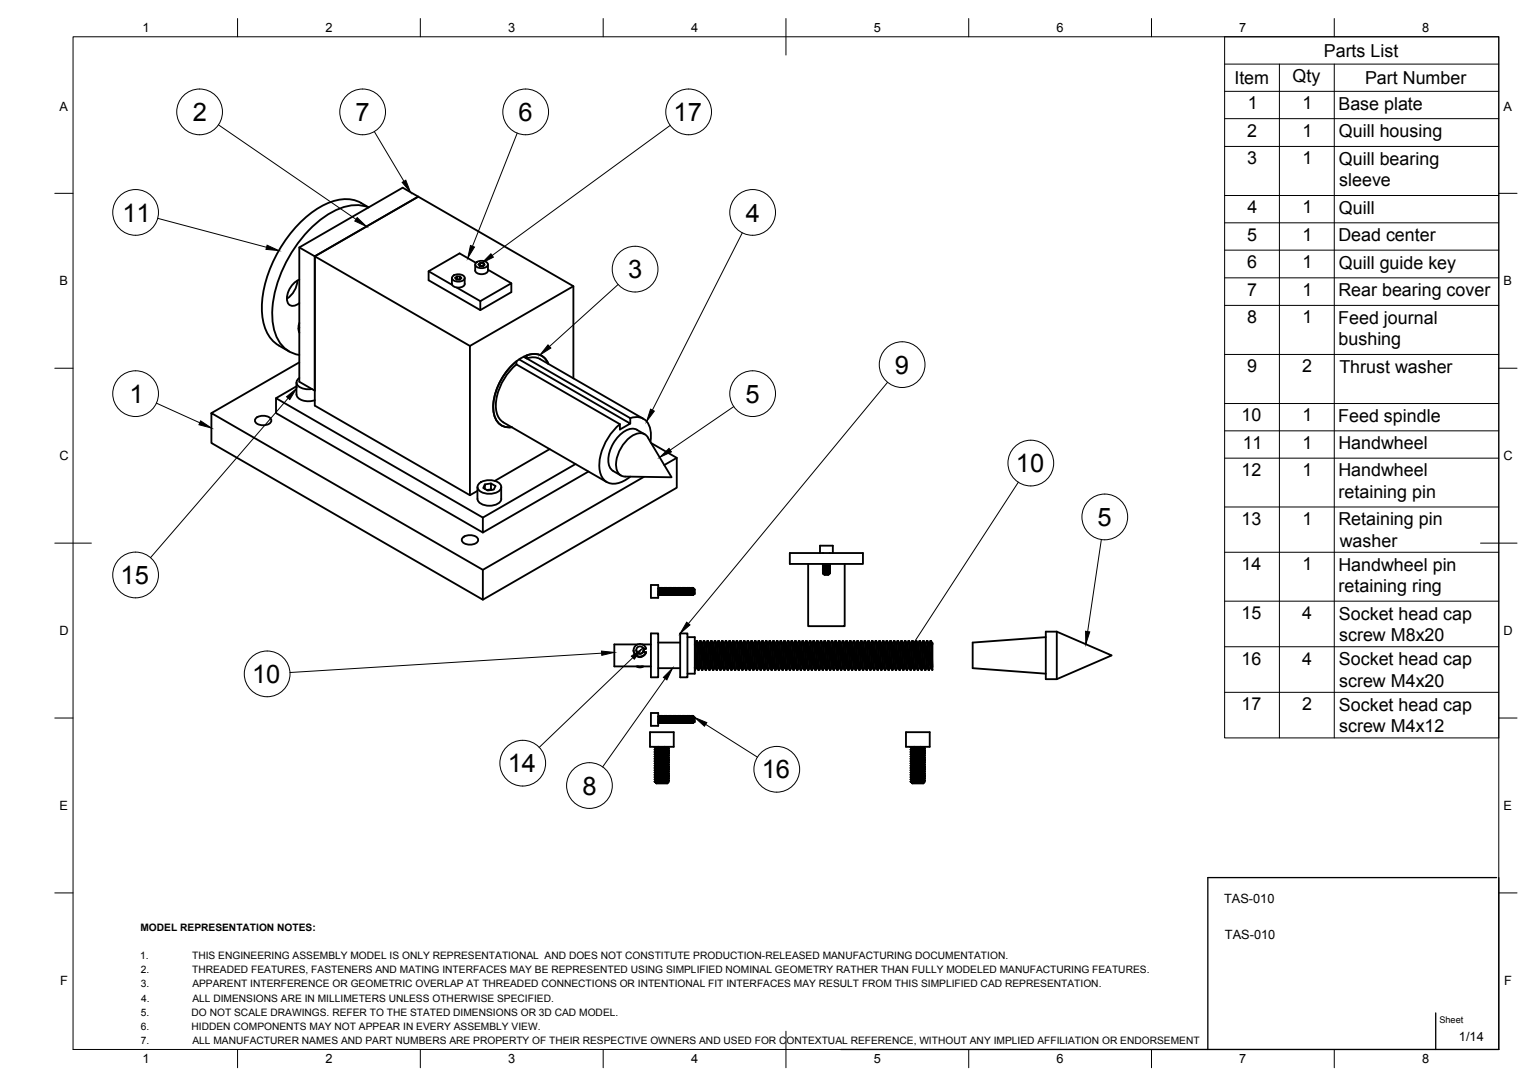
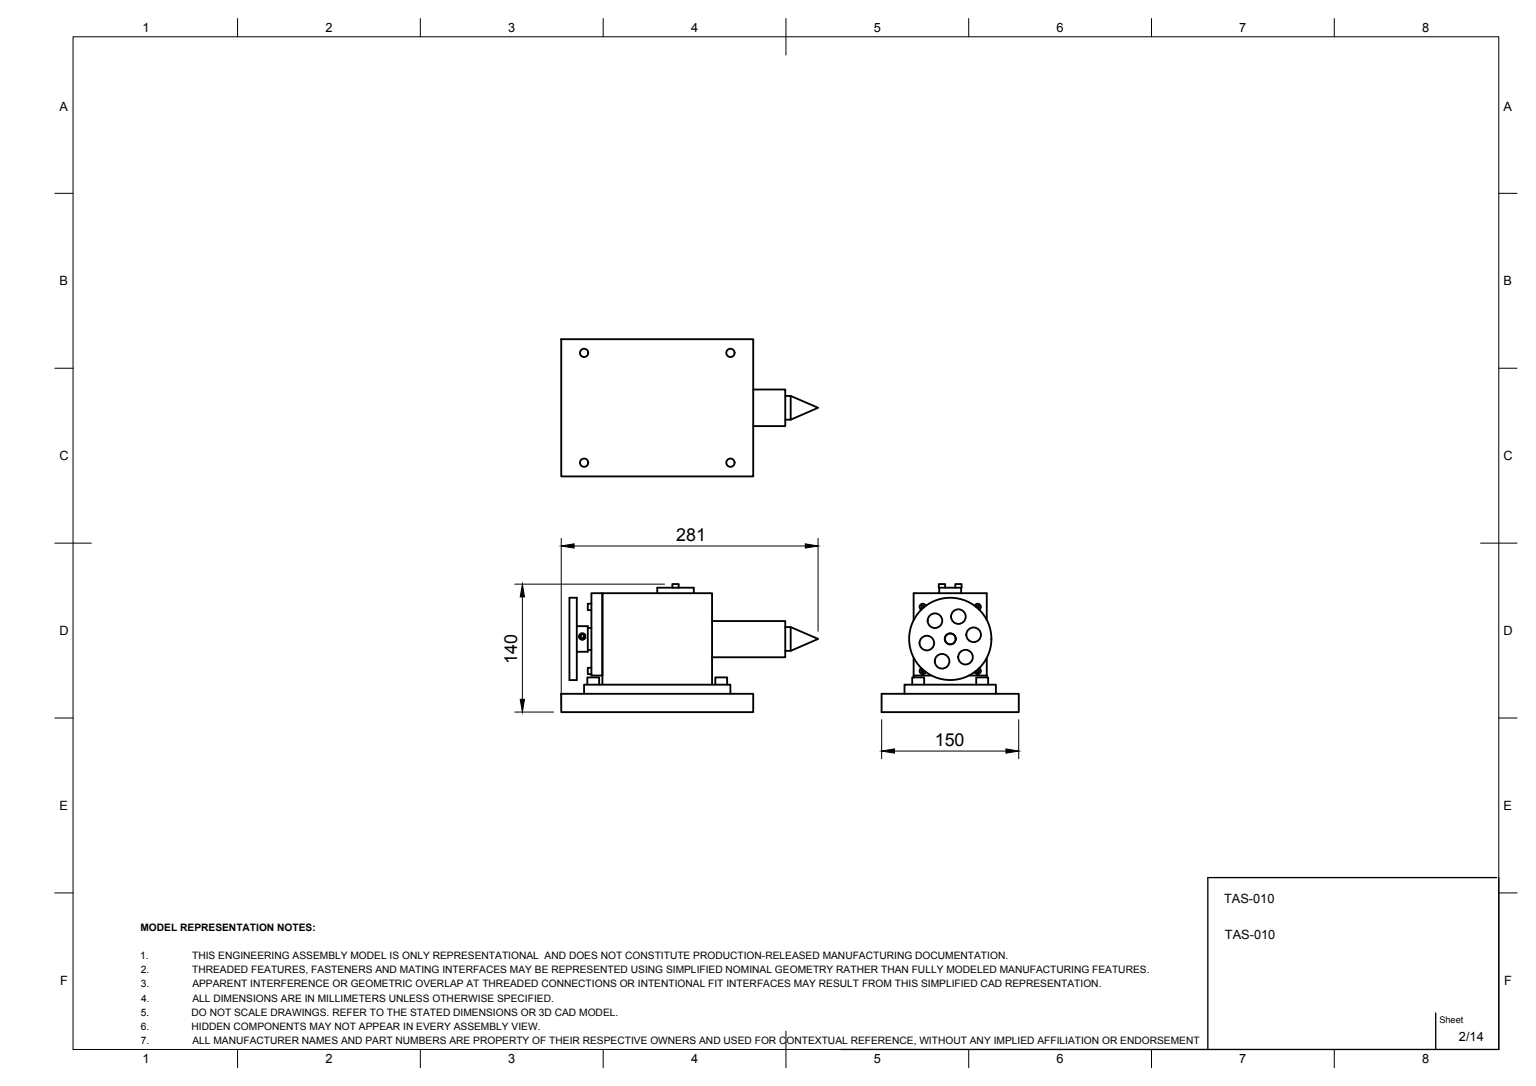
ISO-10303-21;
HEADER;
/* Generated by software containing ST-Developer
 * from STEP Tools, Inc. (www.steptools.com) 
 */

FILE_DESCRIPTION(
/* description */ (
'Independent keyed-quill tailstock, native coupled50mm slider andM16x2
 feed screw, conical dead center, bronze sleeves/thrust washers, cross
-pinned handwheel and bolted guide key. Custom center taper; no standa
rd taper compatibility, machine-bed compatibility or load rating assig
ned.'),
/* implementation_level */ '2;1');

FILE_NAME(
/* name */ 'TAS-010.step',
/* time_stamp */ '2026-11-14T07:17:36-08:00',
/* author */ (''),
/* organization */ (''),
/* preprocessor_version */ 'ST-DEVELOPER v20.2',
/* originating_system */ 'Autodesk Translation Framework v15.17.0.0',
/* authorisation */ '');

FILE_SCHEMA (('AUTOMOTIVE_DESIGN { 1 0 10303 214 3 1 1 }'));
ENDSEC;

DATA;
#10=MECHANICAL_DESIGN_GEOMETRIC_PRESENTATION_REPRESENTATION('',(#153,#154,
#155,#156,#157,#158,#159,#160,#161,#162,#163,#164,#165,#166,#167,#168,#169),
#289387);
#11=ITEM_DEFINED_TRANSFORMATION($,$,#17047,#17864);
#12=ITEM_DEFINED_TRANSFORMATION($,$,#17186,#17865);
#13=ITEM_DEFINED_TRANSFORMATION($,$,#17439,#17866);
#14=ITEM_DEFINED_TRANSFORMATION($,$,#17450,#17867);
#15=ITEM_DEFINED_TRANSFORMATION($,$,#17525,#17868);
#16=ITEM_DEFINED_TRANSFORMATION($,$,#17535,#17869);
#17=ITEM_DEFINED_TRANSFORMATION($,$,#17553,#17870);
#18=ITEM_DEFINED_TRANSFORMATION($,$,#17575,#17871);
#19=ITEM_DEFINED_TRANSFORMATION($,$,#17738,#17872);
#20=ITEM_DEFINED_TRANSFORMATION($,$,#17584,#17873);
#21=ITEM_DEFINED_TRANSFORMATION($,$,#17667,#17874);
#22=ITEM_DEFINED_TRANSFORMATION($,$,#17700,#17875);
#23=ITEM_DEFINED_TRANSFORMATION($,$,#17718,#17876);
#24=ITEM_DEFINED_TRANSFORMATION($,$,#17727,#17877);
#25=ITEM_DEFINED_TRANSFORMATION($,$,#17747,#17878);
#26=ITEM_DEFINED_TRANSFORMATION($,$,#17788,#17879);
#27=ITEM_DEFINED_TRANSFORMATION($,$,#17842,#17880);
#28=ITEM_DEFINED_TRANSFORMATION($,$,#17738,#17881);
#29=ITEM_DEFINED_TRANSFORMATION($,$,#17747,#17882);
#30=ITEM_DEFINED_TRANSFORMATION($,$,#17747,#17883);
#31=ITEM_DEFINED_TRANSFORMATION($,$,#17747,#17884);
#32=ITEM_DEFINED_TRANSFORMATION($,$,#17788,#17885);
#33=ITEM_DEFINED_TRANSFORMATION($,$,#17788,#17886);
#34=ITEM_DEFINED_TRANSFORMATION($,$,#17788,#17887);
#35=ITEM_DEFINED_TRANSFORMATION($,$,#17842,#17888);
#36=(
REPRESENTATION_RELATIONSHIP($,$,#289454,#289453)
REPRESENTATION_RELATIONSHIP_WITH_TRANSFORMATION(#11)
SHAPE_REPRESENTATION_RELATIONSHIP()
);
#37=(
REPRESENTATION_RELATIONSHIP($,$,#289455,#289453)
REPRESENTATION_RELATIONSHIP_WITH_TRANSFORMATION(#12)
SHAPE_REPRESENTATION_RELATIONSHIP()
);
#38=(
REPRESENTATION_RELATIONSHIP($,$,#289456,#289453)
REPRESENTATION_RELATIONSHIP_WITH_TRANSFORMATION(#13)
SHAPE_REPRESENTATION_RELATIONSHIP()
);
#39=(
REPRESENTATION_RELATIONSHIP($,$,#289457,#289453)
REPRESENTATION_RELATIONSHIP_WITH_TRANSFORMATION(#14)
SHAPE_REPRESENTATION_RELATIONSHIP()
);
#40=(
REPRESENTATION_RELATIONSHIP($,$,#289458,#289453)
REPRESENTATION_RELATIONSHIP_WITH_TRANSFORMATION(#15)
SHAPE_REPRESENTATION_RELATIONSHIP()
);
#41=(
REPRESENTATION_RELATIONSHIP($,$,#289459,#289453)
REPRESENTATION_RELATIONSHIP_WITH_TRANSFORMATION(#16)
SHAPE_REPRESENTATION_RELATIONSHIP()
);
#42=(
REPRESENTATION_RELATIONSHIP($,$,#289460,#289453)
REPRESENTATION_RELATIONSHIP_WITH_TRANSFORMATION(#17)
SHAPE_REPRESENTATION_RELATIONSHIP()
);
#43=(
REPRESENTATION_RELATIONSHIP($,$,#289461,#289453)
REPRESENTATION_RELATIONSHIP_WITH_TRANSFORMATION(#18)
SHAPE_REPRESENTATION_RELATIONSHIP()
);
#44=(
REPRESENTATION_RELATIONSHIP($,$,#289467,#289453)
REPRESENTATION_RELATIONSHIP_WITH_TRANSFORMATION(#19)
SHAPE_REPRESENTATION_RELATIONSHIP()
);
#45=(
REPRESENTATION_RELATIONSHIP($,$,#289462,#289453)
REPRESENTATION_RELATIONSHIP_WITH_TRANSFORMATION(#20)
SHAPE_REPRESENTATION_RELATIONSHIP()
);
#46=(
REPRESENTATION_RELATIONSHIP($,$,#289463,#289453)
REPRESENTATION_RELATIONSHIP_WITH_TRANSFORMATION(#21)
SHAPE_REPRESENTATION_RELATIONSHIP()
);
#47=(
REPRESENTATION_RELATIONSHIP($,$,#289464,#289453)
REPRESENTATION_RELATIONSHIP_WITH_TRANSFORMATION(#22)
SHAPE_REPRESENTATION_RELATIONSHIP()
);
#48=(
REPRESENTATION_RELATIONSHIP($,$,#289465,#289453)
REPRESENTATION_RELATIONSHIP_WITH_TRANSFORMATION(#23)
SHAPE_REPRESENTATION_RELATIONSHIP()
);
#49=(
REPRESENTATION_RELATIONSHIP($,$,#289466,#289453)
REPRESENTATION_RELATIONSHIP_WITH_TRANSFORMATION(#24)
SHAPE_REPRESENTATION_RELATIONSHIP()
);
#50=(
REPRESENTATION_RELATIONSHIP($,$,#289468,#289453)
REPRESENTATION_RELATIONSHIP_WITH_TRANSFORMATION(#25)
SHAPE_REPRESENTATION_RELATIONSHIP()
);
#51=(
REPRESENTATION_RELATIONSHIP($,$,#289469,#289453)
REPRESENTATION_RELATIONSHIP_WITH_TRANSFORMATION(#26)
SHAPE_REPRESENTATION_RELATIONSHIP()
);
#52=(
REPRESENTATION_RELATIONSHIP($,$,#289470,#289453)
REPRESENTATION_RELATIONSHIP_WITH_TRANSFORMATION(#27)
SHAPE_REPRESENTATION_RELATIONSHIP()
);
#53=(
REPRESENTATION_RELATIONSHIP($,$,#289467,#289453)
REPRESENTATION_RELATIONSHIP_WITH_TRANSFORMATION(#28)
SHAPE_REPRESENTATION_RELATIONSHIP()
);
#54=(
REPRESENTATION_RELATIONSHIP($,$,#289468,#289453)
REPRESENTATION_RELATIONSHIP_WITH_TRANSFORMATION(#29)
SHAPE_REPRESENTATION_RELATIONSHIP()
);
#55=(
REPRESENTATION_RELATIONSHIP($,$,#289468,#289453)
REPRESENTATION_RELATIONSHIP_WITH_TRANSFORMATION(#30)
SHAPE_REPRESENTATION_RELATIONSHIP()
);
#56=(
REPRESENTATION_RELATIONSHIP($,$,#289468,#289453)
REPRESENTATION_RELATIONSHIP_WITH_TRANSFORMATION(#31)
SHAPE_REPRESENTATION_RELATIONSHIP()
);
#57=(
REPRESENTATION_RELATIONSHIP($,$,#289469,#289453)
REPRESENTATION_RELATIONSHIP_WITH_TRANSFORMATION(#32)
SHAPE_REPRESENTATION_RELATIONSHIP()
);
#58=(
REPRESENTATION_RELATIONSHIP($,$,#289469,#289453)
REPRESENTATION_RELATIONSHIP_WITH_TRANSFORMATION(#33)
SHAPE_REPRESENTATION_RELATIONSHIP()
);
#59=(
REPRESENTATION_RELATIONSHIP($,$,#289469,#289453)
REPRESENTATION_RELATIONSHIP_WITH_TRANSFORMATION(#34)
SHAPE_REPRESENTATION_RELATIONSHIP()
);
#60=(
REPRESENTATION_RELATIONSHIP($,$,#289470,#289453)
REPRESENTATION_RELATIONSHIP_WITH_TRANSFORMATION(#35)
SHAPE_REPRESENTATION_RELATIONSHIP()
);
#61=CONTEXT_DEPENDENT_SHAPE_REPRESENTATION(#36,#289428);
#62=CONTEXT_DEPENDENT_SHAPE_REPRESENTATION(#37,#289429);
#63=CONTEXT_DEPENDENT_SHAPE_REPRESENTATION(#38,#289430);
#64=CONTEXT_DEPENDENT_SHAPE_REPRESENTATION(#39,#289431);
#65=CONTEXT_DEPENDENT_SHAPE_REPRESENTATION(#40,#289432);
#66=CONTEXT_DEPENDENT_SHAPE_REPRESENTATION(#41,#289433);
#67=CONTEXT_DEPENDENT_SHAPE_REPRESENTATION(#42,#289434);
#68=CONTEXT_DEPENDENT_SHAPE_REPRESENTATION(#43,#289435);
#69=CONTEXT_DEPENDENT_SHAPE_REPRESENTATION(#44,#289436);
#70=CONTEXT_DEPENDENT_SHAPE_REPRESENTATION(#45,#289437);
#71=CONTEXT_DEPENDENT_SHAPE_REPRESENTATION(#46,#289438);
#72=CONTEXT_DEPENDENT_SHAPE_REPRESENTATION(#47,#289439);
#73=CONTEXT_DEPENDENT_SHAPE_REPRESENTATION(#48,#289440);
#74=CONTEXT_DEPENDENT_SHAPE_REPRESENTATION(#49,#289441);
#75=CONTEXT_DEPENDENT_SHAPE_REPRESENTATION(#50,#289442);
#76=CONTEXT_DEPENDENT_SHAPE_REPRESENTATION(#51,#289443);
#77=CONTEXT_DEPENDENT_SHAPE_REPRESENTATION(#52,#289444);
#78=CONTEXT_DEPENDENT_SHAPE_REPRESENTATION(#53,#289445);
#79=CONTEXT_DEPENDENT_SHAPE_REPRESENTATION(#54,#289446);
#80=CONTEXT_DEPENDENT_SHAPE_REPRESENTATION(#55,#289447);
#81=CONTEXT_DEPENDENT_SHAPE_REPRESENTATION(#56,#289448);
#82=CONTEXT_DEPENDENT_SHAPE_REPRESENTATION(#57,#289449);
#83=CONTEXT_DEPENDENT_SHAPE_REPRESENTATION(#58,#289450);
#84=CONTEXT_DEPENDENT_SHAPE_REPRESENTATION(#59,#289451);
#85=CONTEXT_DEPENDENT_SHAPE_REPRESENTATION(#60,#289452);
#86=NEXT_ASSEMBLY_USAGE_OCCURRENCE('Base plate:1','Base plate:1',
'Base plate:1',#289472,#289473,'Base plate:1');
#87=NEXT_ASSEMBLY_USAGE_OCCURRENCE('Quill housing:1','Quill housing:1',
'Quill housing:1',#289472,#289474,'Quill housing:1');
#88=NEXT_ASSEMBLY_USAGE_OCCURRENCE('Quill bearing sleeve:1',
'Quill bearing sleeve:1','Quill bearing sleeve:1',#289472,#289475,
'Quill bearing sleeve:1');
#89=NEXT_ASSEMBLY_USAGE_OCCURRENCE('Quill:1','Quill:1','Quill:1',#289472,
#289476,'Quill:1');
#90=NEXT_ASSEMBLY_USAGE_OCCURRENCE('Dead center:1','Dead center:1',
'Dead center:1',#289472,#289477,'Dead center:1');
#91=NEXT_ASSEMBLY_USAGE_OCCURRENCE('Quill guide key:1',
'Quill guide key:1','Quill guide key:1',#289472,#289478,
'Quill guide key:1');
#92=NEXT_ASSEMBLY_USAGE_OCCURRENCE('Rear bearing cover:1',
'Rear bearing cover:1','Rear bearing cover:1',#289472,#289479,
'Rear bearing cover:1');
#93=NEXT_ASSEMBLY_USAGE_OCCURRENCE('Feed journal bushing:1',
'Feed journal bushing:1','Feed journal bushing:1',#289472,#289480,
'Feed journal bushing:1');
#94=NEXT_ASSEMBLY_USAGE_OCCURRENCE('Thrust washer:1','Thrust washer:1',
'Thrust washer:1',#289472,#289486,'Thrust washer:1');
#95=NEXT_ASSEMBLY_USAGE_OCCURRENCE('Feed spindle:1','Feed spindle:1',
'Feed spindle:1',#289472,#289481,'Feed spindle:1');
#96=NEXT_ASSEMBLY_USAGE_OCCURRENCE('Handwheel:1','Handwheel:1',
'Handwheel:1',#289472,#289482,'Handwheel:1');
#97=NEXT_ASSEMBLY_USAGE_OCCURRENCE('Handwheel retaining pin:1',
'Handwheel retaining pin:1','Handwheel retaining pin:1',#289472,#289483,
'Handwheel retaining pin:1');
#98=NEXT_ASSEMBLY_USAGE_OCCURRENCE('Retaining pin washer:1',
'Retaining pin washer:1','Retaining pin washer:1',#289472,#289484,
'Retaining pin washer:1');
#99=NEXT_ASSEMBLY_USAGE_OCCURRENCE('Handwheel pin retaining ring:1',
'Handwheel pin retaining ring:1','Handwheel pin retaining ring:1',#289472,
#289485,'Handwheel pin retaining ring:1');
#100=NEXT_ASSEMBLY_USAGE_OCCURRENCE('Socket head cap screw M8x20:1',
'Socket head cap screw M8x20:1','Socket head cap screw M8x20:1',#289472,
#289487,'Socket head cap screw M8x20:1');
#101=NEXT_ASSEMBLY_USAGE_OCCURRENCE('Socket head cap screw M4x20:1',
'Socket head cap screw M4x20:1','Socket head cap screw M4x20:1',#289472,
#289488,'Socket head cap screw M4x20:1');
#102=NEXT_ASSEMBLY_USAGE_OCCURRENCE('Socket head cap screw M4x12:1',
'Socket head cap screw M4x12:1','Socket head cap screw M4x12:1',#289472,
#289489,'Socket head cap screw M4x12:1');
#103=NEXT_ASSEMBLY_USAGE_OCCURRENCE('Thrust washer:2','Thrust washer:2',
'Thrust washer:2',#289472,#289486,'Thrust washer:2');
#104=NEXT_ASSEMBLY_USAGE_OCCURRENCE('Socket head cap screw M8x20:2',
'Socket head cap screw M8x20:2','Socket head cap screw M8x20:2',#289472,
#289487,'Socket head cap screw M8x20:2');
#105=NEXT_ASSEMBLY_USAGE_OCCURRENCE('Socket head cap screw M8x20:3',
'Socket head cap screw M8x20:3','Socket head cap screw M8x20:3',#289472,
#289487,'Socket head cap screw M8x20:3');
#106=NEXT_ASSEMBLY_USAGE_OCCURRENCE('Socket head cap screw M8x20:4',
'Socket head cap screw M8x20:4','Socket head cap screw M8x20:4',#289472,
#289487,'Socket head cap screw M8x20:4');
#107=NEXT_ASSEMBLY_USAGE_OCCURRENCE('Socket head cap screw M4x20:2',
'Socket head cap screw M4x20:2','Socket head cap screw M4x20:2',#289472,
#289488,'Socket head cap screw M4x20:2');
#108=NEXT_ASSEMBLY_USAGE_OCCURRENCE('Socket head cap screw M4x20:3',
'Socket head cap screw M4x20:3','Socket head cap screw M4x20:3',#289472,
#289488,'Socket head cap screw M4x20:3');
#109=NEXT_ASSEMBLY_USAGE_OCCURRENCE('Socket head cap screw M4x20:4',
'Socket head cap screw M4x20:4','Socket head cap screw M4x20:4',#289472,
#289488,'Socket head cap screw M4x20:4');
#110=NEXT_ASSEMBLY_USAGE_OCCURRENCE('Socket head cap screw M4x12:2',
'Socket head cap screw M4x12:2','Socket head cap screw M4x12:2',#289472,
#289489,'Socket head cap screw M4x12:2');
#111=CONICAL_SURFACE('',#17511,8.5,0.0748598477107669);
#112=CONICAL_SURFACE('',#17528,8.5,0.0748598477107669);
#113=CONICAL_SURFACE('',#17534,13.,0.408907828950925);
#114=CONICAL_SURFACE('',#17748,3.5,0.785398163397448);
#115=CONICAL_SURFACE('',#17774,3.5,0.785398163397448);
#116=CONICAL_SURFACE('',#17789,1.5,0.785398163397448);
#117=CONICAL_SURFACE('',#17828,1.5,0.785398163397448);
#118=CONICAL_SURFACE('',#17849,1.5,0.785398163397449);
#119=SHAPE_REPRESENTATION_RELATIONSHIP('SRR','None',#289454,#136);
#120=SHAPE_REPRESENTATION_RELATIONSHIP('SRR','None',#289455,#137);
#121=SHAPE_REPRESENTATION_RELATIONSHIP('SRR','None',#289456,#138);
#122=SHAPE_REPRESENTATION_RELATIONSHIP('SRR','None',#289457,#139);
#123=SHAPE_REPRESENTATION_RELATIONSHIP('SRR','None',#289458,#140);
#124=SHAPE_REPRESENTATION_RELATIONSHIP('SRR','None',#289459,#141);
#125=SHAPE_REPRESENTATION_RELATIONSHIP('SRR','None',#289460,#142);
#126=SHAPE_REPRESENTATION_RELATIONSHIP('SRR','None',#289461,#143);
#127=SHAPE_REPRESENTATION_RELATIONSHIP('SRR','None',#289462,#144);
#128=SHAPE_REPRESENTATION_RELATIONSHIP('SRR','None',#289463,#145);
#129=SHAPE_REPRESENTATION_RELATIONSHIP('SRR','None',#289464,#146);
#130=SHAPE_REPRESENTATION_RELATIONSHIP('SRR','None',#289465,#147);
#131=SHAPE_REPRESENTATION_RELATIONSHIP('SRR','None',#289466,#148);
#132=SHAPE_REPRESENTATION_RELATIONSHIP('SRR','None',#289467,#149);
#133=SHAPE_REPRESENTATION_RELATIONSHIP('SRR','None',#289468,#150);
#134=SHAPE_REPRESENTATION_RELATIONSHIP('SRR','None',#289469,#151);
#135=SHAPE_REPRESENTATION_RELATIONSHIP('SRR','None',#289470,#152);
#136=ADVANCED_BREP_SHAPE_REPRESENTATION('',(#170),#289370);
#137=ADVANCED_BREP_SHAPE_REPRESENTATION('',(#171),#289371);
#138=ADVANCED_BREP_SHAPE_REPRESENTATION('',(#172),#289372);
#139=ADVANCED_BREP_SHAPE_REPRESENTATION('',(#173),#289373);
#140=ADVANCED_BREP_SHAPE_REPRESENTATION('',(#174),#289374);
#141=ADVANCED_BREP_SHAPE_REPRESENTATION('',(#175),#289375);
#142=ADVANCED_BREP_SHAPE_REPRESENTATION('',(#176),#289376);
#143=ADVANCED_BREP_SHAPE_REPRESENTATION('',(#177),#289377);
#144=ADVANCED_BREP_SHAPE_REPRESENTATION('',(#178),#289378);
#145=ADVANCED_BREP_SHAPE_REPRESENTATION('',(#179),#289379);
#146=ADVANCED_BREP_SHAPE_REPRESENTATION('',(#180),#289380);
#147=ADVANCED_BREP_SHAPE_REPRESENTATION('',(#181),#289381);
#148=ADVANCED_BREP_SHAPE_REPRESENTATION('',(#182),#289382);
#149=ADVANCED_BREP_SHAPE_REPRESENTATION('',(#183),#289383);
#150=ADVANCED_BREP_SHAPE_REPRESENTATION('',(#184),#289384);
#151=ADVANCED_BREP_SHAPE_REPRESENTATION('',(#185),#289385);
#152=ADVANCED_BREP_SHAPE_REPRESENTATION('',(#186),#289386);
#153=STYLED_ITEM('',(#289548),#170);
#154=STYLED_ITEM('',(#289549),#171);
#155=STYLED_ITEM('',(#289550),#172);
#156=STYLED_ITEM('',(#289551),#173);
#157=STYLED_ITEM('',(#289548),#174);
#158=STYLED_ITEM('',(#289552),#175);
#159=STYLED_ITEM('',(#289552),#176);
#160=STYLED_ITEM('',(#289550),#177);
#161=STYLED_ITEM('',(#289548),#178);
#162=STYLED_ITEM('',(#289549),#179);
#163=STYLED_ITEM('',(#289548),#180);
#164=STYLED_ITEM('',(#289550),#181);
#165=STYLED_ITEM('',(#289553),#182);
#166=STYLED_ITEM('',(#289550),#183);
#167=STYLED_ITEM('',(#289553),#184);
#168=STYLED_ITEM('',(#289553),#185);
#169=STYLED_ITEM('',(#289553),#186);
#170=MANIFOLD_SOLID_BREP('Body1',#16841);
#171=MANIFOLD_SOLID_BREP('Body1',#16842);
#172=MANIFOLD_SOLID_BREP('Body1',#16843);
#173=MANIFOLD_SOLID_BREP('Body1',#16844);
#174=MANIFOLD_SOLID_BREP('Body1',#16845);
#175=MANIFOLD_SOLID_BREP('Body1',#16846);
#176=MANIFOLD_SOLID_BREP('Body1',#16847);
#177=MANIFOLD_SOLID_BREP('Body1',#16848);
#178=MANIFOLD_SOLID_BREP('Body1',#16849);
#179=MANIFOLD_SOLID_BREP('Body1',#16850);
#180=MANIFOLD_SOLID_BREP('Body1',#16851);
#181=MANIFOLD_SOLID_BREP('Body1',#16852);
#182=MANIFOLD_SOLID_BREP('Body1',#16853);
#183=MANIFOLD_SOLID_BREP('Body1',#16854);
#184=MANIFOLD_SOLID_BREP('Body1',#16855);
#185=MANIFOLD_SOLID_BREP('Body1',#16856);
#186=MANIFOLD_SOLID_BREP('Body1',#16857);
#187=FACE_BOUND('',#1186,.T.);
#188=FACE_BOUND('',#1187,.T.);
#189=FACE_BOUND('',#1188,.T.);
#190=FACE_BOUND('',#1189,.T.);
#191=FACE_BOUND('',#1190,.T.);
#192=FACE_BOUND('',#1191,.T.);
#193=FACE_BOUND('',#1192,.T.);
#194=FACE_BOUND('',#1193,.T.);
#195=FACE_BOUND('',#1195,.T.);
#196=FACE_BOUND('',#1196,.T.);
#197=FACE_BOUND('',#1197,.T.);
#198=FACE_BOUND('',#1198,.T.);
#199=FACE_BOUND('',#1414,.T.);
#200=FACE_BOUND('',#1416,.T.);
#201=FACE_BOUND('',#1417,.T.);
#202=FACE_BOUND('',#1418,.T.);
#203=FACE_BOUND('',#1419,.T.);
#204=FACE_BOUND('',#1420,.T.);
#205=FACE_BOUND('',#1426,.T.);
#206=FACE_BOUND('',#1427,.T.);
#207=FACE_BOUND('',#1428,.T.);
#208=FACE_BOUND('',#1429,.T.);
#209=FACE_BOUND('',#1432,.T.);
#210=FACE_BOUND('',#1435,.T.);
#211=FACE_BOUND('',#1436,.T.);
#212=FACE_BOUND('',#1437,.T.);
#213=FACE_BOUND('',#1438,.T.);
#214=FACE_BOUND('',#1439,.T.);
#215=FACE_BOUND('',#1441,.T.);
#216=FACE_BOUND('',#1442,.T.);
#217=FACE_BOUND('',#1443,.T.);
#218=FACE_BOUND('',#1502,.T.);
#219=FACE_BOUND('',#1508,.T.);
#220=FACE_BOUND('',#1513,.T.);
#221=FACE_BOUND('',#1517,.T.);
#222=FACE_BOUND('',#1521,.T.);
#223=FACE_BOUND('',#1527,.T.);
#224=FACE_BOUND('',#1528,.T.);
#225=FACE_BOUND('',#1529,.T.);
#226=FACE_BOUND('',#1535,.T.);
#227=FACE_BOUND('',#1536,.T.);
#228=FACE_BOUND('',#1545,.T.);
#229=FACE_BOUND('',#1546,.T.);
#230=FACE_BOUND('',#1547,.T.);
#231=FACE_BOUND('',#1548,.T.);
#232=FACE_BOUND('',#1549,.T.);
#233=FACE_BOUND('',#1558,.T.);
#234=FACE_BOUND('',#1559,.T.);
#235=FACE_BOUND('',#1560,.T.);
#236=FACE_BOUND('',#1561,.T.);
#237=FACE_BOUND('',#1562,.T.);
#238=FACE_BOUND('',#1566,.T.);
#239=FACE_BOUND('',#1568,.T.);
#240=FACE_BOUND('',#1641,.T.);
#241=FACE_BOUND('',#1644,.T.);
#242=FACE_BOUND('',#1646,.T.);
#243=FACE_BOUND('',#1657,.T.);
#244=FACE_BOUND('',#1659,.T.);
#245=FACE_BOUND('',#1661,.T.);
#246=FACE_BOUND('',#1664,.T.);
#247=FACE_BOUND('',#1665,.T.);
#248=FACE_BOUND('',#1666,.T.);
#249=FACE_BOUND('',#1667,.T.);
#250=FACE_BOUND('',#1668,.T.);
#251=FACE_BOUND('',#1669,.T.);
#252=FACE_BOUND('',#1670,.T.);
#253=FACE_BOUND('',#1672,.T.);
#254=FACE_BOUND('',#1673,.T.);
#255=FACE_BOUND('',#1674,.T.);
#256=FACE_BOUND('',#1675,.T.);
#257=FACE_BOUND('',#1676,.T.);
#258=FACE_BOUND('',#1677,.T.);
#259=FACE_BOUND('',#1678,.T.);
#260=FACE_BOUND('',#1681,.T.);
#261=FACE_BOUND('',#1683,.T.);
#262=FACE_BOUND('',#1686,.T.);
#263=FACE_BOUND('',#1694,.T.);
#264=FACE_BOUND('',#1696,.T.);
#265=FACE_BOUND('',#1706,.T.);
#266=FACE_BOUND('',#1708,.T.);
#267=FACE_BOUND('',#1739,.T.);
#268=FACE_BOUND('',#1742,.T.);
#269=FACE_BOUND('',#1786,.T.);
#270=FACE_BOUND('',#1789,.T.);
#271=FACE_BOUND('',#1804,.T.);
#272=FACE_BOUND('',#1807,.T.);
#273=B_SPLINE_SURFACE_WITH_KNOTS('',3,3,((#55782,#55783,#55784,#55785,#55786,
#55787,#55788,#55789,#55790,#55791,#55792,#55793,#55794,#55795,#55796,#55797,
#55798,#55799,#55800,#55801,#55802,#55803,#55804,#55805,#55806,#55807,#55808,
#55809,#55810,#55811,#55812,#55813,#55814,#55815,#55816,#55817,#55818,#55819,
#55820,#55821,#55822,#55823,#55824,#55825,#55826,#55827,#55828,#55829,#55830,
#55831,#55832,#55833,#55834,#55835,#55836,#55837,#55838,#55839,#55840,#55841,
#55842,#55843,#55844,#55845,#55846,#55847,#55848,#55849,#55850,#55851,#55852),
(#55853,#55854,#55855,#55856,#55857,#55858,#55859,#55860,#55861,#55862,
#55863,#55864,#55865,#55866,#55867,#55868,#55869,#55870,#55871,#55872,#55873,
#55874,#55875,#55876,#55877,#55878,#55879,#55880,#55881,#55882,#55883,#55884,
#55885,#55886,#55887,#55888,#55889,#55890,#55891,#55892,#55893,#55894,#55895,
#55896,#55897,#55898,#55899,#55900,#55901,#55902,#55903,#55904,#55905,#55906,
#55907,#55908,#55909,#55910,#55911,#55912,#55913,#55914,#55915,#55916,#55917,
#55918,#55919,#55920,#55921,#55922,#55923),(#55924,#55925,#55926,#55927,
#55928,#55929,#55930,#55931,#55932,#55933,#55934,#55935,#55936,#55937,#55938,
#55939,#55940,#55941,#55942,#55943,#55944,#55945,#55946,#55947,#55948,#55949,
#55950,#55951,#55952,#55953,#55954,#55955,#55956,#55957,#55958,#55959,#55960,
#55961,#55962,#55963,#55964,#55965,#55966,#55967,#55968,#55969,#55970,#55971,
#55972,#55973,#55974,#55975,#55976,#55977,#55978,#55979,#55980,#55981,#55982,
#55983,#55984,#55985,#55986,#55987,#55988,#55989,#55990,#55991,#55992,#55993,
#55994),(#55995,#55996,#55997,#55998,#55999,#56000,#56001,#56002,#56003,
#56004,#56005,#56006,#56007,#56008,#56009,#56010,#56011,#56012,#56013,#56014,
#56015,#56016,#56017,#56018,#56019,#56020,#56021,#56022,#56023,#56024,#56025,
#56026,#56027,#56028,#56029,#56030,#56031,#56032,#56033,#56034,#56035,#56036,
#56037,#56038,#56039,#56040,#56041,#56042,#56043,#56044,#56045,#56046,#56047,
#56048,#56049,#56050,#56051,#56052,#56053,#56054,#56055,#56056,#56057,#56058,
#56059,#56060,#56061,#56062,#56063,#56064,#56065)),.UNSPECIFIED.,.F.,.F.,
 .F.,(4,4),(4,1,1,1,1,1,1,1,1,1,1,1,1,1,1,1,1,1,1,1,1,1,1,1,1,1,1,1,1,1,
1,1,1,1,1,1,1,1,1,1,1,1,1,1,1,1,1,1,1,1,1,1,1,1,1,1,1,1,1,1,1,1,1,1,1,1,
1,1,4),(-0.000703873626500094,0.0807256881124021),(11.8568339491899,12.8481671993964,
13.8387965759765,14.8294259525565,15.8200553291365,16.8106847057165,17.8013140822966,
18.7919434588766,19.7825728354566,20.7732022120367,21.7638315886167,22.7544609651967,
23.7450903417767,24.7357197183568,25.7263490949368,26.7169784715168,27.7076078480968,
28.6982372246769,29.6888666012569,30.6794959778369,31.6701253544169,32.660754730997,
33.651384107577,34.642013484157,35.6326428607371,36.6232722373171,37.6139016138971,
38.6045309904771,39.5951603670572,40.5857897436372,41.5764191202172,42.5670484967972,
43.5576778733773,44.5483072499573,45.5389366265373,46.5295660031174,47.5201953796974,
48.5108247562774,49.5014541328574,50.4920835094375,51.4827128860175,52.4733422625975,
53.4639716391775,54.4546010157576,55.4452303923376,56.4358597689176,57.4264891454977,
58.4171185220777,59.4077478986577,60.3983772752377,61.3890066518178,62.3796360283978,
63.3702654049778,64.3608947815578,65.3515241581379,66.3421535347179,67.3327829112979,
68.3234122878779,69.314041664458,70.304671041038,71.295300417618,72.2859297941981,
73.2765591707781,74.2671885473581,75.2578179239381,76.2484473005182,77.2390766770982,
78.2297060536782,79.2203354302583),.UNSPECIFIED.);
#274=B_SPLINE_SURFACE_WITH_KNOTS('',3,3,((#56163,#56164,#56165,#56166,#56167,
#56168,#56169,#56170,#56171,#56172,#56173,#56174,#56175,#56176,#56177,#56178,
#56179,#56180,#56181,#56182,#56183,#56184,#56185,#56186,#56187,#56188,#56189,
#56190,#56191,#56192,#56193,#56194,#56195,#56196,#56197,#56198,#56199,#56200,
#56201,#56202,#56203,#56204,#56205,#56206,#56207,#56208,#56209,#56210,#56211,
#56212,#56213,#56214,#56215,#56216,#56217,#56218,#56219,#56220,#56221,#56222,
#56223,#56224,#56225,#56226,#56227,#56228,#56229,#56230,#56231,#56232,#56233),
(#56234,#56235,#56236,#56237,#56238,#56239,#56240,#56241,#56242,#56243,
#56244,#56245,#56246,#56247,#56248,#56249,#56250,#56251,#56252,#56253,#56254,
#56255,#56256,#56257,#56258,#56259,#56260,#56261,#56262,#56263,#56264,#56265,
#56266,#56267,#56268,#56269,#56270,#56271,#56272,#56273,#56274,#56275,#56276,
#56277,#56278,#56279,#56280,#56281,#56282,#56283,#56284,#56285,#56286,#56287,
#56288,#56289,#56290,#56291,#56292,#56293,#56294,#56295,#56296,#56297,#56298,
#56299,#56300,#56301,#56302,#56303,#56304),(#56305,#56306,#56307,#56308,
#56309,#56310,#56311,#56312,#56313,#56314,#56315,#56316,#56317,#56318,#56319,
#56320,#56321,#56322,#56323,#56324,#56325,#56326,#56327,#56328,#56329,#56330,
#56331,#56332,#56333,#56334,#56335,#56336,#56337,#56338,#56339,#56340,#56341,
#56342,#56343,#56344,#56345,#56346,#56347,#56348,#56349,#56350,#56351,#56352,
#56353,#56354,#56355,#56356,#56357,#56358,#56359,#56360,#56361,#56362,#56363,
#56364,#56365,#56366,#56367,#56368,#56369,#56370,#56371,#56372,#56373,#56374,
#56375),(#56376,#56377,#56378,#56379,#56380,#56381,#56382,#56383,#56384,
#56385,#56386,#56387,#56388,#56389,#56390,#56391,#56392,#56393,#56394,#56395,
#56396,#56397,#56398,#56399,#56400,#56401,#56402,#56403,#56404,#56405,#56406,
#56407,#56408,#56409,#56410,#56411,#56412,#56413,#56414,#56415,#56416,#56417,
#56418,#56419,#56420,#56421,#56422,#56423,#56424,#56425,#56426,#56427,#56428,
#56429,#56430,#56431,#56432,#56433,#56434,#56435,#56436,#56437,#56438,#56439,
#56440,#56441,#56442,#56443,#56444,#56445,#56446)),.UNSPECIFIED.,.F.,.F.,
 .F.,(4,4),(4,1,1,1,1,1,1,1,1,1,1,1,1,1,1,1,1,1,1,1,1,1,1,1,1,1,1,1,1,1,
1,1,1,1,1,1,1,1,1,1,1,1,1,1,1,1,1,1,1,1,1,1,1,1,1,1,1,1,1,1,1,1,1,1,1,1,
1,1,4),(-0.000445042829947342,0.0809843050226073),(14.3991256467175,15.3897550232976,
16.3803843998776,17.3710137764576,18.3616431530376,19.3522725296177,20.3429019061977,
21.3335312827777,22.3241606593577,23.3147900359378,24.3054194125178,25.2960487890978,
26.2866781656778,27.2773075422579,28.2679369188379,29.2585662954179,30.249195671998,
31.239825048578,32.230454425158,33.221083801738,34.2117131783181,35.2023425548981,
36.1929719314781,37.1836013080582,38.1742306846382,39.1648600612182,40.1554894377982,
41.1461188143783,42.1367481909583,43.1273775675383,44.1180069441183,45.1086363206984,
46.0992656972784,47.0898950738584,48.0805244504384,49.0711538270185,50.0617832035985,
51.0524125801785,52.0430419567586,53.0336713333386,54.0243007099186,55.0149300864986,
56.0055594630787,56.9961888396587,57.9868182162387,58.9774475928187,59.9680769693988,
60.9587063459788,61.9493357225588,62.9399650991389,63.9305944757189,64.9212238522989,
65.9118532288789,66.902482605459,67.893111982039,68.883741358619,69.8743707351991,
70.8650001117791,71.8556294883591,72.8462588649391,73.8368882415191,74.8275176180992,
75.8181469946792,76.8087763712592,77.7994057478393,78.7900351244193,79.7806645009993,
80.7712938775793,81.7626270042512),.UNSPECIFIED.);
#275=B_SPLINE_SURFACE_WITH_KNOTS('',3,3,((#56747,#56748,#56749,#56750,#56751,
#56752,#56753,#56754,#56755,#56756,#56757,#56758,#56759,#56760,#56761,#56762,
#56763,#56764,#56765,#56766,#56767,#56768,#56769,#56770,#56771,#56772,#56773,
#56774,#56775,#56776,#56777,#56778,#56779,#56780,#56781,#56782,#56783,#56784,
#56785,#56786,#56787,#56788,#56789,#56790,#56791,#56792,#56793,#56794,#56795,
#56796,#56797,#56798,#56799,#56800,#56801,#56802,#56803,#56804,#56805,#56806,
#56807,#56808,#56809,#56810,#56811,#56812,#56813,#56814,#56815,#56816,#56817),
(#56818,#56819,#56820,#56821,#56822,#56823,#56824,#56825,#56826,#56827,
#56828,#56829,#56830,#56831,#56832,#56833,#56834,#56835,#56836,#56837,#56838,
#56839,#56840,#56841,#56842,#56843,#56844,#56845,#56846,#56847,#56848,#56849,
#56850,#56851,#56852,#56853,#56854,#56855,#56856,#56857,#56858,#56859,#56860,
#56861,#56862,#56863,#56864,#56865,#56866,#56867,#56868,#56869,#56870,#56871,
#56872,#56873,#56874,#56875,#56876,#56877,#56878,#56879,#56880,#56881,#56882,
#56883,#56884,#56885,#56886,#56887,#56888),(#56889,#56890,#56891,#56892,
#56893,#56894,#56895,#56896,#56897,#56898,#56899,#56900,#56901,#56902,#56903,
#56904,#56905,#56906,#56907,#56908,#56909,#56910,#56911,#56912,#56913,#56914,
#56915,#56916,#56917,#56918,#56919,#56920,#56921,#56922,#56923,#56924,#56925,
#56926,#56927,#56928,#56929,#56930,#56931,#56932,#56933,#56934,#56935,#56936,
#56937,#56938,#56939,#56940,#56941,#56942,#56943,#56944,#56945,#56946,#56947,
#56948,#56949,#56950,#56951,#56952,#56953,#56954,#56955,#56956,#56957,#56958,
#56959),(#56960,#56961,#56962,#56963,#56964,#56965,#56966,#56967,#56968,
#56969,#56970,#56971,#56972,#56973,#56974,#56975,#56976,#56977,#56978,#56979,
#56980,#56981,#56982,#56983,#56984,#56985,#56986,#56987,#56988,#56989,#56990,
#56991,#56992,#56993,#56994,#56995,#56996,#56997,#56998,#56999,#57000,#57001,
#57002,#57003,#57004,#57005,#57006,#57007,#57008,#57009,#57010,#57011,#57012,
#57013,#57014,#57015,#57016,#57017,#57018,#57019,#57020,#57021,#57022,#57023,
#57024,#57025,#57026,#57027,#57028,#57029,#57030)),.UNSPECIFIED.,.F.,.F.,
 .F.,(4,4),(4,1,1,1,1,1,1,1,1,1,1,1,1,1,1,1,1,1,1,1,1,1,1,1,1,1,1,1,1,1,
1,1,1,1,1,1,1,1,1,1,1,1,1,1,1,1,1,1,1,1,1,1,1,1,1,1,1,1,1,1,1,1,1,1,1,1,
1,1,4),(-0.000689732099215623,0.0807182050540442),(11.8568480907172,12.8481671993964,
13.8387965759765,14.8294259525565,15.8200553291365,16.8106847057165,17.8013140822966,
18.7919434588766,19.7825728354566,20.7732022120367,21.7638315886167,22.7544609651967,
23.7450903417767,24.7357197183568,25.7263490949368,26.7169784715168,27.7076078480968,
28.6982372246769,29.6888666012569,30.6794959778369,31.6701253544169,32.660754730997,
33.651384107577,34.642013484157,35.6326428607371,36.6232722373171,37.6139016138971,
38.6045309904771,39.5951603670572,40.5857897436372,41.5764191202172,42.5670484967972,
43.5576778733773,44.5483072499573,45.5389366265373,46.5295660031174,47.5201953796974,
48.5108247562774,49.5014541328574,50.4920835094375,51.4827128860175,52.4733422625975,
53.4639716391775,54.4546010157576,55.4452303923376,56.4358597689176,57.4264891454977,
58.4171185220777,59.4077478986577,60.3983772752377,61.3890066518178,62.3796360283978,
63.3702654049778,64.3608947815578,65.3515241581379,66.3421535347179,67.3327829112979,
68.3234122878779,69.314041664458,70.304671041038,71.295300417618,72.2859297941981,
73.2765591707781,74.2671885473581,75.2578179239381,76.2484473005182,77.2390766770982,
78.2297060536782,79.2203354302583),.UNSPECIFIED.);
#276=B_SPLINE_SURFACE_WITH_KNOTS('',3,3,((#57125,#57126,#57127,#57128,#57129,
#57130,#57131,#57132,#57133,#57134,#57135,#57136,#57137,#57138,#57139,#57140,
#57141,#57142,#57143,#57144,#57145,#57146,#57147,#57148,#57149,#57150,#57151,
#57152,#57153,#57154,#57155,#57156,#57157,#57158,#57159,#57160,#57161,#57162,
#57163,#57164,#57165,#57166,#57167,#57168,#57169,#57170,#57171,#57172,#57173,
#57174,#57175,#57176,#57177,#57178,#57179,#57180,#57181,#57182,#57183,#57184,
#57185,#57186,#57187,#57188,#57189,#57190,#57191,#57192,#57193,#57194,#57195),
(#57196,#57197,#57198,#57199,#57200,#57201,#57202,#57203,#57204,#57205,
#57206,#57207,#57208,#57209,#57210,#57211,#57212,#57213,#57214,#57215,#57216,
#57217,#57218,#57219,#57220,#57221,#57222,#57223,#57224,#57225,#57226,#57227,
#57228,#57229,#57230,#57231,#57232,#57233,#57234,#57235,#57236,#57237,#57238,
#57239,#57240,#57241,#57242,#57243,#57244,#57245,#57246,#57247,#57248,#57249,
#57250,#57251,#57252,#57253,#57254,#57255,#57256,#57257,#57258,#57259,#57260,
#57261,#57262,#57263,#57264,#57265,#57266),(#57267,#57268,#57269,#57270,
#57271,#57272,#57273,#57274,#57275,#57276,#57277,#57278,#57279,#57280,#57281,
#57282,#57283,#57284,#57285,#57286,#57287,#57288,#57289,#57290,#57291,#57292,
#57293,#57294,#57295,#57296,#57297,#57298,#57299,#57300,#57301,#57302,#57303,
#57304,#57305,#57306,#57307,#57308,#57309,#57310,#57311,#57312,#57313,#57314,
#57315,#57316,#57317,#57318,#57319,#57320,#57321,#57322,#57323,#57324,#57325,
#57326,#57327,#57328,#57329,#57330,#57331,#57332,#57333,#57334,#57335,#57336,
#57337),(#57338,#57339,#57340,#57341,#57342,#57343,#57344,#57345,#57346,
#57347,#57348,#57349,#57350,#57351,#57352,#57353,#57354,#57355,#57356,#57357,
#57358,#57359,#57360,#57361,#57362,#57363,#57364,#57365,#57366,#57367,#57368,
#57369,#57370,#57371,#57372,#57373,#57374,#57375,#57376,#57377,#57378,#57379,
#57380,#57381,#57382,#57383,#57384,#57385,#57386,#57387,#57388,#57389,#57390,
#57391,#57392,#57393,#57394,#57395,#57396,#57397,#57398,#57399,#57400,#57401,
#57402,#57403,#57404,#57405,#57406,#57407,#57408)),.UNSPECIFIED.,.F.,.F.,
 .F.,(4,4),(4,1,1,1,1,1,1,1,1,1,1,1,1,1,1,1,1,1,1,1,1,1,1,1,1,1,1,1,1,1,
1,1,1,1,1,1,1,1,1,1,1,1,1,1,1,1,1,1,1,1,1,1,1,1,1,1,1,1,1,1,1,1,1,1,1,1,
1,1,4),(-0.000437656372986427,0.0809703040897196),(14.3991256467175,15.3897550232976,
16.3803843998776,17.3710137764576,18.3616431530376,19.3522725296177,20.3429019061977,
21.3335312827777,22.3241606593577,23.3147900359378,24.3054194125178,25.2960487890978,
26.2866781656779,27.2773075422579,28.2679369188379,29.2585662954179,30.249195671998,
31.239825048578,32.230454425158,33.221083801738,34.2117131783181,35.2023425548981,
36.1929719314781,37.1836013080582,38.1742306846382,39.1648600612182,40.1554894377982,
41.1461188143783,42.1367481909583,43.1273775675383,44.1180069441183,45.1086363206984,
46.0992656972784,47.0898950738584,48.0805244504385,49.0711538270185,50.0617832035985,
51.0524125801785,52.0430419567586,53.0336713333386,54.0243007099186,55.0149300864986,
56.0055594630787,56.9961888396587,57.9868182162387,58.9774475928188,59.9680769693988,
60.9587063459788,61.9493357225588,62.9399650991389,63.9305944757189,64.9212238522989,
65.911853228879,66.902482605459,67.893111982039,68.883741358619,69.8743707351991,
70.8650001117791,71.8556294883591,72.8462588649391,73.8368882415192,74.8275176180992,
75.8181469946792,76.8087763712593,77.7994057478393,78.7900351244193,79.7806645009993,
80.7712938775794,81.7626130033183),.UNSPECIFIED.);
#277=B_SPLINE_SURFACE_WITH_KNOTS('',3,3,((#57712,#57713,#57714,#57715,#57716,
#57717,#57718,#57719,#57720,#57721,#57722,#57723,#57724,#57725,#57726,#57727,
#57728,#57729,#57730,#57731,#57732,#57733,#57734,#57735,#57736,#57737,#57738,
#57739,#57740,#57741,#57742,#57743,#57744,#57745,#57746,#57747,#57748,#57749,
#57750,#57751,#57752,#57753,#57754,#57755,#57756,#57757,#57758,#57759,#57760,
#57761,#57762,#57763,#57764,#57765,#57766,#57767,#57768,#57769,#57770,#57771,
#57772,#57773,#57774,#57775,#57776,#57777,#57778,#57779,#57780,#57781,#57782),
(#57783,#57784,#57785,#57786,#57787,#57788,#57789,#57790,#57791,#57792,
#57793,#57794,#57795,#57796,#57797,#57798,#57799,#57800,#57801,#57802,#57803,
#57804,#57805,#57806,#57807,#57808,#57809,#57810,#57811,#57812,#57813,#57814,
#57815,#57816,#57817,#57818,#57819,#57820,#57821,#57822,#57823,#57824,#57825,
#57826,#57827,#57828,#57829,#57830,#57831,#57832,#57833,#57834,#57835,#57836,
#57837,#57838,#57839,#57840,#57841,#57842,#57843,#57844,#57845,#57846,#57847,
#57848,#57849,#57850,#57851,#57852,#57853),(#57854,#57855,#57856,#57857,
#57858,#57859,#57860,#57861,#57862,#57863,#57864,#57865,#57866,#57867,#57868,
#57869,#57870,#57871,#57872,#57873,#57874,#57875,#57876,#57877,#57878,#57879,
#57880,#57881,#57882,#57883,#57884,#57885,#57886,#57887,#57888,#57889,#57890,
#57891,#57892,#57893,#57894,#57895,#57896,#57897,#57898,#57899,#57900,#57901,
#57902,#57903,#57904,#57905,#57906,#57907,#57908,#57909,#57910,#57911,#57912,
#57913,#57914,#57915,#57916,#57917,#57918,#57919,#57920,#57921,#57922,#57923,
#57924),(#57925,#57926,#57927,#57928,#57929,#57930,#57931,#57932,#57933,
#57934,#57935,#57936,#57937,#57938,#57939,#57940,#57941,#57942,#57943,#57944,
#57945,#57946,#57947,#57948,#57949,#57950,#57951,#57952,#57953,#57954,#57955,
#57956,#57957,#57958,#57959,#57960,#57961,#57962,#57963,#57964,#57965,#57966,
#57967,#57968,#57969,#57970,#57971,#57972,#57973,#57974,#57975,#57976,#57977,
#57978,#57979,#57980,#57981,#57982,#57983,#57984,#57985,#57986,#57987,#57988,
#57989,#57990,#57991,#57992,#57993,#57994,#57995)),.UNSPECIFIED.,.F.,.F.,
 .F.,(4,4),(4,1,1,1,1,1,1,1,1,1,1,1,1,1,1,1,1,1,1,1,1,1,1,1,1,1,1,1,1,1,
1,1,1,1,1,1,1,1,1,1,1,1,1,1,1,1,1,1,1,1,1,1,1,1,1,1,1,1,1,1,1,1,1,1,1,1,
1,1,4),(-0.000703899666689691,0.0807257072263232),(11.8568339231497,12.8481671993964,
13.8387965759764,14.8294259525565,15.8200553291365,16.8106847057165,17.8013140822965,
18.7919434588766,19.7825728354566,20.7732022120366,21.7638315886167,22.7544609651967,
23.7450903417767,24.7357197183567,25.7263490949368,26.7169784715168,27.7076078480968,
28.6982372246768,29.6888666012569,30.6794959778369,31.6701253544169,32.660754730997,
33.651384107577,34.642013484157,35.632642860737,36.6232722373171,37.6139016138971,
38.6045309904771,39.5951603670571,40.5857897436372,41.5764191202172,42.5670484967972,
43.5576778733773,44.5483072499573,45.5389366265373,46.5295660031173,47.5201953796974,
48.5108247562774,49.5014541328574,50.4920835094374,51.4827128860175,52.4733422625975,
53.4639716391775,54.4546010157575,55.4452303923376,56.4358597689176,57.4264891454976,
58.4171185220777,59.4077478986577,60.3983772752377,61.3890066518177,62.3796360283978,
63.3702654049778,64.3608947815578,65.3515241581378,66.3421535347179,67.3327829112979,
68.3234122878779,69.314041664458,70.304671041038,71.295300417618,72.285929794198,
73.2765591707781,74.2671885473581,75.2578179239381,76.2484473005182,77.2390766770982,
78.2297060536782,79.2203354302582),.UNSPECIFIED.);
#278=B_SPLINE_SURFACE_WITH_KNOTS('',3,3,((#58093,#58094,#58095,#58096,#58097,
#58098,#58099,#58100,#58101,#58102,#58103,#58104,#58105,#58106,#58107,#58108,
#58109,#58110,#58111,#58112,#58113,#58114,#58115,#58116,#58117,#58118,#58119,
#58120,#58121,#58122,#58123,#58124,#58125,#58126,#58127,#58128,#58129,#58130,
#58131,#58132,#58133,#58134,#58135,#58136,#58137,#58138,#58139,#58140,#58141,
#58142,#58143,#58144,#58145,#58146,#58147,#58148,#58149,#58150,#58151,#58152,
#58153,#58154,#58155,#58156,#58157,#58158,#58159,#58160,#58161,#58162,#58163),
(#58164,#58165,#58166,#58167,#58168,#58169,#58170,#58171,#58172,#58173,
#58174,#58175,#58176,#58177,#58178,#58179,#58180,#58181,#58182,#58183,#58184,
#58185,#58186,#58187,#58188,#58189,#58190,#58191,#58192,#58193,#58194,#58195,
#58196,#58197,#58198,#58199,#58200,#58201,#58202,#58203,#58204,#58205,#58206,
#58207,#58208,#58209,#58210,#58211,#58212,#58213,#58214,#58215,#58216,#58217,
#58218,#58219,#58220,#58221,#58222,#58223,#58224,#58225,#58226,#58227,#58228,
#58229,#58230,#58231,#58232,#58233,#58234),(#58235,#58236,#58237,#58238,
#58239,#58240,#58241,#58242,#58243,#58244,#58245,#58246,#58247,#58248,#58249,
#58250,#58251,#58252,#58253,#58254,#58255,#58256,#58257,#58258,#58259,#58260,
#58261,#58262,#58263,#58264,#58265,#58266,#58267,#58268,#58269,#58270,#58271,
#58272,#58273,#58274,#58275,#58276,#58277,#58278,#58279,#58280,#58281,#58282,
#58283,#58284,#58285,#58286,#58287,#58288,#58289,#58290,#58291,#58292,#58293,
#58294,#58295,#58296,#58297,#58298,#58299,#58300,#58301,#58302,#58303,#58304,
#58305),(#58306,#58307,#58308,#58309,#58310,#58311,#58312,#58313,#58314,
#58315,#58316,#58317,#58318,#58319,#58320,#58321,#58322,#58323,#58324,#58325,
#58326,#58327,#58328,#58329,#58330,#58331,#58332,#58333,#58334,#58335,#58336,
#58337,#58338,#58339,#58340,#58341,#58342,#58343,#58344,#58345,#58346,#58347,
#58348,#58349,#58350,#58351,#58352,#58353,#58354,#58355,#58356,#58357,#58358,
#58359,#58360,#58361,#58362,#58363,#58364,#58365,#58366,#58367,#58368,#58369,
#58370,#58371,#58372,#58373,#58374,#58375,#58376)),.UNSPECIFIED.,.F.,.F.,
 .F.,(4,4),(4,1,1,1,1,1,1,1,1,1,1,1,1,1,1,1,1,1,1,1,1,1,1,1,1,1,1,1,1,1,
1,1,1,1,1,1,1,1,1,1,1,1,1,1,1,1,1,1,1,1,1,1,1,1,1,1,1,1,1,1,1,1,1,1,1,1,
1,1,4),(-0.000445070994418236,0.080984343609613),(14.3991256467175,15.3897550232975,
16.3803843998776,17.3710137764576,18.3616431530376,19.3522725296176,20.3429019061977,
21.3335312827777,22.3241606593577,23.3147900359377,24.3054194125178,25.2960487890978,
26.2866781656778,27.2773075422579,28.2679369188379,29.2585662954179,30.2491956719979,
31.239825048578,32.230454425158,33.221083801738,34.211713178318,35.2023425548981,
36.1929719314781,37.1836013080581,38.1742306846382,39.1648600612182,40.1554894377982,
41.1461188143782,42.1367481909583,43.1273775675383,44.1180069441183,45.1086363206983,
46.0992656972784,47.0898950738584,48.0805244504384,49.0711538270185,50.0617832035985,
51.0524125801785,52.0430419567585,53.0336713333386,54.0243007099186,55.0149300864986,
56.0055594630786,56.9961888396587,57.9868182162387,58.9774475928187,59.9680769693988,
60.9587063459788,61.9493357225588,62.9399650991388,63.9305944757189,64.9212238522989,
65.9118532288789,66.9024826054589,67.893111982039,68.883741358619,69.874370735199,
70.8650001117791,71.8556294883591,72.8462588649391,73.8368882415191,74.8275176180992,
75.8181469946792,76.8087763712592,77.7994057478392,78.7900351244193,79.7806645009993,
80.7712938775793,81.7626270428382),.UNSPECIFIED.);
#279=B_SPLINE_SURFACE_WITH_KNOTS('',3,3,((#58677,#58678,#58679,#58680,#58681,
#58682,#58683,#58684,#58685,#58686,#58687,#58688,#58689,#58690,#58691,#58692,
#58693,#58694,#58695,#58696,#58697,#58698,#58699,#58700,#58701,#58702,#58703,
#58704,#58705,#58706,#58707,#58708,#58709,#58710,#58711,#58712,#58713,#58714,
#58715,#58716,#58717,#58718,#58719,#58720,#58721,#58722,#58723,#58724,#58725,
#58726,#58727,#58728,#58729,#58730,#58731,#58732,#58733,#58734,#58735,#58736,
#58737,#58738,#58739,#58740,#58741,#58742,#58743,#58744,#58745,#58746,#58747),
(#58748,#58749,#58750,#58751,#58752,#58753,#58754,#58755,#58756,#58757,
#58758,#58759,#58760,#58761,#58762,#58763,#58764,#58765,#58766,#58767,#58768,
#58769,#58770,#58771,#58772,#58773,#58774,#58775,#58776,#58777,#58778,#58779,
#58780,#58781,#58782,#58783,#58784,#58785,#58786,#58787,#58788,#58789,#58790,
#58791,#58792,#58793,#58794,#58795,#58796,#58797,#58798,#58799,#58800,#58801,
#58802,#58803,#58804,#58805,#58806,#58807,#58808,#58809,#58810,#58811,#58812,
#58813,#58814,#58815,#58816,#58817,#58818),(#58819,#58820,#58821,#58822,
#58823,#58824,#58825,#58826,#58827,#58828,#58829,#58830,#58831,#58832,#58833,
#58834,#58835,#58836,#58837,#58838,#58839,#58840,#58841,#58842,#58843,#58844,
#58845,#58846,#58847,#58848,#58849,#58850,#58851,#58852,#58853,#58854,#58855,
#58856,#58857,#58858,#58859,#58860,#58861,#58862,#58863,#58864,#58865,#58866,
#58867,#58868,#58869,#58870,#58871,#58872,#58873,#58874,#58875,#58876,#58877,
#58878,#58879,#58880,#58881,#58882,#58883,#58884,#58885,#58886,#58887,#58888,
#58889),(#58890,#58891,#58892,#58893,#58894,#58895,#58896,#58897,#58898,
#58899,#58900,#58901,#58902,#58903,#58904,#58905,#58906,#58907,#58908,#58909,
#58910,#58911,#58912,#58913,#58914,#58915,#58916,#58917,#58918,#58919,#58920,
#58921,#58922,#58923,#58924,#58925,#58926,#58927,#58928,#58929,#58930,#58931,
#58932,#58933,#58934,#58935,#58936,#58937,#58938,#58939,#58940,#58941,#58942,
#58943,#58944,#58945,#58946,#58947,#58948,#58949,#58950,#58951,#58952,#58953,
#58954,#58955,#58956,#58957,#58958,#58959,#58960)),.UNSPECIFIED.,.F.,.F.,
 .F.,(4,4),(4,1,1,1,1,1,1,1,1,1,1,1,1,1,1,1,1,1,1,1,1,1,1,1,1,1,1,1,1,1,
1,1,1,1,1,1,1,1,1,1,1,1,1,1,1,1,1,1,1,1,1,1,1,1,1,1,1,1,1,1,1,1,1,1,1,1,
1,1,4),(-0.00068967791227708,0.0807181852368366),(11.8568481449041,12.8481671993964,
13.8387965759765,14.8294259525565,15.8200553291365,16.8106847057165,17.8013140822966,
18.7919434588766,19.7825728354566,20.7732022120367,21.7638315886167,22.7544609651967,
23.7450903417767,24.7357197183568,25.7263490949368,26.7169784715168,27.7076078480968,
28.6982372246769,29.6888666012569,30.6794959778369,31.6701253544169,32.660754730997,
33.651384107577,34.642013484157,35.6326428607371,36.6232722373171,37.6139016138971,
38.6045309904771,39.5951603670572,40.5857897436372,41.5764191202172,42.5670484967972,
43.5576778733773,44.5483072499573,45.5389366265373,46.5295660031174,47.5201953796974,
48.5108247562774,49.5014541328574,50.4920835094375,51.4827128860175,52.4733422625975,
53.4639716391775,54.4546010157576,55.4452303923376,56.4358597689176,57.4264891454977,
58.4171185220777,59.4077478986577,60.3983772752377,61.3890066518178,62.3796360283978,
63.3702654049778,64.3608947815578,65.3515241581379,66.3421535347179,67.3327829112979,
68.3234122878779,69.314041664458,70.304671041038,71.295300417618,72.2859297941981,
73.2765591707781,74.2671885473581,75.2578179239381,76.2484473005182,77.2390766770982,
78.2297060536782,79.2203354302583),.UNSPECIFIED.);
#280=B_SPLINE_SURFACE_WITH_KNOTS('',3,3,((#59055,#59056,#59057,#59058,#59059,
#59060,#59061,#59062,#59063,#59064,#59065,#59066,#59067,#59068,#59069,#59070,
#59071,#59072,#59073,#59074,#59075,#59076,#59077,#59078,#59079,#59080,#59081,
#59082,#59083,#59084,#59085,#59086,#59087,#59088,#59089,#59090,#59091,#59092,
#59093,#59094,#59095,#59096,#59097,#59098,#59099,#59100,#59101,#59102,#59103,
#59104,#59105,#59106,#59107,#59108,#59109,#59110,#59111,#59112,#59113,#59114,
#59115,#59116,#59117,#59118,#59119,#59120,#59121,#59122,#59123,#59124,#59125),
(#59126,#59127,#59128,#59129,#59130,#59131,#59132,#59133,#59134,#59135,
#59136,#59137,#59138,#59139,#59140,#59141,#59142,#59143,#59144,#59145,#59146,
#59147,#59148,#59149,#59150,#59151,#59152,#59153,#59154,#59155,#59156,#59157,
#59158,#59159,#59160,#59161,#59162,#59163,#59164,#59165,#59166,#59167,#59168,
#59169,#59170,#59171,#59172,#59173,#59174,#59175,#59176,#59177,#59178,#59179,
#59180,#59181,#59182,#59183,#59184,#59185,#59186,#59187,#59188,#59189,#59190,
#59191,#59192,#59193,#59194,#59195,#59196),(#59197,#59198,#59199,#59200,
#59201,#59202,#59203,#59204,#59205,#59206,#59207,#59208,#59209,#59210,#59211,
#59212,#59213,#59214,#59215,#59216,#59217,#59218,#59219,#59220,#59221,#59222,
#59223,#59224,#59225,#59226,#59227,#59228,#59229,#59230,#59231,#59232,#59233,
#59234,#59235,#59236,#59237,#59238,#59239,#59240,#59241,#59242,#59243,#59244,
#59245,#59246,#59247,#59248,#59249,#59250,#59251,#59252,#59253,#59254,#59255,
#59256,#59257,#59258,#59259,#59260,#59261,#59262,#59263,#59264,#59265,#59266,
#59267),(#59268,#59269,#59270,#59271,#59272,#59273,#59274,#59275,#59276,
#59277,#59278,#59279,#59280,#59281,#59282,#59283,#59284,#59285,#59286,#59287,
#59288,#59289,#59290,#59291,#59292,#59293,#59294,#59295,#59296,#59297,#59298,
#59299,#59300,#59301,#59302,#59303,#59304,#59305,#59306,#59307,#59308,#59309,
#59310,#59311,#59312,#59313,#59314,#59315,#59316,#59317,#59318,#59319,#59320,
#59321,#59322,#59323,#59324,#59325,#59326,#59327,#59328,#59329,#59330,#59331,
#59332,#59333,#59334,#59335,#59336,#59337,#59338)),.UNSPECIFIED.,.F.,.F.,
 .F.,(4,4),(4,1,1,1,1,1,1,1,1,1,1,1,1,1,1,1,1,1,1,1,1,1,1,1,1,1,1,1,1,1,
1,1,1,1,1,1,1,1,1,1,1,1,1,1,1,1,1,1,1,1,1,1,1,1,1,1,1,1,1,1,1,1,1,1,1,1,
1,1,4),(-0.00043763828538554,0.0809702546783821),(14.3991256467175,15.3897550232976,
16.3803843998776,17.3710137764576,18.3616431530376,19.3522725296177,20.3429019061977,
21.3335312827777,22.3241606593577,23.3147900359378,24.3054194125178,25.2960487890978,
26.2866781656779,27.2773075422579,28.2679369188379,29.2585662954179,30.249195671998,
31.239825048578,32.230454425158,33.221083801738,34.2117131783181,35.2023425548981,
36.1929719314781,37.1836013080582,38.1742306846382,39.1648600612182,40.1554894377982,
41.1461188143783,42.1367481909583,43.1273775675383,44.1180069441183,45.1086363206984,
46.0992656972784,47.0898950738584,48.0805244504385,49.0711538270185,50.0617832035985,
51.0524125801785,52.0430419567586,53.0336713333386,54.0243007099186,55.0149300864986,
56.0055594630787,56.9961888396587,57.9868182162387,58.9774475928188,59.9680769693988,
60.9587063459788,61.9493357225588,62.9399650991389,63.9305944757189,64.9212238522989,
65.911853228879,66.902482605459,67.893111982039,68.883741358619,69.8743707351991,
70.8650001117791,71.8556294883591,72.8462588649391,73.8368882415192,74.8275176180992,
75.8181469946792,76.8087763712593,77.7994057478393,78.7900351244193,79.7806645009993,
80.7712938775794,81.7626129539069),.UNSPECIFIED.);
#281=B_SPLINE_SURFACE_WITH_KNOTS('',3,3,((#129776,#129777,#129778,#129779,
#129780,#129781,#129782,#129783,#129784,#129785,#129786,#129787,#129788,
#129789,#129790,#129791,#129792,#129793,#129794,#129795,#129796,#129797,
#129798,#129799,#129800,#129801,#129802,#129803,#129804,#129805,#129806,
#129807,#129808,#129809,#129810,#129811,#129812,#129813,#129814,#129815,
#129816,#129817,#129818,#129819,#129820,#129821,#129822,#129823,#129824,
#129825,#129826,#129827,#129828,#129829,#129830,#129831,#129832,#129833,
#129834,#129835,#129836,#129837,#129838,#129839,#129840,#129841,#129842,
#129843,#129844,#129845,#129846,#129847,#129848,#129849,#129850,#129851,
#129852,#129853,#129854,#129855,#129856,#129857,#129858,#129859,#129860,
#129861,#129862,#129863,#129864,#129865,#129866,#129867,#129868,#129869,
#129870,#129871,#129872,#129873,#129874,#129875,#129876,#129877,#129878,
#129879),(#129880,#129881,#129882,#129883,#129884,#129885,#129886,#129887,
#129888,#129889,#129890,#129891,#129892,#129893,#129894,#129895,#129896,
#129897,#129898,#129899,#129900,#129901,#129902,#129903,#129904,#129905,
#129906,#129907,#129908,#129909,#129910,#129911,#129912,#129913,#129914,
#129915,#129916,#129917,#129918,#129919,#129920,#129921,#129922,#129923,
#129924,#129925,#129926,#129927,#129928,#129929,#129930,#129931,#129932,
#129933,#129934,#129935,#129936,#129937,#129938,#129939,#129940,#129941,
#129942,#129943,#129944,#129945,#129946,#129947,#129948,#129949,#129950,
#129951,#129952,#129953,#129954,#129955,#129956,#129957,#129958,#129959,
#129960,#129961,#129962,#129963,#129964,#129965,#129966,#129967,#129968,
#129969,#129970,#129971,#129972,#129973,#129974,#129975,#129976,#129977,
#129978,#129979,#129980,#129981,#129982,#129983),(#129984,#129985,#129986,
#129987,#129988,#129989,#129990,#129991,#129992,#129993,#129994,#129995,
#129996,#129997,#129998,#129999,#130000,#130001,#130002,#130003,#130004,
#130005,#130006,#130007,#130008,#130009,#130010,#130011,#130012,#130013,
#130014,#130015,#130016,#130017,#130018,#130019,#130020,#130021,#130022,
#130023,#130024,#130025,#130026,#130027,#130028,#130029,#130030,#130031,
#130032,#130033,#130034,#130035,#130036,#130037,#130038,#130039,#130040,
#130041,#130042,#130043,#130044,#130045,#130046,#130047,#130048,#130049,
#130050,#130051,#130052,#130053,#130054,#130055,#130056,#130057,#130058,
#130059,#130060,#130061,#130062,#130063,#130064,#130065,#130066,#130067,
#130068,#130069,#130070,#130071,#130072,#130073,#130074,#130075,#130076,
#130077,#130078,#130079,#130080,#130081,#130082,#130083,#130084,#130085,
#130086,#130087),(#130088,#130089,#130090,#130091,#130092,#130093,#130094,
#130095,#130096,#130097,#130098,#130099,#130100,#130101,#130102,#130103,
#130104,#130105,#130106,#130107,#130108,#130109,#130110,#130111,#130112,
#130113,#130114,#130115,#130116,#130117,#130118,#130119,#130120,#130121,
#130122,#130123,#130124,#130125,#130126,#130127,#130128,#130129,#130130,
#130131,#130132,#130133,#130134,#130135,#130136,#130137,#130138,#130139,
#130140,#130141,#130142,#130143,#130144,#130145,#130146,#130147,#130148,
#130149,#130150,#130151,#130152,#130153,#130154,#130155,#130156,#130157,
#130158,#130159,#130160,#130161,#130162,#130163,#130164,#130165,#130166,
#130167,#130168,#130169,#130170,#130171,#130172,#130173,#130174,#130175,
#130176,#130177,#130178,#130179,#130180,#130181,#130182,#130183,#130184,
#130185,#130186,#130187,#130188,#130189,#130190,#130191)),.UNSPECIFIED.,
 .F.,.F.,.F.,(4,4),(4,1,1,1,1,1,1,1,1,1,1,1,1,1,1,1,1,1,1,1,1,1,1,1,1,1,
1,1,1,1,1,1,1,1,1,1,1,1,1,1,1,1,1,1,1,1,1,1,1,1,1,1,1,1,1,1,1,1,1,1,1,1,
1,1,1,1,1,1,1,1,1,1,1,1,1,1,1,1,1,1,1,1,1,1,1,1,1,1,1,1,1,1,1,1,1,1,1,1,
1,1,1,4),(-0.000353809570517248,0.0451882118607677),(11.8612261946863,12.8591085386934,
13.85663707313,14.8541656075666,15.8516941420032,16.8492226764398,17.8467512108764,
18.844279745313,19.8418082797496,20.8393368141862,21.8368653486228,22.8343938830594,
23.831922417496,24.8294509519326,25.8269794863692,26.8245080208058,27.8220365552424,
28.819565089679,29.8170936241156,30.8146221585522,31.8121506929888,32.8096792274254,
33.807207761862,34.8047362962986,35.8022648307352,36.7997933651718,37.7973218996084,
38.794850434045,39.7923789684816,40.7899075029182,41.7874360373548,42.7849645717913,
43.782493106228,44.7800216406646,45.7775501751012,46.7750787095378,47.7726072439743,
48.7701357784109,49.7676643128475,50.7651928472842,51.7627213817208,52.7602499161573,
53.7577784505939,54.7553069850305,55.7528355194671,56.7503640539037,57.7478925883403,
58.7454211227769,59.7429496572135,60.7404781916501,61.7380067260867,62.7355352605233,
63.7330637949599,64.7305923293965,65.7281208638331,66.7256493982697,67.7231779327063,
68.7207064671429,69.7182350015795,70.7157635360161,71.7132920704527,72.7108206048893,
73.7083491393259,74.7058776737625,75.7034062081991,76.7009347426357,77.6984632770723,
78.6959918115089,79.6935203459455,80.6910488803821,81.6885774148187,82.6861059492553,
83.6836344836919,84.6811630181285,85.6786915525651,86.6762200870017,87.6737486214383,
88.6712771558749,89.6688056903115,90.6663342247481,91.6638627591847,92.6613912936213,
93.6589198280579,94.6564483624945,95.6539768969311,96.6515054313677,97.6490339658043,
98.6465625002409,99.6440910346775,100.641619569114,101.639148103551,102.636676637987,
103.634205172424,104.631733706861,105.629262241297,106.626790775734,107.62431931017,
108.621847844607,109.619376379044,110.61690491348,111.614433447917,112.611961982353),
 .UNSPECIFIED.);
#282=B_SPLINE_SURFACE_WITH_KNOTS('',3,3,((#130274,#130275,#130276,#130277,
#130278,#130279,#130280,#130281,#130282,#130283,#130284,#130285,#130286,
#130287,#130288,#130289,#130290,#130291,#130292,#130293,#130294,#130295,
#130296,#130297,#130298,#130299,#130300,#130301,#130302,#130303,#130304,
#130305,#130306,#130307,#130308,#130309,#130310,#130311,#130312,#130313,
#130314,#130315,#130316,#130317,#130318,#130319,#130320,#130321,#130322,
#130323,#130324,#130325,#130326,#130327,#130328,#130329,#130330,#130331,
#130332,#130333,#130334,#130335,#130336,#130337,#130338,#130339,#130340,
#130341,#130342,#130343,#130344,#130345,#130346,#130347,#130348,#130349,
#130350,#130351,#130352,#130353,#130354,#130355,#130356,#130357,#130358,
#130359,#130360,#130361,#130362,#130363,#130364,#130365,#130366,#130367,
#130368,#130369,#130370,#130371,#130372,#130373,#130374,#130375,#130376,
#130377),(#130378,#130379,#130380,#130381,#130382,#130383,#130384,#130385,
#130386,#130387,#130388,#130389,#130390,#130391,#130392,#130393,#130394,
#130395,#130396,#130397,#130398,#130399,#130400,#130401,#130402,#130403,
#130404,#130405,#130406,#130407,#130408,#130409,#130410,#130411,#130412,
#130413,#130414,#130415,#130416,#130417,#130418,#130419,#130420,#130421,
#130422,#130423,#130424,#130425,#130426,#130427,#130428,#130429,#130430,
#130431,#130432,#130433,#130434,#130435,#130436,#130437,#130438,#130439,
#130440,#130441,#130442,#130443,#130444,#130445,#130446,#130447,#130448,
#130449,#130450,#130451,#130452,#130453,#130454,#130455,#130456,#130457,
#130458,#130459,#130460,#130461,#130462,#130463,#130464,#130465,#130466,
#130467,#130468,#130469,#130470,#130471,#130472,#130473,#130474,#130475,
#130476,#130477,#130478,#130479,#130480,#130481),(#130482,#130483,#130484,
#130485,#130486,#130487,#130488,#130489,#130490,#130491,#130492,#130493,
#130494,#130495,#130496,#130497,#130498,#130499,#130500,#130501,#130502,
#130503,#130504,#130505,#130506,#130507,#130508,#130509,#130510,#130511,
#130512,#130513,#130514,#130515,#130516,#130517,#130518,#130519,#130520,
#130521,#130522,#130523,#130524,#130525,#130526,#130527,#130528,#130529,
#130530,#130531,#130532,#130533,#130534,#130535,#130536,#130537,#130538,
#130539,#130540,#130541,#130542,#130543,#130544,#130545,#130546,#130547,
#130548,#130549,#130550,#130551,#130552,#130553,#130554,#130555,#130556,
#130557,#130558,#130559,#130560,#130561,#130562,#130563,#130564,#130565,
#130566,#130567,#130568,#130569,#130570,#130571,#130572,#130573,#130574,
#130575,#130576,#130577,#130578,#130579,#130580,#130581,#130582,#130583,
#130584,#130585),(#130586,#130587,#130588,#130589,#130590,#130591,#130592,
#130593,#130594,#130595,#130596,#130597,#130598,#130599,#130600,#130601,
#130602,#130603,#130604,#130605,#130606,#130607,#130608,#130609,#130610,
#130611,#130612,#130613,#130614,#130615,#130616,#130617,#130618,#130619,
#130620,#130621,#130622,#130623,#130624,#130625,#130626,#130627,#130628,
#130629,#130630,#130631,#130632,#130633,#130634,#130635,#130636,#130637,
#130638,#130639,#130640,#130641,#130642,#130643,#130644,#130645,#130646,
#130647,#130648,#130649,#130650,#130651,#130652,#130653,#130654,#130655,
#130656,#130657,#130658,#130659,#130660,#130661,#130662,#130663,#130664,
#130665,#130666,#130667,#130668,#130669,#130670,#130671,#130672,#130673,
#130674,#130675,#130676,#130677,#130678,#130679,#130680,#130681,#130682,
#130683,#130684,#130685,#130686,#130687,#130688,#130689)),.UNSPECIFIED.,
 .F.,.F.,.F.,(4,4),(4,1,1,1,1,1,1,1,1,1,1,1,1,1,1,1,1,1,1,1,1,1,1,1,1,1,
1,1,1,1,1,1,1,1,1,1,1,1,1,1,1,1,1,1,1,1,1,1,1,1,1,1,1,1,1,1,1,1,1,1,1,1,
1,1,1,1,1,1,1,1,1,1,1,1,1,1,1,1,1,1,1,1,1,1,1,1,1,1,1,1,1,1,1,1,1,1,1,1,
1,1,1,4),(-0.000311884246383574,0.0452427689821445),(14.398141012777,15.3956695472136,
16.3931980816502,17.3907266160868,18.3882551505234,19.38578368496,20.3833122193966,
21.3808407538332,22.3783692882698,23.3758978227064,24.373426357143,25.3709548915796,
26.3684834260162,27.3660119604528,28.3635404948894,29.361069029326,30.3585975637626,
31.3561260981992,32.3536546326358,33.3511831670724,34.348711701509,35.3462402359456,
36.3437687703822,37.3412973048188,38.3388258392554,39.336354373692,40.3338829081286,
41.3314114425652,42.3289399770018,43.3264685114384,44.323997045875,45.3215255803116,
46.3190541147482,47.3165826491848,48.3141111836214,49.311639718058,50.3091682524946,
51.3066967869312,52.3042253213678,53.3017538558044,54.299282390241,55.2968109246776,
56.2943394591142,57.2918679935508,58.2893965279874,59.286925062424,60.2844535968606,
61.2819821312972,62.2795106657338,63.2770392001704,64.274567734607,65.2720962690436,
66.2696248034802,67.2671533379168,68.2646818723534,69.26221040679,70.2597389412266,
71.2572674756632,72.2547960100998,73.2523245445364,74.249853078973,75.2473816134096,
76.2449101478462,77.2424386822828,78.2399672167194,79.237495751156,80.2350242855926,
81.2325528200292,82.2300813544658,83.2276098889024,84.225138423339,85.2226669577756,
86.2201954922122,87.2177240266488,88.2152525610854,89.212781095522,90.2103096299586,
91.2078381643952,92.2053666988318,93.2028952332684,94.2004237677049,95.1979523021416,
96.1954808365782,97.1930093710148,98.1905379054514,99.1880664398879,100.185594974325,
101.183123508761,102.180652043198,103.178180577634,104.175709112071,105.173237646508,
106.170766180944,107.168294715381,108.165823249817,109.163351784254,110.160880318691,
111.158408853127,112.155937387564,113.153465922,114.150994456437,115.148876776427),
 .UNSPECIFIED.);
#283=B_SPLINE_SURFACE_WITH_KNOTS('',3,3,((#130957,#130958,#130959,#130960,
#130961,#130962,#130963,#130964,#130965,#130966,#130967,#130968,#130969,
#130970,#130971,#130972,#130973,#130974,#130975,#130976,#130977,#130978,
#130979,#130980,#130981,#130982,#130983,#130984,#130985,#130986,#130987,
#130988,#130989,#130990,#130991,#130992,#130993,#130994,#130995,#130996,
#130997,#130998,#130999,#131000,#131001,#131002,#131003,#131004,#131005,
#131006,#131007,#131008,#131009,#131010,#131011,#131012,#131013,#131014,
#131015,#131016,#131017,#131018,#131019,#131020,#131021,#131022,#131023,
#131024,#131025,#131026,#131027,#131028,#131029,#131030,#131031,#131032,
#131033,#131034,#131035,#131036,#131037,#131038,#131039,#131040,#131041,
#131042,#131043,#131044,#131045,#131046,#131047,#131048,#131049,#131050,
#131051,#131052,#131053,#131054,#131055,#131056,#131057,#131058,#131059,
#131060),(#131061,#131062,#131063,#131064,#131065,#131066,#131067,#131068,
#131069,#131070,#131071,#131072,#131073,#131074,#131075,#131076,#131077,
#131078,#131079,#131080,#131081,#131082,#131083,#131084,#131085,#131086,
#131087,#131088,#131089,#131090,#131091,#131092,#131093,#131094,#131095,
#131096,#131097,#131098,#131099,#131100,#131101,#131102,#131103,#131104,
#131105,#131106,#131107,#131108,#131109,#131110,#131111,#131112,#131113,
#131114,#131115,#131116,#131117,#131118,#131119,#131120,#131121,#131122,
#131123,#131124,#131125,#131126,#131127,#131128,#131129,#131130,#131131,
#131132,#131133,#131134,#131135,#131136,#131137,#131138,#131139,#131140,
#131141,#131142,#131143,#131144,#131145,#131146,#131147,#131148,#131149,
#131150,#131151,#131152,#131153,#131154,#131155,#131156,#131157,#131158,
#131159,#131160,#131161,#131162,#131163,#131164),(#131165,#131166,#131167,
#131168,#131169,#131170,#131171,#131172,#131173,#131174,#131175,#131176,
#131177,#131178,#131179,#131180,#131181,#131182,#131183,#131184,#131185,
#131186,#131187,#131188,#131189,#131190,#131191,#131192,#131193,#131194,
#131195,#131196,#131197,#131198,#131199,#131200,#131201,#131202,#131203,
#131204,#131205,#131206,#131207,#131208,#131209,#131210,#131211,#131212,
#131213,#131214,#131215,#131216,#131217,#131218,#131219,#131220,#131221,
#131222,#131223,#131224,#131225,#131226,#131227,#131228,#131229,#131230,
#131231,#131232,#131233,#131234,#131235,#131236,#131237,#131238,#131239,
#131240,#131241,#131242,#131243,#131244,#131245,#131246,#131247,#131248,
#131249,#131250,#131251,#131252,#131253,#131254,#131255,#131256,#131257,
#131258,#131259,#131260,#131261,#131262,#131263,#131264,#131265,#131266,
#131267,#131268),(#131269,#131270,#131271,#131272,#131273,#131274,#131275,
#131276,#131277,#131278,#131279,#131280,#131281,#131282,#131283,#131284,
#131285,#131286,#131287,#131288,#131289,#131290,#131291,#131292,#131293,
#131294,#131295,#131296,#131297,#131298,#131299,#131300,#131301,#131302,
#131303,#131304,#131305,#131306,#131307,#131308,#131309,#131310,#131311,
#131312,#131313,#131314,#131315,#131316,#131317,#131318,#131319,#131320,
#131321,#131322,#131323,#131324,#131325,#131326,#131327,#131328,#131329,
#131330,#131331,#131332,#131333,#131334,#131335,#131336,#131337,#131338,
#131339,#131340,#131341,#131342,#131343,#131344,#131345,#131346,#131347,
#131348,#131349,#131350,#131351,#131352,#131353,#131354,#131355,#131356,
#131357,#131358,#131359,#131360,#131361,#131362,#131363,#131364,#131365,
#131366,#131367,#131368,#131369,#131370,#131371,#131372)),.UNSPECIFIED.,
 .F.,.F.,.F.,(4,4),(4,1,1,1,1,1,1,1,1,1,1,1,1,1,1,1,1,1,1,1,1,1,1,1,1,1,
1,1,1,1,1,1,1,1,1,1,1,1,1,1,1,1,1,1,1,1,1,1,1,1,1,1,1,1,1,1,1,1,1,1,1,1,
1,1,1,1,1,1,1,1,1,1,1,1,1,1,1,1,1,1,1,1,1,1,1,1,1,1,1,1,1,1,1,1,1,1,1,1,
1,1,1,4),(-0.000353803744797756,0.045188208347436),(11.8612262005118,12.8591085386932,
13.8566370731298,14.8541656075664,15.851694142003,16.8492226764396,17.8467512108762,
18.8442797453128,19.8418082797494,20.839336814186,21.8368653486226,22.8343938830592,
23.8319224174958,24.8294509519324,25.826979486369,26.8245080208056,27.8220365552422,
28.8195650896788,29.8170936241154,30.814622158552,31.8121506929886,32.8096792274252,
33.8072077618618,34.8047362962984,35.802264830735,36.7997933651716,37.7973218996082,
38.7948504340448,39.7923789684814,40.789907502918,41.7874360373546,42.7849645717912,
43.7824931062278,44.7800216406644,45.777550175101,46.7750787095376,47.7726072439742,
48.7701357784108,49.7676643128474,50.765192847284,51.7627213817206,52.7602499161572,
53.7577784505938,54.7553069850304,55.752835519467,56.7503640539036,57.7478925883402,
58.7454211227768,59.7429496572134,60.74047819165,61.7380067260866,62.7355352605232,
63.7330637949598,64.7305923293964,65.728120863833,66.7256493982696,67.7231779327062,
68.7207064671428,69.7182350015794,70.715763536016,71.7132920704526,72.7108206048892,
73.7083491393258,74.7058776737624,75.703406208199,76.7009347426356,77.6984632770722,
78.6959918115088,79.6935203459454,80.691048880382,81.6885774148186,82.6861059492552,
83.6836344836918,84.6811630181284,85.678691552565,86.6762200870016,87.6737486214382,
88.6712771558748,89.6688056903114,90.666334224748,91.6638627591846,92.6613912936212,
93.6589198280578,94.6564483624944,95.653976896931,96.6515054313676,97.6490339658042,
98.6465625002408,99.6440910346774,100.641619569114,101.639148103551,102.636676637987,
103.634205172424,104.63173370686,105.629262241297,106.626790775734,107.62431931017,
108.621847844607,109.619376379043,110.61690491348,111.614433447917,112.611961982353),
 .UNSPECIFIED.);
#284=B_SPLINE_SURFACE_WITH_KNOTS('',3,3,((#131455,#131456,#131457,#131458,
#131459,#131460,#131461,#131462,#131463,#131464,#131465,#131466,#131467,
#131468,#131469,#131470,#131471,#131472,#131473,#131474,#131475,#131476,
#131477,#131478,#131479,#131480,#131481,#131482,#131483,#131484,#131485,
#131486,#131487,#131488,#131489,#131490,#131491,#131492,#131493,#131494,
#131495,#131496,#131497,#131498,#131499,#131500,#131501,#131502,#131503,
#131504,#131505,#131506,#131507,#131508,#131509,#131510,#131511,#131512,
#131513,#131514,#131515,#131516,#131517,#131518,#131519,#131520,#131521,
#131522,#131523,#131524,#131525,#131526,#131527,#131528,#131529,#131530,
#131531,#131532,#131533,#131534,#131535,#131536,#131537,#131538,#131539,
#131540,#131541,#131542,#131543,#131544,#131545,#131546,#131547,#131548,
#131549,#131550,#131551,#131552,#131553,#131554,#131555,#131556,#131557,
#131558),(#131559,#131560,#131561,#131562,#131563,#131564,#131565,#131566,
#131567,#131568,#131569,#131570,#131571,#131572,#131573,#131574,#131575,
#131576,#131577,#131578,#131579,#131580,#131581,#131582,#131583,#131584,
#131585,#131586,#131587,#131588,#131589,#131590,#131591,#131592,#131593,
#131594,#131595,#131596,#131597,#131598,#131599,#131600,#131601,#131602,
#131603,#131604,#131605,#131606,#131607,#131608,#131609,#131610,#131611,
#131612,#131613,#131614,#131615,#131616,#131617,#131618,#131619,#131620,
#131621,#131622,#131623,#131624,#131625,#131626,#131627,#131628,#131629,
#131630,#131631,#131632,#131633,#131634,#131635,#131636,#131637,#131638,
#131639,#131640,#131641,#131642,#131643,#131644,#131645,#131646,#131647,
#131648,#131649,#131650,#131651,#131652,#131653,#131654,#131655,#131656,
#131657,#131658,#131659,#131660,#131661,#131662),(#131663,#131664,#131665,
#131666,#131667,#131668,#131669,#131670,#131671,#131672,#131673,#131674,
#131675,#131676,#131677,#131678,#131679,#131680,#131681,#131682,#131683,
#131684,#131685,#131686,#131687,#131688,#131689,#131690,#131691,#131692,
#131693,#131694,#131695,#131696,#131697,#131698,#131699,#131700,#131701,
#131702,#131703,#131704,#131705,#131706,#131707,#131708,#131709,#131710,
#131711,#131712,#131713,#131714,#131715,#131716,#131717,#131718,#131719,
#131720,#131721,#131722,#131723,#131724,#131725,#131726,#131727,#131728,
#131729,#131730,#131731,#131732,#131733,#131734,#131735,#131736,#131737,
#131738,#131739,#131740,#131741,#131742,#131743,#131744,#131745,#131746,
#131747,#131748,#131749,#131750,#131751,#131752,#131753,#131754,#131755,
#131756,#131757,#131758,#131759,#131760,#131761,#131762,#131763,#131764,
#131765,#131766),(#131767,#131768,#131769,#131770,#131771,#131772,#131773,
#131774,#131775,#131776,#131777,#131778,#131779,#131780,#131781,#131782,
#131783,#131784,#131785,#131786,#131787,#131788,#131789,#131790,#131791,
#131792,#131793,#131794,#131795,#131796,#131797,#131798,#131799,#131800,
#131801,#131802,#131803,#131804,#131805,#131806,#131807,#131808,#131809,
#131810,#131811,#131812,#131813,#131814,#131815,#131816,#131817,#131818,
#131819,#131820,#131821,#131822,#131823,#131824,#131825,#131826,#131827,
#131828,#131829,#131830,#131831,#131832,#131833,#131834,#131835,#131836,
#131837,#131838,#131839,#131840,#131841,#131842,#131843,#131844,#131845,
#131846,#131847,#131848,#131849,#131850,#131851,#131852,#131853,#131854,
#131855,#131856,#131857,#131858,#131859,#131860,#131861,#131862,#131863,
#131864,#131865,#131866,#131867,#131868,#131869,#131870)),.UNSPECIFIED.,
 .F.,.F.,.F.,(4,4),(4,1,1,1,1,1,1,1,1,1,1,1,1,1,1,1,1,1,1,1,1,1,1,1,1,1,
1,1,1,1,1,1,1,1,1,1,1,1,1,1,1,1,1,1,1,1,1,1,1,1,1,1,1,1,1,1,1,1,1,1,1,1,
1,1,1,1,1,1,1,1,1,1,1,1,1,1,1,1,1,1,1,1,1,1,1,1,1,1,1,1,1,1,1,1,1,1,1,1,
1,1,1,4),(-0.000311879380046352,0.0452427611100038),(14.3981410127768,15.3956695472134,
16.39319808165,17.3907266160866,18.3882551505232,19.3857836849598,20.3833122193964,
21.380840753833,22.3783692882696,23.3758978227062,24.3734263571428,25.3709548915794,
26.368483426016,27.3660119604526,28.3635404948892,29.3610690293258,30.3585975637624,
31.356126098199,32.3536546326356,33.3511831670722,34.3487117015088,35.3462402359454,
36.343768770382,37.3412973048186,38.3388258392552,39.3363543736918,40.3338829081284,
41.331411442565,42.3289399770016,43.3264685114382,44.3239970458748,45.3215255803114,
46.319054114748,47.3165826491846,48.3141111836212,49.3116397180578,50.3091682524944,
51.306696786931,52.3042253213676,53.3017538558042,54.2992823902408,55.2968109246774,
56.294339459114,57.2918679935506,58.2893965279872,59.2869250624238,60.2844535968604,
61.281982131297,62.2795106657336,63.2770392001702,64.2745677346068,65.2720962690434,
66.26962480348,67.2671533379166,68.2646818723532,69.2622104067898,70.2597389412264,
71.257267475663,72.2547960100996,73.2523245445362,74.2498530789728,75.2473816134094,
76.244910147846,77.2424386822826,78.2399672167192,79.2374957511558,80.2350242855924,
81.232552820029,82.2300813544656,83.2276098889022,84.2251384233388,85.2226669577754,
86.220195492212,87.2177240266486,88.2152525610852,89.2127810955218,90.2103096299584,
91.207838164395,92.2053666988316,93.2028952332682,94.2004237677048,95.1979523021414,
96.195480836578,97.1930093710146,98.1905379054512,99.1880664398878,100.185594974324,
101.183123508761,102.180652043198,103.178180577634,104.175709112071,105.173237646507,
106.170766180944,107.168294715381,108.165823249817,109.163351784254,110.16088031869,
111.158408853127,112.155937387564,113.153465922,114.150994456437,115.148876768553),
 .UNSPECIFIED.);
#285=B_SPLINE_SURFACE_WITH_KNOTS('',3,3,((#132011,#132012,#132013,#132014,
#132015,#132016,#132017,#132018,#132019,#132020,#132021,#132022,#132023,
#132024,#132025,#132026,#132027,#132028,#132029,#132030,#132031,#132032,
#132033,#132034,#132035,#132036,#132037,#132038,#132039,#132040,#132041,
#132042,#132043,#132044,#132045,#132046,#132047,#132048,#132049,#132050,
#132051,#132052,#132053,#132054,#132055,#132056,#132057,#132058,#132059,
#132060,#132061,#132062,#132063,#132064,#132065,#132066,#132067,#132068,
#132069,#132070,#132071,#132072,#132073,#132074,#132075,#132076,#132077,
#132078,#132079,#132080,#132081,#132082,#132083,#132084,#132085,#132086,
#132087,#132088,#132089,#132090,#132091,#132092,#132093,#132094,#132095,
#132096,#132097,#132098,#132099,#132100,#132101,#132102,#132103,#132104,
#132105),(#132106,#132107,#132108,#132109,#132110,#132111,#132112,#132113,
#132114,#132115,#132116,#132117,#132118,#132119,#132120,#132121,#132122,
#132123,#132124,#132125,#132126,#132127,#132128,#132129,#132130,#132131,
#132132,#132133,#132134,#132135,#132136,#132137,#132138,#132139,#132140,
#132141,#132142,#132143,#132144,#132145,#132146,#132147,#132148,#132149,
#132150,#132151,#132152,#132153,#132154,#132155,#132156,#132157,#132158,
#132159,#132160,#132161,#132162,#132163,#132164,#132165,#132166,#132167,
#132168,#132169,#132170,#132171,#132172,#132173,#132174,#132175,#132176,
#132177,#132178,#132179,#132180,#132181,#132182,#132183,#132184,#132185,
#132186,#132187,#132188,#132189,#132190,#132191,#132192,#132193,#132194,
#132195,#132196,#132197,#132198,#132199,#132200),(#132201,#132202,#132203,
#132204,#132205,#132206,#132207,#132208,#132209,#132210,#132211,#132212,
#132213,#132214,#132215,#132216,#132217,#132218,#132219,#132220,#132221,
#132222,#132223,#132224,#132225,#132226,#132227,#132228,#132229,#132230,
#132231,#132232,#132233,#132234,#132235,#132236,#132237,#132238,#132239,
#132240,#132241,#132242,#132243,#132244,#132245,#132246,#132247,#132248,
#132249,#132250,#132251,#132252,#132253,#132254,#132255,#132256,#132257,
#132258,#132259,#132260,#132261,#132262,#132263,#132264,#132265,#132266,
#132267,#132268,#132269,#132270,#132271,#132272,#132273,#132274,#132275,
#132276,#132277,#132278,#132279,#132280,#132281,#132282,#132283,#132284,
#132285,#132286,#132287,#132288,#132289,#132290,#132291,#132292,#132293,
#132294,#132295),(#132296,#132297,#132298,#132299,#132300,#132301,#132302,
#132303,#132304,#132305,#132306,#132307,#132308,#132309,#132310,#132311,
#132312,#132313,#132314,#132315,#132316,#132317,#132318,#132319,#132320,
#132321,#132322,#132323,#132324,#132325,#132326,#132327,#132328,#132329,
#132330,#132331,#132332,#132333,#132334,#132335,#132336,#132337,#132338,
#132339,#132340,#132341,#132342,#132343,#132344,#132345,#132346,#132347,
#132348,#132349,#132350,#132351,#132352,#132353,#132354,#132355,#132356,
#132357,#132358,#132359,#132360,#132361,#132362,#132363,#132364,#132365,
#132366,#132367,#132368,#132369,#132370,#132371,#132372,#132373,#132374,
#132375,#132376,#132377,#132378,#132379,#132380,#132381,#132382,#132383,
#132384,#132385,#132386,#132387,#132388,#132389,#132390)),.UNSPECIFIED.,
 .F.,.F.,.F.,(4,4),(4,1,1,1,1,1,1,1,1,1,1,1,1,1,1,1,1,1,1,1,1,1,1,1,1,1,
1,1,1,1,1,1,1,1,1,1,1,1,1,1,1,1,1,1,1,1,1,1,1,1,1,1,1,1,1,1,1,1,1,1,1,1,
1,1,1,1,1,1,1,1,1,1,1,1,1,1,1,1,1,1,1,1,1,1,1,1,1,1,1,1,1,1,4),(-0.000348318790885902,
0.0451835916777494),(11.8612316854658,12.8591278626027,13.8566757209488,
14.8542235792949,15.851771437641,16.8493192959871,17.8468671543332,18.8444150126793,
19.8419628710254,20.8395107293714,21.8370585877175,22.8346064460636,23.8321543044097,
24.8297021627558,25.8272500211019,26.824797879448,27.822345737794,28.8198935961401,
29.8174414544862,30.8149893128323,31.8125371711784,32.8100850295245,33.8076328878706,
34.8051807462166,35.8027286045627,36.8002764629088,37.7978243212549,38.795372179601,
39.7929200379471,40.7904678962932,41.7880157546393,42.7855636129853,43.7831114713314,
44.7806593296775,45.7782071880236,46.7757550463697,47.7733029047158,48.7708507630619,
49.768398621408,50.765946479754,51.7634943381001,52.7610421964462,53.7585900547923,
54.7561379131384,55.7536857714845,56.7512336298306,57.7487814881766,58.7463293465227,
59.7438772048688,60.7414250632149,61.738972921561,62.7365207799071,63.7340686382532,
64.7316164965993,65.7291643549453,66.7267122132914,67.7242600716375,68.7218079299836,
69.7193557883297,70.7169036466758,71.7144515050219,72.711999363368,73.709547221714,
74.7070950800601,75.7046429384062,76.7021907967523,77.6997386550984,78.6972865134445,
79.6948343717905,80.6923822301366,81.6899300884827,82.6874779468288,83.6850258051749,
84.682573663521,85.6801215218671,86.6776693802132,87.6752172385592,88.6727650969053,
89.6703129552514,90.6678608135975,91.6654086719436,92.6629565302897,93.6605043886358,
94.6580522469819,95.6556001053279,96.653147963674,97.6506958220201,98.6482436803662,
99.6457915387123,100.643339397058,101.640887255404,102.638435113751,103.635982972097),
 .UNSPECIFIED.);
#286=B_SPLINE_SURFACE_WITH_KNOTS('',3,3,((#132563,#132564,#132565,#132566,
#132567,#132568,#132569,#132570,#132571,#132572,#132573,#132574,#132575,
#132576,#132577,#132578,#132579,#132580,#132581,#132582,#132583,#132584,
#132585,#132586,#132587,#132588,#132589,#132590,#132591,#132592,#132593,
#132594,#132595,#132596,#132597,#132598,#132599,#132600,#132601,#132602,
#132603,#132604,#132605,#132606,#132607,#132608,#132609,#132610,#132611,
#132612,#132613,#132614,#132615,#132616,#132617,#132618,#132619,#132620,
#132621,#132622,#132623,#132624,#132625,#132626,#132627,#132628,#132629,
#132630,#132631,#132632,#132633,#132634,#132635,#132636,#132637,#132638,
#132639,#132640,#132641,#132642,#132643,#132644,#132645,#132646,#132647,
#132648,#132649,#132650,#132651,#132652,#132653,#132654,#132655,#132656,
#132657),(#132658,#132659,#132660,#132661,#132662,#132663,#132664,#132665,
#132666,#132667,#132668,#132669,#132670,#132671,#132672,#132673,#132674,
#132675,#132676,#132677,#132678,#132679,#132680,#132681,#132682,#132683,
#132684,#132685,#132686,#132687,#132688,#132689,#132690,#132691,#132692,
#132693,#132694,#132695,#132696,#132697,#132698,#132699,#132700,#132701,
#132702,#132703,#132704,#132705,#132706,#132707,#132708,#132709,#132710,
#132711,#132712,#132713,#132714,#132715,#132716,#132717,#132718,#132719,
#132720,#132721,#132722,#132723,#132724,#132725,#132726,#132727,#132728,
#132729,#132730,#132731,#132732,#132733,#132734,#132735,#132736,#132737,
#132738,#132739,#132740,#132741,#132742,#132743,#132744,#132745,#132746,
#132747,#132748,#132749,#132750,#132751,#132752),(#132753,#132754,#132755,
#132756,#132757,#132758,#132759,#132760,#132761,#132762,#132763,#132764,
#132765,#132766,#132767,#132768,#132769,#132770,#132771,#132772,#132773,
#132774,#132775,#132776,#132777,#132778,#132779,#132780,#132781,#132782,
#132783,#132784,#132785,#132786,#132787,#132788,#132789,#132790,#132791,
#132792,#132793,#132794,#132795,#132796,#132797,#132798,#132799,#132800,
#132801,#132802,#132803,#132804,#132805,#132806,#132807,#132808,#132809,
#132810,#132811,#132812,#132813,#132814,#132815,#132816,#132817,#132818,
#132819,#132820,#132821,#132822,#132823,#132824,#132825,#132826,#132827,
#132828,#132829,#132830,#132831,#132832,#132833,#132834,#132835,#132836,
#132837,#132838,#132839,#132840,#132841,#132842,#132843,#132844,#132845,
#132846,#132847),(#132848,#132849,#132850,#132851,#132852,#132853,#132854,
#132855,#132856,#132857,#132858,#132859,#132860,#132861,#132862,#132863,
#132864,#132865,#132866,#132867,#132868,#132869,#132870,#132871,#132872,
#132873,#132874,#132875,#132876,#132877,#132878,#132879,#132880,#132881,
#132882,#132883,#132884,#132885,#132886,#132887,#132888,#132889,#132890,
#132891,#132892,#132893,#132894,#132895,#132896,#132897,#132898,#132899,
#132900,#132901,#132902,#132903,#132904,#132905,#132906,#132907,#132908,
#132909,#132910,#132911,#132912,#132913,#132914,#132915,#132916,#132917,
#132918,#132919,#132920,#132921,#132922,#132923,#132924,#132925,#132926,
#132927,#132928,#132929,#132930,#132931,#132932,#132933,#132934,#132935,
#132936,#132937,#132938,#132939,#132940,#132941,#132942)),.UNSPECIFIED.,
 .F.,.F.,.F.,(4,4),(4,1,1,1,1,1,1,1,1,1,1,1,1,1,1,1,1,1,1,1,1,1,1,1,1,1,
1,1,1,1,1,1,1,1,1,1,1,1,1,1,1,1,1,1,1,1,1,1,1,1,1,1,1,1,1,1,1,1,1,1,1,1,
1,1,1,1,1,1,1,1,1,1,1,1,1,1,1,1,1,1,1,1,1,1,1,1,1,1,1,1,1,1,4),(-0.000309367040895943,
0.0452373400660471),(14.3981410127769,15.395688871123,16.3932367294691,
17.3907845878152,18.3883324461612,19.3858803045073,20.3834281628534,21.3809760211995,
22.3785238795456,23.3760717378917,24.3736195962378,25.3711674545839,26.3687153129299,
27.366263171276,28.3638110296221,29.3613588879682,30.3589067463143,31.3564546046604,
32.3540024630065,33.3515503213525,34.3490981796986,35.3466460380447,36.3441938963908,
37.3417417547369,38.339289613083,39.3368374714291,40.3343853297752,41.3319331881212,
42.3294810464673,43.3270289048134,44.3245767631595,45.3221246215056,46.3196724798517,
47.3172203381978,48.3147681965438,49.3123160548899,50.309863913236,51.3074117715821,
52.3049596299282,53.3025074882743,54.3000553466204,55.2976032049664,56.2951510633125,
57.2926989216586,58.2902467800047,59.2877946383508,60.2853424966969,61.282890355043,
62.2804382133891,63.2779860717351,64.2755339300812,65.2730817884273,66.2706296467734,
67.2681775051195,68.2657253634656,69.2632732218117,70.2608210801578,71.2583689385038,
72.2559167968499,73.253464655196,74.2510125135421,75.2485603718882,76.2461082302343,
77.2436560885804,78.2412039469264,79.2387518052725,80.2362996636186,81.2338475219647,
82.2313953803108,83.2289432386569,84.226491097003,85.2240389553491,86.2215868136952,
87.2191346720412,88.2166825303873,89.2142303887334,90.2117782470795,91.2093261054256,
92.2068739637717,93.2044218221178,94.2019696804638,95.1995175388099,96.197065397156,
97.1946132555021,98.1921611138482,99.1897089721943,100.18725683054,101.184804688886,
102.182352547233,103.179900405579,104.177448263925,105.174996122271,106.172892337254),
 .UNSPECIFIED.);
#287=B_SPLINE_SURFACE_WITH_KNOTS('',3,3,((#133121,#133122,#133123,#133124,
#133125,#133126,#133127,#133128,#133129,#133130,#133131,#133132,#133133,
#133134,#133135,#133136,#133137,#133138,#133139,#133140,#133141,#133142,
#133143,#133144,#133145,#133146,#133147,#133148,#133149,#133150,#133151,
#133152,#133153,#133154,#133155,#133156,#133157,#133158,#133159,#133160,
#133161,#133162,#133163,#133164,#133165,#133166,#133167,#133168,#133169,
#133170,#133171,#133172,#133173,#133174,#133175,#133176,#133177,#133178,
#133179,#133180,#133181,#133182,#133183,#133184,#133185,#133186,#133187,
#133188,#133189,#133190,#133191,#133192,#133193,#133194,#133195,#133196,
#133197,#133198,#133199,#133200,#133201,#133202,#133203,#133204,#133205,
#133206,#133207,#133208,#133209,#133210,#133211,#133212,#133213,#133214,
#133215),(#133216,#133217,#133218,#133219,#133220,#133221,#133222,#133223,
#133224,#133225,#133226,#133227,#133228,#133229,#133230,#133231,#133232,
#133233,#133234,#133235,#133236,#133237,#133238,#133239,#133240,#133241,
#133242,#133243,#133244,#133245,#133246,#133247,#133248,#133249,#133250,
#133251,#133252,#133253,#133254,#133255,#133256,#133257,#133258,#133259,
#133260,#133261,#133262,#133263,#133264,#133265,#133266,#133267,#133268,
#133269,#133270,#133271,#133272,#133273,#133274,#133275,#133276,#133277,
#133278,#133279,#133280,#133281,#133282,#133283,#133284,#133285,#133286,
#133287,#133288,#133289,#133290,#133291,#133292,#133293,#133294,#133295,
#133296,#133297,#133298,#133299,#133300,#133301,#133302,#133303,#133304,
#133305,#133306,#133307,#133308,#133309,#133310),(#133311,#133312,#133313,
#133314,#133315,#133316,#133317,#133318,#133319,#133320,#133321,#133322,
#133323,#133324,#133325,#133326,#133327,#133328,#133329,#133330,#133331,
#133332,#133333,#133334,#133335,#133336,#133337,#133338,#133339,#133340,
#133341,#133342,#133343,#133344,#133345,#133346,#133347,#133348,#133349,
#133350,#133351,#133352,#133353,#133354,#133355,#133356,#133357,#133358,
#133359,#133360,#133361,#133362,#133363,#133364,#133365,#133366,#133367,
#133368,#133369,#133370,#133371,#133372,#133373,#133374,#133375,#133376,
#133377,#133378,#133379,#133380,#133381,#133382,#133383,#133384,#133385,
#133386,#133387,#133388,#133389,#133390,#133391,#133392,#133393,#133394,
#133395,#133396,#133397,#133398,#133399,#133400,#133401,#133402,#133403,
#133404,#133405),(#133406,#133407,#133408,#133409,#133410,#133411,#133412,
#133413,#133414,#133415,#133416,#133417,#133418,#133419,#133420,#133421,
#133422,#133423,#133424,#133425,#133426,#133427,#133428,#133429,#133430,
#133431,#133432,#133433,#133434,#133435,#133436,#133437,#133438,#133439,
#133440,#133441,#133442,#133443,#133444,#133445,#133446,#133447,#133448,
#133449,#133450,#133451,#133452,#133453,#133454,#133455,#133456,#133457,
#133458,#133459,#133460,#133461,#133462,#133463,#133464,#133465,#133466,
#133467,#133468,#133469,#133470,#133471,#133472,#133473,#133474,#133475,
#133476,#133477,#133478,#133479,#133480,#133481,#133482,#133483,#133484,
#133485,#133486,#133487,#133488,#133489,#133490,#133491,#133492,#133493,
#133494,#133495,#133496,#133497,#133498,#133499,#133500)),.UNSPECIFIED.,
 .F.,.F.,.F.,(4,4),(4,1,1,1,1,1,1,1,1,1,1,1,1,1,1,1,1,1,1,1,1,1,1,1,1,1,
1,1,1,1,1,1,1,1,1,1,1,1,1,1,1,1,1,1,1,1,1,1,1,1,1,1,1,1,1,1,1,1,1,1,1,1,
1,1,1,1,1,1,1,1,1,1,1,1,1,1,1,1,1,1,1,1,1,1,1,1,1,1,1,1,1,1,4),(-0.000348309906186967,
0.0451835872598144),(11.8612316943504,12.8591278626027,13.8566757209488,
14.8542235792949,15.851771437641,16.8493192959871,17.8468671543332,18.8444150126793,
19.8419628710253,20.8395107293714,21.8370585877175,22.8346064460636,23.8321543044097,
24.8297021627558,25.8272500211019,26.8247978794479,27.822345737794,28.8198935961401,
29.8174414544862,30.8149893128323,31.8125371711784,32.8100850295245,33.8076328878706,
34.8051807462166,35.8027286045627,36.8002764629088,37.7978243212549,38.795372179601,
39.7929200379471,40.7904678962932,41.7880157546392,42.7855636129853,43.7831114713314,
44.7806593296775,45.7782071880236,46.7757550463697,47.7733029047158,48.7708507630619,
49.7683986214079,50.765946479754,51.7634943381001,52.7610421964462,53.7585900547923,
54.7561379131384,55.7536857714845,56.7512336298306,57.7487814881766,58.7463293465227,
59.7438772048688,60.7414250632149,61.738972921561,62.7365207799071,63.7340686382532,
64.7316164965992,65.7291643549453,66.7267122132914,67.7242600716375,68.7218079299836,
69.7193557883297,70.7169036466758,71.7144515050219,72.7119993633679,73.709547221714,
74.7070950800601,75.7046429384062,76.7021907967523,77.6997386550984,78.6972865134445,
79.6948343717906,80.6923822301366,81.6899300884827,82.6874779468288,83.6850258051749,
84.682573663521,85.6801215218671,86.6776693802132,87.6752172385592,88.6727650969053,
89.6703129552514,90.6678608135975,91.6654086719436,92.6629565302897,93.6605043886358,
94.6580522469818,95.6556001053279,96.653147963674,97.6506958220201,98.6482436803662,
99.6457915387123,100.643339397058,101.640887255404,102.638435113751,103.635982972097),
 .UNSPECIFIED.);
#288=B_SPLINE_SURFACE_WITH_KNOTS('',3,3,((#133673,#133674,#133675,#133676,
#133677,#133678,#133679,#133680,#133681,#133682,#133683,#133684,#133685,
#133686,#133687,#133688,#133689,#133690,#133691,#133692,#133693,#133694,
#133695,#133696,#133697,#133698,#133699,#133700,#133701,#133702,#133703,
#133704,#133705,#133706,#133707,#133708,#133709,#133710,#133711,#133712,
#133713,#133714,#133715,#133716,#133717,#133718,#133719,#133720,#133721,
#133722,#133723,#133724,#133725,#133726,#133727,#133728,#133729,#133730,
#133731,#133732,#133733,#133734,#133735,#133736,#133737,#133738,#133739,
#133740,#133741,#133742,#133743,#133744,#133745,#133746,#133747,#133748,
#133749,#133750,#133751,#133752,#133753,#133754,#133755,#133756,#133757,
#133758,#133759,#133760,#133761,#133762,#133763,#133764,#133765,#133766,
#133767),(#133768,#133769,#133770,#133771,#133772,#133773,#133774,#133775,
#133776,#133777,#133778,#133779,#133780,#133781,#133782,#133783,#133784,
#133785,#133786,#133787,#133788,#133789,#133790,#133791,#133792,#133793,
#133794,#133795,#133796,#133797,#133798,#133799,#133800,#133801,#133802,
#133803,#133804,#133805,#133806,#133807,#133808,#133809,#133810,#133811,
#133812,#133813,#133814,#133815,#133816,#133817,#133818,#133819,#133820,
#133821,#133822,#133823,#133824,#133825,#133826,#133827,#133828,#133829,
#133830,#133831,#133832,#133833,#133834,#133835,#133836,#133837,#133838,
#133839,#133840,#133841,#133842,#133843,#133844,#133845,#133846,#133847,
#133848,#133849,#133850,#133851,#133852,#133853,#133854,#133855,#133856,
#133857,#133858,#133859,#133860,#133861,#133862),(#133863,#133864,#133865,
#133866,#133867,#133868,#133869,#133870,#133871,#133872,#133873,#133874,
#133875,#133876,#133877,#133878,#133879,#133880,#133881,#133882,#133883,
#133884,#133885,#133886,#133887,#133888,#133889,#133890,#133891,#133892,
#133893,#133894,#133895,#133896,#133897,#133898,#133899,#133900,#133901,
#133902,#133903,#133904,#133905,#133906,#133907,#133908,#133909,#133910,
#133911,#133912,#133913,#133914,#133915,#133916,#133917,#133918,#133919,
#133920,#133921,#133922,#133923,#133924,#133925,#133926,#133927,#133928,
#133929,#133930,#133931,#133932,#133933,#133934,#133935,#133936,#133937,
#133938,#133939,#133940,#133941,#133942,#133943,#133944,#133945,#133946,
#133947,#133948,#133949,#133950,#133951,#133952,#133953,#133954,#133955,
#133956,#133957),(#133958,#133959,#133960,#133961,#133962,#133963,#133964,
#133965,#133966,#133967,#133968,#133969,#133970,#133971,#133972,#133973,
#133974,#133975,#133976,#133977,#133978,#133979,#133980,#133981,#133982,
#133983,#133984,#133985,#133986,#133987,#133988,#133989,#133990,#133991,
#133992,#133993,#133994,#133995,#133996,#133997,#133998,#133999,#134000,
#134001,#134002,#134003,#134004,#134005,#134006,#134007,#134008,#134009,
#134010,#134011,#134012,#134013,#134014,#134015,#134016,#134017,#134018,
#134019,#134020,#134021,#134022,#134023,#134024,#134025,#134026,#134027,
#134028,#134029,#134030,#134031,#134032,#134033,#134034,#134035,#134036,
#134037,#134038,#134039,#134040,#134041,#134042,#134043,#134044,#134045,
#134046,#134047,#134048,#134049,#134050,#134051,#134052)),.UNSPECIFIED.,
 .F.,.F.,.F.,(4,4),(4,1,1,1,1,1,1,1,1,1,1,1,1,1,1,1,1,1,1,1,1,1,1,1,1,1,
1,1,1,1,1,1,1,1,1,1,1,1,1,1,1,1,1,1,1,1,1,1,1,1,1,1,1,1,1,1,1,1,1,1,1,1,
1,1,1,1,1,1,1,1,1,1,1,1,1,1,1,1,1,1,1,1,1,1,1,1,1,1,1,1,1,1,4),(-0.000309363066806194,
0.0452373281646787),(14.3981410127769,15.395688871123,16.3932367294691,
17.3907845878152,18.3883324461612,19.3858803045073,20.3834281628534,21.3809760211995,
22.3785238795456,23.3760717378917,24.3736195962378,25.3711674545838,26.3687153129299,
27.366263171276,28.3638110296221,29.3613588879682,30.3589067463143,31.3564546046604,
32.3540024630065,33.3515503213525,34.3490981796986,35.3466460380447,36.3441938963908,
37.3417417547369,38.339289613083,39.3368374714291,40.3343853297751,41.3319331881212,
42.3294810464673,43.3270289048134,44.3245767631595,45.3221246215056,46.3196724798517,
47.3172203381977,48.3147681965438,49.3123160548899,50.309863913236,51.3074117715821,
52.3049596299282,53.3025074882743,54.3000553466204,55.2976032049664,56.2951510633125,
57.2926989216586,58.2902467800047,59.2877946383508,60.2853424966969,61.282890355043,
62.2804382133891,63.2779860717351,64.2755339300812,65.2730817884273,66.2706296467734,
67.2681775051195,68.2657253634656,69.2632732218117,70.2608210801577,71.2583689385038,
72.2559167968499,73.253464655196,74.2510125135421,75.2485603718882,76.2461082302343,
77.2436560885804,78.2412039469264,79.2387518052725,80.2362996636186,81.2338475219647,
82.2313953803108,83.2289432386569,84.226491097003,85.224038955349,86.2215868136951,
87.2191346720412,88.2166825303873,89.2142303887334,90.2117782470795,91.2093261054256,
92.2068739637717,93.2044218221177,94.2019696804638,95.1995175388099,96.197065397156,
97.1946132555021,98.1921611138482,99.1897089721943,100.18725683054,101.184804688886,
102.182352547233,103.179900405579,104.177448263925,105.174996122271,106.172892325352),
 .UNSPECIFIED.);
#289=B_SPLINE_SURFACE_WITH_KNOTS('',3,3,((#134231,#134232,#134233,#134234,
#134235,#134236,#134237,#134238,#134239,#134240,#134241,#134242,#134243,
#134244,#134245,#134246,#134247,#134248,#134249,#134250,#134251,#134252,
#134253,#134254,#134255,#134256,#134257,#134258,#134259,#134260,#134261,
#134262,#134263,#134264,#134265,#134266,#134267,#134268,#134269,#134270,
#134271,#134272,#134273,#134274,#134275,#134276,#134277,#134278,#134279,
#134280,#134281,#134282,#134283,#134284,#134285,#134286,#134287,#134288,
#134289,#134290,#134291,#134292,#134293,#134294,#134295,#134296,#134297,
#134298,#134299,#134300,#134301,#134302,#134303,#134304,#134305,#134306,
#134307,#134308,#134309,#134310,#134311,#134312,#134313,#134314,#134315,
#134316,#134317,#134318,#134319,#134320,#134321,#134322,#134323,#134324,
#134325),(#134326,#134327,#134328,#134329,#134330,#134331,#134332,#134333,
#134334,#134335,#134336,#134337,#134338,#134339,#134340,#134341,#134342,
#134343,#134344,#134345,#134346,#134347,#134348,#134349,#134350,#134351,
#134352,#134353,#134354,#134355,#134356,#134357,#134358,#134359,#134360,
#134361,#134362,#134363,#134364,#134365,#134366,#134367,#134368,#134369,
#134370,#134371,#134372,#134373,#134374,#134375,#134376,#134377,#134378,
#134379,#134380,#134381,#134382,#134383,#134384,#134385,#134386,#134387,
#134388,#134389,#134390,#134391,#134392,#134393,#134394,#134395,#134396,
#134397,#134398,#134399,#134400,#134401,#134402,#134403,#134404,#134405,
#134406,#134407,#134408,#134409,#134410,#134411,#134412,#134413,#134414,
#134415,#134416,#134417,#134418,#134419,#134420),(#134421,#134422,#134423,
#134424,#134425,#134426,#134427,#134428,#134429,#134430,#134431,#134432,
#134433,#134434,#134435,#134436,#134437,#134438,#134439,#134440,#134441,
#134442,#134443,#134444,#134445,#134446,#134447,#134448,#134449,#134450,
#134451,#134452,#134453,#134454,#134455,#134456,#134457,#134458,#134459,
#134460,#134461,#134462,#134463,#134464,#134465,#134466,#134467,#134468,
#134469,#134470,#134471,#134472,#134473,#134474,#134475,#134476,#134477,
#134478,#134479,#134480,#134481,#134482,#134483,#134484,#134485,#134486,
#134487,#134488,#134489,#134490,#134491,#134492,#134493,#134494,#134495,
#134496,#134497,#134498,#134499,#134500,#134501,#134502,#134503,#134504,
#134505,#134506,#134507,#134508,#134509,#134510,#134511,#134512,#134513,
#134514,#134515),(#134516,#134517,#134518,#134519,#134520,#134521,#134522,
#134523,#134524,#134525,#134526,#134527,#134528,#134529,#134530,#134531,
#134532,#134533,#134534,#134535,#134536,#134537,#134538,#134539,#134540,
#134541,#134542,#134543,#134544,#134545,#134546,#134547,#134548,#134549,
#134550,#134551,#134552,#134553,#134554,#134555,#134556,#134557,#134558,
#134559,#134560,#134561,#134562,#134563,#134564,#134565,#134566,#134567,
#134568,#134569,#134570,#134571,#134572,#134573,#134574,#134575,#134576,
#134577,#134578,#134579,#134580,#134581,#134582,#134583,#134584,#134585,
#134586,#134587,#134588,#134589,#134590,#134591,#134592,#134593,#134594,
#134595,#134596,#134597,#134598,#134599,#134600,#134601,#134602,#134603,
#134604,#134605,#134606,#134607,#134608,#134609,#134610)),.UNSPECIFIED.,
 .F.,.F.,.F.,(4,4),(4,1,1,1,1,1,1,1,1,1,1,1,1,1,1,1,1,1,1,1,1,1,1,1,1,1,
1,1,1,1,1,1,1,1,1,1,1,1,1,1,1,1,1,1,1,1,1,1,1,1,1,1,1,1,1,1,1,1,1,1,1,1,
1,1,1,1,1,1,1,1,1,1,1,1,1,1,1,1,1,1,1,1,1,1,1,1,1,1,1,1,1,1,4),(-0.000351924294538534,
0.0451855438310995),(11.8612280799621,12.8591278626027,13.8566757209488,
14.8542235792949,15.851771437641,16.8493192959871,17.8468671543332,18.8444150126793,
19.8419628710253,20.8395107293714,21.8370585877175,22.8346064460636,23.8321543044097,
24.8297021627558,25.8272500211019,26.8247978794479,27.822345737794,28.8198935961401,
29.8174414544862,30.8149893128323,31.8125371711784,32.8100850295245,33.8076328878706,
34.8051807462166,35.8027286045627,36.8002764629088,37.7978243212549,38.795372179601,
39.7929200379471,40.7904678962932,41.7880157546392,42.7855636129853,43.7831114713314,
44.7806593296775,45.7782071880236,46.7757550463697,47.7733029047158,48.7708507630618,
49.7683986214079,50.765946479754,51.7634943381001,52.7610421964462,53.7585900547923,
54.7561379131384,55.7536857714845,56.7512336298305,57.7487814881766,58.7463293465227,
59.7438772048688,60.7414250632149,61.738972921561,62.7365207799071,63.7340686382531,
64.7316164965992,65.7291643549453,66.7267122132914,67.7242600716375,68.7218079299836,
69.7193557883297,70.7169036466757,71.7144515050218,72.7119993633679,73.709547221714,
74.7070950800601,75.7046429384062,76.7021907967523,77.6997386550984,78.6972865134445,
79.6948343717905,80.6923822301366,81.6899300884827,82.6874779468288,83.6850258051749,
84.682573663521,85.6801215218671,86.6776693802131,87.6752172385592,88.6727650969053,
89.6703129552514,90.6678608135975,91.6654086719436,92.6629565302897,93.6605043886357,
94.6580522469818,95.6556001053279,96.653147963674,97.6506958220201,98.6482436803662,
99.6457915387123,100.643339397058,101.640887255404,102.638435113751,103.635982972097),
 .UNSPECIFIED.);
#290=B_SPLINE_SURFACE_WITH_KNOTS('',3,3,((#134783,#134784,#134785,#134786,
#134787,#134788,#134789,#134790,#134791,#134792,#134793,#134794,#134795,
#134796,#134797,#134798,#134799,#134800,#134801,#134802,#134803,#134804,
#134805,#134806,#134807,#134808,#134809,#134810,#134811,#134812,#134813,
#134814,#134815,#134816,#134817,#134818,#134819,#134820,#134821,#134822,
#134823,#134824,#134825,#134826,#134827,#134828,#134829,#134830,#134831,
#134832,#134833,#134834,#134835,#134836,#134837,#134838,#134839,#134840,
#134841,#134842,#134843,#134844,#134845,#134846,#134847,#134848,#134849,
#134850,#134851,#134852,#134853,#134854,#134855,#134856,#134857,#134858,
#134859,#134860,#134861,#134862,#134863,#134864,#134865,#134866,#134867,
#134868,#134869,#134870,#134871,#134872,#134873,#134874,#134875,#134876,
#134877),(#134878,#134879,#134880,#134881,#134882,#134883,#134884,#134885,
#134886,#134887,#134888,#134889,#134890,#134891,#134892,#134893,#134894,
#134895,#134896,#134897,#134898,#134899,#134900,#134901,#134902,#134903,
#134904,#134905,#134906,#134907,#134908,#134909,#134910,#134911,#134912,
#134913,#134914,#134915,#134916,#134917,#134918,#134919,#134920,#134921,
#134922,#134923,#134924,#134925,#134926,#134927,#134928,#134929,#134930,
#134931,#134932,#134933,#134934,#134935,#134936,#134937,#134938,#134939,
#134940,#134941,#134942,#134943,#134944,#134945,#134946,#134947,#134948,
#134949,#134950,#134951,#134952,#134953,#134954,#134955,#134956,#134957,
#134958,#134959,#134960,#134961,#134962,#134963,#134964,#134965,#134966,
#134967,#134968,#134969,#134970,#134971,#134972),(#134973,#134974,#134975,
#134976,#134977,#134978,#134979,#134980,#134981,#134982,#134983,#134984,
#134985,#134986,#134987,#134988,#134989,#134990,#134991,#134992,#134993,
#134994,#134995,#134996,#134997,#134998,#134999,#135000,#135001,#135002,
#135003,#135004,#135005,#135006,#135007,#135008,#135009,#135010,#135011,
#135012,#135013,#135014,#135015,#135016,#135017,#135018,#135019,#135020,
#135021,#135022,#135023,#135024,#135025,#135026,#135027,#135028,#135029,
#135030,#135031,#135032,#135033,#135034,#135035,#135036,#135037,#135038,
#135039,#135040,#135041,#135042,#135043,#135044,#135045,#135046,#135047,
#135048,#135049,#135050,#135051,#135052,#135053,#135054,#135055,#135056,
#135057,#135058,#135059,#135060,#135061,#135062,#135063,#135064,#135065,
#135066,#135067),(#135068,#135069,#135070,#135071,#135072,#135073,#135074,
#135075,#135076,#135077,#135078,#135079,#135080,#135081,#135082,#135083,
#135084,#135085,#135086,#135087,#135088,#135089,#135090,#135091,#135092,
#135093,#135094,#135095,#135096,#135097,#135098,#135099,#135100,#135101,
#135102,#135103,#135104,#135105,#135106,#135107,#135108,#135109,#135110,
#135111,#135112,#135113,#135114,#135115,#135116,#135117,#135118,#135119,
#135120,#135121,#135122,#135123,#135124,#135125,#135126,#135127,#135128,
#135129,#135130,#135131,#135132,#135133,#135134,#135135,#135136,#135137,
#135138,#135139,#135140,#135141,#135142,#135143,#135144,#135145,#135146,
#135147,#135148,#135149,#135150,#135151,#135152,#135153,#135154,#135155,
#135156,#135157,#135158,#135159,#135160,#135161,#135162)),.UNSPECIFIED.,
 .F.,.F.,.F.,(4,4),(4,1,1,1,1,1,1,1,1,1,1,1,1,1,1,1,1,1,1,1,1,1,1,1,1,1,
1,1,1,1,1,1,1,1,1,1,1,1,1,1,1,1,1,1,1,1,1,1,1,1,1,1,1,1,1,1,1,1,1,1,1,1,
1,1,1,1,1,1,1,1,1,1,1,1,1,1,1,1,1,1,1,1,1,1,1,1,1,1,1,1,1,1,4),(-0.000310865142038579,
0.0452409353936679),(14.3981410127769,15.395688871123,16.3932367294691,
17.3907845878152,18.3883324461612,19.3858803045073,20.3834281628534,21.3809760211995,
22.3785238795456,23.3760717378917,24.3736195962378,25.3711674545838,26.3687153129299,
27.366263171276,28.3638110296221,29.3613588879682,30.3589067463143,31.3564546046604,
32.3540024630065,33.3515503213525,34.3490981796986,35.3466460380447,36.3441938963908,
37.3417417547369,38.339289613083,39.3368374714291,40.3343853297751,41.3319331881212,
42.3294810464673,43.3270289048134,44.3245767631595,45.3221246215056,46.3196724798517,
47.3172203381978,48.3147681965438,49.3123160548899,50.309863913236,51.3074117715821,
52.3049596299282,53.3025074882743,54.3000553466204,55.2976032049664,56.2951510633125,
57.2926989216586,58.2902467800047,59.2877946383508,60.2853424966969,61.282890355043,
62.2804382133891,63.2779860717351,64.2755339300812,65.2730817884273,66.2706296467734,
67.2681775051195,68.2657253634656,69.2632732218117,70.2608210801578,71.2583689385038,
72.2559167968499,73.253464655196,74.2510125135421,75.2485603718882,76.2461082302343,
77.2436560885804,78.2412039469264,79.2387518052725,80.2362996636186,81.2338475219647,
82.2313953803108,83.2289432386569,84.226491097003,85.2240389553491,86.2215868136951,
87.2191346720412,88.2166825303873,89.2142303887334,90.2117782470795,91.2093261054256,
92.2068739637717,93.2044218221178,94.2019696804638,95.1995175388099,96.197065397156,
97.1946132555021,98.1921611138482,99.1897089721943,100.18725683054,101.184804688886,
102.182352547233,103.179900405579,104.177448263925,105.174996122271,106.172895932581),
 .UNSPECIFIED.);
#291=B_SPLINE_SURFACE_WITH_KNOTS('',3,3,((#135341,#135342,#135343,#135344,
#135345,#135346,#135347,#135348,#135349,#135350,#135351,#135352,#135353,
#135354,#135355,#135356,#135357,#135358,#135359,#135360,#135361,#135362,
#135363,#135364,#135365,#135366,#135367,#135368,#135369,#135370,#135371,
#135372,#135373,#135374,#135375,#135376,#135377,#135378,#135379,#135380,
#135381,#135382,#135383,#135384,#135385,#135386,#135387,#135388,#135389,
#135390,#135391,#135392,#135393,#135394,#135395,#135396,#135397,#135398,
#135399,#135400,#135401,#135402,#135403,#135404,#135405,#135406,#135407,
#135408,#135409,#135410,#135411,#135412,#135413,#135414,#135415,#135416,
#135417,#135418,#135419,#135420,#135421,#135422,#135423,#135424,#135425,
#135426,#135427,#135428,#135429,#135430,#135431,#135432,#135433,#135434,
#135435),(#135436,#135437,#135438,#135439,#135440,#135441,#135442,#135443,
#135444,#135445,#135446,#135447,#135448,#135449,#135450,#135451,#135452,
#135453,#135454,#135455,#135456,#135457,#135458,#135459,#135460,#135461,
#135462,#135463,#135464,#135465,#135466,#135467,#135468,#135469,#135470,
#135471,#135472,#135473,#135474,#135475,#135476,#135477,#135478,#135479,
#135480,#135481,#135482,#135483,#135484,#135485,#135486,#135487,#135488,
#135489,#135490,#135491,#135492,#135493,#135494,#135495,#135496,#135497,
#135498,#135499,#135500,#135501,#135502,#135503,#135504,#135505,#135506,
#135507,#135508,#135509,#135510,#135511,#135512,#135513,#135514,#135515,
#135516,#135517,#135518,#135519,#135520,#135521,#135522,#135523,#135524,
#135525,#135526,#135527,#135528,#135529,#135530),(#135531,#135532,#135533,
#135534,#135535,#135536,#135537,#135538,#135539,#135540,#135541,#135542,
#135543,#135544,#135545,#135546,#135547,#135548,#135549,#135550,#135551,
#135552,#135553,#135554,#135555,#135556,#135557,#135558,#135559,#135560,
#135561,#135562,#135563,#135564,#135565,#135566,#135567,#135568,#135569,
#135570,#135571,#135572,#135573,#135574,#135575,#135576,#135577,#135578,
#135579,#135580,#135581,#135582,#135583,#135584,#135585,#135586,#135587,
#135588,#135589,#135590,#135591,#135592,#135593,#135594,#135595,#135596,
#135597,#135598,#135599,#135600,#135601,#135602,#135603,#135604,#135605,
#135606,#135607,#135608,#135609,#135610,#135611,#135612,#135613,#135614,
#135615,#135616,#135617,#135618,#135619,#135620,#135621,#135622,#135623,
#135624,#135625),(#135626,#135627,#135628,#135629,#135630,#135631,#135632,
#135633,#135634,#135635,#135636,#135637,#135638,#135639,#135640,#135641,
#135642,#135643,#135644,#135645,#135646,#135647,#135648,#135649,#135650,
#135651,#135652,#135653,#135654,#135655,#135656,#135657,#135658,#135659,
#135660,#135661,#135662,#135663,#135664,#135665,#135666,#135667,#135668,
#135669,#135670,#135671,#135672,#135673,#135674,#135675,#135676,#135677,
#135678,#135679,#135680,#135681,#135682,#135683,#135684,#135685,#135686,
#135687,#135688,#135689,#135690,#135691,#135692,#135693,#135694,#135695,
#135696,#135697,#135698,#135699,#135700,#135701,#135702,#135703,#135704,
#135705,#135706,#135707,#135708,#135709,#135710,#135711,#135712,#135713,
#135714,#135715,#135716,#135717,#135718,#135719,#135720)),.UNSPECIFIED.,
 .F.,.F.,.F.,(4,4),(4,1,1,1,1,1,1,1,1,1,1,1,1,1,1,1,1,1,1,1,1,1,1,1,1,1,
1,1,1,1,1,1,1,1,1,1,1,1,1,1,1,1,1,1,1,1,1,1,1,1,1,1,1,1,1,1,1,1,1,1,1,1,
1,1,1,1,1,1,1,1,1,1,1,1,1,1,1,1,1,1,1,1,1,1,1,1,1,1,1,1,1,1,4),(-0.000351931351939438,
0.0451855479770649),(11.8612280729047,12.8591278626027,13.8566757209488,
14.8542235792949,15.851771437641,16.8493192959871,17.8468671543332,18.8444150126792,
19.8419628710253,20.8395107293714,21.8370585877175,22.8346064460636,23.8321543044097,
24.8297021627558,25.8272500211019,26.8247978794479,27.822345737794,28.8198935961401,
29.8174414544862,30.8149893128323,31.8125371711784,32.8100850295245,33.8076328878705,
34.8051807462166,35.8027286045627,36.8002764629088,37.7978243212549,38.795372179601,
39.7929200379471,40.7904678962932,41.7880157546392,42.7855636129853,43.7831114713314,
44.7806593296775,45.7782071880236,46.7757550463697,47.7733029047158,48.7708507630618,
49.7683986214079,50.765946479754,51.7634943381001,52.7610421964462,53.7585900547923,
54.7561379131384,55.7536857714844,56.7512336298305,57.7487814881766,58.7463293465227,
59.7438772048688,60.7414250632149,61.738972921561,62.7365207799071,63.7340686382531,
64.7316164965992,65.7291643549453,66.7267122132914,67.7242600716375,68.7218079299836,
69.7193557883297,70.7169036466757,71.7144515050218,72.7119993633679,73.709547221714,
74.7070950800601,75.7046429384062,76.7021907967523,77.6997386550983,78.6972865134445,
79.6948343717905,80.6923822301366,81.6899300884827,82.6874779468288,83.6850258051749,
84.682573663521,85.6801215218671,86.6776693802131,87.6752172385592,88.6727650969053,
89.6703129552514,90.6678608135975,91.6654086719436,92.6629565302896,93.6605043886357,
94.6580522469818,95.6556001053279,96.653147963674,97.6506958220201,98.6482436803662,
99.6457915387122,100.643339397058,101.640887255404,102.638435113751,103.635982972097),
 .UNSPECIFIED.);
#292=B_SPLINE_SURFACE_WITH_KNOTS('',3,3,((#135893,#135894,#135895,#135896,
#135897,#135898,#135899,#135900,#135901,#135902,#135903,#135904,#135905,
#135906,#135907,#135908,#135909,#135910,#135911,#135912,#135913,#135914,
#135915,#135916,#135917,#135918,#135919,#135920,#135921,#135922,#135923,
#135924,#135925,#135926,#135927,#135928,#135929,#135930,#135931,#135932,
#135933,#135934,#135935,#135936,#135937,#135938,#135939,#135940,#135941,
#135942,#135943,#135944,#135945,#135946,#135947,#135948,#135949,#135950,
#135951,#135952,#135953,#135954,#135955,#135956,#135957,#135958,#135959,
#135960,#135961,#135962,#135963,#135964,#135965,#135966,#135967,#135968,
#135969,#135970,#135971,#135972,#135973,#135974,#135975,#135976,#135977,
#135978,#135979,#135980,#135981,#135982,#135983,#135984,#135985,#135986,
#135987),(#135988,#135989,#135990,#135991,#135992,#135993,#135994,#135995,
#135996,#135997,#135998,#135999,#136000,#136001,#136002,#136003,#136004,
#136005,#136006,#136007,#136008,#136009,#136010,#136011,#136012,#136013,
#136014,#136015,#136016,#136017,#136018,#136019,#136020,#136021,#136022,
#136023,#136024,#136025,#136026,#136027,#136028,#136029,#136030,#136031,
#136032,#136033,#136034,#136035,#136036,#136037,#136038,#136039,#136040,
#136041,#136042,#136043,#136044,#136045,#136046,#136047,#136048,#136049,
#136050,#136051,#136052,#136053,#136054,#136055,#136056,#136057,#136058,
#136059,#136060,#136061,#136062,#136063,#136064,#136065,#136066,#136067,
#136068,#136069,#136070,#136071,#136072,#136073,#136074,#136075,#136076,
#136077,#136078,#136079,#136080,#136081,#136082),(#136083,#136084,#136085,
#136086,#136087,#136088,#136089,#136090,#136091,#136092,#136093,#136094,
#136095,#136096,#136097,#136098,#136099,#136100,#136101,#136102,#136103,
#136104,#136105,#136106,#136107,#136108,#136109,#136110,#136111,#136112,
#136113,#136114,#136115,#136116,#136117,#136118,#136119,#136120,#136121,
#136122,#136123,#136124,#136125,#136126,#136127,#136128,#136129,#136130,
#136131,#136132,#136133,#136134,#136135,#136136,#136137,#136138,#136139,
#136140,#136141,#136142,#136143,#136144,#136145,#136146,#136147,#136148,
#136149,#136150,#136151,#136152,#136153,#136154,#136155,#136156,#136157,
#136158,#136159,#136160,#136161,#136162,#136163,#136164,#136165,#136166,
#136167,#136168,#136169,#136170,#136171,#136172,#136173,#136174,#136175,
#136176,#136177),(#136178,#136179,#136180,#136181,#136182,#136183,#136184,
#136185,#136186,#136187,#136188,#136189,#136190,#136191,#136192,#136193,
#136194,#136195,#136196,#136197,#136198,#136199,#136200,#136201,#136202,
#136203,#136204,#136205,#136206,#136207,#136208,#136209,#136210,#136211,
#136212,#136213,#136214,#136215,#136216,#136217,#136218,#136219,#136220,
#136221,#136222,#136223,#136224,#136225,#136226,#136227,#136228,#136229,
#136230,#136231,#136232,#136233,#136234,#136235,#136236,#136237,#136238,
#136239,#136240,#136241,#136242,#136243,#136244,#136245,#136246,#136247,
#136248,#136249,#136250,#136251,#136252,#136253,#136254,#136255,#136256,
#136257,#136258,#136259,#136260,#136261,#136262,#136263,#136264,#136265,
#136266,#136267,#136268,#136269,#136270,#136271,#136272)),.UNSPECIFIED.,
 .F.,.F.,.F.,(4,4),(4,1,1,1,1,1,1,1,1,1,1,1,1,1,1,1,1,1,1,1,1,1,1,1,1,1,
1,1,1,1,1,1,1,1,1,1,1,1,1,1,1,1,1,1,1,1,1,1,1,1,1,1,1,1,1,1,1,1,1,1,1,1,
1,1,1,1,1,1,1,1,1,1,1,1,1,1,1,1,1,1,1,1,1,1,1,1,1,1,1,1,1,1,4),(-0.000310869945906298,
0.0452409448509825),(14.3981410127769,15.395688871123,16.3932367294691,
17.3907845878152,18.3883324461612,19.3858803045073,20.3834281628534,21.3809760211995,
22.3785238795456,23.3760717378917,24.3736195962378,25.3711674545838,26.3687153129299,
27.366263171276,28.3638110296221,29.3613588879682,30.3589067463143,31.3564546046604,
32.3540024630065,33.3515503213525,34.3490981796986,35.3466460380447,36.3441938963908,
37.3417417547369,38.339289613083,39.3368374714291,40.3343853297751,41.3319331881212,
42.3294810464673,43.3270289048134,44.3245767631595,45.3221246215056,46.3196724798517,
47.3172203381978,48.3147681965438,49.3123160548899,50.309863913236,51.3074117715821,
52.3049596299282,53.3025074882743,54.3000553466204,55.2976032049664,56.2951510633125,
57.2926989216586,58.2902467800047,59.2877946383508,60.2853424966969,61.282890355043,
62.2804382133891,63.2779860717351,64.2755339300812,65.2730817884273,66.2706296467734,
67.2681775051195,68.2657253634656,69.2632732218117,70.2608210801578,71.2583689385038,
72.2559167968499,73.253464655196,74.2510125135421,75.2485603718882,76.2461082302343,
77.2436560885804,78.2412039469264,79.2387518052725,80.2362996636186,81.2338475219647,
82.2313953803108,83.2289432386569,84.226491097003,85.2240389553491,86.2215868136951,
87.2191346720412,88.2166825303873,89.2142303887334,90.2117782470795,91.2093261054256,
92.2068739637717,93.2044218221178,94.2019696804638,95.1995175388099,96.197065397156,
97.1946132555021,98.1921611138482,99.1897089721943,100.18725683054,101.184804688886,
102.182352547233,103.179900405579,104.177448263925,105.174996122271,106.172895942038),
 .UNSPECIFIED.);
#293=B_SPLINE_SURFACE_WITH_KNOTS('',3,3,((#180613,#180614,#180615,#180616,
#180617,#180618,#180619,#180620,#180621,#180622,#180623,#180624,#180625,
#180626,#180627,#180628,#180629,#180630,#180631,#180632,#180633,#180634,
#180635,#180636,#180637,#180638,#180639,#180640,#180641,#180642,#180643,
#180644,#180645,#180646,#180647,#180648,#180649,#180650,#180651,#180652,
#180653,#180654,#180655,#180656,#180657,#180658,#180659,#180660,#180661,
#180662,#180663,#180664,#180665,#180666,#180667,#180668,#180669,#180670,
#180671,#180672,#180673,#180674,#180675,#180676,#180677,#180678,#180679,
#180680,#180681,#180682,#180683,#180684,#180685,#180686,#180687,#180688,
#180689,#180690,#180691,#180692,#180693,#180694,#180695,#180696,#180697,
#180698,#180699,#180700,#180701,#180702,#180703,#180704,#180705,#180706,
#180707,#180708,#180709,#180710,#180711,#180712,#180713,#180714,#180715,
#180716,#180717,#180718,#180719,#180720,#180721,#180722,#180723,#180724,
#180725,#180726,#180727,#180728,#180729,#180730,#180731,#180732,#180733,
#180734,#180735,#180736,#180737,#180738,#180739,#180740,#180741,#180742,
#180743,#180744,#180745,#180746,#180747,#180748,#180749,#180750,#180751,
#180752,#180753,#180754,#180755,#180756,#180757,#180758,#180759,#180760,
#180761,#180762,#180763,#180764,#180765,#180766,#180767,#180768,#180769,
#180770,#180771,#180772,#180773,#180774,#180775,#180776,#180777,#180778,
#180779,#180780,#180781,#180782,#180783,#180784,#180785,#180786,#180787,
#180788,#180789,#180790,#180791,#180792,#180793,#180794,#180795,#180796,
#180797,#180798,#180799,#180800,#180801,#180802,#180803,#180804,#180805,
#180806,#180807,#180808,#180809,#180810,#180811,#180812,#180813,#180814,
#180815,#180816,#180817,#180818,#180819,#180820,#180821,#180822,#180823,
#180824,#180825,#180826,#180827,#180828,#180829,#180830,#180831,#180832,
#180833,#180834,#180835,#180836,#180837,#180838,#180839,#180840,#180841,
#180842,#180843,#180844,#180845,#180846,#180847,#180848,#180849,#180850,
#180851,#180852,#180853,#180854,#180855,#180856,#180857,#180858,#180859,
#180860,#180861,#180862,#180863,#180864,#180865,#180866,#180867,#180868,
#180869,#180870,#180871,#180872,#180873,#180874,#180875,#180876,#180877,
#180878,#180879,#180880,#180881,#180882,#180883,#180884,#180885,#180886,
#180887,#180888,#180889,#180890,#180891,#180892,#180893,#180894,#180895,
#180896,#180897,#180898,#180899,#180900,#180901,#180902,#180903,#180904,
#180905,#180906,#180907,#180908,#180909,#180910,#180911,#180912,#180913,
#180914,#180915,#180916,#180917,#180918,#180919,#180920,#180921,#180922,
#180923,#180924,#180925,#180926,#180927,#180928,#180929,#180930,#180931,
#180932,#180933,#180934,#180935,#180936,#180937,#180938,#180939,#180940,
#180941,#180942,#180943,#180944,#180945,#180946,#180947,#180948,#180949,
#180950,#180951,#180952,#180953,#180954,#180955,#180956,#180957,#180958,
#180959,#180960,#180961,#180962,#180963,#180964,#180965,#180966,#180967,
#180968,#180969,#180970,#180971,#180972,#180973,#180974,#180975,#180976,
#180977,#180978,#180979,#180980,#180981,#180982,#180983,#180984,#180985,
#180986,#180987,#180988,#180989,#180990,#180991,#180992,#180993,#180994,
#180995,#180996,#180997,#180998,#180999,#181000,#181001,#181002,#181003,
#181004,#181005,#181006,#181007,#181008,#181009,#181010,#181011,#181012,
#181013,#181014,#181015,#181016,#181017,#181018,#181019,#181020,#181021,
#181022,#181023,#181024,#181025,#181026,#181027,#181028,#181029,#181030,
#181031,#181032,#181033,#181034,#181035,#181036,#181037,#181038,#181039,
#181040,#181041,#181042,#181043,#181044,#181045,#181046,#181047,#181048,
#181049,#181050,#181051,#181052,#181053,#181054,#181055,#181056,#181057,
#181058,#181059,#181060,#181061,#181062,#181063,#181064,#181065,#181066,
#181067,#181068,#181069,#181070,#181071,#181072,#181073,#181074,#181075,
#181076,#181077,#181078,#181079,#181080,#181081,#181082,#181083,#181084,
#181085,#181086,#181087,#181088,#181089,#181090,#181091,#181092,#181093,
#181094,#181095,#181096,#181097,#181098,#181099,#181100,#181101,#181102,
#181103,#181104,#181105,#181106,#181107,#181108,#181109,#181110,#181111,
#181112,#181113,#181114,#181115,#181116,#181117,#181118,#181119,#181120,
#181121,#181122,#181123,#181124,#181125,#181126,#181127,#181128,#181129,
#181130,#181131,#181132,#181133,#181134,#181135,#181136,#181137,#181138,
#181139,#181140,#181141,#181142,#181143,#181144,#181145,#181146,#181147,
#181148,#181149,#181150),(#181151,#181152,#181153,#181154,#181155,#181156,
#181157,#181158,#181159,#181160,#181161,#181162,#181163,#181164,#181165,
#181166,#181167,#181168,#181169,#181170,#181171,#181172,#181173,#181174,
#181175,#181176,#181177,#181178,#181179,#181180,#181181,#181182,#181183,
#181184,#181185,#181186,#181187,#181188,#181189,#181190,#181191,#181192,
#181193,#181194,#181195,#181196,#181197,#181198,#181199,#181200,#181201,
#181202,#181203,#181204,#181205,#181206,#181207,#181208,#181209,#181210,
#181211,#181212,#181213,#181214,#181215,#181216,#181217,#181218,#181219,
#181220,#181221,#181222,#181223,#181224,#181225,#181226,#181227,#181228,
#181229,#181230,#181231,#181232,#181233,#181234,#181235,#181236,#181237,
#181238,#181239,#181240,#181241,#181242,#181243,#181244,#181245,#181246,
#181247,#181248,#181249,#181250,#181251,#181252,#181253,#181254,#181255,
#181256,#181257,#181258,#181259,#181260,#181261,#181262,#181263,#181264,
#181265,#181266,#181267,#181268,#181269,#181270,#181271,#181272,#181273,
#181274,#181275,#181276,#181277,#181278,#181279,#181280,#181281,#181282,
#181283,#181284,#181285,#181286,#181287,#181288,#181289,#181290,#181291,
#181292,#181293,#181294,#181295,#181296,#181297,#181298,#181299,#181300,
#181301,#181302,#181303,#181304,#181305,#181306,#181307,#181308,#181309,
#181310,#181311,#181312,#181313,#181314,#181315,#181316,#181317,#181318,
#181319,#181320,#181321,#181322,#181323,#181324,#181325,#181326,#181327,
#181328,#181329,#181330,#181331,#181332,#181333,#181334,#181335,#181336,
#181337,#181338,#181339,#181340,#181341,#181342,#181343,#181344,#181345,
#181346,#181347,#181348,#181349,#181350,#181351,#181352,#181353,#181354,
#181355,#181356,#181357,#181358,#181359,#181360,#181361,#181362,#181363,
#181364,#181365,#181366,#181367,#181368,#181369,#181370,#181371,#181372,
#181373,#181374,#181375,#181376,#181377,#181378,#181379,#181380,#181381,
#181382,#181383,#181384,#181385,#181386,#181387,#181388,#181389,#181390,
#181391,#181392,#181393,#181394,#181395,#181396,#181397,#181398,#181399,
#181400,#181401,#181402,#181403,#181404,#181405,#181406,#181407,#181408,
#181409,#181410,#181411,#181412,#181413,#181414,#181415,#181416,#181417,
#181418,#181419,#181420,#181421,#181422,#181423,#181424,#181425,#181426,
#181427,#181428,#181429,#181430,#181431,#181432,#181433,#181434,#181435,
#181436,#181437,#181438,#181439,#181440,#181441,#181442,#181443,#181444,
#181445,#181446,#181447,#181448,#181449,#181450,#181451,#181452,#181453,
#181454,#181455,#181456,#181457,#181458,#181459,#181460,#181461,#181462,
#181463,#181464,#181465,#181466,#181467,#181468,#181469,#181470,#181471,
#181472,#181473,#181474,#181475,#181476,#181477,#181478,#181479,#181480,
#181481,#181482,#181483,#181484,#181485,#181486,#181487,#181488,#181489,
#181490,#181491,#181492,#181493,#181494,#181495,#181496,#181497,#181498,
#181499,#181500,#181501,#181502,#181503,#181504,#181505,#181506,#181507,
#181508,#181509,#181510,#181511,#181512,#181513,#181514,#181515,#181516,
#181517,#181518,#181519,#181520,#181521,#181522,#181523,#181524,#181525,
#181526,#181527,#181528,#181529,#181530,#181531,#181532,#181533,#181534,
#181535,#181536,#181537,#181538,#181539,#181540,#181541,#181542,#181543,
#181544,#181545,#181546,#181547,#181548,#181549,#181550,#181551,#181552,
#181553,#181554,#181555,#181556,#181557,#181558,#181559,#181560,#181561,
#181562,#181563,#181564,#181565,#181566,#181567,#181568,#181569,#181570,
#181571,#181572,#181573,#181574,#181575,#181576,#181577,#181578,#181579,
#181580,#181581,#181582,#181583,#181584,#181585,#181586,#181587,#181588,
#181589,#181590,#181591,#181592,#181593,#181594,#181595,#181596,#181597,
#181598,#181599,#181600,#181601,#181602,#181603,#181604,#181605,#181606,
#181607,#181608,#181609,#181610,#181611,#181612,#181613,#181614,#181615,
#181616,#181617,#181618,#181619,#181620,#181621,#181622,#181623,#181624,
#181625,#181626,#181627,#181628,#181629,#181630,#181631,#181632,#181633,
#181634,#181635,#181636,#181637,#181638,#181639,#181640,#181641,#181642,
#181643,#181644,#181645,#181646,#181647,#181648,#181649,#181650,#181651,
#181652,#181653,#181654,#181655,#181656,#181657,#181658,#181659,#181660,
#181661,#181662,#181663,#181664,#181665,#181666,#181667,#181668,#181669,
#181670,#181671,#181672,#181673,#181674,#181675,#181676,#181677,#181678,
#181679,#181680,#181681,#181682,#181683,#181684,#181685,#181686,#181687,
#181688),(#181689,#181690,#181691,#181692,#181693,#181694,#181695,#181696,
#181697,#181698,#181699,#181700,#181701,#181702,#181703,#181704,#181705,
#181706,#181707,#181708,#181709,#181710,#181711,#181712,#181713,#181714,
#181715,#181716,#181717,#181718,#181719,#181720,#181721,#181722,#181723,
#181724,#181725,#181726,#181727,#181728,#181729,#181730,#181731,#181732,
#181733,#181734,#181735,#181736,#181737,#181738,#181739,#181740,#181741,
#181742,#181743,#181744,#181745,#181746,#181747,#181748,#181749,#181750,
#181751,#181752,#181753,#181754,#181755,#181756,#181757,#181758,#181759,
#181760,#181761,#181762,#181763,#181764,#181765,#181766,#181767,#181768,
#181769,#181770,#181771,#181772,#181773,#181774,#181775,#181776,#181777,
#181778,#181779,#181780,#181781,#181782,#181783,#181784,#181785,#181786,
#181787,#181788,#181789,#181790,#181791,#181792,#181793,#181794,#181795,
#181796,#181797,#181798,#181799,#181800,#181801,#181802,#181803,#181804,
#181805,#181806,#181807,#181808,#181809,#181810,#181811,#181812,#181813,
#181814,#181815,#181816,#181817,#181818,#181819,#181820,#181821,#181822,
#181823,#181824,#181825,#181826,#181827,#181828,#181829,#181830,#181831,
#181832,#181833,#181834,#181835,#181836,#181837,#181838,#181839,#181840,
#181841,#181842,#181843,#181844,#181845,#181846,#181847,#181848,#181849,
#181850,#181851,#181852,#181853,#181854,#181855,#181856,#181857,#181858,
#181859,#181860,#181861,#181862,#181863,#181864,#181865,#181866,#181867,
#181868,#181869,#181870,#181871,#181872,#181873,#181874,#181875,#181876,
#181877,#181878,#181879,#181880,#181881,#181882,#181883,#181884,#181885,
#181886,#181887,#181888,#181889,#181890,#181891,#181892,#181893,#181894,
#181895,#181896,#181897,#181898,#181899,#181900,#181901,#181902,#181903,
#181904,#181905,#181906,#181907,#181908,#181909,#181910,#181911,#181912,
#181913,#181914,#181915,#181916,#181917,#181918,#181919,#181920,#181921,
#181922,#181923,#181924,#181925,#181926,#181927,#181928,#181929,#181930,
#181931,#181932,#181933,#181934,#181935,#181936,#181937,#181938,#181939,
#181940,#181941,#181942,#181943,#181944,#181945,#181946,#181947,#181948,
#181949,#181950,#181951,#181952,#181953,#181954,#181955,#181956,#181957,
#181958,#181959,#181960,#181961,#181962,#181963,#181964,#181965,#181966,
#181967,#181968,#181969,#181970,#181971,#181972,#181973,#181974,#181975,
#181976,#181977,#181978,#181979,#181980,#181981,#181982,#181983,#181984,
#181985,#181986,#181987,#181988,#181989,#181990,#181991,#181992,#181993,
#181994,#181995,#181996,#181997,#181998,#181999,#182000,#182001,#182002,
#182003,#182004,#182005,#182006,#182007,#182008,#182009,#182010,#182011,
#182012,#182013,#182014,#182015,#182016,#182017,#182018,#182019,#182020,
#182021,#182022,#182023,#182024,#182025,#182026,#182027,#182028,#182029,
#182030,#182031,#182032,#182033,#182034,#182035,#182036,#182037,#182038,
#182039,#182040,#182041,#182042,#182043,#182044,#182045,#182046,#182047,
#182048,#182049,#182050,#182051,#182052,#182053,#182054,#182055,#182056,
#182057,#182058,#182059,#182060,#182061,#182062,#182063,#182064,#182065,
#182066,#182067,#182068,#182069,#182070,#182071,#182072,#182073,#182074,
#182075,#182076,#182077,#182078,#182079,#182080,#182081,#182082,#182083,
#182084,#182085,#182086,#182087,#182088,#182089,#182090,#182091,#182092,
#182093,#182094,#182095,#182096,#182097,#182098,#182099,#182100,#182101,
#182102,#182103,#182104,#182105,#182106,#182107,#182108,#182109,#182110,
#182111,#182112,#182113,#182114,#182115,#182116,#182117,#182118,#182119,
#182120,#182121,#182122,#182123,#182124,#182125,#182126,#182127,#182128,
#182129,#182130,#182131,#182132,#182133,#182134,#182135,#182136,#182137,
#182138,#182139,#182140,#182141,#182142,#182143,#182144,#182145,#182146,
#182147,#182148,#182149,#182150,#182151,#182152,#182153,#182154,#182155,
#182156,#182157,#182158,#182159,#182160,#182161,#182162,#182163,#182164,
#182165,#182166,#182167,#182168,#182169,#182170,#182171,#182172,#182173,
#182174,#182175,#182176,#182177,#182178,#182179,#182180,#182181,#182182,
#182183,#182184,#182185,#182186,#182187,#182188,#182189,#182190,#182191,
#182192,#182193,#182194,#182195,#182196,#182197,#182198,#182199,#182200,
#182201,#182202,#182203,#182204,#182205,#182206,#182207,#182208,#182209,
#182210,#182211,#182212,#182213,#182214,#182215,#182216,#182217,#182218,
#182219,#182220,#182221,#182222,#182223,#182224,#182225,#182226),(#182227,
#182228,#182229,#182230,#182231,#182232,#182233,#182234,#182235,#182236,
#182237,#182238,#182239,#182240,#182241,#182242,#182243,#182244,#182245,
#182246,#182247,#182248,#182249,#182250,#182251,#182252,#182253,#182254,
#182255,#182256,#182257,#182258,#182259,#182260,#182261,#182262,#182263,
#182264,#182265,#182266,#182267,#182268,#182269,#182270,#182271,#182272,
#182273,#182274,#182275,#182276,#182277,#182278,#182279,#182280,#182281,
#182282,#182283,#182284,#182285,#182286,#182287,#182288,#182289,#182290,
#182291,#182292,#182293,#182294,#182295,#182296,#182297,#182298,#182299,
#182300,#182301,#182302,#182303,#182304,#182305,#182306,#182307,#182308,
#182309,#182310,#182311,#182312,#182313,#182314,#182315,#182316,#182317,
#182318,#182319,#182320,#182321,#182322,#182323,#182324,#182325,#182326,
#182327,#182328,#182329,#182330,#182331,#182332,#182333,#182334,#182335,
#182336,#182337,#182338,#182339,#182340,#182341,#182342,#182343,#182344,
#182345,#182346,#182347,#182348,#182349,#182350,#182351,#182352,#182353,
#182354,#182355,#182356,#182357,#182358,#182359,#182360,#182361,#182362,
#182363,#182364,#182365,#182366,#182367,#182368,#182369,#182370,#182371,
#182372,#182373,#182374,#182375,#182376,#182377,#182378,#182379,#182380,
#182381,#182382,#182383,#182384,#182385,#182386,#182387,#182388,#182389,
#182390,#182391,#182392,#182393,#182394,#182395,#182396,#182397,#182398,
#182399,#182400,#182401,#182402,#182403,#182404,#182405,#182406,#182407,
#182408,#182409,#182410,#182411,#182412,#182413,#182414,#182415,#182416,
#182417,#182418,#182419,#182420,#182421,#182422,#182423,#182424,#182425,
#182426,#182427,#182428,#182429,#182430,#182431,#182432,#182433,#182434,
#182435,#182436,#182437,#182438,#182439,#182440,#182441,#182442,#182443,
#182444,#182445,#182446,#182447,#182448,#182449,#182450,#182451,#182452,
#182453,#182454,#182455,#182456,#182457,#182458,#182459,#182460,#182461,
#182462,#182463,#182464,#182465,#182466,#182467,#182468,#182469,#182470,
#182471,#182472,#182473,#182474,#182475,#182476,#182477,#182478,#182479,
#182480,#182481,#182482,#182483,#182484,#182485,#182486,#182487,#182488,
#182489,#182490,#182491,#182492,#182493,#182494,#182495,#182496,#182497,
#182498,#182499,#182500,#182501,#182502,#182503,#182504,#182505,#182506,
#182507,#182508,#182509,#182510,#182511,#182512,#182513,#182514,#182515,
#182516,#182517,#182518,#182519,#182520,#182521,#182522,#182523,#182524,
#182525,#182526,#182527,#182528,#182529,#182530,#182531,#182532,#182533,
#182534,#182535,#182536,#182537,#182538,#182539,#182540,#182541,#182542,
#182543,#182544,#182545,#182546,#182547,#182548,#182549,#182550,#182551,
#182552,#182553,#182554,#182555,#182556,#182557,#182558,#182559,#182560,
#182561,#182562,#182563,#182564,#182565,#182566,#182567,#182568,#182569,
#182570,#182571,#182572,#182573,#182574,#182575,#182576,#182577,#182578,
#182579,#182580,#182581,#182582,#182583,#182584,#182585,#182586,#182587,
#182588,#182589,#182590,#182591,#182592,#182593,#182594,#182595,#182596,
#182597,#182598,#182599,#182600,#182601,#182602,#182603,#182604,#182605,
#182606,#182607,#182608,#182609,#182610,#182611,#182612,#182613,#182614,
#182615,#182616,#182617,#182618,#182619,#182620,#182621,#182622,#182623,
#182624,#182625,#182626,#182627,#182628,#182629,#182630,#182631,#182632,
#182633,#182634,#182635,#182636,#182637,#182638,#182639,#182640,#182641,
#182642,#182643,#182644,#182645,#182646,#182647,#182648,#182649,#182650,
#182651,#182652,#182653,#182654,#182655,#182656,#182657,#182658,#182659,
#182660,#182661,#182662,#182663,#182664,#182665,#182666,#182667,#182668,
#182669,#182670,#182671,#182672,#182673,#182674,#182675,#182676,#182677,
#182678,#182679,#182680,#182681,#182682,#182683,#182684,#182685,#182686,
#182687,#182688,#182689,#182690,#182691,#182692,#182693,#182694,#182695,
#182696,#182697,#182698,#182699,#182700,#182701,#182702,#182703,#182704,
#182705,#182706,#182707,#182708,#182709,#182710,#182711,#182712,#182713,
#182714,#182715,#182716,#182717,#182718,#182719,#182720,#182721,#182722,
#182723,#182724,#182725,#182726,#182727,#182728,#182729,#182730,#182731,
#182732,#182733,#182734,#182735,#182736,#182737,#182738,#182739,#182740,
#182741,#182742,#182743,#182744,#182745,#182746,#182747,#182748,#182749,
#182750,#182751,#182752,#182753,#182754,#182755,#182756,#182757,#182758,
#182759,#182760,#182761,#182762,#182763,#182764)),.UNSPECIFIED.,.F.,.F.,
 .F.,(4,4),(4,1,1,1,1,1,1,1,1,1,1,1,1,1,1,1,1,1,1,1,1,1,1,1,1,1,1,1,1,1,
1,1,1,1,1,1,1,1,1,1,1,1,1,1,1,1,1,1,1,1,1,1,1,1,1,1,1,1,1,1,1,1,1,1,1,1,
1,1,1,1,1,1,1,1,1,1,1,1,1,1,1,1,1,1,1,1,1,1,1,1,1,1,1,1,1,1,1,1,1,1,1,1,
1,1,1,1,1,1,1,1,1,1,1,1,1,1,1,1,1,1,1,1,1,1,1,1,1,1,1,1,1,1,1,1,1,1,1,1,
1,1,1,1,1,1,1,1,1,1,1,1,1,1,1,1,1,1,1,1,1,1,1,1,1,1,1,1,1,1,1,1,1,1,1,1,
1,1,1,1,1,1,1,1,1,1,1,1,1,1,1,1,1,1,1,1,1,1,1,1,1,1,1,1,1,1,1,1,1,1,1,1,
1,1,1,1,1,1,1,1,1,1,1,1,1,1,1,1,1,1,1,1,1,1,1,1,1,1,1,1,1,1,1,1,1,1,1,1,
1,1,1,1,1,1,1,1,1,1,1,1,1,1,1,1,1,1,1,1,1,1,1,1,1,1,1,1,1,1,1,1,1,1,1,1,
1,1,1,1,1,1,1,1,1,1,1,1,1,1,1,1,1,1,1,1,1,1,1,1,1,1,1,1,1,1,1,1,1,1,1,1,
1,1,1,1,1,1,1,1,1,1,1,1,1,1,1,1,1,1,1,1,1,1,1,1,1,1,1,1,1,1,1,1,1,1,1,1,
1,1,1,1,1,1,1,1,1,1,1,1,1,1,1,1,1,1,1,1,1,1,1,1,1,1,1,1,1,1,1,1,1,1,1,1,
1,1,1,1,1,1,1,1,1,1,1,1,1,1,1,1,1,1,1,1,1,1,1,1,1,1,1,1,1,1,1,1,1,1,1,1,
1,1,1,1,1,1,1,1,1,1,1,1,1,1,1,1,1,1,1,1,1,1,1,1,1,1,1,1,1,1,1,1,1,1,1,1,
1,1,1,1,1,1,1,1,1,1,1,1,1,1,1,1,1,1,1,1,1,1,1,1,1,1,1,1,1,1,1,1,1,1,1,1,
1,1,1,1,1,1,1,1,1,1,1,1,1,1,1,1,1,1,1,1,1,1,1,1,1,1,1,1,1,1,1,1,1,1,1,1,
1,4),(-0.000902833525214243,0.131480103365952),(11.8547611101884,12.3533763570464,
12.851844900354,13.3503134436615,13.8487819869691,14.3472505302766,14.8457190735842,
15.8426561601993,16.8395932468144,17.338061790122,17.8365303334295,18.3349988767371,
18.8334674200446,19.3319359633522,19.8304045066598,20.3288730499673,20.8273415932749,
21.82427867989,22.3227472231976,22.8212157665051,23.8181528531202,24.3166213964278,
24.8150899397353,25.3135584830429,25.8120270263505,26.310495569658,26.8089641129656,
27.3074326562731,27.8059011995807,28.8028382861958,29.3013068295034,29.7997753728109,
30.796712459426,31.2951810027336,31.7936495460412,32.2921180893487,32.7905866326563,
33.2890551759638,33.7875237192714,34.2859922625789,34.7844608058865,35.7813978925016,
36.2798664358092,36.7783349791167,37.7752720657319,38.2737406090394,38.772209152347,
39.2706776956545,39.7691462389621,40.2676147822696,40.7660833255772,41.2645518688848,
41.7630204121923,42.7599574988074,43.258426042115,43.7568945854225,44.7538316720377,
45.2523002153452,45.7507687586528,46.2492373019603,46.7477058452679,47.2461743885754,
47.744642931883,48.2431114751906,48.7415800184981,49.7385171051132,50.2369856484208,
50.7354541917284,51.7323912783435,52.230859821651,52.7293283649586,53.2277969082661,
53.7262654515737,54.2247339948813,54.7232025381888,55.2216710814964,55.7201396248039,
56.7170767114191,57.2155452547266,57.7140137980342,58.7109508846493,59.2094194279568,
59.7078879712644,60.206356514572,60.7048250578795,61.2032936011871,61.7017621444946,
62.2002306878022,62.6986992311097,63.6956363177249,64.1941048610324,64.69257340434,
65.6895104909551,66.1879790342627,66.6864475775702,67.1849161208778,67.6833846641853,
68.1818532074929,68.6803217508004,69.178790294108,69.6772588374156,70.6741959240307,
71.1726644673382,71.6711330106458,72.6680700972609,73.1665386405685,73.665007183876,
74.1634757271836,74.6619442704911,75.1604128137987,75.6588813571063,76.1573499004138,
76.6558184437214,77.6527555303365,78.151224073644,78.6496926169516,79.6466297035667,
80.1450982468743,80.6435667901818,81.1420353334894,81.6405038767969,82.1389724201045,
82.6374409634121,83.1359095067196,83.6343780500272,84.6313151366423,85.1297836799499,
85.6282522232574,86.6251893098725,87.1236578531801,87.6221263964876,88.1205949397952,
88.6190634831028,89.1175320264103,89.6160005697179,90.1144691130254,90.612937656333,
91.6098747429481,92.1083432862557,92.6068118295632,93.6037489161783,94.1022174594859,
94.6006860027935,95.099154546101,95.5976230894086,96.0960916327161,96.5945601760237,
97.0930287193312,97.5914972626388,98.5884343492539,99.0869028925615,99.585371435869,
100.582308522484,101.080777065792,101.579245609099,102.077714152407,102.576182695714,
103.074651239022,103.573119782329,104.071588325637,104.570056868945,105.56699395556,
106.065462498867,106.563931042175,107.56086812879,108.059336672098,108.557805215405,
109.056273758713,109.55474230202,110.053210845328,110.551679388635,111.050147931943,
111.54861647525,112.545553561866,113.044022105173,113.542490648481,114.539427735096,
115.037896278403,115.536364821711,116.034833365018,116.533301908326,117.031770451634,
117.530238994941,118.028707538249,118.527176081556,119.524113168171,120.022581711479,
120.521050254786,121.517987341402,122.016455884709,122.514924428017,123.013392971324,
123.511861514632,124.010330057939,124.508798601247,125.007267144555,125.505735687862,
126.502672774477,127.001141317785,127.499609861092,128.496546947707,128.995015491015,
129.493484034323,129.99195257763,130.490421120938,130.988889664245,131.487358207553,
131.98582675086,132.484295294168,133.481232380783,133.979700924091,134.478169467398,
135.475106554013,135.973575097321,136.472043640628,136.970512183936,137.468980727243,
137.967449270551,138.465917813859,138.964386357166,139.462854900474,140.459791987089,
140.958260530396,141.456729073704,142.453666160319,142.952134703627,143.450603246934,
143.949071790242,144.447540333549,144.946008876857,145.444477420164,145.942945963472,
146.441414506779,147.438351593395,147.936820136702,148.43528868001,149.432225766625,
149.930694309932,150.42916285324,150.927631396547,151.426099939855,151.924568483163,
152.42303702647,152.921505569778,153.419974113085,154.4169111997,154.915379743008,
155.413848286316,156.410785372931,156.909253916238,157.407722459546,157.906191002853,
158.404659546161,158.903128089468,159.401596632776,159.900065176084,160.398533719391,
161.395470806006,161.893939349314,162.392407892621,163.389344979236,163.887813522544,
164.386282065852,164.884750609159,165.383219152467,165.881687695774,166.380156239082,
167.377093325697,168.374030412312,169.370967498927,169.869436042235,170.367904585542,
170.86637312885,171.364841672157,172.361778758772,173.358715845388,174.355652932003,
174.85412147531,175.352590018618,176.349527105233,176.847995648541,177.346464191848,
177.844932735156,178.343401278463,178.841869821771,179.340338365078,179.838806908386,
180.337275451693,181.334212538309,181.832681081616,182.331149624924,183.328086711539,
183.826555254846,184.325023798154,184.823492341461,185.321960884769,185.820429428077,
186.318897971384,186.817366514692,187.315835057999,188.312772144614,188.811240687922,
189.309709231229,190.306646317845,190.805114861152,191.30358340446,191.802051947767,
192.300520491075,192.798989034382,193.29745757769,193.795926120997,194.294394664305,
195.29133175092,195.789800294228,196.288268837535,197.28520592415,197.783674467458,
198.282143010766,198.780611554073,199.279080097381,199.777548640688,200.276017183996,
200.774485727303,201.272954270611,202.269891357226,202.768359900534,203.266828443841,
204.263765530456,204.762234073764,205.260702617071,205.759171160379,206.257639703686,
206.756108246994,207.254576790302,207.753045333609,208.251513876917,209.248450963532,
209.746919506839,210.245388050147,211.242325136762,211.74079368007,212.239262223377,
212.737730766685,213.236199309992,213.7346678533,214.233136396607,214.731604939915,
215.230073483222,216.227010569838,216.725479113145,217.223947656453,218.220884743068,
218.719353286375,219.217821829683,219.71629037299,220.214758916298,220.713227459606,
221.211696002913,221.710164546221,222.208633089528,223.205570176143,223.704038719451,
224.202507262759,225.199444349374,225.697912892681,226.196381435989,226.694849979296,
227.193318522604,227.691787065911,228.190255609219,228.688724152527,229.187192695834,
230.184129782449,230.682598325757,231.181066869064,232.178003955679,232.676472498987,
233.174941042295,233.673409585602,234.17187812891,234.670346672217,235.168815215525,
235.667283758832,236.16575230214,237.162689388755,237.661157932063,238.15962647537,
239.156563561985,239.655032105293,240.1535006486,240.651969191908,241.150437735215,
241.648906278523,242.147374821831,242.645843365138,243.144311908446,244.141248995061,
244.639717538368,245.138186081676,246.135123168291,246.633591711599,247.132060254906,
247.630528798214,248.128997341521,248.627465884829,249.125934428136,249.624402971444,
250.122871514752,251.119808601367,251.618277144674,252.116745687982,253.113682774597,
253.612151317904,254.110619861212,254.60908840452,255.107556947827,255.606025491135,
256.104494034442,256.60296257775,257.101431121057,258.098368207672,258.59683675098,
259.095305294288,260.092242380903,260.59071092421,261.089179467518,261.587648010825,
262.086116554133,262.58458509744,263.083053640748,263.581522184056,264.079990727363,
265.076927813978,265.575396357286,266.073864900593,267.070801987209,267.569270530516,
268.067739073824,268.566207617131,269.064676160439,269.563144703746,270.061613247054,
270.560081790361,271.058550333669,272.055487420284,272.553955963592,273.052424506899,
274.049361593514,274.547830136822,275.046298680129,275.544767223437,276.043235766745,
276.541704310052,277.04017285336,277.538641396667,278.037109939975,279.03404702659,
279.532515569897,280.030984113205,281.02792119982,281.526389743128,282.024858286435,
282.523326829743,283.02179537305,283.520263916358,284.018732459666,284.517201002973,
285.015669546281,286.012606632896,286.511075176203,287.009543719511,288.006480806126,
288.504949349434,289.003417892741,289.501886436049,290.000354979356,290.498823522664,
290.997292065971,291.495760609279,291.994229152586,292.991166239202,293.489634782509,
293.988103325817,294.985040412432,295.483508955739,295.981977499047,296.480446042354,
296.978914585662,297.47738312897,297.975851672277,298.474320215585,298.972788758892,
299.969725845507,300.468194388815,300.966662932122,301.963600018738,302.462068562045,
302.960537105353,303.45900564866,303.957474191968,304.455942735275,304.954411278583,
305.452879821891,305.951348365198,306.948285451813,307.446753995121,307.945222538428,
308.942159625043,309.440628168351,309.939096711659,310.437565254966,310.936033798274,
311.434502341581,311.932970884889,312.431439428196,312.929907971504,313.926845058119,
314.425313601427,314.923782144734,315.920719231349,316.419187774657,316.917656317964,
317.416124861272,317.914593404579,318.413061947887,318.911530491195,319.409999034502,
319.90846757781,320.905404664425,321.90234175104,322.400810294347,322.899278837655,
323.397747380963,323.89621592427,324.394684467578,324.893207835215),
 .UNSPECIFIED.);
#294=B_SPLINE_SURFACE_WITH_KNOTS('',3,3,((#182877,#182878,#182879,#182880,
#182881,#182882,#182883,#182884,#182885,#182886,#182887,#182888,#182889,
#182890,#182891,#182892,#182893,#182894,#182895,#182896,#182897,#182898,
#182899,#182900,#182901,#182902,#182903,#182904,#182905,#182906,#182907,
#182908,#182909,#182910,#182911,#182912,#182913,#182914,#182915,#182916,
#182917,#182918,#182919,#182920,#182921,#182922,#182923,#182924,#182925,
#182926,#182927,#182928,#182929,#182930,#182931,#182932,#182933,#182934,
#182935,#182936,#182937,#182938,#182939,#182940,#182941,#182942,#182943,
#182944,#182945,#182946,#182947,#182948,#182949,#182950,#182951,#182952,
#182953,#182954,#182955,#182956,#182957,#182958,#182959,#182960,#182961,
#182962,#182963,#182964,#182965,#182966,#182967,#182968,#182969,#182970,
#182971,#182972,#182973,#182974,#182975,#182976,#182977,#182978,#182979,
#182980,#182981,#182982,#182983,#182984,#182985,#182986,#182987,#182988,
#182989,#182990,#182991,#182992,#182993,#182994,#182995,#182996,#182997,
#182998,#182999,#183000,#183001,#183002,#183003,#183004,#183005,#183006,
#183007,#183008,#183009,#183010,#183011,#183012,#183013,#183014,#183015,
#183016,#183017,#183018,#183019,#183020,#183021,#183022,#183023,#183024,
#183025,#183026,#183027,#183028,#183029,#183030,#183031,#183032,#183033,
#183034,#183035,#183036,#183037,#183038,#183039,#183040,#183041,#183042,
#183043,#183044,#183045,#183046,#183047,#183048,#183049,#183050,#183051,
#183052,#183053,#183054,#183055,#183056,#183057,#183058,#183059,#183060,
#183061,#183062,#183063,#183064,#183065,#183066,#183067,#183068,#183069,
#183070,#183071,#183072,#183073,#183074,#183075,#183076,#183077,#183078,
#183079,#183080,#183081,#183082,#183083,#183084,#183085,#183086,#183087,
#183088,#183089,#183090,#183091,#183092,#183093,#183094,#183095,#183096,
#183097,#183098,#183099,#183100,#183101,#183102,#183103,#183104,#183105,
#183106,#183107,#183108,#183109,#183110,#183111,#183112,#183113,#183114,
#183115,#183116,#183117,#183118,#183119,#183120,#183121,#183122,#183123,
#183124,#183125,#183126,#183127,#183128,#183129,#183130,#183131,#183132,
#183133,#183134,#183135,#183136,#183137,#183138,#183139,#183140,#183141,
#183142,#183143,#183144,#183145,#183146,#183147,#183148,#183149,#183150,
#183151,#183152,#183153,#183154,#183155,#183156,#183157,#183158,#183159,
#183160,#183161,#183162,#183163,#183164,#183165,#183166,#183167,#183168,
#183169,#183170,#183171,#183172,#183173,#183174,#183175,#183176,#183177,
#183178,#183179,#183180,#183181,#183182,#183183,#183184,#183185,#183186,
#183187,#183188,#183189,#183190,#183191,#183192,#183193,#183194,#183195,
#183196,#183197,#183198,#183199,#183200,#183201,#183202,#183203,#183204,
#183205,#183206,#183207,#183208,#183209,#183210,#183211,#183212,#183213,
#183214,#183215,#183216,#183217,#183218,#183219,#183220,#183221,#183222,
#183223,#183224,#183225,#183226,#183227,#183228,#183229,#183230,#183231,
#183232,#183233,#183234,#183235,#183236,#183237,#183238,#183239,#183240,
#183241,#183242,#183243,#183244,#183245,#183246,#183247,#183248,#183249,
#183250,#183251,#183252,#183253,#183254,#183255,#183256,#183257,#183258,
#183259,#183260,#183261,#183262,#183263,#183264,#183265,#183266,#183267,
#183268,#183269,#183270,#183271,#183272,#183273,#183274,#183275,#183276,
#183277,#183278,#183279,#183280,#183281,#183282,#183283,#183284,#183285,
#183286,#183287,#183288,#183289,#183290,#183291,#183292,#183293,#183294,
#183295,#183296,#183297,#183298,#183299,#183300,#183301,#183302,#183303,
#183304,#183305,#183306,#183307,#183308,#183309,#183310,#183311,#183312,
#183313,#183314,#183315,#183316,#183317,#183318,#183319,#183320,#183321,
#183322,#183323,#183324,#183325,#183326,#183327,#183328,#183329,#183330,
#183331,#183332,#183333,#183334,#183335,#183336,#183337,#183338,#183339,
#183340,#183341,#183342,#183343,#183344,#183345,#183346,#183347,#183348,
#183349,#183350,#183351,#183352,#183353,#183354,#183355,#183356,#183357,
#183358,#183359,#183360,#183361,#183362,#183363,#183364,#183365,#183366,
#183367,#183368,#183369,#183370,#183371,#183372,#183373,#183374,#183375,
#183376,#183377,#183378,#183379,#183380,#183381,#183382,#183383,#183384,
#183385,#183386,#183387,#183388,#183389,#183390,#183391,#183392,#183393,
#183394,#183395,#183396,#183397,#183398,#183399,#183400,#183401,#183402,
#183403,#183404,#183405,#183406,#183407,#183408,#183409,#183410,#183411,
#183412,#183413,#183414),(#183415,#183416,#183417,#183418,#183419,#183420,
#183421,#183422,#183423,#183424,#183425,#183426,#183427,#183428,#183429,
#183430,#183431,#183432,#183433,#183434,#183435,#183436,#183437,#183438,
#183439,#183440,#183441,#183442,#183443,#183444,#183445,#183446,#183447,
#183448,#183449,#183450,#183451,#183452,#183453,#183454,#183455,#183456,
#183457,#183458,#183459,#183460,#183461,#183462,#183463,#183464,#183465,
#183466,#183467,#183468,#183469,#183470,#183471,#183472,#183473,#183474,
#183475,#183476,#183477,#183478,#183479,#183480,#183481,#183482,#183483,
#183484,#183485,#183486,#183487,#183488,#183489,#183490,#183491,#183492,
#183493,#183494,#183495,#183496,#183497,#183498,#183499,#183500,#183501,
#183502,#183503,#183504,#183505,#183506,#183507,#183508,#183509,#183510,
#183511,#183512,#183513,#183514,#183515,#183516,#183517,#183518,#183519,
#183520,#183521,#183522,#183523,#183524,#183525,#183526,#183527,#183528,
#183529,#183530,#183531,#183532,#183533,#183534,#183535,#183536,#183537,
#183538,#183539,#183540,#183541,#183542,#183543,#183544,#183545,#183546,
#183547,#183548,#183549,#183550,#183551,#183552,#183553,#183554,#183555,
#183556,#183557,#183558,#183559,#183560,#183561,#183562,#183563,#183564,
#183565,#183566,#183567,#183568,#183569,#183570,#183571,#183572,#183573,
#183574,#183575,#183576,#183577,#183578,#183579,#183580,#183581,#183582,
#183583,#183584,#183585,#183586,#183587,#183588,#183589,#183590,#183591,
#183592,#183593,#183594,#183595,#183596,#183597,#183598,#183599,#183600,
#183601,#183602,#183603,#183604,#183605,#183606,#183607,#183608,#183609,
#183610,#183611,#183612,#183613,#183614,#183615,#183616,#183617,#183618,
#183619,#183620,#183621,#183622,#183623,#183624,#183625,#183626,#183627,
#183628,#183629,#183630,#183631,#183632,#183633,#183634,#183635,#183636,
#183637,#183638,#183639,#183640,#183641,#183642,#183643,#183644,#183645,
#183646,#183647,#183648,#183649,#183650,#183651,#183652,#183653,#183654,
#183655,#183656,#183657,#183658,#183659,#183660,#183661,#183662,#183663,
#183664,#183665,#183666,#183667,#183668,#183669,#183670,#183671,#183672,
#183673,#183674,#183675,#183676,#183677,#183678,#183679,#183680,#183681,
#183682,#183683,#183684,#183685,#183686,#183687,#183688,#183689,#183690,
#183691,#183692,#183693,#183694,#183695,#183696,#183697,#183698,#183699,
#183700,#183701,#183702,#183703,#183704,#183705,#183706,#183707,#183708,
#183709,#183710,#183711,#183712,#183713,#183714,#183715,#183716,#183717,
#183718,#183719,#183720,#183721,#183722,#183723,#183724,#183725,#183726,
#183727,#183728,#183729,#183730,#183731,#183732,#183733,#183734,#183735,
#183736,#183737,#183738,#183739,#183740,#183741,#183742,#183743,#183744,
#183745,#183746,#183747,#183748,#183749,#183750,#183751,#183752,#183753,
#183754,#183755,#183756,#183757,#183758,#183759,#183760,#183761,#183762,
#183763,#183764,#183765,#183766,#183767,#183768,#183769,#183770,#183771,
#183772,#183773,#183774,#183775,#183776,#183777,#183778,#183779,#183780,
#183781,#183782,#183783,#183784,#183785,#183786,#183787,#183788,#183789,
#183790,#183791,#183792,#183793,#183794,#183795,#183796,#183797,#183798,
#183799,#183800,#183801,#183802,#183803,#183804,#183805,#183806,#183807,
#183808,#183809,#183810,#183811,#183812,#183813,#183814,#183815,#183816,
#183817,#183818,#183819,#183820,#183821,#183822,#183823,#183824,#183825,
#183826,#183827,#183828,#183829,#183830,#183831,#183832,#183833,#183834,
#183835,#183836,#183837,#183838,#183839,#183840,#183841,#183842,#183843,
#183844,#183845,#183846,#183847,#183848,#183849,#183850,#183851,#183852,
#183853,#183854,#183855,#183856,#183857,#183858,#183859,#183860,#183861,
#183862,#183863,#183864,#183865,#183866,#183867,#183868,#183869,#183870,
#183871,#183872,#183873,#183874,#183875,#183876,#183877,#183878,#183879,
#183880,#183881,#183882,#183883,#183884,#183885,#183886,#183887,#183888,
#183889,#183890,#183891,#183892,#183893,#183894,#183895,#183896,#183897,
#183898,#183899,#183900,#183901,#183902,#183903,#183904,#183905,#183906,
#183907,#183908,#183909,#183910,#183911,#183912,#183913,#183914,#183915,
#183916,#183917,#183918,#183919,#183920,#183921,#183922,#183923,#183924,
#183925,#183926,#183927,#183928,#183929,#183930,#183931,#183932,#183933,
#183934,#183935,#183936,#183937,#183938,#183939,#183940,#183941,#183942,
#183943,#183944,#183945,#183946,#183947,#183948,#183949,#183950,#183951,
#183952),(#183953,#183954,#183955,#183956,#183957,#183958,#183959,#183960,
#183961,#183962,#183963,#183964,#183965,#183966,#183967,#183968,#183969,
#183970,#183971,#183972,#183973,#183974,#183975,#183976,#183977,#183978,
#183979,#183980,#183981,#183982,#183983,#183984,#183985,#183986,#183987,
#183988,#183989,#183990,#183991,#183992,#183993,#183994,#183995,#183996,
#183997,#183998,#183999,#184000,#184001,#184002,#184003,#184004,#184005,
#184006,#184007,#184008,#184009,#184010,#184011,#184012,#184013,#184014,
#184015,#184016,#184017,#184018,#184019,#184020,#184021,#184022,#184023,
#184024,#184025,#184026,#184027,#184028,#184029,#184030,#184031,#184032,
#184033,#184034,#184035,#184036,#184037,#184038,#184039,#184040,#184041,
#184042,#184043,#184044,#184045,#184046,#184047,#184048,#184049,#184050,
#184051,#184052,#184053,#184054,#184055,#184056,#184057,#184058,#184059,
#184060,#184061,#184062,#184063,#184064,#184065,#184066,#184067,#184068,
#184069,#184070,#184071,#184072,#184073,#184074,#184075,#184076,#184077,
#184078,#184079,#184080,#184081,#184082,#184083,#184084,#184085,#184086,
#184087,#184088,#184089,#184090,#184091,#184092,#184093,#184094,#184095,
#184096,#184097,#184098,#184099,#184100,#184101,#184102,#184103,#184104,
#184105,#184106,#184107,#184108,#184109,#184110,#184111,#184112,#184113,
#184114,#184115,#184116,#184117,#184118,#184119,#184120,#184121,#184122,
#184123,#184124,#184125,#184126,#184127,#184128,#184129,#184130,#184131,
#184132,#184133,#184134,#184135,#184136,#184137,#184138,#184139,#184140,
#184141,#184142,#184143,#184144,#184145,#184146,#184147,#184148,#184149,
#184150,#184151,#184152,#184153,#184154,#184155,#184156,#184157,#184158,
#184159,#184160,#184161,#184162,#184163,#184164,#184165,#184166,#184167,
#184168,#184169,#184170,#184171,#184172,#184173,#184174,#184175,#184176,
#184177,#184178,#184179,#184180,#184181,#184182,#184183,#184184,#184185,
#184186,#184187,#184188,#184189,#184190,#184191,#184192,#184193,#184194,
#184195,#184196,#184197,#184198,#184199,#184200,#184201,#184202,#184203,
#184204,#184205,#184206,#184207,#184208,#184209,#184210,#184211,#184212,
#184213,#184214,#184215,#184216,#184217,#184218,#184219,#184220,#184221,
#184222,#184223,#184224,#184225,#184226,#184227,#184228,#184229,#184230,
#184231,#184232,#184233,#184234,#184235,#184236,#184237,#184238,#184239,
#184240,#184241,#184242,#184243,#184244,#184245,#184246,#184247,#184248,
#184249,#184250,#184251,#184252,#184253,#184254,#184255,#184256,#184257,
#184258,#184259,#184260,#184261,#184262,#184263,#184264,#184265,#184266,
#184267,#184268,#184269,#184270,#184271,#184272,#184273,#184274,#184275,
#184276,#184277,#184278,#184279,#184280,#184281,#184282,#184283,#184284,
#184285,#184286,#184287,#184288,#184289,#184290,#184291,#184292,#184293,
#184294,#184295,#184296,#184297,#184298,#184299,#184300,#184301,#184302,
#184303,#184304,#184305,#184306,#184307,#184308,#184309,#184310,#184311,
#184312,#184313,#184314,#184315,#184316,#184317,#184318,#184319,#184320,
#184321,#184322,#184323,#184324,#184325,#184326,#184327,#184328,#184329,
#184330,#184331,#184332,#184333,#184334,#184335,#184336,#184337,#184338,
#184339,#184340,#184341,#184342,#184343,#184344,#184345,#184346,#184347,
#184348,#184349,#184350,#184351,#184352,#184353,#184354,#184355,#184356,
#184357,#184358,#184359,#184360,#184361,#184362,#184363,#184364,#184365,
#184366,#184367,#184368,#184369,#184370,#184371,#184372,#184373,#184374,
#184375,#184376,#184377,#184378,#184379,#184380,#184381,#184382,#184383,
#184384,#184385,#184386,#184387,#184388,#184389,#184390,#184391,#184392,
#184393,#184394,#184395,#184396,#184397,#184398,#184399,#184400,#184401,
#184402,#184403,#184404,#184405,#184406,#184407,#184408,#184409,#184410,
#184411,#184412,#184413,#184414,#184415,#184416,#184417,#184418,#184419,
#184420,#184421,#184422,#184423,#184424,#184425,#184426,#184427,#184428,
#184429,#184430,#184431,#184432,#184433,#184434,#184435,#184436,#184437,
#184438,#184439,#184440,#184441,#184442,#184443,#184444,#184445,#184446,
#184447,#184448,#184449,#184450,#184451,#184452,#184453,#184454,#184455,
#184456,#184457,#184458,#184459,#184460,#184461,#184462,#184463,#184464,
#184465,#184466,#184467,#184468,#184469,#184470,#184471,#184472,#184473,
#184474,#184475,#184476,#184477,#184478,#184479,#184480,#184481,#184482,
#184483,#184484,#184485,#184486,#184487,#184488,#184489,#184490),(#184491,
#184492,#184493,#184494,#184495,#184496,#184497,#184498,#184499,#184500,
#184501,#184502,#184503,#184504,#184505,#184506,#184507,#184508,#184509,
#184510,#184511,#184512,#184513,#184514,#184515,#184516,#184517,#184518,
#184519,#184520,#184521,#184522,#184523,#184524,#184525,#184526,#184527,
#184528,#184529,#184530,#184531,#184532,#184533,#184534,#184535,#184536,
#184537,#184538,#184539,#184540,#184541,#184542,#184543,#184544,#184545,
#184546,#184547,#184548,#184549,#184550,#184551,#184552,#184553,#184554,
#184555,#184556,#184557,#184558,#184559,#184560,#184561,#184562,#184563,
#184564,#184565,#184566,#184567,#184568,#184569,#184570,#184571,#184572,
#184573,#184574,#184575,#184576,#184577,#184578,#184579,#184580,#184581,
#184582,#184583,#184584,#184585,#184586,#184587,#184588,#184589,#184590,
#184591,#184592,#184593,#184594,#184595,#184596,#184597,#184598,#184599,
#184600,#184601,#184602,#184603,#184604,#184605,#184606,#184607,#184608,
#184609,#184610,#184611,#184612,#184613,#184614,#184615,#184616,#184617,
#184618,#184619,#184620,#184621,#184622,#184623,#184624,#184625,#184626,
#184627,#184628,#184629,#184630,#184631,#184632,#184633,#184634,#184635,
#184636,#184637,#184638,#184639,#184640,#184641,#184642,#184643,#184644,
#184645,#184646,#184647,#184648,#184649,#184650,#184651,#184652,#184653,
#184654,#184655,#184656,#184657,#184658,#184659,#184660,#184661,#184662,
#184663,#184664,#184665,#184666,#184667,#184668,#184669,#184670,#184671,
#184672,#184673,#184674,#184675,#184676,#184677,#184678,#184679,#184680,
#184681,#184682,#184683,#184684,#184685,#184686,#184687,#184688,#184689,
#184690,#184691,#184692,#184693,#184694,#184695,#184696,#184697,#184698,
#184699,#184700,#184701,#184702,#184703,#184704,#184705,#184706,#184707,
#184708,#184709,#184710,#184711,#184712,#184713,#184714,#184715,#184716,
#184717,#184718,#184719,#184720,#184721,#184722,#184723,#184724,#184725,
#184726,#184727,#184728,#184729,#184730,#184731,#184732,#184733,#184734,
#184735,#184736,#184737,#184738,#184739,#184740,#184741,#184742,#184743,
#184744,#184745,#184746,#184747,#184748,#184749,#184750,#184751,#184752,
#184753,#184754,#184755,#184756,#184757,#184758,#184759,#184760,#184761,
#184762,#184763,#184764,#184765,#184766,#184767,#184768,#184769,#184770,
#184771,#184772,#184773,#184774,#184775,#184776,#184777,#184778,#184779,
#184780,#184781,#184782,#184783,#184784,#184785,#184786,#184787,#184788,
#184789,#184790,#184791,#184792,#184793,#184794,#184795,#184796,#184797,
#184798,#184799,#184800,#184801,#184802,#184803,#184804,#184805,#184806,
#184807,#184808,#184809,#184810,#184811,#184812,#184813,#184814,#184815,
#184816,#184817,#184818,#184819,#184820,#184821,#184822,#184823,#184824,
#184825,#184826,#184827,#184828,#184829,#184830,#184831,#184832,#184833,
#184834,#184835,#184836,#184837,#184838,#184839,#184840,#184841,#184842,
#184843,#184844,#184845,#184846,#184847,#184848,#184849,#184850,#184851,
#184852,#184853,#184854,#184855,#184856,#184857,#184858,#184859,#184860,
#184861,#184862,#184863,#184864,#184865,#184866,#184867,#184868,#184869,
#184870,#184871,#184872,#184873,#184874,#184875,#184876,#184877,#184878,
#184879,#184880,#184881,#184882,#184883,#184884,#184885,#184886,#184887,
#184888,#184889,#184890,#184891,#184892,#184893,#184894,#184895,#184896,
#184897,#184898,#184899,#184900,#184901,#184902,#184903,#184904,#184905,
#184906,#184907,#184908,#184909,#184910,#184911,#184912,#184913,#184914,
#184915,#184916,#184917,#184918,#184919,#184920,#184921,#184922,#184923,
#184924,#184925,#184926,#184927,#184928,#184929,#184930,#184931,#184932,
#184933,#184934,#184935,#184936,#184937,#184938,#184939,#184940,#184941,
#184942,#184943,#184944,#184945,#184946,#184947,#184948,#184949,#184950,
#184951,#184952,#184953,#184954,#184955,#184956,#184957,#184958,#184959,
#184960,#184961,#184962,#184963,#184964,#184965,#184966,#184967,#184968,
#184969,#184970,#184971,#184972,#184973,#184974,#184975,#184976,#184977,
#184978,#184979,#184980,#184981,#184982,#184983,#184984,#184985,#184986,
#184987,#184988,#184989,#184990,#184991,#184992,#184993,#184994,#184995,
#184996,#184997,#184998,#184999,#185000,#185001,#185002,#185003,#185004,
#185005,#185006,#185007,#185008,#185009,#185010,#185011,#185012,#185013,
#185014,#185015,#185016,#185017,#185018,#185019,#185020,#185021,#185022,
#185023,#185024,#185025,#185026,#185027,#185028)),.UNSPECIFIED.,.F.,.F.,
 .F.,(4,4),(4,1,1,1,1,1,1,1,1,1,1,1,1,1,1,1,1,1,1,1,1,1,1,1,1,1,1,1,1,1,
1,1,1,1,1,1,1,1,1,1,1,1,1,1,1,1,1,1,1,1,1,1,1,1,1,1,1,1,1,1,1,1,1,1,1,1,
1,1,1,1,1,1,1,1,1,1,1,1,1,1,1,1,1,1,1,1,1,1,1,1,1,1,1,1,1,1,1,1,1,1,1,1,
1,1,1,1,1,1,1,1,1,1,1,1,1,1,1,1,1,1,1,1,1,1,1,1,1,1,1,1,1,1,1,1,1,1,1,1,
1,1,1,1,1,1,1,1,1,1,1,1,1,1,1,1,1,1,1,1,1,1,1,1,1,1,1,1,1,1,1,1,1,1,1,1,
1,1,1,1,1,1,1,1,1,1,1,1,1,1,1,1,1,1,1,1,1,1,1,1,1,1,1,1,1,1,1,1,1,1,1,1,
1,1,1,1,1,1,1,1,1,1,1,1,1,1,1,1,1,1,1,1,1,1,1,1,1,1,1,1,1,1,1,1,1,1,1,1,
1,1,1,1,1,1,1,1,1,1,1,1,1,1,1,1,1,1,1,1,1,1,1,1,1,1,1,1,1,1,1,1,1,1,1,1,
1,1,1,1,1,1,1,1,1,1,1,1,1,1,1,1,1,1,1,1,1,1,1,1,1,1,1,1,1,1,1,1,1,1,1,1,
1,1,1,1,1,1,1,1,1,1,1,1,1,1,1,1,1,1,1,1,1,1,1,1,1,1,1,1,1,1,1,1,1,1,1,1,
1,1,1,1,1,1,1,1,1,1,1,1,1,1,1,1,1,1,1,1,1,1,1,1,1,1,1,1,1,1,1,1,1,1,1,1,
1,1,1,1,1,1,1,1,1,1,1,1,1,1,1,1,1,1,1,1,1,1,1,1,1,1,1,1,1,1,1,1,1,1,1,1,
1,1,1,1,1,1,1,1,1,1,1,1,1,1,1,1,1,1,1,1,1,1,1,1,1,1,1,1,1,1,1,1,1,1,1,1,
1,1,1,1,1,1,1,1,1,1,1,1,1,1,1,1,1,1,1,1,1,1,1,1,1,1,1,1,1,1,1,1,1,1,1,1,
1,1,1,1,1,1,1,1,1,1,1,1,1,1,1,1,1,1,1,1,1,1,1,1,1,1,1,1,1,1,1,1,1,1,1,1,
1,4),(-0.00284646367232349,0.129536473500696),(14.3987987524829,14.897322120121,
15.3957906634286,15.8942592067361,16.3927277500437,16.8911962933512,17.3896648366588,
18.3866019232739,19.383539009889,19.8820075531966,20.3804760965041,20.8789446398117,
21.3774131831193,21.8758817264268,22.3743502697344,22.8728188130419,23.3712873563495,
24.3682244429646,24.8666929862722,25.3651615295797,26.3620986161948,26.8605671595024,
27.35903570281,27.8575042461175,28.3559727894251,28.8544413327326,29.3529098760402,
29.8513784193477,30.3498469626553,31.3467840492704,31.845252592578,32.3437211358855,
33.3406582225007,33.8391267658082,34.3375953091158,34.8360638524233,35.3345323957309,
35.8330009390384,36.331469482346,36.8299380256536,37.3284065689611,38.3253436555762,
38.8238121988838,39.3222807421914,40.3192178288065,40.817686372114,41.3161549154216,
41.8146234587291,42.3130920020367,42.8115605453443,43.3100290886518,43.8084976319594,
44.3069661752669,45.303903261882,45.8023718051896,46.3008403484972,47.2977774351123,
47.7962459784198,48.2947145217274,48.793183065035,49.2916516083425,49.7901201516501,
50.2885886949576,50.7870572382652,51.2855257815727,52.2824628681879,52.7809314114954,
53.279399954803,54.2763370414181,54.7748055847256,55.2732741280332,55.7717426713408,
56.2702112146483,56.7686797579559,57.2671483012634,57.765616844571,58.2640853878786,
59.2610224744937,59.7594910178012,60.2579595611088,61.2548966477239,61.7533651910315,
62.251833734339,62.7503022776466,63.2487708209541,63.7472393642617,64.2457079075693,
64.7441764508768,65.2426449941844,66.2395820807995,66.738050624107,67.2365191674146,
68.2334562540297,68.7319247973373,69.2303933406448,69.7288618839524,70.22733042726,
70.7257989705675,71.2242675138751,71.7227360571826,72.2212046004902,73.2181416871053,
73.7166102304129,74.2150787737204,75.2120158603355,75.7104844036431,76.2089529469506,
76.7074214902582,77.2058900335658,77.7043585768733,78.2028271201809,78.7012956634885,
79.199764206796,80.1967012934111,80.6951698367187,81.1936383800262,82.1905754666413,
82.6890440099489,83.1875125532565,83.685981096564,84.1844496398716,84.6829181831791,
85.1813867264867,85.6798552697942,86.1783238131018,87.1752608997169,87.6737294430245,
88.1721979863321,89.1691350729472,89.6676036162547,90.1660721595623,90.6645407028698,
91.1630092461774,91.661477789485,92.1599463327925,92.6584148761001,93.1568834194076,
94.1538205060227,94.6522890493303,95.1507575926379,96.147694679253,96.6461632225605,
97.1446317658681,97.6431003091757,98.1415688524832,98.6400373957908,99.1385059390983,
99.6369744824059,100.135443025713,101.132380112329,101.630848655636,102.129317198944,
103.126254285559,103.624722828866,104.123191372174,104.621659915481,105.120128458789,
105.618597002097,106.117065545404,106.615534088712,107.114002632019,108.110939718634,
108.609408261942,109.107876805249,110.104813891865,110.603282435172,111.10175097848,
111.600219521787,112.098688065095,112.597156608402,113.09562515171,113.594093695018,
114.092562238325,115.08949932494,115.587967868248,116.086436411555,117.08337349817,
117.581842041478,118.080310584786,118.578779128093,119.077247671401,119.575716214708,
120.074184758016,120.572653301323,121.071121844631,122.068058931246,122.566527474554,
123.064996017861,124.061933104476,124.560401647784,125.058870191091,125.557338734399,
126.055807277706,126.554275821014,127.052744364322,127.551212907629,128.049681450937,
129.046618537552,129.545087080859,130.043555624167,131.040492710782,131.53896125409,
132.037429797397,132.535898340705,133.034366884012,133.53283542732,134.031303970627,
134.529772513935,135.028241057242,136.025178143858,136.523646687165,137.022115230473,
138.019052317088,138.517520860395,139.015989403703,139.514457947011,140.012926490318,
140.511395033626,141.009863576933,141.508332120241,142.006800663548,143.003737750163,
143.502206293471,144.000674836779,144.997611923394,145.496080466701,145.994549010009,
146.493017553316,146.991486096624,147.489954639931,147.988423183239,148.486891726547,
148.985360269854,149.982297356469,150.480765899777,150.979234443084,151.976171529699,
152.474640073007,152.973108616315,153.471577159622,153.97004570293,154.468514246237,
154.966982789545,155.465451332852,155.96391987616,156.960856962775,157.459325506083,
157.95779404939,158.954731136005,159.453199679313,159.95166822262,160.450136765928,
160.948605309236,161.447073852543,161.945542395851,162.444010939158,162.942479482466,
163.939416569081,164.437885112388,164.936353655696,165.933290742311,166.431759285619,
166.930227828926,167.428696372234,167.927164915541,168.425633458849,168.924102002156,
169.921039088772,170.917976175387,171.914913262002,172.413381805309,172.911850348617,
173.410318891924,173.908787435232,174.905724521847,175.902661608462,176.899598695077,
177.398067238385,177.896535781693,178.893472868308,179.391941411615,179.890409954923,
180.38887849823,180.887347041538,181.385815584845,181.884284128153,182.382752671461,
182.881221214768,183.878158301383,184.376626844691,184.875095387998,185.872032474613,
186.370501017921,186.868969561229,187.367438104536,187.865906647844,188.364375191151,
188.862843734459,189.361312277766,189.859780821074,190.856717907689,191.355186450997,
191.853654994304,192.850592080919,193.349060624227,193.847529167534,194.345997710842,
194.844466254149,195.342934797457,195.841403340765,196.339871884072,196.83834042738,
197.835277513995,198.333746057302,198.83221460061,199.829151687225,200.327620230533,
200.82608877384,201.324557317148,201.823025860455,202.321494403763,202.81996294707,
203.318431490378,203.816900033686,204.813837120301,205.312305663608,205.810774206916,
206.807711293531,207.306179836838,207.804648380146,208.303116923454,208.801585466761,
209.300054010069,209.798522553376,210.296991096684,210.795459639991,211.792396726606,
212.290865269914,212.789333813222,213.786270899837,214.284739443144,214.783207986452,
215.281676529759,215.780145073067,216.278613616374,216.777082159682,217.27555070299,
217.774019246297,218.770956332912,219.26942487622,219.767893419527,220.764830506142,
221.26329904945,221.761767592758,222.260236136065,222.758704679373,223.25717322268,
223.755641765988,224.254110309295,224.752578852603,225.749515939218,226.247984482526,
226.746453025833,227.743390112448,228.241858655756,228.740327199063,229.238795742371,
229.737264285679,230.235732828986,230.734201372294,231.232669915601,231.731138458909,
232.728075545524,233.226544088831,233.725012632139,234.721949718754,235.220418262062,
235.718886805369,236.217355348677,236.715823891984,237.214292435292,237.712760978599,
238.211229521907,238.709698065215,239.70663515183,240.205103695137,240.703572238445,
241.70050932506,242.198977868367,242.697446411675,243.195914954983,243.69438349829,
244.192852041598,244.691320584905,245.189789128213,245.68825767152,246.685194758136,
247.183663301443,247.682131844751,248.679068931366,249.177537474673,249.676006017981,
250.174474561288,250.672943104596,251.171411647904,251.669880191211,252.168348734519,
252.666817277826,253.663754364441,254.162222907749,254.660691451056,255.657628537672,
256.156097080979,256.654565624287,257.153034167594,257.651502710902,258.149971254209,
258.648439797517,259.146908340824,259.645376884132,260.642313970747,261.140782514055,
261.639251057362,262.636188143977,263.134656687285,263.633125230592,264.1315937739,
264.630062317208,265.128530860515,265.626999403823,266.12546794713,266.623936490438,
267.620873577053,268.11934212036,268.617810663668,269.614747750283,270.113216293591,
270.611684836898,271.110153380206,271.608621923513,272.107090466821,272.605559010129,
273.104027553436,273.602496096744,274.599433183359,275.097901726666,275.596370269974,
276.593307356589,277.091775899897,277.590244443204,278.088712986512,278.587181529819,
279.085650073127,279.584118616434,280.082587159742,280.581055703049,281.577992789665,
282.076461332972,282.57492987628,283.571866962895,284.070335506202,284.56880404951,
285.067272592818,285.565741136125,286.064209679433,286.56267822274,287.061146766048,
287.559615309355,288.55655239597,289.055020939278,289.553489482586,290.550426569201,
291.048895112508,291.547363655816,292.045832199123,292.544300742431,293.042769285738,
293.541237829046,294.039706372354,294.538174915661,295.535112002276,296.033580545584,
296.532049088891,297.528986175506,298.027454718814,298.525923262122,299.024391805429,
299.522860348737,300.021328892044,300.519797435352,301.018265978659,301.516734521967,
302.513671608582,303.01214015189,303.510608695197,304.507545781812,305.00601432512,
305.504482868427,306.002951411735,306.501419955042,306.99988849835,307.498357041658,
307.996825584965,308.495294128273,309.492231214888,309.990699758195,310.489168301503,
311.486105388118,311.984573931426,312.483042474733,312.981511018041,313.479979561348,
313.978448104656,314.476916647963,314.975385191271,315.473853734579,316.470790821194,
316.969259364501,317.467727907809,318.464664994424,318.963133537731,319.461602081039,
319.960070624347,320.458539167654,320.957007710962,321.455476254269,321.953944797577,
322.452413340884,323.449350427499,324.446287514115,324.944756057422,325.44322460073,
325.941693144037,326.440161687345,326.938630230652,327.43724547751),
 .UNSPECIFIED.);
#295=B_SPLINE_SURFACE_WITH_KNOTS('',3,3,((#241865,#241866,#241867,#241868,
#241869,#241870,#241871,#241872,#241873,#241874,#241875,#241876,#241877,
#241878,#241879,#241880,#241881,#241882,#241883,#241884,#241885,#241886,
#241887,#241888,#241889,#241890,#241891,#241892,#241893,#241894,#241895,
#241896,#241897,#241898,#241899,#241900,#241901,#241902,#241903,#241904,
#241905,#241906,#241907,#241908,#241909,#241910,#241911,#241912,#241913,
#241914,#241915,#241916,#241917,#241918,#241919,#241920,#241921,#241922,
#241923,#241924,#241925,#241926,#241927,#241928,#241929,#241930,#241931,
#241932,#241933,#241934,#241935,#241936,#241937,#241938,#241939,#241940,
#241941,#241942,#241943,#241944,#241945,#241946,#241947,#241948,#241949,
#241950,#241951,#241952,#241953,#241954,#241955,#241956,#241957,#241958,
#241959,#241960,#241961,#241962,#241963,#241964,#241965,#241966,#241967,
#241968,#241969,#241970,#241971,#241972,#241973,#241974,#241975,#241976,
#241977,#241978,#241979,#241980,#241981,#241982,#241983,#241984,#241985,
#241986,#241987,#241988,#241989,#241990,#241991,#241992,#241993,#241994,
#241995,#241996,#241997,#241998,#241999,#242000,#242001,#242002,#242003,
#242004,#242005,#242006,#242007,#242008,#242009,#242010,#242011,#242012,
#242013,#242014,#242015,#242016,#242017,#242018,#242019,#242020,#242021,
#242022,#242023,#242024,#242025,#242026,#242027,#242028,#242029,#242030,
#242031,#242032,#242033,#242034,#242035,#242036,#242037,#242038,#242039,
#242040,#242041,#242042,#242043,#242044,#242045,#242046,#242047,#242048,
#242049,#242050,#242051,#242052,#242053,#242054,#242055,#242056,#242057,
#242058,#242059,#242060,#242061,#242062,#242063,#242064,#242065,#242066,
#242067,#242068,#242069,#242070,#242071,#242072,#242073,#242074,#242075,
#242076,#242077,#242078,#242079,#242080,#242081,#242082,#242083,#242084,
#242085,#242086,#242087,#242088,#242089,#242090,#242091,#242092,#242093,
#242094,#242095,#242096,#242097,#242098,#242099,#242100,#242101,#242102,
#242103,#242104,#242105,#242106,#242107,#242108,#242109,#242110,#242111,
#242112,#242113,#242114,#242115,#242116,#242117,#242118,#242119,#242120,
#242121,#242122,#242123,#242124,#242125,#242126,#242127,#242128,#242129,
#242130,#242131,#242132,#242133,#242134,#242135,#242136,#242137,#242138,
#242139,#242140,#242141,#242142,#242143,#242144,#242145,#242146,#242147,
#242148,#242149,#242150,#242151,#242152,#242153,#242154,#242155,#242156,
#242157,#242158,#242159,#242160,#242161,#242162,#242163,#242164,#242165,
#242166,#242167,#242168,#242169,#242170,#242171,#242172,#242173,#242174,
#242175,#242176,#242177,#242178,#242179,#242180,#242181,#242182,#242183,
#242184,#242185,#242186,#242187,#242188,#242189,#242190,#242191,#242192,
#242193,#242194,#242195,#242196,#242197,#242198,#242199,#242200,#242201,
#242202,#242203,#242204,#242205,#242206,#242207,#242208,#242209,#242210,
#242211,#242212,#242213,#242214,#242215,#242216,#242217,#242218,#242219,
#242220,#242221,#242222,#242223,#242224,#242225,#242226,#242227,#242228,
#242229,#242230,#242231,#242232,#242233,#242234,#242235,#242236,#242237,
#242238,#242239,#242240,#242241,#242242,#242243,#242244,#242245,#242246,
#242247,#242248,#242249,#242250,#242251,#242252,#242253,#242254,#242255,
#242256,#242257,#242258,#242259,#242260,#242261,#242262,#242263,#242264,
#242265,#242266,#242267,#242268,#242269,#242270,#242271,#242272,#242273,
#242274,#242275,#242276,#242277,#242278,#242279,#242280,#242281,#242282,
#242283,#242284,#242285,#242286,#242287,#242288,#242289,#242290,#242291,
#242292,#242293,#242294,#242295,#242296,#242297,#242298,#242299,#242300,
#242301,#242302,#242303,#242304,#242305,#242306,#242307,#242308,#242309,
#242310,#242311,#242312,#242313,#242314,#242315,#242316,#242317,#242318,
#242319,#242320,#242321,#242322,#242323,#242324,#242325,#242326,#242327,
#242328,#242329,#242330,#242331,#242332,#242333,#242334,#242335,#242336,
#242337,#242338,#242339,#242340,#242341,#242342,#242343,#242344,#242345,
#242346,#242347,#242348,#242349,#242350,#242351,#242352,#242353,#242354,
#242355,#242356,#242357,#242358,#242359,#242360,#242361,#242362,#242363,
#242364,#242365,#242366,#242367,#242368,#242369,#242370,#242371,#242372,
#242373,#242374,#242375,#242376,#242377,#242378,#242379,#242380,#242381,
#242382,#242383,#242384,#242385,#242386,#242387,#242388,#242389,#242390,
#242391,#242392,#242393,#242394,#242395,#242396,#242397,#242398,#242399,
#242400,#242401,#242402,#242403,#242404,#242405,#242406,#242407,#242408,
#242409,#242410,#242411,#242412,#242413,#242414,#242415,#242416,#242417,
#242418,#242419,#242420,#242421,#242422,#242423,#242424,#242425,#242426,
#242427,#242428,#242429,#242430,#242431,#242432,#242433,#242434,#242435,
#242436,#242437,#242438,#242439,#242440,#242441,#242442,#242443,#242444,
#242445,#242446,#242447,#242448,#242449,#242450,#242451,#242452,#242453),
(#242454,#242455,#242456,#242457,#242458,#242459,#242460,#242461,#242462,
#242463,#242464,#242465,#242466,#242467,#242468,#242469,#242470,#242471,
#242472,#242473,#242474,#242475,#242476,#242477,#242478,#242479,#242480,
#242481,#242482,#242483,#242484,#242485,#242486,#242487,#242488,#242489,
#242490,#242491,#242492,#242493,#242494,#242495,#242496,#242497,#242498,
#242499,#242500,#242501,#242502,#242503,#242504,#242505,#242506,#242507,
#242508,#242509,#242510,#242511,#242512,#242513,#242514,#242515,#242516,
#242517,#242518,#242519,#242520,#242521,#242522,#242523,#242524,#242525,
#242526,#242527,#242528,#242529,#242530,#242531,#242532,#242533,#242534,
#242535,#242536,#242537,#242538,#242539,#242540,#242541,#242542,#242543,
#242544,#242545,#242546,#242547,#242548,#242549,#242550,#242551,#242552,
#242553,#242554,#242555,#242556,#242557,#242558,#242559,#242560,#242561,
#242562,#242563,#242564,#242565,#242566,#242567,#242568,#242569,#242570,
#242571,#242572,#242573,#242574,#242575,#242576,#242577,#242578,#242579,
#242580,#242581,#242582,#242583,#242584,#242585,#242586,#242587,#242588,
#242589,#242590,#242591,#242592,#242593,#242594,#242595,#242596,#242597,
#242598,#242599,#242600,#242601,#242602,#242603,#242604,#242605,#242606,
#242607,#242608,#242609,#242610,#242611,#242612,#242613,#242614,#242615,
#242616,#242617,#242618,#242619,#242620,#242621,#242622,#242623,#242624,
#242625,#242626,#242627,#242628,#242629,#242630,#242631,#242632,#242633,
#242634,#242635,#242636,#242637,#242638,#242639,#242640,#242641,#242642,
#242643,#242644,#242645,#242646,#242647,#242648,#242649,#242650,#242651,
#242652,#242653,#242654,#242655,#242656,#242657,#242658,#242659,#242660,
#242661,#242662,#242663,#242664,#242665,#242666,#242667,#242668,#242669,
#242670,#242671,#242672,#242673,#242674,#242675,#242676,#242677,#242678,
#242679,#242680,#242681,#242682,#242683,#242684,#242685,#242686,#242687,
#242688,#242689,#242690,#242691,#242692,#242693,#242694,#242695,#242696,
#242697,#242698,#242699,#242700,#242701,#242702,#242703,#242704,#242705,
#242706,#242707,#242708,#242709,#242710,#242711,#242712,#242713,#242714,
#242715,#242716,#242717,#242718,#242719,#242720,#242721,#242722,#242723,
#242724,#242725,#242726,#242727,#242728,#242729,#242730,#242731,#242732,
#242733,#242734,#242735,#242736,#242737,#242738,#242739,#242740,#242741,
#242742,#242743,#242744,#242745,#242746,#242747,#242748,#242749,#242750,
#242751,#242752,#242753,#242754,#242755,#242756,#242757,#242758,#242759,
#242760,#242761,#242762,#242763,#242764,#242765,#242766,#242767,#242768,
#242769,#242770,#242771,#242772,#242773,#242774,#242775,#242776,#242777,
#242778,#242779,#242780,#242781,#242782,#242783,#242784,#242785,#242786,
#242787,#242788,#242789,#242790,#242791,#242792,#242793,#242794,#242795,
#242796,#242797,#242798,#242799,#242800,#242801,#242802,#242803,#242804,
#242805,#242806,#242807,#242808,#242809,#242810,#242811,#242812,#242813,
#242814,#242815,#242816,#242817,#242818,#242819,#242820,#242821,#242822,
#242823,#242824,#242825,#242826,#242827,#242828,#242829,#242830,#242831,
#242832,#242833,#242834,#242835,#242836,#242837,#242838,#242839,#242840,
#242841,#242842,#242843,#242844,#242845,#242846,#242847,#242848,#242849,
#242850,#242851,#242852,#242853,#242854,#242855,#242856,#242857,#242858,
#242859,#242860,#242861,#242862,#242863,#242864,#242865,#242866,#242867,
#242868,#242869,#242870,#242871,#242872,#242873,#242874,#242875,#242876,
#242877,#242878,#242879,#242880,#242881,#242882,#242883,#242884,#242885,
#242886,#242887,#242888,#242889,#242890,#242891,#242892,#242893,#242894,
#242895,#242896,#242897,#242898,#242899,#242900,#242901,#242902,#242903,
#242904,#242905,#242906,#242907,#242908,#242909,#242910,#242911,#242912,
#242913,#242914,#242915,#242916,#242917,#242918,#242919,#242920,#242921,
#242922,#242923,#242924,#242925,#242926,#242927,#242928,#242929,#242930,
#242931,#242932,#242933,#242934,#242935,#242936,#242937,#242938,#242939,
#242940,#242941,#242942,#242943,#242944,#242945,#242946,#242947,#242948,
#242949,#242950,#242951,#242952,#242953,#242954,#242955,#242956,#242957,
#242958,#242959,#242960,#242961,#242962,#242963,#242964,#242965,#242966,
#242967,#242968,#242969,#242970,#242971,#242972,#242973,#242974,#242975,
#242976,#242977,#242978,#242979,#242980,#242981,#242982,#242983,#242984,
#242985,#242986,#242987,#242988,#242989,#242990,#242991,#242992,#242993,
#242994,#242995,#242996,#242997,#242998,#242999,#243000,#243001,#243002,
#243003,#243004,#243005,#243006,#243007,#243008,#243009,#243010,#243011,
#243012,#243013,#243014,#243015,#243016,#243017,#243018,#243019,#243020,
#243021,#243022,#243023,#243024,#243025,#243026,#243027,#243028,#243029,
#243030,#243031,#243032,#243033,#243034,#243035,#243036,#243037,#243038,
#243039,#243040,#243041,#243042),(#243043,#243044,#243045,#243046,#243047,
#243048,#243049,#243050,#243051,#243052,#243053,#243054,#243055,#243056,
#243057,#243058,#243059,#243060,#243061,#243062,#243063,#243064,#243065,
#243066,#243067,#243068,#243069,#243070,#243071,#243072,#243073,#243074,
#243075,#243076,#243077,#243078,#243079,#243080,#243081,#243082,#243083,
#243084,#243085,#243086,#243087,#243088,#243089,#243090,#243091,#243092,
#243093,#243094,#243095,#243096,#243097,#243098,#243099,#243100,#243101,
#243102,#243103,#243104,#243105,#243106,#243107,#243108,#243109,#243110,
#243111,#243112,#243113,#243114,#243115,#243116,#243117,#243118,#243119,
#243120,#243121,#243122,#243123,#243124,#243125,#243126,#243127,#243128,
#243129,#243130,#243131,#243132,#243133,#243134,#243135,#243136,#243137,
#243138,#243139,#243140,#243141,#243142,#243143,#243144,#243145,#243146,
#243147,#243148,#243149,#243150,#243151,#243152,#243153,#243154,#243155,
#243156,#243157,#243158,#243159,#243160,#243161,#243162,#243163,#243164,
#243165,#243166,#243167,#243168,#243169,#243170,#243171,#243172,#243173,
#243174,#243175,#243176,#243177,#243178,#243179,#243180,#243181,#243182,
#243183,#243184,#243185,#243186,#243187,#243188,#243189,#243190,#243191,
#243192,#243193,#243194,#243195,#243196,#243197,#243198,#243199,#243200,
#243201,#243202,#243203,#243204,#243205,#243206,#243207,#243208,#243209,
#243210,#243211,#243212,#243213,#243214,#243215,#243216,#243217,#243218,
#243219,#243220,#243221,#243222,#243223,#243224,#243225,#243226,#243227,
#243228,#243229,#243230,#243231,#243232,#243233,#243234,#243235,#243236,
#243237,#243238,#243239,#243240,#243241,#243242,#243243,#243244,#243245,
#243246,#243247,#243248,#243249,#243250,#243251,#243252,#243253,#243254,
#243255,#243256,#243257,#243258,#243259,#243260,#243261,#243262,#243263,
#243264,#243265,#243266,#243267,#243268,#243269,#243270,#243271,#243272,
#243273,#243274,#243275,#243276,#243277,#243278,#243279,#243280,#243281,
#243282,#243283,#243284,#243285,#243286,#243287,#243288,#243289,#243290,
#243291,#243292,#243293,#243294,#243295,#243296,#243297,#243298,#243299,
#243300,#243301,#243302,#243303,#243304,#243305,#243306,#243307,#243308,
#243309,#243310,#243311,#243312,#243313,#243314,#243315,#243316,#243317,
#243318,#243319,#243320,#243321,#243322,#243323,#243324,#243325,#243326,
#243327,#243328,#243329,#243330,#243331,#243332,#243333,#243334,#243335,
#243336,#243337,#243338,#243339,#243340,#243341,#243342,#243343,#243344,
#243345,#243346,#243347,#243348,#243349,#243350,#243351,#243352,#243353,
#243354,#243355,#243356,#243357,#243358,#243359,#243360,#243361,#243362,
#243363,#243364,#243365,#243366,#243367,#243368,#243369,#243370,#243371,
#243372,#243373,#243374,#243375,#243376,#243377,#243378,#243379,#243380,
#243381,#243382,#243383,#243384,#243385,#243386,#243387,#243388,#243389,
#243390,#243391,#243392,#243393,#243394,#243395,#243396,#243397,#243398,
#243399,#243400,#243401,#243402,#243403,#243404,#243405,#243406,#243407,
#243408,#243409,#243410,#243411,#243412,#243413,#243414,#243415,#243416,
#243417,#243418,#243419,#243420,#243421,#243422,#243423,#243424,#243425,
#243426,#243427,#243428,#243429,#243430,#243431,#243432,#243433,#243434,
#243435,#243436,#243437,#243438,#243439,#243440,#243441,#243442,#243443,
#243444,#243445,#243446,#243447,#243448,#243449,#243450,#243451,#243452,
#243453,#243454,#243455,#243456,#243457,#243458,#243459,#243460,#243461,
#243462,#243463,#243464,#243465,#243466,#243467,#243468,#243469,#243470,
#243471,#243472,#243473,#243474,#243475,#243476,#243477,#243478,#243479,
#243480,#243481,#243482,#243483,#243484,#243485,#243486,#243487,#243488,
#243489,#243490,#243491,#243492,#243493,#243494,#243495,#243496,#243497,
#243498,#243499,#243500,#243501,#243502,#243503,#243504,#243505,#243506,
#243507,#243508,#243509,#243510,#243511,#243512,#243513,#243514,#243515,
#243516,#243517,#243518,#243519,#243520,#243521,#243522,#243523,#243524,
#243525,#243526,#243527,#243528,#243529,#243530,#243531,#243532,#243533,
#243534,#243535,#243536,#243537,#243538,#243539,#243540,#243541,#243542,
#243543,#243544,#243545,#243546,#243547,#243548,#243549,#243550,#243551,
#243552,#243553,#243554,#243555,#243556,#243557,#243558,#243559,#243560,
#243561,#243562,#243563,#243564,#243565,#243566,#243567,#243568,#243569,
#243570,#243571,#243572,#243573,#243574,#243575,#243576,#243577,#243578,
#243579,#243580,#243581,#243582,#243583,#243584,#243585,#243586,#243587,
#243588,#243589,#243590,#243591,#243592,#243593,#243594,#243595,#243596,
#243597,#243598,#243599,#243600,#243601,#243602,#243603,#243604,#243605,
#243606,#243607,#243608,#243609,#243610,#243611,#243612,#243613,#243614,
#243615,#243616,#243617,#243618,#243619,#243620,#243621,#243622,#243623,
#243624,#243625,#243626,#243627,#243628,#243629,#243630,#243631),(#243632,
#243633,#243634,#243635,#243636,#243637,#243638,#243639,#243640,#243641,
#243642,#243643,#243644,#243645,#243646,#243647,#243648,#243649,#243650,
#243651,#243652,#243653,#243654,#243655,#243656,#243657,#243658,#243659,
#243660,#243661,#243662,#243663,#243664,#243665,#243666,#243667,#243668,
#243669,#243670,#243671,#243672,#243673,#243674,#243675,#243676,#243677,
#243678,#243679,#243680,#243681,#243682,#243683,#243684,#243685,#243686,
#243687,#243688,#243689,#243690,#243691,#243692,#243693,#243694,#243695,
#243696,#243697,#243698,#243699,#243700,#243701,#243702,#243703,#243704,
#243705,#243706,#243707,#243708,#243709,#243710,#243711,#243712,#243713,
#243714,#243715,#243716,#243717,#243718,#243719,#243720,#243721,#243722,
#243723,#243724,#243725,#243726,#243727,#243728,#243729,#243730,#243731,
#243732,#243733,#243734,#243735,#243736,#243737,#243738,#243739,#243740,
#243741,#243742,#243743,#243744,#243745,#243746,#243747,#243748,#243749,
#243750,#243751,#243752,#243753,#243754,#243755,#243756,#243757,#243758,
#243759,#243760,#243761,#243762,#243763,#243764,#243765,#243766,#243767,
#243768,#243769,#243770,#243771,#243772,#243773,#243774,#243775,#243776,
#243777,#243778,#243779,#243780,#243781,#243782,#243783,#243784,#243785,
#243786,#243787,#243788,#243789,#243790,#243791,#243792,#243793,#243794,
#243795,#243796,#243797,#243798,#243799,#243800,#243801,#243802,#243803,
#243804,#243805,#243806,#243807,#243808,#243809,#243810,#243811,#243812,
#243813,#243814,#243815,#243816,#243817,#243818,#243819,#243820,#243821,
#243822,#243823,#243824,#243825,#243826,#243827,#243828,#243829,#243830,
#243831,#243832,#243833,#243834,#243835,#243836,#243837,#243838,#243839,
#243840,#243841,#243842,#243843,#243844,#243845,#243846,#243847,#243848,
#243849,#243850,#243851,#243852,#243853,#243854,#243855,#243856,#243857,
#243858,#243859,#243860,#243861,#243862,#243863,#243864,#243865,#243866,
#243867,#243868,#243869,#243870,#243871,#243872,#243873,#243874,#243875,
#243876,#243877,#243878,#243879,#243880,#243881,#243882,#243883,#243884,
#243885,#243886,#243887,#243888,#243889,#243890,#243891,#243892,#243893,
#243894,#243895,#243896,#243897,#243898,#243899,#243900,#243901,#243902,
#243903,#243904,#243905,#243906,#243907,#243908,#243909,#243910,#243911,
#243912,#243913,#243914,#243915,#243916,#243917,#243918,#243919,#243920,
#243921,#243922,#243923,#243924,#243925,#243926,#243927,#243928,#243929,
#243930,#243931,#243932,#243933,#243934,#243935,#243936,#243937,#243938,
#243939,#243940,#243941,#243942,#243943,#243944,#243945,#243946,#243947,
#243948,#243949,#243950,#243951,#243952,#243953,#243954,#243955,#243956,
#243957,#243958,#243959,#243960,#243961,#243962,#243963,#243964,#243965,
#243966,#243967,#243968,#243969,#243970,#243971,#243972,#243973,#243974,
#243975,#243976,#243977,#243978,#243979,#243980,#243981,#243982,#243983,
#243984,#243985,#243986,#243987,#243988,#243989,#243990,#243991,#243992,
#243993,#243994,#243995,#243996,#243997,#243998,#243999,#244000,#244001,
#244002,#244003,#244004,#244005,#244006,#244007,#244008,#244009,#244010,
#244011,#244012,#244013,#244014,#244015,#244016,#244017,#244018,#244019,
#244020,#244021,#244022,#244023,#244024,#244025,#244026,#244027,#244028,
#244029,#244030,#244031,#244032,#244033,#244034,#244035,#244036,#244037,
#244038,#244039,#244040,#244041,#244042,#244043,#244044,#244045,#244046,
#244047,#244048,#244049,#244050,#244051,#244052,#244053,#244054,#244055,
#244056,#244057,#244058,#244059,#244060,#244061,#244062,#244063,#244064,
#244065,#244066,#244067,#244068,#244069,#244070,#244071,#244072,#244073,
#244074,#244075,#244076,#244077,#244078,#244079,#244080,#244081,#244082,
#244083,#244084,#244085,#244086,#244087,#244088,#244089,#244090,#244091,
#244092,#244093,#244094,#244095,#244096,#244097,#244098,#244099,#244100,
#244101,#244102,#244103,#244104,#244105,#244106,#244107,#244108,#244109,
#244110,#244111,#244112,#244113,#244114,#244115,#244116,#244117,#244118,
#244119,#244120,#244121,#244122,#244123,#244124,#244125,#244126,#244127,
#244128,#244129,#244130,#244131,#244132,#244133,#244134,#244135,#244136,
#244137,#244138,#244139,#244140,#244141,#244142,#244143,#244144,#244145,
#244146,#244147,#244148,#244149,#244150,#244151,#244152,#244153,#244154,
#244155,#244156,#244157,#244158,#244159,#244160,#244161,#244162,#244163,
#244164,#244165,#244166,#244167,#244168,#244169,#244170,#244171,#244172,
#244173,#244174,#244175,#244176,#244177,#244178,#244179,#244180,#244181,
#244182,#244183,#244184,#244185,#244186,#244187,#244188,#244189,#244190,
#244191,#244192,#244193,#244194,#244195,#244196,#244197,#244198,#244199,
#244200,#244201,#244202,#244203,#244204,#244205,#244206,#244207,#244208,
#244209,#244210,#244211,#244212,#244213,#244214,#244215,#244216,#244217,
#244218,#244219,#244220)),.UNSPECIFIED.,.F.,.F.,.F.,(4,4),(4,1,1,1,1,1,
1,1,1,1,1,1,1,1,1,1,1,1,1,1,1,1,1,1,1,1,1,1,1,1,1,1,1,1,1,1,1,1,1,1,1,1,
1,1,1,1,1,1,1,1,1,1,1,1,1,1,1,1,1,1,1,1,1,1,1,1,1,1,1,1,1,1,1,1,1,1,1,1,
1,1,1,1,1,1,1,1,1,1,1,1,1,1,1,1,1,1,1,1,1,1,1,1,1,1,1,1,1,1,1,1,1,1,1,1,
1,1,1,1,1,1,1,1,1,1,1,1,1,1,1,1,1,1,1,1,1,1,1,1,1,1,1,1,1,1,1,1,1,1,1,1,
1,1,1,1,1,1,1,1,1,1,1,1,1,1,1,1,1,1,1,1,1,1,1,1,1,1,1,1,1,1,1,1,1,1,1,1,
1,1,1,1,1,1,1,1,1,1,1,1,1,1,1,1,1,1,1,1,1,1,1,1,1,1,1,1,1,1,1,1,1,1,1,1,
1,1,1,1,1,1,1,1,1,1,1,1,1,1,1,1,1,1,1,1,1,1,1,1,1,1,1,1,1,1,1,1,1,1,1,1,
1,1,1,1,1,1,1,1,1,1,1,1,1,1,1,1,1,1,1,1,1,1,1,1,1,1,1,1,1,1,1,1,1,1,1,1,
1,1,1,1,1,1,1,1,1,1,1,1,1,1,1,1,1,1,1,1,1,1,1,1,1,1,1,1,1,1,1,1,1,1,1,1,
1,1,1,1,1,1,1,1,1,1,1,1,1,1,1,1,1,1,1,1,1,1,1,1,1,1,1,1,1,1,1,1,1,1,1,1,
1,1,1,1,1,1,1,1,1,1,1,1,1,1,1,1,1,1,1,1,1,1,1,1,1,1,1,1,1,1,1,1,1,1,1,1,
1,1,1,1,1,1,1,1,1,1,1,1,1,1,1,1,1,1,1,1,1,1,1,1,1,1,1,1,1,1,1,1,1,1,1,1,
1,1,1,1,1,1,1,1,1,1,1,1,1,1,1,1,1,1,1,1,1,1,1,1,1,1,1,1,1,1,1,1,1,1,1,1,
1,1,1,1,1,1,1,1,1,1,1,1,1,1,1,1,1,1,1,1,1,1,1,1,1,1,1,1,1,1,1,1,1,1,1,1,
1,1,1,1,1,1,1,1,1,1,1,1,1,1,1,1,1,1,1,1,1,1,1,1,1,1,1,1,1,1,1,1,1,1,1,1,
1,1,1,1,1,1,1,1,1,1,1,1,1,1,1,1,1,1,1,1,1,1,1,1,1,1,1,1,1,1,1,1,1,1,1,1,
1,1,1,1,4),(-0.000839536803422264,0.135425581403526),(8.30104296596843,
8.80049912255811,9.2998689904892,9.79923885842029,10.2986087263514,11.2973484622136,
12.2960881980758,13.2948279339379,13.794197801869,14.2935676698001,14.7929375377312,
15.2923074056623,16.2910471415245,16.7904170094556,17.2897868773867,18.2885266132489,
19.287266349111,20.2860060849732,20.7853759529043,21.2847458208354,21.7841156887665,
22.2834855566976,23.2822252925598,23.7815951604909,24.280965028422,25.2797047642841,
26.2784445001463,27.2771842360085,27.7765541039396,28.2759239718707,28.7752938398018,
29.2746637077329,30.2734034435951,30.7727733115261,31.2721431794572,32.2708829153194,
33.2696226511816,34.2683623870438,34.7677322549749,35.267102122906,35.7664719908371,
36.2658418587681,37.2645815946303,37.7639514625614,38.2633213304925,39.2620610663547,
40.2608008022169,41.2595405380791,41.7589104060102,42.2582802739413,42.7576501418723,
43.2570200098034,44.2557597456656,44.7551296135967,45.2544994815278,46.25323921739,
47.2519789532522,48.2507186891144,48.7500885570454,49.2494584249765,49.7488282929076,
50.2481981608387,51.2469378967009,51.746307764632,52.2456776325631,53.2444173684253,
54.2431571042874,55.2418968401496,55.7412667080807,56.2406365760118,56.7400064439429,
57.239376311874,58.2381160477362,58.7374859156673,59.2368557835984,60.2355955194606,
61.2343352553227,62.2330749911849,62.732444859116,63.2318147270471,63.7311845949782,
64.2305544629093,65.2292941987715,65.7286640667025,66.2280339346336,67.2267736704958,
68.225513406358,69.2242531422202,69.7236230101513,70.2229928780824,70.7223627460135,
71.2217326139446,72.2204723498067,72.7198422177378,73.2192120856689,74.2179518215311,
75.2166915573933,76.2154312932555,76.7148011611866,77.2141710291177,77.7135408970487,
78.2129107649798,79.211650500842,79.7110203687731,80.2103902367042,81.2091299725664,
82.2078697084286,83.2066094442908,83.7059793122218,84.2053491801529,84.704719048084,
85.2040889160151,86.2028286518773,86.7021985198084,87.2015683877395,88.2003081236017,
89.1990478594639,90.197787595326,90.6971574632571,91.1965273311882,91.6958971991193,
92.1952670670504,93.1940068029126,93.6933766708437,94.1927465387748,95.191486274637,
96.1902260104991,97.1889657463613,97.6883356142924,98.1877054822235,98.6870753501546,
99.1864452180857,100.185184953948,100.684554821879,101.18392468981,102.182664425672,
103.181404161534,104.180143897397,104.679513765328,105.178883633259,105.67825350119,
106.177623369121,107.176363104983,107.675732972914,108.175102840845,109.173842576708,
110.17258231257,111.171322048432,111.670691916363,112.170061784294,112.669431652225,
113.168801520156,114.167541256018,114.66691112395,115.166280991881,116.165020727743,
117.163760463605,118.162500199467,118.661870067398,119.161239935329,119.66060980326,
120.159979671192,121.158719407054,121.658089274985,122.157459142916,123.156198878778,
124.15493861464,125.153678350502,125.653048218434,126.152418086365,126.651787954296,
127.151157822227,128.149897558089,128.64926742602,129.148637293951,130.147377029813,
131.146116765676,132.144856501538,132.644226369469,133.1435962374,133.642966105331,
134.142335973262,135.141075709124,135.640445577055,136.139815444986,137.138555180849,
138.137294916711,139.136034652573,139.635404520504,140.134774388435,140.634144256366,
141.133514124297,142.13225386016,142.631623728091,143.130993596022,144.129733331884,
145.128473067746,146.127212803608,146.626582671539,147.12595253947,147.625322407402,
148.124692275333,149.123432011195,149.622801879126,150.122171747057,151.120911482919,
152.119651218781,153.118390954644,153.617760822575,154.117130690506,154.616500558437,
155.115870426368,156.11461016223,156.613980030161,157.113349898092,158.112089633955,
159.110829369817,160.109569105679,160.60893897361,161.108308841541,161.607678709472,
162.107048577403,163.105788313265,163.605158181197,164.104528049128,165.10326778499,
166.102007520852,167.100747256714,167.600117124645,168.099486992576,168.598856860507,
169.098226728439,170.096966464301,170.596336332232,171.095706200163,172.094445936025,
173.093185671887,174.091925407749,174.591295275681,175.090665143612,175.590035011543,
176.089404879474,177.088144615336,177.587514483267,178.086884351198,179.08562408706,
180.084363822923,181.083103558785,181.582473426716,182.081843294647,182.581213162578,
183.080583030509,184.079322766371,184.578692634302,185.078062502233,186.076802238096,
187.075541973958,188.07428170982,188.573651577751,189.073021445682,189.572391313613,
190.071761181544,191.070500917407,191.569870785338,192.069240653269,193.067980389131,
194.066720124993,195.065459860855,195.564829728786,196.064199596717,196.563569464649,
197.06293933258,198.061679068442,198.561048936373,199.060418804304,200.059158540166,
201.057898276028,202.056638011891,202.556007879822,203.055377747753,203.554747615684,
204.054117483615,205.052857219477,205.552227087408,206.051596955339,207.050336691201,
208.049076427064,209.047816162926,209.547186030857,210.046555898788,210.545925766719,
211.04529563465,212.044035370512,212.543405238443,213.042775106375,214.041514842237,
215.040254578099,216.038994313961,217.037734049823,218.036473785686,219.035213521548,
220.03395325741,221.032692993272,221.532062861203,222.031432729134,223.030172464996,
223.529542332928,224.028912200859,224.52828206879,225.027651936721,226.026391672583,
227.025131408445,228.023871144307,228.523241012238,229.02261088017,230.021350616032,
230.520720483963,231.020090351894,231.519460219825,232.018830087756,233.017569823618,
234.01630955948,235.015049295343,235.514419163274,236.013789031205,237.012528767067,
237.511898634998,238.011268502929,238.51063837086,239.010008238791,240.008747974654,
241.007487710516,242.006227446378,242.505597314309,243.00496718224,244.003706918102,
244.503076786033,245.002446653964,245.501816521896,246.001186389827,246.999926125689,
247.998665861551,248.997405597413,249.496775465344,249.996145333275,250.994885069138,
251.494254937069,251.993624805,252.492994672931,252.992364540862,253.991104276724,
254.989844012586,255.988583748448,256.48795361638,256.987323484311,257.986063220173,
258.485433088104,258.984802956035,259.484172823966,259.983542691897,260.982282427759,
261.981022163622,262.979761899484,263.479131767415,263.978501635346,264.977241371208,
265.476611239139,265.97598110707,266.475350975001,266.974720842932,267.973460578795,
268.972200314657,269.970940050519,270.47030991845,270.969679786381,271.968419522243,
272.467789390175,272.967159258106,273.466529126037,273.965898993968,274.96463872983,
275.963378465692,276.962118201554,277.461488069485,277.960857937417,278.959597673279,
279.45896754121,279.958337409141,280.457707277072,280.957077145003,281.955816880865,
282.954556616727,283.95329635259,284.452666220521,284.952036088452,285.950775824314,
286.450145692245,286.949515560176,287.448885428107,287.948255296038,288.946995031901,
289.945734767763,290.944474503625,291.443844371556,291.943214239487,292.941953975349,
293.44132384328,293.940693711211,294.440063579143,294.939433447074,295.938173182936,
296.936912918798,297.93565265466,298.435022522591,298.934392390522,299.933132126385,
300.432501994316,300.931871862247,301.431241730178,301.930611598109,302.929351333971,
303.928091069833,304.926830805695,305.426200673627,305.925570541558,306.92431027742,
307.423680145351,307.923050013282,308.422419881213,308.921789749144,309.920529485006,
310.919269220869,311.918008956731,312.417378824662,312.916748692593,313.915488428455,
314.414858296386,314.914228164317,315.413598032248,315.912967900179,316.911707636042,
317.910447371904,318.909187107766,319.408556975697,319.907926843628,320.90666657949,
321.406036447421,321.905406315353,322.404776183284,322.904146051215,323.902885787077,
324.901625522939,325.900365258801,326.399735126732,326.899104994664,327.897844730526,
328.397214598457,328.896584466388,329.395954334319,329.89532420225,330.894063938112,
331.892803673974,332.891543409837,333.390913277768,333.890283145699,334.889022881561,
335.388392749492,335.887762617423,336.387132485354,336.886502353285,337.885242089147,
338.88398182501,339.882721560872,340.382091428803,340.881461296734,341.880201032596,
342.379570900527,342.878940768458,343.37831063639,343.877680504321,344.876420240183,
345.875159976045,346.873899711907,347.373269579838,347.872639447769,348.871379183632,
349.370749051563,349.870118919494,350.369488787425,350.868858655356,351.867598391218,
352.86633812708,353.865077862942,354.364447730874,354.863817598805,355.862557334667,
356.361927202598,356.861297070529,357.36066693846,357.860036806391,358.858776542253,
359.857516278115,360.856256013978,361.355625881909,361.85499574984,362.853735485702,
363.353105353633,363.852475221564,364.351845089495,364.851214957426,365.849954693289,
366.848694429151,367.847434165013,368.346804032944,368.846173900875,369.844913636737,
370.344283504668,370.8436533726,371.343023240531,371.842393108462,372.841132844324,
373.839872580186,374.838612316048,375.337982183979,375.83735205191,376.836091787773,
377.335461655704,377.834831523635,378.334201391566,378.833571259497,379.832310995359,
380.831050731221,381.829790467084,382.329160335015,382.828530202946,383.827269938808,
384.326639806739,384.82600967467,385.325379542601,385.824749410532,386.823489146394,
387.822228882257,388.820968618119,389.32033848605,389.819708353981,390.818448089843,
391.317817957774,391.817187825705,392.316557693636,392.815927561568,393.81466729743,
394.813407033292,395.812146769154,396.311516637085,396.810886505016,397.809626240879,
398.30899610881,398.808365976741,399.307735844672,399.807105712603,400.805845448465,
401.804585184327,402.803324920189,403.302694788121,403.802064656052,404.800804391914,
405.300174259845,405.799544127776,406.298913995707,406.798283863638,407.7970235995,
408.795763335362,409.794503071225,410.293872939156,410.793242807087,411.791982542949,
412.29135241088,412.790722278811,413.290092146742,413.789462014673,414.788201750536,
415.786941486398,416.78568122226,417.285051090191,417.784420958122,418.283790826053,
418.783223976954),.UNSPECIFIED.);
#296=B_SPLINE_SURFACE_WITH_KNOTS('',3,3,((#244442,#244443,#244444,#244445,
#244446,#244447,#244448,#244449,#244450,#244451,#244452,#244453,#244454,
#244455,#244456,#244457,#244458,#244459,#244460,#244461,#244462,#244463,
#244464,#244465,#244466,#244467,#244468,#244469,#244470,#244471,#244472,
#244473,#244474,#244475,#244476,#244477,#244478,#244479,#244480,#244481,
#244482,#244483,#244484,#244485,#244486,#244487,#244488,#244489,#244490,
#244491,#244492,#244493,#244494,#244495,#244496,#244497,#244498,#244499,
#244500,#244501,#244502,#244503,#244504,#244505,#244506,#244507,#244508,
#244509,#244510,#244511,#244512,#244513,#244514,#244515,#244516,#244517,
#244518,#244519,#244520,#244521,#244522,#244523,#244524,#244525,#244526,
#244527,#244528,#244529,#244530,#244531,#244532,#244533,#244534,#244535,
#244536,#244537,#244538,#244539,#244540,#244541,#244542,#244543,#244544,
#244545,#244546,#244547,#244548,#244549,#244550,#244551,#244552,#244553,
#244554,#244555,#244556,#244557,#244558,#244559,#244560,#244561,#244562,
#244563,#244564,#244565,#244566,#244567,#244568,#244569,#244570,#244571,
#244572,#244573,#244574,#244575,#244576,#244577,#244578,#244579,#244580,
#244581,#244582,#244583,#244584,#244585,#244586,#244587,#244588,#244589,
#244590,#244591,#244592,#244593,#244594,#244595,#244596,#244597,#244598,
#244599,#244600,#244601,#244602,#244603,#244604,#244605,#244606,#244607,
#244608,#244609,#244610,#244611,#244612,#244613,#244614,#244615,#244616,
#244617,#244618,#244619,#244620,#244621,#244622,#244623,#244624,#244625,
#244626,#244627,#244628,#244629,#244630,#244631,#244632,#244633,#244634,
#244635,#244636,#244637,#244638,#244639,#244640,#244641,#244642,#244643,
#244644,#244645,#244646,#244647,#244648,#244649,#244650,#244651,#244652,
#244653,#244654,#244655,#244656,#244657,#244658,#244659,#244660,#244661,
#244662,#244663,#244664,#244665,#244666,#244667,#244668,#244669,#244670,
#244671,#244672,#244673,#244674,#244675,#244676,#244677,#244678,#244679,
#244680,#244681,#244682,#244683,#244684,#244685,#244686,#244687,#244688,
#244689,#244690,#244691,#244692,#244693,#244694,#244695,#244696,#244697,
#244698,#244699,#244700,#244701,#244702,#244703,#244704,#244705,#244706,
#244707,#244708,#244709,#244710,#244711,#244712,#244713,#244714,#244715,
#244716,#244717,#244718,#244719,#244720,#244721,#244722,#244723,#244724,
#244725,#244726,#244727,#244728,#244729,#244730,#244731,#244732,#244733,
#244734,#244735,#244736,#244737,#244738,#244739,#244740,#244741,#244742,
#244743,#244744,#244745,#244746,#244747,#244748,#244749,#244750,#244751,
#244752,#244753,#244754,#244755,#244756,#244757,#244758,#244759,#244760,
#244761,#244762,#244763,#244764,#244765,#244766,#244767,#244768,#244769,
#244770,#244771,#244772,#244773,#244774,#244775,#244776,#244777,#244778,
#244779,#244780,#244781,#244782,#244783,#244784,#244785,#244786,#244787,
#244788,#244789,#244790,#244791,#244792,#244793,#244794,#244795,#244796,
#244797,#244798,#244799,#244800,#244801,#244802,#244803,#244804,#244805,
#244806,#244807,#244808,#244809,#244810,#244811,#244812,#244813,#244814,
#244815,#244816,#244817,#244818,#244819,#244820,#244821,#244822,#244823,
#244824,#244825,#244826,#244827,#244828,#244829,#244830,#244831,#244832,
#244833,#244834,#244835,#244836,#244837,#244838,#244839,#244840,#244841,
#244842,#244843,#244844,#244845,#244846,#244847,#244848,#244849,#244850,
#244851,#244852,#244853,#244854,#244855,#244856,#244857,#244858,#244859,
#244860,#244861,#244862,#244863,#244864,#244865,#244866,#244867,#244868,
#244869,#244870,#244871,#244872,#244873,#244874,#244875,#244876,#244877,
#244878,#244879,#244880,#244881,#244882,#244883,#244884,#244885,#244886,
#244887,#244888,#244889,#244890,#244891,#244892,#244893,#244894,#244895,
#244896,#244897,#244898,#244899,#244900,#244901,#244902,#244903,#244904,
#244905,#244906,#244907,#244908,#244909,#244910,#244911,#244912,#244913,
#244914,#244915,#244916,#244917,#244918,#244919,#244920,#244921,#244922,
#244923,#244924,#244925,#244926,#244927,#244928,#244929,#244930,#244931,
#244932,#244933,#244934,#244935,#244936,#244937,#244938,#244939,#244940,
#244941,#244942,#244943,#244944,#244945,#244946,#244947,#244948,#244949,
#244950,#244951,#244952,#244953,#244954,#244955,#244956,#244957,#244958,
#244959,#244960,#244961,#244962,#244963,#244964,#244965,#244966,#244967,
#244968,#244969,#244970,#244971,#244972,#244973,#244974,#244975,#244976,
#244977,#244978,#244979,#244980,#244981,#244982,#244983,#244984,#244985,
#244986,#244987,#244988,#244989,#244990,#244991,#244992,#244993,#244994,
#244995,#244996,#244997,#244998,#244999,#245000,#245001,#245002,#245003,
#245004,#245005,#245006,#245007,#245008,#245009,#245010,#245011,#245012,
#245013,#245014,#245015,#245016,#245017,#245018,#245019,#245020,#245021,
#245022,#245023,#245024,#245025,#245026,#245027,#245028,#245029,#245030),
(#245031,#245032,#245033,#245034,#245035,#245036,#245037,#245038,#245039,
#245040,#245041,#245042,#245043,#245044,#245045,#245046,#245047,#245048,
#245049,#245050,#245051,#245052,#245053,#245054,#245055,#245056,#245057,
#245058,#245059,#245060,#245061,#245062,#245063,#245064,#245065,#245066,
#245067,#245068,#245069,#245070,#245071,#245072,#245073,#245074,#245075,
#245076,#245077,#245078,#245079,#245080,#245081,#245082,#245083,#245084,
#245085,#245086,#245087,#245088,#245089,#245090,#245091,#245092,#245093,
#245094,#245095,#245096,#245097,#245098,#245099,#245100,#245101,#245102,
#245103,#245104,#245105,#245106,#245107,#245108,#245109,#245110,#245111,
#245112,#245113,#245114,#245115,#245116,#245117,#245118,#245119,#245120,
#245121,#245122,#245123,#245124,#245125,#245126,#245127,#245128,#245129,
#245130,#245131,#245132,#245133,#245134,#245135,#245136,#245137,#245138,
#245139,#245140,#245141,#245142,#245143,#245144,#245145,#245146,#245147,
#245148,#245149,#245150,#245151,#245152,#245153,#245154,#245155,#245156,
#245157,#245158,#245159,#245160,#245161,#245162,#245163,#245164,#245165,
#245166,#245167,#245168,#245169,#245170,#245171,#245172,#245173,#245174,
#245175,#245176,#245177,#245178,#245179,#245180,#245181,#245182,#245183,
#245184,#245185,#245186,#245187,#245188,#245189,#245190,#245191,#245192,
#245193,#245194,#245195,#245196,#245197,#245198,#245199,#245200,#245201,
#245202,#245203,#245204,#245205,#245206,#245207,#245208,#245209,#245210,
#245211,#245212,#245213,#245214,#245215,#245216,#245217,#245218,#245219,
#245220,#245221,#245222,#245223,#245224,#245225,#245226,#245227,#245228,
#245229,#245230,#245231,#245232,#245233,#245234,#245235,#245236,#245237,
#245238,#245239,#245240,#245241,#245242,#245243,#245244,#245245,#245246,
#245247,#245248,#245249,#245250,#245251,#245252,#245253,#245254,#245255,
#245256,#245257,#245258,#245259,#245260,#245261,#245262,#245263,#245264,
#245265,#245266,#245267,#245268,#245269,#245270,#245271,#245272,#245273,
#245274,#245275,#245276,#245277,#245278,#245279,#245280,#245281,#245282,
#245283,#245284,#245285,#245286,#245287,#245288,#245289,#245290,#245291,
#245292,#245293,#245294,#245295,#245296,#245297,#245298,#245299,#245300,
#245301,#245302,#245303,#245304,#245305,#245306,#245307,#245308,#245309,
#245310,#245311,#245312,#245313,#245314,#245315,#245316,#245317,#245318,
#245319,#245320,#245321,#245322,#245323,#245324,#245325,#245326,#245327,
#245328,#245329,#245330,#245331,#245332,#245333,#245334,#245335,#245336,
#245337,#245338,#245339,#245340,#245341,#245342,#245343,#245344,#245345,
#245346,#245347,#245348,#245349,#245350,#245351,#245352,#245353,#245354,
#245355,#245356,#245357,#245358,#245359,#245360,#245361,#245362,#245363,
#245364,#245365,#245366,#245367,#245368,#245369,#245370,#245371,#245372,
#245373,#245374,#245375,#245376,#245377,#245378,#245379,#245380,#245381,
#245382,#245383,#245384,#245385,#245386,#245387,#245388,#245389,#245390,
#245391,#245392,#245393,#245394,#245395,#245396,#245397,#245398,#245399,
#245400,#245401,#245402,#245403,#245404,#245405,#245406,#245407,#245408,
#245409,#245410,#245411,#245412,#245413,#245414,#245415,#245416,#245417,
#245418,#245419,#245420,#245421,#245422,#245423,#245424,#245425,#245426,
#245427,#245428,#245429,#245430,#245431,#245432,#245433,#245434,#245435,
#245436,#245437,#245438,#245439,#245440,#245441,#245442,#245443,#245444,
#245445,#245446,#245447,#245448,#245449,#245450,#245451,#245452,#245453,
#245454,#245455,#245456,#245457,#245458,#245459,#245460,#245461,#245462,
#245463,#245464,#245465,#245466,#245467,#245468,#245469,#245470,#245471,
#245472,#245473,#245474,#245475,#245476,#245477,#245478,#245479,#245480,
#245481,#245482,#245483,#245484,#245485,#245486,#245487,#245488,#245489,
#245490,#245491,#245492,#245493,#245494,#245495,#245496,#245497,#245498,
#245499,#245500,#245501,#245502,#245503,#245504,#245505,#245506,#245507,
#245508,#245509,#245510,#245511,#245512,#245513,#245514,#245515,#245516,
#245517,#245518,#245519,#245520,#245521,#245522,#245523,#245524,#245525,
#245526,#245527,#245528,#245529,#245530,#245531,#245532,#245533,#245534,
#245535,#245536,#245537,#245538,#245539,#245540,#245541,#245542,#245543,
#245544,#245545,#245546,#245547,#245548,#245549,#245550,#245551,#245552,
#245553,#245554,#245555,#245556,#245557,#245558,#245559,#245560,#245561,
#245562,#245563,#245564,#245565,#245566,#245567,#245568,#245569,#245570,
#245571,#245572,#245573,#245574,#245575,#245576,#245577,#245578,#245579,
#245580,#245581,#245582,#245583,#245584,#245585,#245586,#245587,#245588,
#245589,#245590,#245591,#245592,#245593,#245594,#245595,#245596,#245597,
#245598,#245599,#245600,#245601,#245602,#245603,#245604,#245605,#245606,
#245607,#245608,#245609,#245610,#245611,#245612,#245613,#245614,#245615,
#245616,#245617,#245618,#245619),(#245620,#245621,#245622,#245623,#245624,
#245625,#245626,#245627,#245628,#245629,#245630,#245631,#245632,#245633,
#245634,#245635,#245636,#245637,#245638,#245639,#245640,#245641,#245642,
#245643,#245644,#245645,#245646,#245647,#245648,#245649,#245650,#245651,
#245652,#245653,#245654,#245655,#245656,#245657,#245658,#245659,#245660,
#245661,#245662,#245663,#245664,#245665,#245666,#245667,#245668,#245669,
#245670,#245671,#245672,#245673,#245674,#245675,#245676,#245677,#245678,
#245679,#245680,#245681,#245682,#245683,#245684,#245685,#245686,#245687,
#245688,#245689,#245690,#245691,#245692,#245693,#245694,#245695,#245696,
#245697,#245698,#245699,#245700,#245701,#245702,#245703,#245704,#245705,
#245706,#245707,#245708,#245709,#245710,#245711,#245712,#245713,#245714,
#245715,#245716,#245717,#245718,#245719,#245720,#245721,#245722,#245723,
#245724,#245725,#245726,#245727,#245728,#245729,#245730,#245731,#245732,
#245733,#245734,#245735,#245736,#245737,#245738,#245739,#245740,#245741,
#245742,#245743,#245744,#245745,#245746,#245747,#245748,#245749,#245750,
#245751,#245752,#245753,#245754,#245755,#245756,#245757,#245758,#245759,
#245760,#245761,#245762,#245763,#245764,#245765,#245766,#245767,#245768,
#245769,#245770,#245771,#245772,#245773,#245774,#245775,#245776,#245777,
#245778,#245779,#245780,#245781,#245782,#245783,#245784,#245785,#245786,
#245787,#245788,#245789,#245790,#245791,#245792,#245793,#245794,#245795,
#245796,#245797,#245798,#245799,#245800,#245801,#245802,#245803,#245804,
#245805,#245806,#245807,#245808,#245809,#245810,#245811,#245812,#245813,
#245814,#245815,#245816,#245817,#245818,#245819,#245820,#245821,#245822,
#245823,#245824,#245825,#245826,#245827,#245828,#245829,#245830,#245831,
#245832,#245833,#245834,#245835,#245836,#245837,#245838,#245839,#245840,
#245841,#245842,#245843,#245844,#245845,#245846,#245847,#245848,#245849,
#245850,#245851,#245852,#245853,#245854,#245855,#245856,#245857,#245858,
#245859,#245860,#245861,#245862,#245863,#245864,#245865,#245866,#245867,
#245868,#245869,#245870,#245871,#245872,#245873,#245874,#245875,#245876,
#245877,#245878,#245879,#245880,#245881,#245882,#245883,#245884,#245885,
#245886,#245887,#245888,#245889,#245890,#245891,#245892,#245893,#245894,
#245895,#245896,#245897,#245898,#245899,#245900,#245901,#245902,#245903,
#245904,#245905,#245906,#245907,#245908,#245909,#245910,#245911,#245912,
#245913,#245914,#245915,#245916,#245917,#245918,#245919,#245920,#245921,
#245922,#245923,#245924,#245925,#245926,#245927,#245928,#245929,#245930,
#245931,#245932,#245933,#245934,#245935,#245936,#245937,#245938,#245939,
#245940,#245941,#245942,#245943,#245944,#245945,#245946,#245947,#245948,
#245949,#245950,#245951,#245952,#245953,#245954,#245955,#245956,#245957,
#245958,#245959,#245960,#245961,#245962,#245963,#245964,#245965,#245966,
#245967,#245968,#245969,#245970,#245971,#245972,#245973,#245974,#245975,
#245976,#245977,#245978,#245979,#245980,#245981,#245982,#245983,#245984,
#245985,#245986,#245987,#245988,#245989,#245990,#245991,#245992,#245993,
#245994,#245995,#245996,#245997,#245998,#245999,#246000,#246001,#246002,
#246003,#246004,#246005,#246006,#246007,#246008,#246009,#246010,#246011,
#246012,#246013,#246014,#246015,#246016,#246017,#246018,#246019,#246020,
#246021,#246022,#246023,#246024,#246025,#246026,#246027,#246028,#246029,
#246030,#246031,#246032,#246033,#246034,#246035,#246036,#246037,#246038,
#246039,#246040,#246041,#246042,#246043,#246044,#246045,#246046,#246047,
#246048,#246049,#246050,#246051,#246052,#246053,#246054,#246055,#246056,
#246057,#246058,#246059,#246060,#246061,#246062,#246063,#246064,#246065,
#246066,#246067,#246068,#246069,#246070,#246071,#246072,#246073,#246074,
#246075,#246076,#246077,#246078,#246079,#246080,#246081,#246082,#246083,
#246084,#246085,#246086,#246087,#246088,#246089,#246090,#246091,#246092,
#246093,#246094,#246095,#246096,#246097,#246098,#246099,#246100,#246101,
#246102,#246103,#246104,#246105,#246106,#246107,#246108,#246109,#246110,
#246111,#246112,#246113,#246114,#246115,#246116,#246117,#246118,#246119,
#246120,#246121,#246122,#246123,#246124,#246125,#246126,#246127,#246128,
#246129,#246130,#246131,#246132,#246133,#246134,#246135,#246136,#246137,
#246138,#246139,#246140,#246141,#246142,#246143,#246144,#246145,#246146,
#246147,#246148,#246149,#246150,#246151,#246152,#246153,#246154,#246155,
#246156,#246157,#246158,#246159,#246160,#246161,#246162,#246163,#246164,
#246165,#246166,#246167,#246168,#246169,#246170,#246171,#246172,#246173,
#246174,#246175,#246176,#246177,#246178,#246179,#246180,#246181,#246182,
#246183,#246184,#246185,#246186,#246187,#246188,#246189,#246190,#246191,
#246192,#246193,#246194,#246195,#246196,#246197,#246198,#246199,#246200,
#246201,#246202,#246203,#246204,#246205,#246206,#246207,#246208),(#246209,
#246210,#246211,#246212,#246213,#246214,#246215,#246216,#246217,#246218,
#246219,#246220,#246221,#246222,#246223,#246224,#246225,#246226,#246227,
#246228,#246229,#246230,#246231,#246232,#246233,#246234,#246235,#246236,
#246237,#246238,#246239,#246240,#246241,#246242,#246243,#246244,#246245,
#246246,#246247,#246248,#246249,#246250,#246251,#246252,#246253,#246254,
#246255,#246256,#246257,#246258,#246259,#246260,#246261,#246262,#246263,
#246264,#246265,#246266,#246267,#246268,#246269,#246270,#246271,#246272,
#246273,#246274,#246275,#246276,#246277,#246278,#246279,#246280,#246281,
#246282,#246283,#246284,#246285,#246286,#246287,#246288,#246289,#246290,
#246291,#246292,#246293,#246294,#246295,#246296,#246297,#246298,#246299,
#246300,#246301,#246302,#246303,#246304,#246305,#246306,#246307,#246308,
#246309,#246310,#246311,#246312,#246313,#246314,#246315,#246316,#246317,
#246318,#246319,#246320,#246321,#246322,#246323,#246324,#246325,#246326,
#246327,#246328,#246329,#246330,#246331,#246332,#246333,#246334,#246335,
#246336,#246337,#246338,#246339,#246340,#246341,#246342,#246343,#246344,
#246345,#246346,#246347,#246348,#246349,#246350,#246351,#246352,#246353,
#246354,#246355,#246356,#246357,#246358,#246359,#246360,#246361,#246362,
#246363,#246364,#246365,#246366,#246367,#246368,#246369,#246370,#246371,
#246372,#246373,#246374,#246375,#246376,#246377,#246378,#246379,#246380,
#246381,#246382,#246383,#246384,#246385,#246386,#246387,#246388,#246389,
#246390,#246391,#246392,#246393,#246394,#246395,#246396,#246397,#246398,
#246399,#246400,#246401,#246402,#246403,#246404,#246405,#246406,#246407,
#246408,#246409,#246410,#246411,#246412,#246413,#246414,#246415,#246416,
#246417,#246418,#246419,#246420,#246421,#246422,#246423,#246424,#246425,
#246426,#246427,#246428,#246429,#246430,#246431,#246432,#246433,#246434,
#246435,#246436,#246437,#246438,#246439,#246440,#246441,#246442,#246443,
#246444,#246445,#246446,#246447,#246448,#246449,#246450,#246451,#246452,
#246453,#246454,#246455,#246456,#246457,#246458,#246459,#246460,#246461,
#246462,#246463,#246464,#246465,#246466,#246467,#246468,#246469,#246470,
#246471,#246472,#246473,#246474,#246475,#246476,#246477,#246478,#246479,
#246480,#246481,#246482,#246483,#246484,#246485,#246486,#246487,#246488,
#246489,#246490,#246491,#246492,#246493,#246494,#246495,#246496,#246497,
#246498,#246499,#246500,#246501,#246502,#246503,#246504,#246505,#246506,
#246507,#246508,#246509,#246510,#246511,#246512,#246513,#246514,#246515,
#246516,#246517,#246518,#246519,#246520,#246521,#246522,#246523,#246524,
#246525,#246526,#246527,#246528,#246529,#246530,#246531,#246532,#246533,
#246534,#246535,#246536,#246537,#246538,#246539,#246540,#246541,#246542,
#246543,#246544,#246545,#246546,#246547,#246548,#246549,#246550,#246551,
#246552,#246553,#246554,#246555,#246556,#246557,#246558,#246559,#246560,
#246561,#246562,#246563,#246564,#246565,#246566,#246567,#246568,#246569,
#246570,#246571,#246572,#246573,#246574,#246575,#246576,#246577,#246578,
#246579,#246580,#246581,#246582,#246583,#246584,#246585,#246586,#246587,
#246588,#246589,#246590,#246591,#246592,#246593,#246594,#246595,#246596,
#246597,#246598,#246599,#246600,#246601,#246602,#246603,#246604,#246605,
#246606,#246607,#246608,#246609,#246610,#246611,#246612,#246613,#246614,
#246615,#246616,#246617,#246618,#246619,#246620,#246621,#246622,#246623,
#246624,#246625,#246626,#246627,#246628,#246629,#246630,#246631,#246632,
#246633,#246634,#246635,#246636,#246637,#246638,#246639,#246640,#246641,
#246642,#246643,#246644,#246645,#246646,#246647,#246648,#246649,#246650,
#246651,#246652,#246653,#246654,#246655,#246656,#246657,#246658,#246659,
#246660,#246661,#246662,#246663,#246664,#246665,#246666,#246667,#246668,
#246669,#246670,#246671,#246672,#246673,#246674,#246675,#246676,#246677,
#246678,#246679,#246680,#246681,#246682,#246683,#246684,#246685,#246686,
#246687,#246688,#246689,#246690,#246691,#246692,#246693,#246694,#246695,
#246696,#246697,#246698,#246699,#246700,#246701,#246702,#246703,#246704,
#246705,#246706,#246707,#246708,#246709,#246710,#246711,#246712,#246713,
#246714,#246715,#246716,#246717,#246718,#246719,#246720,#246721,#246722,
#246723,#246724,#246725,#246726,#246727,#246728,#246729,#246730,#246731,
#246732,#246733,#246734,#246735,#246736,#246737,#246738,#246739,#246740,
#246741,#246742,#246743,#246744,#246745,#246746,#246747,#246748,#246749,
#246750,#246751,#246752,#246753,#246754,#246755,#246756,#246757,#246758,
#246759,#246760,#246761,#246762,#246763,#246764,#246765,#246766,#246767,
#246768,#246769,#246770,#246771,#246772,#246773,#246774,#246775,#246776,
#246777,#246778,#246779,#246780,#246781,#246782,#246783,#246784,#246785,
#246786,#246787,#246788,#246789,#246790,#246791,#246792,#246793,#246794,
#246795,#246796,#246797)),.UNSPECIFIED.,.F.,.F.,.F.,(4,4),(4,1,1,1,1,1,
1,1,1,1,1,1,1,1,1,1,1,1,1,1,1,1,1,1,1,1,1,1,1,1,1,1,1,1,1,1,1,1,1,1,1,1,
1,1,1,1,1,1,1,1,1,1,1,1,1,1,1,1,1,1,1,1,1,1,1,1,1,1,1,1,1,1,1,1,1,1,1,1,
1,1,1,1,1,1,1,1,1,1,1,1,1,1,1,1,1,1,1,1,1,1,1,1,1,1,1,1,1,1,1,1,1,1,1,1,
1,1,1,1,1,1,1,1,1,1,1,1,1,1,1,1,1,1,1,1,1,1,1,1,1,1,1,1,1,1,1,1,1,1,1,1,
1,1,1,1,1,1,1,1,1,1,1,1,1,1,1,1,1,1,1,1,1,1,1,1,1,1,1,1,1,1,1,1,1,1,1,1,
1,1,1,1,1,1,1,1,1,1,1,1,1,1,1,1,1,1,1,1,1,1,1,1,1,1,1,1,1,1,1,1,1,1,1,1,
1,1,1,1,1,1,1,1,1,1,1,1,1,1,1,1,1,1,1,1,1,1,1,1,1,1,1,1,1,1,1,1,1,1,1,1,
1,1,1,1,1,1,1,1,1,1,1,1,1,1,1,1,1,1,1,1,1,1,1,1,1,1,1,1,1,1,1,1,1,1,1,1,
1,1,1,1,1,1,1,1,1,1,1,1,1,1,1,1,1,1,1,1,1,1,1,1,1,1,1,1,1,1,1,1,1,1,1,1,
1,1,1,1,1,1,1,1,1,1,1,1,1,1,1,1,1,1,1,1,1,1,1,1,1,1,1,1,1,1,1,1,1,1,1,1,
1,1,1,1,1,1,1,1,1,1,1,1,1,1,1,1,1,1,1,1,1,1,1,1,1,1,1,1,1,1,1,1,1,1,1,1,
1,1,1,1,1,1,1,1,1,1,1,1,1,1,1,1,1,1,1,1,1,1,1,1,1,1,1,1,1,1,1,1,1,1,1,1,
1,1,1,1,1,1,1,1,1,1,1,1,1,1,1,1,1,1,1,1,1,1,1,1,1,1,1,1,1,1,1,1,1,1,1,1,
1,1,1,1,1,1,1,1,1,1,1,1,1,1,1,1,1,1,1,1,1,1,1,1,1,1,1,1,1,1,1,1,1,1,1,1,
1,1,1,1,1,1,1,1,1,1,1,1,1,1,1,1,1,1,1,1,1,1,1,1,1,1,1,1,1,1,1,1,1,1,1,1,
1,1,1,1,1,1,1,1,1,1,1,1,1,1,1,1,1,1,1,1,1,1,1,1,1,1,1,1,1,1,1,1,1,1,1,1,
1,1,1,1,4),(-0.00304463950594017,0.132890720296283),(11.6147257896704,12.1144027157503,
12.6137725836814,13.1131424516125,13.6125123195436,14.6112520554058,15.6099917912679,
16.6087315271301,17.1081013950612,17.6074712629923,18.1068411309234,18.6062109988545,
19.6049507347167,20.1043206026478,20.6036904705788,21.602430206441,22.6011699423032,
23.5999096781654,24.0992795460965,24.5986494140276,25.0980192819587,25.5973891498898,
26.5961288857519,27.095498753683,27.5948686216141,28.5936083574763,29.5923480933385,
30.5910878292007,31.0904576971318,31.5898275650629,32.0891974329939,32.588567300925,
33.5873070367872,34.0866769047183,34.5860467726494,35.5847865085116,36.5835262443738,
37.582265980236,38.081635848167,38.5810057160981,39.0803755840292,39.5797454519603,
40.5784851878225,41.0778550557536,41.5772249236847,42.5759646595469,43.5747043954091,
44.5734441312712,45.0728139992023,45.5721838671334,46.0715537350645,46.5709236029956,
47.5696633388578,48.0690332067889,48.56840307472,49.5671428105821,50.5658825464443,
51.5646222823065,52.0639921502376,52.5633620181687,53.0627318860998,53.5621017540309,
54.5608414898931,55.0602113578242,55.5595812257552,56.5583209616174,57.5570606974796,
58.5558004333418,59.0551703012729,59.554540169204,60.0539100371351,60.5532799050662,
61.5520196409283,62.0513895088594,62.5507593767905,63.5494991126527,64.5482388485149,
65.5469785843771,66.0463484523082,66.5457183202393,67.0450881881704,67.5444580561014,
68.5431977919636,69.0425676598947,69.5419375278258,70.540677263688,71.5394169995502,
72.5381567354124,73.0375266033435,73.5368964712745,74.0362663392056,74.5356362071367,
75.5343759429989,76.03374581093,76.5331156788611,77.5318554147233,78.5305951505855,
79.5293348864476,80.0287047543787,80.5280746223098,81.0274444902409,81.526814358172,
82.5255540940342,83.0249239619653,83.5242938298964,84.5230335657586,85.5217733016207,
86.5205130374829,87.019882905414,87.5192527733451,88.0186226412762,88.5179925092073,
89.5167322450695,90.0161021130006,90.5154719809317,91.5142117167938,92.512951452656,
93.5116911885182,94.0110610564493,94.5104309243804,95.0098007923115,95.5091706602426,
96.5079103961047,97.0072802640358,97.5066501319669,98.5053898678291,99.5041296036913,
100.502869339553,101.002239207485,101.501609075416,102.000978943347,102.500348811278,
103.49908854714,103.998458415071,104.497828283002,105.496568018864,106.495307754727,
107.494047490589,107.99341735852,108.492787226451,108.992157094382,109.491526962313,
110.490266698175,110.989636566106,111.489006434037,112.4877461699,113.486485905762,
114.485225641624,114.984595509555,115.483965377486,115.983335245417,116.482705113348,
117.481444849211,117.980814717142,118.480184585073,119.478924320935,120.477664056797,
121.476403792659,121.97577366059,122.475143528521,122.974513396453,123.473883264384,
124.472623000246,124.971992868177,125.471362736108,126.47010247197,127.468842207832,
128.467581943695,128.966951811626,129.466321679557,129.965691547488,130.465061415419,
131.463801151281,131.963171019212,132.462540887143,133.461280623006,134.460020358868,
135.45876009473,135.958129962661,136.457499830592,136.956869698523,137.456239566454,
138.454979302316,138.954349170247,139.453719038179,140.452458774041,141.451198509903,
142.449938245765,142.949308113696,143.448677981627,143.948047849558,144.44741771749,
145.446157453352,145.945527321283,146.444897189214,147.443636925076,148.442376660938,
149.4411163968,149.940486264732,150.439856132663,150.939226000594,151.438595868525,
152.437335604387,152.936705472318,153.436075340249,154.434815076111,155.433554811974,
156.432294547836,156.931664415767,157.431034283698,157.930404151629,158.42977401956,
159.428513755422,159.927883623353,160.427253491284,161.425993227147,162.424732963009,
163.423472698871,163.922842566802,164.422212434733,164.921582302664,165.420952170595,
166.419691906458,166.919061774389,167.41843164232,168.417171378182,169.415911114044,
170.414650849906,170.914020717837,171.413390585768,171.9127604537,172.412130321631,
173.410870057493,173.910239925424,174.409609793355,175.408349529217,176.407089265079,
177.405829000942,177.905198868873,178.404568736804,178.903938604735,179.403308472666,
180.402048208528,180.901418076459,181.40078794439,182.399527680252,183.398267416115,
184.397007151977,184.896377019908,185.395746887839,185.89511675577,186.394486623701,
187.393226359563,187.892596227494,188.391966095426,189.390705831288,190.38944556715,
191.388185303012,191.887555170943,192.386925038874,192.886294906805,193.385664774736,
194.384404510599,194.88377437853,195.383144246461,196.381883982323,197.380623718185,
198.379363454047,198.878733321978,199.37810318991,199.877473057841,200.376842925772,
201.375582661634,201.874952529565,202.374322397496,203.373062133358,204.37180186922,
205.370541605083,205.869911473014,206.369281340945,206.868651208876,207.368021076807,
208.366760812669,208.8661306806,209.365500548531,210.364240284394,211.362980020256,
212.361719756118,212.861089624049,213.36045949198,213.859829359911,214.359199227842,
215.357938963704,215.857308831636,216.356678699567,217.355418435429,218.354158171291,
219.352897907153,220.351637643015,221.350377378878,222.34911711474,223.347856850602,
224.346596586464,224.845966454395,225.345336322326,226.344076058189,226.84344592612,
227.342815794051,227.842185661982,228.341555529913,229.340295265775,230.339035001637,
231.337774737499,231.837144605431,232.336514473362,233.335254209224,233.834624077155,
234.333993945086,234.833363813017,235.332733680948,236.33147341681,237.330213152673,
238.328952888535,238.828322756466,239.327692624397,240.326432360259,240.82580222819,
241.325172096121,241.824541964052,242.323911831983,243.322651567846,244.321391303708,
245.32013103957,245.819500907501,246.318870775432,247.317610511294,247.816980379225,
248.316350247157,248.815720115088,249.315089983019,250.313829718881,251.312569454743,
252.311309190605,252.810679058536,253.310048926467,254.30878866233,254.808158530261,
255.307528398192,255.806898266123,256.306268134054,257.305007869916,258.303747605778,
259.302487341641,259.801857209572,260.301227077503,261.299966813365,261.799336681296,
262.298706549227,262.798076417158,263.297446285089,264.296186020951,265.294925756814,
266.293665492676,266.793035360607,267.292405228538,268.2911449644,268.790514832331,
269.289884700262,269.789254568193,270.288624436125,271.287364171987,272.286103907849,
273.284843643711,273.784213511642,274.283583379573,275.282323115435,275.781692983366,
276.281062851298,276.780432719229,277.27980258716,278.278542323022,279.277282058884,
280.276021794746,280.775391662677,281.274761530609,282.273501266471,282.772871134402,
283.272241002333,283.771610870264,284.270980738195,285.269720474057,286.268460209919,
287.267199945782,287.766569813713,288.265939681644,289.264679417506,289.764049285437,
290.263419153368,290.762789021299,291.26215888923,292.260898625093,293.259638360955,
294.258378096817,294.757747964748,295.257117832679,296.255857568541,296.755227436472,
297.254597304403,297.753967172335,298.253337040266,299.252076776128,300.25081651199,
301.249556247852,301.748926115783,302.248295983714,303.247035719577,303.746405587508,
304.245775455439,304.74514532337,305.244515191301,306.243254927163,307.241994663025,
308.240734398887,308.740104266819,309.23947413475,310.238213870612,310.737583738543,
311.236953606474,311.736323474405,312.235693342336,313.234433078198,314.233172814061,
315.231912549923,315.731282417854,316.230652285785,317.229392021647,317.728761889578,
318.228131757509,318.72750162544,319.226871493372,320.225611229234,321.224350965096,
322.223090700958,322.722460568889,323.22183043682,324.220570172682,324.719940040613,
325.219309908545,325.718679776476,326.218049644407,327.216789380269,328.215529116131,
329.214268851993,329.713638719924,330.213008587855,331.211748323718,331.711118191649,
332.21048805958,332.709857927511,333.209227795442,334.207967531304,335.206707267166,
336.205447003029,336.70481687096,337.204186738891,338.202926474753,338.702296342684,
339.201666210615,339.701036078546,340.200405946477,341.19914568234,342.197885418202,
343.196625154064,343.695995021995,344.195364889926,345.194104625788,345.693474493719,
346.19284436165,346.692214229582,347.191584097513,348.190323833375,349.189063569237,
350.187803305099,350.68717317303,351.186543040961,352.185282776823,352.684652644755,
353.184022512686,353.683392380617,354.182762248548,355.18150198441,356.180241720272,
357.178981456134,357.678351324065,358.177721191997,359.176460927859,359.67583079579,
360.175200663721,360.674570531652,361.173940399583,362.172680135445,363.171419871308,
364.17015960717,364.669529475101,365.168899343032,366.167639078894,366.667008946825,
367.166378814756,367.665748682687,368.165118550618,369.163858286481,370.162598022343,
371.161337758205,371.660707626136,372.160077494067,373.158817229929,373.65818709786,
374.157556965792,374.656926833723,375.156296701654,376.155036437516,377.153776173378,
378.15251590924,378.651885777171,379.151255645102,380.149995380965,380.649365248896,
381.148735116827,381.648104984758,382.147474852689,383.146214588551,384.144954324413,
385.143694060276,385.643063928207,386.142433796138,387.141173532,387.640543399931,
388.139913267862,388.639283135793,389.138653003724,390.137392739586,391.136132475449,
392.134872211311,392.634242079242,393.133611947173,394.132351683035,394.631721550966,
395.131091418897,395.630461286828,396.12983115476,397.128570890622,398.127310626484,
399.126050362346,399.625420230277,400.124790098208,401.12352983407,401.622899702002,
402.122269569933,402.621639437864,403.121009305795,404.119749041657,405.118488777519,
406.117228513381,406.616598381312,407.115968249244,408.114707985106,408.614077853037,
409.113447720968,409.612817588899,410.11218745683,411.110927192692,412.109666928554,
413.108406664417,413.607776532348,414.107146400279,415.105886136141,415.605256004072,
416.104625872003,416.603995739934,417.103365607865,418.102105343728,419.10084507959,
420.099584815452,420.598954683383,421.098324551314,421.597694419245,422.097674725987),
 .UNSPECIFIED.);
#297=B_SPLINE_SURFACE_WITH_KNOTS('',3,3,((#259610,#259611,#259612,#259613,
#259614,#259615,#259616,#259617,#259618,#259619,#259620,#259621,#259622,
#259623,#259624,#259625,#259626,#259627,#259628,#259629,#259630,#259631,
#259632,#259633,#259634,#259635,#259636,#259637,#259638,#259639,#259640,
#259641,#259642,#259643,#259644,#259645,#259646,#259647,#259648,#259649,
#259650,#259651,#259652,#259653,#259654,#259655,#259656,#259657,#259658,
#259659,#259660,#259661,#259662,#259663,#259664,#259665,#259666,#259667,
#259668,#259669,#259670,#259671,#259672,#259673,#259674,#259675,#259676,
#259677,#259678,#259679,#259680,#259681,#259682,#259683,#259684,#259685,
#259686,#259687,#259688,#259689,#259690,#259691,#259692,#259693,#259694,
#259695,#259696,#259697,#259698,#259699,#259700,#259701,#259702,#259703,
#259704,#259705,#259706,#259707,#259708,#259709,#259710,#259711,#259712),
(#259713,#259714,#259715,#259716,#259717,#259718,#259719,#259720,#259721,
#259722,#259723,#259724,#259725,#259726,#259727,#259728,#259729,#259730,
#259731,#259732,#259733,#259734,#259735,#259736,#259737,#259738,#259739,
#259740,#259741,#259742,#259743,#259744,#259745,#259746,#259747,#259748,
#259749,#259750,#259751,#259752,#259753,#259754,#259755,#259756,#259757,
#259758,#259759,#259760,#259761,#259762,#259763,#259764,#259765,#259766,
#259767,#259768,#259769,#259770,#259771,#259772,#259773,#259774,#259775,
#259776,#259777,#259778,#259779,#259780,#259781,#259782,#259783,#259784,
#259785,#259786,#259787,#259788,#259789,#259790,#259791,#259792,#259793,
#259794,#259795,#259796,#259797,#259798,#259799,#259800,#259801,#259802,
#259803,#259804,#259805,#259806,#259807,#259808,#259809,#259810,#259811,
#259812,#259813,#259814,#259815),(#259816,#259817,#259818,#259819,#259820,
#259821,#259822,#259823,#259824,#259825,#259826,#259827,#259828,#259829,
#259830,#259831,#259832,#259833,#259834,#259835,#259836,#259837,#259838,
#259839,#259840,#259841,#259842,#259843,#259844,#259845,#259846,#259847,
#259848,#259849,#259850,#259851,#259852,#259853,#259854,#259855,#259856,
#259857,#259858,#259859,#259860,#259861,#259862,#259863,#259864,#259865,
#259866,#259867,#259868,#259869,#259870,#259871,#259872,#259873,#259874,
#259875,#259876,#259877,#259878,#259879,#259880,#259881,#259882,#259883,
#259884,#259885,#259886,#259887,#259888,#259889,#259890,#259891,#259892,
#259893,#259894,#259895,#259896,#259897,#259898,#259899,#259900,#259901,
#259902,#259903,#259904,#259905,#259906,#259907,#259908,#259909,#259910,
#259911,#259912,#259913,#259914,#259915,#259916,#259917,#259918),(#259919,
#259920,#259921,#259922,#259923,#259924,#259925,#259926,#259927,#259928,
#259929,#259930,#259931,#259932,#259933,#259934,#259935,#259936,#259937,
#259938,#259939,#259940,#259941,#259942,#259943,#259944,#259945,#259946,
#259947,#259948,#259949,#259950,#259951,#259952,#259953,#259954,#259955,
#259956,#259957,#259958,#259959,#259960,#259961,#259962,#259963,#259964,
#259965,#259966,#259967,#259968,#259969,#259970,#259971,#259972,#259973,
#259974,#259975,#259976,#259977,#259978,#259979,#259980,#259981,#259982,
#259983,#259984,#259985,#259986,#259987,#259988,#259989,#259990,#259991,
#259992,#259993,#259994,#259995,#259996,#259997,#259998,#259999,#260000,
#260001,#260002,#260003,#260004,#260005,#260006,#260007,#260008,#260009,
#260010,#260011,#260012,#260013,#260014,#260015,#260016,#260017,#260018,
#260019,#260020,#260021)),.UNSPECIFIED.,.F.,.F.,.F.,(4,4),(4,1,1,1,1,1,
1,1,1,1,1,1,1,1,1,1,1,1,1,1,1,1,1,1,1,1,1,1,1,1,1,1,1,1,1,1,1,1,1,1,1,1,
1,1,1,1,1,1,1,1,1,1,1,1,1,1,1,1,1,1,1,1,1,1,1,1,1,1,1,1,1,1,1,1,1,1,1,1,
1,1,1,1,1,1,1,1,1,1,1,1,1,1,1,1,1,1,1,1,1,1,4),(-0.000373081420709297,0.0826691585557874),
(11.61455969934,12.609327240686,13.6034402536173,14.5975532665487,15.59166627948,
16.5857792924113,17.5798923053427,18.574005318274,19.5681183312054,20.5622313441367,
21.556344357068,22.5504573699994,23.5445703829307,24.5386833958621,25.5327964087934,
26.5269094217247,27.5210224346561,28.5151354475874,29.5092484605188,30.5033614734501,
31.4974744863814,32.4915874993128,33.4857005122441,34.4798135251755,35.4739265381068,
36.4680395510381,37.4621525639695,38.4562655769008,39.4503785898322,40.4444916027635,
41.4386046156948,42.4327176286262,43.4268306415575,44.4209436544889,45.4150566674202,
46.4091696803515,47.4032826932829,48.3973957062142,49.3915087191456,50.3856217320769,
51.3797347450082,52.3738477579396,53.3679607708709,54.3620737838023,55.3561867967336,
56.3502998096649,57.3444128225963,58.3385258355276,59.332638848459,60.3267518613903,
61.3208648743217,62.314977887253,63.3090909001843,64.3032039131157,65.297316926047,
66.2914299389783,67.2855429519097,68.279655964841,69.2737689777724,70.2678819907037,
71.2619950036351,72.2561080165664,73.2502210294977,74.2443340424291,75.2384470553604,
76.2325600682917,77.2266730812231,78.2207860941544,79.2148991070858,80.2090121200171,
81.2031251329484,82.1972381458798,83.1913511588111,84.1854641717425,85.1795771846738,
86.1736901976051,87.1678032105365,88.1619162234678,89.1560292363992,90.1501422493305,
91.1442552622619,92.1383682751932,93.1324812881245,94.1265943010559,95.1207073139872,
96.1148203269185,97.1089333398499,98.1030463527812,99.0971593657126,100.091272378644,
101.085385391575,102.079498404507,103.073611417438,104.067724430369,105.061837443301,
106.055950456232,107.050063469163,108.044176482095,109.038289495026,110.032402507957,
111.027172073706),.UNSPECIFIED.);
#298=B_SPLINE_SURFACE_WITH_KNOTS('',3,3,((#260116,#260117,#260118,#260119,
#260120,#260121,#260122,#260123,#260124,#260125,#260126,#260127,#260128,
#260129,#260130,#260131,#260132,#260133,#260134,#260135,#260136,#260137,
#260138,#260139,#260140,#260141,#260142,#260143,#260144,#260145,#260146,
#260147,#260148,#260149,#260150,#260151,#260152,#260153,#260154,#260155,
#260156,#260157,#260158,#260159,#260160,#260161,#260162,#260163,#260164,
#260165,#260166,#260167,#260168,#260169,#260170,#260171,#260172,#260173,
#260174,#260175,#260176,#260177,#260178,#260179,#260180,#260181,#260182,
#260183,#260184,#260185,#260186,#260187,#260188,#260189,#260190,#260191,
#260192,#260193,#260194,#260195,#260196,#260197,#260198,#260199,#260200,
#260201,#260202,#260203,#260204,#260205,#260206,#260207,#260208,#260209,
#260210,#260211,#260212,#260213,#260214,#260215,#260216,#260217,#260218,
#260219,#260220),(#260221,#260222,#260223,#260224,#260225,#260226,#260227,
#260228,#260229,#260230,#260231,#260232,#260233,#260234,#260235,#260236,
#260237,#260238,#260239,#260240,#260241,#260242,#260243,#260244,#260245,
#260246,#260247,#260248,#260249,#260250,#260251,#260252,#260253,#260254,
#260255,#260256,#260257,#260258,#260259,#260260,#260261,#260262,#260263,
#260264,#260265,#260266,#260267,#260268,#260269,#260270,#260271,#260272,
#260273,#260274,#260275,#260276,#260277,#260278,#260279,#260280,#260281,
#260282,#260283,#260284,#260285,#260286,#260287,#260288,#260289,#260290,
#260291,#260292,#260293,#260294,#260295,#260296,#260297,#260298,#260299,
#260300,#260301,#260302,#260303,#260304,#260305,#260306,#260307,#260308,
#260309,#260310,#260311,#260312,#260313,#260314,#260315,#260316,#260317,
#260318,#260319,#260320,#260321,#260322,#260323,#260324,#260325),(#260326,
#260327,#260328,#260329,#260330,#260331,#260332,#260333,#260334,#260335,
#260336,#260337,#260338,#260339,#260340,#260341,#260342,#260343,#260344,
#260345,#260346,#260347,#260348,#260349,#260350,#260351,#260352,#260353,
#260354,#260355,#260356,#260357,#260358,#260359,#260360,#260361,#260362,
#260363,#260364,#260365,#260366,#260367,#260368,#260369,#260370,#260371,
#260372,#260373,#260374,#260375,#260376,#260377,#260378,#260379,#260380,
#260381,#260382,#260383,#260384,#260385,#260386,#260387,#260388,#260389,
#260390,#260391,#260392,#260393,#260394,#260395,#260396,#260397,#260398,
#260399,#260400,#260401,#260402,#260403,#260404,#260405,#260406,#260407,
#260408,#260409,#260410,#260411,#260412,#260413,#260414,#260415,#260416,
#260417,#260418,#260419,#260420,#260421,#260422,#260423,#260424,#260425,
#260426,#260427,#260428,#260429,#260430),(#260431,#260432,#260433,#260434,
#260435,#260436,#260437,#260438,#260439,#260440,#260441,#260442,#260443,
#260444,#260445,#260446,#260447,#260448,#260449,#260450,#260451,#260452,
#260453,#260454,#260455,#260456,#260457,#260458,#260459,#260460,#260461,
#260462,#260463,#260464,#260465,#260466,#260467,#260468,#260469,#260470,
#260471,#260472,#260473,#260474,#260475,#260476,#260477,#260478,#260479,
#260480,#260481,#260482,#260483,#260484,#260485,#260486,#260487,#260488,
#260489,#260490,#260491,#260492,#260493,#260494,#260495,#260496,#260497,
#260498,#260499,#260500,#260501,#260502,#260503,#260504,#260505,#260506,
#260507,#260508,#260509,#260510,#260511,#260512,#260513,#260514,#260515,
#260516,#260517,#260518,#260519,#260520,#260521,#260522,#260523,#260524,
#260525,#260526,#260527,#260528,#260529,#260530,#260531,#260532,#260533,
#260534,#260535)),.UNSPECIFIED.,.F.,.F.,.F.,(4,4),(4,1,1,1,1,1,1,1,1,1,
1,1,1,1,1,1,1,1,1,1,1,1,1,1,1,1,1,1,1,1,1,1,1,1,1,1,1,1,1,1,1,1,1,1,1,1,
1,1,1,1,1,1,1,1,1,1,1,1,1,1,1,1,1,1,1,1,1,1,1,1,1,1,1,1,1,1,1,1,1,1,1,1,
1,1,1,1,1,1,1,1,1,1,1,1,1,1,1,1,1,1,1,1,4),(-0.000656555906784362,0.0823778368201467),
(8.31473274985795,9.3095612095702,10.3043896692825,11.2992181289947,12.294046588707,
13.2888750484192,14.2837035081315,15.2785319678437,16.273360427556,17.2681888872682,
18.2630173469805,19.2578458066927,20.252674266405,21.2475027261172,22.2423311858295,
23.2371596455417,24.231988105254,25.2268165649662,26.2216450246785,27.2164734843908,
28.211301944103,29.2061304038153,30.2009588635275,31.1957873232398,32.190615782952,
33.1854442426643,34.1802727023765,35.1751011620888,36.169929621801,37.1647580815133,
38.1595865412255,39.1544150009378,40.14924346065,41.1440719203623,42.1389003800745,
43.1337288397868,44.1285572994991,45.1233857592113,46.1182142189236,47.1130426786358,
48.1078711383481,49.1026995980603,50.0975280577726,51.0923565174848,52.0871849771971,
53.0820134369093,54.0768418966216,55.0716703563338,56.0664988160461,57.0613272757583,
58.0561557354706,59.0509841951828,60.0458126548951,61.0406411146073,62.0354695743196,
63.0302980340319,64.0251264937441,65.0199549534563,66.0147834131686,67.0096118728809,
68.0044403325931,68.9992687923054,69.9940972520176,70.9889257117299,71.9837541714421,
72.9785826311544,73.9734110908666,74.9682395505789,75.9630680102911,76.9578964700034,
77.9527249297156,78.9475533894279,79.9423818491401,80.9372103088524,81.9320387685647,
82.9268672282769,83.9216956879892,84.9165241477014,85.9113526074137,86.9061810671259,
87.9010095268382,88.8958379865504,89.8906664462627,90.8854949059749,91.8803233656872,
92.8751518253994,93.8699802851117,94.8648087448239,95.8596372045362,96.8544656642484,
97.8492941239607,98.8441225836729,99.8389510433852,100.833779503097,101.82860796281,
102.823436422522,103.818264882234,104.813093341946,105.807921801659,106.802750261371,
107.797578721083,108.792407180795,109.787892196415),.UNSPECIFIED.);
#299=B_SPLINE_SURFACE_WITH_KNOTS('',3,3,((#277484,#277485,#277486,#277487,
#277488,#277489,#277490,#277491,#277492,#277493,#277494,#277495,#277496,
#277497,#277498,#277499,#277500,#277501,#277502,#277503,#277504,#277505,
#277506,#277507,#277508,#277509,#277510,#277511,#277512,#277513,#277514,
#277515,#277516,#277517,#277518,#277519,#277520,#277521,#277522,#277523,
#277524,#277525,#277526,#277527,#277528,#277529,#277530,#277531,#277532,
#277533,#277534,#277535,#277536,#277537,#277538,#277539,#277540,#277541,
#277542,#277543,#277544,#277545,#277546,#277547,#277548,#277549,#277550,
#277551,#277552,#277553,#277554,#277555,#277556,#277557,#277558,#277559,
#277560,#277561,#277562,#277563,#277564,#277565,#277566,#277567,#277568,
#277569,#277570,#277571,#277572,#277573,#277574,#277575,#277576,#277577,
#277578,#277579,#277580,#277581,#277582,#277583,#277584,#277585,#277586,
#277587,#277588,#277589,#277590,#277591,#277592,#277593,#277594,#277595,
#277596,#277597,#277598,#277599,#277600,#277601,#277602,#277603,#277604,
#277605,#277606,#277607,#277608,#277609,#277610,#277611,#277612,#277613,
#277614,#277615,#277616,#277617,#277618,#277619,#277620,#277621,#277622,
#277623,#277624,#277625,#277626,#277627,#277628,#277629,#277630,#277631,
#277632,#277633,#277634,#277635,#277636,#277637,#277638,#277639,#277640,
#277641,#277642,#277643,#277644,#277645,#277646,#277647,#277648,#277649,
#277650,#277651,#277652,#277653,#277654,#277655,#277656,#277657,#277658,
#277659,#277660,#277661),(#277662,#277663,#277664,#277665,#277666,#277667,
#277668,#277669,#277670,#277671,#277672,#277673,#277674,#277675,#277676,
#277677,#277678,#277679,#277680,#277681,#277682,#277683,#277684,#277685,
#277686,#277687,#277688,#277689,#277690,#277691,#277692,#277693,#277694,
#277695,#277696,#277697,#277698,#277699,#277700,#277701,#277702,#277703,
#277704,#277705,#277706,#277707,#277708,#277709,#277710,#277711,#277712,
#277713,#277714,#277715,#277716,#277717,#277718,#277719,#277720,#277721,
#277722,#277723,#277724,#277725,#277726,#277727,#277728,#277729,#277730,
#277731,#277732,#277733,#277734,#277735,#277736,#277737,#277738,#277739,
#277740,#277741,#277742,#277743,#277744,#277745,#277746,#277747,#277748,
#277749,#277750,#277751,#277752,#277753,#277754,#277755,#277756,#277757,
#277758,#277759,#277760,#277761,#277762,#277763,#277764,#277765,#277766,
#277767,#277768,#277769,#277770,#277771,#277772,#277773,#277774,#277775,
#277776,#277777,#277778,#277779,#277780,#277781,#277782,#277783,#277784,
#277785,#277786,#277787,#277788,#277789,#277790,#277791,#277792,#277793,
#277794,#277795,#277796,#277797,#277798,#277799,#277800,#277801,#277802,
#277803,#277804,#277805,#277806,#277807,#277808,#277809,#277810,#277811,
#277812,#277813,#277814,#277815,#277816,#277817,#277818,#277819,#277820,
#277821,#277822,#277823,#277824,#277825,#277826,#277827,#277828,#277829,
#277830,#277831,#277832,#277833,#277834,#277835,#277836,#277837,#277838,
#277839),(#277840,#277841,#277842,#277843,#277844,#277845,#277846,#277847,
#277848,#277849,#277850,#277851,#277852,#277853,#277854,#277855,#277856,
#277857,#277858,#277859,#277860,#277861,#277862,#277863,#277864,#277865,
#277866,#277867,#277868,#277869,#277870,#277871,#277872,#277873,#277874,
#277875,#277876,#277877,#277878,#277879,#277880,#277881,#277882,#277883,
#277884,#277885,#277886,#277887,#277888,#277889,#277890,#277891,#277892,
#277893,#277894,#277895,#277896,#277897,#277898,#277899,#277900,#277901,
#277902,#277903,#277904,#277905,#277906,#277907,#277908,#277909,#277910,
#277911,#277912,#277913,#277914,#277915,#277916,#277917,#277918,#277919,
#277920,#277921,#277922,#277923,#277924,#277925,#277926,#277927,#277928,
#277929,#277930,#277931,#277932,#277933,#277934,#277935,#277936,#277937,
#277938,#277939,#277940,#277941,#277942,#277943,#277944,#277945,#277946,
#277947,#277948,#277949,#277950,#277951,#277952,#277953,#277954,#277955,
#277956,#277957,#277958,#277959,#277960,#277961,#277962,#277963,#277964,
#277965,#277966,#277967,#277968,#277969,#277970,#277971,#277972,#277973,
#277974,#277975,#277976,#277977,#277978,#277979,#277980,#277981,#277982,
#277983,#277984,#277985,#277986,#277987,#277988,#277989,#277990,#277991,
#277992,#277993,#277994,#277995,#277996,#277997,#277998,#277999,#278000,
#278001,#278002,#278003,#278004,#278005,#278006,#278007,#278008,#278009,
#278010,#278011,#278012,#278013,#278014,#278015,#278016,#278017),(#278018,
#278019,#278020,#278021,#278022,#278023,#278024,#278025,#278026,#278027,
#278028,#278029,#278030,#278031,#278032,#278033,#278034,#278035,#278036,
#278037,#278038,#278039,#278040,#278041,#278042,#278043,#278044,#278045,
#278046,#278047,#278048,#278049,#278050,#278051,#278052,#278053,#278054,
#278055,#278056,#278057,#278058,#278059,#278060,#278061,#278062,#278063,
#278064,#278065,#278066,#278067,#278068,#278069,#278070,#278071,#278072,
#278073,#278074,#278075,#278076,#278077,#278078,#278079,#278080,#278081,
#278082,#278083,#278084,#278085,#278086,#278087,#278088,#278089,#278090,
#278091,#278092,#278093,#278094,#278095,#278096,#278097,#278098,#278099,
#278100,#278101,#278102,#278103,#278104,#278105,#278106,#278107,#278108,
#278109,#278110,#278111,#278112,#278113,#278114,#278115,#278116,#278117,
#278118,#278119,#278120,#278121,#278122,#278123,#278124,#278125,#278126,
#278127,#278128,#278129,#278130,#278131,#278132,#278133,#278134,#278135,
#278136,#278137,#278138,#278139,#278140,#278141,#278142,#278143,#278144,
#278145,#278146,#278147,#278148,#278149,#278150,#278151,#278152,#278153,
#278154,#278155,#278156,#278157,#278158,#278159,#278160,#278161,#278162,
#278163,#278164,#278165,#278166,#278167,#278168,#278169,#278170,#278171,
#278172,#278173,#278174,#278175,#278176,#278177,#278178,#278179,#278180,
#278181,#278182,#278183,#278184,#278185,#278186,#278187,#278188,#278189,
#278190,#278191,#278192,#278193,#278194,#278195)),.UNSPECIFIED.,.F.,.F.,
 .F.,(4,4),(4,1,1,1,1,1,1,1,1,1,1,1,1,1,1,1,1,1,1,1,1,1,1,1,1,1,1,1,1,1,
1,1,1,1,1,1,1,1,1,1,1,1,1,1,1,1,1,1,1,1,1,1,1,1,1,1,1,1,1,1,1,1,1,1,1,1,
1,1,1,1,1,1,1,1,1,1,1,1,1,1,1,1,1,1,1,1,1,1,1,1,1,1,1,1,1,1,1,1,1,1,1,1,
1,1,1,1,1,1,1,1,1,1,1,1,1,1,1,1,1,1,1,1,1,1,1,1,1,1,1,1,1,1,1,1,1,1,1,1,
1,1,1,1,1,1,1,1,1,1,1,1,1,1,1,1,1,1,1,1,1,1,1,1,1,1,1,1,1,1,1,1,1,1,1,1,
1,4),(-0.000292625423985075,0.0463342147672139),(11.6151021207979,12.6127553697675,
13.6100892204243,14.607423071081,15.6047569217378,16.6020907723946,17.5994246230513,
18.5967584737081,19.5940923243649,20.5914261750216,21.5887600256784,22.5860938763352,
23.5834277269919,24.5807615776487,25.5780954283055,26.5754292789622,27.572763129619,
28.5700969802757,29.5674308309325,30.5647646815893,31.562098532246,32.5594323829028,
33.5567662335596,34.5541000842163,35.5514339348731,36.5487677855299,37.5461016361866,
38.5434354868434,39.5407693375002,40.5381031881569,41.5354370388137,42.5327708894705,
43.5301047401272,44.527438590784,45.5247724414408,46.5221062920975,47.5194401427543,
48.5167739934111,49.5141078440678,50.5114416947246,51.5087755453814,52.5061093960381,
53.5034432466949,54.5007770973516,55.4981109480084,56.4954447986652,57.4927786493219,
58.4901124999787,59.4874463506355,60.4847802012922,61.482114051949,62.4794479026058,
63.4767817532625,64.4741156039193,65.4714494545761,66.4687833052328,67.4661171558896,
68.4634510065464,69.4607848572031,70.4581187078599,71.4554525585167,72.4527864091734,
73.4501202598302,74.447454110487,75.4447879611437,76.4421218118005,77.4394556624572,
78.436789513114,79.4341233637708,80.4314572144275,81.4287910650843,82.4261249157411,
83.4234587663978,84.4207926170546,85.4181264677114,86.4154603183681,87.4127941690249,
88.4101280196817,89.4074618703384,90.4047957209952,91.402129571652,92.3994634223087,
93.3967972729655,94.3941311236223,95.391464974279,96.3887988249358,97.3861326755925,
98.3834665262493,99.3808003769061,100.378134227563,101.37546807822,102.372801928876,
103.370135779533,104.36746963019,105.364803480847,106.362137331503,107.35947118216,
108.356805032817,109.354138883474,110.35147273413,111.348806584787,112.346140435444,
113.343474286101,114.340808136758,115.338141987414,116.335475838071,117.332809688728,
118.330143539385,119.327477390041,120.324811240698,121.322145091355,122.319478942012,
123.316812792668,124.314146643325,125.311480493982,126.308814344639,127.306148195296,
128.303482045952,129.300815896609,130.298149747266,131.295483597923,132.292817448579,
133.290151299236,134.287485149893,135.28481900055,136.282152851206,137.279486701863,
138.27682055252,139.274154403177,140.271488253833,141.26882210449,142.266155955147,
143.263489805804,144.260823656461,145.258157507117,146.255491357774,147.252825208431,
148.250159059088,149.247492909744,150.244826760401,151.242160611058,152.239494461715,
153.236828312371,154.234162163028,155.231496013685,156.228829864342,157.226163714998,
158.223497565655,159.220831416312,160.218165266969,161.215499117626,162.212832968282,
163.210166818939,164.207500669596,165.204834520253,166.202168370909,167.199502221566,
168.196836072223,169.19416992288,170.191503773536,171.188837624193,172.18617147485,
173.183505325507,174.180839176163,175.17817302682,176.175506877477,177.172840728134,
178.170174578791,179.167508429447,180.164842280104,181.162176130761,182.159509981418,
183.156843832074,184.154177682731,185.151511533388,186.148902899087),
 .UNSPECIFIED.);
#300=B_SPLINE_SURFACE_WITH_KNOTS('',3,3,((#278281,#278282,#278283,#278284,
#278285,#278286,#278287,#278288,#278289,#278290,#278291,#278292,#278293,
#278294,#278295,#278296,#278297,#278298,#278299,#278300,#278301,#278302,
#278303,#278304,#278305,#278306,#278307,#278308,#278309,#278310,#278311,
#278312,#278313,#278314,#278315,#278316,#278317,#278318,#278319,#278320,
#278321,#278322,#278323,#278324,#278325,#278326,#278327,#278328,#278329,
#278330,#278331,#278332,#278333,#278334,#278335,#278336,#278337,#278338,
#278339,#278340,#278341,#278342,#278343,#278344,#278345,#278346,#278347,
#278348,#278349,#278350,#278351,#278352,#278353,#278354,#278355,#278356,
#278357,#278358,#278359,#278360,#278361,#278362,#278363,#278364,#278365,
#278366,#278367,#278368,#278369,#278370,#278371,#278372,#278373,#278374,
#278375,#278376,#278377,#278378,#278379,#278380,#278381,#278382,#278383,
#278384,#278385,#278386,#278387,#278388,#278389,#278390,#278391,#278392,
#278393,#278394,#278395,#278396,#278397,#278398,#278399,#278400,#278401,
#278402,#278403,#278404,#278405,#278406,#278407,#278408,#278409,#278410,
#278411,#278412,#278413,#278414,#278415,#278416,#278417,#278418,#278419,
#278420,#278421,#278422,#278423,#278424,#278425,#278426,#278427,#278428,
#278429,#278430,#278431,#278432,#278433,#278434,#278435,#278436,#278437,
#278438,#278439,#278440,#278441,#278442,#278443,#278444,#278445,#278446,
#278447,#278448,#278449,#278450,#278451,#278452,#278453,#278454,#278455,
#278456,#278457,#278458,#278459,#278460),(#278461,#278462,#278463,#278464,
#278465,#278466,#278467,#278468,#278469,#278470,#278471,#278472,#278473,
#278474,#278475,#278476,#278477,#278478,#278479,#278480,#278481,#278482,
#278483,#278484,#278485,#278486,#278487,#278488,#278489,#278490,#278491,
#278492,#278493,#278494,#278495,#278496,#278497,#278498,#278499,#278500,
#278501,#278502,#278503,#278504,#278505,#278506,#278507,#278508,#278509,
#278510,#278511,#278512,#278513,#278514,#278515,#278516,#278517,#278518,
#278519,#278520,#278521,#278522,#278523,#278524,#278525,#278526,#278527,
#278528,#278529,#278530,#278531,#278532,#278533,#278534,#278535,#278536,
#278537,#278538,#278539,#278540,#278541,#278542,#278543,#278544,#278545,
#278546,#278547,#278548,#278549,#278550,#278551,#278552,#278553,#278554,
#278555,#278556,#278557,#278558,#278559,#278560,#278561,#278562,#278563,
#278564,#278565,#278566,#278567,#278568,#278569,#278570,#278571,#278572,
#278573,#278574,#278575,#278576,#278577,#278578,#278579,#278580,#278581,
#278582,#278583,#278584,#278585,#278586,#278587,#278588,#278589,#278590,
#278591,#278592,#278593,#278594,#278595,#278596,#278597,#278598,#278599,
#278600,#278601,#278602,#278603,#278604,#278605,#278606,#278607,#278608,
#278609,#278610,#278611,#278612,#278613,#278614,#278615,#278616,#278617,
#278618,#278619,#278620,#278621,#278622,#278623,#278624,#278625,#278626,
#278627,#278628,#278629,#278630,#278631,#278632,#278633,#278634,#278635,
#278636,#278637,#278638,#278639,#278640),(#278641,#278642,#278643,#278644,
#278645,#278646,#278647,#278648,#278649,#278650,#278651,#278652,#278653,
#278654,#278655,#278656,#278657,#278658,#278659,#278660,#278661,#278662,
#278663,#278664,#278665,#278666,#278667,#278668,#278669,#278670,#278671,
#278672,#278673,#278674,#278675,#278676,#278677,#278678,#278679,#278680,
#278681,#278682,#278683,#278684,#278685,#278686,#278687,#278688,#278689,
#278690,#278691,#278692,#278693,#278694,#278695,#278696,#278697,#278698,
#278699,#278700,#278701,#278702,#278703,#278704,#278705,#278706,#278707,
#278708,#278709,#278710,#278711,#278712,#278713,#278714,#278715,#278716,
#278717,#278718,#278719,#278720,#278721,#278722,#278723,#278724,#278725,
#278726,#278727,#278728,#278729,#278730,#278731,#278732,#278733,#278734,
#278735,#278736,#278737,#278738,#278739,#278740,#278741,#278742,#278743,
#278744,#278745,#278746,#278747,#278748,#278749,#278750,#278751,#278752,
#278753,#278754,#278755,#278756,#278757,#278758,#278759,#278760,#278761,
#278762,#278763,#278764,#278765,#278766,#278767,#278768,#278769,#278770,
#278771,#278772,#278773,#278774,#278775,#278776,#278777,#278778,#278779,
#278780,#278781,#278782,#278783,#278784,#278785,#278786,#278787,#278788,
#278789,#278790,#278791,#278792,#278793,#278794,#278795,#278796,#278797,
#278798,#278799,#278800,#278801,#278802,#278803,#278804,#278805,#278806,
#278807,#278808,#278809,#278810,#278811,#278812,#278813,#278814,#278815,
#278816,#278817,#278818,#278819,#278820),(#278821,#278822,#278823,#278824,
#278825,#278826,#278827,#278828,#278829,#278830,#278831,#278832,#278833,
#278834,#278835,#278836,#278837,#278838,#278839,#278840,#278841,#278842,
#278843,#278844,#278845,#278846,#278847,#278848,#278849,#278850,#278851,
#278852,#278853,#278854,#278855,#278856,#278857,#278858,#278859,#278860,
#278861,#278862,#278863,#278864,#278865,#278866,#278867,#278868,#278869,
#278870,#278871,#278872,#278873,#278874,#278875,#278876,#278877,#278878,
#278879,#278880,#278881,#278882,#278883,#278884,#278885,#278886,#278887,
#278888,#278889,#278890,#278891,#278892,#278893,#278894,#278895,#278896,
#278897,#278898,#278899,#278900,#278901,#278902,#278903,#278904,#278905,
#278906,#278907,#278908,#278909,#278910,#278911,#278912,#278913,#278914,
#278915,#278916,#278917,#278918,#278919,#278920,#278921,#278922,#278923,
#278924,#278925,#278926,#278927,#278928,#278929,#278930,#278931,#278932,
#278933,#278934,#278935,#278936,#278937,#278938,#278939,#278940,#278941,
#278942,#278943,#278944,#278945,#278946,#278947,#278948,#278949,#278950,
#278951,#278952,#278953,#278954,#278955,#278956,#278957,#278958,#278959,
#278960,#278961,#278962,#278963,#278964,#278965,#278966,#278967,#278968,
#278969,#278970,#278971,#278972,#278973,#278974,#278975,#278976,#278977,
#278978,#278979,#278980,#278981,#278982,#278983,#278984,#278985,#278986,
#278987,#278988,#278989,#278990,#278991,#278992,#278993,#278994,#278995,
#278996,#278997,#278998,#278999,#279000)),.UNSPECIFIED.,.F.,.F.,.F.,(4,
4),(4,1,1,1,1,1,1,1,1,1,1,1,1,1,1,1,1,1,1,1,1,1,1,1,1,1,1,1,1,1,1,1,1,1,
1,1,1,1,1,1,1,1,1,1,1,1,1,1,1,1,1,1,1,1,1,1,1,1,1,1,1,1,1,1,1,1,1,1,1,1,
1,1,1,1,1,1,1,1,1,1,1,1,1,1,1,1,1,1,1,1,1,1,1,1,1,1,1,1,1,1,1,1,1,1,1,1,
1,1,1,1,1,1,1,1,1,1,1,1,1,1,1,1,1,1,1,1,1,1,1,1,1,1,1,1,1,1,1,1,1,1,1,1,
1,1,1,1,1,1,1,1,1,1,1,1,1,1,1,1,1,1,1,1,1,1,1,1,1,1,1,1,1,1,1,1,1,1,1,4),
(-0.000319937213065475,0.0463079691845939),(8.31044140786475,9.30831892272975,
10.3060509227196,11.3037829227095,12.3015149226994,13.2992469226893,14.2969789226792,
15.2947109226691,16.292442922659,17.2901749226489,18.2879069226388,19.2856389226287,
20.2833709226186,21.2811029226085,22.2788349225984,23.2765669225883,24.2742989225782,
25.2720309225681,26.269762922558,27.2674949225479,28.2652269225378,29.2629589225277,
30.2606909225176,31.2584229225075,32.2561549224974,33.2538869224873,34.2516189224772,
35.2493509224671,36.247082922457,37.2448149224469,38.2425469224368,39.2402789224267,
40.2380109224166,41.2357429224065,42.2334749223964,43.2312069223863,44.2289389223762,
45.2266709223661,46.224402922356,47.2221349223459,48.2198669223358,49.2175989223257,
50.2153309223156,51.2130629223055,52.2107949222954,53.2085269222853,54.2062589222752,
55.2039909222651,56.201722922255,57.1994549222449,58.1971869222348,59.1949189222247,
60.1926509222146,61.1903829222045,62.1881149221944,63.1858469221843,64.1835789221742,
65.1813109221641,66.179042922154,67.1767749221439,68.1745069221338,69.1722389221237,
70.1699709221136,71.1677029221035,72.1654349220934,73.1631669220833,74.1608989220732,
75.1586309220631,76.1563629220529,77.1540949220428,78.1518269220327,79.1495589220227,
80.1472909220126,81.1450229220025,82.1427549219923,83.1404869219822,84.1382189219721,
85.135950921962,86.1336829219519,87.1314149219419,88.1291469219317,89.1268789219216,
90.1246109219115,91.1223429219014,92.1200749218913,93.1178069218812,94.1155389218711,
95.113270921861,96.1110029218509,97.1087349218408,98.1064669218307,99.1041989218206,
100.101930921811,101.0996629218,102.09739492179,103.09512692178,104.09285892177,
105.09059092176,106.08832292175,107.08605492174,108.08378692173,109.08151892172,
110.07925092171,111.076982921699,112.074714921689,113.072446921679,114.070178921669,
115.067910921659,116.065642921649,117.063374921639,118.061106921629,119.058838921619,
120.056570921608,121.054302921598,122.052034921588,123.049766921578,124.047498921568,
125.045230921558,126.042962921548,127.040694921538,128.038426921528,129.036158921518,
130.033890921507,131.031622921497,132.029354921487,133.027086921477,134.024818921467,
135.022550921457,136.020282921447,137.018014921437,138.015746921427,139.013478921417,
140.011210921406,141.008942921396,142.006674921386,143.004406921376,144.002138921366,
144.999870921356,145.997602921346,146.995334921336,147.993066921326,148.990798921316,
149.988530921305,150.986262921295,151.983994921285,152.981726921275,153.979458921265,
154.977190921255,155.974922921245,156.972654921235,157.970386921225,158.968118921215,
159.965850921204,160.963582921194,161.961314921184,162.959046921174,163.956778921164,
164.954510921154,165.952242921144,166.949974921134,167.947706921124,168.945438921114,
169.943170921103,170.940902921093,171.938634921083,172.936366921073,173.934098921063,
174.931830921053,175.929562921043,176.927294921033,177.925026921023,178.922758921013,
179.920490921002,180.918222920992,181.915954920982,182.913686920972,183.911418920962,
184.909470858165),.UNSPECIFIED.);
#301=B_SPLINE_SURFACE_WITH_KNOTS('',3,3,((#288259,#288260,#288261,#288262,
#288263,#288264,#288265,#288266,#288267,#288268,#288269,#288270,#288271,
#288272,#288273,#288274,#288275,#288276,#288277,#288278,#288279,#288280,
#288281,#288282,#288283,#288284,#288285,#288286,#288287,#288288,#288289,
#288290,#288291,#288292,#288293,#288294,#288295,#288296,#288297,#288298,
#288299,#288300,#288301,#288302,#288303,#288304,#288305,#288306,#288307,
#288308,#288309,#288310,#288311,#288312,#288313,#288314,#288315,#288316,
#288317,#288318,#288319,#288320,#288321,#288322,#288323,#288324,#288325,
#288326,#288327,#288328,#288329,#288330,#288331,#288332,#288333,#288334,
#288335,#288336,#288337,#288338,#288339,#288340,#288341,#288342,#288343,
#288344,#288345,#288346,#288347,#288348,#288349,#288350,#288351,#288352,
#288353,#288354,#288355,#288356,#288357,#288358,#288359,#288360,#288361,
#288362,#288363,#288364),(#288365,#288366,#288367,#288368,#288369,#288370,
#288371,#288372,#288373,#288374,#288375,#288376,#288377,#288378,#288379,
#288380,#288381,#288382,#288383,#288384,#288385,#288386,#288387,#288388,
#288389,#288390,#288391,#288392,#288393,#288394,#288395,#288396,#288397,
#288398,#288399,#288400,#288401,#288402,#288403,#288404,#288405,#288406,
#288407,#288408,#288409,#288410,#288411,#288412,#288413,#288414,#288415,
#288416,#288417,#288418,#288419,#288420,#288421,#288422,#288423,#288424,
#288425,#288426,#288427,#288428,#288429,#288430,#288431,#288432,#288433,
#288434,#288435,#288436,#288437,#288438,#288439,#288440,#288441,#288442,
#288443,#288444,#288445,#288446,#288447,#288448,#288449,#288450,#288451,
#288452,#288453,#288454,#288455,#288456,#288457,#288458,#288459,#288460,
#288461,#288462,#288463,#288464,#288465,#288466,#288467,#288468,#288469,
#288470),(#288471,#288472,#288473,#288474,#288475,#288476,#288477,#288478,
#288479,#288480,#288481,#288482,#288483,#288484,#288485,#288486,#288487,
#288488,#288489,#288490,#288491,#288492,#288493,#288494,#288495,#288496,
#288497,#288498,#288499,#288500,#288501,#288502,#288503,#288504,#288505,
#288506,#288507,#288508,#288509,#288510,#288511,#288512,#288513,#288514,
#288515,#288516,#288517,#288518,#288519,#288520,#288521,#288522,#288523,
#288524,#288525,#288526,#288527,#288528,#288529,#288530,#288531,#288532,
#288533,#288534,#288535,#288536,#288537,#288538,#288539,#288540,#288541,
#288542,#288543,#288544,#288545,#288546,#288547,#288548,#288549,#288550,
#288551,#288552,#288553,#288554,#288555,#288556,#288557,#288558,#288559,
#288560,#288561,#288562,#288563,#288564,#288565,#288566,#288567,#288568,
#288569,#288570,#288571,#288572,#288573,#288574,#288575,#288576),(#288577,
#288578,#288579,#288580,#288581,#288582,#288583,#288584,#288585,#288586,
#288587,#288588,#288589,#288590,#288591,#288592,#288593,#288594,#288595,
#288596,#288597,#288598,#288599,#288600,#288601,#288602,#288603,#288604,
#288605,#288606,#288607,#288608,#288609,#288610,#288611,#288612,#288613,
#288614,#288615,#288616,#288617,#288618,#288619,#288620,#288621,#288622,
#288623,#288624,#288625,#288626,#288627,#288628,#288629,#288630,#288631,
#288632,#288633,#288634,#288635,#288636,#288637,#288638,#288639,#288640,
#288641,#288642,#288643,#288644,#288645,#288646,#288647,#288648,#288649,
#288650,#288651,#288652,#288653,#288654,#288655,#288656,#288657,#288658,
#288659,#288660,#288661,#288662,#288663,#288664,#288665,#288666,#288667,
#288668,#288669,#288670,#288671,#288672,#288673,#288674,#288675,#288676,
#288677,#288678,#288679,#288680,#288681,#288682)),.UNSPECIFIED.,.F.,.F.,
 .F.,(4,4),(4,1,1,1,1,1,1,1,1,1,1,1,1,1,1,1,1,1,1,1,1,1,1,1,1,1,1,1,1,1,
1,1,1,1,1,1,1,1,1,1,1,1,1,1,1,1,1,1,1,1,1,1,1,1,1,1,1,1,1,1,1,1,1,1,1,1,
1,1,1,1,1,1,1,1,1,1,1,1,1,1,1,1,1,1,1,1,1,1,1,1,1,1,1,1,1,1,1,1,1,1,1,1,
1,4),(-0.000292638147730025,0.0463354487950187),(11.6151020518147,12.6127573616628,
13.610093204215,14.6074290467673,15.6047648893195,16.6021007318718,17.599436574424,
18.5967724169762,19.5941082595285,20.5914441020807,21.588779944633,22.5861157871852,
23.5834516297375,24.5807874722897,25.5781233148419,26.5754591573942,27.5727949999464,
28.5701308424987,29.5674666850509,30.5648025276032,31.5621383701554,32.5594742127077,
33.5568100552599,34.5541458978121,35.5514817403644,36.5488175829166,37.5461534254689,
38.5434892680211,39.5408251105734,40.5381609531256,41.5354967956779,42.5328326382301,
43.5301684807823,44.5275043233346,45.5248401658868,46.5221760084391,47.5195118509913,
48.5168476935436,49.5141835360958,50.5115193786481,51.5088552212003,52.5061910637525,
53.5035269063048,54.500862748857,55.4981985914093,56.4955344339615,57.4928702765138,
58.490206119066,59.4875419616182,60.4848778041705,61.4822136467227,62.479549489275,
63.4768853318272,64.4742211743795,65.4715570169317,66.468892859484,67.4662287020362,
68.4635645445884,69.4609003871407,70.4582362296929,71.4555720722452,72.4529079147974,
73.4502437573497,74.4475795999019,75.4449154424541,76.4422512850064,77.4395871275586,
78.4369229701109,79.4342588126631,80.4315946552154,81.4289304977676,82.4262663403199,
83.4236021828721,84.4209380254243,85.4182738679766,86.4156097105288,87.4129455530811,
88.4102813956333,89.4076172381856,90.4049530807378,91.4022889232901,92.3996247658423,
93.3969606083945,94.3942964509468,95.391632293499,96.3889681360513,97.3863039786035,
98.3836398211558,99.380975663708,100.37831150626,101.375647348812,102.372983191365,
103.370319033917,104.367654876469,105.364990719021,106.362326561574,107.359662404126,
108.356998246678,109.35433408923,110.351669931783,111.349005774335,112.346341616887,
113.343677459439,114.341333934333),.UNSPECIFIED.);
#302=B_SPLINE_SURFACE_WITH_KNOTS('',3,3,((#288765,#288766,#288767,#288768,
#288769,#288770,#288771,#288772,#288773,#288774,#288775,#288776,#288777,
#288778,#288779,#288780,#288781,#288782,#288783,#288784,#288785,#288786,
#288787,#288788,#288789,#288790,#288791,#288792,#288793,#288794,#288795,
#288796,#288797,#288798,#288799,#288800,#288801,#288802,#288803,#288804,
#288805,#288806,#288807,#288808,#288809,#288810,#288811,#288812,#288813,
#288814,#288815,#288816,#288817,#288818,#288819,#288820,#288821,#288822,
#288823,#288824,#288825,#288826,#288827,#288828,#288829,#288830,#288831,
#288832,#288833,#288834,#288835,#288836,#288837,#288838,#288839,#288840,
#288841,#288842,#288843,#288844,#288845,#288846,#288847,#288848,#288849,
#288850,#288851,#288852,#288853,#288854,#288855,#288856,#288857,#288858,
#288859,#288860,#288861,#288862,#288863,#288864,#288865,#288866,#288867,
#288868,#288869,#288870,#288871,#288872),(#288873,#288874,#288875,#288876,
#288877,#288878,#288879,#288880,#288881,#288882,#288883,#288884,#288885,
#288886,#288887,#288888,#288889,#288890,#288891,#288892,#288893,#288894,
#288895,#288896,#288897,#288898,#288899,#288900,#288901,#288902,#288903,
#288904,#288905,#288906,#288907,#288908,#288909,#288910,#288911,#288912,
#288913,#288914,#288915,#288916,#288917,#288918,#288919,#288920,#288921,
#288922,#288923,#288924,#288925,#288926,#288927,#288928,#288929,#288930,
#288931,#288932,#288933,#288934,#288935,#288936,#288937,#288938,#288939,
#288940,#288941,#288942,#288943,#288944,#288945,#288946,#288947,#288948,
#288949,#288950,#288951,#288952,#288953,#288954,#288955,#288956,#288957,
#288958,#288959,#288960,#288961,#288962,#288963,#288964,#288965,#288966,
#288967,#288968,#288969,#288970,#288971,#288972,#288973,#288974,#288975,
#288976,#288977,#288978,#288979,#288980),(#288981,#288982,#288983,#288984,
#288985,#288986,#288987,#288988,#288989,#288990,#288991,#288992,#288993,
#288994,#288995,#288996,#288997,#288998,#288999,#289000,#289001,#289002,
#289003,#289004,#289005,#289006,#289007,#289008,#289009,#289010,#289011,
#289012,#289013,#289014,#289015,#289016,#289017,#289018,#289019,#289020,
#289021,#289022,#289023,#289024,#289025,#289026,#289027,#289028,#289029,
#289030,#289031,#289032,#289033,#289034,#289035,#289036,#289037,#289038,
#289039,#289040,#289041,#289042,#289043,#289044,#289045,#289046,#289047,
#289048,#289049,#289050,#289051,#289052,#289053,#289054,#289055,#289056,
#289057,#289058,#289059,#289060,#289061,#289062,#289063,#289064,#289065,
#289066,#289067,#289068,#289069,#289070,#289071,#289072,#289073,#289074,
#289075,#289076,#289077,#289078,#289079,#289080,#289081,#289082,#289083,
#289084,#289085,#289086,#289087,#289088),(#289089,#289090,#289091,#289092,
#289093,#289094,#289095,#289096,#289097,#289098,#289099,#289100,#289101,
#289102,#289103,#289104,#289105,#289106,#289107,#289108,#289109,#289110,
#289111,#289112,#289113,#289114,#289115,#289116,#289117,#289118,#289119,
#289120,#289121,#289122,#289123,#289124,#289125,#289126,#289127,#289128,
#289129,#289130,#289131,#289132,#289133,#289134,#289135,#289136,#289137,
#289138,#289139,#289140,#289141,#289142,#289143,#289144,#289145,#289146,
#289147,#289148,#289149,#289150,#289151,#289152,#289153,#289154,#289155,
#289156,#289157,#289158,#289159,#289160,#289161,#289162,#289163,#289164,
#289165,#289166,#289167,#289168,#289169,#289170,#289171,#289172,#289173,
#289174,#289175,#289176,#289177,#289178,#289179,#289180,#289181,#289182,
#289183,#289184,#289185,#289186,#289187,#289188,#289189,#289190,#289191,
#289192,#289193,#289194,#289195,#289196)),.UNSPECIFIED.,.F.,.F.,.F.,(4,
4),(4,1,1,1,1,1,1,1,1,1,1,1,1,1,1,1,1,1,1,1,1,1,1,1,1,1,1,1,1,1,1,1,1,1,
1,1,1,1,1,1,1,1,1,1,1,1,1,1,1,1,1,1,1,1,1,1,1,1,1,1,1,1,1,1,1,1,1,1,1,1,
1,1,1,1,1,1,1,1,1,1,1,1,1,1,1,1,1,1,1,1,1,1,1,1,1,1,1,1,1,1,1,1,1,1,1,4),
(-0.000320373313366601,0.0463083434471542),(8.31044130225981,9.30859389336977,
10.3066008639999,11.30460783463,12.30261480526,13.3006217758901,14.2986287465202,
15.2966357171503,16.2946426877804,17.2926496584105,18.2906566290406,19.2886635996707,
20.2866705703008,21.2846775409308,22.2826845115609,23.280691482191,24.2786984528211,
25.2767054234512,26.2747123940813,27.2727193647114,28.2707263353415,29.2687333059716,
30.2667402766016,31.2647472472317,32.2627542178618,33.2607611884919,34.258768159122,
35.2567751297521,36.2547821003822,37.2527890710123,38.2507960416424,39.2488030122724,
40.2468099829025,41.2448169535326,42.2428239241627,43.2408308947928,44.2388378654229,
45.236844836053,46.2348518066831,47.2328587773132,48.2308657479432,49.2288727185733,
50.2268796892034,51.2248866598335,52.2228936304636,53.2209006010937,54.2189075717238,
55.2169145423539,56.214921512984,57.212928483614,58.2109354542441,59.2089424248742,
60.2069493955043,61.2049563661344,62.2029633367645,63.2009703073946,64.1989772780247,
65.1969842486548,66.1949912192848,67.1929981899149,68.191005160545,69.1890121311751,
70.1870191018052,71.1850260724353,72.1830330430654,73.1810400136955,74.1790469843256,
75.1770539549557,76.1750609255857,77.1730678962158,78.1710748668459,79.169081837476,
80.1670888081061,81.1650957787362,82.1631027493663,83.1611097199964,84.1591166906264,
85.1571236612565,86.1551306318866,87.1531376025167,88.1511445731468,89.1491515437769,
90.147158514407,91.1451654850371,92.1431724556672,93.1411794262973,94.1391863969273,
95.1371933675574,96.1352003381875,97.1332073088176,98.1312142794477,99.1292212500778,
100.127228220708,101.125235191338,102.123242161968,103.121249132598,104.119256103228,
105.117263073858,106.115270044488,107.113277015118,108.111283985749,109.109290956379,
110.107297927009,111.105304897639,112.103311868269,113.101639212212),
 .UNSPECIFIED.);
#303=PLANE('',#17160);
#304=PLANE('',#17161);
#305=PLANE('',#17162);
#306=PLANE('',#17163);
#307=PLANE('',#17164);
#308=PLANE('',#17165);
#309=PLANE('',#17166);
#310=PLANE('',#17167);
#311=PLANE('',#17180);
#312=PLANE('',#17181);
#313=PLANE('',#17182);
#314=PLANE('',#17183);
#315=PLANE('',#17184);
#316=PLANE('',#17185);
#317=PLANE('',#17399);
#318=PLANE('',#17400);
#319=PLANE('',#17401);
#320=PLANE('',#17402);
#321=PLANE('',#17403);
#322=PLANE('',#17404);
#323=PLANE('',#17406);
#324=PLANE('',#17407);
#325=PLANE('',#17421);
#326=PLANE('',#17422);
#327=PLANE('',#17423);
#328=PLANE('',#17424);
#329=PLANE('',#17428);
#330=PLANE('',#17429);
#331=PLANE('',#17430);
#332=PLANE('',#17431);
#333=PLANE('',#17432);
#334=PLANE('',#17433);
#335=PLANE('',#17434);
#336=PLANE('',#17435);
#337=PLANE('',#17436);
#338=PLANE('',#17437);
#339=PLANE('',#17438);
#340=PLANE('',#17440);
#341=PLANE('',#17441);
#342=PLANE('',#17442);
#343=PLANE('',#17449);
#344=PLANE('',#17508);
#345=PLANE('',#17513);
#346=PLANE('',#17514);
#347=PLANE('',#17515);
#348=PLANE('',#17516);
#349=PLANE('',#17518);
#350=PLANE('',#17519);
#351=PLANE('',#17524);
#352=PLANE('',#17526);
#353=PLANE('',#17530);
#354=PLANE('',#17542);
#355=PLANE('',#17543);
#356=PLANE('',#17544);
#357=PLANE('',#17545);
#358=PLANE('',#17546);
#359=PLANE('',#17547);
#360=PLANE('',#17548);
#361=PLANE('',#17549);
#362=PLANE('',#17550);
#363=PLANE('',#17551);
#364=PLANE('',#17552);
#365=PLANE('',#17554);
#366=PLANE('',#17555);
#367=PLANE('',#17556);
#368=PLANE('',#17572);
#369=PLANE('',#17573);
#370=PLANE('',#17574);
#371=PLANE('',#17582);
#372=PLANE('',#17583);
#373=PLANE('',#17657);
#374=PLANE('',#17658);
#375=PLANE('',#17665);
#376=PLANE('',#17666);
#377=PLANE('',#17691);
#378=PLANE('',#17698);
#379=PLANE('',#17699);
#380=PLANE('',#17704);
#381=PLANE('',#17706);
#382=PLANE('',#17710);
#383=PLANE('',#17715);
#384=PLANE('',#17717);
#385=PLANE('',#17725);
#386=PLANE('',#17726);
#387=PLANE('',#17728);
#388=PLANE('',#17729);
#389=PLANE('',#17730);
#390=PLANE('',#17737);
#391=PLANE('',#17745);
#392=PLANE('',#17746);
#393=PLANE('',#17775);
#394=PLANE('',#17776);
#395=PLANE('',#17777);
#396=PLANE('',#17778);
#397=PLANE('',#17779);
#398=PLANE('',#17780);
#399=PLANE('',#17781);
#400=PLANE('',#17782);
#401=PLANE('',#17786);
#402=PLANE('',#17787);
#403=PLANE('',#17829);
#404=PLANE('',#17830);
#405=PLANE('',#17831);
#406=PLANE('',#17832);
#407=PLANE('',#17833);
#408=PLANE('',#17834);
#409=PLANE('',#17835);
#410=PLANE('',#17836);
#411=PLANE('',#17840);
#412=PLANE('',#17841);
#413=PLANE('',#17851);
#414=PLANE('',#17852);
#415=PLANE('',#17853);
#416=PLANE('',#17854);
#417=PLANE('',#17855);
#418=PLANE('',#17856);
#419=PLANE('',#17857);
#420=PLANE('',#17858);
#421=PLANE('',#17862);
#422=PLANE('',#17863);
#423=FACE_OUTER_BOUND('',#1073,.T.);
#424=FACE_OUTER_BOUND('',#1074,.T.);
#425=FACE_OUTER_BOUND('',#1075,.T.);
#426=FACE_OUTER_BOUND('',#1076,.T.);
#427=FACE_OUTER_BOUND('',#1077,.T.);
#428=FACE_OUTER_BOUND('',#1078,.T.);
#429=FACE_OUTER_BOUND('',#1079,.T.);
#430=FACE_OUTER_BOUND('',#1080,.T.);
#431=FACE_OUTER_BOUND('',#1081,.T.);
#432=FACE_OUTER_BOUND('',#1082,.T.);
#433=FACE_OUTER_BOUND('',#1083,.T.);
#434=FACE_OUTER_BOUND('',#1084,.T.);
#435=FACE_OUTER_BOUND('',#1085,.T.);
#436=FACE_OUTER_BOUND('',#1086,.T.);
#437=FACE_OUTER_BOUND('',#1087,.T.);
#438=FACE_OUTER_BOUND('',#1088,.T.);
#439=FACE_OUTER_BOUND('',#1089,.T.);
#440=FACE_OUTER_BOUND('',#1090,.T.);
#441=FACE_OUTER_BOUND('',#1091,.T.);
#442=FACE_OUTER_BOUND('',#1092,.T.);
#443=FACE_OUTER_BOUND('',#1093,.T.);
#444=FACE_OUTER_BOUND('',#1094,.T.);
#445=FACE_OUTER_BOUND('',#1095,.T.);
#446=FACE_OUTER_BOUND('',#1096,.T.);
#447=FACE_OUTER_BOUND('',#1097,.T.);
#448=FACE_OUTER_BOUND('',#1098,.T.);
#449=FACE_OUTER_BOUND('',#1099,.T.);
#450=FACE_OUTER_BOUND('',#1100,.T.);
#451=FACE_OUTER_BOUND('',#1101,.T.);
#452=FACE_OUTER_BOUND('',#1102,.T.);
#453=FACE_OUTER_BOUND('',#1103,.T.);
#454=FACE_OUTER_BOUND('',#1104,.T.);
#455=FACE_OUTER_BOUND('',#1105,.T.);
#456=FACE_OUTER_BOUND('',#1106,.T.);
#457=FACE_OUTER_BOUND('',#1107,.T.);
#458=FACE_OUTER_BOUND('',#1108,.T.);
#459=FACE_OUTER_BOUND('',#1109,.T.);
#460=FACE_OUTER_BOUND('',#1110,.T.);
#461=FACE_OUTER_BOUND('',#1111,.T.);
#462=FACE_OUTER_BOUND('',#1112,.T.);
#463=FACE_OUTER_BOUND('',#1113,.T.);
#464=FACE_OUTER_BOUND('',#1114,.T.);
#465=FACE_OUTER_BOUND('',#1115,.T.);
#466=FACE_OUTER_BOUND('',#1116,.T.);
#467=FACE_OUTER_BOUND('',#1117,.T.);
#468=FACE_OUTER_BOUND('',#1118,.T.);
#469=FACE_OUTER_BOUND('',#1119,.T.);
#470=FACE_OUTER_BOUND('',#1120,.T.);
#471=FACE_OUTER_BOUND('',#1121,.T.);
#472=FACE_OUTER_BOUND('',#1122,.T.);
#473=FACE_OUTER_BOUND('',#1123,.T.);
#474=FACE_OUTER_BOUND('',#1124,.T.);
#475=FACE_OUTER_BOUND('',#1125,.T.);
#476=FACE_OUTER_BOUND('',#1126,.T.);
#477=FACE_OUTER_BOUND('',#1127,.T.);
#478=FACE_OUTER_BOUND('',#1128,.T.);
#479=FACE_OUTER_BOUND('',#1129,.T.);
#480=FACE_OUTER_BOUND('',#1130,.T.);
#481=FACE_OUTER_BOUND('',#1131,.T.);
#482=FACE_OUTER_BOUND('',#1132,.T.);
#483=FACE_OUTER_BOUND('',#1133,.T.);
#484=FACE_OUTER_BOUND('',#1134,.T.);
#485=FACE_OUTER_BOUND('',#1135,.T.);
#486=FACE_OUTER_BOUND('',#1136,.T.);
#487=FACE_OUTER_BOUND('',#1137,.T.);
#488=FACE_OUTER_BOUND('',#1138,.T.);
#489=FACE_OUTER_BOUND('',#1139,.T.);
#490=FACE_OUTER_BOUND('',#1140,.T.);
#491=FACE_OUTER_BOUND('',#1141,.T.);
#492=FACE_OUTER_BOUND('',#1142,.T.);
#493=FACE_OUTER_BOUND('',#1143,.T.);
#494=FACE_OUTER_BOUND('',#1144,.T.);
#495=FACE_OUTER_BOUND('',#1145,.T.);
#496=FACE_OUTER_BOUND('',#1146,.T.);
#497=FACE_OUTER_BOUND('',#1147,.T.);
#498=FACE_OUTER_BOUND('',#1148,.T.);
#499=FACE_OUTER_BOUND('',#1149,.T.);
#500=FACE_OUTER_BOUND('',#1150,.T.);
#501=FACE_OUTER_BOUND('',#1151,.T.);
#502=FACE_OUTER_BOUND('',#1152,.T.);
#503=FACE_OUTER_BOUND('',#1153,.T.);
#504=FACE_OUTER_BOUND('',#1154,.T.);
#505=FACE_OUTER_BOUND('',#1155,.T.);
#506=FACE_OUTER_BOUND('',#1156,.T.);
#507=FACE_OUTER_BOUND('',#1157,.T.);
#508=FACE_OUTER_BOUND('',#1158,.T.);
#509=FACE_OUTER_BOUND('',#1159,.T.);
#510=FACE_OUTER_BOUND('',#1160,.T.);
#511=FACE_OUTER_BOUND('',#1161,.T.);
#512=FACE_OUTER_BOUND('',#1162,.T.);
#513=FACE_OUTER_BOUND('',#1163,.T.);
#514=FACE_OUTER_BOUND('',#1164,.T.);
#515=FACE_OUTER_BOUND('',#1165,.T.);
#516=FACE_OUTER_BOUND('',#1166,.T.);
#517=FACE_OUTER_BOUND('',#1167,.T.);
#518=FACE_OUTER_BOUND('',#1168,.T.);
#519=FACE_OUTER_BOUND('',#1169,.T.);
#520=FACE_OUTER_BOUND('',#1170,.T.);
#521=FACE_OUTER_BOUND('',#1171,.T.);
#522=FACE_OUTER_BOUND('',#1172,.T.);
#523=FACE_OUTER_BOUND('',#1173,.T.);
#524=FACE_OUTER_BOUND('',#1174,.T.);
#525=FACE_OUTER_BOUND('',#1175,.T.);
#526=FACE_OUTER_BOUND('',#1176,.T.);
#527=FACE_OUTER_BOUND('',#1177,.T.);
#528=FACE_OUTER_BOUND('',#1178,.T.);
#529=FACE_OUTER_BOUND('',#1179,.T.);
#530=FACE_OUTER_BOUND('',#1180,.T.);
#531=FACE_OUTER_BOUND('',#1181,.T.);
#532=FACE_OUTER_BOUND('',#1182,.T.);
#533=FACE_OUTER_BOUND('',#1183,.T.);
#534=FACE_OUTER_BOUND('',#1184,.T.);
#535=FACE_OUTER_BOUND('',#1185,.T.);
#536=FACE_OUTER_BOUND('',#1194,.T.);
#537=FACE_OUTER_BOUND('',#1199,.T.);
#538=FACE_OUTER_BOUND('',#1200,.T.);
#539=FACE_OUTER_BOUND('',#1201,.T.);
#540=FACE_OUTER_BOUND('',#1202,.T.);
#541=FACE_OUTER_BOUND('',#1203,.T.);
#542=FACE_OUTER_BOUND('',#1204,.T.);
#543=FACE_OUTER_BOUND('',#1205,.T.);
#544=FACE_OUTER_BOUND('',#1206,.T.);
#545=FACE_OUTER_BOUND('',#1207,.T.);
#546=FACE_OUTER_BOUND('',#1208,.T.);
#547=FACE_OUTER_BOUND('',#1209,.T.);
#548=FACE_OUTER_BOUND('',#1210,.T.);
#549=FACE_OUTER_BOUND('',#1211,.T.);
#550=FACE_OUTER_BOUND('',#1212,.T.);
#551=FACE_OUTER_BOUND('',#1213,.T.);
#552=FACE_OUTER_BOUND('',#1214,.T.);
#553=FACE_OUTER_BOUND('',#1215,.T.);
#554=FACE_OUTER_BOUND('',#1216,.T.);
#555=FACE_OUTER_BOUND('',#1217,.T.);
#556=FACE_OUTER_BOUND('',#1218,.T.);
#557=FACE_OUTER_BOUND('',#1219,.T.);
#558=FACE_OUTER_BOUND('',#1220,.T.);
#559=FACE_OUTER_BOUND('',#1221,.T.);
#560=FACE_OUTER_BOUND('',#1222,.T.);
#561=FACE_OUTER_BOUND('',#1223,.T.);
#562=FACE_OUTER_BOUND('',#1224,.T.);
#563=FACE_OUTER_BOUND('',#1225,.T.);
#564=FACE_OUTER_BOUND('',#1226,.T.);
#565=FACE_OUTER_BOUND('',#1227,.T.);
#566=FACE_OUTER_BOUND('',#1228,.T.);
#567=FACE_OUTER_BOUND('',#1229,.T.);
#568=FACE_OUTER_BOUND('',#1230,.T.);
#569=FACE_OUTER_BOUND('',#1231,.T.);
#570=FACE_OUTER_BOUND('',#1232,.T.);
#571=FACE_OUTER_BOUND('',#1233,.T.);
#572=FACE_OUTER_BOUND('',#1234,.T.);
#573=FACE_OUTER_BOUND('',#1235,.T.);
#574=FACE_OUTER_BOUND('',#1236,.T.);
#575=FACE_OUTER_BOUND('',#1237,.T.);
#576=FACE_OUTER_BOUND('',#1238,.T.);
#577=FACE_OUTER_BOUND('',#1239,.T.);
#578=FACE_OUTER_BOUND('',#1240,.T.);
#579=FACE_OUTER_BOUND('',#1241,.T.);
#580=FACE_OUTER_BOUND('',#1242,.T.);
#581=FACE_OUTER_BOUND('',#1243,.T.);
#582=FACE_OUTER_BOUND('',#1244,.T.);
#583=FACE_OUTER_BOUND('',#1245,.T.);
#584=FACE_OUTER_BOUND('',#1246,.T.);
#585=FACE_OUTER_BOUND('',#1247,.T.);
#586=FACE_OUTER_BOUND('',#1248,.T.);
#587=FACE_OUTER_BOUND('',#1249,.T.);
#588=FACE_OUTER_BOUND('',#1250,.T.);
#589=FACE_OUTER_BOUND('',#1251,.T.);
#590=FACE_OUTER_BOUND('',#1252,.T.);
#591=FACE_OUTER_BOUND('',#1253,.T.);
#592=FACE_OUTER_BOUND('',#1254,.T.);
#593=FACE_OUTER_BOUND('',#1255,.T.);
#594=FACE_OUTER_BOUND('',#1256,.T.);
#595=FACE_OUTER_BOUND('',#1257,.T.);
#596=FACE_OUTER_BOUND('',#1258,.T.);
#597=FACE_OUTER_BOUND('',#1259,.T.);
#598=FACE_OUTER_BOUND('',#1260,.T.);
#599=FACE_OUTER_BOUND('',#1261,.T.);
#600=FACE_OUTER_BOUND('',#1262,.T.);
#601=FACE_OUTER_BOUND('',#1263,.T.);
#602=FACE_OUTER_BOUND('',#1264,.T.);
#603=FACE_OUTER_BOUND('',#1265,.T.);
#604=FACE_OUTER_BOUND('',#1266,.T.);
#605=FACE_OUTER_BOUND('',#1267,.T.);
#606=FACE_OUTER_BOUND('',#1268,.T.);
#607=FACE_OUTER_BOUND('',#1269,.T.);
#608=FACE_OUTER_BOUND('',#1270,.T.);
#609=FACE_OUTER_BOUND('',#1271,.T.);
#610=FACE_OUTER_BOUND('',#1272,.T.);
#611=FACE_OUTER_BOUND('',#1273,.T.);
#612=FACE_OUTER_BOUND('',#1274,.T.);
#613=FACE_OUTER_BOUND('',#1275,.T.);
#614=FACE_OUTER_BOUND('',#1276,.T.);
#615=FACE_OUTER_BOUND('',#1277,.T.);
#616=FACE_OUTER_BOUND('',#1278,.T.);
#617=FACE_OUTER_BOUND('',#1279,.T.);
#618=FACE_OUTER_BOUND('',#1280,.T.);
#619=FACE_OUTER_BOUND('',#1281,.T.);
#620=FACE_OUTER_BOUND('',#1282,.T.);
#621=FACE_OUTER_BOUND('',#1283,.T.);
#622=FACE_OUTER_BOUND('',#1284,.T.);
#623=FACE_OUTER_BOUND('',#1285,.T.);
#624=FACE_OUTER_BOUND('',#1286,.T.);
#625=FACE_OUTER_BOUND('',#1287,.T.);
#626=FACE_OUTER_BOUND('',#1288,.T.);
#627=FACE_OUTER_BOUND('',#1289,.T.);
#628=FACE_OUTER_BOUND('',#1290,.T.);
#629=FACE_OUTER_BOUND('',#1291,.T.);
#630=FACE_OUTER_BOUND('',#1292,.T.);
#631=FACE_OUTER_BOUND('',#1293,.T.);
#632=FACE_OUTER_BOUND('',#1294,.T.);
#633=FACE_OUTER_BOUND('',#1295,.T.);
#634=FACE_OUTER_BOUND('',#1296,.T.);
#635=FACE_OUTER_BOUND('',#1297,.T.);
#636=FACE_OUTER_BOUND('',#1298,.T.);
#637=FACE_OUTER_BOUND('',#1299,.T.);
#638=FACE_OUTER_BOUND('',#1300,.T.);
#639=FACE_OUTER_BOUND('',#1301,.T.);
#640=FACE_OUTER_BOUND('',#1302,.T.);
#641=FACE_OUTER_BOUND('',#1303,.T.);
#642=FACE_OUTER_BOUND('',#1304,.T.);
#643=FACE_OUTER_BOUND('',#1305,.T.);
#644=FACE_OUTER_BOUND('',#1306,.T.);
#645=FACE_OUTER_BOUND('',#1307,.T.);
#646=FACE_OUTER_BOUND('',#1308,.T.);
#647=FACE_OUTER_BOUND('',#1309,.T.);
#648=FACE_OUTER_BOUND('',#1310,.T.);
#649=FACE_OUTER_BOUND('',#1311,.T.);
#650=FACE_OUTER_BOUND('',#1312,.T.);
#651=FACE_OUTER_BOUND('',#1313,.T.);
#652=FACE_OUTER_BOUND('',#1314,.T.);
#653=FACE_OUTER_BOUND('',#1315,.T.);
#654=FACE_OUTER_BOUND('',#1316,.T.);
#655=FACE_OUTER_BOUND('',#1317,.T.);
#656=FACE_OUTER_BOUND('',#1318,.T.);
#657=FACE_OUTER_BOUND('',#1319,.T.);
#658=FACE_OUTER_BOUND('',#1320,.T.);
#659=FACE_OUTER_BOUND('',#1321,.T.);
#660=FACE_OUTER_BOUND('',#1322,.T.);
#661=FACE_OUTER_BOUND('',#1323,.T.);
#662=FACE_OUTER_BOUND('',#1324,.T.);
#663=FACE_OUTER_BOUND('',#1325,.T.);
#664=FACE_OUTER_BOUND('',#1326,.T.);
#665=FACE_OUTER_BOUND('',#1327,.T.);
#666=FACE_OUTER_BOUND('',#1328,.T.);
#667=FACE_OUTER_BOUND('',#1329,.T.);
#668=FACE_OUTER_BOUND('',#1330,.T.);
#669=FACE_OUTER_BOUND('',#1331,.T.);
#670=FACE_OUTER_BOUND('',#1332,.T.);
#671=FACE_OUTER_BOUND('',#1333,.T.);
#672=FACE_OUTER_BOUND('',#1334,.T.);
#673=FACE_OUTER_BOUND('',#1335,.T.);
#674=FACE_OUTER_BOUND('',#1336,.T.);
#675=FACE_OUTER_BOUND('',#1337,.T.);
#676=FACE_OUTER_BOUND('',#1338,.T.);
#677=FACE_OUTER_BOUND('',#1339,.T.);
#678=FACE_OUTER_BOUND('',#1340,.T.);
#679=FACE_OUTER_BOUND('',#1341,.T.);
#680=FACE_OUTER_BOUND('',#1342,.T.);
#681=FACE_OUTER_BOUND('',#1343,.T.);
#682=FACE_OUTER_BOUND('',#1344,.T.);
#683=FACE_OUTER_BOUND('',#1345,.T.);
#684=FACE_OUTER_BOUND('',#1346,.T.);
#685=FACE_OUTER_BOUND('',#1347,.T.);
#686=FACE_OUTER_BOUND('',#1348,.T.);
#687=FACE_OUTER_BOUND('',#1349,.T.);
#688=FACE_OUTER_BOUND('',#1350,.T.);
#689=FACE_OUTER_BOUND('',#1351,.T.);
#690=FACE_OUTER_BOUND('',#1352,.T.);
#691=FACE_OUTER_BOUND('',#1353,.T.);
#692=FACE_OUTER_BOUND('',#1354,.T.);
#693=FACE_OUTER_BOUND('',#1355,.T.);
#694=FACE_OUTER_BOUND('',#1356,.T.);
#695=FACE_OUTER_BOUND('',#1357,.T.);
#696=FACE_OUTER_BOUND('',#1358,.T.);
#697=FACE_OUTER_BOUND('',#1359,.T.);
#698=FACE_OUTER_BOUND('',#1360,.T.);
#699=FACE_OUTER_BOUND('',#1361,.T.);
#700=FACE_OUTER_BOUND('',#1362,.T.);
#701=FACE_OUTER_BOUND('',#1363,.T.);
#702=FACE_OUTER_BOUND('',#1364,.T.);
#703=FACE_OUTER_BOUND('',#1365,.T.);
#704=FACE_OUTER_BOUND('',#1366,.T.);
#705=FACE_OUTER_BOUND('',#1367,.T.);
#706=FACE_OUTER_BOUND('',#1368,.T.);
#707=FACE_OUTER_BOUND('',#1369,.T.);
#708=FACE_OUTER_BOUND('',#1370,.T.);
#709=FACE_OUTER_BOUND('',#1371,.T.);
#710=FACE_OUTER_BOUND('',#1372,.T.);
#711=FACE_OUTER_BOUND('',#1373,.T.);
#712=FACE_OUTER_BOUND('',#1374,.T.);
#713=FACE_OUTER_BOUND('',#1375,.T.);
#714=FACE_OUTER_BOUND('',#1376,.T.);
#715=FACE_OUTER_BOUND('',#1377,.T.);
#716=FACE_OUTER_BOUND('',#1378,.T.);
#717=FACE_OUTER_BOUND('',#1379,.T.);
#718=FACE_OUTER_BOUND('',#1380,.T.);
#719=FACE_OUTER_BOUND('',#1381,.T.);
#720=FACE_OUTER_BOUND('',#1382,.T.);
#721=FACE_OUTER_BOUND('',#1383,.T.);
#722=FACE_OUTER_BOUND('',#1384,.T.);
#723=FACE_OUTER_BOUND('',#1385,.T.);
#724=FACE_OUTER_BOUND('',#1386,.T.);
#725=FACE_OUTER_BOUND('',#1387,.T.);
#726=FACE_OUTER_BOUND('',#1388,.T.);
#727=FACE_OUTER_BOUND('',#1389,.T.);
#728=FACE_OUTER_BOUND('',#1390,.T.);
#729=FACE_OUTER_BOUND('',#1391,.T.);
#730=FACE_OUTER_BOUND('',#1392,.T.);
#731=FACE_OUTER_BOUND('',#1393,.T.);
#732=FACE_OUTER_BOUND('',#1394,.T.);
#733=FACE_OUTER_BOUND('',#1395,.T.);
#734=FACE_OUTER_BOUND('',#1396,.T.);
#735=FACE_OUTER_BOUND('',#1397,.T.);
#736=FACE_OUTER_BOUND('',#1398,.T.);
#737=FACE_OUTER_BOUND('',#1399,.T.);
#738=FACE_OUTER_BOUND('',#1400,.T.);
#739=FACE_OUTER_BOUND('',#1401,.T.);
#740=FACE_OUTER_BOUND('',#1402,.T.);
#741=FACE_OUTER_BOUND('',#1403,.T.);
#742=FACE_OUTER_BOUND('',#1404,.T.);
#743=FACE_OUTER_BOUND('',#1405,.T.);
#744=FACE_OUTER_BOUND('',#1406,.T.);
#745=FACE_OUTER_BOUND('',#1407,.T.);
#746=FACE_OUTER_BOUND('',#1408,.T.);
#747=FACE_OUTER_BOUND('',#1409,.T.);
#748=FACE_OUTER_BOUND('',#1410,.T.);
#749=FACE_OUTER_BOUND('',#1411,.T.);
#750=FACE_OUTER_BOUND('',#1412,.T.);
#751=FACE_OUTER_BOUND('',#1413,.T.);
#752=FACE_OUTER_BOUND('',#1415,.T.);
#753=FACE_OUTER_BOUND('',#1421,.T.);
#754=FACE_OUTER_BOUND('',#1422,.T.);
#755=FACE_OUTER_BOUND('',#1423,.T.);
#756=FACE_OUTER_BOUND('',#1424,.T.);
#757=FACE_OUTER_BOUND('',#1425,.T.);
#758=FACE_OUTER_BOUND('',#1430,.T.);
#759=FACE_OUTER_BOUND('',#1431,.T.);
#760=FACE_OUTER_BOUND('',#1433,.T.);
#761=FACE_OUTER_BOUND('',#1434,.T.);
#762=FACE_OUTER_BOUND('',#1440,.T.);
#763=FACE_OUTER_BOUND('',#1444,.T.);
#764=FACE_OUTER_BOUND('',#1445,.T.);
#765=FACE_OUTER_BOUND('',#1446,.T.);
#766=FACE_OUTER_BOUND('',#1447,.T.);
#767=FACE_OUTER_BOUND('',#1448,.T.);
#768=FACE_OUTER_BOUND('',#1449,.T.);
#769=FACE_OUTER_BOUND('',#1450,.T.);
#770=FACE_OUTER_BOUND('',#1451,.T.);
#771=FACE_OUTER_BOUND('',#1452,.T.);
#772=FACE_OUTER_BOUND('',#1453,.T.);
#773=FACE_OUTER_BOUND('',#1454,.T.);
#774=FACE_OUTER_BOUND('',#1455,.T.);
#775=FACE_OUTER_BOUND('',#1456,.T.);
#776=FACE_OUTER_BOUND('',#1457,.T.);
#777=FACE_OUTER_BOUND('',#1458,.T.);
#778=FACE_OUTER_BOUND('',#1459,.T.);
#779=FACE_OUTER_BOUND('',#1460,.T.);
#780=FACE_OUTER_BOUND('',#1461,.T.);
#781=FACE_OUTER_BOUND('',#1462,.T.);
#782=FACE_OUTER_BOUND('',#1463,.T.);
#783=FACE_OUTER_BOUND('',#1464,.T.);
#784=FACE_OUTER_BOUND('',#1465,.T.);
#785=FACE_OUTER_BOUND('',#1466,.T.);
#786=FACE_OUTER_BOUND('',#1467,.T.);
#787=FACE_OUTER_BOUND('',#1468,.T.);
#788=FACE_OUTER_BOUND('',#1469,.T.);
#789=FACE_OUTER_BOUND('',#1470,.T.);
#790=FACE_OUTER_BOUND('',#1471,.T.);
#791=FACE_OUTER_BOUND('',#1472,.T.);
#792=FACE_OUTER_BOUND('',#1473,.T.);
#793=FACE_OUTER_BOUND('',#1474,.T.);
#794=FACE_OUTER_BOUND('',#1475,.T.);
#795=FACE_OUTER_BOUND('',#1476,.T.);
#796=FACE_OUTER_BOUND('',#1477,.T.);
#797=FACE_OUTER_BOUND('',#1478,.T.);
#798=FACE_OUTER_BOUND('',#1479,.T.);
#799=FACE_OUTER_BOUND('',#1480,.T.);
#800=FACE_OUTER_BOUND('',#1481,.T.);
#801=FACE_OUTER_BOUND('',#1482,.T.);
#802=FACE_OUTER_BOUND('',#1483,.T.);
#803=FACE_OUTER_BOUND('',#1484,.T.);
#804=FACE_OUTER_BOUND('',#1485,.T.);
#805=FACE_OUTER_BOUND('',#1486,.T.);
#806=FACE_OUTER_BOUND('',#1487,.T.);
#807=FACE_OUTER_BOUND('',#1488,.T.);
#808=FACE_OUTER_BOUND('',#1489,.T.);
#809=FACE_OUTER_BOUND('',#1490,.T.);
#810=FACE_OUTER_BOUND('',#1491,.T.);
#811=FACE_OUTER_BOUND('',#1492,.T.);
#812=FACE_OUTER_BOUND('',#1493,.T.);
#813=FACE_OUTER_BOUND('',#1494,.T.);
#814=FACE_OUTER_BOUND('',#1495,.T.);
#815=FACE_OUTER_BOUND('',#1496,.T.);
#816=FACE_OUTER_BOUND('',#1497,.T.);
#817=FACE_OUTER_BOUND('',#1498,.T.);
#818=FACE_OUTER_BOUND('',#1499,.T.);
#819=FACE_OUTER_BOUND('',#1500,.T.);
#820=FACE_OUTER_BOUND('',#1501,.T.);
#821=FACE_OUTER_BOUND('',#1503,.T.);
#822=FACE_OUTER_BOUND('',#1504,.T.);
#823=FACE_OUTER_BOUND('',#1505,.T.);
#824=FACE_OUTER_BOUND('',#1506,.T.);
#825=FACE_OUTER_BOUND('',#1507,.T.);
#826=FACE_OUTER_BOUND('',#1509,.T.);
#827=FACE_OUTER_BOUND('',#1510,.T.);
#828=FACE_OUTER_BOUND('',#1511,.T.);
#829=FACE_OUTER_BOUND('',#1512,.T.);
#830=FACE_OUTER_BOUND('',#1514,.T.);
#831=FACE_OUTER_BOUND('',#1515,.T.);
#832=FACE_OUTER_BOUND('',#1516,.T.);
#833=FACE_OUTER_BOUND('',#1518,.T.);
#834=FACE_OUTER_BOUND('',#1519,.T.);
#835=FACE_OUTER_BOUND('',#1520,.T.);
#836=FACE_OUTER_BOUND('',#1522,.T.);
#837=FACE_OUTER_BOUND('',#1523,.T.);
#838=FACE_OUTER_BOUND('',#1524,.T.);
#839=FACE_OUTER_BOUND('',#1525,.T.);
#840=FACE_OUTER_BOUND('',#1526,.T.);
#841=FACE_OUTER_BOUND('',#1530,.T.);
#842=FACE_OUTER_BOUND('',#1531,.T.);
#843=FACE_OUTER_BOUND('',#1532,.T.);
#844=FACE_OUTER_BOUND('',#1533,.T.);
#845=FACE_OUTER_BOUND('',#1534,.T.);
#846=FACE_OUTER_BOUND('',#1537,.T.);
#847=FACE_OUTER_BOUND('',#1538,.T.);
#848=FACE_OUTER_BOUND('',#1539,.T.);
#849=FACE_OUTER_BOUND('',#1540,.T.);
#850=FACE_OUTER_BOUND('',#1541,.T.);
#851=FACE_OUTER_BOUND('',#1542,.T.);
#852=FACE_OUTER_BOUND('',#1543,.T.);
#853=FACE_OUTER_BOUND('',#1544,.T.);
#854=FACE_OUTER_BOUND('',#1550,.T.);
#855=FACE_OUTER_BOUND('',#1551,.T.);
#856=FACE_OUTER_BOUND('',#1552,.T.);
#857=FACE_OUTER_BOUND('',#1553,.T.);
#858=FACE_OUTER_BOUND('',#1554,.T.);
#859=FACE_OUTER_BOUND('',#1555,.T.);
#860=FACE_OUTER_BOUND('',#1556,.T.);
#861=FACE_OUTER_BOUND('',#1557,.T.);
#862=FACE_OUTER_BOUND('',#1563,.T.);
#863=FACE_OUTER_BOUND('',#1564,.T.);
#864=FACE_OUTER_BOUND('',#1565,.T.);
#865=FACE_OUTER_BOUND('',#1567,.T.);
#866=FACE_OUTER_BOUND('',#1569,.T.);
#867=FACE_OUTER_BOUND('',#1570,.T.);
#868=FACE_OUTER_BOUND('',#1571,.T.);
#869=FACE_OUTER_BOUND('',#1572,.T.);
#870=FACE_OUTER_BOUND('',#1573,.T.);
#871=FACE_OUTER_BOUND('',#1574,.T.);
#872=FACE_OUTER_BOUND('',#1575,.T.);
#873=FACE_OUTER_BOUND('',#1576,.T.);
#874=FACE_OUTER_BOUND('',#1577,.T.);
#875=FACE_OUTER_BOUND('',#1578,.T.);
#876=FACE_OUTER_BOUND('',#1579,.T.);
#877=FACE_OUTER_BOUND('',#1580,.T.);
#878=FACE_OUTER_BOUND('',#1581,.T.);
#879=FACE_OUTER_BOUND('',#1582,.T.);
#880=FACE_OUTER_BOUND('',#1583,.T.);
#881=FACE_OUTER_BOUND('',#1584,.T.);
#882=FACE_OUTER_BOUND('',#1585,.T.);
#883=FACE_OUTER_BOUND('',#1586,.T.);
#884=FACE_OUTER_BOUND('',#1587,.T.);
#885=FACE_OUTER_BOUND('',#1588,.T.);
#886=FACE_OUTER_BOUND('',#1589,.T.);
#887=FACE_OUTER_BOUND('',#1590,.T.);
#888=FACE_OUTER_BOUND('',#1591,.T.);
#889=FACE_OUTER_BOUND('',#1592,.T.);
#890=FACE_OUTER_BOUND('',#1593,.T.);
#891=FACE_OUTER_BOUND('',#1594,.T.);
#892=FACE_OUTER_BOUND('',#1595,.T.);
#893=FACE_OUTER_BOUND('',#1596,.T.);
#894=FACE_OUTER_BOUND('',#1597,.T.);
#895=FACE_OUTER_BOUND('',#1598,.T.);
#896=FACE_OUTER_BOUND('',#1599,.T.);
#897=FACE_OUTER_BOUND('',#1600,.T.);
#898=FACE_OUTER_BOUND('',#1601,.T.);
#899=FACE_OUTER_BOUND('',#1602,.T.);
#900=FACE_OUTER_BOUND('',#1603,.T.);
#901=FACE_OUTER_BOUND('',#1604,.T.);
#902=FACE_OUTER_BOUND('',#1605,.T.);
#903=FACE_OUTER_BOUND('',#1606,.T.);
#904=FACE_OUTER_BOUND('',#1607,.T.);
#905=FACE_OUTER_BOUND('',#1608,.T.);
#906=FACE_OUTER_BOUND('',#1609,.T.);
#907=FACE_OUTER_BOUND('',#1610,.T.);
#908=FACE_OUTER_BOUND('',#1611,.T.);
#909=FACE_OUTER_BOUND('',#1612,.T.);
#910=FACE_OUTER_BOUND('',#1613,.T.);
#911=FACE_OUTER_BOUND('',#1614,.T.);
#912=FACE_OUTER_BOUND('',#1615,.T.);
#913=FACE_OUTER_BOUND('',#1616,.T.);
#914=FACE_OUTER_BOUND('',#1617,.T.);
#915=FACE_OUTER_BOUND('',#1618,.T.);
#916=FACE_OUTER_BOUND('',#1619,.T.);
#917=FACE_OUTER_BOUND('',#1620,.T.);
#918=FACE_OUTER_BOUND('',#1621,.T.);
#919=FACE_OUTER_BOUND('',#1622,.T.);
#920=FACE_OUTER_BOUND('',#1623,.T.);
#921=FACE_OUTER_BOUND('',#1624,.T.);
#922=FACE_OUTER_BOUND('',#1625,.T.);
#923=FACE_OUTER_BOUND('',#1626,.T.);
#924=FACE_OUTER_BOUND('',#1627,.T.);
#925=FACE_OUTER_BOUND('',#1628,.T.);
#926=FACE_OUTER_BOUND('',#1629,.T.);
#927=FACE_OUTER_BOUND('',#1630,.T.);
#928=FACE_OUTER_BOUND('',#1631,.T.);
#929=FACE_OUTER_BOUND('',#1632,.T.);
#930=FACE_OUTER_BOUND('',#1633,.T.);
#931=FACE_OUTER_BOUND('',#1634,.T.);
#932=FACE_OUTER_BOUND('',#1635,.T.);
#933=FACE_OUTER_BOUND('',#1636,.T.);
#934=FACE_OUTER_BOUND('',#1637,.T.);
#935=FACE_OUTER_BOUND('',#1638,.T.);
#936=FACE_OUTER_BOUND('',#1639,.T.);
#937=FACE_OUTER_BOUND('',#1640,.T.);
#938=FACE_OUTER_BOUND('',#1642,.T.);
#939=FACE_OUTER_BOUND('',#1643,.T.);
#940=FACE_OUTER_BOUND('',#1645,.T.);
#941=FACE_OUTER_BOUND('',#1647,.T.);
#942=FACE_OUTER_BOUND('',#1648,.T.);
#943=FACE_OUTER_BOUND('',#1649,.T.);
#944=FACE_OUTER_BOUND('',#1650,.T.);
#945=FACE_OUTER_BOUND('',#1651,.T.);
#946=FACE_OUTER_BOUND('',#1652,.T.);
#947=FACE_OUTER_BOUND('',#1653,.T.);
#948=FACE_OUTER_BOUND('',#1654,.T.);
#949=FACE_OUTER_BOUND('',#1655,.T.);
#950=FACE_OUTER_BOUND('',#1656,.T.);
#951=FACE_OUTER_BOUND('',#1658,.T.);
#952=FACE_OUTER_BOUND('',#1660,.T.);
#953=FACE_OUTER_BOUND('',#1662,.T.);
#954=FACE_OUTER_BOUND('',#1663,.T.);
#955=FACE_OUTER_BOUND('',#1671,.T.);
#956=FACE_OUTER_BOUND('',#1679,.T.);
#957=FACE_OUTER_BOUND('',#1680,.T.);
#958=FACE_OUTER_BOUND('',#1682,.T.);
#959=FACE_OUTER_BOUND('',#1684,.T.);
#960=FACE_OUTER_BOUND('',#1685,.T.);
#961=FACE_OUTER_BOUND('',#1687,.T.);
#962=FACE_OUTER_BOUND('',#1688,.T.);
#963=FACE_OUTER_BOUND('',#1689,.T.);
#964=FACE_OUTER_BOUND('',#1690,.T.);
#965=FACE_OUTER_BOUND('',#1691,.T.);
#966=FACE_OUTER_BOUND('',#1692,.T.);
#967=FACE_OUTER_BOUND('',#1693,.T.);
#968=FACE_OUTER_BOUND('',#1695,.T.);
#969=FACE_OUTER_BOUND('',#1697,.T.);
#970=FACE_OUTER_BOUND('',#1698,.T.);
#971=FACE_OUTER_BOUND('',#1699,.T.);
#972=FACE_OUTER_BOUND('',#1700,.T.);
#973=FACE_OUTER_BOUND('',#1701,.T.);
#974=FACE_OUTER_BOUND('',#1702,.T.);
#975=FACE_OUTER_BOUND('',#1703,.T.);
#976=FACE_OUTER_BOUND('',#1704,.T.);
#977=FACE_OUTER_BOUND('',#1705,.T.);
#978=FACE_OUTER_BOUND('',#1707,.T.);
#979=FACE_OUTER_BOUND('',#1709,.T.);
#980=FACE_OUTER_BOUND('',#1710,.T.);
#981=FACE_OUTER_BOUND('',#1711,.T.);
#982=FACE_OUTER_BOUND('',#1712,.T.);
#983=FACE_OUTER_BOUND('',#1713,.T.);
#984=FACE_OUTER_BOUND('',#1714,.T.);
#985=FACE_OUTER_BOUND('',#1715,.T.);
#986=FACE_OUTER_BOUND('',#1716,.T.);
#987=FACE_OUTER_BOUND('',#1717,.T.);
#988=FACE_OUTER_BOUND('',#1718,.T.);
#989=FACE_OUTER_BOUND('',#1719,.T.);
#990=FACE_OUTER_BOUND('',#1720,.T.);
#991=FACE_OUTER_BOUND('',#1721,.T.);
#992=FACE_OUTER_BOUND('',#1722,.T.);
#993=FACE_OUTER_BOUND('',#1723,.T.);
#994=FACE_OUTER_BOUND('',#1724,.T.);
#995=FACE_OUTER_BOUND('',#1725,.T.);
#996=FACE_OUTER_BOUND('',#1726,.T.);
#997=FACE_OUTER_BOUND('',#1727,.T.);
#998=FACE_OUTER_BOUND('',#1728,.T.);
#999=FACE_OUTER_BOUND('',#1729,.T.);
#1000=FACE_OUTER_BOUND('',#1730,.T.);
#1001=FACE_OUTER_BOUND('',#1731,.T.);
#1002=FACE_OUTER_BOUND('',#1732,.T.);
#1003=FACE_OUTER_BOUND('',#1733,.T.);
#1004=FACE_OUTER_BOUND('',#1734,.T.);
#1005=FACE_OUTER_BOUND('',#1735,.T.);
#1006=FACE_OUTER_BOUND('',#1736,.T.);
#1007=FACE_OUTER_BOUND('',#1737,.T.);
#1008=FACE_OUTER_BOUND('',#1738,.T.);
#1009=FACE_OUTER_BOUND('',#1740,.T.);
#1010=FACE_OUTER_BOUND('',#1741,.T.);
#1011=FACE_OUTER_BOUND('',#1743,.T.);
#1012=FACE_OUTER_BOUND('',#1744,.T.);
#1013=FACE_OUTER_BOUND('',#1745,.T.);
#1014=FACE_OUTER_BOUND('',#1746,.T.);
#1015=FACE_OUTER_BOUND('',#1747,.T.);
#1016=FACE_OUTER_BOUND('',#1748,.T.);
#1017=FACE_OUTER_BOUND('',#1749,.T.);
#1018=FACE_OUTER_BOUND('',#1750,.T.);
#1019=FACE_OUTER_BOUND('',#1751,.T.);
#1020=FACE_OUTER_BOUND('',#1752,.T.);
#1021=FACE_OUTER_BOUND('',#1753,.T.);
#1022=FACE_OUTER_BOUND('',#1754,.T.);
#1023=FACE_OUTER_BOUND('',#1755,.T.);
#1024=FACE_OUTER_BOUND('',#1756,.T.);
#1025=FACE_OUTER_BOUND('',#1757,.T.);
#1026=FACE_OUTER_BOUND('',#1758,.T.);
#1027=FACE_OUTER_BOUND('',#1759,.T.);
#1028=FACE_OUTER_BOUND('',#1760,.T.);
#1029=FACE_OUTER_BOUND('',#1761,.T.);
#1030=FACE_OUTER_BOUND('',#1762,.T.);
#1031=FACE_OUTER_BOUND('',#1763,.T.);
#1032=FACE_OUTER_BOUND('',#1764,.T.);
#1033=FACE_OUTER_BOUND('',#1765,.T.);
#1034=FACE_OUTER_BOUND('',#1766,.T.);
#1035=FACE_OUTER_BOUND('',#1767,.T.);
#1036=FACE_OUTER_BOUND('',#1768,.T.);
#1037=FACE_OUTER_BOUND('',#1769,.T.);
#1038=FACE_OUTER_BOUND('',#1770,.T.);
#1039=FACE_OUTER_BOUND('',#1771,.T.);
#1040=FACE_OUTER_BOUND('',#1772,.T.);
#1041=FACE_OUTER_BOUND('',#1773,.T.);
#1042=FACE_OUTER_BOUND('',#1774,.T.);
#1043=FACE_OUTER_BOUND('',#1775,.T.);
#1044=FACE_OUTER_BOUND('',#1776,.T.);
#1045=FACE_OUTER_BOUND('',#1777,.T.);
#1046=FACE_OUTER_BOUND('',#1778,.T.);
#1047=FACE_OUTER_BOUND('',#1779,.T.);
#1048=FACE_OUTER_BOUND('',#1780,.T.);
#1049=FACE_OUTER_BOUND('',#1781,.T.);
#1050=FACE_OUTER_BOUND('',#1782,.T.);
#1051=FACE_OUTER_BOUND('',#1783,.T.);
#1052=FACE_OUTER_BOUND('',#1784,.T.);
#1053=FACE_OUTER_BOUND('',#1785,.T.);
#1054=FACE_OUTER_BOUND('',#1787,.T.);
#1055=FACE_OUTER_BOUND('',#1788,.T.);
#1056=FACE_OUTER_BOUND('',#1790,.T.);
#1057=FACE_OUTER_BOUND('',#1791,.T.);
#1058=FACE_OUTER_BOUND('',#1792,.T.);
#1059=FACE_OUTER_BOUND('',#1793,.T.);
#1060=FACE_OUTER_BOUND('',#1794,.T.);
#1061=FACE_OUTER_BOUND('',#1795,.T.);
#1062=FACE_OUTER_BOUND('',#1796,.T.);
#1063=FACE_OUTER_BOUND('',#1797,.T.);
#1064=FACE_OUTER_BOUND('',#1798,.T.);
#1065=FACE_OUTER_BOUND('',#1799,.T.);
#1066=FACE_OUTER_BOUND('',#1800,.T.);
#1067=FACE_OUTER_BOUND('',#1801,.T.);
#1068=FACE_OUTER_BOUND('',#1802,.T.);
#1069=FACE_OUTER_BOUND('',#1803,.T.);
#1070=FACE_OUTER_BOUND('',#1805,.T.);
#1071=FACE_OUTER_BOUND('',#1806,.T.);
#1072=FACE_OUTER_BOUND('',#1808,.T.);
#1073=EDGE_LOOP('',(#10161,#10162,#10163,#10164,#10165,#10166));
#1074=EDGE_LOOP('',(#10167,#10168,#10169,#10170,#10171,#10172));
#1075=EDGE_LOOP('',(#10173,#10174,#10175,#10176,#10177,#10178));
#1076=EDGE_LOOP('',(#10179,#10180,#10181,#10182,#10183,#10184));
#1077=EDGE_LOOP('',(#10185,#10186,#10187,#10188,#10189,#10190));
#1078=EDGE_LOOP('',(#10191,#10192,#10193,#10194,#10195,#10196));
#1079=EDGE_LOOP('',(#10197,#10198,#10199,#10200,#10201,#10202));
#1080=EDGE_LOOP('',(#10203,#10204,#10205,#10206,#10207,#10208));
#1081=EDGE_LOOP('',(#10209,#10210,#10211,#10212,#10213,#10214));
#1082=EDGE_LOOP('',(#10215,#10216,#10217,#10218,#10219,#10220));
#1083=EDGE_LOOP('',(#10221,#10222,#10223,#10224,#10225,#10226,#10227,#10228));
#1084=EDGE_LOOP('',(#10229,#10230,#10231,#10232,#10233));
#1085=EDGE_LOOP('',(#10234,#10235,#10236,#10237,#10238));
#1086=EDGE_LOOP('',(#10239,#10240,#10241,#10242,#10243));
#1087=EDGE_LOOP('',(#10244,#10245,#10246,#10247,#10248));
#1088=EDGE_LOOP('',(#10249,#10250,#10251,#10252,#10253));
#1089=EDGE_LOOP('',(#10254,#10255,#10256,#10257,#10258));
#1090=EDGE_LOOP('',(#10259,#10260,#10261,#10262,#10263));
#1091=EDGE_LOOP('',(#10264,#10265,#10266,#10267,#10268));
#1092=EDGE_LOOP('',(#10269,#10270,#10271,#10272));
#1093=EDGE_LOOP('',(#10273,#10274,#10275,#10276,#10277,#10278));
#1094=EDGE_LOOP('',(#10279,#10280,#10281,#10282,#10283,#10284));
#1095=EDGE_LOOP('',(#10285,#10286,#10287,#10288,#10289,#10290));
#1096=EDGE_LOOP('',(#10291,#10292,#10293,#10294,#10295,#10296));
#1097=EDGE_LOOP('',(#10297,#10298,#10299,#10300,#10301,#10302));
#1098=EDGE_LOOP('',(#10303,#10304,#10305,#10306,#10307,#10308));
#1099=EDGE_LOOP('',(#10309,#10310,#10311,#10312,#10313,#10314));
#1100=EDGE_LOOP('',(#10315,#10316,#10317,#10318,#10319,#10320));
#1101=EDGE_LOOP('',(#10321,#10322,#10323,#10324,#10325,#10326));
#1102=EDGE_LOOP('',(#10327,#10328,#10329,#10330,#10331,#10332));
#1103=EDGE_LOOP('',(#10333,#10334,#10335,#10336,#10337,#10338,#10339,#10340));
#1104=EDGE_LOOP('',(#10341,#10342,#10343,#10344,#10345));
#1105=EDGE_LOOP('',(#10346,#10347,#10348,#10349,#10350));
#1106=EDGE_LOOP('',(#10351,#10352,#10353,#10354,#10355));
#1107=EDGE_LOOP('',(#10356,#10357,#10358,#10359,#10360));
#1108=EDGE_LOOP('',(#10361,#10362,#10363,#10364,#10365));
#1109=EDGE_LOOP('',(#10366,#10367,#10368,#10369,#10370));
#1110=EDGE_LOOP('',(#10371,#10372,#10373,#10374,#10375));
#1111=EDGE_LOOP('',(#10376,#10377,#10378,#10379,#10380));
#1112=EDGE_LOOP('',(#10381,#10382,#10383,#10384));
#1113=EDGE_LOOP('',(#10385,#10386,#10387,#10388,#10389,#10390));
#1114=EDGE_LOOP('',(#10391,#10392,#10393,#10394,#10395,#10396));
#1115=EDGE_LOOP('',(#10397,#10398,#10399,#10400,#10401,#10402));
#1116=EDGE_LOOP('',(#10403,#10404,#10405,#10406,#10407,#10408));
#1117=EDGE_LOOP('',(#10409,#10410,#10411,#10412,#10413,#10414));
#1118=EDGE_LOOP('',(#10415,#10416,#10417,#10418,#10419,#10420));
#1119=EDGE_LOOP('',(#10421,#10422,#10423,#10424,#10425,#10426));
#1120=EDGE_LOOP('',(#10427,#10428,#10429,#10430,#10431,#10432));
#1121=EDGE_LOOP('',(#10433,#10434,#10435,#10436,#10437,#10438));
#1122=EDGE_LOOP('',(#10439,#10440,#10441,#10442,#10443,#10444));
#1123=EDGE_LOOP('',(#10445,#10446,#10447,#10448,#10449,#10450,#10451,#10452));
#1124=EDGE_LOOP('',(#10453,#10454,#10455,#10456,#10457));
#1125=EDGE_LOOP('',(#10458,#10459,#10460,#10461,#10462));
#1126=EDGE_LOOP('',(#10463,#10464,#10465,#10466,#10467));
#1127=EDGE_LOOP('',(#10468,#10469,#10470,#10471,#10472));
#1128=EDGE_LOOP('',(#10473,#10474,#10475,#10476,#10477));
#1129=EDGE_LOOP('',(#10478,#10479,#10480,#10481,#10482));
#1130=EDGE_LOOP('',(#10483,#10484,#10485,#10486,#10487));
#1131=EDGE_LOOP('',(#10488,#10489,#10490,#10491,#10492));
#1132=EDGE_LOOP('',(#10493,#10494,#10495,#10496));
#1133=EDGE_LOOP('',(#10497,#10498,#10499,#10500,#10501,#10502));
#1134=EDGE_LOOP('',(#10503,#10504,#10505,#10506,#10507,#10508));
#1135=EDGE_LOOP('',(#10509,#10510,#10511,#10512,#10513,#10514));
#1136=EDGE_LOOP('',(#10515,#10516,#10517,#10518,#10519,#10520));
#1137=EDGE_LOOP('',(#10521,#10522,#10523,#10524,#10525,#10526));
#1138=EDGE_LOOP('',(#10527,#10528,#10529,#10530,#10531,#10532));
#1139=EDGE_LOOP('',(#10533,#10534,#10535,#10536,#10537,#10538));
#1140=EDGE_LOOP('',(#10539,#10540,#10541,#10542,#10543,#10544));
#1141=EDGE_LOOP('',(#10545,#10546,#10547,#10548,#10549,#10550));
#1142=EDGE_LOOP('',(#10551,#10552,#10553,#10554,#10555,#10556));
#1143=EDGE_LOOP('',(#10557,#10558,#10559,#10560,#10561,#10562,#10563,#10564));
#1144=EDGE_LOOP('',(#10565,#10566,#10567,#10568,#10569));
#1145=EDGE_LOOP('',(#10570,#10571,#10572,#10573,#10574));
#1146=EDGE_LOOP('',(#10575,#10576,#10577,#10578,#10579));
#1147=EDGE_LOOP('',(#10580,#10581,#10582,#10583,#10584));
#1148=EDGE_LOOP('',(#10585,#10586,#10587,#10588,#10589));
#1149=EDGE_LOOP('',(#10590,#10591,#10592,#10593,#10594));
#1150=EDGE_LOOP('',(#10595,#10596,#10597,#10598,#10599));
#1151=EDGE_LOOP('',(#10600,#10601,#10602,#10603,#10604));
#1152=EDGE_LOOP('',(#10605,#10606,#10607,#10608));
#1153=EDGE_LOOP('',(#10609,#10610,#10611,#10612,#10613,#10614));
#1154=EDGE_LOOP('',(#10615,#10616,#10617,#10618,#10619,#10620));
#1155=EDGE_LOOP('',(#10621,#10622,#10623,#10624,#10625,#10626));
#1156=EDGE_LOOP('',(#10627,#10628,#10629,#10630,#10631,#10632));
#1157=EDGE_LOOP('',(#10633,#10634,#10635,#10636,#10637,#10638));
#1158=EDGE_LOOP('',(#10639,#10640,#10641,#10642,#10643,#10644));
#1159=EDGE_LOOP('',(#10645,#10646,#10647,#10648,#10649,#10650));
#1160=EDGE_LOOP('',(#10651,#10652,#10653,#10654,#10655,#10656));
#1161=EDGE_LOOP('',(#10657,#10658,#10659,#10660,#10661));
#1162=EDGE_LOOP('',(#10662,#10663,#10664,#10665,#10666,#10667,#10668,#10669,
#10670,#10671,#10672,#10673,#10674,#10675,#10676,#10677,#10678,#10679,#10680,
#10681,#10682,#10683,#10684,#10685,#10686,#10687,#10688,#10689,#10690,#10691,
#10692,#10693,#10694,#10695,#10696,#10697,#10698,#10699,#10700,#10701));
#1163=EDGE_LOOP('',(#10702,#10703,#10704,#10705,#10706,#10707,#10708,#10709,
#10710,#10711,#10712,#10713,#10714,#10715,#10716,#10717,#10718,#10719,#10720,
#10721,#10722,#10723,#10724,#10725,#10726,#10727,#10728,#10729,#10730,#10731,
#10732,#10733,#10734,#10735,#10736,#10737,#10738,#10739,#10740,#10741,#10742));
#1164=EDGE_LOOP('',(#10743,#10744,#10745,#10746,#10747));
#1165=EDGE_LOOP('',(#10748,#10749,#10750,#10751,#10752,#10753,#10754,#10755,
#10756,#10757,#10758,#10759,#10760,#10761,#10762,#10763,#10764,#10765,#10766,
#10767,#10768,#10769,#10770,#10771,#10772,#10773,#10774,#10775,#10776,#10777,
#10778,#10779,#10780,#10781,#10782,#10783,#10784,#10785,#10786,#10787));
#1166=EDGE_LOOP('',(#10788,#10789,#10790,#10791,#10792,#10793,#10794,#10795,
#10796,#10797,#10798,#10799,#10800,#10801,#10802,#10803,#10804,#10805,#10806,
#10807,#10808,#10809,#10810,#10811,#10812,#10813,#10814,#10815,#10816,#10817,
#10818,#10819,#10820,#10821,#10822,#10823,#10824,#10825,#10826,#10827,#10828));
#1167=EDGE_LOOP('',(#10829,#10830,#10831,#10832,#10833));
#1168=EDGE_LOOP('',(#10834,#10835,#10836,#10837,#10838,#10839,#10840,#10841,
#10842,#10843,#10844,#10845,#10846,#10847,#10848,#10849,#10850,#10851,#10852,
#10853,#10854,#10855,#10856,#10857,#10858,#10859,#10860,#10861,#10862,#10863,
#10864,#10865,#10866,#10867,#10868,#10869,#10870,#10871,#10872,#10873));
#1169=EDGE_LOOP('',(#10874,#10875,#10876,#10877,#10878,#10879,#10880,#10881,
#10882,#10883,#10884,#10885,#10886,#10887,#10888,#10889,#10890,#10891,#10892,
#10893,#10894,#10895,#10896,#10897,#10898,#10899,#10900,#10901,#10902,#10903,
#10904,#10905,#10906,#10907,#10908,#10909,#10910,#10911,#10912,#10913,#10914));
#1170=EDGE_LOOP('',(#10915,#10916,#10917,#10918,#10919));
#1171=EDGE_LOOP('',(#10920,#10921,#10922,#10923,#10924,#10925,#10926,#10927,
#10928,#10929,#10930,#10931,#10932,#10933,#10934,#10935,#10936,#10937,#10938,
#10939,#10940,#10941,#10942,#10943,#10944,#10945,#10946,#10947,#10948,#10949,
#10950,#10951,#10952,#10953,#10954,#10955,#10956,#10957,#10958,#10959));
#1172=EDGE_LOOP('',(#10960,#10961,#10962,#10963,#10964,#10965,#10966,#10967,
#10968,#10969,#10970,#10971,#10972,#10973,#10974,#10975,#10976,#10977,#10978,
#10979,#10980,#10981,#10982,#10983,#10984,#10985,#10986,#10987,#10988,#10989,
#10990,#10991,#10992,#10993,#10994,#10995,#10996,#10997,#10998,#10999,#11000));
#1173=EDGE_LOOP('',(#11001));
#1174=EDGE_LOOP('',(#11002));
#1175=EDGE_LOOP('',(#11003));
#1176=EDGE_LOOP('',(#11004));
#1177=EDGE_LOOP('',(#11005,#11006,#11007,#11008));
#1178=EDGE_LOOP('',(#11009,#11010,#11011,#11012));
#1179=EDGE_LOOP('',(#11013,#11014,#11015,#11016));
#1180=EDGE_LOOP('',(#11017,#11018,#11019,#11020));
#1181=EDGE_LOOP('',(#11021,#11022,#11023,#11024));
#1182=EDGE_LOOP('',(#11025,#11026,#11027,#11028));
#1183=EDGE_LOOP('',(#11029,#11030,#11031,#11032));
#1184=EDGE_LOOP('',(#11033,#11034,#11035,#11036));
#1185=EDGE_LOOP('',(#11037,#11038,#11039,#11040));
#1186=EDGE_LOOP('',(#11041,#11042,#11043,#11044,#11045));
#1187=EDGE_LOOP('',(#11046,#11047,#11048,#11049,#11050));
#1188=EDGE_LOOP('',(#11051));
#1189=EDGE_LOOP('',(#11052));
#1190=EDGE_LOOP('',(#11053));
#1191=EDGE_LOOP('',(#11054));
#1192=EDGE_LOOP('',(#11055,#11056,#11057,#11058,#11059));
#1193=EDGE_LOOP('',(#11060,#11061,#11062,#11063,#11064));
#1194=EDGE_LOOP('',(#11065,#11066,#11067,#11068));
#1195=EDGE_LOOP('',(#11069));
#1196=EDGE_LOOP('',(#11070));
#1197=EDGE_LOOP('',(#11071));
#1198=EDGE_LOOP('',(#11072));
#1199=EDGE_LOOP('',(#11073,#11074,#11075,#11076));
#1200=EDGE_LOOP('',(#11077,#11078,#11079,#11080,#11081,#11082));
#1201=EDGE_LOOP('',(#11083,#11084,#11085,#11086,#11087,#11088));
#1202=EDGE_LOOP('',(#11089,#11090,#11091,#11092,#11093,#11094));
#1203=EDGE_LOOP('',(#11095,#11096,#11097,#11098,#11099,#11100));
#1204=EDGE_LOOP('',(#11101,#11102,#11103,#11104,#11105,#11106));
#1205=EDGE_LOOP('',(#11107,#11108,#11109,#11110,#11111,#11112));
#1206=EDGE_LOOP('',(#11113,#11114,#11115,#11116,#11117,#11118));
#1207=EDGE_LOOP('',(#11119,#11120,#11121,#11122,#11123,#11124));
#1208=EDGE_LOOP('',(#11125,#11126,#11127,#11128,#11129,#11130));
#1209=EDGE_LOOP('',(#11131,#11132,#11133,#11134,#11135,#11136));
#1210=EDGE_LOOP('',(#11137,#11138,#11139,#11140,#11141,#11142));
#1211=EDGE_LOOP('',(#11143,#11144,#11145,#11146,#11147,#11148));
#1212=EDGE_LOOP('',(#11149,#11150,#11151,#11152,#11153,#11154));
#1213=EDGE_LOOP('',(#11155,#11156,#11157,#11158,#11159,#11160));
#1214=EDGE_LOOP('',(#11161,#11162,#11163,#11164,#11165,#11166));
#1215=EDGE_LOOP('',(#11167,#11168,#11169,#11170,#11171,#11172,#11173,#11174));
#1216=EDGE_LOOP('',(#11175,#11176,#11177,#11178,#11179));
#1217=EDGE_LOOP('',(#11180,#11181,#11182,#11183,#11184,#11185));
#1218=EDGE_LOOP('',(#11186,#11187,#11188,#11189));
#1219=EDGE_LOOP('',(#11190,#11191,#11192,#11193,#11194,#11195));
#1220=EDGE_LOOP('',(#11196,#11197,#11198,#11199));
#1221=EDGE_LOOP('',(#11200,#11201,#11202,#11203,#11204,#11205));
#1222=EDGE_LOOP('',(#11206,#11207,#11208,#11209));
#1223=EDGE_LOOP('',(#11210,#11211,#11212,#11213,#11214,#11215));
#1224=EDGE_LOOP('',(#11216,#11217,#11218,#11219));
#1225=EDGE_LOOP('',(#11220,#11221,#11222,#11223,#11224,#11225));
#1226=EDGE_LOOP('',(#11226,#11227,#11228,#11229));
#1227=EDGE_LOOP('',(#11230,#11231,#11232,#11233,#11234,#11235));
#1228=EDGE_LOOP('',(#11236,#11237,#11238,#11239));
#1229=EDGE_LOOP('',(#11240,#11241,#11242,#11243));
#1230=EDGE_LOOP('',(#11244,#11245,#11246,#11247));
#1231=EDGE_LOOP('',(#11248,#11249,#11250,#11251,#11252,#11253));
#1232=EDGE_LOOP('',(#11254,#11255,#11256,#11257,#11258,#11259));
#1233=EDGE_LOOP('',(#11260,#11261,#11262,#11263,#11264,#11265));
#1234=EDGE_LOOP('',(#11266,#11267,#11268,#11269,#11270,#11271));
#1235=EDGE_LOOP('',(#11272,#11273,#11274,#11275,#11276,#11277));
#1236=EDGE_LOOP('',(#11278,#11279,#11280,#11281,#11282,#11283));
#1237=EDGE_LOOP('',(#11284,#11285,#11286,#11287,#11288,#11289));
#1238=EDGE_LOOP('',(#11290,#11291,#11292,#11293,#11294,#11295));
#1239=EDGE_LOOP('',(#11296,#11297,#11298,#11299,#11300,#11301));
#1240=EDGE_LOOP('',(#11302,#11303,#11304,#11305,#11306,#11307));
#1241=EDGE_LOOP('',(#11308,#11309,#11310,#11311,#11312,#11313));
#1242=EDGE_LOOP('',(#11314,#11315,#11316,#11317,#11318,#11319));
#1243=EDGE_LOOP('',(#11320,#11321,#11322,#11323,#11324,#11325));
#1244=EDGE_LOOP('',(#11326,#11327,#11328,#11329,#11330,#11331));
#1245=EDGE_LOOP('',(#11332,#11333,#11334,#11335,#11336,#11337));
#1246=EDGE_LOOP('',(#11338,#11339,#11340,#11341,#11342,#11343,#11344,#11345));
#1247=EDGE_LOOP('',(#11346,#11347,#11348,#11349,#11350));
#1248=EDGE_LOOP('',(#11351,#11352,#11353,#11354,#11355,#11356));
#1249=EDGE_LOOP('',(#11357,#11358,#11359,#11360));
#1250=EDGE_LOOP('',(#11361,#11362,#11363,#11364,#11365,#11366));
#1251=EDGE_LOOP('',(#11367,#11368,#11369,#11370));
#1252=EDGE_LOOP('',(#11371,#11372,#11373,#11374,#11375,#11376));
#1253=EDGE_LOOP('',(#11377,#11378,#11379,#11380));
#1254=EDGE_LOOP('',(#11381,#11382,#11383,#11384,#11385,#11386));
#1255=EDGE_LOOP('',(#11387,#11388,#11389,#11390));
#1256=EDGE_LOOP('',(#11391,#11392,#11393,#11394,#11395,#11396));
#1257=EDGE_LOOP('',(#11397,#11398,#11399,#11400));
#1258=EDGE_LOOP('',(#11401,#11402,#11403,#11404,#11405,#11406));
#1259=EDGE_LOOP('',(#11407,#11408,#11409,#11410));
#1260=EDGE_LOOP('',(#11411,#11412,#11413,#11414));
#1261=EDGE_LOOP('',(#11415,#11416,#11417,#11418,#11419));
#1262=EDGE_LOOP('',(#11420,#11421,#11422,#11423,#11424,#11425));
#1263=EDGE_LOOP('',(#11426,#11427,#11428,#11429,#11430,#11431));
#1264=EDGE_LOOP('',(#11432,#11433,#11434,#11435,#11436,#11437));
#1265=EDGE_LOOP('',(#11438,#11439,#11440,#11441,#11442,#11443));
#1266=EDGE_LOOP('',(#11444,#11445,#11446,#11447,#11448,#11449));
#1267=EDGE_LOOP('',(#11450,#11451,#11452,#11453,#11454,#11455));
#1268=EDGE_LOOP('',(#11456,#11457,#11458,#11459,#11460,#11461));
#1269=EDGE_LOOP('',(#11462,#11463,#11464,#11465,#11466,#11467));
#1270=EDGE_LOOP('',(#11468,#11469,#11470,#11471,#11472,#11473));
#1271=EDGE_LOOP('',(#11474,#11475,#11476,#11477,#11478,#11479));
#1272=EDGE_LOOP('',(#11480,#11481,#11482,#11483,#11484,#11485));
#1273=EDGE_LOOP('',(#11486,#11487,#11488,#11489,#11490,#11491));
#1274=EDGE_LOOP('',(#11492,#11493,#11494,#11495,#11496,#11497));
#1275=EDGE_LOOP('',(#11498,#11499,#11500,#11501,#11502));
#1276=EDGE_LOOP('',(#11503,#11504,#11505,#11506,#11507,#11508));
#1277=EDGE_LOOP('',(#11509,#11510,#11511,#11512,#11513,#11514));
#1278=EDGE_LOOP('',(#11515,#11516,#11517,#11518,#11519,#11520));
#1279=EDGE_LOOP('',(#11521,#11522,#11523,#11524,#11525,#11526));
#1280=EDGE_LOOP('',(#11527,#11528,#11529,#11530,#11531,#11532));
#1281=EDGE_LOOP('',(#11533,#11534,#11535,#11536,#11537,#11538));
#1282=EDGE_LOOP('',(#11539,#11540,#11541,#11542,#11543,#11544));
#1283=EDGE_LOOP('',(#11545,#11546,#11547,#11548,#11549,#11550));
#1284=EDGE_LOOP('',(#11551,#11552,#11553,#11554,#11555,#11556));
#1285=EDGE_LOOP('',(#11557,#11558,#11559,#11560,#11561,#11562));
#1286=EDGE_LOOP('',(#11563,#11564,#11565,#11566,#11567,#11568));
#1287=EDGE_LOOP('',(#11569,#11570,#11571,#11572,#11573,#11574));
#1288=EDGE_LOOP('',(#11575,#11576,#11577,#11578,#11579,#11580));
#1289=EDGE_LOOP('',(#11581,#11582,#11583,#11584,#11585));
#1290=EDGE_LOOP('',(#11586,#11587,#11588,#11589,#11590,#11591));
#1291=EDGE_LOOP('',(#11592,#11593,#11594,#11595,#11596,#11597));
#1292=EDGE_LOOP('',(#11598,#11599,#11600,#11601,#11602,#11603));
#1293=EDGE_LOOP('',(#11604,#11605,#11606,#11607,#11608,#11609));
#1294=EDGE_LOOP('',(#11610,#11611,#11612,#11613,#11614,#11615));
#1295=EDGE_LOOP('',(#11616,#11617,#11618,#11619,#11620,#11621));
#1296=EDGE_LOOP('',(#11622,#11623,#11624,#11625,#11626,#11627));
#1297=EDGE_LOOP('',(#11628,#11629,#11630,#11631,#11632,#11633));
#1298=EDGE_LOOP('',(#11634,#11635,#11636,#11637,#11638,#11639));
#1299=EDGE_LOOP('',(#11640,#11641,#11642,#11643,#11644,#11645));
#1300=EDGE_LOOP('',(#11646,#11647,#11648,#11649,#11650,#11651));
#1301=EDGE_LOOP('',(#11652,#11653,#11654,#11655,#11656,#11657));
#1302=EDGE_LOOP('',(#11658,#11659,#11660,#11661,#11662,#11663));
#1303=EDGE_LOOP('',(#11664,#11665,#11666,#11667,#11668));
#1304=EDGE_LOOP('',(#11669,#11670,#11671,#11672,#11673,#11674));
#1305=EDGE_LOOP('',(#11675,#11676,#11677,#11678,#11679,#11680));
#1306=EDGE_LOOP('',(#11681,#11682,#11683,#11684,#11685,#11686));
#1307=EDGE_LOOP('',(#11687,#11688,#11689,#11690,#11691,#11692));
#1308=EDGE_LOOP('',(#11693,#11694,#11695,#11696,#11697,#11698));
#1309=EDGE_LOOP('',(#11699,#11700,#11701,#11702,#11703,#11704));
#1310=EDGE_LOOP('',(#11705,#11706,#11707,#11708,#11709,#11710));
#1311=EDGE_LOOP('',(#11711,#11712,#11713,#11714,#11715,#11716));
#1312=EDGE_LOOP('',(#11717,#11718,#11719,#11720,#11721,#11722));
#1313=EDGE_LOOP('',(#11723,#11724,#11725,#11726,#11727,#11728));
#1314=EDGE_LOOP('',(#11729,#11730,#11731,#11732,#11733,#11734));
#1315=EDGE_LOOP('',(#11735,#11736,#11737,#11738,#11739,#11740));
#1316=EDGE_LOOP('',(#11741,#11742,#11743,#11744,#11745,#11746));
#1317=EDGE_LOOP('',(#11747,#11748,#11749,#11750));
#1318=EDGE_LOOP('',(#11751,#11752,#11753,#11754,#11755));
#1319=EDGE_LOOP('',(#11756,#11757,#11758,#11759,#11760));
#1320=EDGE_LOOP('',(#11761,#11762,#11763,#11764,#11765));
#1321=EDGE_LOOP('',(#11766,#11767,#11768,#11769,#11770));
#1322=EDGE_LOOP('',(#11771,#11772,#11773,#11774,#11775));
#1323=EDGE_LOOP('',(#11776,#11777,#11778,#11779,#11780));
#1324=EDGE_LOOP('',(#11781,#11782,#11783,#11784,#11785,#11786));
#1325=EDGE_LOOP('',(#11787,#11788,#11789,#11790,#11791));
#1326=EDGE_LOOP('',(#11792,#11793,#11794,#11795,#11796));
#1327=EDGE_LOOP('',(#11797,#11798,#11799,#11800,#11801));
#1328=EDGE_LOOP('',(#11802,#11803,#11804,#11805,#11806));
#1329=EDGE_LOOP('',(#11807,#11808,#11809,#11810,#11811));
#1330=EDGE_LOOP('',(#11812,#11813,#11814,#11815,#11816));
#1331=EDGE_LOOP('',(#11817,#11818,#11819,#11820));
#1332=EDGE_LOOP('',(#11821,#11822,#11823,#11824,#11825));
#1333=EDGE_LOOP('',(#11826,#11827,#11828,#11829,#11830));
#1334=EDGE_LOOP('',(#11831,#11832,#11833,#11834,#11835));
#1335=EDGE_LOOP('',(#11836,#11837,#11838,#11839,#11840));
#1336=EDGE_LOOP('',(#11841,#11842,#11843,#11844,#11845));
#1337=EDGE_LOOP('',(#11846,#11847,#11848,#11849,#11850));
#1338=EDGE_LOOP('',(#11851,#11852,#11853,#11854,#11855,#11856));
#1339=EDGE_LOOP('',(#11857,#11858,#11859,#11860,#11861));
#1340=EDGE_LOOP('',(#11862,#11863,#11864,#11865,#11866));
#1341=EDGE_LOOP('',(#11867,#11868,#11869,#11870,#11871));
#1342=EDGE_LOOP('',(#11872,#11873,#11874,#11875,#11876));
#1343=EDGE_LOOP('',(#11877,#11878,#11879,#11880,#11881));
#1344=EDGE_LOOP('',(#11882,#11883,#11884,#11885,#11886));
#1345=EDGE_LOOP('',(#11887,#11888,#11889,#11890));
#1346=EDGE_LOOP('',(#11891,#11892,#11893,#11894));
#1347=EDGE_LOOP('',(#11895,#11896,#11897,#11898,#11899));
#1348=EDGE_LOOP('',(#11900,#11901,#11902,#11903));
#1349=EDGE_LOOP('',(#11904,#11905,#11906,#11907,#11908));
#1350=EDGE_LOOP('',(#11909,#11910,#11911,#11912,#11913));
#1351=EDGE_LOOP('',(#11914,#11915,#11916,#11917,#11918));
#1352=EDGE_LOOP('',(#11919,#11920,#11921,#11922,#11923,#11924));
#1353=EDGE_LOOP('',(#11925,#11926,#11927,#11928,#11929));
#1354=EDGE_LOOP('',(#11930,#11931,#11932,#11933,#11934));
#1355=EDGE_LOOP('',(#11935,#11936,#11937,#11938,#11939));
#1356=EDGE_LOOP('',(#11940,#11941,#11942,#11943,#11944));
#1357=EDGE_LOOP('',(#11945,#11946,#11947,#11948));
#1358=EDGE_LOOP('',(#11949,#11950,#11951,#11952));
#1359=EDGE_LOOP('',(#11953,#11954,#11955,#11956));
#1360=EDGE_LOOP('',(#11957,#11958,#11959,#11960));
#1361=EDGE_LOOP('',(#11961,#11962,#11963,#11964,#11965));
#1362=EDGE_LOOP('',(#11966,#11967,#11968,#11969));
#1363=EDGE_LOOP('',(#11970,#11971,#11972,#11973,#11974));
#1364=EDGE_LOOP('',(#11975,#11976,#11977,#11978,#11979));
#1365=EDGE_LOOP('',(#11980,#11981,#11982,#11983,#11984));
#1366=EDGE_LOOP('',(#11985,#11986,#11987,#11988,#11989,#11990));
#1367=EDGE_LOOP('',(#11991,#11992,#11993,#11994,#11995));
#1368=EDGE_LOOP('',(#11996,#11997,#11998,#11999,#12000));
#1369=EDGE_LOOP('',(#12001,#12002,#12003,#12004,#12005));
#1370=EDGE_LOOP('',(#12006,#12007,#12008,#12009,#12010));
#1371=EDGE_LOOP('',(#12011,#12012,#12013,#12014));
#1372=EDGE_LOOP('',(#12015,#12016,#12017,#12018));
#1373=EDGE_LOOP('',(#12019,#12020,#12021,#12022,#12023));
#1374=EDGE_LOOP('',(#12024,#12025,#12026,#12027,#12028));
#1375=EDGE_LOOP('',(#12029,#12030,#12031,#12032,#12033));
#1376=EDGE_LOOP('',(#12034,#12035,#12036,#12037,#12038));
#1377=EDGE_LOOP('',(#12039,#12040,#12041,#12042,#12043,#12044));
#1378=EDGE_LOOP('',(#12045,#12046,#12047,#12048,#12049,#12050));
#1379=EDGE_LOOP('',(#12051,#12052,#12053,#12054,#12055,#12056));
#1380=EDGE_LOOP('',(#12057,#12058,#12059,#12060,#12061,#12062));
#1381=EDGE_LOOP('',(#12063,#12064,#12065,#12066,#12067));
#1382=EDGE_LOOP('',(#12068,#12069,#12070,#12071,#12072,#12073));
#1383=EDGE_LOOP('',(#12074,#12075,#12076,#12077,#12078));
#1384=EDGE_LOOP('',(#12079,#12080,#12081,#12082,#12083,#12084));
#1385=EDGE_LOOP('',(#12085,#12086,#12087,#12088));
#1386=EDGE_LOOP('',(#12089,#12090,#12091,#12092,#12093,#12094,#12095,#12096,
#12097,#12098,#12099,#12100,#12101,#12102,#12103,#12104,#12105,#12106,#12107,
#12108,#12109,#12110,#12111,#12112,#12113,#12114,#12115,#12116,#12117,#12118,
#12119,#12120,#12121,#12122,#12123,#12124,#12125,#12126,#12127,#12128,#12129,
#12130,#12131,#12132,#12133,#12134,#12135,#12136,#12137,#12138,#12139,#12140,
#12141,#12142,#12143,#12144,#12145,#12146,#12147));
#1387=EDGE_LOOP('',(#12148,#12149,#12150,#12151,#12152,#12153,#12154,#12155,
#12156,#12157,#12158,#12159,#12160,#12161,#12162,#12163,#12164,#12165,#12166,
#12167,#12168,#12169,#12170,#12171,#12172,#12173,#12174,#12175,#12176,#12177,
#12178,#12179,#12180,#12181,#12182,#12183,#12184,#12185,#12186,#12187,#12188,
#12189,#12190,#12191,#12192,#12193,#12194,#12195,#12196,#12197,#12198,#12199,
#12200,#12201,#12202,#12203,#12204,#12205,#12206));
#1388=EDGE_LOOP('',(#12207,#12208,#12209,#12210));
#1389=EDGE_LOOP('',(#12211,#12212,#12213,#12214,#12215,#12216,#12217,#12218,
#12219,#12220,#12221,#12222,#12223,#12224,#12225,#12226,#12227,#12228,#12229,
#12230,#12231,#12232,#12233,#12234,#12235,#12236,#12237,#12238,#12239,#12240,
#12241,#12242,#12243,#12244,#12245,#12246,#12247,#12248,#12249,#12250,#12251,
#12252,#12253,#12254,#12255,#12256,#12257,#12258,#12259,#12260,#12261,#12262,
#12263,#12264,#12265,#12266,#12267,#12268,#12269));
#1390=EDGE_LOOP('',(#12270,#12271,#12272,#12273,#12274,#12275,#12276,#12277,
#12278,#12279,#12280,#12281,#12282,#12283,#12284,#12285,#12286,#12287,#12288,
#12289,#12290,#12291,#12292,#12293,#12294,#12295,#12296,#12297,#12298,#12299,
#12300,#12301,#12302,#12303,#12304,#12305,#12306,#12307,#12308,#12309,#12310,
#12311,#12312,#12313,#12314,#12315,#12316,#12317,#12318,#12319,#12320,#12321,
#12322,#12323,#12324,#12325,#12326,#12327,#12328));
#1391=EDGE_LOOP('',(#12329));
#1392=EDGE_LOOP('',(#12330));
#1393=EDGE_LOOP('',(#12331,#12332,#12333,#12334));
#1394=EDGE_LOOP('',(#12335,#12336,#12337,#12338));
#1395=EDGE_LOOP('',(#12339,#12340,#12341,#12342));
#1396=EDGE_LOOP('',(#12343,#12344,#12345,#12346));
#1397=EDGE_LOOP('',(#12347,#12348,#12349,#12350));
#1398=EDGE_LOOP('',(#12351,#12352,#12353,#12354));
#1399=EDGE_LOOP('',(#12355,#12356,#12357,#12358));
#1400=EDGE_LOOP('',(#12359,#12360,#12361,#12362));
#1401=EDGE_LOOP('',(#12363,#12364,#12365,#12366,#12367,#12368,#12369,#12370,
#12371,#12372,#12373,#12374,#12375,#12376,#12377,#12378,#12379,#12380,#12381,
#12382,#12383,#12384,#12385,#12386,#12387,#12388,#12389,#12390,#12391,#12392,
#12393,#12394,#12395,#12396,#12397,#12398,#12399,#12400,#12401,#12402,#12403,
#12404,#12405,#12406,#12407,#12408,#12409,#12410,#12411,#12412,#12413,#12414,
#12415,#12416,#12417));
#1402=EDGE_LOOP('',(#12418,#12419,#12420,#12421,#12422,#12423,#12424,#12425,
#12426,#12427,#12428,#12429,#12430,#12431,#12432,#12433,#12434,#12435,#12436,
#12437,#12438,#12439,#12440,#12441,#12442,#12443,#12444,#12445,#12446,#12447,
#12448,#12449,#12450,#12451,#12452,#12453,#12454,#12455,#12456,#12457,#12458,
#12459,#12460,#12461,#12462,#12463,#12464,#12465,#12466,#12467,#12468,#12469,
#12470,#12471,#12472));
#1403=EDGE_LOOP('',(#12473,#12474,#12475,#12476,#12477,#12478,#12479,#12480,
#12481,#12482,#12483,#12484,#12485,#12486,#12487,#12488,#12489,#12490,#12491,
#12492,#12493,#12494,#12495,#12496,#12497,#12498,#12499,#12500,#12501,#12502,
#12503,#12504,#12505,#12506,#12507,#12508,#12509,#12510,#12511,#12512,#12513,
#12514,#12515,#12516,#12517,#12518,#12519,#12520,#12521,#12522,#12523,#12524,
#12525,#12526,#12527));
#1404=EDGE_LOOP('',(#12528,#12529,#12530,#12531,#12532,#12533,#12534,#12535,
#12536,#12537,#12538,#12539,#12540,#12541,#12542,#12543,#12544,#12545,#12546,
#12547,#12548,#12549,#12550,#12551,#12552,#12553,#12554,#12555,#12556,#12557,
#12558,#12559,#12560,#12561,#12562,#12563,#12564,#12565,#12566,#12567,#12568,
#12569,#12570,#12571,#12572,#12573,#12574,#12575,#12576,#12577,#12578,#12579,
#12580,#12581,#12582));
#1405=EDGE_LOOP('',(#12583,#12584,#12585,#12586,#12587,#12588,#12589,#12590,
#12591,#12592,#12593,#12594,#12595,#12596,#12597,#12598,#12599,#12600,#12601,
#12602,#12603,#12604,#12605,#12606,#12607,#12608,#12609,#12610,#12611,#12612,
#12613,#12614,#12615,#12616,#12617,#12618,#12619,#12620,#12621,#12622,#12623,
#12624,#12625,#12626,#12627,#12628,#12629,#12630,#12631,#12632,#12633,#12634,
#12635));
#1406=EDGE_LOOP('',(#12636,#12637,#12638,#12639,#12640,#12641,#12642,#12643,
#12644,#12645,#12646,#12647,#12648,#12649,#12650,#12651,#12652,#12653,#12654,
#12655,#12656,#12657,#12658,#12659,#12660,#12661,#12662,#12663,#12664,#12665,
#12666,#12667,#12668,#12669,#12670,#12671,#12672,#12673,#12674,#12675,#12676,
#12677,#12678,#12679,#12680,#12681,#12682,#12683,#12684,#12685,#12686,#12687,
#12688));
#1407=EDGE_LOOP('',(#12689,#12690,#12691,#12692,#12693,#12694,#12695,#12696,
#12697,#12698,#12699,#12700,#12701,#12702,#12703,#12704,#12705,#12706,#12707,
#12708,#12709,#12710,#12711,#12712,#12713,#12714,#12715,#12716,#12717,#12718,
#12719,#12720,#12721,#12722,#12723,#12724,#12725,#12726,#12727,#12728,#12729,
#12730,#12731,#12732,#12733,#12734,#12735,#12736,#12737,#12738,#12739,#12740,
#12741));
#1408=EDGE_LOOP('',(#12742,#12743,#12744,#12745,#12746,#12747,#12748,#12749,
#12750,#12751,#12752,#12753,#12754,#12755,#12756,#12757,#12758,#12759,#12760,
#12761,#12762,#12763,#12764,#12765,#12766,#12767,#12768,#12769,#12770,#12771,
#12772,#12773,#12774,#12775,#12776,#12777,#12778,#12779,#12780,#12781,#12782,
#12783,#12784,#12785,#12786,#12787,#12788,#12789,#12790,#12791,#12792,#12793,
#12794));
#1409=EDGE_LOOP('',(#12795,#12796,#12797,#12798,#12799));
#1410=EDGE_LOOP('',(#12800,#12801,#12802,#12803,#12804));
#1411=EDGE_LOOP('',(#12805,#12806,#12807,#12808,#12809));
#1412=EDGE_LOOP('',(#12810,#12811,#12812,#12813,#12814));
#1413=EDGE_LOOP('',(#12815,#12816,#12817,#12818));
#1414=EDGE_LOOP('',(#12819,#12820,#12821,#12822));
#1415=EDGE_LOOP('',(#12823,#12824,#12825,#12826));
#1416=EDGE_LOOP('',(#12827,#12828,#12829,#12830));
#1417=EDGE_LOOP('',(#12831));
#1418=EDGE_LOOP('',(#12832));
#1419=EDGE_LOOP('',(#12833));
#1420=EDGE_LOOP('',(#12834));
#1421=EDGE_LOOP('',(#12835,#12836,#12837,#12838));
#1422=EDGE_LOOP('',(#12839,#12840,#12841,#12842));
#1423=EDGE_LOOP('',(#12843,#12844,#12845,#12846));
#1424=EDGE_LOOP('',(#12847,#12848,#12849,#12850));
#1425=EDGE_LOOP('',(#12851,#12852,#12853,#12854));
#1426=EDGE_LOOP('',(#12855));
#1427=EDGE_LOOP('',(#12856));
#1428=EDGE_LOOP('',(#12857));
#1429=EDGE_LOOP('',(#12858));
#1430=EDGE_LOOP('',(#12859,#12860,#12861,#12862));
#1431=EDGE_LOOP('',(#12863,#12864,#12865,#12866));
#1432=EDGE_LOOP('',(#12867));
#1433=EDGE_LOOP('',(#12868,#12869,#12870,#12871));
#1434=EDGE_LOOP('',(#12872,#12873,#12874,#12875));
#1435=EDGE_LOOP('',(#12876,#12877,#12878,#12879,#12880));
#1436=EDGE_LOOP('',(#12881,#12882,#12883,#12884,#12885));
#1437=EDGE_LOOP('',(#12886,#12887,#12888,#12889,#12890));
#1438=EDGE_LOOP('',(#12891,#12892,#12893,#12894,#12895));
#1439=EDGE_LOOP('',(#12896));
#1440=EDGE_LOOP('',(#12897,#12898,#12899,#12900));
#1441=EDGE_LOOP('',(#12901,#12902,#12903,#12904,#12905));
#1442=EDGE_LOOP('',(#12906,#12907,#12908,#12909,#12910));
#1443=EDGE_LOOP('',(#12911,#12912,#12913,#12914));
#1444=EDGE_LOOP('',(#12915,#12916,#12917,#12918));
#1445=EDGE_LOOP('',(#12919,#12920,#12921,#12922));
#1446=EDGE_LOOP('',(#12923,#12924,#12925,#12926));
#1447=EDGE_LOOP('',(#12927,#12928,#12929,#12930));
#1448=EDGE_LOOP('',(#12931,#12932,#12933,#12934));
#1449=EDGE_LOOP('',(#12935,#12936,#12937,#12938));
#1450=EDGE_LOOP('',(#12939,#12940,#12941,#12942,#12943,#12944,#12945,#12946));
#1451=EDGE_LOOP('',(#12947,#12948,#12949,#12950,#12951,#12952));
#1452=EDGE_LOOP('',(#12953,#12954,#12955,#12956,#12957,#12958));
#1453=EDGE_LOOP('',(#12959,#12960,#12961,#12962,#12963,#12964));
#1454=EDGE_LOOP('',(#12965,#12966,#12967,#12968,#12969,#12970));
#1455=EDGE_LOOP('',(#12971,#12972,#12973,#12974,#12975,#12976));
#1456=EDGE_LOOP('',(#12977,#12978,#12979,#12980,#12981,#12982));
#1457=EDGE_LOOP('',(#12983,#12984,#12985,#12986,#12987,#12988));
#1458=EDGE_LOOP('',(#12989,#12990,#12991,#12992,#12993,#12994));
#1459=EDGE_LOOP('',(#12995,#12996,#12997,#12998,#12999,#13000));
#1460=EDGE_LOOP('',(#13001,#13002,#13003,#13004,#13005,#13006));
#1461=EDGE_LOOP('',(#13007,#13008,#13009,#13010,#13011,#13012));
#1462=EDGE_LOOP('',(#13013,#13014,#13015,#13016,#13017,#13018));
#1463=EDGE_LOOP('',(#13019,#13020,#13021,#13022,#13023,#13024));
#1464=EDGE_LOOP('',(#13025,#13026,#13027,#13028,#13029,#13030));
#1465=EDGE_LOOP('',(#13031,#13032,#13033,#13034,#13035,#13036));
#1466=EDGE_LOOP('',(#13037,#13038,#13039,#13040,#13041,#13042));
#1467=EDGE_LOOP('',(#13043,#13044,#13045,#13046,#13047,#13048));
#1468=EDGE_LOOP('',(#13049,#13050,#13051,#13052,#13053,#13054));
#1469=EDGE_LOOP('',(#13055,#13056,#13057,#13058,#13059,#13060));
#1470=EDGE_LOOP('',(#13061,#13062,#13063,#13064,#13065,#13066));
#1471=EDGE_LOOP('',(#13067,#13068,#13069,#13070,#13071,#13072));
#1472=EDGE_LOOP('',(#13073,#13074,#13075,#13076,#13077,#13078));
#1473=EDGE_LOOP('',(#13079,#13080,#13081,#13082,#13083,#13084));
#1474=EDGE_LOOP('',(#13085,#13086,#13087,#13088,#13089,#13090));
#1475=EDGE_LOOP('',(#13091,#13092,#13093,#13094,#13095,#13096));
#1476=EDGE_LOOP('',(#13097,#13098,#13099,#13100,#13101,#13102));
#1477=EDGE_LOOP('',(#13103,#13104,#13105,#13106,#13107,#13108));
#1478=EDGE_LOOP('',(#13109,#13110,#13111,#13112,#13113,#13114));
#1479=EDGE_LOOP('',(#13115,#13116,#13117,#13118,#13119,#13120));
#1480=EDGE_LOOP('',(#13121,#13122,#13123,#13124,#13125,#13126));
#1481=EDGE_LOOP('',(#13127,#13128,#13129,#13130,#13131,#13132));
#1482=EDGE_LOOP('',(#13133,#13134,#13135,#13136,#13137,#13138));
#1483=EDGE_LOOP('',(#13139,#13140,#13141,#13142,#13143,#13144));
#1484=EDGE_LOOP('',(#13145,#13146,#13147,#13148,#13149,#13150));
#1485=EDGE_LOOP('',(#13151,#13152,#13153,#13154,#13155,#13156));
#1486=EDGE_LOOP('',(#13157,#13158,#13159,#13160,#13161,#13162));
#1487=EDGE_LOOP('',(#13163,#13164,#13165,#13166,#13167,#13168));
#1488=EDGE_LOOP('',(#13169,#13170,#13171,#13172,#13173,#13174));
#1489=EDGE_LOOP('',(#13175,#13176,#13177,#13178,#13179,#13180));
#1490=EDGE_LOOP('',(#13181,#13182,#13183,#13184,#13185,#13186));
#1491=EDGE_LOOP('',(#13187,#13188,#13189,#13190,#13191,#13192));
#1492=EDGE_LOOP('',(#13193,#13194,#13195,#13196,#13197,#13198));
#1493=EDGE_LOOP('',(#13199,#13200,#13201,#13202,#13203,#13204));
#1494=EDGE_LOOP('',(#13205,#13206,#13207,#13208,#13209,#13210));
#1495=EDGE_LOOP('',(#13211,#13212,#13213,#13214,#13215,#13216));
#1496=EDGE_LOOP('',(#13217,#13218,#13219,#13220,#13221,#13222));
#1497=EDGE_LOOP('',(#13223,#13224,#13225,#13226,#13227,#13228));
#1498=EDGE_LOOP('',(#13229,#13230,#13231,#13232,#13233,#13234));
#1499=EDGE_LOOP('',(#13235,#13236,#13237,#13238,#13239,#13240));
#1500=EDGE_LOOP('',(#13241,#13242,#13243,#13244,#13245,#13246,#13247,#13248,
#13249,#13250,#13251,#13252,#13253,#13254,#13255,#13256,#13257,#13258,#13259,
#13260,#13261,#13262,#13263,#13264,#13265,#13266,#13267,#13268,#13269,#13270,
#13271,#13272,#13273,#13274,#13275,#13276,#13277,#13278,#13279,#13280,#13281,
#13282,#13283,#13284,#13285,#13286,#13287,#13288,#13289,#13290,#13291,#13292,
#13293,#13294,#13295,#13296,#13297,#13298,#13299,#13300,#13301,#13302,#13303,
#13304,#13305,#13306,#13307,#13308,#13309,#13310,#13311,#13312,#13313,#13314,
#13315,#13316,#13317,#13318,#13319,#13320,#13321,#13322,#13323,#13324,#13325,
#13326));
#1501=EDGE_LOOP('',(#13327));
#1502=EDGE_LOOP('',(#13328));
#1503=EDGE_LOOP('',(#13329,#13330,#13331,#13332));
#1504=EDGE_LOOP('',(#13333,#13334,#13335,#13336));
#1505=EDGE_LOOP('',(#13337,#13338,#13339,#13340));
#1506=EDGE_LOOP('',(#13341,#13342,#13343,#13344));
#1507=EDGE_LOOP('',(#13345,#13346,#13347,#13348));
#1508=EDGE_LOOP('',(#13349));
#1509=EDGE_LOOP('',(#13350,#13351,#13352,#13353,#13354));
#1510=EDGE_LOOP('',(#13355,#13356,#13357,#13358,#13359,#13360,#13361,#13362,
#13363,#13364,#13365,#13366,#13367,#13368,#13369,#13370,#13371,#13372,#13373,
#13374,#13375,#13376,#13377,#13378,#13379,#13380,#13381,#13382,#13383,#13384,
#13385,#13386,#13387,#13388,#13389,#13390,#13391,#13392,#13393,#13394,#13395,
#13396,#13397,#13398,#13399,#13400,#13401,#13402,#13403,#13404,#13405,#13406,
#13407,#13408,#13409,#13410,#13411,#13412,#13413,#13414,#13415,#13416,#13417,
#13418,#13419,#13420,#13421,#13422,#13423,#13424,#13425,#13426,#13427,#13428,
#13429,#13430,#13431,#13432,#13433,#13434,#13435,#13436,#13437,#13438,#13439,
#13440,#13441,#13442,#13443,#13444,#13445,#13446,#13447,#13448,#13449,#13450,
#13451,#13452,#13453,#13454,#13455,#13456,#13457,#13458,#13459,#13460,#13461,
#13462,#13463,#13464,#13465,#13466,#13467,#13468,#13469,#13470,#13471,#13472,
#13473,#13474,#13475,#13476,#13477,#13478,#13479,#13480,#13481,#13482,#13483,
#13484,#13485,#13486,#13487,#13488,#13489,#13490,#13491,#13492,#13493,#13494,
#13495,#13496,#13497));
#1511=EDGE_LOOP('',(#13498,#13499,#13500,#13501,#13502,#13503,#13504,#13505,
#13506,#13507,#13508,#13509,#13510,#13511,#13512,#13513,#13514,#13515,#13516,
#13517,#13518,#13519,#13520,#13521,#13522,#13523,#13524,#13525,#13526,#13527,
#13528,#13529,#13530,#13531,#13532,#13533,#13534,#13535,#13536,#13537,#13538,
#13539,#13540,#13541,#13542,#13543,#13544,#13545,#13546,#13547,#13548,#13549,
#13550,#13551,#13552,#13553,#13554,#13555,#13556,#13557,#13558,#13559,#13560,
#13561,#13562,#13563,#13564,#13565,#13566,#13567,#13568,#13569,#13570,#13571,
#13572,#13573,#13574,#13575,#13576,#13577,#13578,#13579,#13580,#13581,#13582,
#13583,#13584,#13585,#13586,#13587,#13588,#13589,#13590,#13591,#13592,#13593,
#13594,#13595,#13596,#13597,#13598,#13599,#13600,#13601,#13602,#13603,#13604,
#13605,#13606,#13607,#13608,#13609,#13610,#13611,#13612,#13613,#13614,#13615,
#13616,#13617,#13618,#13619,#13620,#13621,#13622,#13623,#13624,#13625,#13626,
#13627,#13628,#13629,#13630,#13631,#13632,#13633,#13634,#13635,#13636,#13637,
#13638,#13639,#13640));
#1512=EDGE_LOOP('',(#13641));
#1513=EDGE_LOOP('',(#13642));
#1514=EDGE_LOOP('',(#13643,#13644,#13645,#13646));
#1515=EDGE_LOOP('',(#13647,#13648,#13649,#13650));
#1516=EDGE_LOOP('',(#13651,#13652,#13653,#13654));
#1517=EDGE_LOOP('',(#13655,#13656,#13657,#13658));
#1518=EDGE_LOOP('',(#13659));
#1519=EDGE_LOOP('',(#13660,#13661,#13662,#13663));
#1520=EDGE_LOOP('',(#13664));
#1521=EDGE_LOOP('',(#13665));
#1522=EDGE_LOOP('',(#13666,#13667,#13668,#13669));
#1523=EDGE_LOOP('',(#13670,#13671,#13672));
#1524=EDGE_LOOP('',(#13673,#13674,#13675,#13676));
#1525=EDGE_LOOP('',(#13677,#13678,#13679,#13680));
#1526=EDGE_LOOP('',(#13681,#13682,#13683,#13684));
#1527=EDGE_LOOP('',(#13685));
#1528=EDGE_LOOP('',(#13686));
#1529=EDGE_LOOP('',(#13687,#13688,#13689,#13690));
#1530=EDGE_LOOP('',(#13691,#13692,#13693,#13694));
#1531=EDGE_LOOP('',(#13695,#13696,#13697,#13698));
#1532=EDGE_LOOP('',(#13699,#13700,#13701,#13702));
#1533=EDGE_LOOP('',(#13703,#13704,#13705,#13706));
#1534=EDGE_LOOP('',(#13707,#13708,#13709,#13710));
#1535=EDGE_LOOP('',(#13711));
#1536=EDGE_LOOP('',(#13712));
#1537=EDGE_LOOP('',(#13713,#13714,#13715,#13716));
#1538=EDGE_LOOP('',(#13717,#13718,#13719,#13720));
#1539=EDGE_LOOP('',(#13721,#13722,#13723,#13724));
#1540=EDGE_LOOP('',(#13725,#13726,#13727,#13728));
#1541=EDGE_LOOP('',(#13729,#13730,#13731,#13732));
#1542=EDGE_LOOP('',(#13733,#13734,#13735,#13736));
#1543=EDGE_LOOP('',(#13737,#13738,#13739,#13740));
#1544=EDGE_LOOP('',(#13741,#13742,#13743,#13744));
#1545=EDGE_LOOP('',(#13745));
#1546=EDGE_LOOP('',(#13746));
#1547=EDGE_LOOP('',(#13747));
#1548=EDGE_LOOP('',(#13748));
#1549=EDGE_LOOP('',(#13749));
#1550=EDGE_LOOP('',(#13750,#13751,#13752,#13753));
#1551=EDGE_LOOP('',(#13754,#13755,#13756,#13757));
#1552=EDGE_LOOP('',(#13758,#13759,#13760,#13761));
#1553=EDGE_LOOP('',(#13762,#13763,#13764,#13765));
#1554=EDGE_LOOP('',(#13766,#13767,#13768,#13769));
#1555=EDGE_LOOP('',(#13770,#13771,#13772,#13773));
#1556=EDGE_LOOP('',(#13774,#13775,#13776,#13777));
#1557=EDGE_LOOP('',(#13778,#13779,#13780,#13781));
#1558=EDGE_LOOP('',(#13782));
#1559=EDGE_LOOP('',(#13783));
#1560=EDGE_LOOP('',(#13784));
#1561=EDGE_LOOP('',(#13785));
#1562=EDGE_LOOP('',(#13786));
#1563=EDGE_LOOP('',(#13787,#13788,#13789,#13790));
#1564=EDGE_LOOP('',(#13791,#13792,#13793,#13794));
#1565=EDGE_LOOP('',(#13795));
#1566=EDGE_LOOP('',(#13796));
#1567=EDGE_LOOP('',(#13797));
#1568=EDGE_LOOP('',(#13798));
#1569=EDGE_LOOP('',(#13799,#13800,#13801,#13802));
#1570=EDGE_LOOP('',(#13803,#13804,#13805,#13806,#13807,#13808));
#1571=EDGE_LOOP('',(#13809,#13810,#13811,#13812,#13813,#13814));
#1572=EDGE_LOOP('',(#13815,#13816,#13817,#13818,#13819,#13820));
#1573=EDGE_LOOP('',(#13821,#13822,#13823,#13824,#13825,#13826));
#1574=EDGE_LOOP('',(#13827,#13828,#13829,#13830,#13831,#13832));
#1575=EDGE_LOOP('',(#13833,#13834,#13835,#13836,#13837,#13838));
#1576=EDGE_LOOP('',(#13839,#13840,#13841,#13842,#13843,#13844));
#1577=EDGE_LOOP('',(#13845,#13846,#13847,#13848,#13849,#13850));
#1578=EDGE_LOOP('',(#13851,#13852,#13853,#13854,#13855,#13856));
#1579=EDGE_LOOP('',(#13857,#13858,#13859,#13860,#13861,#13862));
#1580=EDGE_LOOP('',(#13863,#13864,#13865,#13866,#13867,#13868));
#1581=EDGE_LOOP('',(#13869,#13870,#13871,#13872,#13873,#13874));
#1582=EDGE_LOOP('',(#13875,#13876,#13877,#13878,#13879,#13880));
#1583=EDGE_LOOP('',(#13881,#13882,#13883,#13884,#13885,#13886));
#1584=EDGE_LOOP('',(#13887,#13888,#13889,#13890,#13891,#13892));
#1585=EDGE_LOOP('',(#13893,#13894,#13895,#13896,#13897,#13898));
#1586=EDGE_LOOP('',(#13899,#13900,#13901,#13902,#13903,#13904));
#1587=EDGE_LOOP('',(#13905,#13906,#13907,#13908,#13909,#13910));
#1588=EDGE_LOOP('',(#13911,#13912,#13913,#13914,#13915,#13916));
#1589=EDGE_LOOP('',(#13917,#13918,#13919,#13920,#13921,#13922));
#1590=EDGE_LOOP('',(#13923,#13924,#13925,#13926,#13927,#13928));
#1591=EDGE_LOOP('',(#13929,#13930,#13931,#13932,#13933,#13934));
#1592=EDGE_LOOP('',(#13935,#13936,#13937,#13938,#13939,#13940));
#1593=EDGE_LOOP('',(#13941,#13942,#13943,#13944,#13945,#13946));
#1594=EDGE_LOOP('',(#13947,#13948,#13949,#13950,#13951,#13952));
#1595=EDGE_LOOP('',(#13953,#13954,#13955,#13956,#13957,#13958));
#1596=EDGE_LOOP('',(#13959,#13960,#13961,#13962,#13963,#13964));
#1597=EDGE_LOOP('',(#13965,#13966,#13967,#13968,#13969,#13970));
#1598=EDGE_LOOP('',(#13971,#13972,#13973,#13974,#13975,#13976));
#1599=EDGE_LOOP('',(#13977,#13978,#13979,#13980,#13981,#13982));
#1600=EDGE_LOOP('',(#13983,#13984,#13985,#13986,#13987,#13988));
#1601=EDGE_LOOP('',(#13989,#13990,#13991,#13992,#13993,#13994));
#1602=EDGE_LOOP('',(#13995,#13996,#13997,#13998,#13999,#14000));
#1603=EDGE_LOOP('',(#14001,#14002,#14003,#14004,#14005,#14006));
#1604=EDGE_LOOP('',(#14007,#14008,#14009,#14010,#14011,#14012));
#1605=EDGE_LOOP('',(#14013,#14014,#14015,#14016,#14017,#14018));
#1606=EDGE_LOOP('',(#14019,#14020,#14021,#14022,#14023,#14024));
#1607=EDGE_LOOP('',(#14025,#14026,#14027,#14028,#14029,#14030));
#1608=EDGE_LOOP('',(#14031,#14032,#14033,#14034,#14035,#14036));
#1609=EDGE_LOOP('',(#14037,#14038,#14039,#14040,#14041,#14042));
#1610=EDGE_LOOP('',(#14043,#14044,#14045,#14046,#14047,#14048));
#1611=EDGE_LOOP('',(#14049,#14050,#14051,#14052,#14053,#14054));
#1612=EDGE_LOOP('',(#14055,#14056,#14057,#14058,#14059,#14060));
#1613=EDGE_LOOP('',(#14061,#14062,#14063,#14064,#14065,#14066));
#1614=EDGE_LOOP('',(#14067,#14068,#14069,#14070,#14071,#14072));
#1615=EDGE_LOOP('',(#14073,#14074,#14075,#14076,#14077,#14078));
#1616=EDGE_LOOP('',(#14079,#14080,#14081,#14082,#14083,#14084));
#1617=EDGE_LOOP('',(#14085,#14086,#14087,#14088,#14089,#14090));
#1618=EDGE_LOOP('',(#14091,#14092,#14093,#14094,#14095,#14096));
#1619=EDGE_LOOP('',(#14097,#14098,#14099,#14100,#14101,#14102));
#1620=EDGE_LOOP('',(#14103,#14104,#14105,#14106,#14107,#14108));
#1621=EDGE_LOOP('',(#14109,#14110,#14111,#14112,#14113,#14114));
#1622=EDGE_LOOP('',(#14115,#14116,#14117,#14118,#14119,#14120));
#1623=EDGE_LOOP('',(#14121,#14122,#14123,#14124,#14125,#14126));
#1624=EDGE_LOOP('',(#14127,#14128,#14129,#14130,#14131,#14132));
#1625=EDGE_LOOP('',(#14133,#14134,#14135,#14136,#14137,#14138));
#1626=EDGE_LOOP('',(#14139,#14140,#14141,#14142,#14143,#14144));
#1627=EDGE_LOOP('',(#14145,#14146,#14147,#14148,#14149,#14150));
#1628=EDGE_LOOP('',(#14151,#14152,#14153,#14154,#14155,#14156));
#1629=EDGE_LOOP('',(#14157,#14158,#14159,#14160,#14161,#14162));
#1630=EDGE_LOOP('',(#14163,#14164,#14165,#14166,#14167,#14168));
#1631=EDGE_LOOP('',(#14169,#14170,#14171,#14172,#14173,#14174));
#1632=EDGE_LOOP('',(#14175,#14176,#14177,#14178,#14179,#14180));
#1633=EDGE_LOOP('',(#14181,#14182,#14183,#14184,#14185,#14186));
#1634=EDGE_LOOP('',(#14187,#14188,#14189,#14190,#14191,#14192,#14193,#14194,
#14195,#14196,#14197,#14198,#14199,#14200,#14201,#14202,#14203,#14204,#14205,
#14206,#14207,#14208,#14209,#14210,#14211,#14212,#14213,#14214,#14215,#14216,
#14217,#14218,#14219,#14220,#14221,#14222,#14223,#14224,#14225,#14226,#14227,
#14228,#14229,#14230,#14231,#14232,#14233,#14234,#14235,#14236,#14237,#14238,
#14239,#14240,#14241,#14242,#14243,#14244,#14245,#14246,#14247,#14248,#14249,
#14250,#14251,#14252,#14253,#14254,#14255,#14256,#14257,#14258,#14259,#14260,
#14261,#14262,#14263,#14264,#14265,#14266,#14267,#14268,#14269,#14270,#14271,
#14272,#14273,#14274,#14275,#14276,#14277,#14278,#14279,#14280,#14281,#14282,
#14283,#14284,#14285));
#1635=EDGE_LOOP('',(#14286,#14287,#14288,#14289,#14290,#14291));
#1636=EDGE_LOOP('',(#14292,#14293,#14294,#14295,#14296,#14297,#14298,#14299));
#1637=EDGE_LOOP('',(#14300,#14301,#14302,#14303,#14304,#14305,#14306,#14307,
#14308,#14309,#14310,#14311,#14312,#14313,#14314,#14315,#14316,#14317,#14318,
#14319,#14320,#14321,#14322,#14323,#14324,#14325,#14326,#14327,#14328,#14329,
#14330,#14331,#14332,#14333,#14334,#14335,#14336,#14337,#14338,#14339,#14340,
#14341,#14342,#14343,#14344,#14345,#14346,#14347,#14348,#14349,#14350,#14351,
#14352,#14353,#14354,#14355,#14356,#14357,#14358,#14359,#14360,#14361,#14362,
#14363,#14364,#14365,#14366,#14367,#14368,#14369,#14370,#14371,#14372,#14373,
#14374,#14375,#14376,#14377,#14378,#14379,#14380,#14381,#14382,#14383,#14384,
#14385,#14386,#14387,#14388,#14389,#14390,#14391,#14392,#14393,#14394,#14395,
#14396,#14397,#14398,#14399,#14400,#14401,#14402,#14403,#14404,#14405,#14406,
#14407,#14408,#14409,#14410,#14411,#14412,#14413,#14414,#14415,#14416,#14417,
#14418,#14419,#14420,#14421,#14422,#14423,#14424,#14425,#14426,#14427,#14428,
#14429,#14430,#14431,#14432,#14433,#14434,#14435,#14436,#14437,#14438,#14439,
#14440,#14441,#14442,#14443,#14444,#14445,#14446,#14447,#14448,#14449,#14450,
#14451,#14452,#14453,#14454,#14455,#14456,#14457,#14458,#14459,#14460,#14461,
#14462,#14463,#14464,#14465,#14466,#14467,#14468,#14469,#14470,#14471,#14472,
#14473,#14474,#14475,#14476,#14477,#14478,#14479,#14480,#14481));
#1638=EDGE_LOOP('',(#14482,#14483,#14484,#14485,#14486,#14487,#14488,#14489,
#14490,#14491,#14492,#14493,#14494,#14495,#14496,#14497,#14498,#14499,#14500,
#14501,#14502,#14503,#14504,#14505,#14506,#14507,#14508,#14509,#14510,#14511,
#14512,#14513,#14514,#14515,#14516,#14517,#14518,#14519,#14520,#14521,#14522,
#14523,#14524,#14525,#14526,#14527,#14528,#14529,#14530,#14531,#14532,#14533,
#14534,#14535,#14536,#14537,#14538,#14539,#14540,#14541,#14542,#14543,#14544,
#14545,#14546,#14547,#14548,#14549,#14550,#14551,#14552,#14553,#14554,#14555,
#14556,#14557,#14558,#14559,#14560,#14561,#14562,#14563,#14564,#14565,#14566,
#14567,#14568,#14569,#14570,#14571,#14572,#14573,#14574,#14575,#14576,#14577,
#14578,#14579,#14580,#14581,#14582,#14583,#14584,#14585,#14586,#14587,#14588,
#14589,#14590,#14591,#14592,#14593,#14594,#14595,#14596,#14597,#14598,#14599,
#14600,#14601,#14602,#14603,#14604,#14605,#14606,#14607,#14608,#14609,#14610,
#14611,#14612,#14613,#14614,#14615,#14616,#14617,#14618,#14619,#14620,#14621,
#14622,#14623,#14624,#14625,#14626,#14627,#14628,#14629,#14630,#14631,#14632,
#14633,#14634,#14635,#14636,#14637,#14638,#14639,#14640,#14641,#14642,#14643,
#14644,#14645,#14646,#14647,#14648,#14649,#14650,#14651,#14652,#14653,#14654,
#14655,#14656,#14657,#14658,#14659,#14660,#14661,#14662));
#1639=EDGE_LOOP('',(#14663,#14664,#14665,#14666));
#1640=EDGE_LOOP('',(#14667));
#1641=EDGE_LOOP('',(#14668));
#1642=EDGE_LOOP('',(#14669,#14670,#14671,#14672));
#1643=EDGE_LOOP('',(#14673,#14674,#14675,#14676,#14677,#14678,#14679,#14680,
#14681));
#1644=EDGE_LOOP('',(#14682,#14683,#14684));
#1645=EDGE_LOOP('',(#14685));
#1646=EDGE_LOOP('',(#14686,#14687,#14688,#14689));
#1647=EDGE_LOOP('',(#14690));
#1648=EDGE_LOOP('',(#14691,#14692,#14693,#14694,#14695,#14696));
#1649=EDGE_LOOP('',(#14697,#14698,#14699,#14700,#14701,#14702,#14703,#14704));
#1650=EDGE_LOOP('',(#14705,#14706,#14707,#14708));
#1651=EDGE_LOOP('',(#14709,#14710,#14711,#14712));
#1652=EDGE_LOOP('',(#14713,#14714,#14715,#14716));
#1653=EDGE_LOOP('',(#14717,#14718,#14719,#14720));
#1654=EDGE_LOOP('',(#14721,#14722,#14723,#14724));
#1655=EDGE_LOOP('',(#14725,#14726,#14727,#14728));
#1656=EDGE_LOOP('',(#14729,#14730,#14731,#14732,#14733,#14734,#14735,#14736,
#14737));
#1657=EDGE_LOOP('',(#14738,#14739,#14740));
#1658=EDGE_LOOP('',(#14741));
#1659=EDGE_LOOP('',(#14742));
#1660=EDGE_LOOP('',(#14743,#14744,#14745,#14746,#14747,#14748,#14749,#14750,
#14751));
#1661=EDGE_LOOP('',(#14752));
#1662=EDGE_LOOP('',(#14753,#14754,#14755,#14756));
#1663=EDGE_LOOP('',(#14757));
#1664=EDGE_LOOP('',(#14758));
#1665=EDGE_LOOP('',(#14759));
#1666=EDGE_LOOP('',(#14760));
#1667=EDGE_LOOP('',(#14761));
#1668=EDGE_LOOP('',(#14762));
#1669=EDGE_LOOP('',(#14763));
#1670=EDGE_LOOP('',(#14764));
#1671=EDGE_LOOP('',(#14765));
#1672=EDGE_LOOP('',(#14766));
#1673=EDGE_LOOP('',(#14767));
#1674=EDGE_LOOP('',(#14768));
#1675=EDGE_LOOP('',(#14769));
#1676=EDGE_LOOP('',(#14770));
#1677=EDGE_LOOP('',(#14771));
#1678=EDGE_LOOP('',(#14772));
#1679=EDGE_LOOP('',(#14773,#14774,#14775,#14776));
#1680=EDGE_LOOP('',(#14777));
#1681=EDGE_LOOP('',(#14778));
#1682=EDGE_LOOP('',(#14779));
#1683=EDGE_LOOP('',(#14780));
#1684=EDGE_LOOP('',(#14781,#14782,#14783,#14784));
#1685=EDGE_LOOP('',(#14785));
#1686=EDGE_LOOP('',(#14786));
#1687=EDGE_LOOP('',(#14787,#14788,#14789,#14790));
#1688=EDGE_LOOP('',(#14791));
#1689=EDGE_LOOP('',(#14792,#14793,#14794,#14795));
#1690=EDGE_LOOP('',(#14796));
#1691=EDGE_LOOP('',(#14797,#14798,#14799,#14800));
#1692=EDGE_LOOP('',(#14801,#14802,#14803,#14804));
#1693=EDGE_LOOP('',(#14805));
#1694=EDGE_LOOP('',(#14806));
#1695=EDGE_LOOP('',(#14807));
#1696=EDGE_LOOP('',(#14808));
#1697=EDGE_LOOP('',(#14809,#14810,#14811,#14812));
#1698=EDGE_LOOP('',(#14813,#14814,#14815,#14816));
#1699=EDGE_LOOP('',(#14817,#14818,#14819,#14820));
#1700=EDGE_LOOP('',(#14821,#14822,#14823,#14824));
#1701=EDGE_LOOP('',(#14825,#14826,#14827,#14828));
#1702=EDGE_LOOP('',(#14829,#14830,#14831,#14832));
#1703=EDGE_LOOP('',(#14833,#14834,#14835,#14836));
#1704=EDGE_LOOP('',(#14837,#14838,#14839,#14840));
#1705=EDGE_LOOP('',(#14841));
#1706=EDGE_LOOP('',(#14842));
#1707=EDGE_LOOP('',(#14843));
#1708=EDGE_LOOP('',(#14844));
#1709=EDGE_LOOP('',(#14845,#14846,#14847,#14848,#14849,#14850,#14851,#14852,
#14853));
#1710=EDGE_LOOP('',(#14854,#14855,#14856,#14857));
#1711=EDGE_LOOP('',(#14858,#14859,#14860,#14861));
#1712=EDGE_LOOP('',(#14862,#14863,#14864,#14865,#14866));
#1713=EDGE_LOOP('',(#14867,#14868,#14869,#14870,#14871));
#1714=EDGE_LOOP('',(#14872,#14873,#14874,#14875,#14876));
#1715=EDGE_LOOP('',(#14877,#14878,#14879,#14880,#14881));
#1716=EDGE_LOOP('',(#14882,#14883,#14884,#14885,#14886,#14887));
#1717=EDGE_LOOP('',(#14888,#14889,#14890,#14891));
#1718=EDGE_LOOP('',(#14892,#14893,#14894,#14895));
#1719=EDGE_LOOP('',(#14896,#14897,#14898,#14899,#14900,#14901));
#1720=EDGE_LOOP('',(#14902,#14903,#14904,#14905,#14906));
#1721=EDGE_LOOP('',(#14907,#14908,#14909,#14910,#14911));
#1722=EDGE_LOOP('',(#14912,#14913,#14914,#14915,#14916));
#1723=EDGE_LOOP('',(#14917,#14918,#14919,#14920,#14921));
#1724=EDGE_LOOP('',(#14922,#14923,#14924,#14925));
#1725=EDGE_LOOP('',(#14926,#14927,#14928,#14929,#14930));
#1726=EDGE_LOOP('',(#14931,#14932,#14933,#14934,#14935,#14936,#14937,#14938,
#14939,#14940,#14941,#14942,#14943,#14944,#14945,#14946,#14947,#14948,#14949,
#14950,#14951,#14952,#14953,#14954,#14955,#14956,#14957,#14958,#14959,#14960,
#14961,#14962,#14963,#14964,#14965,#14966));
#1727=EDGE_LOOP('',(#14967,#14968,#14969));
#1728=EDGE_LOOP('',(#14970,#14971,#14972));
#1729=EDGE_LOOP('',(#14973,#14974,#14975,#14976,#14977,#14978,#14979,#14980,
#14981,#14982,#14983,#14984,#14985,#14986,#14987,#14988,#14989,#14990,#14991,
#14992,#14993,#14994,#14995,#14996,#14997,#14998,#14999,#15000,#15001,#15002,
#15003,#15004,#15005,#15006,#15007,#15008,#15009,#15010,#15011,#15012,#15013,
#15014));
#1730=EDGE_LOOP('',(#15015,#15016,#15017,#15018,#15019,#15020,#15021,#15022,
#15023,#15024,#15025,#15026,#15027,#15028,#15029,#15030,#15031,#15032,#15033,
#15034,#15035,#15036,#15037,#15038,#15039,#15040,#15041,#15042,#15043,#15044,
#15045,#15046,#15047,#15048,#15049,#15050,#15051,#15052,#15053,#15054,#15055));
#1731=EDGE_LOOP('',(#15056,#15057,#15058,#15059));
#1732=EDGE_LOOP('',(#15060,#15061,#15062,#15063));
#1733=EDGE_LOOP('',(#15064,#15065,#15066,#15067));
#1734=EDGE_LOOP('',(#15068,#15069,#15070,#15071));
#1735=EDGE_LOOP('',(#15072,#15073,#15074,#15075));
#1736=EDGE_LOOP('',(#15076,#15077,#15078,#15079));
#1737=EDGE_LOOP('',(#15080,#15081,#15082,#15083,#15084,#15085));
#1738=EDGE_LOOP('',(#15086));
#1739=EDGE_LOOP('',(#15087,#15088,#15089,#15090));
#1740=EDGE_LOOP('',(#15091,#15092,#15093,#15094));
#1741=EDGE_LOOP('',(#15095));
#1742=EDGE_LOOP('',(#15096,#15097,#15098,#15099,#15100,#15101));
#1743=EDGE_LOOP('',(#15102));
#1744=EDGE_LOOP('',(#15103,#15104,#15105,#15106,#15107,#15108,#15109,#15110,
#15111));
#1745=EDGE_LOOP('',(#15112,#15113,#15114,#15115));
#1746=EDGE_LOOP('',(#15116,#15117,#15118,#15119,#15120,#15121));
#1747=EDGE_LOOP('',(#15122,#15123,#15124,#15125));
#1748=EDGE_LOOP('',(#15126,#15127,#15128,#15129,#15130,#15131));
#1749=EDGE_LOOP('',(#15132,#15133,#15134,#15135));
#1750=EDGE_LOOP('',(#15136,#15137,#15138,#15139,#15140,#15141));
#1751=EDGE_LOOP('',(#15142,#15143,#15144,#15145));
#1752=EDGE_LOOP('',(#15146,#15147,#15148,#15149,#15150,#15151));
#1753=EDGE_LOOP('',(#15152,#15153,#15154,#15155,#15156));
#1754=EDGE_LOOP('',(#15157,#15158,#15159,#15160,#15161));
#1755=EDGE_LOOP('',(#15162,#15163,#15164,#15165,#15166,#15167));
#1756=EDGE_LOOP('',(#15168,#15169,#15170,#15171));
#1757=EDGE_LOOP('',(#15172,#15173,#15174,#15175,#15176,#15177));
#1758=EDGE_LOOP('',(#15178,#15179,#15180,#15181,#15182));
#1759=EDGE_LOOP('',(#15183,#15184,#15185,#15186,#15187));
#1760=EDGE_LOOP('',(#15188,#15189,#15190,#15191,#15192));
#1761=EDGE_LOOP('',(#15193,#15194,#15195,#15196,#15197));
#1762=EDGE_LOOP('',(#15198,#15199,#15200,#15201,#15202,#15203));
#1763=EDGE_LOOP('',(#15204,#15205,#15206,#15207,#15208));
#1764=EDGE_LOOP('',(#15209,#15210,#15211,#15212,#15213));
#1765=EDGE_LOOP('',(#15214,#15215,#15216,#15217,#15218));
#1766=EDGE_LOOP('',(#15219,#15220,#15221,#15222,#15223));
#1767=EDGE_LOOP('',(#15224,#15225,#15226,#15227,#15228));
#1768=EDGE_LOOP('',(#15229,#15230,#15231,#15232,#15233));
#1769=EDGE_LOOP('',(#15234,#15235,#15236,#15237,#15238));
#1770=EDGE_LOOP('',(#15239,#15240,#15241,#15242,#15243));
#1771=EDGE_LOOP('',(#15244,#15245,#15246,#15247,#15248));
#1772=EDGE_LOOP('',(#15249,#15250,#15251,#15252,#15253,#15254));
#1773=EDGE_LOOP('',(#15255,#15256,#15257,#15258,#15259,#15260,#15261,#15262,
#15263,#15264,#15265,#15266,#15267,#15268,#15269,#15270,#15271,#15272,#15273,
#15274,#15275,#15276,#15277,#15278,#15279,#15280,#15281,#15282,#15283,#15284,
#15285,#15286,#15287,#15288,#15289,#15290,#15291,#15292,#15293,#15294,#15295,
#15296,#15297,#15298,#15299,#15300,#15301,#15302,#15303,#15304,#15305,#15306,
#15307,#15308,#15309,#15310,#15311,#15312,#15313,#15314));
#1774=EDGE_LOOP('',(#15315,#15316,#15317,#15318,#15319,#15320));
#1775=EDGE_LOOP('',(#15321,#15322,#15323));
#1776=EDGE_LOOP('',(#15324,#15325,#15326,#15327,#15328,#15329,#15330,#15331,
#15332,#15333,#15334,#15335,#15336,#15337,#15338,#15339,#15340,#15341,#15342,
#15343,#15344,#15345,#15346,#15347,#15348,#15349,#15350,#15351,#15352,#15353,
#15354,#15355,#15356,#15357,#15358,#15359,#15360,#15361,#15362,#15363,#15364,
#15365,#15366,#15367,#15368,#15369,#15370,#15371,#15372,#15373,#15374,#15375,
#15376,#15377,#15378,#15379,#15380,#15381,#15382,#15383,#15384,#15385,#15386,
#15387,#15388,#15389,#15390,#15391,#15392,#15393,#15394,#15395,#15396,#15397,
#15398,#15399,#15400));
#1777=EDGE_LOOP('',(#15401,#15402,#15403,#15404,#15405,#15406,#15407,#15408,
#15409,#15410,#15411,#15412,#15413,#15414,#15415,#15416,#15417,#15418,#15419,
#15420,#15421,#15422,#15423,#15424,#15425,#15426,#15427,#15428,#15429,#15430,
#15431,#15432,#15433,#15434,#15435,#15436,#15437,#15438,#15439,#15440,#15441,
#15442,#15443,#15444,#15445,#15446,#15447,#15448,#15449,#15450,#15451,#15452,
#15453,#15454,#15455,#15456,#15457,#15458,#15459,#15460,#15461,#15462,#15463,
#15464,#15465,#15466,#15467,#15468,#15469,#15470,#15471,#15472,#15473,#15474,
#15475));
#1778=EDGE_LOOP('',(#15476,#15477,#15478,#15479));
#1779=EDGE_LOOP('',(#15480,#15481,#15482,#15483));
#1780=EDGE_LOOP('',(#15484,#15485,#15486,#15487));
#1781=EDGE_LOOP('',(#15488,#15489,#15490,#15491));
#1782=EDGE_LOOP('',(#15492,#15493,#15494,#15495));
#1783=EDGE_LOOP('',(#15496,#15497,#15498,#15499));
#1784=EDGE_LOOP('',(#15500,#15501,#15502,#15503,#15504,#15505));
#1785=EDGE_LOOP('',(#15506));
#1786=EDGE_LOOP('',(#15507,#15508,#15509,#15510));
#1787=EDGE_LOOP('',(#15511,#15512,#15513,#15514));
#1788=EDGE_LOOP('',(#15515));
#1789=EDGE_LOOP('',(#15516,#15517,#15518,#15519,#15520,#15521));
#1790=EDGE_LOOP('',(#15522));
#1791=EDGE_LOOP('',(#15523,#15524,#15525,#15526,#15527,#15528,#15529,#15530,
#15531,#15532,#15533,#15534,#15535,#15536,#15537,#15538,#15539,#15540,#15541,
#15542,#15543,#15544,#15545,#15546,#15547,#15548,#15549,#15550,#15551,#15552,
#15553,#15554,#15555,#15556,#15557,#15558));
#1792=EDGE_LOOP('',(#15559,#15560,#15561,#15562,#15563,#15564,#15565,#15566,
#15567,#15568,#15569,#15570,#15571,#15572,#15573,#15574,#15575,#15576,#15577,
#15578,#15579,#15580,#15581));
#1793=EDGE_LOOP('',(#15582,#15583,#15584,#15585,#15586,#15587,#15588,#15589,
#15590));
#1794=EDGE_LOOP('',(#15591,#15592,#15593,#15594,#15595,#15596,#15597,#15598,
#15599,#15600,#15601,#15602,#15603,#15604,#15605,#15606,#15607,#15608,#15609,
#15610,#15611,#15612,#15613,#15614,#15615,#15616,#15617,#15618,#15619));
#1795=EDGE_LOOP('',(#15620,#15621,#15622,#15623,#15624,#15625,#15626,#15627,
#15628,#15629,#15630,#15631,#15632,#15633,#15634,#15635,#15636,#15637,#15638,
#15639,#15640,#15641,#15642,#15643,#15644,#15645,#15646,#15647,#15648,#15649,
#15650,#15651));
#1796=EDGE_LOOP('',(#15652,#15653,#15654,#15655));
#1797=EDGE_LOOP('',(#15656,#15657,#15658,#15659));
#1798=EDGE_LOOP('',(#15660,#15661,#15662,#15663));
#1799=EDGE_LOOP('',(#15664,#15665,#15666,#15667));
#1800=EDGE_LOOP('',(#15668,#15669,#15670,#15671));
#1801=EDGE_LOOP('',(#15672,#15673,#15674,#15675));
#1802=EDGE_LOOP('',(#15676,#15677,#15678,#15679,#15680,#15681));
#1803=EDGE_LOOP('',(#15682));
#1804=EDGE_LOOP('',(#15683,#15684,#15685,#15686));
#1805=EDGE_LOOP('',(#15687,#15688,#15689,#15690));
#1806=EDGE_LOOP('',(#15691));
#1807=EDGE_LOOP('',(#15692,#15693,#15694,#15695,#15696,#15697));
#1808=EDGE_LOOP('',(#15698));
#1809=CIRCLE('',#17049,4.085);
#1810=CIRCLE('',#17059,4.085);
#1811=CIRCLE('',#17061,3.38975);
#1812=CIRCLE('',#17062,3.38975);
#1813=CIRCLE('',#17063,3.38975);
#1814=CIRCLE('',#17073,3.38975);
#1815=CIRCLE('',#17075,4.085);
#1816=CIRCLE('',#17085,4.085);
#1817=CIRCLE('',#17087,3.38975);
#1818=CIRCLE('',#17088,3.38975);
#1819=CIRCLE('',#17089,3.38975);
#1820=CIRCLE('',#17099,3.38975);
#1821=CIRCLE('',#17101,4.085);
#1822=CIRCLE('',#17111,4.085);
#1823=CIRCLE('',#17113,3.38975);
#1824=CIRCLE('',#17114,3.38975);
#1825=CIRCLE('',#17115,3.38975);
#1826=CIRCLE('',#17125,3.38975);
#1827=CIRCLE('',#17127,4.085);
#1828=CIRCLE('',#17137,4.085);
#1829=CIRCLE('',#17139,3.38975);
#1830=CIRCLE('',#17140,3.38975);
#1831=CIRCLE('',#17141,3.38975);
#1832=CIRCLE('',#17151,3.38975);
#1833=CIRCLE('',#17169,4.5);
#1834=CIRCLE('',#17170,4.5);
#1835=CIRCLE('',#17172,4.5);
#1836=CIRCLE('',#17173,4.5);
#1837=CIRCLE('',#17175,4.5);
#1838=CIRCLE('',#17176,4.5);
#1839=CIRCLE('',#17178,4.5);
#1840=CIRCLE('',#17179,4.5);
#1841=CIRCLE('',#17188,2.05475);
#1842=CIRCLE('',#17204,2.05475);
#1843=CIRCLE('',#17206,1.666);
#1844=CIRCLE('',#17207,1.666);
#1845=CIRCLE('',#17222,1.666);
#1846=CIRCLE('',#17224,2.05475);
#1847=CIRCLE('',#17240,2.05475);
#1848=CIRCLE('',#17242,1.666);
#1849=CIRCLE('',#17243,1.666);
#1850=CIRCLE('',#17258,1.666);
#1851=CIRCLE('',#17260,2.05475);
#1852=CIRCLE('',#17274,2.05475);
#1853=CIRCLE('',#17276,2.05475);
#1854=CIRCLE('',#17290,2.05475);
#1855=CIRCLE('',#17292,2.05475);
#1856=CIRCLE('',#17306,2.05475);
#1857=CIRCLE('',#17308,2.05475);
#1858=CIRCLE('',#17322,2.05475);
#1859=CIRCLE('',#17324,1.666);
#1860=CIRCLE('',#17338,1.666);
#1861=CIRCLE('',#17340,1.666);
#1862=CIRCLE('',#17354,1.666);
#1863=CIRCLE('',#17356,1.666);
#1864=CIRCLE('',#17370,1.666);
#1865=CIRCLE('',#17372,1.666);
#1866=CIRCLE('',#17386,1.666);
#1867=CIRCLE('',#17405,22.);
#1868=CIRCLE('',#17408,22.);
#1869=CIRCLE('',#17410,4.5);
#1870=CIRCLE('',#17411,4.5);
#1871=CIRCLE('',#17413,4.5);
#1872=CIRCLE('',#17414,4.5);
#1873=CIRCLE('',#17416,4.5);
#1874=CIRCLE('',#17417,4.5);
#1875=CIRCLE('',#17419,4.5);
#1876=CIRCLE('',#17420,4.5);
#1877=CIRCLE('',#17426,22.);
#1878=CIRCLE('',#17427,22.);
#1879=CIRCLE('',#17443,22.);
#1880=CIRCLE('',#17444,20.);
#1881=CIRCLE('',#17446,20.);
#1882=CIRCLE('',#17448,22.);
#1883=CIRCLE('',#17452,7.01125);
#1884=CIRCLE('',#17453,7.01125);
#1885=CIRCLE('',#17454,7.01125);
#1886=CIRCLE('',#17503,7.01125);
#1887=CIRCLE('',#17506,8.12525);
#1888=CIRCLE('',#17507,8.12524999999999);
#1889=CIRCLE('',#17509,7.);
#1890=CIRCLE('',#17510,4.);
#1891=CIRCLE('',#17512,10.);
#1892=CIRCLE('',#17517,20.);
#1893=CIRCLE('',#17520,4.);
#1894=CIRCLE('',#17523,20.);
#1895=CIRCLE('',#17527,7.);
#1896=CIRCLE('',#17529,10.);
#1897=CIRCLE('',#17531,13.);
#1898=CIRCLE('',#17533,13.);
#1899=CIRCLE('',#17537,2.5);
#1900=CIRCLE('',#17538,2.5);
#1901=CIRCLE('',#17540,2.5);
#1902=CIRCLE('',#17541,2.5);
#1903=CIRCLE('',#17557,2.5);
#1904=CIRCLE('',#17558,2.5);
#1905=CIRCLE('',#17559,2.5);
#1906=CIRCLE('',#17560,2.5);
#1907=CIRCLE('',#17561,7.);
#1908=CIRCLE('',#17563,2.5);
#1909=CIRCLE('',#17565,2.5);
#1910=CIRCLE('',#17567,2.5);
#1911=CIRCLE('',#17569,2.5);
#1912=CIRCLE('',#17571,7.);
#1913=CIRCLE('',#17577,6.);
#1914=CIRCLE('',#17578,6.);
#1915=CIRCLE('',#17580,7.);
#1916=CIRCLE('',#17581,7.);
#1917=CIRCLE('',#17586,6.767);
#1918=CIRCLE('',#17652,7.911);
#1919=CIRCLE('',#17653,7.911);
#1920=CIRCLE('',#17655,6.767);
#1921=CIRCLE('',#17659,10.);
#1922=CIRCLE('',#17660,6.);
#1923=CIRCLE('',#17662,10.);
#1924=CIRCLE('',#17664,6.);
#1925=CIRCLE('',#17671,8.);
#1926=CIRCLE('',#17672,8.);
#1927=CIRCLE('',#17674,8.);
#1928=CIRCLE('',#17675,8.);
#1929=CIRCLE('',#17677,8.);
#1930=CIRCLE('',#17678,8.);
#1931=CIRCLE('',#17680,8.);
#1932=CIRCLE('',#17681,8.);
#1933=CIRCLE('',#17683,8.);
#1934=CIRCLE('',#17684,8.);
#1935=CIRCLE('',#17686,8.);
#1936=CIRCLE('',#17687,8.);
#1937=CIRCLE('',#17689,14.);
#1938=CIRCLE('',#17690,14.);
#1939=CIRCLE('',#17692,6.);
#1940=CIRCLE('',#17694,6.);
#1941=CIRCLE('',#17696,45.);
#1942=CIRCLE('',#17697,45.);
#1943=CIRCLE('',#17702,1.5);
#1944=CIRCLE('',#17703,1.5);
#1945=CIRCLE('',#17705,2.);
#1946=CIRCLE('',#17707,2.);
#1947=CIRCLE('',#17709,2.);
#1948=CIRCLE('',#17711,3.5);
#1949=CIRCLE('',#17712,2.);
#1950=CIRCLE('',#17714,3.5);
#1951=CIRCLE('',#17720,2.);
#1952=CIRCLE('',#17721,2.);
#1953=CIRCLE('',#17723,3.5);
#1954=CIRCLE('',#17724,3.5);
#1955=CIRCLE('',#17731,3.5);
#1956=CIRCLE('',#17732,1.5);
#1957=CIRCLE('',#17734,1.5);
#1958=CIRCLE('',#17736,3.5);
#1959=CIRCLE('',#17740,6.);
#1960=CIRCLE('',#17741,6.);
#1961=CIRCLE('',#17743,12.);
#1962=CIRCLE('',#17744,12.);
#1963=CIRCLE('',#17749,3.933);
#1964=CIRCLE('',#17750,3.22275);
#1965=CIRCLE('',#17751,3.);
#1966=CIRCLE('',#17752,3.22275);
#1967=CIRCLE('',#17754,3.22275);
#1968=CIRCLE('',#17771,3.933);
#1969=CIRCLE('',#17772,3.933);
#1970=CIRCLE('',#17783,6.5);
#1971=CIRCLE('',#17785,6.5);
#1972=CIRCLE('',#17790,1.954);
#1973=CIRCLE('',#17791,1.5555);
#1974=CIRCLE('',#17792,1.);
#1975=CIRCLE('',#17793,1.5555);
#1976=CIRCLE('',#17795,1.5555);
#1977=CIRCLE('',#17824,1.954);
#1978=CIRCLE('',#17825,1.96035170728095);
#1979=CIRCLE('',#17826,1.954);
#1980=CIRCLE('',#17837,3.5);
#1981=CIRCLE('',#17839,3.5);
#1982=CIRCLE('',#17844,1.954);
#1983=CIRCLE('',#17845,1.954);
#1984=CIRCLE('',#17847,1.5555);
#1985=CIRCLE('',#17848,1.5555);
#1986=CIRCLE('',#17850,1.);
#1987=CIRCLE('',#17859,3.5);
#1988=CIRCLE('',#17861,3.5);
#1989=B_SPLINE_CURVE_WITH_KNOTS('',3,(#20219,#20220,#20221,#20222,#20223,
#20224,#20225,#20226,#20227,#20228,#20229,#20230,#20231,#20232,#20233,#20234,
#20235,#20236,#20237,#20238,#20239,#20240,#20241,#20242,#20243,#20244,#20245,
#20246,#20247,#20248,#20249,#20250,#20251,#20252,#20253,#20254,#20255,#20256,
#20257,#20258,#20259,#20260,#20261,#20262,#20263,#20264,#20265,#20266,#20267,
#20268,#20269,#20270,#20271,#20272,#20273,#20274,#20275,#20276,#20277,#20278,
#20279,#20280,#20281,#20282,#20283,#20284,#20285,#20286,#20287,#20288,#20289,
#20290,#20291,#20292,#20293,#20294,#20295,#20296,#20297,#20298,#20299,#20300,
#20301,#20302,#20303,#20304,#20305,#20306,#20307,#20308,#20309,#20310,#20311,
#20312,#20313,#20314,#20315,#20316,#20317,#20318,#20319,#20320,#20321,#20322,
#20323,#20324,#20325,#20326,#20327,#20328,#20329,#20330,#20331,#20332,#20333,
#20334,#20335,#20336,#20337,#20338,#20339,#20340,#20341,#20342,#20343,#20344,
#20345,#20346,#20347,#20348,#20349,#20350,#20351,#20352,#20353,#20354,#20355,
#20356,#20357,#20358,#20359,#20360,#20361,#20362,#20363),.UNSPECIFIED.,
 .F.,.F.,(4,3,3,3,3,3,3,3,3,3,3,3,3,3,3,3,3,3,3,3,3,3,3,3,3,3,3,3,3,3,3,
3,3,3,3,3,3,3,3,3,3,3,3,3,3,3,3,3,4),(74.4826090335725,74.5701170669696,
74.6575762165587,74.7450105784093,74.8324408957047,74.9198879037736,75.0074269134415,
75.0950130962531,75.1827404978775,75.2578179239381,75.3457798849692,75.4336308010057,
75.5213935021216,75.6122752269211,75.6999373474644,75.7875855687495,75.8752403914981,
75.962922316007,76.0506986045304,76.1385311052508,76.2264862371109,76.2484473005182,
76.3362730397008,76.4239894702698,76.5116195619046,76.6025517013038,76.6900866998096,
76.7776100410487,76.8651423567182,76.9527042798826,77.0403648632325,77.1280840300195,
77.2159301399878,77.2390766770982,77.3262112033101,77.4132347402867,77.5001710454324,
77.5913629214631,77.6782061467429,77.7650395395892,77.8518844243916,77.9387621301685,
78.0257467155559,78.1127937623897,78.199978776898,78.2297060536782,78.3409628987117,
78.4504383987289,78.5398161890533),.UNSPECIFIED.);
#1990=B_SPLINE_CURVE_WITH_KNOTS('',3,(#20365,#20366,#20367,#20368),
 .UNSPECIFIED.,.F.,.F.,(4,4),(78.5398163397448,79.2203354302583),
 .UNSPECIFIED.);
#1991=B_SPLINE_CURVE_WITH_KNOTS('',3,(#20372,#20373,#20374,#20375,#20376,
#20377,#20378,#20379,#20380,#20381,#20382,#20383,#20384,#20385,#20386,#20387,
#20388,#20389,#20390,#20391,#20392,#20393,#20394,#20395,#20396,#20397,#20398,
#20399,#20400,#20401,#20402,#20403,#20404,#20405,#20406,#20407,#20408,#20409,
#20410,#20411,#20412,#20413,#20414),.UNSPECIFIED.,.F.,.F.,(4,3,3,3,3,3,
3,3,3,3,3,3,3,3,4),(78.5398163399586,78.6513081866131,78.7649916437635,
78.7900351244193,78.8773287774196,78.9645133671013,79.0516124728846,79.1386521216673,
79.2256605320351,79.3126588903471,79.3996683708265,79.4867645491849,79.5739037704035,
79.6611841726733,79.7442522064414),.UNSPECIFIED.);
#1992=B_SPLINE_CURVE_WITH_KNOTS('',3,(#20415,#20416,#20417,#20418,#20419,
#20420,#20421,#20422,#20423,#20424,#20425,#20426,#20427,#20428,#20429,#20430,
#20431,#20432,#20433,#20434,#20435,#20436,#20437,#20438,#20439,#20440,#20441,
#20442,#20443,#20444,#20445,#20446,#20447,#20448,#20449,#20450,#20451,#20452,
#20453,#20454,#20455,#20456,#20457,#20458,#20459,#20460,#20461,#20462,#20463,
#20464,#20465,#20466,#20467,#20468,#20469,#20470,#20471,#20472,#20473,#20474,
#20475,#20476,#20477,#20478,#20479,#20480,#20481,#20482,#20483,#20484,#20485,
#20486,#20487,#20488,#20489,#20490,#20491,#20492,#20493,#20494,#20495,#20496,
#20497,#20498,#20499,#20500,#20501,#20502,#20503,#20504,#20505,#20506,#20507,
#20508,#20509,#20510,#20511,#20512,#20513,#20514,#20515,#20516,#20517,#20518,
#20519,#20520,#20521,#20522,#20523,#20524,#20525,#20526,#20527,#20528,#20529,
#20530,#20531,#20532,#20533,#20534,#20535,#20536,#20537,#20538,#20539,#20540,
#20541,#20542,#20543,#20544,#20545,#20546,#20547,#20548,#20549,#20550,#20551,
#20552,#20553,#20554,#20555,#20556,#20557,#20558,#20559,#20560,#20561,#20562),
 .UNSPECIFIED.,.F.,.F.,(4,3,3,3,3,3,3,3,3,3,3,3,3,3,3,3,3,3,3,3,3,3,3,3,
3,3,3,3,3,3,3,3,3,3,3,3,3,3,3,3,3,3,3,3,3,3,3,3,3,4),(74.4816274087652,
74.5692304822722,74.6568785799873,74.7446691313286,74.8275176180992,74.9153495028009,
75.0030705517629,75.0907037488907,75.1816341546142,75.2691685016855,75.3566898130181,
75.4442187278137,75.531775885644,75.6194297201104,75.7071409756895,75.7949775432399,
75.8181469946792,75.9059726632625,75.9936877005556,76.0813150947037,76.1722477542731,
76.2597768495321,76.3472931203132,76.4348172103102,76.5223697637486,76.6100193409493,
76.6977265363025,76.785559361159,76.8087763712592,76.8965156836257,76.9841440069646,
77.0716844351596,77.1626495992445,77.2500916523099,77.3375210019096,77.4249583849954,
77.5124245392801,77.5999886071116,77.6876107096917,77.7753597026586,77.7994057478393,
77.8864293135118,77.9733148215533,78.0601212169649,78.1468700360845,78.2335827631578,
78.3203031262511,78.4070268007935,78.4938095091331,78.5398163397448),
 .UNSPECIFIED.);
#1993=B_SPLINE_CURVE_WITH_KNOTS('',3,(#20568,#20569,#20570,#20571,#20572,
#20573,#20574,#20575,#20576,#20577,#20578,#20579,#20580,#20581,#20582,#20583,
#20584,#20585,#20586,#20587,#20588,#20589,#20590,#20591,#20592,#20593,#20594,
#20595,#20596,#20597,#20598,#20599,#20600,#20601,#20602,#20603,#20604,#20605,
#20606,#20607,#20608,#20609,#20610,#20611,#20612,#20613,#20614,#20615,#20616,
#20617,#20618,#20619,#20620,#20621,#20622,#20623,#20624,#20625,#20626,#20627,
#20628,#20629,#20630,#20631,#20632,#20633,#20634,#20635,#20636,#20637,#20638,
#20639,#20640,#20641,#20642,#20643,#20644,#20645,#20646,#20647,#20648,#20649,
#20650,#20651,#20652,#20653,#20654,#20655,#20656,#20657,#20658,#20659,#20660,
#20661,#20662,#20663,#20664,#20665,#20666,#20667,#20668,#20669,#20670,#20671,
#20672,#20673,#20674,#20675,#20676,#20677,#20678,#20679,#20680,#20681,#20682,
#20683,#20684,#20685,#20686,#20687,#20688,#20689,#20690,#20691,#20692,#20693,
#20694,#20695,#20696,#20697,#20698,#20699,#20700,#20701,#20702,#20703,#20704,
#20705,#20706,#20707,#20708,#20709,#20710,#20711,#20712,#20713,#20714,#20715),
 .UNSPECIFIED.,.F.,.F.,(4,3,3,3,3,3,3,3,3,3,3,3,3,3,3,3,3,3,3,3,3,3,3,3,
3,3,3,3,3,3,3,3,3,3,3,3,3,3,3,3,3,3,3,3,3,3,3,3,3,4),(68.1983639736923,
68.2861814027768,68.3234122878779,68.4112289331686,68.4989347821535,68.5865528361021,
68.6774889396466,68.7650083795268,68.8525148961314,68.9400291443268,69.0275717794539,
69.1152113763737,69.2029085438011,69.2907313485085,69.314041664458,69.4018606984001,
69.4895689314358,69.5771893620946,69.6681245719626,69.755646355417,69.8431551993798,
69.9306717562514,70.0182166788918,70.1058585206193,70.19355791062,70.2813828885069,
70.304671041038,70.3924904087626,70.4801989997041,70.5678198116346,70.6587548873826,
70.7462771072879,70.8337864071766,70.9213034388543,71.0088488545995,71.0964912138051,
71.184191136065,71.2720166636101,71.295300417618,71.3826886082915,71.4699662262677,
71.5571567686942,71.6445910516527,71.731686798181,71.8187708746251,71.9058643773058,
71.9935560410698,72.0807764618647,72.1687037471133,72.2566310323619),
 .UNSPECIFIED.);
#1994=B_SPLINE_CURVE_WITH_KNOTS('',3,(#20716,#20717,#20718,#20719,#20720,
#20721,#20722,#20723,#20724,#20725,#20726,#20727,#20728,#20729,#20730,#20731,
#20732,#20733,#20734,#20735,#20736,#20737,#20738,#20739,#20740,#20741,#20742,
#20743,#20744,#20745,#20746,#20747,#20748,#20749,#20750,#20751,#20752,#20753,
#20754,#20755,#20756,#20757,#20758,#20759,#20760,#20761,#20762,#20763,#20764,
#20765,#20766,#20767,#20768,#20769,#20770,#20771,#20772,#20773,#20774,#20775,
#20776,#20777,#20778,#20779,#20780,#20781,#20782,#20783,#20784,#20785,#20786,
#20787,#20788,#20789,#20790,#20791,#20792,#20793,#20794,#20795,#20796,#20797,
#20798,#20799,#20800),.UNSPECIFIED.,.F.,.F.,(4,3,3,3,3,3,3,3,3,3,3,3,3,
3,3,3,3,3,3,3,3,3,3,3,3,3,3,3,4),(72.2566310325652,72.2859297941981,72.3737616647174,
72.4614826996036,72.5491158827769,72.640046293777,72.7275806272787,72.8151019252055,
72.9026308267726,72.9901879715657,73.0778417933396,73.1655530364124,73.2533895918213,
73.2765591707781,73.3643847882656,73.4520997741813,73.5397271167352,73.6306597955631,
73.7181888390195,73.8057050580113,73.8932290962889,73.9807815981339,74.068431124189,
74.1561382685975,74.2439710431921,74.2671885473581,74.3549358239911,74.4425594684545,
74.4826090335725),.UNSPECIFIED.);
#1995=B_SPLINE_CURVE_WITH_KNOTS('',3,(#20802,#20803,#20804,#20805,#20806,
#20807,#20808,#20809,#20810,#20811,#20812,#20813,#20814,#20815,#20816,#20817,
#20818,#20819,#20820,#20821,#20822,#20823,#20824,#20825,#20826,#20827,#20828,
#20829,#20830,#20831,#20832,#20833,#20834,#20835,#20836,#20837,#20838,#20839,
#20840,#20841,#20842,#20843,#20844,#20845,#20846,#20847,#20848,#20849,#20850,
#20851,#20852,#20853,#20854,#20855,#20856,#20857,#20858,#20859,#20860,#20861,
#20862,#20863,#20864,#20865,#20866,#20867,#20868,#20869,#20870,#20871,#20872,
#20873,#20874,#20875,#20876,#20877,#20878,#20879,#20880,#20881,#20882,#20883),
 .UNSPECIFIED.,.F.,.F.,(4,3,3,3,3,3,3,3,3,3,3,3,3,3,3,3,3,3,3,3,3,3,3,3,
3,3,3,4),(72.2566310325652,72.3454126124315,72.4342219267591,72.5230774207564,
72.6120589912192,72.7011092478249,72.7903164501228,72.8462588649391,72.9340782408894,
73.0217868401024,73.1094076603398,73.2003427329872,73.2878649612343,73.3753742694632,
73.4628913094705,73.5504367335256,73.63807910097,73.725779031437,73.8136045670799,
73.8368882415191,73.924681465638,74.0123709321393,74.0999774797657,74.1875218796041,
74.2750311973064,74.362520405566,74.4500269116099,74.4816274087652),
 .UNSPECIFIED.);
#1996=B_SPLINE_CURVE_WITH_KNOTS('',3,(#20884,#20885,#20886,#20887,#20888,
#20889,#20890,#20891,#20892,#20893,#20894,#20895,#20896,#20897,#20898,#20899,
#20900,#20901,#20902,#20903,#20904,#20905,#20906,#20907,#20908,#20909,#20910,
#20911,#20912,#20913,#20914,#20915,#20916,#20917,#20918,#20919,#20920,#20921,
#20922,#20923,#20924,#20925,#20926,#20927,#20928,#20929,#20930,#20931,#20932,
#20933,#20934,#20935,#20936,#20937,#20938,#20939,#20940,#20941,#20942,#20943,
#20944,#20945,#20946,#20947,#20948,#20949,#20950,#20951,#20952,#20953,#20954,
#20955,#20956,#20957,#20958,#20959,#20960,#20961,#20962,#20963,#20964,#20965,
#20966,#20967,#20968,#20969,#20970,#20971,#20972,#20973,#20974,#20975,#20976,
#20977,#20978,#20979,#20980,#20981,#20982,#20983,#20984,#20985,#20986,#20987,
#20988,#20989,#20990,#20991,#20992,#20993,#20994,#20995,#20996,#20997,#20998,
#20999,#21000,#21001,#21002,#21003,#21004,#21005,#21006,#21007,#21008,#21009,
#21010,#21011,#21012,#21013,#21014,#21015,#21016,#21017,#21018,#21019,#21020,
#21021,#21022,#21023,#21024,#21025,#21026,#21027,#21028,#21029,#21030,#21031),
 .UNSPECIFIED.,.F.,.F.,(4,3,3,3,3,3,3,3,3,3,3,3,3,3,3,3,3,3,3,3,3,3,3,3,
3,3,3,3,3,3,3,3,3,3,3,3,3,3,3,3,3,3,3,3,3,3,3,3,3,4),(68.1993401913434,
68.2868763835785,68.3743883543492,68.4618967634435,68.5494222631017,68.6370391881809,
68.7247035247109,68.8125067513156,68.883741358619,68.9715591938061,69.0592662331119,
69.1468854764006,69.2378211337504,69.3253417530268,69.4128494433357,69.5003648582877,
69.5879086519626,69.6755493894878,69.763247688409,69.8510716026728,69.8743707351991,
69.9621887255292,70.0498959227571,70.1375153265216,70.2284509246788,70.3159717097113,
70.4034795674247,70.4909951512383,70.5785391150419,70.6661800236928,70.7538784945183,
70.8417025804987,70.8650001117791,70.9528167537017,71.0405225993166,71.1281406498969,
71.2190767547046,71.3065961912421,71.3941027045195,71.4816169494061,71.569159581247,
71.6567991749293,71.7444963391443,71.8323191406998,71.8556294883591,71.9558798743633,
72.0526975273649,72.1492455770458,72.2453959286712,72.256631032376),
 .UNSPECIFIED.);
#1997=B_SPLINE_CURVE_WITH_KNOTS('',3,(#21037,#21038,#21039,#21040,#21041,
#21042,#21043,#21044,#21045,#21046,#21047,#21048,#21049,#21050,#21051,#21052,
#21053,#21054,#21055,#21056,#21057,#21058,#21059,#21060,#21061,#21062,#21063,
#21064,#21065,#21066,#21067,#21068,#21069,#21070,#21071,#21072,#21073,#21074,
#21075,#21076,#21077,#21078,#21079,#21080,#21081,#21082,#21083,#21084,#21085,
#21086,#21087,#21088,#21089,#21090,#21091,#21092,#21093,#21094,#21095,#21096,
#21097,#21098,#21099,#21100,#21101,#21102,#21103,#21104,#21105,#21106,#21107,
#21108,#21109,#21110,#21111,#21112,#21113,#21114,#21115,#21116,#21117,#21118,
#21119,#21120,#21121,#21122,#21123,#21124,#21125,#21126,#21127,#21128,#21129,
#21130,#21131,#21132,#21133,#21134,#21135,#21136,#21137,#21138,#21139,#21140,
#21141,#21142,#21143,#21144,#21145,#21146,#21147,#21148,#21149,#21150,#21151,
#21152,#21153,#21154,#21155,#21156,#21157,#21158,#21159,#21160,#21161,#21162,
#21163,#21164,#21165,#21166,#21167,#21168,#21169,#21170,#21171,#21172,#21173,
#21174,#21175,#21176,#21177,#21178,#21179,#21180,#21181,#21182,#21183,#21184),
 .UNSPECIFIED.,.F.,.F.,(4,3,3,3,3,3,3,3,3,3,3,3,3,3,3,3,3,3,3,3,3,3,3,3,
3,3,3,3,3,3,3,3,3,3,3,3,3,3,3,3,3,3,3,3,3,3,3,3,3,4),(61.9155759069306,
62.0030907077314,62.0906332894479,62.1782725403716,62.2659688151231,62.3537913799992,
62.3796360283978,62.467453738876,62.5551606542545,62.642779774532,62.7337154783378,
62.8212359776401,62.9087435492969,62.9962588470419,63.0838025250797,63.1714431498601,
63.2591413375884,63.3469651437694,63.3702654049778,63.4580831367133,63.5457900732474,
63.6334092145556,63.7243449104309,63.8118654303222,63.8993730223703,63.986888340288,
64.0744320382573,64.162072682515,64.249770889479,64.337594714396,64.3608947815578,
64.4487125433212,64.5364195101921,64.6240386821059,64.7149743666099,64.8024949175758,
64.8900025408166,64.9775178900099,65.0650616193034,65.1527022947983,65.2404005329847,
65.3282243888632,65.3515241581379,65.4399938083171,65.5283489317369,65.6166094520782,
65.705818520405,65.7939460921638,65.8836959087747,65.9734457253856),
 .UNSPECIFIED.);
#1998=B_SPLINE_CURVE_WITH_KNOTS('',3,(#21185,#21186,#21187,#21188,#21189,
#21190,#21191,#21192,#21193,#21194,#21195,#21196,#21197,#21198,#21199,#21200,
#21201,#21202,#21203,#21204,#21205,#21206,#21207,#21208,#21209,#21210,#21211,
#21212,#21213,#21214,#21215,#21216,#21217,#21218,#21219,#21220,#21221,#21222,
#21223,#21224,#21225,#21226,#21227,#21228,#21229,#21230,#21231,#21232,#21233,
#21234,#21235,#21236,#21237,#21238,#21239,#21240,#21241,#21242,#21243,#21244,
#21245,#21246,#21247,#21248,#21249,#21250,#21251,#21252,#21253,#21254,#21255,
#21256,#21257,#21258,#21259,#21260,#21261,#21262,#21263),.UNSPECIFIED.,
 .F.,.F.,(4,3,3,3,3,3,3,3,3,3,3,3,3,3,3,3,3,3,3,3,3,3,3,3,3,3,4),(65.9734457255974,
66.0719666577025,66.1708766449107,66.2703103694164,66.3421535347179,66.4299713697137,
66.5176784088316,66.6052976519356,66.6962333093559,66.7837539284567,66.8712616185937,
66.9587770333778,67.0463208268888,67.1339615642567,67.2216598630244,67.3094837771413,
67.3327829112979,67.4206084666378,67.5083214326648,67.5959318437032,67.6834846166537,
67.7710004523481,67.8585000197182,67.9460405122724,68.033599715588,68.1212547564394,
68.1983639736923),.UNSPECIFIED.);
#1999=B_SPLINE_CURVE_WITH_KNOTS('',3,(#21265,#21266,#21267,#21268,#21269,
#21270,#21271,#21272,#21273,#21274,#21275,#21276,#21277,#21278,#21279,#21280,
#21281,#21282,#21283,#21284,#21285,#21286,#21287,#21288,#21289,#21290,#21291,
#21292,#21293,#21294,#21295,#21296,#21297,#21298,#21299,#21300,#21301,#21302,
#21303,#21304,#21305,#21306,#21307,#21308,#21309,#21310,#21311,#21312,#21313,
#21314,#21315,#21316,#21317,#21318,#21319,#21320,#21321,#21322,#21323,#21324,
#21325,#21326,#21327,#21328,#21329,#21330,#21331,#21332,#21333,#21334,#21335,
#21336,#21337,#21338,#21339,#21340,#21341,#21342,#21343,#21344,#21345,#21346),
 .UNSPECIFIED.,.F.,.F.,(4,3,3,3,3,3,3,3,3,3,3,3,3,3,3,3,3,3,3,3,3,3,3,3,
3,3,3,4),(65.9734457255662,66.0604573171653,66.1473630253179,66.2341866877522,
66.3209558483152,66.4076973522101,66.4944326209606,66.5811830669334,66.6680217727008,
66.7549076097697,66.8419276275401,66.902482605459,66.9903003674263,67.0780073345023,
67.1656265066219,67.2565621910491,67.3440827422207,67.4315903656668,67.5191057150651,
67.6066494445629,67.6942901202597,67.7819883586472,67.8698122147238,67.893111982039,
67.9809173626158,68.0686254649819,68.1562390275125,68.1993401913434),
 .UNSPECIFIED.);
#2000=B_SPLINE_CURVE_WITH_KNOTS('',3,(#21347,#21348,#21349,#21350,#21351,
#21352,#21353,#21354,#21355,#21356,#21357,#21358,#21359,#21360,#21361,#21362,
#21363,#21364,#21365,#21366,#21367,#21368,#21369,#21370,#21371,#21372,#21373,
#21374,#21375,#21376,#21377,#21378,#21379,#21380,#21381,#21382,#21383,#21384,
#21385,#21386,#21387,#21388,#21389,#21390,#21391,#21392,#21393,#21394,#21395,
#21396,#21397,#21398,#21399,#21400,#21401,#21402,#21403,#21404,#21405,#21406,
#21407,#21408,#21409,#21410,#21411,#21412,#21413,#21414,#21415,#21416,#21417,
#21418,#21419,#21420,#21421,#21422,#21423,#21424,#21425,#21426,#21427,#21428,
#21429,#21430,#21431,#21432,#21433,#21434,#21435,#21436,#21437,#21438,#21439,
#21440,#21441,#21442,#21443,#21444,#21445,#21446,#21447,#21448,#21449,#21450,
#21451,#21452,#21453,#21454,#21455,#21456,#21457,#21458,#21459,#21460,#21461,
#21462,#21463,#21464,#21465,#21466,#21467,#21468,#21469,#21470,#21471,#21472,
#21473,#21474,#21475,#21476,#21477,#21478,#21479,#21480,#21481,#21482,#21483,
#21484,#21485,#21486,#21487,#21488,#21489,#21490,#21491,#21492,#21493,#21494,
#21495,#21496,#21497),.UNSPECIFIED.,.F.,.F.,(4,3,3,3,3,3,3,3,3,3,3,3,3,
3,3,3,3,3,3,3,3,3,3,3,3,3,3,3,3,3,3,3,3,3,3,3,3,3,3,3,3,3,3,3,3,3,3,3,3,
3,4),(61.9154863879853,61.9493357225588,62.0371534448199,62.1248603719797,
62.2124795040232,62.3034152034126,62.3909357143681,62.4784432976163,62.5659586068789,
62.6535022963475,62.741142932374,62.8288411312538,62.9166649483632,62.9399650991389,
63.0277828231756,63.1154897520975,63.2031088858876,63.2940445846165,63.3815650972695,
63.4690726821944,63.5565879931111,63.6441316842093,63.7317723218213,63.8194705222627,
63.9072943408872,63.9305944757189,64.018412204507,64.1061191382139,64.1937382768165,
64.2846739737518,64.3721944912548,64.4597020810347,64.5472173968066,64.6347610927545,
64.7224017351837,64.8100999404289,64.8979237638009,64.9212238522989,65.0090415627175,
65.0967484780368,65.1843675982553,65.2753033020833,65.3628238013271,65.4503313729256,
65.537846670613,65.6253903485929,65.7130309733168,65.800729160989,65.8885529671151,
65.9118532288789,65.9734457253856),.UNSPECIFIED.);
#2001=B_SPLINE_CURVE_WITH_KNOTS('',3,(#21503,#21504,#21505,#21506,#21507,
#21508,#21509,#21510,#21511,#21512,#21513,#21514,#21515,#21516,#21517,#21518,
#21519,#21520,#21521,#21522,#21523,#21524,#21525,#21526,#21527,#21528,#21529,
#21530,#21531,#21532,#21533,#21534,#21535,#21536,#21537,#21538,#21539,#21540,
#21541,#21542,#21543,#21544,#21545,#21546,#21547,#21548,#21549,#21550,#21551,
#21552,#21553,#21554,#21555,#21556,#21557,#21558,#21559,#21560,#21561,#21562,
#21563,#21564,#21565,#21566,#21567,#21568,#21569,#21570,#21571,#21572,#21573,
#21574,#21575,#21576,#21577,#21578,#21579,#21580,#21581,#21582,#21583,#21584,
#21585,#21586,#21587,#21588,#21589,#21590,#21591,#21592,#21593,#21594,#21595,
#21596,#21597,#21598,#21599,#21600,#21601,#21602,#21603,#21604,#21605,#21606,
#21607,#21608,#21609,#21610,#21611,#21612,#21613,#21614,#21615,#21616,#21617,
#21618,#21619,#21620,#21621,#21622,#21623,#21624,#21625,#21626,#21627,#21628,
#21629,#21630,#21631,#21632,#21633,#21634,#21635,#21636,#21637,#21638,#21639,
#21640,#21641,#21642,#21643,#21644,#21645,#21646,#21647,#21648,#21649,#21650),
 .UNSPECIFIED.,.F.,.F.,(4,3,3,3,3,3,3,3,3,3,3,3,3,3,3,3,3,3,3,3,3,3,3,3,
3,3,3,3,3,3,3,3,3,3,3,3,3,3,3,3,3,3,3,3,3,3,3,3,3,4),(55.6330521042359,
55.7206607554735,55.810060632154,55.8975784438563,55.9850858650237,56.0726035486431,
56.1634176037117,56.2510662026952,56.3387753400529,56.4266064512809,56.4358597689176,
56.5236774924357,56.6113844208514,56.6990035541482,56.7899392530668,56.8774597652612,
56.964967349741,57.0524826602265,57.1400263509079,57.2276669881264,57.3153651881873,
57.4031890064531,57.4264891454977,57.5143068691386,57.6020137976755,57.6896329310915,
57.7805686299648,57.8680891422733,57.955596726865,58.0431120374602,58.130655728249,
58.2182963655708,58.305994565733,58.393818384096,58.4171185220777,58.5049362463864,
58.5926431755944,58.6802623096844,58.7711980083061,58.8587185212908,58.9462261065584,
59.0337414178285,59.1212851092902,59.2089257472791,59.2966239481054,59.3844477671235,
59.4077478986577,59.5162980940452,59.6233575451915,59.6902604180837),
 .UNSPECIFIED.);
#2002=B_SPLINE_CURVE_WITH_KNOTS('',3,(#21651,#21652,#21653,#21654,#21655,
#21656,#21657,#21658,#21659,#21660,#21661,#21662,#21663,#21664,#21665,#21666,
#21667,#21668,#21669,#21670,#21671,#21672,#21673,#21674,#21675,#21676,#21677,
#21678,#21679,#21680,#21681,#21682,#21683,#21684,#21685,#21686,#21687,#21688,
#21689,#21690,#21691,#21692,#21693,#21694,#21695,#21696,#21697,#21698,#21699,
#21700,#21701,#21702,#21703,#21704,#21705,#21706,#21707,#21708,#21709,#21710,
#21711,#21712,#21713,#21714,#21715,#21716,#21717,#21718,#21719,#21720,#21721,
#21722,#21723,#21724,#21725,#21726,#21727,#21728,#21729),.UNSPECIFIED.,
 .F.,.F.,(4,3,3,3,3,3,3,3,3,3,3,3,3,3,3,3,3,3,3,3,3,3,3,3,3,3,4),(59.690260418206,
59.778775025335,59.8656202876019,59.9524524305452,60.0392927619904,60.1290638903022,
60.2160327288199,60.3072050020288,60.3983772752377,60.4861949992754,60.5739019281985,
60.6615210619898,60.7524567607183,60.8399772733726,60.9274848582988,61.0150001692168,
61.1025438603164,61.1901844979299,61.2778826983729,61.365706516999,61.3890066518178,
61.4768208703852,61.564528918874,61.6522906658881,61.7398425050512,61.8277092059909,
61.9155759069306),.UNSPECIFIED.);
#2003=B_SPLINE_CURVE_WITH_KNOTS('',3,(#21731,#21732,#21733,#21734,#21735,
#21736,#21737,#21738,#21739,#21740,#21741,#21742,#21743,#21744,#21745,#21746,
#21747,#21748,#21749,#21750,#21751,#21752,#21753,#21754,#21755,#21756,#21757,
#21758,#21759,#21760,#21761,#21762,#21763,#21764,#21765,#21766,#21767,#21768,
#21769,#21770,#21771,#21772,#21773,#21774,#21775,#21776,#21777,#21778,#21779,
#21780,#21781,#21782,#21783,#21784,#21785,#21786,#21787,#21788,#21789,#21790,
#21791,#21792,#21793,#21794,#21795,#21796,#21797,#21798,#21799,#21800,#21801,
#21802,#21803,#21804,#21805,#21806,#21807,#21808,#21809),.UNSPECIFIED.,
 .F.,.F.,(4,3,3,3,3,3,3,3,3,3,3,3,3,3,3,3,3,3,3,3,3,3,3,3,3,3,4),(59.69026041843,
59.7976956857346,59.9067549033635,59.9680769693988,60.0558946930392,60.1436016215755,
60.2312207549911,60.3221564538646,60.4096769661725,60.4971845507636,60.5846998613582,
60.6722435521463,60.7598841894676,60.8475823896291,60.9354062079916,60.9587063459788,
61.0465260468161,61.1342344663959,61.2218546067637,61.3094092403329,61.3969287920588,
61.4844339306926,61.5719453095894,61.6595334389296,61.7471595670043,61.8349150953348,
61.9154863879853),.UNSPECIFIED.);
#2004=B_SPLINE_CURVE_WITH_KNOTS('',3,(#21810,#21811,#21812,#21813,#21814,
#21815,#21816,#21817,#21818,#21819,#21820,#21821,#21822,#21823,#21824,#21825,
#21826,#21827,#21828,#21829,#21830,#21831,#21832,#21833,#21834,#21835,#21836,
#21837,#21838,#21839,#21840,#21841,#21842,#21843,#21844,#21845,#21846,#21847,
#21848,#21849,#21850,#21851,#21852,#21853,#21854,#21855,#21856,#21857,#21858,
#21859,#21860,#21861,#21862,#21863,#21864,#21865,#21866,#21867,#21868,#21869,
#21870,#21871,#21872,#21873,#21874,#21875,#21876,#21877,#21878,#21879,#21880,
#21881,#21882,#21883,#21884,#21885,#21886,#21887,#21888,#21889,#21890,#21891,
#21892,#21893,#21894,#21895,#21896,#21897,#21898,#21899,#21900,#21901,#21902,
#21903,#21904,#21905,#21906,#21907,#21908,#21909,#21910,#21911,#21912,#21913,
#21914,#21915,#21916,#21917,#21918,#21919,#21920,#21921,#21922,#21923,#21924,
#21925,#21926,#21927,#21928,#21929,#21930,#21931,#21932,#21933,#21934,#21935,
#21936,#21937,#21938,#21939,#21940,#21941,#21942,#21943,#21944,#21945,#21946,
#21947,#21948,#21949,#21950,#21951,#21952,#21953,#21954,#21955,#21956,#21957,
#21958,#21959,#21960),.UNSPECIFIED.,.F.,.F.,(4,3,3,3,3,3,3,3,3,3,3,3,3,
3,3,3,3,3,3,3,3,3,3,3,3,3,3,3,3,3,3,3,3,3,3,3,3,3,3,3,3,3,3,3,3,3,3,3,3,
3,4),(55.6321400113866,55.7196839623112,55.8073249236283,55.8950235724135,
55.9828476845365,56.0055594630787,56.0933771867246,56.1810841152679,56.2687032486923,
56.3596389475631,56.4471594598829,56.5346670444873,56.6221823550963,56.7097260459,
56.7973666832387,56.8850648834184,56.9728887018007,56.9961888396587,57.0840065633094,
57.1717134918572,57.2593326252856,57.3502683241548,57.4377888364785,57.5252964210864,
57.6128117316991,57.7003554225064,57.7879960598478,57.8756942600305,57.9635180784152,
57.9868182162387,58.0746359399784,58.1623428686156,58.2499620021338,58.3408977009694,
58.4284182133827,58.51592579808,58.6034411087818,58.6909847996785,58.778625437108,
58.8663236373786,58.9541474558496,58.9774475928187,59.0665491959921,59.1535112710725,
59.2403929922435,59.3272158153754,59.4179769660831,59.5047630081782,59.5915521904114,
59.6783867689599,59.690260418206),.UNSPECIFIED.);
#2005=B_SPLINE_CURVE_WITH_KNOTS('',3,(#21966,#21967,#21968,#21969,#21970,
#21971,#21972,#21973,#21974,#21975,#21976,#21977,#21978,#21979,#21980,#21981,
#21982,#21983,#21984,#21985,#21986,#21987,#21988,#21989,#21990,#21991,#21992,
#21993,#21994,#21995,#21996,#21997,#21998,#21999,#22000,#22001,#22002,#22003,
#22004,#22005,#22006,#22007,#22008,#22009,#22010,#22011,#22012,#22013,#22014,
#22015,#22016,#22017,#22018,#22019,#22020,#22021,#22022,#22023,#22024,#22025,
#22026,#22027,#22028,#22029,#22030,#22031,#22032,#22033,#22034,#22035,#22036,
#22037,#22038,#22039,#22040,#22041,#22042,#22043,#22044,#22045,#22046,#22047,
#22048,#22049,#22050,#22051,#22052,#22053,#22054,#22055,#22056,#22057,#22058,
#22059,#22060,#22061,#22062,#22063,#22064,#22065,#22066,#22067,#22068,#22069,
#22070,#22071,#22072,#22073,#22074,#22075,#22076,#22077,#22078,#22079,#22080,
#22081,#22082,#22083,#22084,#22085,#22086,#22087,#22088,#22089,#22090,#22091,
#22092,#22093,#22094,#22095,#22096,#22097,#22098,#22099,#22100,#22101,#22102,
#22103,#22104,#22105,#22106,#22107,#22108,#22109,#22110,#22111,#22112,#22113),
 .UNSPECIFIED.,.F.,.F.,(4,3,3,3,3,3,3,3,3,3,3,3,3,3,3,3,3,3,3,3,3,3,3,3,
3,3,3,3,3,3,3,3,3,3,3,3,3,3,3,3,3,3,3,3,3,3,3,3,3,4),(49.3487618580268,
49.4365675179812,49.5014541328574,49.5892718565182,49.6769787850765,49.7645979185153,
49.8555336173805,49.943054129715,50.0305617143339,50.1180770249574,50.2056207157755,
50.2932613531282,50.3809595533219,50.4687833717177,50.4920835094375,50.5799012330959,
50.6676081616517,50.7552272950882,50.8461629939543,50.9336835062864,51.0211910909029,
51.1087064015241,51.1962500923399,51.2838907296903,51.3715889298819,51.4594127482754,
51.4827128860175,51.5705306096754,51.6582375382308,51.7458566716667,51.836792370533,
51.9243128828645,52.0118204674805,52.099335778101,52.1868794689162,52.274520106266,
52.3622183064568,52.4500421248497,52.4733422625975,52.5604221705833,52.647391777892,
52.7342748965892,52.8210968701786,52.9078870050405,52.994666687068,53.0814572896196,
53.168330509625,53.2552470964572,53.3422944291726,53.4070751108548),
 .UNSPECIFIED.);
#2006=B_SPLINE_CURVE_WITH_KNOTS('',3,(#22114,#22115,#22116,#22117,#22118,
#22119,#22120,#22121,#22122,#22123,#22124,#22125,#22126,#22127,#22128,#22129,
#22130,#22131,#22132,#22133,#22134,#22135,#22136,#22137,#22138,#22139,#22140,
#22141,#22142,#22143,#22144,#22145,#22146,#22147,#22148,#22149,#22150,#22151,
#22152,#22153,#22154,#22155,#22156,#22157,#22158,#22159,#22160,#22161,#22162,
#22163,#22164,#22165,#22166,#22167,#22168,#22169,#22170,#22171,#22172,#22173,
#22174,#22175,#22176,#22177,#22178,#22179,#22180,#22181,#22182,#22183,#22184,
#22185,#22186,#22187,#22188,#22189,#22190,#22191,#22192,#22193,#22194,#22195,
#22196,#22197,#22198),.UNSPECIFIED.,.F.,.F.,(4,3,3,3,3,3,3,3,3,3,3,3,3,
3,3,3,3,3,3,3,3,3,3,3,3,3,3,3,4),(53.4070751110265,53.4639716391775,53.5517893628235,
53.6394962913669,53.727115424791,53.8180511236619,53.9055716359818,53.9930792205862,
54.0805945311955,54.1681382219994,54.2557788593382,54.3434770595181,54.4313008779004,
54.4546010157576,54.5424187394083,54.6301256679562,54.7177448013845,54.8086805002537,
54.8962010125774,54.9837085971854,55.0712239077979,55.1587675986051,55.2464082359467,
55.3341064361294,55.4219302545142,55.4452303923376,55.5330632331826,55.6207748462577,
55.6330521042359),.UNSPECIFIED.);
#2007=B_SPLINE_CURVE_WITH_KNOTS('',3,(#22200,#22201,#22202,#22203,#22204,
#22205,#22206,#22207,#22208,#22209,#22210,#22211,#22212,#22213,#22214,#22215,
#22216,#22217,#22218,#22219,#22220,#22221,#22222,#22223,#22224,#22225,#22226,
#22227,#22228,#22229,#22230,#22231,#22232,#22233,#22234,#22235,#22236,#22237,
#22238,#22239,#22240,#22241,#22242,#22243,#22244,#22245,#22246,#22247,#22248,
#22249,#22250,#22251,#22252,#22253,#22254,#22255,#22256,#22257,#22258,#22259,
#22260,#22261,#22262,#22263,#22264,#22265,#22266,#22267,#22268,#22269,#22270,
#22271,#22272,#22273,#22274,#22275,#22276,#22277,#22278),.UNSPECIFIED.,
 .F.,.F.,(4,3,3,3,3,3,3,3,3,3,3,3,3,3,3,3,3,3,3,3,3,3,3,3,3,3,4),(53.4070751110265,
53.4952697145472,53.5834738756985,53.6717071431052,53.7600512896597,53.8484511190458,
53.9370104138994,54.0243007099186,54.1121184335766,54.199825362132,54.287444495568,
54.3783801944343,54.465900706766,54.5534082913819,54.6409236020024,54.7284672928175,
54.8161079301673,54.9038061303585,54.9916299487513,55.0149300864986,55.1027351464046,
55.1904358985645,55.2780531741883,55.3665748834878,55.4540907992995,55.543115405343,
55.6321400113866),.UNSPECIFIED.);
#2008=B_SPLINE_CURVE_WITH_KNOTS('',3,(#22279,#22280,#22281,#22282,#22283,
#22284,#22285,#22286,#22287,#22288,#22289,#22290,#22291,#22292,#22293,#22294,
#22295,#22296,#22297,#22298,#22299,#22300,#22301,#22302,#22303,#22304,#22305,
#22306,#22307,#22308,#22309,#22310,#22311,#22312,#22313,#22314,#22315,#22316,
#22317,#22318,#22319,#22320,#22321,#22322,#22323,#22324,#22325,#22326,#22327,
#22328,#22329,#22330,#22331,#22332,#22333,#22334,#22335,#22336,#22337,#22338,
#22339,#22340,#22341,#22342,#22343,#22344,#22345,#22346,#22347,#22348,#22349,
#22350,#22351,#22352,#22353,#22354,#22355,#22356,#22357,#22358,#22359,#22360,
#22361,#22362,#22363,#22364,#22365,#22366,#22367,#22368,#22369,#22370,#22371,
#22372,#22373,#22374,#22375,#22376,#22377,#22378,#22379,#22380,#22381,#22382,
#22383,#22384,#22385,#22386,#22387,#22388,#22389,#22390,#22391,#22392,#22393,
#22394,#22395,#22396,#22397,#22398,#22399,#22400,#22401,#22402,#22403,#22404,
#22405,#22406,#22407,#22408,#22409,#22410,#22411,#22412,#22413,#22414,#22415,
#22416,#22417,#22418,#22419,#22420,#22421,#22422,#22423),.UNSPECIFIED.,
 .F.,.F.,(4,3,3,3,3,3,3,3,3,3,3,3,3,3,3,3,3,3,3,3,3,3,3,3,3,3,3,3,3,3,3,
3,3,3,3,3,3,3,3,3,3,3,3,3,3,3,3,3,4),(49.3498253603234,49.4388200907328,
49.5263372418594,49.6138446717405,49.7013630332064,49.7914680758044,49.8791179240511,
49.9704505638248,50.0617832035985,50.1496009272582,50.2373078558154,50.3249269892531,
50.4158626881187,50.5033832004519,50.5908907850695,50.678406095692,50.7659497865093,
50.853590423861,50.9412886240534,51.029112442448,51.0524125801785,51.1402303038378,
51.2279372323945,51.3155563658318,51.4064920646977,51.4940125770307,51.581520161648,
51.6690354722701,51.7565791630868,51.8442198004381,51.9319180006304,52.0197418190249,
52.0430419567586,52.1308596804195,52.2185666089776,52.3061857424166,52.3971214412818,
52.4846419536162,52.5721495382348,52.6596648488581,52.7472085396768,52.8348491770294,
52.922547377223,53.0103711956187,53.0336713333386,53.1327118219618,53.2314411214165,
53.3295918555088,53.4070751108161),.UNSPECIFIED.);
#2009=B_SPLINE_CURVE_WITH_KNOTS('',3,(#22429,#22430,#22431,#22432,#22433,
#22434,#22435,#22436,#22437,#22438,#22439,#22440,#22441,#22442,#22443,#22444,
#22445,#22446,#22447,#22448,#22449,#22450,#22451,#22452,#22453,#22454,#22455,
#22456,#22457,#22458,#22459,#22460,#22461,#22462,#22463,#22464,#22465,#22466,
#22467,#22468,#22469,#22470,#22471,#22472,#22473,#22474,#22475,#22476,#22477,
#22478,#22479,#22480,#22481,#22482,#22483,#22484,#22485,#22486,#22487,#22488,
#22489,#22490,#22491,#22492,#22493,#22494,#22495,#22496,#22497,#22498,#22499,
#22500,#22501,#22502,#22503,#22504,#22505,#22506,#22507,#22508,#22509,#22510,
#22511,#22512,#22513,#22514,#22515,#22516,#22517,#22518,#22519,#22520,#22521,
#22522,#22523,#22524,#22525,#22526,#22527,#22528,#22529,#22530,#22531,#22532,
#22533,#22534,#22535,#22536,#22537,#22538,#22539,#22540,#22541,#22542,#22543,
#22544,#22545,#22546,#22547,#22548,#22549,#22550,#22551,#22552,#22553,#22554,
#22555,#22556,#22557,#22558,#22559,#22560,#22561,#22562,#22563,#22564,#22565,
#22566,#22567,#22568,#22569,#22570,#22571,#22572,#22573,#22574,#22575,#22576),
 .UNSPECIFIED.,.F.,.F.,(4,3,3,3,3,3,3,3,3,3,3,3,3,3,3,3,3,3,3,3,3,3,3,3,
3,3,3,3,3,3,3,3,3,3,3,3,3,3,3,3,3,3,3,3,3,3,3,3,3,4),(43.0661023012462,
43.1536126300917,43.2411442446049,43.3287694089535,43.4164457561466,43.5042559095106,
43.5576778733773,43.6454955970372,43.7332025255944,43.8208216590323,43.9117573578979,
43.9992778702314,44.0867854548493,44.1743007654716,44.2618444562889,44.3494850936406,
44.4371832938334,44.5250071122282,44.5483072499573,44.6361249736169,44.7238319021739,
44.8114510356116,44.9023867344773,44.9899072468106,45.0774148314283,45.1649301420504,
45.2524738328672,45.3401144702188,45.4278126704111,45.5156364888057,45.5389366265373,
45.6267543501969,45.7144612787542,45.802080412192,45.8930161110577,45.980536623391,
46.0680442080088,46.1555595186313,46.2431032094489,46.3307438468006,46.4184420469933,
46.5062658653882,46.5295660031174,46.6186563250419,46.7076259258587,46.7964937259141,
46.885263700463,46.9739759768097,47.062651294479,47.1238898038469),
 .UNSPECIFIED.);
#2010=B_SPLINE_CURVE_WITH_KNOTS('',3,(#22577,#22578,#22579,#22580,#22581,
#22582,#22583,#22584,#22585,#22586,#22587,#22588,#22589,#22590,#22591,#22592,
#22593,#22594,#22595,#22596,#22597,#22598,#22599,#22600,#22601,#22602,#22603,
#22604,#22605,#22606,#22607,#22608,#22609,#22610,#22611,#22612,#22613,#22614,
#22615,#22616,#22617,#22618,#22619,#22620,#22621,#22622,#22623,#22624,#22625,
#22626,#22627,#22628,#22629,#22630,#22631,#22632,#22633,#22634,#22635,#22636,
#22637,#22638,#22639,#22640,#22641,#22642,#22643,#22644,#22645,#22646,#22647,
#22648,#22649,#22650,#22651,#22652,#22653,#22654,#22655),.UNSPECIFIED.,
 .F.,.F.,(4,3,3,3,3,3,3,3,3,3,3,3,3,3,3,3,3,3,3,3,3,3,3,3,3,3,4),(47.123889804041,
47.2229661979551,47.3199017158507,47.420048547774,47.5201953796974,47.608013103357,
47.695720031914,47.7833391653517,47.8742748642174,47.9617953765507,48.0493029611683,
48.1368182717907,48.2243619626077,48.3120025999592,48.3997008001519,48.4875246185464,
48.5108247562774,48.5986518170988,48.6863658894003,48.773976252068,48.8615284126728,
48.9490430731687,49.0365409030647,49.1240737168936,49.2116250160482,49.2992578782039,
49.3487618580268),.UNSPECIFIED.);
#2011=B_SPLINE_CURVE_WITH_KNOTS('',3,(#22657,#22658,#22659,#22660,#22661,
#22662,#22663,#22664,#22665,#22666,#22667,#22668,#22669,#22670,#22671,#22672,
#22673,#22674,#22675,#22676,#22677,#22678,#22679,#22680,#22681,#22682,#22683,
#22684,#22685,#22686,#22687,#22688,#22689,#22690,#22691,#22692,#22693,#22694,
#22695,#22696,#22697,#22698,#22699,#22700,#22701,#22702,#22703,#22704,#22705,
#22706,#22707,#22708,#22709,#22710,#22711,#22712,#22713,#22714,#22715,#22716,
#22717,#22718,#22719,#22720,#22721,#22722,#22723,#22724,#22725,#22726,#22727,
#22728,#22729,#22730,#22731,#22732,#22733,#22734,#22735,#22736,#22737,#22738),
 .UNSPECIFIED.,.F.,.F.,(4,3,3,3,3,3,3,3,3,3,3,3,3,3,3,3,3,3,3,3,3,3,3,3,
3,3,3,4),(47.1238898040778,47.2112205230625,47.2984421477901,47.3855782233591,
47.4726547355854,47.5596998923632,47.646734849843,47.7337807519318,47.8209134726754,
47.9080890145208,47.9954065966317,48.0805244504384,48.1683421740981,48.2560491026553,
48.3436682360932,48.4346039349589,48.5221244472922,48.60963203191,48.6971473425325,
48.7846910333495,48.8723316707012,48.9600298708938,49.0478536892886,49.0711538270185,
49.1589647615717,49.2466781854582,49.3342970290963,49.3498253603234),
 .UNSPECIFIED.);
#2012=B_SPLINE_CURVE_WITH_KNOTS('',3,(#22739,#22740,#22741,#22742,#22743,
#22744,#22745,#22746,#22747,#22748,#22749,#22750,#22751,#22752,#22753,#22754,
#22755,#22756,#22757,#22758,#22759,#22760,#22761,#22762,#22763,#22764,#22765,
#22766,#22767,#22768,#22769,#22770,#22771,#22772,#22773,#22774,#22775,#22776,
#22777,#22778,#22779,#22780,#22781,#22782,#22783,#22784,#22785,#22786,#22787,
#22788,#22789,#22790,#22791,#22792,#22793,#22794,#22795,#22796,#22797,#22798,
#22799,#22800,#22801,#22802,#22803,#22804,#22805,#22806,#22807,#22808,#22809,
#22810,#22811,#22812,#22813,#22814,#22815,#22816,#22817,#22818,#22819,#22820,
#22821,#22822,#22823,#22824,#22825,#22826,#22827,#22828,#22829,#22830,#22831,
#22832,#22833,#22834,#22835,#22836,#22837,#22838,#22839,#22840,#22841,#22842,
#22843,#22844,#22845,#22846,#22847,#22848,#22849,#22850,#22851,#22852,#22853,
#22854,#22855,#22856,#22857,#22858,#22859,#22860,#22861,#22862,#22863,#22864,
#22865,#22866,#22867,#22868,#22869,#22870,#22871,#22872,#22873,#22874,#22875,
#22876,#22877,#22878,#22879,#22880,#22881,#22882,#22883,#22884,#22885,#22886,
#22887,#22888,#22889),.UNSPECIFIED.,.F.,.F.,(4,3,3,3,3,3,3,3,3,3,3,3,3,
3,3,3,3,3,3,3,3,3,3,3,3,3,3,3,3,3,3,3,3,3,3,3,3,3,3,3,3,3,3,3,3,3,3,3,3,
3,4),(43.0658096208517,43.1273775675383,43.215195291199,43.3029022197572,
43.3905213531959,43.4814570520612,43.5689775643956,43.6564851490144,43.7440004596378,
43.831544150456,43.9191847878087,44.0068829880025,44.0947068063982,44.1180069441183,
44.2058246677777,44.2935315963345,44.381150729772,44.4720864286378,44.5596069409708,
44.6471145255883,44.7346298362104,44.8221735270271,44.9098141643784,44.9975123645708,
45.0853361829653,45.1086363206984,45.1964540443581,45.2841609729151,45.3717801063527,
45.4627158052184,45.5502363175517,45.6377439021694,45.7252592127917,45.8128029036086,
45.9004435409601,45.9881417411528,46.0759655595475,46.0992656972784,46.1870834209382,
46.2747903494953,46.362409482933,46.4533451817987,46.5408656941322,46.62837327875,
46.7158885893725,46.8034322801896,46.8910729175413,46.9787711177341,47.0665949361289,
47.0898950738584,47.1238898038469),.UNSPECIFIED.);
#2013=B_SPLINE_CURVE_WITH_KNOTS('',3,(#22895,#22896,#22897,#22898,#22899,
#22900,#22901,#22902,#22903,#22904,#22905,#22906,#22907,#22908,#22909,#22910,
#22911,#22912,#22913,#22914,#22915,#22916,#22917,#22918,#22919,#22920,#22921,
#22922,#22923,#22924,#22925,#22926,#22927,#22928,#22929,#22930,#22931,#22932,
#22933,#22934,#22935,#22936,#22937,#22938,#22939,#22940,#22941,#22942,#22943,
#22944,#22945,#22946,#22947,#22948,#22949,#22950,#22951,#22952,#22953,#22954,
#22955,#22956,#22957,#22958,#22959,#22960,#22961,#22962,#22963,#22964,#22965,
#22966,#22967,#22968,#22969,#22970,#22971,#22972,#22973,#22974,#22975,#22976,
#22977,#22978,#22979,#22980,#22981,#22982,#22983,#22984,#22985,#22986,#22987,
#22988,#22989,#22990,#22991,#22992,#22993,#22994,#22995,#22996,#22997,#22998,
#22999,#23000,#23001,#23002,#23003,#23004,#23005,#23006,#23007,#23008,#23009,
#23010,#23011,#23012,#23013,#23014,#23015,#23016,#23017,#23018,#23019,#23020,
#23021,#23022,#23023,#23024,#23025,#23026,#23027,#23028,#23029,#23030,#23031,
#23032,#23033,#23034,#23035,#23036,#23037,#23038,#23039,#23040,#23041,#23042),
 .UNSPECIFIED.,.F.,.F.,(4,3,3,3,3,3,3,3,3,3,3,3,3,3,3,3,3,3,3,3,3,3,3,3,
3,3,3,3,3,3,3,3,3,3,3,3,3,3,3,3,3,3,3,3,3,3,3,3,3,4),(36.7834743401322,
36.8711071637446,36.9586711087439,37.0461970549791,37.1337056646341,37.2212175932281,
37.3087534936155,37.3963842592218,37.4840686230105,37.5718836331408,37.6139016138971,
37.7017193375657,37.7894262661317,37.8770453995785,37.9679810984408,38.0555016107834,
38.1430091954105,38.2305245060423,38.3180681968688,38.4057088342298,38.493407034432,
38.5812308528361,38.6045309904771,38.6923487141351,38.7800556426903,38.8676747761262,
38.9586104749926,39.0461309873241,39.13363857194,39.2211538825605,39.3086975733757,
39.3963382107255,39.4840364109164,39.5718602293094,39.5951603670572,39.6829780907158,
39.7706850192718,39.8583041527084,39.9492398515745,40.0367603639067,40.1242679485233,
40.2117832591444,40.2993269499602,40.3869675873106,40.4746657875022,40.5624896058956,
40.5857897436372,40.69875304535,40.809605914276,40.8407044964449),
 .UNSPECIFIED.);
#2014=B_SPLINE_CURVE_WITH_KNOTS('',3,(#23043,#23044,#23045,#23046,#23047,
#23048,#23049,#23050,#23051,#23052,#23053,#23054,#23055,#23056,#23057,#23058,
#23059,#23060,#23061,#23062,#23063,#23064,#23065,#23066,#23067,#23068,#23069,
#23070,#23071,#23072,#23073,#23074,#23075,#23076,#23077,#23078,#23079,#23080,
#23081,#23082,#23083,#23084,#23085,#23086,#23087,#23088,#23089,#23090,#23091,
#23092,#23093,#23094,#23095,#23096,#23097,#23098,#23099,#23100,#23101,#23102,
#23103,#23104,#23105,#23106,#23107,#23108,#23109,#23110,#23111,#23112,#23113,
#23114,#23115,#23116,#23117,#23118,#23119,#23120,#23121,#23122,#23123,#23124),
 .UNSPECIFIED.,.F.,.F.,(4,3,3,3,3,3,3,3,3,3,3,3,3,3,3,3,3,3,3,3,3,3,3,3,
3,3,3,4),(40.8407044966673,40.9273584362594,41.0139637234753,41.1005454082162,
41.1871250286611,41.273724117299,41.360413926364,41.4471549251205,41.5340255171113,
41.5764191202172,41.6642368438767,41.7519437724335,41.8395629058709,41.9304986047367,
42.0180191170698,42.1055267016873,42.1930420123095,42.2805857031267,42.3682263404781,
42.4559245406708,42.5437483590651,42.5670484967972,42.6548657909635,42.7425763493776,
42.8301869080249,42.917739060608,43.005257970339,43.0661023012462),
 .UNSPECIFIED.);
#2015=B_SPLINE_CURVE_WITH_KNOTS('',3,(#23126,#23127,#23128,#23129,#23130,
#23131,#23132,#23133,#23134,#23135,#23136,#23137,#23138,#23139,#23140,#23141,
#23142,#23143,#23144,#23145,#23146,#23147,#23148,#23149,#23150,#23151,#23152,
#23153,#23154,#23155,#23156,#23157,#23158,#23159,#23160,#23161,#23162,#23163,
#23164,#23165,#23166,#23167,#23168,#23169,#23170,#23171,#23172,#23173,#23174,
#23175,#23176,#23177,#23178,#23179,#23180,#23181,#23182,#23183,#23184,#23185,
#23186,#23187,#23188,#23189,#23190,#23191,#23192,#23193,#23194,#23195,#23196,
#23197,#23198,#23199,#23200,#23201,#23202,#23203,#23204),.UNSPECIFIED.,
 .F.,.F.,(4,3,3,3,3,3,3,3,3,3,3,3,3,3,3,3,3,3,3,3,3,3,3,3,3,3,4),(40.8407044968328,
40.9448640922798,41.0502373864949,41.1461188143783,41.2339365380362,41.3216434665914,
41.4092626000271,41.5001982988935,41.5877188112251,41.6752263958409,41.7627417064615,
41.8502853972766,41.9379260346264,42.0256242348173,42.1134480532102,42.1367481909583,
42.224569549295,42.31227922823,42.3999002315181,42.4874540511531,42.574972225742,
42.6624754241101,42.7499842991571,42.8375628974725,42.9251792654583,43.0129084798028,
43.0658096208517),.UNSPECIFIED.);
#2016=B_SPLINE_CURVE_WITH_KNOTS('',3,(#23205,#23206,#23207,#23208,#23209,
#23210,#23211,#23212,#23213,#23214,#23215,#23216,#23217,#23218,#23219,#23220,
#23221,#23222,#23223,#23224,#23225,#23226,#23227,#23228,#23229,#23230,#23231,
#23232,#23233,#23234,#23235,#23236,#23237,#23238,#23239,#23240,#23241,#23242,
#23243,#23244,#23245,#23246,#23247,#23248,#23249,#23250,#23251,#23252,#23253,
#23254,#23255,#23256,#23257,#23258,#23259,#23260,#23261,#23262,#23263,#23264,
#23265,#23266,#23267,#23268,#23269,#23270,#23271,#23272,#23273,#23274,#23275,
#23276,#23277,#23278,#23279,#23280,#23281,#23282,#23283,#23284,#23285,#23286,
#23287,#23288,#23289,#23290,#23291,#23292,#23293,#23294,#23295,#23296,#23297,
#23298,#23299,#23300,#23301,#23302,#23303,#23304,#23305,#23306,#23307,#23308,
#23309,#23310,#23311,#23312,#23313,#23314,#23315,#23316,#23317,#23318,#23319,
#23320,#23321,#23322,#23323,#23324,#23325,#23326,#23327,#23328,#23329,#23330,
#23331,#23332,#23333,#23334,#23335,#23336,#23337,#23338,#23339,#23340,#23341,
#23342,#23343,#23344,#23345,#23346,#23347,#23348,#23349,#23350,#23351,#23352),
 .UNSPECIFIED.,.F.,.F.,(4,3,3,3,3,3,3,3,3,3,3,3,3,3,3,3,3,3,3,3,3,3,3,3,
3,3,3,3,3,3,3,3,3,3,3,3,3,3,3,3,3,3,3,3,3,3,3,3,3,4),(36.7826549237052,
36.8701876778202,36.9578143457823,37.0454928584368,37.1333043041305,37.1836013080582,
37.2714190317939,37.359125960428,37.446745093943,37.5376807927799,37.6252013051928,
37.7127088898905,37.800224200593,37.8877678914908,37.9754085289231,38.0631067291966,
38.1509305476717,38.1742306846382,38.2620484082878,38.349755336835,38.4373744702625,
38.528310169132,38.6158306814555,38.7033382660635,38.7908535766762,38.8783972674837,
38.9660379048259,39.053736105009,39.1415599233944,39.1648600612182,39.2526777848656,
39.3403847134099,39.4280038468351,39.5189395457055,39.6064600580255,39.6939676426297,
39.7814829532385,39.8690266440421,39.9566672813798,40.0443654815587,40.1321892999396,
40.1554894377982,40.242885923383,40.3301773559143,40.4173849585116,40.5045298834924,
40.5916445938404,40.6787389692804,40.7658659689735,40.8407044966673),
 .UNSPECIFIED.);
#2017=B_SPLINE_CURVE_WITH_KNOTS('',3,(#23358,#23359,#23360,#23361,#23362,
#23363,#23364,#23365,#23366,#23367,#23368,#23369,#23370,#23371,#23372,#23373,
#23374,#23375,#23376,#23377,#23378,#23379,#23380,#23381,#23382,#23383,#23384,
#23385,#23386,#23387,#23388,#23389,#23390,#23391,#23392,#23393,#23394,#23395,
#23396,#23397,#23398,#23399,#23400,#23401,#23402,#23403,#23404,#23405,#23406,
#23407,#23408,#23409,#23410,#23411,#23412,#23413,#23414,#23415,#23416,#23417,
#23418,#23419,#23420,#23421,#23422,#23423,#23424,#23425,#23426,#23427,#23428,
#23429,#23430,#23431,#23432,#23433,#23434,#23435,#23436,#23437,#23438,#23439,
#23440,#23441,#23442,#23443,#23444,#23445,#23446,#23447,#23448,#23449,#23450,
#23451,#23452,#23453,#23454,#23455,#23456,#23457,#23458,#23459,#23460,#23461,
#23462,#23463,#23464,#23465,#23466,#23467,#23468,#23469,#23470,#23471,#23472,
#23473,#23474,#23475,#23476,#23477,#23478,#23479,#23480,#23481,#23482,#23483,
#23484,#23485,#23486,#23487,#23488,#23489,#23490,#23491,#23492,#23493,#23494,
#23495,#23496,#23497,#23498,#23499,#23500,#23501,#23502,#23503,#23504,#23505),
 .UNSPECIFIED.,.F.,.F.,(4,3,3,3,3,3,3,3,3,3,3,3,3,3,3,3,3,3,3,3,3,3,3,3,
3,3,3,3,3,3,3,3,3,3,3,3,3,3,3,3,3,3,3,3,3,3,3,3,3,4),(30.499179135538,30.5893375566874,
30.6794959778369,30.7673137002222,30.855020627484,30.9426397596071,31.0335754589583,
31.1210959699375,31.2086035531887,31.2961188624336,31.3836625518638,31.4713031878215,
31.5590013866146,31.6468252036119,31.6701253544169,31.7579430786979,31.8456500078836,
31.9332691419565,32.0242048405866,32.1117253535674,32.1992329388361,32.286748250112,
32.3742919415847,32.4619325795915,32.5496307804401,32.6374545994864,32.660754730997,
32.7485724546252,32.8362793831518,32.9238985165601,33.0148342154372,33.1023547277439,
33.1898623123359,33.2773776229338,33.3649213137274,33.4525619510574,33.5402601512295,
33.6280839696054,33.651384107577,33.738220097311,33.8249459930007,33.9115858335185,
33.9981647381679,34.0847124762968,34.1712506300867,34.2578007697305,34.3444298640546,
34.4311037988402,34.5178962961427,34.557519189277),.UNSPECIFIED.);
#2018=B_SPLINE_CURVE_WITH_KNOTS('',3,(#23506,#23507,#23508,#23509,#23510,
#23511,#23512,#23513,#23514,#23515,#23516,#23517,#23518,#23519,#23520,#23521,
#23522,#23523,#23524,#23525,#23526,#23527,#23528,#23529,#23530,#23531,#23532,
#23533,#23534,#23535,#23536,#23537,#23538,#23539,#23540,#23541,#23542,#23543,
#23544,#23545,#23546,#23547,#23548,#23549,#23550,#23551,#23552,#23553,#23554,
#23555,#23556,#23557,#23558,#23559,#23560,#23561,#23562,#23563,#23564,#23565,
#23566,#23567,#23568,#23569,#23570,#23571,#23572,#23573,#23574,#23575,#23576,
#23577,#23578,#23579,#23580,#23581,#23582,#23583,#23584,#23585,#23586,#23587),
 .UNSPECIFIED.,.F.,.F.,(4,3,3,3,3,3,3,3,3,3,3,3,3,3,3,3,3,3,3,3,3,3,3,3,
3,3,3,4),(34.5575191894877,34.642013484157,34.7298312078922,34.8175381365257,
34.9051572700407,34.9960929688778,35.08361348129,35.1711210659872,35.2586363766893,
35.3461800675866,35.4338207050184,35.5215189052913,35.6093427237659,35.6326428607371,
35.7204605843868,35.8081675129339,35.8957866463615,35.986722345231,36.0742428575545,
36.1617504421624,36.2492657527751,36.3368094435825,36.4244500809247,36.5121482811081,
36.5999720994938,36.6232722373171,36.7110751645277,36.7834743401322),
 .UNSPECIFIED.);
#2019=B_SPLINE_CURVE_WITH_KNOTS('',3,(#23589,#23590,#23591,#23592,#23593,
#23594,#23595,#23596,#23597,#23598,#23599,#23600,#23601,#23602,#23603,#23604,
#23605,#23606,#23607,#23608,#23609,#23610,#23611,#23612,#23613,#23614,#23615,
#23616,#23617,#23618,#23619,#23620,#23621,#23622,#23623,#23624,#23625,#23626,
#23627,#23628,#23629,#23630,#23631,#23632,#23633,#23634,#23635,#23636,#23637,
#23638,#23639,#23640,#23641,#23642,#23643,#23644,#23645,#23646,#23647,#23648,
#23649,#23650,#23651,#23652,#23653,#23654,#23655,#23656,#23657,#23658,#23659,
#23660,#23661,#23662,#23663,#23664,#23665,#23666,#23667,#23668,#23669,#23670),
 .UNSPECIFIED.,.F.,.F.,(4,3,3,3,3,3,3,3,3,3,3,3,3,3,3,3,3,3,3,3,3,3,3,3,
3,3,3,4),(34.5575191894877,34.6452189793789,34.7329127217104,34.8206207339508,
34.9083633387032,34.9962128811143,35.0841246971867,35.1721722031937,35.2023425548981,
35.2901602785259,35.377867207052,35.4654863404597,35.556422039337,35.6439425516432,
35.731450136235,35.8189654468322,35.9065091376253,35.9941497749548,36.0818479751265,
36.1696717935019,36.1929719314781,36.2807796097188,36.3684824147923,36.4561011804982,
36.543654685054,36.6311690814345,36.7186812679009,36.7826549237052),
 .UNSPECIFIED.);
#2020=B_SPLINE_CURVE_WITH_KNOTS('',3,(#23671,#23672,#23673,#23674,#23675,
#23676,#23677,#23678,#23679,#23680,#23681,#23682,#23683,#23684,#23685,#23686,
#23687,#23688,#23689,#23690,#23691,#23692,#23693,#23694,#23695,#23696,#23697,
#23698,#23699,#23700,#23701,#23702,#23703,#23704,#23705,#23706,#23707,#23708,
#23709,#23710,#23711,#23712,#23713,#23714,#23715,#23716,#23717,#23718,#23719,
#23720,#23721,#23722,#23723,#23724,#23725,#23726,#23727,#23728,#23729,#23730,
#23731,#23732,#23733,#23734,#23735,#23736,#23737,#23738,#23739,#23740,#23741,
#23742,#23743,#23744,#23745,#23746,#23747,#23748,#23749,#23750,#23751,#23752,
#23753,#23754,#23755,#23756,#23757,#23758,#23759,#23760,#23761,#23762,#23763,
#23764,#23765,#23766,#23767,#23768,#23769,#23770,#23771,#23772,#23773,#23774,
#23775,#23776,#23777,#23778,#23779,#23780,#23781,#23782,#23783,#23784,#23785,
#23786,#23787,#23788,#23789,#23790,#23791,#23792,#23793,#23794,#23795,#23796,
#23797,#23798,#23799,#23800,#23801,#23802,#23803,#23804,#23805,#23806,#23807,
#23808,#23809,#23810,#23811,#23812,#23813,#23814,#23815,#23816,#23817,#23818),
 .UNSPECIFIED.,.F.,.F.,(4,3,3,3,3,3,3,3,3,3,3,3,3,3,3,3,3,3,3,3,3,3,3,3,
3,3,3,3,3,3,3,3,3,3,3,3,3,3,3,3,3,3,3,3,3,3,3,3,3,4),(30.5002984399058,
30.5878602452616,30.6753851607737,30.7628935103742,30.8504059492333,30.9379431304048,
31.0255755475,31.1132622557034,31.2010787172136,31.239825048578,31.3276427771969,
31.415349710767,31.5029688492647,31.5939045462514,31.6814250637303,31.7689326535164,
31.8564479693238,31.9439916653367,32.0316323078755,32.1193305132559,32.2071543367997,
32.230454425158,32.3182721490473,32.4059790778497,32.4935982115487,32.5845339103224,
32.6720544229544,32.7595620078844,32.8470773188319,32.9346210099875,33.0222616476948,
33.1099598482538,33.1977836670276,33.221083801738,33.3089015241168,33.3966084513723,
33.4842275834887,33.5751632828423,33.6626837938146,33.7501913770588,33.8377066862966,
33.9252503757199,34.0128910116704,34.1005892104557,34.1884130274459,34.2117131783181,
34.313067474497,34.4140179484392,34.5142334839579,34.5575191892806),
 .UNSPECIFIED.);
#2021=B_SPLINE_CURVE_WITH_KNOTS('',3,(#23824,#23825,#23826,#23827,#23828,
#23829,#23830,#23831,#23832,#23833,#23834,#23835,#23836,#23837,#23838,#23839,
#23840,#23841,#23842,#23843,#23844,#23845,#23846,#23847,#23848,#23849,#23850,
#23851,#23852,#23853,#23854,#23855,#23856,#23857,#23858,#23859,#23860,#23861,
#23862,#23863,#23864,#23865,#23866,#23867,#23868,#23869,#23870,#23871,#23872,
#23873,#23874,#23875,#23876,#23877,#23878,#23879,#23880,#23881,#23882,#23883,
#23884,#23885,#23886,#23887,#23888,#23889,#23890,#23891,#23892,#23893,#23894,
#23895,#23896,#23897,#23898,#23899,#23900,#23901,#23902,#23903,#23904,#23905,
#23906,#23907,#23908,#23909,#23910,#23911,#23912,#23913,#23914,#23915,#23916,
#23917,#23918,#23919,#23920,#23921,#23922,#23923,#23924,#23925,#23926,#23927,
#23928,#23929,#23930,#23931,#23932,#23933,#23934,#23935,#23936,#23937,#23938,
#23939,#23940,#23941,#23942,#23943,#23944,#23945,#23946,#23947,#23948,#23949,
#23950,#23951,#23952,#23953,#23954,#23955,#23956,#23957,#23958,#23959,#23960,
#23961,#23962,#23963,#23964,#23965,#23966,#23967,#23968,#23969,#23970,#23971),
 .UNSPECIFIED.,.F.,.F.,(4,3,3,3,3,3,3,3,3,3,3,3,3,3,3,3,3,3,3,3,3,3,3,3,
3,3,3,3,3,3,3,3,3,3,3,3,3,3,3,3,3,3,3,3,3,3,3,3,3,4),(24.2166288571228,
24.3041368674925,24.3916596706009,24.4792726971757,24.566931069276,24.6547311885646,
24.7357197183568,24.8235373294678,24.9112441438101,24.9988631615165,25.0897989031941,
25.1773192967496,25.2648267616694,25.3523419518016,25.4398855214642,25.5275260372822,
25.6152241155778,25.7030478124688,25.7263490949368,25.8141668559407,25.9018738221971,
25.9894929936409,26.0804286783753,26.1679492292338,26.2554568525008,26.3429722018544,
26.4305159314423,26.5181566074283,26.6058548462211,26.6936787028705,26.7169784715168,
26.8047962016822,26.8925031369463,26.9801222772827,27.0710579736345,27.1585784933031,
27.2460860854053,27.3336014036538,27.4211451022311,27.5087857475037,27.5964839557206,
27.6843077822307,27.7076078480968,27.7974230850532,27.8871096166564,27.9766849091007,
28.0661443963394,28.1555357321797,28.2448678041985,28.2743338823081),
 .UNSPECIFIED.);
#2022=B_SPLINE_CURVE_WITH_KNOTS('',3,(#23972,#23973,#23974,#23975,#23976,
#23977,#23978,#23979,#23980,#23981,#23982,#23983,#23984,#23985,#23986,#23987,
#23988,#23989,#23990,#23991,#23992,#23993,#23994,#23995,#23996,#23997,#23998,
#23999,#24000,#24001,#24002,#24003,#24004,#24005,#24006,#24007,#24008,#24009,
#24010,#24011,#24012,#24013,#24014,#24015,#24016,#24017,#24018,#24019,#24020,
#24021,#24022,#24023,#24024,#24025,#24026,#24027,#24028,#24029,#24030,#24031,
#24032,#24033,#24034,#24035,#24036,#24037,#24038,#24039,#24040,#24041,#24042,
#24043,#24044,#24045,#24046,#24047,#24048,#24049,#24050,#24051,#24052,#24053),
 .UNSPECIFIED.,.F.,.F.,(4,3,3,3,3,3,3,3,3,3,3,3,3,3,3,3,3,3,3,3,3,3,3,3,
3,3,3,4),(28.2743338824658,28.3691609854844,28.4643913559285,28.5598306987876,
28.655571310451,28.6982372246769,28.7860549532668,28.8737618868075,28.9613810252757,
29.0523167222734,29.1398372397223,29.227344829478,29.3148601452551,29.4024038412383,
29.4900444837466,29.5777426890967,29.6655665126103,29.6888666012569,29.7766954671533,
29.8670059257014,29.9546146136881,30.0421651506947,30.1296782383663,30.2171745458006,
30.3047008000479,30.392245862666,30.4798596297893,30.499179135538),
 .UNSPECIFIED.);
#2023=B_SPLINE_CURVE_WITH_KNOTS('',3,(#24055,#24056,#24057,#24058,#24059,
#24060,#24061,#24062,#24063,#24064,#24065,#24066,#24067,#24068,#24069,#24070,
#24071,#24072,#24073,#24074,#24075,#24076,#24077,#24078,#24079,#24080,#24081,
#24082,#24083,#24084,#24085,#24086,#24087,#24088,#24089,#24090,#24091,#24092,
#24093,#24094,#24095,#24096,#24097,#24098,#24099,#24100,#24101,#24102,#24103,
#24104,#24105,#24106,#24107,#24108,#24109,#24110,#24111,#24112,#24113,#24114,
#24115,#24116,#24117,#24118,#24119,#24120,#24121,#24122,#24123,#24124,#24125,
#24126,#24127,#24128,#24129,#24130,#24131,#24132,#24133,#24134,#24135,#24136),
 .UNSPECIFIED.,.F.,.F.,(4,3,3,3,3,3,3,3,3,3,3,3,3,3,3,3,3,3,3,3,3,3,3,3,
3,3,3,4),(28.2743338824903,28.3620519963626,28.4496594121888,28.5371792514047,
28.6273526319063,28.7147749201041,28.8021846607065,28.8896026161822,28.9770495498907,
29.0645934767364,29.1521957096281,29.2399222139786,29.2585662954179,29.3463840255884,
29.4340909608579,29.5217101012003,29.61264579755,29.7001663172262,29.7876739093364,
29.8751892275934,29.9627329261795,30.0503735714618,30.1380717796889,30.2258956062094,
30.249195671998,30.3370125939292,30.4247058191897,30.5002984399058),
 .UNSPECIFIED.);
#2024=B_SPLINE_CURVE_WITH_KNOTS('',3,(#24137,#24138,#24139,#24140,#24141,
#24142,#24143,#24144,#24145,#24146,#24147,#24148,#24149,#24150,#24151,#24152,
#24153,#24154,#24155,#24156,#24157,#24158,#24159,#24160,#24161,#24162,#24163,
#24164,#24165,#24166,#24167,#24168,#24169,#24170,#24171,#24172,#24173,#24174,
#24175,#24176,#24177,#24178,#24179,#24180,#24181,#24182,#24183,#24184,#24185,
#24186,#24187,#24188,#24189,#24190,#24191,#24192,#24193,#24194,#24195,#24196,
#24197,#24198,#24199,#24200,#24201,#24202,#24203,#24204,#24205,#24206,#24207,
#24208,#24209,#24210,#24211,#24212,#24213,#24214,#24215,#24216,#24217,#24218,
#24219,#24220,#24221,#24222,#24223,#24224,#24225,#24226,#24227,#24228,#24229,
#24230,#24231,#24232,#24233,#24234,#24235,#24236,#24237,#24238,#24239,#24240,
#24241,#24242,#24243,#24244,#24245,#24246,#24247,#24248,#24249,#24250,#24251,
#24252,#24253,#24254,#24255,#24256,#24257,#24258,#24259,#24260,#24261,#24262,
#24263,#24264,#24265,#24266,#24267,#24268,#24269,#24270,#24271,#24272,#24273,
#24274,#24275,#24276,#24277,#24278,#24279,#24280,#24281,#24282,#24283,#24284,
#24285,#24286,#24287),.UNSPECIFIED.,.F.,.F.,(4,3,3,3,3,3,3,3,3,3,3,3,3,
3,3,3,3,3,3,3,3,3,3,3,3,3,3,3,3,3,3,3,3,3,3,3,3,3,3,3,3,3,3,3,3,3,3,3,3,
3,4),(24.2161577207422,24.3054194125178,24.3932361228833,24.4809420238797,
24.5685601168336,24.6594962008666,24.7470156471117,24.8345221580275,24.9220363884866,
25.0095789938273,25.0972185432613,25.1849156528371,25.272738384953,25.2960487890978,
25.3838667793172,25.4715739764554,25.5591933801517,25.6501289783424,25.7376497633592,
25.8251576210765,25.9126732049139,26.0002171687608,26.0878580774833,26.1755565483974,
26.2633806344902,26.2866781656778,26.374495984922,26.4622030113276,26.5498222447462,
26.6407579069351,26.7282785239503,26.8157862148092,26.9033016331222,26.9908454329701,
27.0784861808025,27.1661844924512,27.2540084228901,27.2773075422579,27.3651251529403,
27.4528319668475,27.540450984113,27.6313867259536,27.7189071190562,27.8064145835193,
27.8939297731919,27.981473342392,28.0691138577458,28.1568119355757,28.2446356320024,
28.2679369188379,28.2743338823081),.UNSPECIFIED.);
#2025=B_SPLINE_CURVE_WITH_KNOTS('',3,(#24293,#24294,#24295,#24296,#24297,
#24298,#24299,#24300,#24301,#24302,#24303,#24304,#24305,#24306,#24307,#24308,
#24309,#24310,#24311,#24312,#24313,#24314,#24315,#24316,#24317,#24318,#24319,
#24320,#24321,#24322,#24323,#24324,#24325,#24326,#24327,#24328,#24329,#24330,
#24331,#24332,#24333,#24334,#24335,#24336,#24337,#24338,#24339,#24340,#24341,
#24342,#24343,#24344,#24345,#24346,#24347,#24348,#24349,#24350,#24351,#24352,
#24353,#24354,#24355,#24356,#24357,#24358,#24359,#24360,#24361,#24362,#24363,
#24364,#24365,#24366,#24367,#24368,#24369,#24370,#24371,#24372,#24373,#24374),
 .UNSPECIFIED.,.F.,.F.,(4,3,3,3,3,3,3,3,3,3,3,3,3,3,3,3,3,3,3,3,3,3,3,3,
3,3,3,4),(15.7079632679489,15.7948129073667,15.8816405851577,15.9684675747776,
16.0553151447895,16.1422596712941,16.2292557094213,16.3163945808846,16.3803843998776,
16.4682246539636,16.5559529120477,16.6435921541955,16.7345198569782,16.8220572814542,
16.9095805630079,16.9971103333933,17.0846672239183,17.1723191161491,17.2600274501478,
17.3478596747392,17.3710137764576,17.4589553852618,17.5467937138014,17.6345494372581,
17.7222397192476,17.8098921203792,17.8975365443745,17.9331346413009),
 .UNSPECIFIED.);
#2026=B_SPLINE_CURVE_WITH_KNOTS('',3,(#24376,#24377,#24378,#24379,#24380),
 .UNSPECIFIED.,.F.,.F.,(4,1,4),(14.3991256467175,15.3897550232976,15.7079551067824),
 .UNSPECIFIED.);
#2027=B_SPLINE_CURVE_WITH_KNOTS('',3,(#24384,#24385,#24386,#24387,#24388,
#24389,#24390,#24391,#24392,#24393,#24394,#24395,#24396,#24397,#24398,#24399,
#24400,#24401,#24402,#24403,#24404,#24405,#24406,#24407,#24408,#24409,#24410,
#24411,#24412,#24413,#24414,#24415,#24416,#24417,#24418,#24419,#24420,#24421,
#24422,#24423,#24424,#24425,#24426,#24427,#24428,#24429,#24430,#24431,#24432,
#24433,#24434,#24435,#24436,#24437,#24438,#24439,#24440,#24441,#24442,#24443,
#24444,#24445,#24446,#24447),.UNSPECIFIED.,.F.,.F.,(4,3,3,3,3,3,3,3,3,3,
3,3,3,3,3,3,3,3,3,3,3,4),(13.8752088702729,13.9625086734267,14.0496981221134,
14.1368008016614,14.2238420656039,14.3108508994986,14.3978484911417,14.4848560152793,
14.5719483730037,14.6590827513909,14.7463566208474,14.8294259525565,14.9162035714637,
15.0028731802399,15.0910094411765,15.1775356372996,15.2640329274542,15.3505229365851,
15.4398830193721,15.5264647163637,15.6172139920484,15.707963267733),
 .UNSPECIFIED.);
#2028=B_SPLINE_CURVE_WITH_KNOTS('',3,(#24448,#24449,#24450,#24451,#24452,
#24453,#24454,#24455,#24456,#24457,#24458,#24459,#24460,#24461,#24462,#24463,
#24464,#24465,#24466,#24467,#24468,#24469,#24470,#24471,#24472,#24473,#24474,
#24475,#24476,#24477,#24478,#24479,#24480,#24481,#24482,#24483,#24484,#24485,
#24486,#24487,#24488,#24489,#24490,#24491,#24492,#24493,#24494,#24495,#24496,
#24497,#24498,#24499,#24500,#24501,#24502,#24503,#24504,#24505,#24506,#24507,
#24508,#24509,#24510,#24511,#24512,#24513,#24514,#24515,#24516,#24517,#24518,
#24519,#24520,#24521,#24522,#24523,#24524,#24525,#24526,#24527,#24528,#24529),
 .UNSPECIFIED.,.F.,.F.,(4,3,3,3,3,3,3,3,3,3,3,3,3,3,3,3,3,3,3,3,3,3,3,3,
3,3,3,4),(15.7079632679489,15.8200553291365,15.9077986255125,15.9954301993008,
16.0829731472548,16.1739370920625,16.2613798278848,16.3488091818115,16.4362458908085,
16.5237106921039,16.6112724073114,16.6988915726886,16.7866367930526,16.8106847057165,
16.8985113458652,16.9862271592627,17.0738551349147,17.1647875033374,17.2523166917918,
17.3398328754298,17.4273566980425,17.5149088038202,17.6025576686082,17.6902639964774,
17.7780957334192,17.8013140822966,17.8891406047116,17.9338701936111),
 .UNSPECIFIED.);
#2029=B_SPLINE_CURVE_WITH_KNOTS('',3,(#24535,#24536,#24537,#24538,#24539,
#24540,#24541,#24542,#24543,#24544,#24545,#24546,#24547,#24548,#24549,#24550,
#24551,#24552,#24553,#24554,#24555,#24556,#24557,#24558,#24559,#24560,#24561,
#24562,#24563,#24564,#24565,#24566,#24567,#24568,#24569,#24570,#24571,#24572,
#24573,#24574,#24575,#24576,#24577,#24578,#24579,#24580,#24581,#24582,#24583,
#24584,#24585,#24586,#24587,#24588,#24589,#24590,#24591,#24592,#24593,#24594,
#24595,#24596,#24597,#24598,#24599,#24600,#24601,#24602,#24603,#24604,#24605,
#24606,#24607,#24608,#24609,#24610,#24611,#24612,#24613,#24614,#24615,#24616,
#24617,#24618,#24619,#24620,#24621,#24622,#24623,#24624,#24625,#24626,#24627,
#24628,#24629,#24630,#24631),.UNSPECIFIED.,.F.,.F.,(4,3,3,3,3,3,3,3,3,3,
3,3,3,3,3,3,3,3,3,3,3,3,3,3,3,3,3,3,3,3,3,3,4),(64.4958550710578,64.5877405518754,
64.6795367572376,64.7712749401722,64.8629839192416,64.9546874336248,65.0464092117959,
65.1382299601248,65.2301041586777,65.3221260934564,65.3815388542818,65.4728325704167,
65.5640050659998,65.655083664424,65.7461008284763,65.837086533478,65.9280653184272,
66.0190617110135,66.1101639042974,66.2013201136695,66.2926413727528,66.3721682308618,
66.4665065443583,66.560706841006,66.6547911225413,66.7487656647496,66.8426763541279,
66.9365429023764,67.0303849773091,67.1242488409515,67.218122240913,67.3120618969904,
67.3627976074418),.UNSPECIFIED.);
#2030=B_SPLINE_CURVE_WITH_KNOTS('',3,(#24639,#24640,#24641,#24642,#24643,
#24644,#24645,#24646,#24647,#24648,#24649,#24650,#24651,#24652,#24653,#24654,
#24655,#24656,#24657,#24658,#24659,#24660,#24661,#24662,#24663,#24664,#24665,
#24666,#24667,#24668,#24669,#24670,#24671,#24672,#24673,#24674,#24675,#24676,
#24677,#24678,#24679,#24680,#24681,#24682,#24683,#24684,#24685,#24686,#24687,
#24688,#24689,#24690,#24691,#24692,#24693,#24694,#24695,#24696,#24697,#24698,
#24699,#24700,#24701,#24702,#24703,#24704,#24705,#24706,#24707,#24708,#24709,
#24710,#24711,#24712,#24713,#24714,#24715,#24716,#24717,#24718,#24719,#24720,
#24721,#24722,#24723,#24724,#24725,#24726,#24727,#24728,#24729,#24730,#24731,
#24732,#24733,#24734,#24735,#24736,#24737,#24738,#24739,#24740,#24741,#24742,
#24743,#24744,#24745,#24746,#24747,#24748,#24749,#24750,#24751,#24752,#24753,
#24754,#24755,#24756,#24757,#24758,#24759,#24760,#24761,#24762,#24763,#24764,
#24765,#24766,#24767,#24768,#24769,#24770,#24771,#24772),.UNSPECIFIED.,
 .F.,.F.,(4,2,2,2,2,2,2,2,2,2,2,2,2,2,2,2,2,2,2,2,2,2,2,2,2,2,2,2,2,2,2,
2,2,2,2,2,2,2,2,2,2,2,2,2,2,2,2,2,2,2,2,2,2,2,2,2,2,2,2,2,2,2,2,2,2,2,4),
(-3.81628572195454,-3.80643866773546,-3.7289890269469,-3.69635642028847,
-3.67358696555601,-3.66320759461619,-3.65514947879411,-3.64613200947775,
-3.63063531030959,-3.55907881352723,-3.50755825416349,-3.49841117462634,
-3.49325168255072,-3.48862143572503,-3.48299898076068,-3.46907587129048,
-3.40635520315938,-3.35744886171428,-3.33831875457717,-3.32860719420934,
-3.32140484128649,-3.31228641200962,-3.29661977844063,-3.21096461869517,
-3.1695503074049,-3.16116346153608,-3.15621127170026,-3.15164116660213,
-3.14477432000345,-3.12611839396488,-3.06726478415051,-3.0201942606498,
-3.0012775305463,-2.99166579553305,-2.98453840907989,-2.97551984633461,
-2.96004985263678,-2.88696905702268,-2.83345567295407,-2.82454988046004,
-2.81951645394583,-2.81494804271254,-2.80940386974122,-2.7983829638169,
-2.73357372147411,-2.67347785362427,-2.65993518965042,-2.65136291329667,
-2.64324935287387,-2.6321021168385,-2.6056649026294,-2.52424439657405,-2.50434946360095,
-2.49082995178553,-2.48488795705161,-2.48038824328513,-2.47493942167255,
-2.46410293089154,-2.41853432457841,-2.37833645217606,-2.33545254736092,
-2.32278435908247,-2.314394627258,-2.30627661646385,-2.29644905848072,-2.27193380836389,
-2.2561223525901),.UNSPECIFIED.);
#2031=B_SPLINE_CURVE_WITH_KNOTS('',3,(#24778,#24779,#24780,#24781,#24782,
#24783,#24784,#24785,#24786,#24787,#24788,#24789,#24790,#24791,#24792,#24793,
#24794,#24795,#24796,#24797,#24798,#24799,#24800,#24801,#24802,#24803,#24804,
#24805,#24806,#24807,#24808,#24809,#24810,#24811,#24812,#24813,#24814,#24815,
#24816,#24817,#24818,#24819,#24820,#24821,#24822,#24823,#24824,#24825,#24826,
#24827,#24828,#24829,#24830,#24831,#24832,#24833,#24834,#24835,#24836,#24837,
#24838,#24839,#24840,#24841,#24842,#24843,#24844,#24845,#24846,#24847,#24848,
#24849,#24850,#24851,#24852,#24853,#24854,#24855,#24856,#24857,#24858,#24859,
#24860,#24861,#24862,#24863,#24864,#24865,#24866,#24867,#24868,#24869,#24870,
#24871,#24872,#24873,#24874,#24875,#24876,#24877,#24878,#24879,#24880,#24881,
#24882,#24883,#24884,#24885,#24886,#24887,#24888,#24889,#24890,#24891,#24892,
#24893,#24894,#24895,#24896,#24897,#24898,#24899,#24900,#24901,#24902,#24903,
#24904,#24905,#24906,#24907,#24908,#24909,#24910,#24911,#24912,#24913,#24914,
#24915,#24916,#24917,#24918,#24919,#24920,#24921,#24922,#24923,#24924,#24925,
#24926,#24927,#24928,#24929,#24930,#24931,#24932,#24933,#24934,#24935,#24936,
#24937,#24938,#24939,#24940,#24941,#24942,#24943,#24944,#24945,#24946,#24947,
#24948,#24949,#24950,#24951,#24952,#24953,#24954,#24955,#24956,#24957),
 .UNSPECIFIED.,.F.,.F.,(4,2,2,2,2,2,2,2,2,2,2,2,2,2,2,2,2,2,2,2,2,2,2,2,
2,2,2,2,2,2,2,2,2,2,2,2,2,2,2,2,2,2,2,2,2,2,2,2,2,2,2,2,2,2,2,2,2,2,2,2,
2,2,2,2,2,2,2,2,2,2,2,2,2,2,2,2,2,2,2,2,2,2,2,2,2,2,2,2,2,4),(-2.01531219133444,
-1.97096131187465,-1.94756113517625,-1.94012698067682,-1.93585896379917,
-1.93117853264063,-1.92401861146501,-1.90127538153087,-1.85608032338612,
-1.7953930822805,-1.77945826407955,-1.77031186389807,-1.76235986603929,
-1.75241944841608,-1.73187216898625,-1.7036030330738,-1.63827855192118,
-1.61166123377425,-1.60392378503505,-1.59912260304415,-1.59439272034915,
-1.58697909918242,-1.56155070245692,-1.50514178477934,-1.45364292800775,
-1.4402684875885,-1.43174241624239,-1.42363150611853,-1.41242250868104,
-1.38366511411774,-1.33624150178711,-1.28002778215006,-1.26961715772864,
-1.26419204985738,-1.25970042936202,-1.25375555082318,-1.24017236639701,
-1.22013779695266,-1.13714097247456,-1.11180009033715,-1.10185986700301,
-1.09371496844786,-1.08536373188661,-1.07288434001335,-1.03233235013473,
-0.990736192507835,-0.940181824435997,-0.931553161911691,-0.926558014688438,
-0.921941243659147,-0.91514398324735,-0.89569732817667,-0.861273493568097,
-0.784285653885893,-0.769118888227675,-0.760212979008701,-0.752212948901535,
-0.741854731159591,-0.718910832501713,-0.685777787176493,-0.621731810715002,
-0.601004644388216,-0.593859184212681,-0.589646692354204,-0.584937044622535,
-0.57754343499821,-0.552081844565888,-0.495521376069438,-0.443741022768495,
-0.430382057575451,-0.421885099929604,-0.413817257681648,-0.402695451495442,
-0.374366526264463,-0.32808343751111,-0.270131437119352,-0.259755235098674,
-0.254347945347254,-0.249852551390498,-0.243889204688283,-0.230266639408721,
-0.210171112010424,-0.130796095410969,-0.10267291099376,-0.0912231649876788,
-0.0831159360069332,-0.0746101682316521,-0.065963232373048,-0.0534862628334782,
-0.00100290464424951),.UNSPECIFIED.);
#2032=B_SPLINE_CURVE_WITH_KNOTS('',3,(#24958,#24959,#24960,#24961,#24962,
#24963,#24964,#24965,#24966,#24967,#24968,#24969,#24970,#24971,#24972,#24973),
 .UNSPECIFIED.,.F.,.F.,(4,3,3,3,3,4),(64.140690693207,64.2575058528083,
64.3766585668236,64.3909094777018,64.4829385165591,64.4958550710578),
 .UNSPECIFIED.);
#2033=B_SPLINE_CURVE_WITH_KNOTS('',3,(#24974,#24975,#24976,#24977,#24978,
#24979,#24980,#24981,#24982,#24983,#24984,#24985,#24986,#24987,#24988,#24989,
#24990,#24991,#24992,#24993,#24994,#24995,#24996,#24997,#24998,#24999,#25000,
#25001,#25002,#25003,#25004,#25005,#25006,#25007,#25008,#25009,#25010,#25011,
#25012,#25013,#25014,#25015,#25016,#25017,#25018,#25019,#25020,#25021,#25022,
#25023,#25024,#25025,#25026,#25027,#25028,#25029,#25030,#25031,#25032,#25033,
#25034,#25035,#25036,#25037,#25038,#25039,#25040,#25041,#25042,#25043,#25044,
#25045,#25046,#25047,#25048,#25049,#25050,#25051,#25052,#25053,#25054,#25055,
#25056,#25057,#25058,#25059,#25060,#25061,#25062,#25063,#25064,#25065,#25066,
#25067,#25068,#25069,#25070,#25071,#25072,#25073,#25074,#25075,#25076,#25077,
#25078,#25079,#25080,#25081,#25082,#25083,#25084,#25085,#25086,#25087,#25088,
#25089,#25090,#25091,#25092,#25093,#25094,#25095,#25096,#25097,#25098,#25099,
#25100,#25101,#25102,#25103,#25104,#25105,#25106,#25107,#25108,#25109,#25110,
#25111,#25112,#25113,#25114,#25115,#25116,#25117,#25118,#25119,#25120,#25121,
#25122,#25123,#25124,#25125,#25126,#25127,#25128,#25129,#25130,#25131,#25132,
#25133,#25134,#25135,#25136,#25137,#25138,#25139,#25140,#25141,#25142,#25143,
#25144,#25145,#25146,#25147,#25148,#25149,#25150,#25151,#25152,#25153,#25154,
#25155,#25156,#25157,#25158,#25159,#25160,#25161,#25162,#25163),
 .UNSPECIFIED.,.F.,.F.,(4,2,2,2,2,2,2,2,2,2,2,2,2,2,2,2,2,2,2,2,2,2,2,2,
2,2,2,2,2,2,2,2,2,2,2,2,2,2,2,2,2,2,2,2,2,2,2,2,2,2,2,2,2,2,2,2,2,2,2,2,
2,2,2,2,2,2,2,2,2,2,2,2,2,2,2,2,2,2,2,2,2,2,2,2,2,2,2,2,2,2,2,2,2,2,4),
(-2.2561223525901,-2.18794493316781,-2.16784145467791,-2.15422362973131,
-2.14827233054965,-2.14377949514829,-2.1383574728123,-2.12763696378004,
-2.07557068505986,-2.02542814297983,-1.99574320518035,-1.98441137185593,
-1.97627866777529,-1.96778863923089,-1.95459516740641,-1.90824864460455,
-1.89817232295126,-1.84077040935874,-1.82031324231676,-1.8132018540541,
-1.80899524807701,-1.80424703975124,-1.79675841565914,-1.77051407282385,
-1.71005738041494,-1.66326870247198,-1.6500470236948,-1.64154701615231,
-1.63341026123651,-1.62208140725898,-1.59245367695536,-1.54248569914341,
-1.49027052229501,-1.47955910320356,-1.47413652359918,-1.46964222528885,
-1.46368601126918,-1.45003657433854,-1.42986341020308,-1.3449342106813,
-1.32115512340047,-1.31144513322938,-1.30335826944968,-1.2949329915766,
-1.28207363598626,-1.23646386735105,-1.22321428986379,-1.16289446283588,
-1.14605691371847,-1.13943804721623,-1.1349042727704,-1.12986844816081,
-1.12103714641948,-1.06611443058207,-0.994986364904734,-0.979376181905608,
-0.970300594820869,-0.96313886242011,-0.953492839907699,-0.93454392951832,
-0.887477121232493,-0.828581870965259,-0.810035182976642,-0.80316990231603,
-0.798593420351695,-0.793649828027475,-0.785249947783325,-0.742837271944505,
-0.671029293352246,-0.647770207755661,-0.637195310418267,-0.629151311747035,
-0.620455931256036,-0.606272863559826,-0.54151183771968,-0.479609055870956,
-0.469567961823065,-0.464219184322762,-0.45971757121563,-0.453661550533784,
-0.439401333543605,-0.41792941366668,-0.369125605709504,-0.317542713439205,
-0.30405674825885,-0.295504788460245,-0.287400283035914,-0.276250164385121,
-0.247956891016996,-0.201846031289555,-0.143710562412784,-0.133296880966846,
-0.127869765806824,-0.123377778264526,-0.121332009443736),.UNSPECIFIED.);
#2034=B_SPLINE_CURVE_WITH_KNOTS('',3,(#25168,#25169,#25170,#25171,#25172,
#25173,#25174,#25175,#25176,#25177,#25178,#25179,#25180,#25181,#25182,#25183,
#25184,#25185,#25186,#25187,#25188,#25189,#25190,#25191,#25192,#25193,#25194,
#25195,#25196,#25197,#25198,#25199,#25200,#25201,#25202,#25203,#25204,#25205,
#25206,#25207,#25208,#25209,#25210,#25211,#25212,#25213,#25214,#25215,#25216,
#25217,#25218,#25219,#25220,#25221,#25222,#25223,#25224,#25225,#25226,#25227,
#25228,#25229,#25230,#25231,#25232,#25233,#25234,#25235,#25236,#25237,#25238,
#25239,#25240,#25241,#25242,#25243,#25244,#25245,#25246,#25247,#25248,#25249,
#25250,#25251,#25252,#25253,#25254,#25255,#25256,#25257,#25258,#25259,#25260,
#25261,#25262,#25263,#25264,#25265,#25266,#25267,#25268,#25269,#25270,#25271,
#25272,#25273,#25274,#25275,#25276,#25277,#25278,#25279,#25280,#25281,#25282,
#25283,#25284,#25285,#25286,#25287,#25288,#25289,#25290,#25291,#25292,#25293,
#25294,#25295,#25296,#25297,#25298,#25299,#25300,#25301,#25302,#25303,#25304,
#25305,#25306,#25307,#25308,#25309,#25310,#25311,#25312,#25313,#25314,#25315,
#25316,#25317,#25318,#25319,#25320,#25321,#25322,#25323,#25324,#25325,#25326,
#25327,#25328,#25329,#25330,#25331,#25332,#25333,#25334,#25335,#25336,#25337,
#25338,#25339,#25340,#25341,#25342,#25343,#25344,#25345,#25346,#25347,#25348,
#25349,#25350,#25351,#25352,#25353,#25354,#25355,#25356,#25357,#25358,#25359),
 .UNSPECIFIED.,.F.,.F.,(4,2,2,2,2,2,2,2,2,2,2,2,2,2,2,2,2,2,2,2,2,2,2,2,
2,2,2,2,2,2,2,2,2,2,2,2,2,2,2,2,2,2,2,2,2,2,2,2,2,2,2,2,2,2,2,2,2,2,2,2,
2,2,2,2,2,2,2,2,2,2,2,2,2,2,2,2,2,2,2,2,2,2,2,2,2,2,2,2,2,2,2,2,2,2,2,4),
(-4.14997297189533,-4.14175280985412,-4.13037581294682,-4.12223295960013,
-4.11375152378661,-4.10061097619511,-4.05524450759479,-3.99356736209229,
-3.96709865418571,-3.95959235541146,-3.95484099186147,-3.95063549212644,
-3.94353654203057,-3.92319554151643,-3.86570010853809,-3.81412382355199,
-3.79835311594367,-3.78933105270749,-3.78136549577479,-3.77124412373233,
-3.74965750732048,-3.67556716598835,-3.63231136666082,-3.62388542106676,
-3.61893613379583,-3.61436226395951,-3.6075125494846,-3.58908242772295,
-3.52272435917552,-3.48920764799781,-3.46609479234241,-3.45571694454457,
-3.44772376651123,-3.43884840681707,-3.42379430597422,-3.34567611473376,
-3.31168948387026,-3.2923933633627,-3.28562337163558,-3.28101831218048,
-3.27602491719038,-3.26739292921559,-3.21666532276177,-3.17490649941335,
-3.13454377999092,-3.12208197223847,-3.11373638625083,-3.10559262176385,
-3.09375529190372,-3.06254761665708,-2.98649192995047,-2.96703260199048,
-2.9537273454854,-2.94783011469683,-2.94338221750868,-2.93793826692684,
-2.92711143942573,-2.88161821217879,-2.84160645049755,-2.79846740250153,
-2.78578352559344,-2.77739365405816,-2.76928310847887,-2.7594740325812,
-2.73505907295769,-2.65099954408003,-2.63089631075354,-2.61727987405498,
-2.61132973271163,-2.60683699047224,-2.60141327344442,-2.59101639031986,
-2.53442580253256,-2.48719093474166,-2.45849676747668,-2.44729230058081,
-2.43917868153043,-2.43064426261403,-2.41724435874358,-2.36459778103599,
-2.31678983370526,-2.29528955557359,-2.28101511737841,-2.27495678142308,
-2.27045484688171,-2.26510755064471,-2.25507378871593,-2.19290431935607,
-2.13594938551761,-2.11923113358561,-2.1090566243364,-2.10108555629539,
-2.09209533465508,-2.07648189546139,-2.02609908967989,-2.01531219133444),
 .UNSPECIFIED.);
#2035=B_SPLINE_CURVE_WITH_KNOTS('',3,(#25361,#25362,#25363,#25364,#25365,
#25366,#25367,#25368,#25369,#25370),.UNSPECIFIED.,.F.,.F.,(4,2,2,2,4),(-0.121332009443736,
-0.117433076213923,-0.103846755183921,-0.0838035258490438,-0.000973468615732111),
 .UNSPECIFIED.);
#2036=B_SPLINE_CURVE_WITH_KNOTS('',3,(#25371,#25372,#25373,#25374,#25375,
#25376,#25377,#25378,#25379,#25380,#25381,#25382,#25383,#25384,#25385,#25386,
#25387,#25388,#25389,#25390,#25391,#25392,#25393,#25394,#25395,#25396,#25397,
#25398,#25399,#25400,#25401,#25402,#25403,#25404,#25405,#25406,#25407,#25408,
#25409,#25410,#25411,#25412,#25413,#25414,#25415,#25416,#25417,#25418,#25419,
#25420,#25421,#25422,#25423,#25424,#25425,#25426,#25427,#25428,#25429,#25430,
#25431,#25432,#25433,#25434,#25435,#25436,#25437,#25438,#25439,#25440,#25441,
#25442,#25443,#25444,#25445,#25446,#25447,#25448,#25449,#25450,#25451,#25452,
#25453,#25454,#25455,#25456,#25457,#25458,#25459,#25460,#25461,#25462,#25463,
#25464,#25465,#25466,#25467,#25468,#25469,#25470,#25471,#25472,#25473,#25474,
#25475,#25476,#25477,#25478,#25479,#25480,#25481,#25482,#25483,#25484,#25485,
#25486,#25487,#25488,#25489,#25490,#25491,#25492,#25493,#25494,#25495,#25496,
#25497,#25498,#25499,#25500,#25501,#25502,#25503,#25504,#25505,#25506,#25507,
#25508,#25509,#25510,#25511,#25512,#25513,#25514,#25515,#25516,#25517,#25518,
#25519,#25520,#25521,#25522,#25523,#25524,#25525,#25526,#25527,#25528,#25529,
#25530,#25531,#25532,#25533,#25534,#25535,#25536,#25537,#25538,#25539,#25540,
#25541,#25542,#25543,#25544,#25545,#25546,#25547,#25548,#25549,#25550),
 .UNSPECIFIED.,.F.,.F.,(4,2,2,2,2,2,2,2,2,2,2,2,2,2,2,2,2,2,2,2,2,2,2,2,
2,2,2,2,2,2,2,2,2,2,2,2,2,2,2,2,2,2,2,2,2,2,2,2,2,2,2,2,2,2,2,2,2,2,2,2,
2,2,2,2,2,2,2,2,2,2,2,2,2,2,2,2,2,2,2,2,2,2,2,2,2,2,2,2,2,4),(-4.27052942922916,
-4.25429608667662,-4.24189246233734,-4.23394077902904,-4.22637806059236,
-4.21788881580779,-4.20471119481784,-4.15669264777507,-4.09273857851959,
-4.07044249891397,-4.06333035151339,-4.05866025259778,-4.05438312449549,
-4.04690037690266,-4.02298512396386,-3.9619226238932,-3.92931818631836,
-3.90663328978521,-3.89632577966203,-3.88834058971791,-3.87942704856534,
-3.86418783388835,-3.78754415413371,-3.75277100860208,-3.73320376740374,
-3.72640049481753,-3.72178935922745,-3.71680797056926,-3.70823233804472,
-3.65874078138611,-3.61839519129027,-3.58981122413048,-3.56910490693356,
-3.55913713158848,-3.55125708078362,-3.54215973658435,-3.52645005771721,
-3.44140062524049,-3.39977130676857,-3.39139790766936,-3.38645964699668,
-3.38187920586303,-3.37499521014691,-3.35631764829852,-3.29020497394183,
-3.25672740134996,-3.23363211907124,-3.22325655728246,-3.21526304321925,
-3.20638518967482,-3.19132148289614,-3.11326159206311,-3.07923831950518,
-3.0599288293698,-3.05315679855113,-3.04855106943138,-3.04355775160095,
-3.03492742643413,-2.98424479437167,-2.94252974762593,-2.90207995312105,
-2.88961004440993,-2.88126237069658,-2.8731190523521,-2.86128689714784,
-2.83012900129916,-2.75400889655473,-2.73454282862846,-2.72123399018241,
-2.71533586833474,-2.7108876553485,-2.70544381965799,-2.69461841189559,
-2.6491539582444,-2.59445299180117,-2.57335947109049,-2.55676425383213,
-2.54757474456073,-2.5396276892574,-2.52974884828246,-2.50954160536983,
-2.41915711567073,-2.39863016650045,-2.38481135655669,-2.37882708512889,
-2.37433114919786,-2.36893101188502,-2.3583292058588,-2.30335561144317,
-2.25592392382822),.UNSPECIFIED.);
#2037=B_SPLINE_CURVE_WITH_KNOTS('',3,(#25556,#25557,#25558,#25559,#25560,
#25561,#25562,#25563,#25564,#25565,#25566,#25567,#25568,#25569,#25570,#25571,
#25572,#25573,#25574,#25575,#25576,#25577,#25578,#25579,#25580,#25581,#25582,
#25583,#25584,#25585,#25586,#25587,#25588,#25589,#25590,#25591,#25592,#25593,
#25594,#25595,#25596,#25597,#25598,#25599,#25600,#25601,#25602,#25603,#25604,
#25605,#25606,#25607,#25608,#25609,#25610,#25611,#25612,#25613,#25614,#25615,
#25616,#25617,#25618,#25619,#25620,#25621,#25622,#25623,#25624,#25625,#25626,
#25627,#25628,#25629,#25630,#25631,#25632,#25633,#25634,#25635,#25636,#25637,
#25638,#25639,#25640,#25641,#25642,#25643,#25644,#25645,#25646,#25647,#25648,
#25649,#25650,#25651,#25652,#25653,#25654,#25655,#25656,#25657,#25658,#25659,
#25660,#25661,#25662,#25663,#25664,#25665,#25666,#25667,#25668,#25669,#25670,
#25671,#25672,#25673,#25674,#25675,#25676,#25677,#25678,#25679,#25680,#25681,
#25682,#25683,#25684,#25685,#25686,#25687,#25688,#25689,#25690,#25691,#25692,
#25693,#25694,#25695,#25696,#25697,#25698,#25699,#25700,#25701,#25702,#25703,
#25704,#25705,#25706,#25707,#25708,#25709,#25710,#25711,#25712,#25713,#25714,
#25715,#25716,#25717,#25718,#25719,#25720,#25721,#25722,#25723,#25724,#25725,
#25726,#25727,#25728,#25729,#25730,#25731,#25732,#25733,#25734,#25735),
 .UNSPECIFIED.,.F.,.F.,(4,2,2,2,2,2,2,2,2,2,2,2,2,2,2,2,2,2,2,2,2,2,2,2,
2,2,2,2,2,2,2,2,2,2,2,2,2,2,2,2,2,2,2,2,2,2,2,2,2,2,2,2,2,2,2,2,2,2,2,2,
2,2,2,2,2,2,2,2,2,2,2,2,2,2,2,2,2,2,2,2,2,2,2,2,2,2,2,2,2,4),(-2.01483558329388,
-1.98146997080009,-1.9013990607951,-1.88509494854619,-1.87587112226953,
-1.86792759796362,-1.85809598862794,-1.83814631598668,-1.81102482899631,
-1.76935892470915,-1.7187272628708,-1.71009908524082,-1.70510649637509,
-1.70050108304905,-1.69372891065386,-1.674416017502,-1.64037990843735,-1.56228782284944,
-1.54722317896616,-1.53834566574842,-1.5303530491234,-1.5199794815247,-1.49689167240493,
-1.46343162693712,-1.39734653935908,-1.3786915508109,-1.37181125363298,
-1.36723185993088,-1.36229324201418,-1.35391632785418,-1.31218521735816,
-1.22725870489533,-1.21151793100958,-1.20241466060299,-1.19453648803323,
-1.18458036031997,-1.16393443449333,-1.13546984099662,-1.09503163767455,
-1.04551525724752,-1.03693915802589,-1.03195810524928,-1.02734787554124,
-1.02054666436825,-1.00099204092101,-0.966251665472124,-0.889497804930624,
-0.874268311749744,-0.865357625128378,-0.857373361616169,-0.84706473601712,
-0.824366315493667,-0.791734014558436,-0.730439506069875,-0.706837621557959,
-0.699385320367477,-0.695114480357264,-0.690439835975098,-0.683302146968559,
-0.660756391237086,-0.616280905357298,-0.554591487400057,-0.538669151672547,
-0.529527229051855,-0.521577711713218,-0.511638641921982,-0.491087788238012,
-0.462808205106245,-0.397376080178613,-0.37088946344326,-0.363163975281902,
-0.358365921414574,-0.353631480009471,-0.346203280632927,-0.320633563231771,
-0.263539306729855,-0.212920748432954,-0.199566083306558,-0.191041640922275,
-0.182924372277182,-0.171693313924057,-0.142789756659854,-0.0949498372545458,
-0.0645510533513762,-0.0348535101730009,-0.026907829164859,-0.0220624118465178,
-0.0178631925402166,-0.0131574371654451,-0.000968299569621017),
 .UNSPECIFIED.);
#2038=B_SPLINE_CURVE_WITH_KNOTS('',3,(#25736,#25737,#25738,#25739,#25740,
#25741),.UNSPECIFIED.,.F.,.F.,(4,2,4),(-4.27074430843839,-4.17177255499699,
-4.14997297189533),.UNSPECIFIED.);
#2039=B_SPLINE_CURVE_WITH_KNOTS('',3,(#25742,#25743,#25744,#25745,#25746,
#25747,#25748,#25749,#25750,#25751,#25752,#25753,#25754,#25755,#25756,#25757,
#25758,#25759,#25760,#25761,#25762,#25763,#25764,#25765,#25766,#25767,#25768,
#25769,#25770,#25771,#25772,#25773,#25774,#25775,#25776,#25777,#25778,#25779,
#25780,#25781,#25782,#25783,#25784,#25785,#25786,#25787,#25788,#25789,#25790,
#25791,#25792,#25793,#25794,#25795,#25796,#25797,#25798,#25799,#25800,#25801,
#25802,#25803,#25804,#25805,#25806,#25807,#25808,#25809,#25810,#25811,#25812,
#25813,#25814,#25815,#25816,#25817,#25818,#25819,#25820,#25821,#25822,#25823,
#25824,#25825,#25826,#25827,#25828,#25829,#25830,#25831,#25832,#25833,#25834,
#25835,#25836,#25837,#25838,#25839,#25840,#25841,#25842,#25843,#25844,#25845,
#25846,#25847,#25848,#25849,#25850,#25851,#25852,#25853,#25854,#25855,#25856,
#25857,#25858,#25859,#25860,#25861,#25862,#25863,#25864,#25865,#25866,#25867,
#25868,#25869,#25870,#25871,#25872,#25873,#25874,#25875,#25876,#25877,#25878,
#25879,#25880,#25881,#25882,#25883,#25884,#25885,#25886,#25887,#25888,#25889,
#25890,#25891,#25892,#25893,#25894,#25895,#25896,#25897,#25898,#25899,#25900,
#25901,#25902,#25903,#25904,#25905,#25906,#25907,#25908,#25909,#25910,#25911,
#25912,#25913,#25914,#25915,#25916,#25917,#25918,#25919,#25920,#25921,#25922,
#25923,#25924,#25925,#25926,#25927,#25928,#25929,#25930,#25931,#25932,#25933,
#25934,#25935),.UNSPECIFIED.,.F.,.F.,(4,2,2,2,2,2,2,2,2,2,2,2,2,2,2,2,2,
2,2,2,2,2,2,2,2,2,2,2,2,2,2,2,2,2,2,2,2,2,2,2,2,2,2,2,2,2,2,2,2,2,2,2,2,
2,2,2,2,2,2,2,2,2,2,2,2,2,2,2,2,2,2,2,2,2,2,2,2,2,2,2,2,2,2,2,2,2,2,2,2,
2,2,2,2,2,2,2,4),(-2.25592392382822,-2.25509772448687,-2.22604616088193,
-2.2147931936834,-2.20667046526772,-2.19814949501622,-2.18481979597181,
-2.13515473211171,-2.06928391620988,-2.05040305233839,-2.04349142525006,
-2.03890564972634,-2.03397616402601,-2.02564434418445,-1.98519838365541,
-1.89804659705601,-1.88275775494733,-1.87375049727423,-1.86578182040898,
-1.85563434551231,-1.83389918493884,-1.80326680949065,-1.78895291866272,
-1.72636402023525,-1.71223008409015,-1.70660547898419,-1.70205886177658,
-1.69705307334562,-1.68836334520215,-1.63267645076848,-1.56213408797115,
-1.54648335400425,-1.53739885166856,-1.52951760645157,-1.51953197034122,
-1.49872281005177,-1.46993969556415,-1.42987384975932,-1.38436881565051,
-1.3735413800765,-1.36809765563457,-1.36365022117063,-1.35775393485197,
-1.34445274399215,-1.3249993145377,-1.24906216761986,-1.21770995572906,
-1.20585609420836,-1.19844969266466,-1.19024380732931,-1.17851142796023,
-1.14552960020076,-1.08405886506413,-1.04375992626897,-1.03531772755092,
-1.03036519774514,-1.02573955510586,-1.0188557138071,-0.998611340913551,
-0.961807728180398,-0.888710974307031,-0.873265031959592,-0.864224769029754,
-0.857058841488895,-0.847365324935507,-0.828162119087105,-0.778739690749397,
-0.715111736795599,-0.701762200208794,-0.695920275116706,-0.691428623404823,
-0.686000538516135,-0.675252405452841,-0.632026708672024,-0.550141623298073,
-0.535601750725324,-0.526833217318771,-0.51881386196569,-0.508222603528512,
-0.483765704786974,-0.447274539175102,-0.392165484605573,-0.368738970813097,
-0.361303430491097,-0.35703583624684,-0.352358179246472,-0.345205180855147,
-0.3225106488646,-0.277490393886692,-0.216546810538548,-0.200615633642746,
-0.19147192401294,-0.183522738882751,-0.173586563679768,-0.153051329620543,
-0.124801908219954,-0.121337432739625),.UNSPECIFIED.);
#2040=B_SPLINE_CURVE_WITH_KNOTS('',3,(#25940,#25941,#25942,#25943,#25944,
#25945,#25946,#25947,#25948,#25949,#25950,#25951,#25952,#25953,#25954,#25955,
#25956,#25957,#25958,#25959,#25960,#25961,#25962,#25963,#25964,#25965,#25966,
#25967,#25968,#25969,#25970,#25971,#25972,#25973,#25974,#25975,#25976,#25977,
#25978,#25979,#25980,#25981,#25982,#25983,#25984,#25985,#25986,#25987,#25988,
#25989,#25990,#25991,#25992,#25993,#25994,#25995,#25996,#25997,#25998,#25999,
#26000,#26001,#26002,#26003,#26004,#26005,#26006,#26007,#26008,#26009,#26010,
#26011,#26012,#26013,#26014,#26015,#26016,#26017,#26018,#26019,#26020,#26021,
#26022,#26023,#26024,#26025,#26026,#26027,#26028,#26029,#26030,#26031,#26032,
#26033,#26034,#26035,#26036,#26037,#26038,#26039,#26040,#26041,#26042,#26043,
#26044,#26045,#26046,#26047,#26048,#26049,#26050,#26051,#26052,#26053,#26054,
#26055,#26056,#26057,#26058,#26059,#26060,#26061,#26062,#26063,#26064,#26065,
#26066,#26067,#26068,#26069,#26070,#26071,#26072,#26073,#26074,#26075,#26076,
#26077,#26078,#26079,#26080,#26081,#26082,#26083,#26084,#26085,#26086,#26087,
#26088,#26089,#26090,#26091,#26092,#26093,#26094,#26095,#26096,#26097,#26098,
#26099,#26100,#26101,#26102,#26103,#26104,#26105,#26106,#26107,#26108,#26109,
#26110,#26111,#26112,#26113,#26114,#26115,#26116,#26117,#26118,#26119,#26120,
#26121,#26122,#26123,#26124,#26125,#26126,#26127,#26128,#26129,#26130,#26131,
#26132,#26133),.UNSPECIFIED.,.F.,.F.,(4,2,2,2,2,2,2,2,2,2,2,2,2,2,2,2,2,
2,2,2,2,2,2,2,2,2,2,2,2,2,2,2,2,2,2,2,2,2,2,2,2,2,2,2,2,2,2,2,2,2,2,2,2,
2,2,2,2,2,2,2,2,2,2,2,2,2,2,2,2,2,2,2,2,2,2,2,2,2,2,2,2,2,2,2,2,2,2,2,2,
2,2,2,2,2,2,2,4),(-4.14962318045641,-4.1028957960099,-4.08275900568692,
-4.06912658694941,-4.06317385603533,-4.0586808858808,-4.0532588951427,-4.04254418367616,
-3.99908569264534,-3.96184529779788,-3.93011045994395,-3.9078403237579,
-3.89760179270109,-3.88962379880533,-3.88067061621028,-3.86523959745287,
-3.79024039014005,-3.75455682673976,-3.73468134476241,-3.72784069100265,
-3.7232225535565,-3.71825409106203,-3.70973957344812,-3.66381801838261,
-3.60658244311081,-3.57472885223454,-3.56312605608663,-3.55494288680084,
-3.54652272604857,-3.53368745502535,-3.49270668607016,-3.42685734092462,
-3.40842353150009,-3.39562367392045,-3.38981395054324,-3.3853295905105,
-3.37979394882608,-3.36849150217141,-3.30279723580273,-3.24230950096875,
-3.22877073103537,-3.22020776403621,-3.21210828654061,-3.20099001525198,
-3.17474106010809,-3.0928213271413,-3.07287792515606,-3.05933836039104,
-3.05340129179138,-3.04890953367263,-3.04347597965416,-3.03270210301197,
-2.98804432518389,-2.94981852831422,-2.91940699686237,-2.89778214898395,
-2.88765353987126,-2.87968669941273,-2.8706678483747,-2.85532494797824,
-2.7812012098716,-2.74502247619566,-2.72498228424258,-2.71812207451106,
-2.71350036536338,-2.70853880595768,-2.70005630817717,-2.65817569796323,
-2.59789249244724,-2.56521190653692,-2.55351264110632,-2.54531207950257,
-2.53789891706674,-2.52791603502456,-2.50204181511961,-2.41971468496225,
-2.39973982716349,-2.38618501249799,-2.38024525794339,-2.37575317598825,
-2.37032132615861,-2.35988651544004,-2.30402094495244,-2.25633609613713,
-2.22748416951023,-2.216258275786,-2.20814066078074,-2.19961225283119,-2.18624359390648,
-2.13506495998405,-2.06320870499089,-2.04961366545058,-2.04373013050453,
-2.03923443671887,-2.0338363107999,-2.02324313951954,-2.01483558329388),
 .UNSPECIFIED.);
#2041=B_SPLINE_CURVE_WITH_KNOTS('',3,(#26135,#26136,#26137,#26138,#26139,
#26140,#26141,#26142,#26143,#26144,#26145,#26146,#26147,#26148,#26149,#26150),
 .UNSPECIFIED.,.F.,.F.,(4,2,2,2,2,2,2,4),(-0.121337432739625,-0.0618078407377174,
-0.0331277321209469,-0.0252541111211411,-0.0204242108037896,-0.0162322866714006,
-0.0115143057840549,-0.000968283308026432),.UNSPECIFIED.);
#2042=B_SPLINE_CURVE_WITH_KNOTS('',3,(#26151,#26152,#26153,#26154,#26155,
#26156,#26157,#26158,#26159,#26160,#26161,#26162,#26163,#26164,#26165,#26166,
#26167,#26168,#26169,#26170,#26171,#26172,#26173,#26174,#26175,#26176,#26177,
#26178,#26179,#26180,#26181,#26182,#26183,#26184,#26185,#26186,#26187,#26188,
#26189,#26190,#26191,#26192,#26193,#26194,#26195,#26196,#26197,#26198,#26199,
#26200,#26201,#26202,#26203,#26204,#26205,#26206,#26207,#26208,#26209,#26210,
#26211,#26212,#26213,#26214,#26215,#26216,#26217,#26218,#26219,#26220,#26221,
#26222,#26223,#26224,#26225,#26226,#26227,#26228,#26229,#26230,#26231,#26232,
#26233,#26234,#26235,#26236,#26237,#26238,#26239,#26240,#26241,#26242,#26243,
#26244,#26245,#26246,#26247,#26248,#26249,#26250,#26251,#26252,#26253,#26254,
#26255,#26256,#26257,#26258,#26259,#26260,#26261,#26262,#26263,#26264,#26265,
#26266,#26267,#26268,#26269,#26270,#26271,#26272,#26273,#26274,#26275,#26276,
#26277,#26278,#26279,#26280,#26281,#26282,#26283,#26284,#26285,#26286,#26287,
#26288,#26289,#26290,#26291,#26292,#26293,#26294,#26295,#26296,#26297,#26298,
#26299,#26300,#26301,#26302,#26303,#26304,#26305,#26306,#26307,#26308,#26309,
#26310,#26311,#26312,#26313,#26314,#26315,#26316,#26317,#26318,#26319,#26320,
#26321,#26322,#26323,#26324,#26325,#26326),.UNSPECIFIED.,.F.,.F.,(4,2,2,
2,2,2,2,2,2,2,2,2,2,2,2,2,2,2,2,2,2,2,2,2,2,2,2,2,2,2,2,2,2,2,2,2,2,2,2,
2,2,2,2,2,2,2,2,2,2,2,2,2,2,2,2,2,2,2,2,2,2,2,2,2,2,2,2,2,2,2,2,2,2,2,2,
2,2,2,2,2,2,2,2,2,2,2,2,4),(-4.27088769108607,-4.20004372531903,-4.14914235892196,
-4.13345932591378,-4.12445452384894,-4.11648529184639,-4.10633337336792,
-4.08457294509138,-3.99632771463989,-3.97593631328513,-3.96218203730146,
-3.95620862655621,-3.95171370854859,-3.94630606005889,-3.93566562522522,
-3.88209760055788,-3.8329164599968,-3.80355051269102,-3.79225658557803,
-3.78412711381278,-3.77561918178471,-3.76235248873147,-3.71447525398381,
-3.65504464061249,-3.62900339592296,-3.62153293064927,-3.6167887482915,
-3.6119989428363,-3.60431519313883,-3.57812380107546,-3.51231833243977,
-3.4839748807748,-3.46339133305325,-3.45344491365451,-3.44549321287851,
-3.436352820761,-3.42044367120488,-3.35783884579242,-3.31405513001084,-3.291699619411,
-3.28458093032357,-3.27990932723283,-3.27563324685243,-3.26815678962916,
-3.24431268032594,-3.18318042327872,-3.15056237791546,-3.12787064523814,
-3.11756164931361,-3.10957592699966,-3.10066242502559,-3.08542491170151,
-3.00875537939623,-2.97399161419925,-2.95442714487183,-2.94762397493205,
-2.9430126787236,-2.93803084840681,-2.92945397631968,-2.87994016749372,
-2.83954993887013,-2.79689367558644,-2.78424620441127,-2.77586347760682,
-2.76774748335614,-2.75791658437811,-2.73336054434251,-2.66292898004654,
-2.62103789304483,-2.61265543376131,-2.60771519135555,-2.60313575224147,
-2.59625740450049,-2.57762166966302,-2.51146558949516,-2.47798053908104,
-2.45488169541337,-2.444505478082,-2.43651181103716,-2.42763414294334,-2.41257164953648,
-2.33450029544884,-2.30048227697617,-2.28117453168675,-2.2744026674282,
-2.26979693117235,-2.2648034725179,-2.2563897994296),.UNSPECIFIED.);
#2043=B_SPLINE_CURVE_WITH_KNOTS('',3,(#26332,#26333,#26334,#26335,#26336,
#26337,#26338,#26339,#26340,#26341,#26342,#26343,#26344,#26345,#26346,#26347,
#26348,#26349,#26350,#26351,#26352,#26353,#26354,#26355,#26356,#26357,#26358,
#26359,#26360,#26361,#26362,#26363,#26364,#26365,#26366,#26367,#26368,#26369,
#26370,#26371,#26372,#26373,#26374,#26375,#26376,#26377,#26378,#26379,#26380,
#26381,#26382,#26383,#26384,#26385,#26386,#26387,#26388,#26389,#26390,#26391,
#26392,#26393,#26394,#26395,#26396,#26397,#26398,#26399,#26400,#26401,#26402,
#26403,#26404,#26405,#26406,#26407,#26408,#26409,#26410,#26411,#26412,#26413,
#26414,#26415,#26416,#26417,#26418,#26419,#26420,#26421,#26422,#26423,#26424,
#26425,#26426,#26427,#26428,#26429,#26430,#26431,#26432,#26433,#26434,#26435,
#26436,#26437,#26438,#26439,#26440,#26441,#26442,#26443,#26444,#26445,#26446,
#26447,#26448,#26449,#26450,#26451,#26452,#26453,#26454,#26455,#26456,#26457,
#26458,#26459,#26460,#26461,#26462,#26463,#26464,#26465,#26466,#26467,#26468,
#26469,#26470,#26471,#26472,#26473,#26474,#26475,#26476,#26477,#26478,#26479,
#26480,#26481,#26482,#26483,#26484,#26485,#26486,#26487,#26488,#26489,#26490,
#26491,#26492,#26493,#26494,#26495,#26496,#26497,#26498,#26499,#26500,#26501,
#26502,#26503,#26504,#26505,#26506,#26507),.UNSPECIFIED.,.F.,.F.,(4,2,2,
2,2,2,2,2,2,2,2,2,2,2,2,2,2,2,2,2,2,2,2,2,2,2,2,2,2,2,2,2,2,2,2,2,2,2,2,
2,2,2,2,2,2,2,2,2,2,2,2,2,2,2,2,2,2,2,2,2,2,2,2,2,2,2,2,2,2,2,2,2,2,2,2,
2,2,2,2,2,2,2,2,2,2,2,2,4),(-2.01518237751153,-2.00712267182729,-1.99118164185661,
-1.98203396219234,-1.97408229311294,-1.96414428584733,-1.94361021744035,
-1.86818283021456,-1.82477456357156,-1.81627202923764,-1.81130564793156,
-1.8066853654038,-1.79983560130326,-1.77989048470612,-1.74400127065025,
-1.66927830353965,-1.65398749885286,-1.64497896036268,-1.63700907656819,
-1.62685996487116,-1.60512088576757,-1.57448259577334,-1.56016142804056,
-1.49755033751929,-1.48342800771361,-1.47780476550589,-1.47325798139218,
-1.46825028170607,-1.45955381381507,-1.40415589212679,-1.33327440080836,
-1.31764360669135,-1.3085625158484,-1.30139983486098,-1.29175690289879,
-1.27283051875749,-1.22620615384422,-1.16811132376968,-1.14856092222509,
-1.14156124308222,-1.13737299838398,-1.13259503869666,-1.12496641779449,
-1.09700639176037,-1.02650397903811,-0.989979396661249,-0.977603521736925,
-0.970106193280953,-0.961980596347843,-0.950708124087972,-0.921502356220064,
-0.872791769537386,-0.818514677423666,-0.80806324464688,-0.80262790350713,
-0.798136169257348,-0.792200997560694,-0.778673625854444,-0.758753957580906,
-0.677230124270598,-0.650589393444395,-0.639425461393946,-0.631318364546774,
-0.622770363894216,-0.609305026236667,-0.551308156133949,-0.490366365208866,
-0.474257389725327,-0.467756145605437,-0.463196460717531,-0.458092893110004,
-0.448941605778493,-0.395505074884607,-0.323317398358109,-0.30778705253575,
-0.29872841746435,-0.291564419957689,-0.281895001676472,-0.262822232408237,
-0.214022824110003,-0.151869558229802,-0.137260569222616,-0.13156168362851,
-0.126997564361412,-0.122030045159923,-0.113518120049323,-0.0671101170439002,
-0.000969905577444465),.UNSPECIFIED.);
#2044=B_SPLINE_CURVE_WITH_KNOTS('',3,(#26508,#26509,#26510,#26511,#26512,
#26513,#26514,#26515,#26516,#26517,#26518,#26519,#26520,#26521,#26522,#26523,
#26524,#26525),.UNSPECIFIED.,.F.,.F.,(4,2,2,2,2,2,2,2,4),(-4.27030726125859,
-4.25516597735123,-4.24333685644313,-4.23537379914972,-4.22781707357167,
-4.21934216175756,-4.20623630186715,-4.15957631638503,-4.14962318045641),
 .UNSPECIFIED.);
#2045=B_SPLINE_CURVE_WITH_KNOTS('',3,(#26526,#26527,#26528,#26529,#26530,
#26531,#26532,#26533,#26534,#26535,#26536,#26537,#26538,#26539,#26540,#26541,
#26542,#26543,#26544,#26545,#26546,#26547,#26548,#26549,#26550,#26551,#26552,
#26553,#26554,#26555,#26556,#26557,#26558,#26559,#26560,#26561,#26562,#26563,
#26564,#26565,#26566,#26567,#26568,#26569,#26570,#26571,#26572,#26573,#26574,
#26575,#26576,#26577,#26578,#26579,#26580,#26581,#26582,#26583,#26584,#26585,
#26586,#26587,#26588,#26589,#26590,#26591,#26592,#26593,#26594,#26595,#26596,
#26597,#26598,#26599,#26600,#26601,#26602,#26603,#26604,#26605,#26606,#26607,
#26608,#26609,#26610,#26611,#26612,#26613,#26614,#26615,#26616,#26617,#26618,
#26619,#26620,#26621,#26622,#26623,#26624,#26625,#26626,#26627,#26628,#26629,
#26630,#26631,#26632,#26633,#26634,#26635,#26636,#26637,#26638,#26639,#26640,
#26641,#26642,#26643,#26644,#26645,#26646,#26647,#26648,#26649,#26650,#26651,
#26652,#26653,#26654,#26655,#26656,#26657,#26658,#26659,#26660,#26661,#26662,
#26663,#26664,#26665,#26666,#26667,#26668,#26669,#26670,#26671,#26672,#26673,
#26674,#26675,#26676,#26677,#26678,#26679,#26680,#26681,#26682,#26683,#26684,
#26685,#26686,#26687,#26688,#26689,#26690,#26691,#26692,#26693,#26694,#26695,
#26696,#26697,#26698,#26699,#26700,#26701,#26702,#26703,#26704,#26705,#26706,
#26707,#26708,#26709,#26710,#26711,#26712,#26713),.UNSPECIFIED.,.F.,.F.,
(4,2,2,2,2,2,2,2,2,2,2,2,2,2,2,2,2,2,2,2,2,2,2,2,2,2,2,2,2,2,2,2,2,2,2,
2,2,2,2,2,2,2,2,2,2,2,2,2,2,2,2,2,2,2,2,2,2,2,2,2,2,2,2,2,2,2,2,2,2,2,2,
2,2,2,2,2,2,2,2,2,2,2,2,2,2,2,2,2,2,2,2,2,2,4),(-2.2563897994296,-2.25617264032142,
-2.20548091493677,-2.16239880479492,-2.13603967360701,-2.11649455008548,
-2.10673645545922,-2.09879612689942,-2.08951252865022,-2.0724450112368,
-2.05054452174938,-1.9913809212883,-1.94809717958013,-1.93959655682586,
-1.93463094162031,-1.93001107380822,-1.92316149683891,-1.90321368826529,
-1.86731364179743,-1.79262592726506,-1.77733406828992,-1.76832595052375,
-1.76035706376507,-1.75021007597095,-1.72847913483958,-1.69785584032169,
-1.6835832988613,-1.62109641911143,-1.60684770186615,-1.60120462159643,
-1.59665354252745,-1.59165708695002,-1.58301162189285,-1.52731288514099,
-1.45668679721837,-1.44104088890487,-1.43195720885795,-1.42407552750146,
-1.41408781097425,-1.39326820372732,-1.36446501805632,-1.32442006286722,
-1.27892357405158,-1.26809647150321,-1.26265268935592,-1.25820507785457,
-1.25230838856538,-1.23900562082609,-1.21954924184611,-1.14358421193059,
-1.11225368255816,-1.1004020157078,-1.09299578363841,-1.08478911903266,
-1.07305370419699,-1.04004773065855,-0.978484287935924,-0.938296895608987,
-0.929857768897369,-0.924905782371132,-0.920279569120465,-0.913393334851917,
-0.89312996778754,-0.856269068150209,-0.783264590511267,-0.767809334516993,
-0.758766858735784,-0.751600905690986,-0.741909614046922,-0.722719555433789,
-0.673279741278467,-0.609661140823291,-0.596298622174021,-0.590454380069076,
-0.585962399243232,-0.580535735965111,-0.569795483902219,-0.526646412262396,
-0.444631843080524,-0.43010976242088,-0.421344692650201,-0.413323926836748,
-0.402724014990961,-0.378213109111515,-0.34159938752182,-0.286177902529273,
-0.263172628756111,-0.255777931681658,-0.251517996100755,-0.246832340785092,
-0.239640249955974,-0.216564334649234,-0.170119922424535,-0.121724239606687),
 .UNSPECIFIED.);
#2046=B_SPLINE_CURVE_WITH_KNOTS('',3,(#26718,#26719,#26720,#26721,#26722,
#26723,#26724,#26725,#26726,#26727,#26728,#26729,#26730,#26731,#26732,#26733,
#26734,#26735,#26736,#26737,#26738,#26739,#26740,#26741,#26742,#26743,#26744,
#26745,#26746,#26747,#26748,#26749,#26750,#26751,#26752,#26753,#26754,#26755,
#26756,#26757,#26758,#26759,#26760,#26761,#26762,#26763,#26764,#26765,#26766,
#26767,#26768,#26769,#26770,#26771,#26772,#26773,#26774,#26775,#26776,#26777,
#26778,#26779,#26780,#26781,#26782,#26783,#26784,#26785,#26786,#26787,#26788,
#26789,#26790,#26791,#26792,#26793,#26794,#26795,#26796,#26797,#26798,#26799,
#26800,#26801,#26802,#26803,#26804,#26805,#26806,#26807,#26808,#26809,#26810,
#26811,#26812,#26813,#26814,#26815,#26816,#26817,#26818,#26819,#26820,#26821,
#26822,#26823,#26824,#26825,#26826,#26827,#26828,#26829,#26830,#26831,#26832,
#26833,#26834,#26835,#26836,#26837,#26838,#26839,#26840,#26841,#26842,#26843,
#26844,#26845,#26846,#26847,#26848,#26849,#26850,#26851,#26852,#26853,#26854,
#26855,#26856,#26857,#26858,#26859,#26860,#26861,#26862,#26863,#26864,#26865,
#26866,#26867,#26868,#26869,#26870,#26871,#26872,#26873,#26874,#26875,#26876,
#26877,#26878,#26879,#26880,#26881,#26882,#26883,#26884,#26885,#26886,#26887,
#26888,#26889,#26890,#26891,#26892,#26893,#26894,#26895,#26896,#26897,#26898,
#26899),.UNSPECIFIED.,.F.,.F.,(4,2,2,2,2,2,2,2,2,2,2,2,2,2,2,2,2,2,2,2,
2,2,2,2,2,2,2,2,2,2,2,2,2,2,2,2,2,2,2,2,2,2,2,2,2,2,2,2,2,2,2,2,2,2,2,2,
2,2,2,2,2,2,2,2,2,2,2,2,2,2,2,2,2,2,2,2,2,2,2,2,2,2,2,2,2,2,2,2,2,2,4),
(-4.150311630865,-4.10299606945067,-4.04866005705388,-4.02763646472151,
-4.01108239179314,-4.00190113589708,-3.9939533593162,-3.98406339802608,
-3.96379447430992,-3.87349631164672,-3.85297464905975,-3.83915834661892,
-3.83317449473006,-3.82867859751466,-3.82327817113619,-3.81267488599199,
-3.75791305318404,-3.70951103085173,-3.68040989731729,-3.66915040706937,
-3.66102658338615,-3.65250766041913,-3.63918796389323,-3.5898475880222,
-3.53168627666754,-3.51420208619552,-3.50188153059365,-3.49615681753122,
-3.49167467013618,-3.48606190448439,-3.47435184063762,-3.40907058508016,
-3.3487781532683,-3.33524332664059,-3.32668061176186,-3.31857983213367,
-3.3074572917442,-3.28117326184155,-3.19928156222836,-3.17933899259548,
-3.16579944878879,-3.15986203239535,-3.1553698585564,-3.14993561436056,
-3.13915984533944,-3.08863721037576,-3.03849098707347,-3.01760520099758,
-3.00113222885726,-2.99196706203714,-2.98401750621197,-2.97410481560841,
-2.95371062609174,-2.87829723089774,-2.83455551857323,-2.82611372437498,
-2.82116050704404,-2.81658746736636,-2.8097455165801,-2.7913770206207,-2.73228693213745,
-2.67531679882263,-2.66188268054417,-2.65334022653678,-2.64522853396833,
-2.63404222977097,-2.60725359781217,-2.52594021823729,-2.50604141679827,
-2.49252268731131,-2.48658854971494,-2.48209635260447,-2.47665900551617,
-2.46619983429442,-2.41081304996555,-2.36281507161715,-2.33385274932512,
-2.32261126610228,-2.31449022374852,-2.30596517243245,-2.29261662411509,
-2.24230405587675,-2.18496900304924,-2.15934795996631,-2.15191388056291,
-2.14717717336084,-2.14295913276517,-2.13579418290333,-2.11299865930798,
-2.06761808012842,-2.01518237751153),.UNSPECIFIED.);
#2047=B_SPLINE_CURVE_WITH_KNOTS('',3,(#26901,#26902,#26903,#26904,#26905,
#26906,#26907,#26908,#26909,#26910,#26911,#26912,#26913,#26914,#26915,#26916),
 .UNSPECIFIED.,.F.,.F.,(4,2,2,2,2,2,2,4),(-0.121724239606687,-0.109689116409445,
-0.0943349200454781,-0.085398485909038,-0.077419071321713,-0.0671558646773077,
-0.0559205022536955,-0.000968878777332341),.UNSPECIFIED.);
#2048=B_SPLINE_CURVE_WITH_KNOTS('',3,(#26917,#26918,#26919,#26920,#26921,
#26922,#26923,#26924,#26925,#26926,#26927,#26928,#26929,#26930,#26931,#26932,
#26933,#26934,#26935,#26936,#26937,#26938,#26939,#26940,#26941,#26942,#26943,
#26944,#26945,#26946,#26947,#26948,#26949,#26950,#26951,#26952,#26953,#26954,
#26955,#26956,#26957,#26958,#26959,#26960,#26961,#26962,#26963,#26964,#26965,
#26966,#26967,#26968,#26969,#26970,#26971,#26972,#26973,#26974,#26975,#26976,
#26977,#26978,#26979,#26980,#26981,#26982,#26983,#26984,#26985,#26986,#26987,
#26988,#26989,#26990,#26991,#26992,#26993,#26994,#26995,#26996,#26997,#26998,
#26999,#27000,#27001,#27002,#27003,#27004,#27005,#27006,#27007,#27008,#27009,
#27010,#27011,#27012,#27013,#27014,#27015,#27016,#27017,#27018,#27019,#27020,
#27021,#27022,#27023,#27024,#27025,#27026,#27027,#27028,#27029,#27030,#27031,
#27032,#27033,#27034,#27035,#27036,#27037,#27038,#27039,#27040,#27041,#27042,
#27043,#27044,#27045,#27046,#27047,#27048,#27049,#27050,#27051,#27052,#27053,
#27054,#27055,#27056,#27057,#27058,#27059,#27060,#27061,#27062,#27063,#27064,
#27065,#27066,#27067,#27068,#27069,#27070,#27071,#27072,#27073,#27074,#27075,
#27076,#27077,#27078,#27079,#27080,#27081,#27082,#27083,#27084,#27085,#27086,
#27087,#27088,#27089,#27090,#27091,#27092,#27093,#27094),.UNSPECIFIED.,
 .F.,.F.,(4,2,2,2,2,2,2,2,2,2,2,2,2,2,2,2,2,2,2,2,2,2,2,2,2,2,2,2,2,2,2,
2,2,2,2,2,2,2,2,2,2,2,2,2,2,2,2,2,2,2,2,2,2,2,2,2,2,2,2,2,2,2,2,2,2,2,2,
2,2,2,2,2,2,2,2,2,2,2,2,2,2,2,2,2,2,2,2,2,4),(-4.27045015464869,-4.20640916810718,
-4.19280331839385,-4.1868548159002,-4.18236190733064,-4.17693615137862,
-4.16620333481853,-4.12235615445556,-4.06637267137441,-4.0450377523509,
-4.02830086392083,-4.01908294880951,-4.01113813674298,-4.00129671497593,
-3.98129639143793,-3.89061914063169,-3.87007413576324,-3.85624671806726,
-3.85026097593406,-3.84576487366844,-3.84036568257061,-3.82976885373702,
-3.77510230313344,-3.7266266749074,-3.69750016649203,-3.68623725311328,
-3.67811277671187,-3.66959477443106,-3.65627992672295,-3.60709454706857,
-3.54879891223297,-3.5229826891724,-3.51553158633684,-3.51079137281393,
-3.50657624053097,-3.49942682828737,-3.47867763530581,-3.41462090646091,
-3.38149031616098,-3.35855667068276,-3.34820724436601,-3.34021640822844,
-3.3313238356518,-3.3161901806783,-3.23866728094364,-3.20435570605279,-3.18494596439479,
-3.17816136321212,-3.17355318203797,-3.16856406508616,-3.15995420526856,
-3.10969996494943,-3.06864322732716,-3.02723231353269,-3.01468240993723,
-3.0063186188984,-2.99818727124355,-2.98829591405804,-2.96334071683561,
-2.87995589929294,-2.85990049593513,-2.84630657219629,-2.84035983369153,
-2.83586679092081,-2.83043907458261,-2.8200257796388,-2.76371298148047,
-2.71629917337403,-2.68754071533038,-2.67632645442353,-2.66821011019436,
-2.65967668629844,-2.64628656644235,-2.59419721711936,-2.54575881315529,
-2.52428005794654,-2.51001496540451,-2.50395752044758,-2.49945507387976,
-2.49410576206915,-2.48406438087974,-2.40806717401893,-2.37295270227563,
-2.34910749997286,-2.3386109027513,-2.33060247116314,-2.32178599736271,
-2.30702015288851,-2.25620565721006),.UNSPECIFIED.);
#2049=B_SPLINE_CURVE_WITH_KNOTS('',3,(#27100,#27101,#27102,#27103,#27104,
#27105,#27106,#27107,#27108,#27109,#27110,#27111,#27112,#27113,#27114,#27115,
#27116,#27117,#27118,#27119,#27120,#27121,#27122,#27123,#27124,#27125,#27126,
#27127,#27128,#27129,#27130,#27131,#27132,#27133,#27134,#27135,#27136,#27137,
#27138,#27139,#27140,#27141,#27142,#27143,#27144,#27145,#27146,#27147,#27148,
#27149,#27150,#27151,#27152,#27153,#27154,#27155,#27156,#27157,#27158,#27159,
#27160,#27161,#27162,#27163,#27164,#27165,#27166,#27167,#27168,#27169,#27170,
#27171,#27172,#27173,#27174,#27175,#27176,#27177,#27178,#27179,#27180,#27181,
#27182,#27183,#27184,#27185,#27186,#27187,#27188,#27189,#27190,#27191,#27192,
#27193,#27194,#27195,#27196,#27197,#27198,#27199,#27200,#27201,#27202,#27203,
#27204,#27205,#27206,#27207,#27208,#27209,#27210,#27211,#27212,#27213,#27214,
#27215,#27216,#27217,#27218,#27219,#27220,#27221,#27222,#27223,#27224,#27225,
#27226,#27227,#27228,#27229,#27230,#27231,#27232,#27233,#27234,#27235,#27236,
#27237,#27238,#27239,#27240,#27241,#27242,#27243,#27244,#27245,#27246,#27247,
#27248,#27249,#27250,#27251,#27252,#27253,#27254,#27255,#27256,#27257,#27258,
#27259,#27260,#27261,#27262,#27263,#27264,#27265,#27266,#27267,#27268,#27269,
#27270,#27271,#27272,#27273,#27274,#27275,#27276,#27277,#27278,#27279),
 .UNSPECIFIED.,.F.,.F.,(4,2,2,2,2,2,2,2,2,2,2,2,2,2,2,2,2,2,2,2,2,2,2,2,
2,2,2,2,2,2,2,2,2,2,2,2,2,2,2,2,2,2,2,2,2,2,2,2,2,2,2,2,2,2,2,2,2,2,2,2,
2,2,2,2,2,2,2,2,2,2,2,2,2,2,2,2,2,2,2,2,2,2,2,2,2,2,2,2,2,4),(-2.01551633957596,
-1.97100294214132,-1.93094368306841,-1.92250712211063,-1.9175550915435,
-1.91292751069057,-1.90603734297219,-1.88574768779601,-1.8488109357755,
-1.77590885108523,-1.76044003913263,-1.75139356733603,-1.74422654750104,
-1.73453655721479,-1.7153596835281,-1.66592165405107,-1.60236003205732,
-1.5889210109553,-1.58306324824702,-1.57856943506887,-1.57315126665527,
-1.562457496166,-1.51975618965176,-1.43698418138697,-1.42256787867547,-1.41382358314604,
-1.40579449200453,-1.39514277907982,-1.37030500794304,-1.33294258801471,
-1.27558170491081,-1.25510795881394,-1.2479925161802,-1.24378379757422,
-1.2390360088733,-1.23154760573345,-1.20529809726063,-1.14480583622687,
-1.09807169318314,-1.08485524782977,-1.07635792298543,-1.06822333168301,
-1.0568969728353,-1.02727497182618,-0.977325459186844,-0.925052903035115,
-0.914344412661386,-0.908923649618214,-0.904430599112063,-0.898476233371473,
-0.884834196318552,-0.864675376124207,-0.779929506593619,-0.75593463786887,
-0.746231063123578,-0.73814638105055,-0.729720122856109,-0.716852606929916,
-0.671103401529981,-0.657071987480944,-0.595146126709241,-0.580266777580344,
-0.574533852783794,-0.569961289634649,-0.565009983052622,-0.556573928640137,
-0.513005122451566,-0.438075136822825,-0.417225725296742,-0.407233269581727,
-0.399279360523891,-0.390173951717792,-0.373990834946602,-0.319159360216256,
-0.254820611503855,-0.242215616854905,-0.23644079240197,-0.231958330174234,
-0.226393722524574,-0.214936164036624,-0.19910293447049,-0.164283060489829,
-0.0964739508057076,-0.0805613449356902,-0.0706123990424877,-0.0626618732903943,
-0.05517979311657,-0.0461811186475704,-0.029023611973482,-0.000968453055024552),
 .UNSPECIFIED.);
#2050=B_SPLINE_CURVE_WITH_KNOTS('',3,(#27280,#27281,#27282,#27283,#27284,
#27285,#27286,#27287,#27288,#27289,#27290,#27291,#27292,#27293,#27294,#27295),
 .UNSPECIFIED.,.F.,.F.,(4,2,2,2,2,2,2,4),(-4.27056840112397,-4.19726488735619,
-4.17775155830065,-4.17095443887722,-4.16634410714741,-4.16135979777357,
-4.15277192253053,-4.150311630865),.UNSPECIFIED.);
#2051=B_SPLINE_CURVE_WITH_KNOTS('',3,(#27296,#27297,#27298,#27299,#27300,
#27301,#27302,#27303,#27304,#27305,#27306,#27307,#27308,#27309,#27310,#27311,
#27312,#27313,#27314,#27315,#27316,#27317,#27318,#27319,#27320,#27321,#27322,
#27323,#27324,#27325,#27326,#27327,#27328,#27329,#27330,#27331,#27332,#27333,
#27334,#27335,#27336,#27337,#27338,#27339,#27340,#27341,#27342,#27343,#27344,
#27345,#27346,#27347,#27348,#27349,#27350,#27351,#27352,#27353,#27354,#27355,
#27356,#27357,#27358,#27359,#27360,#27361,#27362,#27363,#27364,#27365,#27366,
#27367,#27368,#27369,#27370,#27371,#27372,#27373,#27374,#27375,#27376,#27377,
#27378,#27379,#27380,#27381,#27382,#27383,#27384,#27385,#27386,#27387,#27388,
#27389,#27390,#27391,#27392,#27393,#27394,#27395,#27396,#27397,#27398,#27399,
#27400,#27401,#27402,#27403,#27404,#27405,#27406,#27407,#27408,#27409,#27410,
#27411,#27412,#27413,#27414,#27415,#27416,#27417,#27418,#27419,#27420,#27421,
#27422,#27423,#27424,#27425,#27426,#27427,#27428,#27429,#27430,#27431,#27432,
#27433,#27434,#27435,#27436,#27437,#27438,#27439,#27440,#27441,#27442,#27443,
#27444,#27445,#27446,#27447,#27448,#27449,#27450,#27451,#27452,#27453,#27454,
#27455,#27456,#27457,#27458,#27459,#27460,#27461,#27462,#27463,#27464,#27465,
#27466,#27467,#27468,#27469,#27470,#27471,#27472,#27473,#27474,#27475,#27476,
#27477,#27478,#27479,#27480,#27481,#27482,#27483,#27484,#27485,#27486,#27487),
 .UNSPECIFIED.,.F.,.F.,(4,2,2,2,2,2,2,2,2,2,2,2,2,2,2,2,2,2,2,2,2,2,2,2,
2,2,2,2,2,2,2,2,2,2,2,2,2,2,2,2,2,2,2,2,2,2,2,2,2,2,2,2,2,2,2,2,2,2,2,2,
2,2,2,2,2,2,2,2,2,2,2,2,2,2,2,2,2,2,2,2,2,2,2,2,2,2,2,2,2,2,2,2,2,2,2,4),
(-2.25620565721006,-2.22674092288587,-2.17861356694801,-2.17006384376556,
-2.1650876096842,-2.16052647962773,-2.15375021966668,-2.13584867970713,
-2.10485121727545,-2.02455130533443,-2.00841585248802,-1.99922720731249,
-1.99127998732835,-1.98139975680707,-1.96118516900079,-1.886341567801,-1.84187966313487,
-1.83337239223273,-1.82840520954572,-1.82378584202544,-1.81693979999276,
-1.79702333186233,-1.76121833635185,-1.68635600701543,-1.6709014944024,
-1.66194303702644,-1.65396529365384,-1.64373395712913,-1.62150869152567,
-1.5898710638916,-1.55255422062084,-1.50907080851806,-1.49835548384483,
-1.49293315610587,-1.4884399269554,-1.48248678176424,-1.468853485301,-1.44871347772828,
-1.36424333154351,-1.34002873882752,-1.33029090831023,-1.32219763087632,
-1.31378292792677,-1.30097492012888,-1.25610984146421,-1.21740752431863,
-1.17258687220201,-1.16180380234664,-1.15636845560637,-1.15187691404446,
-1.14594225158098,-1.13241706141475,-1.11250160188752,-1.03102495646972,
-1.00434833218206,-0.993179787569088,-0.985072168699662,-0.976526147784555,
-0.963069388925572,-0.905323299020189,-0.844829562827071,-0.828205390863629,
-0.82162099049646,-0.817048046047516,-0.811981325450983,-0.80300411144634,
-0.791565098502637,-0.764730777377551,-0.675964674855657,-0.660849409084116,
-0.651962019042687,-0.643972513331658,-0.633620067058567,-0.610657365934555,
-0.577463843072448,-0.512945867461247,-0.492732449152739,-0.485649855044167,
-0.481447554902438,-0.476692727640427,-0.469168693905066,-0.442487052039814,
-0.379663346979327,-0.335488782814744,-0.322421084625329,-0.313955024257332,
-0.305804270204379,-0.294378107978197,-0.263960037262439,-0.187834051313414,
-0.157993534932162,-0.150022430082447,-0.145171331567268,-0.140480200037555,
-0.133261617963766,-0.121363534210794),.UNSPECIFIED.);
#2052=B_SPLINE_CURVE_WITH_KNOTS('',3,(#27492,#27493,#27494,#27495,#27496,
#27497,#27498,#27499,#27500,#27501,#27502,#27503,#27504,#27505,#27506,#27507,
#27508,#27509,#27510,#27511,#27512,#27513,#27514,#27515,#27516,#27517,#27518,
#27519,#27520,#27521,#27522,#27523,#27524,#27525,#27526,#27527,#27528,#27529,
#27530,#27531,#27532,#27533,#27534,#27535,#27536,#27537,#27538,#27539,#27540,
#27541,#27542,#27543,#27544,#27545,#27546,#27547,#27548,#27549,#27550,#27551,
#27552,#27553,#27554,#27555,#27556,#27557,#27558,#27559,#27560,#27561,#27562,
#27563,#27564,#27565,#27566,#27567,#27568,#27569,#27570,#27571,#27572,#27573,
#27574,#27575,#27576,#27577,#27578,#27579,#27580,#27581,#27582,#27583,#27584,
#27585,#27586,#27587,#27588,#27589,#27590,#27591,#27592,#27593,#27594,#27595,
#27596,#27597,#27598,#27599,#27600,#27601,#27602,#27603,#27604,#27605,#27606,
#27607,#27608,#27609,#27610,#27611,#27612,#27613,#27614,#27615,#27616,#27617,
#27618,#27619,#27620,#27621,#27622,#27623,#27624,#27625,#27626,#27627,#27628,
#27629,#27630,#27631,#27632,#27633,#27634,#27635,#27636,#27637,#27638,#27639,
#27640,#27641,#27642,#27643,#27644,#27645,#27646,#27647,#27648,#27649,#27650,
#27651,#27652,#27653,#27654,#27655,#27656,#27657,#27658,#27659,#27660,#27661,
#27662,#27663,#27664,#27665,#27666,#27667,#27668,#27669,#27670,#27671,#27672,
#27673,#27674,#27675,#27676,#27677,#27678,#27679,#27680,#27681,#27682,#27683,
#27684,#27685),.UNSPECIFIED.,.F.,.F.,(4,2,2,2,2,2,2,2,2,2,2,2,2,2,2,2,2,
2,2,2,2,2,2,2,2,2,2,2,2,2,2,2,2,2,2,2,2,2,2,2,2,2,2,2,2,2,2,2,2,2,2,2,2,
2,2,2,2,2,2,2,2,2,2,2,2,2,2,2,2,2,2,2,2,2,2,2,2,2,2,2,2,2,2,2,2,2,2,2,2,
2,2,2,2,2,2,2,4),(-4.15043685499169,-4.1419927963705,-4.12026298144975,
-4.11011617157691,-4.10214740112473,-4.09313939879801,-4.07784758435589,
-4.00322628867515,-3.967329236326,-3.94738238206905,-3.94053314281837,-3.93591337263554,
-3.93094781458924,-3.92244702024144,-3.87896328723779,-3.80354361600812,
-3.78302437652005,-3.77308986646971,-3.76513953175498,-3.75599179194078,
-3.74004631031488,-3.68203228549128,-3.63484953189147,-3.61158047460792,
-3.60436854905171,-3.59967841803399,-3.5954216481394,-3.58804559255959,
-3.56523623776591,-3.5031541827577,-3.47036983655162,-3.4476000414642,-3.43727858967008,
-3.4292919530732,-3.4203863402354,-3.4051851838402,-3.31684715138366,-3.28986934246889,
-3.27839204643009,-3.26939110276455,-3.26431904240687,-3.25974754922955,
-3.25421199364198,-3.2406204803456,-3.17748921793959,-3.11828981083343,
-3.10478579052343,-3.09622964950842,-3.0881261934985,-3.07698561908038,
-3.05053063620219,-2.96883599039273,-2.94890917238161,-2.93537738443129,
-2.92944143940272,-2.92494955409566,-2.91951464673511,-2.90873472537767,
-2.86397913383808,-2.82548925544464,-2.78030972617508,-2.76747877868622,
-2.75905919739266,-2.7509685826569,-2.74124295120193,-2.71710846127403,
-2.63257753541481,-2.61243936553908,-2.59880592406649,-2.59285268922707,
-2.58835931440768,-2.58293680561772,-2.5722209886904,-2.52875550863412,
-2.49150493957345,-2.45977309719104,-2.43750376856466,-2.42726478468193,
-2.41928611753453,-2.4103318480017,-2.39489808849618,-2.319904261361,-2.28421062147483,
-2.26433104739607,-2.25748949931945,-2.25287089246033,-2.24790207488413,
-2.23938723230488,-2.19354971461565,-2.13624343551609,-2.10493442165203,
-2.09308368434727,-2.08567658415935,-2.07746779196152,-2.06572701939312,
-2.03268716434458,-2.01551633957596),.UNSPECIFIED.);
#2053=B_SPLINE_CURVE_WITH_KNOTS('',3,(#27687,#27688,#27689,#27690,#27691,
#27692,#27693,#27694),.UNSPECIFIED.,.F.,.F.,(4,2,2,4),(-0.121363534210794,
-0.109923186150701,-0.0624718254002537,-0.000969694913198329),
 .UNSPECIFIED.);
#2054=B_SPLINE_CURVE_WITH_KNOTS('',3,(#27695,#27696,#27697,#27698,#27699,
#27700,#27701,#27702,#27703,#27704,#27705,#27706,#27707,#27708,#27709,#27710,
#27711,#27712,#27713,#27714,#27715,#27716,#27717,#27718,#27719,#27720,#27721,
#27722,#27723,#27724,#27725,#27726,#27727,#27728,#27729,#27730,#27731,#27732,
#27733,#27734,#27735,#27736,#27737,#27738,#27739,#27740,#27741,#27742,#27743,
#27744,#27745,#27746,#27747,#27748,#27749,#27750,#27751,#27752,#27753,#27754,
#27755,#27756,#27757,#27758,#27759,#27760,#27761,#27762,#27763,#27764,#27765,
#27766,#27767,#27768,#27769,#27770,#27771,#27772,#27773,#27774,#27775,#27776,
#27777,#27778,#27779,#27780,#27781,#27782,#27783,#27784,#27785,#27786,#27787,
#27788,#27789,#27790,#27791,#27792,#27793,#27794,#27795,#27796,#27797,#27798,
#27799,#27800,#27801,#27802,#27803,#27804,#27805,#27806,#27807,#27808,#27809,
#27810,#27811,#27812,#27813,#27814,#27815,#27816,#27817,#27818,#27819,#27820,
#27821,#27822,#27823,#27824,#27825,#27826,#27827,#27828,#27829,#27830,#27831,
#27832,#27833,#27834,#27835,#27836,#27837,#27838,#27839,#27840,#27841,#27842,
#27843,#27844,#27845,#27846,#27847,#27848,#27849,#27850,#27851,#27852,#27853,
#27854,#27855,#27856,#27857,#27858,#27859,#27860,#27861,#27862,#27863,#27864,
#27865,#27866,#27867,#27868,#27869,#27870,#27871,#27872,#27873,#27874,#27875,
#27876,#27877,#27878,#27879,#27880,#27881,#27882,#27883,#27884,#27885,#27886,
#27887,#27888,#27889,#27890,#27891,#27892,#27893),.UNSPECIFIED.,.F.,.F.,
(4,3,3,3,3,3,3,3,3,3,3,3,3,3,3,3,3,3,3,3,3,3,3,3,3,3,3,3,3,3,3,3,3,3,3,
3,3,3,3,3,3,3,3,3,3,3,3,3,3,3,3,3,3,3,3,3,3,3,3,3,3,3,3,3,3,3,4),(-16.4167960594917,
-16.3231866235492,-16.2295268848231,-16.1346626699374,-16.040780714902,
-15.9454253700912,-15.8500700252804,-15.7580593298271,-15.6661696621755,
-15.574374570756,-15.4826447796787,-15.3909489505858,-15.2992633144944,
-15.207564116827,-15.1157697393145,-15.023926043559,-14.9319324069698,-14.8594406487004,
-14.7674299217847,-14.6755402223328,-14.5837450988209,-14.492015275348,
-14.4003194136853,-14.3086337448901,-14.2169345144247,-14.1251401041729,
-14.0332963756617,-13.9413027066307,-13.8688112721204,-13.7768007118962,
-13.6849111794219,-13.5931162229543,-13.5013865659418,-13.4096908703253,
-13.318005366967,-13.2263063011332,-13.1345120532514,-13.0426684861021,
-12.9506749751077,-12.8781818955404,-12.786171091896,-12.6942813167991,
-12.6024861188083,-12.5107562228943,-12.4190602900613,-12.3273745514424,
-12.2356752525775,-12.1438807765432,-12.0520369835985,-11.9600432530071,
-11.8875525189603,-11.7955415539488,-11.7036516144507,-11.6118562492808,
-11.5201261827394,-11.4284300772306,-11.3367441641075,-11.2450446891281,
-11.1532500355945,-11.0614060641193,-10.969412155172,-10.8969231423803,
-10.8060912020345,-10.7154002356709,-10.6247905981352,-10.5342411095498,
-10.4882942057671),.UNSPECIFIED.);
#2055=B_SPLINE_CURVE_WITH_KNOTS('',3,(#27899,#27900,#27901,#27902,#27903,
#27904,#27905,#27906,#27907,#27908,#27909,#27910,#27911,#27912,#27913,#27914,
#27915,#27916,#27917,#27918,#27919,#27920,#27921,#27922,#27923,#27924,#27925,
#27926,#27927,#27928,#27929,#27930,#27931,#27932,#27933,#27934,#27935,#27936,
#27937,#27938,#27939,#27940,#27941,#27942,#27943,#27944,#27945,#27946,#27947,
#27948,#27949,#27950,#27951,#27952,#27953,#27954,#27955,#27956,#27957,#27958,
#27959,#27960,#27961,#27962,#27963,#27964,#27965,#27966,#27967,#27968,#27969,
#27970,#27971,#27972,#27973,#27974,#27975,#27976,#27977,#27978,#27979,#27980,
#27981,#27982,#27983,#27984,#27985,#27986,#27987,#27988,#27989,#27990,#27991,
#27992,#27993,#27994,#27995,#27996,#27997,#27998,#27999,#28000,#28001,#28002,
#28003,#28004,#28005,#28006,#28007,#28008,#28009,#28010,#28011,#28012,#28013,
#28014,#28015,#28016,#28017,#28018,#28019,#28020,#28021,#28022,#28023,#28024),
 .UNSPECIFIED.,.F.,.F.,(4,2,2,2,2,2,2,2,2,2,2,2,2,2,2,2,2,2,2,2,2,2,2,2,
2,2,2,2,2,2,2,2,2,2,2,2,2,2,2,2,2,2,2,2,2,2,2,2,2,2,2,2,2,2,2,2,2,2,2,2,
2,2,4),(0.000239007866642453,0.00318305016454312,0.00679207464510367,0.0172466284369836,
0.0769673619474505,0.122954072103129,0.140861551821579,0.150881365847671,
0.1596828971895,0.170863291190468,0.194007000851062,0.273005688525858,0.305932246158347,
0.325093786965003,0.331890676084245,0.336513067537287,0.341376727708402,
0.34972879403149,0.393628126390447,0.468758665022071,0.487766655437066,
0.497199828562151,0.5048357524462,0.513704255035803,0.529324403857262,0.619191266485426,
0.658198851426284,0.668293771046563,0.673423197069837,0.677846792969457,
0.683626747950734,0.696674199810325,0.760803263280959,0.8107866841944,0.830135837775079,
0.839912206488528,0.847146427656818,0.856286215974925,0.871959717286507,
0.937838545693914,0.977402766009273,0.998499383907113,1.005550638497,1.0102651641193,
1.01526232509509,1.02379215622777,1.06623872462077,1.12578115720227,1.14775073965833,
1.16486976607114,1.17419354231179,1.1821771218247,1.19200168904993,1.21173750065209,
1.30303662410998,1.32365591982206,1.33752876585011,1.34353448614347,1.34803425906185,
1.35341223548036,1.36396453008937,1.41961717955807,1.42898336541552),
 .UNSPECIFIED.);
#2056=B_SPLINE_CURVE_WITH_KNOTS('',3,(#28027,#28028,#28029,#28030,#28031,
#28032,#28033,#28034,#28035,#28036,#28037,#28038,#28039,#28040,#28041,#28042,
#28043,#28044,#28045,#28046,#28047,#28048,#28049,#28050,#28051,#28052,#28053,
#28054,#28055,#28056,#28057,#28058,#28059,#28060,#28061,#28062,#28063,#28064,
#28065,#28066,#28067,#28068,#28069,#28070,#28071,#28072,#28073,#28074,#28075,
#28076,#28077,#28078,#28079,#28080,#28081,#28082,#28083,#28084,#28085,#28086,
#28087,#28088,#28089,#28090,#28091,#28092,#28093,#28094,#28095,#28096,#28097,
#28098,#28099,#28100,#28101,#28102,#28103,#28104,#28105,#28106,#28107,#28108,
#28109,#28110,#28111,#28112,#28113,#28114,#28115,#28116,#28117,#28118,#28119,
#28120,#28121,#28122,#28123,#28124,#28125,#28126,#28127,#28128,#28129,#28130,
#28131,#28132,#28133,#28134,#28135,#28136,#28137,#28138,#28139,#28140,#28141,
#28142,#28143,#28144,#28145,#28146,#28147,#28148,#28149,#28150,#28151,#28152,
#28153,#28154,#28155,#28156,#28157,#28158,#28159,#28160,#28161,#28162,#28163,
#28164,#28165,#28166,#28167,#28168,#28169,#28170,#28171,#28172,#28173,#28174,
#28175,#28176,#28177,#28178,#28179,#28180,#28181,#28182,#28183,#28184,#28185,
#28186,#28187,#28188,#28189,#28190,#28191,#28192,#28193,#28194,#28195,#28196,
#28197,#28198,#28199,#28200,#28201,#28202,#28203,#28204),.UNSPECIFIED.,
 .F.,.F.,(4,2,2,2,2,2,2,2,2,2,2,2,2,2,2,2,2,2,2,2,2,2,2,2,2,2,2,2,2,2,2,
2,2,2,2,2,2,2,2,2,2,2,2,2,2,2,2,2,2,2,2,2,2,2,2,2,2,2,2,2,2,2,2,2,2,2,2,
2,2,2,2,2,2,2,2,2,2,2,2,2,2,2,2,2,2,2,2,2,4),(-4.02407322506492,-4.01684615812316,
-3.95297570902188,-3.90421498575493,-3.88504620935784,-3.87530282427345,
-3.86807088789497,-3.8589047995826,-3.8431108092334,-3.78310802528751,-3.73942647125242,
-3.71713566051703,-3.70995356631042,-3.70521239123192,-3.70087298610828,
-3.69319560061104,-3.6674783872908,-3.60819888538897,-3.57598547663887,
-3.55347551207692,-3.54316464254709,-3.53514145305865,-3.52614721469809,
-3.51066566198414,-3.43551533470643,-3.39979648673552,-3.37988975750343,
-3.3730303874555,-3.36840094064498,-3.3634498747333,-3.35496208612577,-3.31077821760017,
-3.25221004912553,-3.22001510984916,-3.20840641653873,-3.2002529590541,
-3.19189373426824,-3.1792165221942,-3.14073896558892,-3.07209761455203,
-3.04442119374092,-3.03684141370282,-3.03209247807399,-3.02790838978219,
-3.02091953792342,-3.00145052028715,-2.94323825833587,-2.89127770623233,
-2.87544548946516,-2.86640260894449,-2.85842629218569,-2.84830073736399,
-2.82673707096946,-2.7385292621348,-2.7181541427148,-2.70440489058742,-2.6984244324262,
-2.69392191030839,-2.68850207349082,-2.67813783289135,-2.62020502255187,
-2.57387140102453,-2.5454981561429,-2.53433364362457,-2.52622347853048,
-2.51766973302586,-2.50418970510008,-2.44896022657446,-2.39571829556286,
-2.37097857255921,-2.36362402375918,-2.35890401615598,-2.35467501666104,
-2.34744182311128,-2.32595316564627,-2.26934029012784,-2.21377276203436,
-2.20039586146863,-2.19186910195483,-2.18375812457399,-2.17255001510732,
-2.14562312531643,-2.06445987829934,-2.04457410756517,-2.03106334885449,
-2.02513323148761,-2.02064327949749,-2.01520731591665,-2.01509656764977),
 .UNSPECIFIED.);
#2057=B_SPLINE_CURVE_WITH_KNOTS('',3,(#28210,#28211,#28212,#28213,#28214,
#28215,#28216,#28217,#28218,#28219,#28220,#28221,#28222,#28223,#28224,#28225,
#28226,#28227,#28228,#28229,#28230,#28231,#28232,#28233,#28234,#28235,#28236,
#28237,#28238,#28239,#28240,#28241,#28242,#28243,#28244,#28245,#28246,#28247,
#28248,#28249,#28250,#28251,#28252,#28253,#28254,#28255,#28256,#28257,#28258,
#28259,#28260,#28261,#28262,#28263,#28264,#28265,#28266,#28267,#28268,#28269,
#28270,#28271,#28272,#28273,#28274,#28275,#28276,#28277,#28278,#28279,#28280,
#28281,#28282,#28283,#28284,#28285,#28286,#28287,#28288,#28289,#28290,#28291,
#28292,#28293,#28294,#28295,#28296,#28297,#28298,#28299,#28300,#28301,#28302,
#28303,#28304,#28305,#28306,#28307,#28308,#28309,#28310,#28311,#28312,#28313,
#28314,#28315,#28316,#28317,#28318,#28319,#28320,#28321,#28322,#28323,#28324,
#28325,#28326,#28327,#28328,#28329,#28330,#28331,#28332,#28333,#28334,#28335,
#28336,#28337,#28338,#28339,#28340,#28341,#28342,#28343,#28344,#28345,#28346,
#28347,#28348,#28349,#28350,#28351,#28352,#28353,#28354),.UNSPECIFIED.,
 .F.,.F.,(4,3,3,3,3,3,3,3,3,3,3,3,3,3,3,3,3,3,3,3,3,3,3,3,3,3,3,3,3,3,3,
3,3,3,3,3,3,3,3,3,3,3,3,3,3,3,3,3,4),(74.4826134213612,74.5701017723267,
74.6575413414613,74.7449561905202,74.8323670824359,74.9197947723584,75.0073147299331,
75.0948819850037,75.182590823232,75.2578179239381,75.345788390083,75.4336477306673,
75.5214187672958,75.6122973339486,75.6999675202677,75.787623694431,75.8752863492957,
75.9629759772044,76.0507597426102,76.138599596557,76.2265618479682,76.2484473005182,
76.3363312061505,76.4241058872677,76.5117942396746,76.6027045443526,76.690297437038,
76.7778784327587,76.865468097327,76.9530869976608,77.0408037132434,77.1285785844341,
77.2164793426409,77.2390766770982,77.3260776811172,77.4129675814226,77.4997702486672,
77.5910122242935,77.677722446241,77.7644232260262,77.8511359862967,77.9378821551616,
78.0247366814142,78.1116543275945,78.1987119327436,78.2297060536782,78.3416490186313,
78.4517318766385,78.5398162005936),.UNSPECIFIED.);
#2058=B_SPLINE_CURVE_WITH_KNOTS('',3,(#28356,#28357,#28358,#28359),
 .UNSPECIFIED.,.F.,.F.,(4,4),(78.5398163397448,79.2203354302583),
 .UNSPECIFIED.);
#2059=B_SPLINE_CURVE_WITH_KNOTS('',3,(#28363,#28364,#28365,#28366,#28367,
#28368,#28369,#28370,#28371,#28372,#28373,#28374,#28375,#28376,#28377,#28378,
#28379,#28380,#28381,#28382,#28383,#28384,#28385,#28386,#28387,#28388,#28389,
#28390,#28391,#28392,#28393,#28394,#28395,#28396,#28397,#28398,#28399,#28400,
#28401,#28402,#28403,#28404,#28405),.UNSPECIFIED.,.F.,.F.,(4,3,3,3,3,3,
3,3,3,3,3,3,3,3,4),(78.5398163398758,78.6511929986185,78.7647319104916,
78.7900351244193,78.8773823755869,78.9646206369788,79.0517734317144,79.1388666078676,
79.2259284415399,79.3129800697699,79.4000426173296,79.4871912470598,79.5743826688074,
79.6617143219692,79.7442523237011),.UNSPECIFIED.);
#2060=B_SPLINE_CURVE_WITH_KNOTS('',3,(#28406,#28407,#28408,#28409,#28410,
#28411,#28412,#28413,#28414,#28415,#28416,#28417,#28418,#28419,#28420,#28421,
#28422,#28423,#28424,#28425,#28426,#28427,#28428,#28429,#28430,#28431,#28432,
#28433,#28434,#28435,#28436,#28437,#28438,#28439,#28440,#28441,#28442,#28443,
#28444,#28445,#28446,#28447,#28448,#28449,#28450,#28451,#28452,#28453,#28454,
#28455,#28456,#28457,#28458,#28459,#28460,#28461,#28462,#28463,#28464,#28465,
#28466,#28467,#28468,#28469,#28470,#28471,#28472,#28473,#28474,#28475,#28476,
#28477,#28478,#28479,#28480,#28481,#28482,#28483,#28484,#28485,#28486,#28487,
#28488,#28489,#28490,#28491,#28492,#28493,#28494,#28495,#28496,#28497,#28498,
#28499,#28500,#28501,#28502,#28503,#28504,#28505,#28506,#28507,#28508,#28509,
#28510,#28511,#28512,#28513,#28514,#28515,#28516,#28517,#28518,#28519,#28520,
#28521,#28522,#28523,#28524,#28525,#28526,#28527,#28528,#28529,#28530,#28531,
#28532,#28533,#28534,#28535,#28536,#28537,#28538,#28539,#28540,#28541,#28542,
#28543,#28544,#28545,#28546,#28547,#28548,#28549,#28550,#28551,#28552,#28553),
 .UNSPECIFIED.,.F.,.F.,(4,3,3,3,3,3,3,3,3,3,3,3,3,3,3,3,3,3,3,3,3,3,3,3,
3,3,3,3,3,3,3,3,3,3,3,3,3,3,3,3,3,3,3,3,3,3,3,3,3,4),(74.4816293874842,
74.5692291182483,74.6568738997928,74.7446611966697,74.8275176180992,74.9153514936717,
75.0030745173814,75.0907096711157,75.1816393365611,75.2691755835765,75.356698770865,
75.4442295357681,75.531788515978,75.6194441230468,75.7071571243338,75.7949953852759,
75.8181469946792,75.9059803180108,75.9937030526064,76.0813381770006,76.172267951283,
76.259804809245,76.3473288411951,76.4348606823757,76.522420968548,76.6100782122204,
76.6977930443859,76.7856334044264,76.8087763712593,76.8964962279262,76.9841050707776,
77.0716260157815,77.1625984822888,77.2500211632198,77.3374312133021,77.4248493891094,
77.5122964480626,77.5998416802232,77.6874450752849,77.7751756908071,77.7994057478393,
77.8864521187219,77.9733602235073,78.0601890785893,78.1469602031835,78.2336950644677,
78.3204372261484,78.4071825266451,78.493986476461,78.5398163397448),
 .UNSPECIFIED.);
#2061=B_SPLINE_CURVE_WITH_KNOTS('',3,(#28559,#28560,#28561,#28562,#28563,
#28564,#28565,#28566,#28567,#28568,#28569,#28570,#28571,#28572,#28573,#28574,
#28575,#28576,#28577,#28578,#28579,#28580,#28581,#28582,#28583,#28584,#28585,
#28586,#28587,#28588,#28589,#28590,#28591,#28592,#28593,#28594,#28595,#28596,
#28597,#28598,#28599,#28600,#28601,#28602,#28603,#28604,#28605,#28606,#28607,
#28608,#28609,#28610,#28611,#28612,#28613,#28614,#28615,#28616,#28617,#28618,
#28619,#28620,#28621,#28622,#28623,#28624,#28625,#28626,#28627,#28628,#28629,
#28630,#28631,#28632,#28633,#28634,#28635,#28636,#28637,#28638,#28639,#28640,
#28641,#28642,#28643,#28644,#28645,#28646,#28647,#28648,#28649,#28650,#28651,
#28652,#28653,#28654,#28655,#28656,#28657,#28658,#28659,#28660,#28661,#28662,
#28663,#28664,#28665,#28666,#28667,#28668,#28669,#28670,#28671,#28672,#28673,
#28674,#28675,#28676,#28677,#28678,#28679,#28680,#28681,#28682,#28683,#28684,
#28685,#28686,#28687,#28688,#28689,#28690,#28691,#28692,#28693,#28694,#28695,
#28696,#28697,#28698,#28699,#28700,#28701,#28702,#28703,#28704,#28705,#28706),
 .UNSPECIFIED.,.F.,.F.,(4,3,3,3,3,3,3,3,3,3,3,3,3,3,3,3,3,3,3,3,3,3,3,3,
3,3,3,3,3,3,3,3,3,3,3,3,3,3,3,3,3,3,3,3,3,3,3,3,3,4),(68.1983677761468,
68.2861854312294,68.3234122878779,68.4112283839335,68.4989336833237,68.5865511879601,
68.6774874975223,68.7650063922156,68.8525123660811,68.9400260745581,69.0275681735632,
69.115207242346,69.2029038856652,69.2907261761316,69.314041664458,69.4018609765982,
69.4895694847055,69.5771901870388,69.6681252937887,69.7556473388717,69.8431564403359,
69.9306732503291,70.0182184214548,70.1058605036167,70.1935601296495,70.2813853353724,
70.304671041038,70.392491752492,70.4802016945542,70.5678238633181,70.6587584326056,
70.7462820149109,70.8337926768927,70.9213110688809,71.0088578416761,71.0965015462834,
71.1842028087346,71.2720296586304,71.295300417618,71.3826851492496,71.4699593048868,
71.557146385153,71.6445819660545,71.7316742688595,71.8187549134235,71.9058449991257,
71.9935415074355,72.0807585750809,72.1686948037228,72.2566310323648),
 .UNSPECIFIED.);
#2062=B_SPLINE_CURVE_WITH_KNOTS('',3,(#28707,#28708,#28709,#28710,#28711,
#28712,#28713,#28714,#28715,#28716,#28717,#28718,#28719,#28720,#28721,#28722,
#28723,#28724,#28725,#28726,#28727,#28728,#28729,#28730,#28731,#28732,#28733,
#28734,#28735,#28736,#28737,#28738,#28739,#28740,#28741,#28742,#28743,#28744,
#28745,#28746,#28747,#28748,#28749,#28750,#28751,#28752,#28753,#28754,#28755,
#28756,#28757,#28758,#28759,#28760,#28761,#28762,#28763,#28764,#28765,#28766,
#28767,#28768,#28769,#28770,#28771,#28772,#28773,#28774,#28775,#28776,#28777,
#28778,#28779,#28780,#28781,#28782,#28783,#28784,#28785,#28786,#28787,#28788,
#28789,#28790,#28791),.UNSPECIFIED.,.F.,.F.,(4,3,3,3,3,3,3,3,3,3,3,3,3,
3,3,3,3,3,3,3,3,3,3,3,3,3,3,3,4),(72.2566310325652,72.2859297941981,72.3737636727309,
72.461486699375,72.5491218560152,72.6400515203606,72.7275877701938,72.8151109602629,
72.9026417279069,72.9902007108153,73.0778563205066,73.1655693243747,73.2534075878187,
73.2765591707781,73.3643925061663,73.4521152528864,73.5397503894581,73.6306801591956,
73.7182170293888,73.8057410735688,73.8932729269646,73.9808332253236,74.0684904810804,
74.1562053252846,74.244045697205,74.2671885473581,74.3549162028477,74.4425201963733,
74.4826134213612),.UNSPECIFIED.);
#2063=B_SPLINE_CURVE_WITH_KNOTS('',3,(#28793,#28794,#28795,#28796,#28797,
#28798,#28799,#28800,#28801,#28802,#28803,#28804,#28805,#28806,#28807,#28808,
#28809,#28810,#28811,#28812,#28813,#28814,#28815,#28816,#28817,#28818,#28819,
#28820,#28821,#28822,#28823,#28824,#28825,#28826,#28827,#28828,#28829,#28830,
#28831,#28832,#28833,#28834,#28835,#28836,#28837,#28838,#28839,#28840,#28841,
#28842,#28843,#28844,#28845,#28846,#28847,#28848,#28849,#28850,#28851,#28852,
#28853,#28854,#28855,#28856,#28857,#28858,#28859,#28860,#28861,#28862,#28863,
#28864,#28865,#28866,#28867,#28868,#28869,#28870,#28871,#28872,#28873,#28874),
 .UNSPECIFIED.,.F.,.F.,(4,3,3,3,3,3,3,3,3,3,3,3,3,3,3,3,3,3,3,3,3,3,3,3,
3,3,3,4),(72.2566310325652,72.3454121702325,72.4342210251386,72.5230760434829,
72.6120571169164,72.701106864289,72.7903135426155,72.8462588649391,72.9340795741427,
73.0217895139422,73.1094116804342,73.2003462505698,73.2878698305936,73.3753804902946,
73.462898880005,73.550445650528,73.6380893528825,73.7257906130895,73.8136174607711,
73.8368882415192,73.924678010106,74.0123640175841,74.0999671063111,74.1875080509712,
74.2750139307472,74.3624997101212,74.4500028156712,74.4816293874842),
 .UNSPECIFIED.);
#2064=B_SPLINE_CURVE_WITH_KNOTS('',3,(#28875,#28876,#28877,#28878,#28879,
#28880,#28881,#28882,#28883,#28884,#28885,#28886,#28887,#28888,#28889,#28890,
#28891,#28892,#28893,#28894,#28895,#28896,#28897,#28898,#28899,#28900,#28901,
#28902,#28903,#28904,#28905,#28906,#28907,#28908,#28909,#28910,#28911,#28912,
#28913,#28914,#28915,#28916,#28917,#28918,#28919,#28920,#28921,#28922,#28923,
#28924,#28925,#28926,#28927,#28928,#28929,#28930,#28931,#28932,#28933,#28934,
#28935,#28936,#28937,#28938,#28939,#28940,#28941,#28942,#28943,#28944,#28945,
#28946,#28947,#28948,#28949,#28950,#28951,#28952,#28953,#28954,#28955,#28956,
#28957,#28958,#28959,#28960,#28961,#28962,#28963,#28964,#28965,#28966,#28967,
#28968,#28969,#28970,#28971,#28972,#28973,#28974,#28975,#28976,#28977,#28978,
#28979,#28980,#28981,#28982,#28983,#28984,#28985,#28986,#28987,#28988,#28989,
#28990,#28991,#28992,#28993,#28994,#28995,#28996,#28997,#28998,#28999,#29000,
#29001,#29002,#29003,#29004,#29005,#29006,#29007,#29008,#29009,#29010,#29011,
#29012,#29013,#29014,#29015,#29016,#29017,#29018,#29019,#29020,#29021,#29022),
 .UNSPECIFIED.,.F.,.F.,(4,3,3,3,3,3,3,3,3,3,3,3,3,3,3,3,3,3,3,3,3,3,3,3,
3,3,3,3,3,3,3,3,3,3,3,3,3,3,3,3,3,3,3,3,3,3,3,3,3,4),(68.1993438421936,
68.2868799544457,68.3743918464848,68.4619001781807,68.5494256018561,68.6370424526399,
68.7247067162602,68.8125098704793,68.883741358619,68.9715592198387,69.0592662846378,
69.146885552858,69.2378212006506,69.3253418433216,69.4128495564218,69.5003649935408,
69.5879088087369,69.6755495667265,69.7632478855214,69.8510718186493,69.8743707351991,
69.9621889539972,70.0498963808031,70.1375160149733,70.228451527074,70.3159725431061,
70.403480631639,70.4909964458431,70.5785406393583,70.666181775562,70.75388047295,
70.8417047823176,70.8650001117791,70.9528162087551,71.0405215090665,71.1281390146236,
71.2190753238406,71.306594219448,71.3941001942232,71.4816139036052,71.5691560035092,
71.6567950731775,71.7444917173757,71.8323140087043,71.8556294883591,71.9558798743625,
72.0526994036399,72.149249270526,72.2454013365002,72.2566310323726),
 .UNSPECIFIED.);
#2065=B_SPLINE_CURVE_WITH_KNOTS('',3,(#29028,#29029,#29030,#29031,#29032,
#29033,#29034,#29035,#29036,#29037,#29038,#29039,#29040,#29041,#29042,#29043,
#29044,#29045,#29046,#29047,#29048,#29049,#29050,#29051,#29052,#29053,#29054,
#29055,#29056,#29057,#29058,#29059,#29060,#29061,#29062,#29063,#29064,#29065,
#29066,#29067,#29068,#29069,#29070,#29071,#29072,#29073,#29074,#29075,#29076,
#29077,#29078,#29079,#29080,#29081,#29082,#29083,#29084,#29085,#29086,#29087,
#29088,#29089,#29090,#29091,#29092,#29093,#29094,#29095,#29096,#29097,#29098,
#29099,#29100,#29101,#29102,#29103,#29104,#29105,#29106,#29107,#29108,#29109,
#29110,#29111,#29112,#29113,#29114,#29115,#29116,#29117,#29118,#29119,#29120,
#29121,#29122,#29123,#29124,#29125,#29126,#29127,#29128,#29129,#29130,#29131,
#29132,#29133,#29134,#29135,#29136,#29137,#29138,#29139,#29140,#29141,#29142,
#29143,#29144,#29145,#29146,#29147,#29148,#29149,#29150,#29151,#29152,#29153,
#29154,#29155,#29156,#29157,#29158,#29159,#29160,#29161,#29162,#29163,#29164,
#29165,#29166,#29167,#29168,#29169,#29170,#29171,#29172,#29173,#29174,#29175),
 .UNSPECIFIED.,.F.,.F.,(4,3,3,3,3,3,3,3,3,3,3,3,3,3,3,3,3,3,3,3,3,3,3,3,
3,3,3,3,3,3,3,3,3,3,3,3,3,3,3,3,3,3,3,3,3,3,3,3,3,4),(61.9155795617456,
62.0030943691385,62.0906369582788,62.1782762169576,62.2659725002026,62.3537950725185,
62.3796360283978,62.4674537280612,62.5551606326324,62.6427797421225,62.7337154499794,
62.8212359386107,62.9087434996574,62.9962587868648,63.0838024544475,63.1714430689489,
63.2591412464879,63.3469650426888,63.3702654049778,63.4580831375179,63.5457900747693,
63.6334092167075,63.7243449123138,63.8118654326169,63.8993730249961,63.986888343164,
64.0744320413037,64.1620726856125,64.2497708925579,64.3375947173568,64.3608947815578,
64.4487125810028,64.5364195857099,64.6240387955683,64.7149744658895,64.8024950548288,
64.8900027159882,64.9775181030047,65.0650618699846,65.1527025827746,65.2404008580718,
65.3282247505097,65.3515241581379,65.4399937122585,65.5283487397423,65.6166091643991,
65.7058183046457,65.793945781903,65.8836957536443,65.9734457253856),
 .UNSPECIFIED.);
#2066=B_SPLINE_CURVE_WITH_KNOTS('',3,(#29176,#29177,#29178,#29179,#29180,
#29181,#29182,#29183,#29184,#29185,#29186,#29187,#29188,#29189,#29190,#29191,
#29192,#29193,#29194,#29195,#29196,#29197,#29198,#29199,#29200,#29201,#29202,
#29203,#29204,#29205,#29206,#29207,#29208,#29209,#29210,#29211,#29212,#29213,
#29214,#29215,#29216,#29217,#29218,#29219,#29220,#29221,#29222,#29223,#29224,
#29225,#29226,#29227,#29228,#29229,#29230,#29231,#29232,#29233,#29234,#29235,
#29236,#29237,#29238,#29239,#29240,#29241,#29242,#29243,#29244,#29245,#29246,
#29247,#29248,#29249,#29250,#29251,#29252,#29253,#29254),.UNSPECIFIED.,
 .F.,.F.,(4,3,3,3,3,3,3,3,3,3,3,3,3,3,3,3,3,3,3,3,3,3,3,3,3,3,4),(65.9734457256018,
66.071966587094,66.170876506416,66.2703101698331,66.3421535347179,66.4299713959743,
66.5176784608089,66.6052977290641,66.6962333768433,66.7837540195464,66.8712617326777,
66.9587771698269,67.0463209850518,67.1339617430687,67.2216600618898,67.3094839950423,
67.3327829112979,67.4206086965015,67.508321893594,67.5959325367783,67.6834855424027,
67.7710016110476,67.8585014113932,67.9460421365112,68.0336015719711,68.1212568443822,
68.1983677761468),.UNSPECIFIED.);
#2067=B_SPLINE_CURVE_WITH_KNOTS('',3,(#29256,#29257,#29258,#29259,#29260,
#29261,#29262,#29263,#29264,#29265,#29266,#29267,#29268,#29269,#29270,#29271,
#29272,#29273,#29274,#29275,#29276,#29277,#29278,#29279,#29280,#29281,#29282,
#29283,#29284,#29285,#29286,#29287,#29288,#29289,#29290,#29291,#29292,#29293,
#29294,#29295,#29296,#29297,#29298,#29299,#29300,#29301,#29302,#29303,#29304,
#29305,#29306,#29307,#29308,#29309,#29310,#29311,#29312,#29313,#29314,#29315,
#29316,#29317,#29318,#29319,#29320,#29321,#29322,#29323,#29324,#29325,#29326,
#29327,#29328,#29329,#29330,#29331,#29332,#29333,#29334,#29335,#29336,#29337),
 .UNSPECIFIED.,.F.,.F.,(4,3,3,3,3,3,3,3,3,3,3,3,3,3,3,3,3,3,3,3,3,3,3,3,
3,3,3,4),(65.9734457255634,66.0604573157416,66.1473630223652,66.2341866831643,
66.3209558419399,66.4076973439539,66.4944326107321,66.5811830546428,66.6680217582215,
66.7549075930277,66.8419276084371,66.902482605459,66.9903004048339,67.0780074094708,
67.1656266192589,67.2565622896064,67.3440828784753,67.4315905395642,67.5191059265102,
67.6066496934205,67.6942904061413,67.7819886813696,67.8698125737395,67.893111982039,
67.9809172828592,68.0686253054638,68.1562387884845,68.1993438421936),
 .UNSPECIFIED.);
#2068=B_SPLINE_CURVE_WITH_KNOTS('',3,(#29338,#29339,#29340,#29341,#29342,
#29343,#29344,#29345,#29346,#29347,#29348,#29349,#29350,#29351,#29352,#29353,
#29354,#29355,#29356,#29357,#29358,#29359,#29360,#29361,#29362,#29363,#29364,
#29365,#29366,#29367,#29368,#29369,#29370,#29371,#29372,#29373,#29374,#29375,
#29376,#29377,#29378,#29379,#29380,#29381,#29382,#29383,#29384,#29385,#29386,
#29387,#29388,#29389,#29390,#29391,#29392,#29393,#29394,#29395,#29396,#29397,
#29398,#29399,#29400,#29401,#29402,#29403,#29404,#29405,#29406,#29407,#29408,
#29409,#29410,#29411,#29412,#29413,#29414,#29415,#29416,#29417,#29418,#29419,
#29420,#29421,#29422,#29423,#29424,#29425,#29426,#29427,#29428,#29429,#29430,
#29431,#29432,#29433,#29434,#29435,#29436,#29437,#29438,#29439,#29440,#29441,
#29442,#29443,#29444,#29445,#29446,#29447,#29448,#29449,#29450,#29451,#29452,
#29453,#29454,#29455,#29456,#29457,#29458,#29459,#29460,#29461,#29462,#29463,
#29464,#29465,#29466,#29467,#29468,#29469,#29470,#29471,#29472,#29473,#29474,
#29475,#29476,#29477,#29478,#29479,#29480,#29481,#29482,#29483,#29484,#29485,
#29486,#29487,#29488),.UNSPECIFIED.,.F.,.F.,(4,3,3,3,3,3,3,3,3,3,3,3,3,
3,3,3,3,3,3,3,3,3,3,3,3,3,3,3,3,3,3,3,3,3,3,3,3,3,3,3,3,3,3,3,3,3,3,3,3,
3,4),(61.9154900696683,61.9493357225588,62.0371534434491,62.1248603692403,
62.2124794999189,62.3034151998214,62.3909357094296,62.4784432913393,62.5659585992737,
62.6535022874257,62.7411429221594,62.8288411197586,62.9166649356151,62.9399650991389,
63.0277828228104,63.115489751354,63.2031088847533,63.294044583624,63.3815650958578,
63.4690726803538,63.5565879908324,63.644131681484,63.7317723186389,63.8194705186166,
63.9072943367714,63.9305944757189,64.0184122103381,64.1061191498958,64.1937382943618,
64.2846739891039,64.3721945124643,64.4597021080895,64.5472174296879,64.6347611314377,
64.722401779603,64.8100999905526,64.8979238195393,64.9212238522989,65.0090415519821,
65.0967484565731,65.184367566083,65.2753032739325,65.3628237625834,65.4503313236495,
65.5378466108761,65.6253902784785,65.7130308929987,65.8007290705565,65.8885528667756,
65.911853228879,65.9734457253856),.UNSPECIFIED.);
#2069=B_SPLINE_CURVE_WITH_KNOTS('',3,(#29494,#29495,#29496,#29497,#29498,
#29499,#29500,#29501,#29502,#29503,#29504,#29505,#29506,#29507,#29508,#29509,
#29510,#29511,#29512,#29513,#29514,#29515,#29516,#29517,#29518,#29519,#29520,
#29521,#29522,#29523,#29524,#29525,#29526,#29527,#29528,#29529,#29530,#29531,
#29532,#29533,#29534,#29535,#29536,#29537,#29538,#29539,#29540,#29541,#29542,
#29543,#29544,#29545,#29546,#29547,#29548,#29549,#29550,#29551,#29552,#29553,
#29554,#29555,#29556,#29557,#29558,#29559,#29560,#29561,#29562,#29563,#29564,
#29565,#29566,#29567,#29568,#29569,#29570,#29571,#29572,#29573,#29574,#29575,
#29576,#29577,#29578,#29579,#29580,#29581,#29582,#29583,#29584,#29585,#29586,
#29587,#29588,#29589,#29590,#29591,#29592,#29593,#29594,#29595,#29596,#29597,
#29598,#29599,#29600,#29601,#29602,#29603,#29604,#29605,#29606,#29607,#29608,
#29609,#29610,#29611,#29612,#29613,#29614,#29615,#29616,#29617,#29618,#29619,
#29620,#29621,#29622,#29623,#29624,#29625,#29626,#29627,#29628,#29629,#29630,
#29631,#29632,#29633,#29634,#29635,#29636,#29637,#29638,#29639,#29640,#29641),
 .UNSPECIFIED.,.F.,.F.,(4,3,3,3,3,3,3,3,3,3,3,3,3,3,3,3,3,3,3,3,3,3,3,3,
3,3,3,3,3,3,3,3,3,3,3,3,3,3,3,3,3,3,3,3,3,3,3,3,3,4),(55.6330557694626,
55.7206644177684,55.8100638366621,55.8975816477305,55.9850890690198,56.0726067535167,
56.1634200073669,56.2510686078768,56.3387777472702,56.4266088599168,56.4358597689176,
56.5236774922701,56.6113844205208,56.699003553653,56.7899392526336,56.8774597646661,
56.9649673489852,57.0524826593115,57.1400263498352,57.227666986899,57.315365186807,
57.4031890049234,57.4264891454977,57.5143068690178,57.6020137974319,57.6896329307235,
57.7805686296428,57.8680891418233,57.955596726286,58.0431120367513,58.1306557274094,
58.2182963646001,58.3059945646306,58.3938183828625,58.4171185220777,58.5049362472607,
58.5926431773456,58.6802623123135,58.7711980106065,58.8587185244669,58.9462261106077,
59.0337414227479,59.1212851150754,59.2089257539194,59.2966239555957,59.3844477754498,
59.4077478986577,59.5162980886054,59.6233575348318,59.6902604180773),
 .UNSPECIFIED.);
#2070=B_SPLINE_CURVE_WITH_KNOTS('',3,(#29642,#29643,#29644,#29645,#29646,
#29647,#29648,#29649,#29650,#29651,#29652,#29653,#29654,#29655,#29656,#29657,
#29658,#29659,#29660,#29661,#29662,#29663,#29664,#29665,#29666,#29667,#29668,
#29669,#29670,#29671,#29672,#29673,#29674,#29675,#29676,#29677,#29678,#29679,
#29680,#29681,#29682,#29683,#29684,#29685,#29686,#29687,#29688,#29689,#29690,
#29691,#29692,#29693,#29694,#29695,#29696,#29697,#29698,#29699,#29700,#29701,
#29702,#29703,#29704,#29705,#29706,#29707,#29708,#29709,#29710,#29711,#29712,
#29713,#29714,#29715,#29716,#29717,#29718,#29719,#29720),.UNSPECIFIED.,
 .F.,.F.,(4,3,3,3,3,3,3,3,3,3,3,3,3,3,3,3,3,3,3,3,3,3,3,3,3,3,4),(59.690260418206,
59.778775025335,59.8656202866809,59.9524524287172,60.0392927592702,60.1290638882621,
60.21603272593,60.3072050005838,60.3983772752377,60.4861949989082,60.5739019274507,
60.661521060849,60.7524567597201,60.8399772719529,60.9274848564478,61.0150001669254,
61.1025438575758,61.1901844947297,61.2778826947062,61.3657065128596,61.3890066518178,
61.4768208758585,61.5645289299151,61.6522915878727,61.7398434324448,61.8277114970952,
61.9155795617456),.UNSPECIFIED.);
#2071=B_SPLINE_CURVE_WITH_KNOTS('',3,(#29722,#29723,#29724,#29725,#29726,
#29727,#29728,#29729,#29730,#29731,#29732,#29733,#29734,#29735,#29736,#29737,
#29738,#29739,#29740,#29741,#29742,#29743,#29744,#29745,#29746,#29747,#29748,
#29749,#29750,#29751,#29752,#29753,#29754,#29755,#29756,#29757,#29758,#29759,
#29760,#29761,#29762,#29763,#29764,#29765,#29766,#29767,#29768,#29769,#29770,
#29771,#29772,#29773,#29774,#29775,#29776,#29777,#29778,#29779,#29780,#29781,
#29782,#29783,#29784,#29785,#29786,#29787,#29788,#29789,#29790,#29791,#29792,
#29793,#29794,#29795,#29796,#29797,#29798,#29799,#29800),.UNSPECIFIED.,
 .F.,.F.,(4,3,3,3,3,3,3,3,3,3,3,3,3,3,3,3,3,3,3,3,3,3,3,3,3,3,4),(59.6902604184428,
59.7976956859157,59.9067549038095,59.9680769693988,60.0558946929192,60.1436016213334,
60.2312207546254,60.3221564535446,60.4096769657254,60.4971845501883,60.5846998606539,
60.6722435513123,60.7598841885032,60.8475823885341,60.9354062067663,60.9587063459788,
61.0465260474664,61.1342344677518,61.2218546088791,61.3094092434363,61.3969287962241,
61.4844339359927,61.5719453160961,61.6595334475953,61.7471595778553,61.8349151106683,
61.9154900696683),.UNSPECIFIED.);
#2072=B_SPLINE_CURVE_WITH_KNOTS('',3,(#29801,#29802,#29803,#29804,#29805,
#29806,#29807,#29808,#29809,#29810,#29811,#29812,#29813,#29814,#29815,#29816,
#29817,#29818,#29819,#29820,#29821,#29822,#29823,#29824,#29825,#29826,#29827,
#29828,#29829,#29830,#29831,#29832,#29833,#29834,#29835,#29836,#29837,#29838,
#29839,#29840,#29841,#29842,#29843,#29844,#29845,#29846,#29847,#29848,#29849,
#29850,#29851,#29852,#29853,#29854,#29855,#29856,#29857,#29858,#29859,#29860,
#29861,#29862,#29863,#29864,#29865,#29866,#29867,#29868,#29869,#29870,#29871,
#29872,#29873,#29874,#29875,#29876,#29877,#29878,#29879,#29880,#29881,#29882,
#29883,#29884,#29885,#29886,#29887,#29888,#29889,#29890,#29891,#29892,#29893,
#29894,#29895,#29896,#29897,#29898,#29899,#29900,#29901,#29902,#29903,#29904,
#29905,#29906,#29907,#29908,#29909,#29910,#29911,#29912,#29913,#29914,#29915,
#29916,#29917,#29918,#29919,#29920,#29921,#29922,#29923,#29924,#29925,#29926,
#29927,#29928,#29929,#29930,#29931,#29932,#29933,#29934,#29935,#29936,#29937,
#29938,#29939,#29940,#29941,#29942,#29943,#29944,#29945,#29946,#29947,#29948,
#29949,#29950,#29951),.UNSPECIFIED.,.F.,.F.,(4,3,3,3,3,3,3,3,3,3,3,3,3,
3,3,3,3,3,3,3,3,3,3,3,3,3,3,3,3,3,3,3,3,3,3,3,3,3,3,3,3,3,3,3,3,3,3,3,3,
3,4),(55.6321436659148,55.7196876184786,55.8073285818317,55.8950272334287,
55.9828513473999,56.0055594630787,56.0933771867062,56.1810841152312,56.268703248637,
56.3596389475147,56.4471594598168,56.5346670444033,56.622182354995,56.7097260457814,
56.7973666831032,56.8850648832665,56.9728887016325,56.9961888396587,57.0840065632835,
57.1717134918052,57.259332625207,57.350268324086,57.4377888363829,57.525296420964,
57.6128117315495,57.7003554223297,57.7879960596445,57.8756942598004,57.9635180781585,
57.9868182162387,58.0746359401024,58.1623428688641,58.2499620025063,58.3408977012954,
58.4284182138326,58.5159257986535,58.6034411094777,58.6909848004959,58.7786254380462,
58.8663236384361,58.954147457025,58.9774475928188,59.0665491959922,59.1535112708394,
59.2403929917781,59.3272158146787,59.4179769655605,59.5047630074283,59.5915521894354,
59.6783867677613,59.690260418206),.UNSPECIFIED.);
#2073=B_SPLINE_CURVE_WITH_KNOTS('',3,(#29957,#29958,#29959,#29960,#29961,
#29962,#29963,#29964,#29965,#29966,#29967,#29968,#29969,#29970,#29971,#29972,
#29973,#29974,#29975,#29976,#29977,#29978,#29979,#29980,#29981,#29982,#29983,
#29984,#29985,#29986,#29987,#29988,#29989,#29990,#29991,#29992,#29993,#29994,
#29995,#29996,#29997,#29998,#29999,#30000,#30001,#30002,#30003,#30004,#30005,
#30006,#30007,#30008,#30009,#30010,#30011,#30012,#30013,#30014,#30015,#30016,
#30017,#30018,#30019,#30020,#30021,#30022,#30023,#30024,#30025,#30026,#30027,
#30028,#30029,#30030,#30031,#30032,#30033,#30034,#30035,#30036,#30037,#30038,
#30039,#30040,#30041,#30042,#30043,#30044,#30045,#30046,#30047,#30048,#30049,
#30050,#30051,#30052,#30053,#30054,#30055,#30056,#30057,#30058,#30059,#30060,
#30061,#30062,#30063,#30064,#30065,#30066,#30067,#30068,#30069,#30070,#30071,
#30072,#30073,#30074,#30075,#30076,#30077,#30078,#30079,#30080,#30081,#30082,
#30083,#30084,#30085,#30086,#30087,#30088,#30089,#30090,#30091,#30092,#30093,
#30094,#30095,#30096,#30097,#30098,#30099,#30100,#30101,#30102,#30103,#30104),
 .UNSPECIFIED.,.F.,.F.,(4,3,3,3,3,3,3,3,3,3,3,3,3,3,3,3,3,3,3,3,3,3,3,3,
3,3,3,3,3,3,3,3,3,3,3,3,3,3,3,3,3,3,3,3,3,3,3,3,3,4),(49.3487655263348,
49.4365711876644,49.5014541328574,49.5892718565205,49.676978785081,49.764597918522,
49.8555336173865,49.9430541297232,50.0305617143443,50.11807702497,50.2056207157903,
50.2932613531451,50.3809595533411,50.4687833717389,50.4920835094375,50.5799012330941,
50.6676081616481,50.7552272950827,50.8461629939495,50.9336835062799,51.0211910908946,
51.108706401514,51.1962500923282,51.2838907296769,51.3715889298668,51.4594127482588,
51.4827128860175,51.5705306096707,51.6582375382213,51.7458566716524,51.8367923705205,
51.9243128828472,52.0118204674583,52.0993357780739,52.1868794688843,52.2745201062292,
52.3622183064152,52.4500421248034,52.4733422625975,52.5604221705999,52.6473917779251,
52.7342748966387,52.8210968702446,52.9078870051228,52.9946666871667,53.0814572897348,
53.1683305097564,53.2552470966048,53.3422944293362,53.4070751108575),
 .UNSPECIFIED.);
#2074=B_SPLINE_CURVE_WITH_KNOTS('',3,(#30105,#30106,#30107,#30108,#30109,
#30110,#30111,#30112,#30113,#30114,#30115,#30116,#30117,#30118,#30119,#30120,
#30121,#30122,#30123,#30124,#30125,#30126,#30127,#30128,#30129,#30130,#30131,
#30132,#30133,#30134,#30135,#30136,#30137,#30138,#30139,#30140,#30141,#30142,
#30143,#30144,#30145,#30146,#30147,#30148,#30149,#30150,#30151,#30152,#30153,
#30154,#30155,#30156,#30157,#30158,#30159,#30160,#30161,#30162,#30163,#30164,
#30165,#30166,#30167,#30168,#30169,#30170,#30171,#30172,#30173,#30174,#30175,
#30176,#30177,#30178,#30179,#30180,#30181,#30182,#30183,#30184,#30185,#30186,
#30187,#30188,#30189),.UNSPECIFIED.,.F.,.F.,(4,3,3,3,3,3,3,3,3,3,3,3,3,
3,3,3,3,3,3,3,3,3,3,3,3,3,3,3,4),(53.4070751110265,53.4639716391775,53.551789362805,
53.63949629133,53.7271154247358,53.8180511236135,53.9055716359155,53.9930792205021,
54.0805945310936,54.1681382218801,54.2557788592019,54.3434770593653,54.4313008777312,
54.4546010157576,54.5424187393823,54.6301256679039,54.7177448013059,54.8086805001848,
54.8962010124817,54.9837085970627,55.0712239076482,55.1587675984283,55.2464082357429,
55.3341064358986,55.4219302542566,55.4452303923376,55.5330632323005,55.6207748440915,
55.6330557694626),.UNSPECIFIED.);
#2075=B_SPLINE_CURVE_WITH_KNOTS('',3,(#30191,#30192,#30193,#30194,#30195,
#30196,#30197,#30198,#30199,#30200,#30201,#30202,#30203,#30204,#30205,#30206,
#30207,#30208,#30209,#30210,#30211,#30212,#30213,#30214,#30215,#30216,#30217,
#30218,#30219,#30220,#30221,#30222,#30223,#30224,#30225,#30226,#30227,#30228,
#30229,#30230,#30231,#30232,#30233,#30234,#30235,#30236,#30237,#30238,#30239,
#30240,#30241,#30242,#30243,#30244,#30245,#30246,#30247,#30248,#30249,#30250,
#30251,#30252,#30253,#30254,#30255,#30256,#30257,#30258,#30259,#30260,#30261,
#30262,#30263,#30264,#30265,#30266,#30267,#30268,#30269),.UNSPECIFIED.,
 .F.,.F.,(4,3,3,3,3,3,3,3,3,3,3,3,3,3,3,3,3,3,3,3,3,3,3,3,3,3,4),(53.4070751110265,
53.4952697145479,53.5834738756999,53.6717071431074,53.7600512896627,53.8484511190497,
53.9370104139044,54.0243007099186,54.1121184335719,54.1998253621223,54.2874444955536,
54.3783801944217,54.4659007067484,54.5534082913594,54.6409236019752,54.7284672927857,
54.8161079301308,54.9038061303171,54.9916299487052,55.0149300864986,55.1027351460835,
55.1904358979974,55.2780531734501,55.3665757965662,55.4540917123707,55.5431176891427,
55.6321436659148),.UNSPECIFIED.);
#2076=B_SPLINE_CURVE_WITH_KNOTS('',3,(#30270,#30271,#30272,#30273,#30274,
#30275,#30276,#30277,#30278,#30279,#30280,#30281,#30282,#30283,#30284,#30285,
#30286,#30287,#30288,#30289,#30290,#30291,#30292,#30293,#30294,#30295,#30296,
#30297,#30298,#30299,#30300,#30301,#30302,#30303,#30304,#30305,#30306,#30307,
#30308,#30309,#30310,#30311,#30312,#30313,#30314,#30315,#30316,#30317,#30318,
#30319,#30320,#30321,#30322,#30323,#30324,#30325,#30326,#30327,#30328,#30329,
#30330,#30331,#30332,#30333,#30334,#30335,#30336,#30337,#30338,#30339,#30340,
#30341,#30342,#30343,#30344,#30345,#30346,#30347,#30348,#30349,#30350,#30351,
#30352,#30353,#30354,#30355,#30356,#30357,#30358,#30359,#30360,#30361,#30362,
#30363,#30364,#30365,#30366,#30367,#30368,#30369,#30370,#30371,#30372,#30373,
#30374,#30375,#30376,#30377,#30378,#30379,#30380,#30381,#30382,#30383,#30384,
#30385,#30386,#30387,#30388,#30389,#30390,#30391,#30392,#30393,#30394,#30395,
#30396,#30397,#30398,#30399,#30400,#30401,#30402,#30403,#30404,#30405,#30406,
#30407,#30408,#30409,#30410,#30411,#30412,#30413,#30414),.UNSPECIFIED.,
 .F.,.F.,(4,3,3,3,3,3,3,3,3,3,3,3,3,3,3,3,3,3,3,3,3,3,3,3,3,3,3,3,3,3,3,
3,3,3,3,3,3,3,3,3,3,3,3,3,3,3,3,3,4),(49.3498290191458,49.4388232922024,
49.5263404425959,49.6138478724993,49.7013662347429,49.7914704769568,49.8791203266202,
49.9704517651093,50.0617832035985,50.1496009272579,50.2373078558148,50.3249269892522,
50.4158626881179,50.5033832004509,50.5908907850685,50.6784060956906,50.7659497865075,
50.8535904238588,50.9412886240512,51.0291124424458,51.0524125801785,51.1402303038372,
51.2279372323932,51.3155563658296,51.4064920646957,51.494012577028,51.5815201616446,
51.6690354722663,51.7565791630819,51.8442198004324,51.9319180006241,52.0197418190178,
52.0430419567586,52.1308596804216,52.218566608982,52.3061857424226,52.3971214412871,
52.4846419536238,52.572149538245,52.6596648488705,52.7472085396912,52.834849177046,
52.9225473772421,53.0103711956399,53.0336713333386,53.132711821951,53.2314411213962,
53.3295918554785,53.4070751108119),.UNSPECIFIED.);
#2077=B_SPLINE_CURVE_WITH_KNOTS('',3,(#30420,#30421,#30422,#30423,#30424,
#30425,#30426,#30427,#30428,#30429,#30430,#30431,#30432,#30433,#30434,#30435,
#30436,#30437,#30438,#30439,#30440,#30441,#30442,#30443,#30444,#30445,#30446,
#30447,#30448,#30449,#30450,#30451,#30452,#30453,#30454,#30455,#30456,#30457,
#30458,#30459,#30460,#30461,#30462,#30463,#30464,#30465,#30466,#30467,#30468,
#30469,#30470,#30471,#30472,#30473,#30474,#30475,#30476,#30477,#30478,#30479,
#30480,#30481,#30482,#30483,#30484,#30485,#30486,#30487,#30488,#30489,#30490,
#30491,#30492,#30493,#30494,#30495,#30496,#30497,#30498,#30499,#30500,#30501,
#30502,#30503,#30504,#30505,#30506,#30507,#30508,#30509,#30510,#30511,#30512,
#30513,#30514,#30515,#30516,#30517,#30518,#30519,#30520,#30521,#30522,#30523,
#30524,#30525,#30526,#30527,#30528,#30529,#30530,#30531,#30532,#30533,#30534,
#30535,#30536,#30537,#30538,#30539,#30540,#30541,#30542,#30543,#30544,#30545,
#30546,#30547,#30548,#30549,#30550,#30551,#30552,#30553,#30554,#30555,#30556,
#30557,#30558,#30559,#30560,#30561,#30562,#30563,#30564,#30565,#30566,#30567),
 .UNSPECIFIED.,.F.,.F.,(4,3,3,3,3,3,3,3,3,3,3,3,3,3,3,3,3,3,3,3,3,3,3,3,
3,3,3,3,3,3,3,3,3,3,3,3,3,3,3,3,3,3,3,3,3,3,3,3,3,4),(43.066105953779,43.1536162830819,
43.2411478989153,43.3287730650111,43.4164494147267,43.5042595695875,43.5576778733773,
43.6454955970374,43.733202525595,43.8208216590329,43.9117573578984,43.9992778702323,
44.0867854548505,44.1743007654736,44.2618444562913,44.3494850936434,44.4371832938366,
44.5250071122318,44.5483072499573,44.6361249736168,44.7238319021737,44.8114510356111,
44.9023867344769,44.9899072468099,45.0774148314276,45.1649301420498,45.2524738328665,
45.3401144702178,45.42781267041,45.5156364888046,45.5389366265373,45.6267543501968,
45.7144612787537,45.802080412191,45.8930161110568,45.9805366233901,46.0680442080077,
46.1555595186299,46.2431032094466,46.3307438467981,46.418442046991,46.5062658653857,
46.5295660031174,46.6186563250424,46.7076259258596,46.796493725915,46.8852637004644,
46.9739759768119,47.0626512944817,47.1238898038469),.UNSPECIFIED.);
#2078=B_SPLINE_CURVE_WITH_KNOTS('',3,(#30568,#30569,#30570,#30571,#30572,
#30573,#30574,#30575,#30576,#30577,#30578,#30579,#30580,#30581,#30582,#30583,
#30584,#30585,#30586,#30587,#30588,#30589,#30590,#30591,#30592,#30593,#30594,
#30595,#30596,#30597,#30598,#30599,#30600,#30601,#30602,#30603,#30604,#30605,
#30606,#30607,#30608,#30609,#30610,#30611,#30612,#30613,#30614,#30615,#30616,
#30617,#30618,#30619,#30620,#30621,#30622,#30623,#30624,#30625,#30626,#30627,
#30628,#30629,#30630,#30631,#30632,#30633,#30634,#30635,#30636,#30637,#30638,
#30639,#30640,#30641,#30642,#30643,#30644,#30645,#30646),.UNSPECIFIED.,
 .F.,.F.,(4,3,3,3,3,3,3,3,3,3,3,3,3,3,3,3,3,3,3,3,3,3,3,3,3,3,4),(47.1238898040446,
47.2229661979578,47.3199017158542,47.4200485477758,47.5201953796974,47.6080131033568,
47.6957200319136,47.783339165351,47.8742748642168,47.96179537655,48.0493029611675,
48.1368182717895,48.2243619626063,48.3120025999577,48.3997008001501,48.4875246185446,
48.5108247562774,48.5986518168607,48.6863658889768,48.773976251605,48.8615284122451,
48.9490430728508,49.0365409029311,49.1240737177044,49.2116250178335,49.2992578827453,
49.3487655263348),.UNSPECIFIED.);
#2079=B_SPLINE_CURVE_WITH_KNOTS('',3,(#30648,#30649,#30650,#30651,#30652,
#30653,#30654,#30655,#30656,#30657,#30658,#30659,#30660,#30661,#30662,#30663,
#30664,#30665,#30666,#30667,#30668,#30669,#30670,#30671,#30672,#30673,#30674,
#30675,#30676,#30677,#30678,#30679,#30680,#30681,#30682,#30683,#30684,#30685,
#30686,#30687,#30688,#30689,#30690,#30691,#30692,#30693,#30694,#30695,#30696,
#30697,#30698,#30699,#30700,#30701,#30702,#30703,#30704,#30705,#30706,#30707,
#30708,#30709,#30710,#30711,#30712,#30713,#30714,#30715,#30716,#30717,#30718,
#30719,#30720,#30721,#30722,#30723,#30724,#30725,#30726,#30727,#30728,#30729),
 .UNSPECIFIED.,.F.,.F.,(4,3,3,3,3,3,3,3,3,3,3,3,3,3,3,3,3,3,3,3,3,3,3,3,
3,3,3,4),(47.1238898040745,47.2112205230592,47.2984421477868,47.3855782233556,
47.4726547355819,47.5596998923597,47.6467348498394,47.7337807519277,47.8209134726712,
47.9080890145165,47.9954065966275,48.0805244504385,48.1683421740981,48.2560491026549,
48.3436682360924,48.4346039349582,48.5221244472913,48.609632031909,48.6971473425312,
48.7846910333482,48.8723316706997,48.9600298708923,49.047853689287,49.0711538270185,
49.1589647608137,49.2466781839727,49.3342970267764,49.3498290191458),
 .UNSPECIFIED.);
#2080=B_SPLINE_CURVE_WITH_KNOTS('',3,(#30730,#30731,#30732,#30733,#30734,
#30735,#30736,#30737,#30738,#30739,#30740,#30741,#30742,#30743,#30744,#30745,
#30746,#30747,#30748,#30749,#30750,#30751,#30752,#30753,#30754,#30755,#30756,
#30757,#30758,#30759,#30760,#30761,#30762,#30763,#30764,#30765,#30766,#30767,
#30768,#30769,#30770,#30771,#30772,#30773,#30774,#30775,#30776,#30777,#30778,
#30779,#30780,#30781,#30782,#30783,#30784,#30785,#30786,#30787,#30788,#30789,
#30790,#30791,#30792,#30793,#30794,#30795,#30796,#30797,#30798,#30799,#30800,
#30801,#30802,#30803,#30804,#30805,#30806,#30807,#30808,#30809,#30810,#30811,
#30812,#30813,#30814,#30815,#30816,#30817,#30818,#30819,#30820,#30821,#30822,
#30823,#30824,#30825,#30826,#30827,#30828,#30829,#30830,#30831,#30832,#30833,
#30834,#30835,#30836,#30837,#30838,#30839,#30840,#30841,#30842,#30843,#30844,
#30845,#30846,#30847,#30848,#30849,#30850,#30851,#30852,#30853,#30854,#30855,
#30856,#30857,#30858,#30859,#30860,#30861,#30862,#30863,#30864,#30865,#30866,
#30867,#30868,#30869,#30870,#30871,#30872,#30873,#30874,#30875,#30876,#30877,
#30878,#30879,#30880),.UNSPECIFIED.,.F.,.F.,(4,3,3,3,3,3,3,3,3,3,3,3,3,
3,3,3,3,3,3,3,3,3,3,3,3,3,3,3,3,3,3,3,3,3,3,3,3,3,3,3,3,3,3,3,3,3,3,3,3,
3,4),(43.0658132987337,43.1273775675383,43.2151952912011,43.3029022197614,
43.3905213532023,43.4814570520668,43.5689775644035,43.6564851490246,43.7440004596503,
43.8315441504707,43.9191847878257,44.0068829880218,44.0947068064199,44.1180069441183,
44.205824667777,44.293531596333,44.3811507297697,44.4720864286357,44.559606940968,
44.6471145255847,44.734629836206,44.8221735270219,44.9098141643725,44.9975123645641,
45.0853361829578,45.1086363206984,45.1964540443579,45.2841609729148,45.3717801063522,
45.462715805218,45.5502363175511,45.6377439021686,45.7252592127907,45.8128029036075,
45.9004435409588,45.9881417411512,46.0759655595456,46.0992656972784,46.1870834209385,
46.274790349496,46.3624094829342,46.4533451817997,46.5408656941335,46.6283732787517,
46.7158885893745,46.803432280192,46.8910729175441,46.9787711177372,47.0665949361323,
47.0898950738584,47.1238898038469),.UNSPECIFIED.);
#2081=B_SPLINE_CURVE_WITH_KNOTS('',3,(#30886,#30887,#30888,#30889,#30890,
#30891,#30892,#30893,#30894,#30895,#30896,#30897,#30898,#30899,#30900,#30901,
#30902,#30903,#30904,#30905,#30906,#30907,#30908,#30909,#30910,#30911,#30912,
#30913,#30914,#30915,#30916,#30917,#30918,#30919,#30920,#30921,#30922,#30923,
#30924,#30925,#30926,#30927,#30928,#30929,#30930,#30931,#30932,#30933,#30934,
#30935,#30936,#30937,#30938,#30939,#30940,#30941,#30942,#30943,#30944,#30945,
#30946,#30947,#30948,#30949,#30950,#30951,#30952,#30953,#30954,#30955,#30956,
#30957,#30958,#30959,#30960,#30961,#30962,#30963,#30964,#30965,#30966,#30967,
#30968,#30969,#30970,#30971,#30972,#30973,#30974,#30975,#30976,#30977,#30978,
#30979,#30980,#30981,#30982,#30983,#30984,#30985,#30986,#30987,#30988,#30989,
#30990,#30991,#30992,#30993,#30994,#30995,#30996,#30997,#30998,#30999,#31000,
#31001,#31002,#31003,#31004,#31005,#31006,#31007,#31008,#31009,#31010,#31011,
#31012,#31013,#31014,#31015,#31016,#31017,#31018,#31019,#31020,#31021,#31022,
#31023,#31024,#31025,#31026,#31027,#31028,#31029,#31030,#31031,#31032,#31033),
 .UNSPECIFIED.,.F.,.F.,(4,3,3,3,3,3,3,3,3,3,3,3,3,3,3,3,3,3,3,3,3,3,3,3,
3,3,3,3,3,3,3,3,3,3,3,3,3,3,3,3,3,3,3,3,3,3,3,3,3,4),(36.7834780077634,
36.8711108279984,36.9586747705779,37.0462007156381,37.1337093249822,37.221221254129,
37.308757155933,37.3963879233731,37.4840722897725,37.5718873015088,37.6139016138971,
37.7017193375818,37.7894262661642,37.8770453996276,37.9679810984838,38.0555016108434,
38.1430091954876,38.2305245061365,38.3180681969803,38.4057088343586,38.4934070345781,
38.5812308529995,38.6045309904771,38.6923487141303,38.7800556426808,38.867674776112,
38.9586104749801,39.0461309873068,39.1336385719179,39.2211538825335,39.3086975733438,
39.3963382106888,39.484036410875,39.5718602292632,39.5951603670572,39.6829780907142,
39.7706850192686,39.8583041527034,39.9492398515702,40.0367603639006,40.1242679485154,
40.2117832591348,40.2993269499485,40.386967587297,40.4746657874866,40.5624896058781,
40.5857897436372,40.6987530453557,40.8096059142877,40.8407044965426),
 .UNSPECIFIED.);
#2082=B_SPLINE_CURVE_WITH_KNOTS('',3,(#31034,#31035,#31036,#31037,#31038,
#31039,#31040,#31041,#31042,#31043,#31044,#31045,#31046,#31047,#31048,#31049,
#31050,#31051,#31052,#31053,#31054,#31055,#31056,#31057,#31058,#31059,#31060,
#31061,#31062,#31063,#31064,#31065,#31066,#31067,#31068,#31069,#31070,#31071,
#31072,#31073,#31074,#31075,#31076,#31077,#31078,#31079,#31080,#31081,#31082,
#31083,#31084,#31085,#31086,#31087,#31088,#31089,#31090,#31091,#31092,#31093,
#31094,#31095,#31096,#31097,#31098,#31099,#31100,#31101,#31102,#31103,#31104,
#31105,#31106,#31107,#31108,#31109,#31110,#31111,#31112,#31113,#31114,#31115),
 .UNSPECIFIED.,.F.,.F.,(4,3,3,3,3,3,3,3,3,3,3,3,3,3,3,3,3,3,3,3,3,3,3,3,
3,3,3,4),(40.8407044966673,40.9273584362615,41.0139637234795,41.1005454082225,
41.1871250286696,41.2737241173095,41.3604139263767,41.4471549251354,41.5340255171284,
41.5764191202172,41.6642368438759,41.751943772432,41.8395629058689,41.9304986047349,
42.0180191170672,42.1055267016839,42.1930420123052,42.2805857031212,42.3682263404716,
42.4559245406634,42.543748359057,42.5670484967972,42.6548657905452,42.7425763486162,
42.8301869071651,42.9177390596797,43.0052579701394,43.066105953779),
 .UNSPECIFIED.);
#2083=B_SPLINE_CURVE_WITH_KNOTS('',3,(#31117,#31118,#31119,#31120,#31121,
#31122,#31123,#31124,#31125,#31126,#31127,#31128,#31129,#31130,#31131,#31132,
#31133,#31134,#31135,#31136,#31137,#31138,#31139,#31140,#31141,#31142,#31143,
#31144,#31145,#31146,#31147,#31148,#31149,#31150,#31151,#31152,#31153,#31154,
#31155,#31156,#31157,#31158,#31159,#31160,#31161,#31162,#31163,#31164,#31165,
#31166,#31167,#31168,#31169,#31170,#31171,#31172,#31173,#31174,#31175,#31176,
#31177,#31178,#31179,#31180,#31181,#31182,#31183,#31184,#31185,#31186,#31187,
#31188,#31189,#31190,#31191,#31192,#31193,#31194,#31195),.UNSPECIFIED.,
 .F.,.F.,(4,3,3,3,3,3,3,3,3,3,3,3,3,3,3,3,3,3,3,3,3,3,3,3,3,3,4),(40.8407044968387,
40.9448640923073,41.0502373865448,41.1461188143783,41.2339365380315,41.321643466582,
41.4092626000131,41.5001982988812,41.5877188112079,41.675226395819,41.7627417064346,
41.8502853972449,41.9379260345899,42.0256242347759,42.1134480531641,42.1367481909583,
42.224569549071,42.3122792278348,42.3999002310044,42.487454050736,42.5749722254964,
42.6624754241107,42.7499842994785,42.8375628990187,42.9251792682597,43.0129084859427,
43.0658132987337),.UNSPECIFIED.);
#2084=B_SPLINE_CURVE_WITH_KNOTS('',3,(#31196,#31197,#31198,#31199,#31200,
#31201,#31202,#31203,#31204,#31205,#31206,#31207,#31208,#31209,#31210,#31211,
#31212,#31213,#31214,#31215,#31216,#31217,#31218,#31219,#31220,#31221,#31222,
#31223,#31224,#31225,#31226,#31227,#31228,#31229,#31230,#31231,#31232,#31233,
#31234,#31235,#31236,#31237,#31238,#31239,#31240,#31241,#31242,#31243,#31244,
#31245,#31246,#31247,#31248,#31249,#31250,#31251,#31252,#31253,#31254,#31255,
#31256,#31257,#31258,#31259,#31260,#31261,#31262,#31263,#31264,#31265,#31266,
#31267,#31268,#31269,#31270,#31271,#31272,#31273,#31274,#31275,#31276,#31277,
#31278,#31279,#31280,#31281,#31282,#31283,#31284,#31285,#31286,#31287,#31288,
#31289,#31290,#31291,#31292,#31293,#31294,#31295,#31296,#31297,#31298,#31299,
#31300,#31301,#31302,#31303,#31304,#31305,#31306,#31307,#31308,#31309,#31310,
#31311,#31312,#31313,#31314,#31315,#31316,#31317,#31318,#31319,#31320,#31321,
#31322,#31323,#31324,#31325,#31326,#31327,#31328,#31329,#31330,#31331,#31332,
#31333,#31334,#31335,#31336,#31337,#31338,#31339,#31340,#31341,#31342,#31343),
 .UNSPECIFIED.,.F.,.F.,(4,3,3,3,3,3,3,3,3,3,3,3,3,3,3,3,3,3,3,3,3,3,3,3,
3,3,3,3,3,3,3,3,3,3,3,3,3,3,3,3,3,3,3,3,3,3,3,3,3,4),(36.7826585774627,
36.8701913327661,36.9578180023401,37.0454965173817,37.1333079644416,37.1836013080582,
37.2714190319113,37.3591259606641,37.4467450942998,37.5376807930921,37.6252013056277,
37.7127088904491,37.8002242012759,37.8877678922981,37.9754085298552,38.0631067302538,
38.1509305488533,38.1742306846382,38.2620484082614,38.3497553367818,38.4373744701828,
38.5283101690622,38.6158306813589,38.7033382659399,38.7908535765259,38.8783972673068,
38.9660379046225,39.0537361047798,39.1415599231395,39.1648600612182,39.2526777848493,
39.3403847133773,39.4280038467855,39.5189395456621,39.6064600579645,39.6939676425513,
39.7814829531424,39.8690266439274,39.9566672812469,40.0443654814074,40.1321892997699,
40.1554894377982,40.2428859234006,40.3301773559497,40.417384958565,40.5045298835637,
40.5916445939301,40.6787389693881,40.7658659690996,40.8407044966673),
 .UNSPECIFIED.);
#2085=B_SPLINE_CURVE_WITH_KNOTS('',3,(#31349,#31350,#31351,#31352,#31353,
#31354,#31355,#31356,#31357,#31358,#31359,#31360,#31361,#31362,#31363,#31364,
#31365,#31366,#31367,#31368,#31369,#31370,#31371,#31372,#31373,#31374,#31375,
#31376,#31377,#31378,#31379,#31380,#31381,#31382,#31383,#31384,#31385,#31386,
#31387,#31388,#31389,#31390,#31391,#31392,#31393,#31394,#31395,#31396,#31397,
#31398,#31399,#31400,#31401,#31402,#31403,#31404,#31405,#31406,#31407,#31408,
#31409,#31410,#31411,#31412,#31413,#31414,#31415,#31416,#31417,#31418,#31419,
#31420,#31421,#31422,#31423,#31424,#31425,#31426,#31427,#31428,#31429,#31430,
#31431,#31432,#31433,#31434,#31435,#31436,#31437,#31438,#31439,#31440,#31441,
#31442,#31443,#31444,#31445,#31446,#31447,#31448,#31449,#31450,#31451,#31452,
#31453,#31454,#31455,#31456,#31457,#31458,#31459,#31460,#31461,#31462,#31463,
#31464,#31465,#31466,#31467,#31468,#31469,#31470,#31471,#31472,#31473,#31474,
#31475,#31476,#31477,#31478,#31479,#31480,#31481,#31482,#31483,#31484,#31485,
#31486,#31487,#31488,#31489,#31490,#31491,#31492,#31493,#31494,#31495,#31496),
 .UNSPECIFIED.,.F.,.F.,(4,3,3,3,3,3,3,3,3,3,3,3,3,3,3,3,3,3,3,3,3,3,3,3,
3,3,3,3,3,3,3,3,3,3,3,3,3,3,3,3,3,3,3,3,3,3,3,3,3,4),(30.4991828016751,
30.589339389756,30.6794959778369,30.7673136989645,30.8550206249472,30.9426397557717,
31.0335754556023,31.1210959652419,31.2086035471408,31.2961188550221,31.3836625430786,
31.4713031776546,31.5590013750598,31.6468251906704,31.6701253544169,31.7579430795308,
31.8456500095597,31.9332691444848,32.0242048427988,32.1117253566494,32.1992329427927,
32.2867482549473,32.3742919473016,32.4619325861903,32.5496307879217,32.637454607846,
32.660754730997,32.7485724544946,32.8362793828906,32.9238985161683,33.0148342150944,
33.1023547272717,33.1898623117352,33.2773776222052,33.3649213128719,33.4525619500772,
33.5402601501255,33.6280839683802,33.651384107577,33.738220097186,33.8249459927482,
33.9115858331361,33.9981647376526,34.0847124756467,34.1712506293001,34.2578007688055,
34.3444298629893,34.4311037976332,34.517896294793,34.5575191892807),
 .UNSPECIFIED.);
#2086=B_SPLINE_CURVE_WITH_KNOTS('',3,(#31497,#31498,#31499,#31500,#31501,
#31502,#31503,#31504,#31505,#31506,#31507,#31508,#31509,#31510,#31511,#31512,
#31513,#31514,#31515,#31516,#31517,#31518,#31519,#31520,#31521,#31522,#31523,
#31524,#31525,#31526,#31527,#31528,#31529,#31530,#31531,#31532,#31533,#31534,
#31535,#31536,#31537,#31538,#31539,#31540,#31541,#31542,#31543,#31544,#31545,
#31546,#31547,#31548,#31549,#31550,#31551,#31552,#31553,#31554,#31555,#31556,
#31557,#31558,#31559,#31560,#31561,#31562,#31563,#31564,#31565,#31566,#31567,
#31568,#31569,#31570,#31571,#31572,#31573,#31574,#31575,#31576,#31577,#31578),
 .UNSPECIFIED.,.F.,.F.,(4,3,3,3,3,3,3,3,3,3,3,3,3,3,3,3,3,3,3,3,3,3,3,3,
3,3,3,4),(34.5575191894877,34.642013484157,34.7298312080103,34.8175381367635,
34.9051572703995,34.9960929691917,35.0836134817277,35.1711210665493,35.2586363773767,
35.3461800683992,35.4338207059567,35.5215189063556,35.6093427249555,35.6326428607371,
35.7204605843602,35.8081675128806,35.8957866462814,35.9867223451609,36.0742428574575,
36.1617504420386,36.2492657526244,36.336809443405,36.4244500807206,36.5121482808776,
36.5999720992373,36.6232722373171,36.7110751632177,36.7834780077634),
 .UNSPECIFIED.);
#2087=B_SPLINE_CURVE_WITH_KNOTS('',3,(#31580,#31581,#31582,#31583,#31584,
#31585,#31586,#31587,#31588,#31589,#31590,#31591,#31592,#31593,#31594,#31595,
#31596,#31597,#31598,#31599,#31600,#31601,#31602,#31603,#31604,#31605,#31606,
#31607,#31608,#31609,#31610,#31611,#31612,#31613,#31614,#31615,#31616,#31617,
#31618,#31619,#31620,#31621,#31622,#31623,#31624,#31625,#31626,#31627,#31628,
#31629,#31630,#31631,#31632,#31633,#31634,#31635,#31636,#31637,#31638,#31639,
#31640,#31641,#31642,#31643,#31644,#31645,#31646,#31647,#31648,#31649,#31650,
#31651,#31652,#31653,#31654,#31655,#31656,#31657,#31658,#31659,#31660,#31661),
 .UNSPECIFIED.,.F.,.F.,(4,3,3,3,3,3,3,3,3,3,3,3,3,3,3,3,3,3,3,3,3,3,3,3,
3,3,3,4),(34.5575191894877,34.6452189800033,34.7329127229612,34.820620735829,
34.9083633412095,34.9962128842465,35.0841247009442,35.1721722075712,35.2023425548981,
35.2901602783961,35.3778672067924,35.4654863400703,35.5564220389963,35.643942551174,
35.7314501356379,35.8189654461081,35.9065091367756,35.9941497739812,36.08184797403,
36.1696717922849,36.1929719314781,36.2807796092137,36.3684824138544,36.4561011792004,
36.543654683778,36.6311690802082,36.7186812678126,36.7826585774627),
 .UNSPECIFIED.);
#2088=B_SPLINE_CURVE_WITH_KNOTS('',3,(#31662,#31663,#31664,#31665,#31666,
#31667,#31668,#31669,#31670,#31671,#31672,#31673,#31674,#31675,#31676,#31677,
#31678,#31679,#31680,#31681,#31682,#31683,#31684,#31685,#31686,#31687,#31688,
#31689,#31690,#31691,#31692,#31693,#31694,#31695,#31696,#31697,#31698,#31699,
#31700,#31701,#31702,#31703,#31704,#31705,#31706,#31707,#31708,#31709,#31710,
#31711,#31712,#31713,#31714,#31715,#31716,#31717,#31718,#31719,#31720,#31721,
#31722,#31723,#31724,#31725,#31726,#31727,#31728,#31729,#31730,#31731,#31732,
#31733,#31734,#31735,#31736,#31737,#31738,#31739,#31740,#31741,#31742,#31743,
#31744,#31745,#31746,#31747,#31748,#31749,#31750,#31751,#31752,#31753,#31754,
#31755,#31756,#31757,#31758,#31759,#31760,#31761,#31762,#31763,#31764,#31765,
#31766,#31767,#31768,#31769,#31770,#31771,#31772,#31773,#31774,#31775,#31776,
#31777,#31778,#31779,#31780,#31781,#31782,#31783,#31784,#31785,#31786,#31787,
#31788,#31789,#31790,#31791,#31792,#31793,#31794,#31795,#31796,#31797,#31798,
#31799,#31800,#31801,#31802,#31803,#31804,#31805,#31806,#31807,#31808,#31809),
 .UNSPECIFIED.,.F.,.F.,(4,3,3,3,3,3,3,3,3,3,3,3,3,3,3,3,3,3,3,3,3,3,3,3,
3,3,3,3,3,3,3,3,3,3,3,3,3,3,3,3,3,3,3,3,3,3,3,3,3,4),(30.5003021062259,
30.5878638989066,30.6753888028352,30.7628971416267,30.8504095704628,30.9379467424075,
31.0255791506396,31.1132658507174,31.20108230312,31.239825048578,31.3276427827913,
31.4153497220206,31.5029688662351,31.5939045611004,31.6814250844032,31.7689326800424,
31.8564480017262,31.9439917036335,32.0316323520613,32.1193305633352,32.2071543927338,
32.230454425158,32.31827214858,32.4059790769219,32.4935982101664,32.5845339091129,
32.6720544213114,32.7595620058162,32.8470773163472,32.9346210070955,33.0222616444118,
33.1099598445888,33.1977836629968,33.221083801738,33.308901522868,33.3966084488531,
33.4842275796802,33.5751632795099,33.6626837891521,33.7501913710535,33.8377066789376,
33.9252503669967,34.0128910015754,34.100589198983,34.1884130145959,34.2117131783181,
34.3130674767471,34.4140179529364,34.514233490631,34.5575191892756),
 .UNSPECIFIED.);
#2089=B_SPLINE_CURVE_WITH_KNOTS('',3,(#31815,#31816,#31817,#31818,#31819,
#31820,#31821,#31822,#31823,#31824,#31825,#31826,#31827,#31828,#31829,#31830,
#31831,#31832,#31833,#31834,#31835,#31836,#31837,#31838,#31839,#31840,#31841,
#31842,#31843,#31844,#31845,#31846,#31847,#31848,#31849,#31850,#31851,#31852,
#31853,#31854,#31855,#31856,#31857,#31858,#31859,#31860,#31861,#31862,#31863,
#31864,#31865,#31866,#31867,#31868,#31869,#31870,#31871,#31872,#31873,#31874,
#31875,#31876,#31877,#31878,#31879,#31880,#31881,#31882,#31883,#31884,#31885,
#31886,#31887,#31888,#31889,#31890,#31891,#31892,#31893,#31894,#31895,#31896,
#31897,#31898,#31899,#31900,#31901,#31902,#31903,#31904,#31905,#31906,#31907,
#31908,#31909,#31910,#31911,#31912,#31913,#31914,#31915,#31916,#31917,#31918,
#31919,#31920,#31921,#31922,#31923,#31924,#31925,#31926,#31927,#31928,#31929,
#31930,#31931,#31932,#31933,#31934,#31935,#31936,#31937,#31938,#31939,#31940,
#31941,#31942,#31943,#31944,#31945,#31946,#31947,#31948,#31949,#31950,#31951,
#31952,#31953,#31954,#31955,#31956,#31957,#31958,#31959,#31960,#31961,#31962),
 .UNSPECIFIED.,.F.,.F.,(4,3,3,3,3,3,3,3,3,3,3,3,3,3,3,3,3,3,3,3,3,3,3,3,
3,3,3,3,3,3,3,3,3,3,3,3,3,3,3,3,3,3,3,3,3,3,3,3,3,4),(24.2166325011217,
24.3041405351431,24.3916633633866,24.4792764164281,24.5669348162689,24.6547349628873,
24.7357197183568,24.8235372555985,24.9112439949562,24.9988629366597,25.0897987064443,
25.1773190219343,25.2648264081598,25.3523415190524,25.4398850090128,25.527525444838,
25.615223442877,25.7030470597342,25.7263490949368,25.814166892366,25.9018738954422,
25.9894931040527,26.0804287749857,26.1679493636392,26.2554570248679,26.3429724123092,
26.4305161800693,26.5181568941627,26.6058551710695,26.6936790655524,26.7169784715168,
26.804796201569,26.8925031368074,26.9801222772054,27.0710579735669,27.1585784935172,
27.2460860859821,27.3336014046745,27.4211451037779,27.508785749695,27.5964839586264,
27.6843077859491,27.7076078480968,27.7974230785268,27.8871096033914,27.9766848889006,
28.0661443689486,28.1555356974574,28.2448677619689,28.2743338823081),
 .UNSPECIFIED.);
#2090=B_SPLINE_CURVE_WITH_KNOTS('',3,(#31963,#31964,#31965,#31966,#31967,
#31968,#31969,#31970,#31971,#31972,#31973,#31974,#31975,#31976,#31977,#31978,
#31979,#31980,#31981,#31982,#31983,#31984,#31985,#31986,#31987,#31988,#31989,
#31990,#31991,#31992,#31993,#31994,#31995,#31996,#31997,#31998,#31999,#32000,
#32001,#32002,#32003,#32004,#32005,#32006,#32007,#32008,#32009,#32010,#32011,
#32012,#32013,#32014,#32015,#32016,#32017,#32018,#32019,#32020,#32021,#32022,
#32023,#32024,#32025,#32026,#32027,#32028,#32029,#32030,#32031,#32032,#32033,
#32034,#32035,#32036,#32037,#32038,#32039,#32040,#32041,#32042,#32043,#32044),
 .UNSPECIFIED.,.F.,.F.,(4,3,3,3,3,3,3,3,3,3,3,3,3,3,3,3,3,3,3,3,3,3,3,3,
3,3,3,4),(28.2743338824685,28.3691609663371,28.4643913168018,28.5598306393145,
28.6555712304409,28.6982372246769,28.7860549589011,28.8737618981413,28.9613810423672,
29.0523167372284,29.1398372605426,29.2273448561933,29.3148601778887,29.4024038798072,
29.4900445282464,29.5777427395317,29.6655665689418,29.6888666012569,29.7766954664404,
29.8670063833447,29.9546150704636,30.0421656067926,30.1296786939772,30.2171750011152,
30.3047012558658,30.3922463191219,30.4798600883877,30.4991828016751),
 .UNSPECIFIED.);
#2091=B_SPLINE_CURVE_WITH_KNOTS('',3,(#32046,#32047,#32048,#32049,#32050,
#32051,#32052,#32053,#32054,#32055,#32056,#32057,#32058,#32059,#32060,#32061,
#32062,#32063,#32064,#32065,#32066,#32067,#32068,#32069,#32070,#32071,#32072,
#32073,#32074,#32075,#32076,#32077,#32078,#32079,#32080,#32081,#32082,#32083,
#32084,#32085,#32086,#32087,#32088,#32089,#32090,#32091,#32092,#32093,#32094,
#32095,#32096,#32097,#32098,#32099,#32100,#32101,#32102,#32103,#32104,#32105,
#32106,#32107,#32108,#32109,#32110,#32111,#32112,#32113,#32114,#32115,#32116,
#32117,#32118,#32119,#32120,#32121,#32122,#32123,#32124,#32125,#32126,#32127),
 .UNSPECIFIED.,.F.,.F.,(4,3,3,3,3,3,3,3,3,3,3,3,3,3,3,3,3,3,3,3,3,3,3,3,
3,3,3,4),(28.2743338824878,28.3620520321736,28.4496594841827,28.5371793599059,
28.6273527268449,28.7147750521331,28.8021848299805,28.8896028228172,28.9770497939646,
29.0645937581805,29.1521960284464,29.2399225699005,29.2585662954179,29.3463840254717,
29.4340909607114,29.5217101011108,29.6126457974717,29.7001663174231,29.7876739098888,
29.8751892285822,29.9627329276854,30.0503735736029,30.1380717825348,30.2258956098576,
30.249195671998,30.3370125832184,30.4247057976887,30.5003021062259),
 .UNSPECIFIED.);
#2092=B_SPLINE_CURVE_WITH_KNOTS('',3,(#32128,#32129,#32130,#32131,#32132,
#32133,#32134,#32135,#32136,#32137,#32138,#32139,#32140,#32141,#32142,#32143,
#32144,#32145,#32146,#32147,#32148,#32149,#32150,#32151,#32152,#32153,#32154,
#32155,#32156,#32157,#32158,#32159,#32160,#32161,#32162,#32163,#32164,#32165,
#32166,#32167,#32168,#32169,#32170,#32171,#32172,#32173,#32174,#32175,#32176,
#32177,#32178,#32179,#32180,#32181,#32182,#32183,#32184,#32185,#32186,#32187,
#32188,#32189,#32190,#32191,#32192,#32193,#32194,#32195,#32196,#32197,#32198,
#32199,#32200,#32201,#32202,#32203,#32204,#32205,#32206,#32207,#32208,#32209,
#32210,#32211,#32212,#32213,#32214,#32215,#32216,#32217,#32218,#32219,#32220,
#32221,#32222,#32223,#32224,#32225,#32226,#32227,#32228,#32229,#32230,#32231,
#32232,#32233,#32234,#32235,#32236,#32237,#32238,#32239,#32240,#32241,#32242,
#32243,#32244,#32245,#32246,#32247,#32248,#32249,#32250,#32251,#32252,#32253,
#32254,#32255,#32256,#32257,#32258,#32259,#32260,#32261,#32262,#32263,#32264,
#32265,#32266,#32267,#32268,#32269,#32270,#32271,#32272,#32273,#32274,#32275,
#32276,#32277,#32278),.UNSPECIFIED.,.F.,.F.,(4,3,3,3,3,3,3,3,3,3,3,3,3,
3,3,3,3,3,3,3,3,3,3,3,3,3,3,3,3,3,3,3,3,3,3,3,3,3,3,3,3,3,3,3,3,3,3,3,3,
3,4),(24.2161615786844,24.3054194125178,24.393235614427,24.4809409996466,
24.5685585701688,24.6594948475349,24.7470137580256,24.8345197291811,24.922033416444,
25.0095754757204,25.0972144775499,25.1849110379788,25.2727332228469,25.2960487890978,
25.3838670018774,25.4715744238134,25.5591940542576,25.6501295681851,25.7376505833635,
25.8251586721042,25.9126744875772,26.0002186834226,26.0878598235176,26.1755585257106,
26.2633828411844,26.2866781656779,26.3744960037511,26.4622030498209,26.5498223037114,
26.6407579585298,26.7282785979179,26.8157863118169,26.9033017538155,26.9908455779736,
27.0784863509278,27.1661846882012,27.2540086448129,27.2773075422579,27.3651250796296,
27.4528318191191,27.5404507609564,27.6313865306916,27.7189068463188,27.8064142326825,
27.8939293437142,27.9814728338144,28.0691132697803,28.1568112679608,28.2446348849586,
28.2679369188379,28.2743338823081),.UNSPECIFIED.);
#2093=B_SPLINE_CURVE_WITH_KNOTS('',3,(#32284,#32285,#32286,#32287,#32288,
#32289,#32290,#32291,#32292,#32293,#32294,#32295,#32296,#32297,#32298,#32299,
#32300,#32301,#32302,#32303,#32304,#32305,#32306,#32307,#32308,#32309,#32310,
#32311,#32312,#32313,#32314,#32315,#32316,#32317,#32318,#32319,#32320,#32321,
#32322,#32323,#32324,#32325,#32326,#32327,#32328,#32329,#32330,#32331,#32332,
#32333,#32334,#32335,#32336,#32337,#32338,#32339,#32340,#32341,#32342,#32343,
#32344,#32345,#32346,#32347,#32348,#32349,#32350,#32351,#32352,#32353,#32354,
#32355,#32356,#32357,#32358,#32359,#32360,#32361,#32362,#32363,#32364,#32365),
 .UNSPECIFIED.,.F.,.F.,(4,3,3,3,3,3,3,3,3,3,3,3,3,3,3,3,3,3,3,3,3,3,3,3,
3,3,3,4),(15.7079632679489,15.7946703424306,15.8813545315613,15.9680372193346,
16.0547397844141,16.1415388412398,16.228388975724,16.3153822983035,16.3803843998776,
16.4682786364247,16.5560616599551,16.6437563744183,16.7346635496732,16.8222578350669,
16.9098383863582,16.9974257698594,17.0850405516535,17.1727504498517,17.260516922345,
17.3484070344364,17.3710137764576,17.4589624375309,17.5468079926991,17.6345711086995,
17.7222690062869,17.8099291514913,17.897581481792,17.933138501431),
 .UNSPECIFIED.);
#2094=B_SPLINE_CURVE_WITH_KNOTS('',3,(#32367,#32368,#32369,#32370,#32371),
 .UNSPECIFIED.,.F.,.F.,(4,1,4),(14.3991256467175,15.3897550232976,15.7079550219993),
 .UNSPECIFIED.);
#2095=B_SPLINE_CURVE_WITH_KNOTS('',3,(#32375,#32376,#32377,#32378,#32379,
#32380,#32381,#32382,#32383,#32384,#32385,#32386,#32387,#32388,#32389,#32390,
#32391,#32392,#32393,#32394,#32395,#32396,#32397,#32398,#32399,#32400,#32401,
#32402,#32403,#32404,#32405,#32406,#32407,#32408,#32409,#32410,#32411,#32412,
#32413,#32414,#32415,#32416,#32417,#32418,#32419,#32420,#32421,#32422,#32423,
#32424,#32425,#32426,#32427,#32428,#32429,#32430,#32431,#32432,#32433,#32434,
#32435,#32436,#32437,#32438),.UNSPECIFIED.,.F.,.F.,(4,3,3,3,3,3,3,3,3,3,
3,3,3,3,3,3,3,3,3,3,3,4),(13.8752087529905,13.9625599527458,14.049801399386,
14.1369566191565,14.2240510610285,14.3111134548194,14.3981649381222,14.4852266357263,
14.5723733096138,14.6595621693105,14.7468902564328,14.8294259525565,14.9162044260086,
15.0028750623154,15.091011087993,15.1775387385182,15.2640376415103,15.3505294215583,
15.4398878831029,15.5264717366794,15.617217502208,15.7079632677367),
 .UNSPECIFIED.);
#2096=B_SPLINE_CURVE_WITH_KNOTS('',3,(#32439,#32440,#32441,#32442,#32443,
#32444,#32445,#32446,#32447,#32448,#32449,#32450,#32451,#32452,#32453,#32454,
#32455,#32456,#32457,#32458,#32459,#32460,#32461,#32462,#32463,#32464,#32465,
#32466,#32467,#32468,#32469,#32470,#32471,#32472,#32473,#32474,#32475,#32476,
#32477,#32478,#32479,#32480,#32481,#32482,#32483,#32484,#32485,#32486,#32487,
#32488,#32489,#32490,#32491,#32492,#32493,#32494,#32495,#32496,#32497,#32498,
#32499,#32500,#32501,#32502,#32503,#32504,#32505,#32506,#32507,#32508,#32509,
#32510,#32511,#32512,#32513,#32514,#32515,#32516,#32517,#32518,#32519,#32520),
 .UNSPECIFIED.,.F.,.F.,(4,3,3,3,3,3,3,3,3,3,3,3,3,3,3,3,3,3,3,3,3,3,3,3,
3,3,3,4),(15.7079632679489,15.8200553291365,15.9077801590785,15.9953930214419,
16.0829170361697,16.173887994863,16.2613113585393,16.3487212103233,16.4361383070159,
16.5235834056171,16.6111253805921,16.6987247599939,16.7864502769504,16.8106847057165,
16.8985189148338,16.9862423685142,17.0738780459568,17.1648075504993,17.2523445445389,
17.3398685584644,17.4274002275394,17.5149601874335,17.602616878146,17.6903310246347,
17.7781705099498,17.8013140822966,17.8891423087798,17.9338728552279),
 .UNSPECIFIED.);
#2097=B_SPLINE_CURVE_WITH_KNOTS('',3,(#32526,#32527,#32528,#32529,#32530,
#32531,#32532,#32533,#32534,#32535,#32536,#32537,#32538,#32539,#32540,#32541,
#32542,#32543,#32544,#32545,#32546,#32547,#32548,#32549,#32550,#32551,#32552,
#32553,#32554,#32555,#32556,#32557,#32558,#32559,#32560,#32561,#32562,#32563,
#32564,#32565,#32566,#32567,#32568,#32569,#32570,#32571,#32572,#32573,#32574,
#32575,#32576,#32577,#32578,#32579,#32580,#32581,#32582,#32583,#32584,#32585,
#32586,#32587,#32588,#32589,#32590,#32591,#32592,#32593,#32594,#32595,#32596,
#32597,#32598,#32599,#32600,#32601,#32602,#32603,#32604,#32605,#32606,#32607,
#32608,#32609,#32610,#32611,#32612,#32613,#32614,#32615,#32616,#32617,#32618,
#32619,#32620,#32621,#32622),.UNSPECIFIED.,.F.,.F.,(4,3,3,3,3,3,3,3,3,3,
3,3,3,3,3,3,3,3,3,3,3,3,3,3,3,3,3,3,3,3,3,3,4),(64.4958654271813,64.5878114726323,
64.6796682202886,64.7714666576999,64.8632356888753,64.9549989780416,65.0467801784818,
65.1386594553566,65.2305917565556,65.3226705696143,65.3815388542818,65.4726940042981,
65.5637278110629,65.6546677268432,65.7455466697704,65.8363944318674,65.9272356637036,
66.0180950050278,66.1090616969139,66.200083004819,66.2912717783792,66.3721682308618,
66.4666155697857,66.5609252154487,66.6551188983848,66.7492022645659,66.8432212250325,
66.9371952485092,67.0311437590025,67.1251117412093,67.2190879270455,67.3131274215545,
67.3627976074418),.UNSPECIFIED.);
#2098=B_SPLINE_CURVE_WITH_KNOTS('',3,(#32630,#32631,#32632,#32633,#32634,
#32635,#32636,#32637,#32638,#32639,#32640,#32641,#32642,#32643,#32644,#32645,
#32646,#32647,#32648,#32649,#32650,#32651,#32652,#32653,#32654,#32655,#32656,
#32657,#32658,#32659,#32660,#32661,#32662,#32663,#32664,#32665,#32666,#32667,
#32668,#32669,#32670,#32671,#32672,#32673,#32674,#32675,#32676,#32677,#32678,
#32679,#32680,#32681,#32682,#32683,#32684,#32685,#32686,#32687,#32688,#32689,
#32690,#32691,#32692,#32693,#32694,#32695,#32696,#32697,#32698,#32699,#32700,
#32701,#32702,#32703,#32704,#32705,#32706,#32707,#32708,#32709,#32710,#32711,
#32712,#32713,#32714,#32715,#32716,#32717,#32718,#32719,#32720,#32721,#32722,
#32723,#32724,#32725,#32726,#32727,#32728,#32729,#32730,#32731,#32732,#32733,
#32734,#32735,#32736,#32737,#32738,#32739,#32740,#32741,#32742,#32743,#32744,
#32745,#32746,#32747,#32748,#32749,#32750,#32751,#32752,#32753,#32754,#32755,
#32756,#32757,#32758,#32759,#32760,#32761,#32762,#32763,#32764,#32765,#32766,
#32767),.UNSPECIFIED.,.F.,.F.,(4,2,2,2,2,2,2,2,2,2,2,2,2,2,2,2,2,2,2,2,
2,2,2,2,2,2,2,2,2,2,2,2,2,2,2,2,2,2,2,2,2,2,2,2,2,2,2,2,2,2,2,2,2,2,2,2,
2,2,2,2,2,2,2,2,2,2,2,2,4),(-3.81646514822443,-3.80352815874458,-3.74055056205899,
-3.6908910055397,-3.67160982941172,-3.66182442746867,-3.65456573177332,
-3.64537017487538,-3.62953057477486,-3.57391740471288,-3.52733622427903,
-3.50426956775655,-3.49698761023047,-3.49221053925842,-3.48787708604674,
-3.48025265988004,-3.45518881362056,-3.39537599510592,-3.36309191692142,
-3.34055429809831,-3.33024160712699,-3.32222124734079,-3.31323481495827,
-3.29778023865283,-3.22209772637379,-3.18651335334593,-3.16664977008392,
-3.15980085945556,-3.15517806771929,-3.15023395777695,-3.1417623667696,
-3.09904416338619,-3.03933890749073,-3.00684096618422,-2.99520428269995,
-2.98705224957573,-2.97968775404413,-2.9678900560391,-2.93669357636674,
-2.86010100596757,-2.84058945054392,-2.82727147287481,-2.82139621045025,
-2.81696558366223,-2.81154234728002,-2.80082238375559,-2.74751669952281,
-2.69817545346558,-2.66873737097169,-2.65742225990942,-2.64927841175236,
-2.64075547667854,-2.62746323568623,-2.57899698750133,-2.52042991410282,
-2.49457147695174,-2.48710482355436,-2.48235212473586,-2.47755031232083,
-2.46982254882778,-2.44342430688665,-2.37789105680805,-2.33561274883014,
-2.32299363831771,-2.31461541659801,-2.30649326662958,-2.29664195739933,
-2.27196551483348,-2.25634167253437),.UNSPECIFIED.);
#2099=B_SPLINE_CURVE_WITH_KNOTS('',3,(#32773,#32774,#32775,#32776,#32777,
#32778,#32779,#32780,#32781,#32782,#32783,#32784,#32785,#32786,#32787,#32788,
#32789,#32790,#32791,#32792,#32793,#32794,#32795,#32796,#32797,#32798,#32799,
#32800,#32801,#32802,#32803,#32804,#32805,#32806,#32807,#32808,#32809,#32810,
#32811,#32812,#32813,#32814,#32815,#32816,#32817,#32818,#32819,#32820,#32821,
#32822,#32823,#32824,#32825,#32826,#32827,#32828,#32829,#32830,#32831,#32832,
#32833,#32834,#32835,#32836,#32837,#32838,#32839,#32840,#32841,#32842,#32843,
#32844,#32845,#32846,#32847,#32848,#32849,#32850,#32851,#32852,#32853,#32854,
#32855,#32856,#32857,#32858,#32859,#32860,#32861,#32862,#32863,#32864,#32865,
#32866,#32867,#32868,#32869,#32870,#32871,#32872,#32873,#32874,#32875,#32876,
#32877,#32878,#32879,#32880,#32881,#32882,#32883,#32884,#32885,#32886,#32887,
#32888,#32889,#32890,#32891,#32892,#32893,#32894,#32895,#32896,#32897,#32898,
#32899,#32900,#32901,#32902,#32903,#32904,#32905,#32906,#32907,#32908,#32909,
#32910,#32911,#32912,#32913,#32914,#32915,#32916,#32917,#32918,#32919,#32920,
#32921,#32922,#32923,#32924,#32925,#32926,#32927,#32928,#32929,#32930,#32931,
#32932,#32933,#32934,#32935,#32936,#32937,#32938,#32939,#32940,#32941,#32942,
#32943,#32944,#32945,#32946,#32947,#32948,#32949,#32950,#32951,#32952),
 .UNSPECIFIED.,.F.,.F.,(4,2,2,2,2,2,2,2,2,2,2,2,2,2,2,2,2,2,2,2,2,2,2,2,
2,2,2,2,2,2,2,2,2,2,2,2,2,2,2,2,2,2,2,2,2,2,2,2,2,2,2,2,2,2,2,2,2,2,2,2,
2,2,2,2,2,2,2,2,2,2,2,2,2,2,2,2,2,2,2,2,2,2,2,2,2,2,2,2,2,4),(-2.0152369081143,
-1.97116093935254,-1.94753091842145,-1.94007625758421,-1.93580516021273,
-1.93112989406986,-1.92399263265513,-1.90146055648256,-1.85703316133956,
-1.79531564131364,-1.77939599561947,-1.77025411929421,-1.76230369882244,
-1.75236221422394,-1.73180134000087,-1.70350427661139,-1.63795986816285,
-1.61155643991754,-1.60384784489885,-1.59905375859423,-1.59432123444,-1.58688781614374,
-1.56121123397106,-1.50359636533397,-1.45351941985236,-1.4401843381907,
-1.43166916120953,-1.42355885213667,-1.41233493704493,-1.38344051228533,
-1.33561744850789,-1.2800359484559,-1.2695959769893,-1.26416635707667,-1.25967788516117,
-1.25374660794778,-1.2402335856419,-1.22034290657674,-1.13923059349499,
-1.11220447488099,-1.10097379473918,-1.09285550331387,-1.08432887637475,
-1.07096819851719,-1.01584699984061,-0.959944641081289,-0.937610543838119,
-0.930280989868928,-0.926030573676456,-0.92131532273394,-0.914023034669241,
-0.890052052828789,-0.840042899972904,-0.786122648137173,-0.770164885024668,
-0.761006059984599,-0.753042549073807,-0.74308594691075,-0.722494924734582,
-0.694157093842313,-0.628436109119681,-0.602158900285102,-0.594468386963779,
-0.589677894380495,-0.584971859334526,-0.577579010137999,-0.55206638376495,
-0.495245912786879,-0.443731306813558,-0.430386365139749,-0.421899033029062,
-0.413841244311261,-0.402735400359603,-0.374467917606038,-0.32834286763478,
-0.270175548509306,-0.259654219484075,-0.254286783417145,-0.249794225459742,
-0.243797336648389,-0.229943113817842,-0.209358714925704,-0.130315938037314,
-0.102350790602122,-0.0909273173276217,-0.082827828262194,-0.0743211133442966,
-0.0656697704768997,-0.0531761502260062,-0.00100806979219698),
 .UNSPECIFIED.);
#2100=B_SPLINE_CURVE_WITH_KNOTS('',3,(#32953,#32954,#32955,#32956,#32957,
#32958,#32959,#32960,#32961,#32962,#32963,#32964,#32965,#32966,#32967,#32968),
 .UNSPECIFIED.,.F.,.F.,(4,3,3,3,3,4),(64.1406906932474,64.2573851651463,
64.3763858948088,64.3909094777018,64.482998908666,64.4958654271813),
 .UNSPECIFIED.);
#2101=B_SPLINE_CURVE_WITH_KNOTS('',3,(#32969,#32970,#32971,#32972,#32973,
#32974,#32975,#32976,#32977,#32978,#32979,#32980,#32981,#32982,#32983,#32984,
#32985,#32986,#32987,#32988,#32989,#32990,#32991,#32992,#32993,#32994,#32995,
#32996,#32997,#32998,#32999,#33000,#33001,#33002,#33003,#33004,#33005,#33006,
#33007,#33008,#33009,#33010,#33011,#33012,#33013,#33014,#33015,#33016,#33017,
#33018,#33019,#33020,#33021,#33022,#33023,#33024,#33025,#33026,#33027,#33028,
#33029,#33030,#33031,#33032,#33033,#33034,#33035,#33036,#33037,#33038,#33039,
#33040,#33041,#33042,#33043,#33044,#33045,#33046,#33047,#33048,#33049,#33050,
#33051,#33052,#33053,#33054,#33055,#33056,#33057,#33058,#33059,#33060,#33061,
#33062,#33063,#33064,#33065,#33066,#33067,#33068,#33069,#33070,#33071,#33072,
#33073,#33074,#33075,#33076,#33077,#33078,#33079,#33080,#33081,#33082,#33083,
#33084,#33085,#33086,#33087,#33088,#33089,#33090,#33091,#33092,#33093,#33094,
#33095,#33096,#33097,#33098,#33099,#33100,#33101,#33102,#33103,#33104,#33105,
#33106,#33107,#33108,#33109,#33110,#33111,#33112,#33113,#33114,#33115,#33116,
#33117,#33118,#33119,#33120,#33121,#33122,#33123,#33124,#33125,#33126,#33127,
#33128,#33129,#33130,#33131,#33132,#33133,#33134,#33135,#33136,#33137,#33138,
#33139,#33140,#33141,#33142,#33143,#33144,#33145,#33146,#33147,#33148,#33149,
#33150,#33151,#33152,#33153,#33154,#33155,#33156,#33157,#33158,#33159,#33160),
 .UNSPECIFIED.,.F.,.F.,(4,2,2,2,2,2,2,2,2,2,2,2,2,2,2,2,2,2,2,2,2,2,2,2,
2,2,2,2,2,2,2,2,2,2,2,2,2,2,2,2,2,2,2,2,2,2,2,2,2,2,2,2,2,2,2,2,2,2,2,2,
2,2,2,2,2,2,2,2,2,2,2,2,2,2,2,2,2,2,2,2,2,2,2,2,2,2,2,2,2,2,2,2,2,2,2,4),
(-2.25634167253437,-2.1881420344393,-2.168049575673,-2.15443780714628,-2.14848912535191,
-2.14399843087398,-2.13857965438789,-2.1278681277045,-2.07562952988243,
-2.02559161652123,-1.99594302048512,-1.98461882665343,-1.97649022553089,
-1.96800342456545,-1.95481309853747,-1.90846483912855,-1.89825580196821,
-1.8406412797465,-1.82044982449514,-1.81337296613433,-1.8091737887011,-1.80441908458761,
-1.79689650610624,-1.77023834151946,-1.70756403287971,-1.66318085017836,
-1.65010005426361,-1.64162975442101,-1.63347794624088,-1.62205532028647,
-1.59167987103848,-1.51168740437092,-1.4851849960617,-1.47745602659865,
-1.47265573711118,-1.46792043575924,-1.46049050806918,-1.43491065187996,
-1.37778351626714,-1.32717028643306,-1.31381420923002,-1.30528918918205,
-1.29717168323605,-1.28594095701279,-1.25704474645925,-1.2092365884578,
-1.15360020172603,-1.14315697578276,-1.13772406855693,-1.13323346151996,
-1.12729891705099,-1.11376971895252,-1.09384515720563,-1.01225908311068,
-0.985657119725443,-0.97450007176338,-0.966395847790362,-0.957849093610993,
-0.944382161237028,-0.886282830960741,-0.825168733458591,-0.809251393647724,
-0.802779764037206,-0.798225573719969,-0.793110374492047,-0.78390122175292,
-0.77207225341405,-0.743743823259087,-0.658682421702079,-0.642964108802933,
-0.633866118567348,-0.62598815048635,-0.616026594938854,-0.595347393056453,
-0.5668176888279,-0.526448952506956,-0.476958390382105,-0.468383587220673,
-0.463403023196974,-0.458793320209024,-0.451992976380947,-0.432442005601048,
-0.397712976123245,-0.320904985965978,-0.305683162035318,-0.296774785984468,
-0.288791398065986,-0.278482337522529,-0.255776856562214,-0.223129826757771,
-0.16177743509034,-0.138221073863547,-0.130773566383219,-0.126504039896551,
-0.121829508555764,-0.121375378727905),.UNSPECIFIED.);
#2102=B_SPLINE_CURVE_WITH_KNOTS('',3,(#33165,#33166,#33167,#33168,#33169,
#33170,#33171,#33172,#33173,#33174,#33175,#33176,#33177,#33178,#33179,#33180,
#33181,#33182,#33183,#33184,#33185,#33186,#33187,#33188,#33189,#33190,#33191,
#33192,#33193,#33194,#33195,#33196,#33197,#33198,#33199,#33200,#33201,#33202,
#33203,#33204,#33205,#33206,#33207,#33208,#33209,#33210,#33211,#33212,#33213,
#33214,#33215,#33216,#33217,#33218,#33219,#33220,#33221,#33222,#33223,#33224,
#33225,#33226,#33227,#33228,#33229,#33230,#33231,#33232,#33233,#33234,#33235,
#33236,#33237,#33238,#33239,#33240,#33241,#33242,#33243,#33244,#33245,#33246,
#33247,#33248,#33249,#33250,#33251,#33252,#33253,#33254,#33255,#33256,#33257,
#33258,#33259,#33260,#33261,#33262,#33263,#33264,#33265,#33266,#33267,#33268,
#33269,#33270,#33271,#33272,#33273,#33274,#33275,#33276,#33277,#33278,#33279,
#33280,#33281,#33282,#33283,#33284,#33285,#33286,#33287,#33288,#33289,#33290,
#33291,#33292,#33293,#33294,#33295,#33296,#33297,#33298,#33299,#33300,#33301,
#33302,#33303,#33304,#33305,#33306,#33307,#33308,#33309,#33310,#33311,#33312,
#33313,#33314,#33315,#33316,#33317,#33318,#33319,#33320,#33321,#33322,#33323,
#33324,#33325,#33326,#33327,#33328,#33329,#33330,#33331,#33332,#33333,#33334,
#33335,#33336,#33337,#33338,#33339,#33340,#33341,#33342,#33343,#33344,#33345,
#33346,#33347,#33348,#33349,#33350,#33351,#33352),.UNSPECIFIED.,.F.,.F.,
(4,2,2,2,2,2,2,2,2,2,2,2,2,2,2,2,2,2,2,2,2,2,2,2,2,2,2,2,2,2,2,2,2,2,2,
2,2,2,2,2,2,2,2,2,2,2,2,2,2,2,2,2,2,2,2,2,2,2,2,2,2,2,2,2,2,2,2,2,2,2,2,
2,2,2,2,2,2,2,2,2,2,2,2,2,2,2,2,2,2,2,2,2,2,4),(-4.14975517296478,-4.13455580645905,
-4.12556746444321,-4.11760059569648,-4.10743503864127,-4.08557563722847,
-3.99748878645955,-3.97711222049083,-3.96336669675091,-3.95739663488861,
-3.95290411702709,-3.94749941603641,-3.93686532659078,-3.88059503089609,
-3.83328555535685,-3.80456852375864,-3.79336379782498,-3.7852526376491,
-3.77672322487416,-3.76333652335401,-3.71114023639411,-3.6554136412058,
-3.63013529370559,-3.62273467647168,-3.61800690547128,-3.61378676931684,
-3.6066006522728,-3.58551993804436,-3.52860828680488,-3.47287461898424,
-3.45949144678285,-3.45096297484923,-3.44285184213696,-3.43164571717561,
-3.4047296050034,-3.3256044775181,-3.30454586333963,-3.29047843660382,-3.28445526310384,
-3.27995829565801,-3.27459140202592,-3.26445852073142,-3.18899221391022,
-3.15366979070076,-3.12973423087392,-3.11922683391053,-3.11122072388365,
-3.10241733510474,-3.08769953292715,-3.00713677151403,-2.9592361420963,
-2.95069446403207,-2.94572163867358,-2.94116251510814,-2.93547991723627,
-2.92097098527908,-2.85870140447019,-2.79996955020488,-2.7864838334342,
-2.77793401815398,-2.76983299011081,-2.75869010586304,-2.73218762975779,
-2.65056516586576,-2.63064755019404,-2.61712164255023,-2.61118836144776,
-2.60669880272143,-2.60126746436783,-2.59049618255,-2.54583656858252,-2.50760199607605,
-2.47720377496632,-2.45558779147849,-2.4454639032615,-2.43750120172481,
-2.42848761357944,-2.41315551316623,-2.33897810795571,-2.28628831249504,
-2.27767187816894,-2.27268312163263,-2.26813184656009,-2.26140143449232,
-2.24380539206789,-2.18408900143524,-2.1358713255419,-2.11914928345012,
-2.10897547445082,-2.10100681350048,-2.09202135067769,-2.0764219268981,
-2.02612709481119,-2.0152369081143),.UNSPECIFIED.);
#2103=B_SPLINE_CURVE_WITH_KNOTS('',3,(#33354,#33355,#33356,#33357,#33358,
#33359,#33360,#33361),.UNSPECIFIED.,.F.,.F.,(4,2,2,4),(-0.121375378727905,
-0.114690093556633,-0.0921226174557673,-0.000975323762489068),
 .UNSPECIFIED.);
#2104=B_SPLINE_CURVE_WITH_KNOTS('',3,(#33362,#33363,#33364,#33365,#33366,
#33367,#33368,#33369,#33370,#33371,#33372,#33373,#33374,#33375,#33376,#33377,
#33378,#33379,#33380,#33381,#33382,#33383,#33384,#33385,#33386,#33387,#33388,
#33389,#33390,#33391,#33392,#33393,#33394,#33395,#33396,#33397,#33398,#33399,
#33400,#33401,#33402,#33403,#33404,#33405,#33406,#33407,#33408,#33409,#33410,
#33411,#33412,#33413,#33414,#33415,#33416,#33417,#33418,#33419,#33420,#33421,
#33422,#33423,#33424,#33425,#33426,#33427,#33428,#33429,#33430,#33431,#33432,
#33433,#33434,#33435,#33436,#33437,#33438,#33439,#33440,#33441,#33442,#33443,
#33444,#33445,#33446,#33447,#33448,#33449,#33450,#33451,#33452,#33453,#33454,
#33455,#33456,#33457,#33458,#33459,#33460,#33461,#33462,#33463,#33464,#33465,
#33466,#33467,#33468,#33469,#33470,#33471,#33472,#33473,#33474,#33475,#33476,
#33477,#33478,#33479,#33480,#33481,#33482,#33483,#33484,#33485,#33486,#33487,
#33488,#33489,#33490,#33491,#33492,#33493,#33494,#33495,#33496,#33497,#33498,
#33499,#33500,#33501,#33502,#33503,#33504,#33505,#33506,#33507,#33508,#33509,
#33510,#33511,#33512,#33513,#33514,#33515,#33516,#33517,#33518,#33519,#33520,
#33521,#33522,#33523,#33524,#33525,#33526,#33527,#33528,#33529,#33530,#33531,
#33532,#33533,#33534,#33535,#33536,#33537,#33538,#33539),.UNSPECIFIED.,
 .F.,.F.,(4,2,2,2,2,2,2,2,2,2,2,2,2,2,2,2,2,2,2,2,2,2,2,2,2,2,2,2,2,2,2,
2,2,2,2,2,2,2,2,2,2,2,2,2,2,2,2,2,2,2,2,2,2,2,2,2,2,2,2,2,2,2,2,2,2,2,2,
2,2,2,2,2,2,2,2,2,2,2,2,2,2,2,2,2,2,2,2,2,4),(-4.27125438342981,-4.25501503648509,
-4.24260511705344,-4.23465441741718,-4.22709219941081,-4.21860334803321,
-4.20542534814838,-4.15740314793215,-4.09923643068426,-4.07206829635785,
-4.06450393322421,-4.05974027376557,-4.05497257873807,-4.04738941569824,
-4.02234537977007,-3.96228631289094,-3.91372246976973,-3.90067833068308,
-3.89221664485113,-3.88415466816843,-3.8727770921359,-3.84489478392995,
-3.7649527655659,-3.74516285058777,-3.73169712707356,-3.72577274294145,
-3.72128221104,-3.71584007187348,-3.70502115078077,-3.65964884495702,-3.61991933351525,
-3.57638523703159,-3.56367201746124,-3.55527675665466,-3.54717128623843,
-3.53738109235133,-3.51308591487986,-3.42884257392313,-3.40872384254713,
-3.39509979276722,-3.38914856092271,-3.38465589053771,-3.37923346272373,
-3.36851601051705,-3.32501628043338,-3.28770273394464,-3.25601417416582,
-3.23376567816179,-3.22353092260851,-3.21555361718432,-3.20659896962883,
-3.19115987088382,-3.11619463079249,-3.08046995413687,-3.06057975224822,
-3.05373739595098,-3.04911907461424,-3.04415168149525,-3.03564167781744,
-2.9908661521944,-2.91482699786847,-2.89552106398494,-2.88580792449511,
-2.87863983810974,-2.8696129527188,-2.85423082916165,-2.78046699105375,
-2.7274082730617,-2.71878458698864,-2.71379288662701,-2.7092400356556,-2.70250860873931,
-2.6849169020748,-2.61766719826348,-2.56722834046539,-2.55407975898685,
-2.54559653088004,-2.53754623185693,-2.52623989463462,-2.49882076215399,
-2.41830902274939,-2.39847263128795,-2.38498422640902,-2.37905578439826,
-2.37456471207313,-2.36912503088202,-2.35865213340398,-2.30357121827838,
-2.25622471834554),.UNSPECIFIED.);
#2105=B_SPLINE_CURVE_WITH_KNOTS('',3,(#33545,#33546,#33547,#33548,#33549,
#33550,#33551,#33552,#33553,#33554,#33555,#33556,#33557,#33558,#33559,#33560,
#33561,#33562,#33563,#33564,#33565,#33566,#33567,#33568,#33569,#33570,#33571,
#33572,#33573,#33574,#33575,#33576,#33577,#33578,#33579,#33580,#33581,#33582,
#33583,#33584,#33585,#33586,#33587,#33588,#33589,#33590,#33591,#33592,#33593,
#33594,#33595,#33596,#33597,#33598,#33599,#33600,#33601,#33602,#33603,#33604,
#33605,#33606,#33607,#33608,#33609,#33610,#33611,#33612,#33613,#33614,#33615,
#33616,#33617,#33618,#33619,#33620,#33621,#33622,#33623,#33624,#33625,#33626,
#33627,#33628,#33629,#33630,#33631,#33632,#33633,#33634,#33635,#33636,#33637,
#33638,#33639,#33640,#33641,#33642,#33643,#33644,#33645,#33646,#33647,#33648,
#33649,#33650,#33651,#33652,#33653,#33654,#33655,#33656,#33657,#33658,#33659,
#33660,#33661,#33662,#33663,#33664,#33665,#33666,#33667,#33668,#33669,#33670,
#33671,#33672,#33673,#33674,#33675,#33676,#33677,#33678,#33679,#33680,#33681,
#33682,#33683,#33684,#33685,#33686,#33687,#33688,#33689,#33690,#33691,#33692,
#33693,#33694,#33695,#33696,#33697,#33698,#33699,#33700,#33701,#33702,#33703,
#33704,#33705,#33706,#33707,#33708,#33709,#33710,#33711,#33712,#33713,#33714,
#33715,#33716,#33717,#33718,#33719,#33720,#33721,#33722),.UNSPECIFIED.,
 .F.,.F.,(4,2,2,2,2,2,2,2,2,2,2,2,2,2,2,2,2,2,2,2,2,2,2,2,2,2,2,2,2,2,2,
2,2,2,2,2,2,2,2,2,2,2,2,2,2,2,2,2,2,2,2,2,2,2,2,2,2,2,2,2,2,2,2,2,2,2,2,
2,2,2,2,2,2,2,2,2,2,2,2,2,2,2,2,2,2,2,2,2,4),(-2.01521772153702,-1.98189085311168,
-1.90192497698326,-1.88553068491922,-1.87628868202977,-1.86834789004264,
-1.85854333615922,-1.838736961262,-1.81188688524793,-1.76967090638649,-1.71907053077995,
-1.71044459355391,-1.70545297332107,-1.7008483173261,-1.69407731971124,
-1.67476911418862,-1.64074638077149,-1.56260627468835,-1.54754614456766,
-1.53867045799165,-1.53067908408467,-1.52030667513674,-1.4972202789615,
-1.46376290481328,-1.39771405901254,-1.37901132537832,-1.37212511413708,
-1.36754516291517,-1.36260988022624,-1.35424621040038,-1.31287723514507,
-1.22731770615837,-1.21170187761505,-1.20262624485003,-1.19546625661394,
-1.18582495524724,-1.16689470595396,-1.1201291530442,-1.06178273901728,
-1.04255668617962,-1.03560095446714,-1.0310083758883,-1.02609650594405,
-1.01784021525856,-0.979217569618965,-0.891117769050643,-0.875281537132275,
-0.866159406749446,-0.858285873741104,-0.848363292283576,-0.827896276301347,
-0.752617947548739,-0.709000681849122,-0.700500487252411,-0.69553636561546,
-0.69091907495662,-0.684075273781897,-0.664160007638736,-0.628350626862018,
-0.553520026184348,-0.538248685217414,-0.529247523979435,-0.521281811057072,
-0.511134897410401,-0.489388178113713,-0.458728402328911,-0.444277199347154,
-0.381359106747041,-0.367591630640181,-0.36202819565,-0.357496954051565,
-0.352461575228102,-0.343626805114538,-0.332424032639677,-0.306467348974908,
-0.220414383883096,-0.204698632238166,-0.194807308056524,-0.186863593828534,
-0.177692822509181,-0.16117448170027,-0.14021024908188,-0.0645403267953068,
-0.0348516411336477,-0.0269078611245573,-0.0220637278553226,-0.0178656397223858,
-0.0131614481692901,-0.000969409447366421),.UNSPECIFIED.);
#2106=B_SPLINE_CURVE_WITH_KNOTS('',3,(#33723,#33724,#33725,#33726,#33727,
#33728,#33729,#33730),.UNSPECIFIED.,.F.,.F.,(4,2,2,4),(-4.27041062777532,
-4.20060841514599,-4.15017306640079,-4.14975517296478),.UNSPECIFIED.);
#2107=B_SPLINE_CURVE_WITH_KNOTS('',3,(#33731,#33732,#33733,#33734,#33735,
#33736,#33737,#33738,#33739,#33740,#33741,#33742,#33743,#33744,#33745,#33746,
#33747,#33748,#33749,#33750,#33751,#33752,#33753,#33754,#33755,#33756,#33757,
#33758,#33759,#33760,#33761,#33762,#33763,#33764,#33765,#33766,#33767,#33768,
#33769,#33770,#33771,#33772,#33773,#33774,#33775,#33776,#33777,#33778,#33779,
#33780,#33781,#33782,#33783,#33784,#33785,#33786,#33787,#33788,#33789,#33790,
#33791,#33792,#33793,#33794,#33795,#33796,#33797,#33798,#33799,#33800,#33801,
#33802,#33803,#33804,#33805,#33806,#33807,#33808,#33809,#33810,#33811,#33812,
#33813,#33814,#33815,#33816,#33817,#33818,#33819,#33820,#33821,#33822,#33823,
#33824,#33825,#33826,#33827,#33828,#33829,#33830,#33831,#33832,#33833,#33834,
#33835,#33836,#33837,#33838,#33839,#33840,#33841,#33842,#33843,#33844,#33845,
#33846,#33847,#33848,#33849,#33850,#33851,#33852,#33853,#33854,#33855,#33856,
#33857,#33858,#33859,#33860,#33861,#33862,#33863,#33864,#33865,#33866,#33867,
#33868,#33869,#33870,#33871,#33872,#33873,#33874,#33875,#33876,#33877,#33878,
#33879,#33880,#33881,#33882,#33883,#33884,#33885,#33886,#33887,#33888,#33889,
#33890,#33891,#33892,#33893,#33894,#33895,#33896,#33897,#33898,#33899,#33900,
#33901,#33902,#33903,#33904,#33905,#33906,#33907,#33908,#33909,#33910,#33911,
#33912,#33913,#33914,#33915,#33916,#33917,#33918,#33919,#33920,#33921,#33922),
 .UNSPECIFIED.,.F.,.F.,(4,2,2,2,2,2,2,2,2,2,2,2,2,2,2,2,2,2,2,2,2,2,2,2,
2,2,2,2,2,2,2,2,2,2,2,2,2,2,2,2,2,2,2,2,2,2,2,2,2,2,2,2,2,2,2,2,2,2,2,2,
2,2,2,2,2,2,2,2,2,2,2,2,2,2,2,2,2,2,2,2,2,2,2,2,2,2,2,2,2,2,2,2,2,2,2,4),
(-2.25622471834554,-2.25536552022434,-2.2263312213498,-2.21508125273909,
-2.20695984282477,-2.19843959820622,-2.18510984640676,-2.13543462955219,
-2.06954903287775,-2.0506677105141,-2.04375646235058,-2.03917118349923,
-2.03424269187976,-2.02591367806257,-1.98553135179024,-1.89823898096635,
-1.88279518260011,-1.87384010957296,-1.8658638278209,-1.85563232409652,
-1.83339864969124,-1.8017424399485,-1.76444015904065,-1.72095929769792,
-1.71024466643675,-1.70482314777365,-1.70033095952526,-1.69437991573311,
-1.68075482211882,-1.66063109265217,-1.57638798090588,-1.55206705678386,
-1.5422734746708,-1.53416791689761,-1.52577529122092,-1.51307147037056,
-1.46963808682529,-1.42987874954713,-1.38450816488483,-1.37369021161422,
-1.36824872106627,-1.36380174637027,-1.3579045354989,-1.34459559291259,
-1.32512609984941,-1.24902049537014,-1.21780106291181,-1.20596326157002,
-1.19782065680891,-1.18947759237621,-1.17702226000682,-1.13671198085963,
-1.09495253559571,-1.04786311567467,-1.03708992884157,-1.03165735441404,
-1.0271669086193,-1.02123237517546,-1.00770260449622,-0.987776380251331,
-0.90615254887284,-0.879595278557972,-0.868444245878143,-0.86034116349014,
-0.851792687214371,-0.838316633907228,-0.779904302837737,-0.718216134589707,
-0.703027116179809,-0.696639467277713,-0.692098004501017,-0.686943111476073,
-0.677542229674619,-0.626720905989134,-0.551878241313314,-0.536607702827611,
-0.527606601711726,-0.519640694239043,-0.509493193811317,-0.487743790768027,
-0.45707882617708,-0.442614713573513,-0.379658936821854,-0.365930164001574,
-0.360373089550245,-0.355798193213172,-0.350742414127901,-0.341811809955642,
-0.287605582224593,-0.215870373411604,-0.200310179304,-0.191247303456596,
-0.184087022954339,-0.174431897017359,-0.155423316492378,-0.121316291652191),
 .UNSPECIFIED.);
#2108=B_SPLINE_CURVE_WITH_KNOTS('',3,(#33927,#33928,#33929,#33930,#33931,
#33932,#33933,#33934,#33935,#33936,#33937,#33938,#33939,#33940,#33941,#33942,
#33943,#33944,#33945,#33946,#33947,#33948,#33949,#33950,#33951,#33952,#33953,
#33954,#33955,#33956,#33957,#33958,#33959,#33960,#33961,#33962,#33963,#33964,
#33965,#33966,#33967,#33968,#33969,#33970,#33971,#33972,#33973,#33974,#33975,
#33976,#33977,#33978,#33979,#33980,#33981,#33982,#33983,#33984,#33985,#33986,
#33987,#33988,#33989,#33990,#33991,#33992,#33993,#33994,#33995,#33996,#33997,
#33998,#33999,#34000,#34001,#34002,#34003,#34004,#34005,#34006,#34007,#34008,
#34009,#34010,#34011,#34012,#34013,#34014,#34015,#34016,#34017,#34018,#34019,
#34020,#34021,#34022,#34023,#34024,#34025,#34026,#34027,#34028,#34029,#34030,
#34031,#34032,#34033,#34034,#34035,#34036,#34037,#34038,#34039,#34040,#34041,
#34042,#34043,#34044,#34045,#34046,#34047,#34048,#34049,#34050,#34051,#34052,
#34053,#34054,#34055,#34056,#34057,#34058,#34059,#34060,#34061,#34062,#34063,
#34064,#34065,#34066,#34067,#34068,#34069,#34070,#34071,#34072,#34073,#34074,
#34075,#34076,#34077,#34078,#34079,#34080,#34081,#34082,#34083,#34084,#34085,
#34086,#34087,#34088,#34089,#34090,#34091,#34092,#34093,#34094,#34095,#34096,
#34097,#34098,#34099,#34100,#34101,#34102,#34103,#34104,#34105,#34106,#34107,
#34108,#34109,#34110,#34111,#34112,#34113,#34114,#34115,#34116),
 .UNSPECIFIED.,.F.,.F.,(4,2,2,2,2,2,2,2,2,2,2,2,2,2,2,2,2,2,2,2,2,2,2,2,
2,2,2,2,2,2,2,2,2,2,2,2,2,2,2,2,2,2,2,2,2,2,2,2,2,2,2,2,2,2,2,2,2,2,2,2,
2,2,2,2,2,2,2,2,2,2,2,2,2,2,2,2,2,2,2,2,2,2,2,2,2,2,2,2,2,2,2,2,2,2,4),
(-4.15039881543784,-4.11479463190062,-4.07497675799088,-4.06667127640619,
-4.06174828731719,-4.05716099185009,-4.0502361285809,-4.03124919218212,
-3.94184048425317,-3.92126782833572,-3.90498135058491,-3.89585576632678,
-3.88790537197335,-3.87794541119152,-3.85727461500573,-3.76753823808888,
-3.74705294636872,-3.73325477609339,-3.72727507837133,-3.72278084264605,
-3.71738084643567,-3.70709482045411,-3.63244252110455,-3.59675740841868,
-3.57265758734148,-3.56212247252427,-3.55411104617841,-3.54531736437953,
-3.53065379020532,-3.44965729922197,-3.40203535889951,-3.393497559649,-3.38852479200425,
-3.38396413034893,-3.37827791318012,-3.36375025005964,-3.30147516923983,
-3.25260141180522,-3.23351915224546,-3.22384857891598,-3.21668531871961,
-3.20762973691661,-3.19211032229828,-3.11987835296335,-3.06558246290022,
-3.05694859346522,-3.05195516559223,-3.04740408765511,-3.04068009896399,
-3.0231356547161,-2.96336771938735,-2.95040476509661,-2.91993745716488,
-2.89828531993084,-2.88815294038015,-2.88018689362551,-2.87117299847572,
-2.85584900336914,-2.78152778202518,-2.74544933135652,-2.72544237557882,
-2.71858671558012,-2.71396639039326,-2.70900463200773,-2.70051891299499,
-2.65843322432584,-2.59829384919797,-2.56565012929148,-2.55395607632598,
-2.54575744642759,-2.53834497438165,-2.52836151328386,-2.50246524163413,
-2.42014337336625,-2.40016819903877,-2.3866134437444,-2.38067423788575,
-2.37618287581889,-2.37075248957991,-2.36032231954279,-2.30435307992658,
-2.25671992832685,-2.22788576231526,-2.21666318913448,-2.20854714480596,
-2.20001973962504,-2.18665147938341,-2.13546424758547,-2.06359329968271,
-2.05000033540087,-2.04411768037304,-2.03962273002691,-2.0342258026487,
-2.02363614110582,-2.01521772153702),.UNSPECIFIED.);
#2109=B_SPLINE_CURVE_WITH_KNOTS('',3,(#34118,#34119,#34120,#34121,#34122,
#34123,#34124,#34125,#34126,#34127,#34128,#34129,#34130,#34131,#34132,#34133,
#34134,#34135),.UNSPECIFIED.,.F.,.F.,(4,2,2,2,2,2,2,2,4),(-0.121316291652191,
-0.107361750950517,-0.061796577017454,-0.0331257074193108,-0.0252540591814017,
-0.0204254665052418,-0.0162346899153542,-0.0115182785010899,-0.000969384353663965),
 .UNSPECIFIED.);
#2110=B_SPLINE_CURVE_WITH_KNOTS('',3,(#34136,#34137,#34138,#34139,#34140,
#34141,#34142,#34143,#34144,#34145,#34146,#34147,#34148,#34149,#34150,#34151,
#34152,#34153,#34154,#34155,#34156,#34157,#34158,#34159,#34160,#34161,#34162,
#34163,#34164,#34165,#34166,#34167,#34168,#34169,#34170,#34171,#34172,#34173,
#34174,#34175,#34176,#34177,#34178,#34179,#34180,#34181,#34182,#34183,#34184,
#34185,#34186,#34187,#34188,#34189,#34190,#34191,#34192,#34193,#34194,#34195,
#34196,#34197,#34198,#34199,#34200,#34201,#34202,#34203,#34204,#34205,#34206,
#34207,#34208,#34209,#34210,#34211,#34212,#34213,#34214,#34215,#34216,#34217,
#34218,#34219,#34220,#34221,#34222,#34223,#34224,#34225,#34226,#34227,#34228,
#34229,#34230,#34231,#34232,#34233,#34234,#34235,#34236,#34237,#34238,#34239,
#34240,#34241,#34242,#34243,#34244,#34245,#34246,#34247,#34248,#34249,#34250,
#34251,#34252,#34253,#34254,#34255,#34256,#34257,#34258,#34259,#34260,#34261,
#34262,#34263,#34264,#34265,#34266,#34267,#34268,#34269,#34270,#34271,#34272,
#34273,#34274,#34275,#34276,#34277,#34278,#34279,#34280,#34281,#34282,#34283,
#34284,#34285,#34286,#34287,#34288,#34289,#34290,#34291,#34292,#34293,#34294,
#34295,#34296,#34297,#34298,#34299,#34300,#34301,#34302,#34303,#34304,#34305,
#34306,#34307,#34308,#34309),.UNSPECIFIED.,.F.,.F.,(4,2,2,2,2,2,2,2,2,2,
2,2,2,2,2,2,2,2,2,2,2,2,2,2,2,2,2,2,2,2,2,2,2,2,2,2,2,2,2,2,2,2,2,2,2,2,
2,2,2,2,2,2,2,2,2,2,2,2,2,2,2,2,2,2,2,2,2,2,2,2,2,2,2,2,2,2,2,2,2,2,2,2,
2,2,2,2,4),(-4.27162971850408,-4.21647145483053,-4.16935911810154,-4.14070617443029,
-4.12950679259992,-4.12139380677792,-4.11285740367882,-4.09944885629476,
-4.04646006949341,-3.99134782946366,-3.96619574600893,-3.95880428730962,
-3.95407704652289,-3.94985293354377,-3.94265223304114,-3.92146440205188,
-3.86460330963846,-3.8133320373352,-3.79760013347601,-3.7885857185974,-3.78061867797267,
-3.77048429354131,-3.75391110738484,-3.67617235962659,-3.63512231336485,
-3.62460829613906,-3.619225870845,-3.61472848607077,-3.60882420596542,-3.59510384854512,
-3.53175324938251,-3.47242878199998,-3.45892037960446,-3.45036351153777,
-3.44226087351411,-3.43112399531668,-3.40470154143459,-3.32293733235216,
-3.30300268693756,-3.2894668338292,-3.28353027001578,-3.2790384958121,-3.2736046531874,
-3.26316023679669,-3.20744021218963,-3.15963795216371,-3.13074302890395,
-3.11951128464398,-3.11139276834333,-3.10286645866028,-3.08950780457596,
-3.03879173020421,-2.98880058588685,-2.96737538921008,-2.95313516320461,
-2.94708214192599,-2.94262071031482,-2.93728822221085,-2.92732429090972,
-2.85089527879434,-2.80115910526737,-2.78657615176535,-2.77779812319084,
-2.76978053137152,-2.7593874387562,-2.73644951866057,-2.66407402854572,
-2.6214472071367,-2.61304066857376,-2.60809559919181,-2.60351970426755,
-2.59665861654961,-2.57814627226511,-2.51184798938324,-2.47833472858878,
-2.45522256679618,-2.44484479204605,-2.43685173195352,-2.42797665594156,
-2.41292369964032,-2.33475596651531,-2.30077297787767,-2.28147708800115,
-2.27470707716446,-2.27010206256504,-2.26510897589423,-2.25669555075149),
 .UNSPECIFIED.);
#2111=B_SPLINE_CURVE_WITH_KNOTS('',3,(#34315,#34316,#34317,#34318,#34319,
#34320,#34321,#34322,#34323,#34324,#34325,#34326,#34327,#34328,#34329,#34330,
#34331,#34332,#34333,#34334,#34335,#34336,#34337,#34338,#34339,#34340,#34341,
#34342,#34343,#34344,#34345,#34346,#34347,#34348,#34349,#34350,#34351,#34352,
#34353,#34354,#34355,#34356,#34357,#34358,#34359,#34360,#34361,#34362,#34363,
#34364,#34365,#34366,#34367,#34368,#34369,#34370,#34371,#34372,#34373,#34374,
#34375,#34376,#34377,#34378,#34379,#34380,#34381,#34382,#34383,#34384,#34385,
#34386,#34387,#34388,#34389,#34390,#34391,#34392,#34393,#34394,#34395,#34396,
#34397,#34398,#34399,#34400,#34401,#34402,#34403,#34404,#34405,#34406,#34407,
#34408,#34409,#34410,#34411,#34412,#34413,#34414,#34415,#34416,#34417,#34418,
#34419,#34420,#34421,#34422,#34423,#34424,#34425,#34426,#34427,#34428,#34429,
#34430,#34431,#34432,#34433,#34434,#34435,#34436,#34437,#34438,#34439,#34440,
#34441,#34442,#34443,#34444,#34445,#34446,#34447,#34448,#34449,#34450,#34451,
#34452,#34453,#34454,#34455,#34456,#34457,#34458,#34459,#34460,#34461,#34462,
#34463,#34464,#34465,#34466,#34467,#34468,#34469,#34470,#34471,#34472,#34473,
#34474,#34475,#34476,#34477,#34478,#34479,#34480,#34481,#34482,#34483,#34484,
#34485,#34486,#34487,#34488,#34489,#34490,#34491,#34492,#34493,#34494,#34495,
#34496,#34497,#34498),.UNSPECIFIED.,.F.,.F.,(4,2,2,2,2,2,2,2,2,2,2,2,2,
2,2,2,2,2,2,2,2,2,2,2,2,2,2,2,2,2,2,2,2,2,2,2,2,2,2,2,2,2,2,2,2,2,2,2,2,
2,2,2,2,2,2,2,2,2,2,2,2,2,2,2,2,2,2,2,2,2,2,2,2,2,2,2,2,2,2,2,2,2,2,2,2,
2,2,2,2,2,2,4),(-2.01520948096664,-2.00714966847584,-1.99120964466136,-1.98206359854776,
-1.9741140621053,-1.96417976659391,-1.9436580874181,-1.86826470998595,-1.82479760849636,
-1.81629583250565,-1.811330398371,-1.80671156184379,-1.79986500223167,-1.77993818866968,
-1.74410159940624,-1.66927627089529,-1.65399714801093,-1.64499254446706,
-1.63702447368903,-1.62687550007638,-1.60512834508337,-1.57447188850431,
-1.56005588883022,-1.49722787237706,-1.48333823662209,-1.47775362881404,
-1.47321658496489,-1.46819038909922,-1.45940341807256,-1.44828100046701,
-1.42262517206948,-1.33898213335442,-1.319984716643,-1.31021051423517,-1.30227130083805,
-1.2930051921322,-1.27601870830014,-1.25425667506102,-1.19588572288241,
-1.151537258383,-1.14303198573574,-1.13806614390089,-1.13344830994648,-1.12660520695635,
-1.10670328369768,-1.07093864220888,-0.996000658509977,-0.980556083160654,
-0.971601336953702,-0.963625801812645,-0.953395889306798,-0.931168427582342,
-0.899523888576052,-0.862214307362673,-0.818732447730419,-0.808018510606879,
-0.802597406683794,-0.798105599198714,-0.79215510823377,-0.778531478421417,
-0.758410106682633,-0.674183301024425,-0.649857248695053,-0.640063376602571,
-0.631958227018882,-0.623566683980017,-0.610865829747433,-0.567461727852808,
-0.527686177663002,-0.482310317332872,-0.47149264194447,-0.466051484430089,
-0.461604893462648,-0.455708335641188,-0.442401438811369,-0.422935488793669,
-0.346857777686487,-0.315621487148793,-0.303782398475346,-0.295640057984666,
-0.287298202427402,-0.274846507863389,-0.234570170721794,-0.192797259552049,
-0.145692833123208,-0.134920400312372,-0.129488251705744,-0.124998184520262,
-0.119064185883121,-0.105535772772246,-0.0856116831592208,-0.000971006619263802),
 .UNSPECIFIED.);
#2112=B_SPLINE_CURVE_WITH_KNOTS('',3,(#34499,#34500,#34501,#34502,#34503,
#34504,#34505,#34506,#34507,#34508,#34509,#34510,#34511,#34512,#34513,#34514,
#34515,#34516),.UNSPECIFIED.,.F.,.F.,(4,2,2,2,2,2,2,2,4),(-4.27109517320269,
-4.25595028618041,-4.24411643550503,-4.23615525313697,-4.22859989927471,
-4.22012636940361,-4.20702173602339,-4.16036421318888,-4.15039881543784),
 .UNSPECIFIED.);
#2113=B_SPLINE_CURVE_WITH_KNOTS('',3,(#34517,#34518,#34519,#34520,#34521,
#34522,#34523,#34524,#34525,#34526,#34527,#34528,#34529,#34530,#34531,#34532,
#34533,#34534,#34535,#34536,#34537,#34538,#34539,#34540,#34541,#34542,#34543,
#34544,#34545,#34546,#34547,#34548,#34549,#34550,#34551,#34552,#34553,#34554,
#34555,#34556,#34557,#34558,#34559,#34560,#34561,#34562,#34563,#34564,#34565,
#34566,#34567,#34568,#34569,#34570,#34571,#34572,#34573,#34574,#34575,#34576,
#34577,#34578,#34579,#34580,#34581,#34582,#34583,#34584,#34585,#34586,#34587,
#34588,#34589,#34590,#34591,#34592,#34593,#34594,#34595,#34596,#34597,#34598,
#34599,#34600,#34601,#34602,#34603,#34604,#34605,#34606,#34607,#34608,#34609,
#34610,#34611,#34612,#34613,#34614,#34615,#34616,#34617,#34618,#34619,#34620,
#34621,#34622,#34623,#34624,#34625,#34626,#34627,#34628,#34629,#34630,#34631,
#34632,#34633,#34634,#34635,#34636,#34637,#34638,#34639,#34640,#34641,#34642,
#34643,#34644,#34645,#34646,#34647,#34648,#34649,#34650,#34651,#34652,#34653,
#34654,#34655,#34656,#34657,#34658,#34659,#34660,#34661,#34662,#34663,#34664,
#34665,#34666,#34667,#34668,#34669,#34670,#34671,#34672,#34673,#34674,#34675,
#34676,#34677,#34678,#34679,#34680,#34681,#34682,#34683,#34684,#34685,#34686,
#34687,#34688,#34689,#34690,#34691,#34692,#34693,#34694,#34695,#34696,#34697,
#34698,#34699,#34700,#34701,#34702,#34703,#34704),.UNSPECIFIED.,.F.,.F.,
(4,2,2,2,2,2,2,2,2,2,2,2,2,2,2,2,2,2,2,2,2,2,2,2,2,2,2,2,2,2,2,2,2,2,2,
2,2,2,2,2,2,2,2,2,2,2,2,2,2,2,2,2,2,2,2,2,2,2,2,2,2,2,2,2,2,2,2,2,2,2,2,
2,2,2,2,2,2,2,2,2,2,2,2,2,2,2,2,2,2,2,2,2,2,4),(-2.25669555075149,-2.25647827895454,
-2.20578058586402,-2.16268910067092,-2.13632276437092,-2.11677383023448,
-2.10701565089744,-2.09907620001544,-2.08979480068367,-2.07273525067124,
-2.05084829556189,-1.99176820740479,-1.94834782052542,-1.93984615853667,
-1.9348806641097,-1.9302616643194,-1.92341471009007,-1.90348559916168,-1.86764277222077,
-1.79282472224593,-1.7775441896738,-1.76853912840511,-1.76057087696362,
-1.75042198070147,-1.72867628794975,-1.69802317465763,-1.68362096182469,
-1.62082906624937,-1.60689818337004,-1.60130672704128,-1.59676803218511,
-1.59174535291663,-1.58297530352149,-1.52841708151284,-1.45670808658164,
-1.4411391115441,-1.43207254033551,-1.42491009139806,-1.41525301632689,
-1.39624432081175,-1.34825113184082,-1.28766038015784,-1.27113260619435,
-1.26456398245095,-1.2599939956188,-1.25492155714437,-1.24591584879435,
-1.19490619992112,-1.11940826874441,-1.10402666402093,-1.09508498211598,
-1.0871072916481,-1.07685537733022,-1.05449601422997,-1.02257682305855,
-0.985463330744092,-0.942240468954855,-0.931538012105892,-0.926119254621201,
-0.921627344919087,-0.915674046792797,-0.902033083617493,-0.881875275748018,
-0.797135529117148,-0.773130621423109,-0.763426894080399,-0.755343659332821,
-0.746920618150429,-0.734061707832606,-0.688413450433646,-0.674871928842943,
-0.613983211505506,-0.597814347758796,-0.591304877975362,-0.586745006251162,
-0.581647886094767,-0.572522621328682,-0.519828088916931,-0.446696116133087,
-0.431254578705578,-0.422216765547528,-0.415052805950926,-0.405362078722874,
-0.386165424468412,-0.336727645992747,-0.273083181667143,-0.259746139481906,
-0.253907238003859,-0.249416934433612,-0.24398947565407,-0.233240119710802,
-0.189992222714209,-0.121892388973597,-0.121708560596655),.UNSPECIFIED.);
#2114=B_SPLINE_CURVE_WITH_KNOTS('',3,(#34709,#34710,#34711,#34712,#34713,
#34714,#34715,#34716,#34717,#34718,#34719,#34720,#34721,#34722,#34723,#34724,
#34725,#34726,#34727,#34728,#34729,#34730,#34731,#34732,#34733,#34734,#34735,
#34736,#34737,#34738,#34739,#34740,#34741,#34742,#34743,#34744,#34745,#34746,
#34747,#34748,#34749,#34750,#34751,#34752,#34753,#34754,#34755,#34756,#34757,
#34758,#34759,#34760,#34761,#34762,#34763,#34764,#34765,#34766,#34767,#34768,
#34769,#34770,#34771,#34772,#34773,#34774,#34775,#34776,#34777,#34778,#34779,
#34780,#34781,#34782,#34783,#34784,#34785,#34786,#34787,#34788,#34789,#34790,
#34791,#34792,#34793,#34794,#34795,#34796,#34797,#34798,#34799,#34800,#34801,
#34802,#34803,#34804,#34805,#34806,#34807,#34808,#34809,#34810,#34811,#34812,
#34813,#34814,#34815,#34816,#34817,#34818,#34819,#34820,#34821,#34822,#34823,
#34824,#34825,#34826,#34827,#34828,#34829,#34830,#34831,#34832,#34833,#34834,
#34835,#34836,#34837,#34838,#34839,#34840,#34841,#34842,#34843,#34844,#34845,
#34846,#34847,#34848,#34849,#34850,#34851,#34852,#34853,#34854,#34855,#34856,
#34857,#34858,#34859,#34860,#34861,#34862,#34863,#34864,#34865,#34866,#34867,
#34868,#34869,#34870,#34871,#34872,#34873,#34874,#34875,#34876,#34877,#34878,
#34879,#34880,#34881,#34882,#34883,#34884,#34885,#34886,#34887,#34888,#34889,
#34890,#34891,#34892),.UNSPECIFIED.,.F.,.F.,(4,2,2,2,2,2,2,2,2,2,2,2,2,
2,2,2,2,2,2,2,2,2,2,2,2,2,2,2,2,2,2,2,2,2,2,2,2,2,2,2,2,2,2,2,2,2,2,2,2,
2,2,2,2,2,2,2,2,2,2,2,2,2,2,2,2,2,2,2,2,2,2,2,2,2,2,2,2,2,2,2,2,2,2,2,2,
2,2,2,2,2,2,4),(-4.15027967554863,-4.14937388203919,-4.09344939889395,-4.04579468576531,
-4.01695395733201,-4.00573109430837,-3.99761549210625,-3.98908913029071,
-3.97572374309468,-3.92130918179524,-3.86728344800363,-3.84237233664458,
-3.83500391597726,-3.83028216152486,-3.82605527591796,-3.81883620293387,
-3.79747995843651,-3.73401372265628,-3.68454609972552,-3.67145226361893,
-3.6629814182495,-3.65492686095805,-3.64358731177808,-3.61594467822811,
-3.5357293408631,-3.51591949993915,-3.50244476091155,-3.49651942694312,
-3.49202946323963,-3.48658959364629,-3.47577970153583,-3.43052383209003,
-3.39103653714101,-3.34719942263865,-3.33446540892421,-3.32606687266516,
-3.31796581536067,-3.30819023665638,-3.28398326157704,-3.19964409645301,
-3.17952059517719,-3.16589485981238,-3.15994389013728,-3.15545184075872,
-3.15003067911981,-3.13931715331926,-3.09587695755976,-3.05868726476909,
-3.02690120917323,-3.0046068268778,-2.99436531761095,-2.98638832381839,
-2.97743978961056,-2.96202630565742,-2.88686132114048,-2.83575042883008,
-2.82667852656827,-2.82159194461223,-2.8170269386768,-2.81048989921304,
-2.79415938011912,-2.73335926399411,-2.67542744237923,-2.6619629098778,
-2.65341568467747,-2.64530963875434,-2.63414777431965,-2.6075155577395,
-2.52600660098006,-2.50609318920533,-2.49256800147907,-2.48663365013921,
-2.48214249519008,-2.47670810662228,-2.46625930554312,-2.41066259864094,
-2.36279188127302,-2.33387455273174,-2.3226406742808,-2.31452250201875,
-2.30599822709262,-2.29264633273593,-2.24214136140902,-2.18496208613476,
-2.15937392327269,-2.1519438744113,-2.14720881417966,-2.14299161146603,
-2.13582721378967,-2.11302658787055,-2.06762420495383,-2.01520948096664),
 .UNSPECIFIED.);
#2115=B_SPLINE_CURVE_WITH_KNOTS('',3,(#34894,#34895,#34896,#34897,#34898,
#34899,#34900,#34901,#34902,#34903,#34904,#34905,#34906,#34907,#34908,#34909),
 .UNSPECIFIED.,.F.,.F.,(4,2,2,2,2,2,2,4),(-0.121708560596655,-0.0989053417075304,
-0.0886612869199451,-0.0806657415004705,-0.0718170542222974,-0.0626305895064228,
-0.0422719233860505,-0.000969933537610637),.UNSPECIFIED.);
#2116=B_SPLINE_CURVE_WITH_KNOTS('',3,(#34910,#34911,#34912,#34913,#34914,
#34915,#34916,#34917,#34918,#34919,#34920,#34921,#34922,#34923,#34924,#34925,
#34926,#34927,#34928,#34929,#34930,#34931,#34932,#34933,#34934,#34935,#34936,
#34937,#34938,#34939,#34940,#34941,#34942,#34943,#34944,#34945,#34946,#34947,
#34948,#34949,#34950,#34951,#34952,#34953,#34954,#34955,#34956,#34957,#34958,
#34959,#34960,#34961,#34962,#34963,#34964,#34965,#34966,#34967,#34968,#34969,
#34970,#34971,#34972,#34973,#34974,#34975,#34976,#34977,#34978,#34979,#34980,
#34981,#34982,#34983,#34984,#34985,#34986,#34987,#34988,#34989,#34990,#34991,
#34992,#34993,#34994,#34995,#34996,#34997,#34998,#34999,#35000,#35001,#35002,
#35003,#35004,#35005,#35006,#35007,#35008,#35009,#35010,#35011,#35012,#35013,
#35014,#35015,#35016,#35017,#35018,#35019,#35020,#35021,#35022,#35023,#35024,
#35025,#35026,#35027,#35028,#35029,#35030,#35031,#35032,#35033,#35034,#35035,
#35036,#35037,#35038,#35039,#35040,#35041,#35042,#35043,#35044,#35045,#35046,
#35047,#35048,#35049,#35050,#35051,#35052,#35053,#35054,#35055,#35056,#35057,
#35058,#35059,#35060,#35061,#35062,#35063,#35064,#35065,#35066,#35067,#35068,
#35069,#35070,#35071,#35072,#35073,#35074,#35075,#35076,#35077,#35078,#35079,
#35080,#35081,#35082,#35083,#35084,#35085),.UNSPECIFIED.,.F.,.F.,(4,2,2,
2,2,2,2,2,2,2,2,2,2,2,2,2,2,2,2,2,2,2,2,2,2,2,2,2,2,2,2,2,2,2,2,2,2,2,2,
2,2,2,2,2,2,2,2,2,2,2,2,2,2,2,2,2,2,2,2,2,2,2,2,2,2,2,2,2,2,2,2,2,2,2,2,
2,2,2,2,2,2,2,2,2,2,2,2,4),(-4.27062365544879,-4.2045854016667,-4.19594776882903,
-4.18871320832504,-4.1840190730819,-4.17917307545253,-4.17122421916764,
-4.14176590148942,-4.07982410625505,-4.05144086621091,-4.03083792688231,
-4.02088977072974,-4.01294005531295,-4.00380572398322,-3.98791739849639,
-3.92090316498426,-3.86210949373818,-3.85345171741014,-3.84845329333739,
-3.84390473758457,-3.83719463006745,-3.81975505817798,-3.75990468608033,
-3.7123058962321,-3.69332118613209,-3.68366884260179,-3.67650714934979,
-3.66743785317878,-3.65185473269206,-3.58041310104364,-3.5256247144009,
-3.51689024162895,-3.51187532397132,-3.50733377283615,-3.50172882381573,
-3.48771414779401,-3.42496923263108,-3.36597081471164,-3.35247377611142,
-3.34392014424755,-3.3358178393593,-3.32467700619564,-3.29820919005584,
-3.21651417438742,-3.19658699185784,-3.18305534790896,-3.17712006671082,
-3.17262902203515,-3.167195766215,-3.15642123192552,-3.11175150030842,-3.0735105775042,
-3.02801563126963,-3.0151644298852,-3.00674187060416,-2.99865586845352,
-2.9889449512708,-2.96489947351059,-2.88023905105316,-2.86009124081783,
-2.84645350092496,-2.84050018196501,-2.83600758449604,-2.83058726262261,
-2.82020597141197,-2.76330846481984,-2.71624935782424,-2.68761628669727,
-2.67642022183258,-2.66830834663445,-2.65977196016267,-2.6463609650568,
-2.59320424871988,-2.54532411989866,-2.52417145256917,-2.51005861896083,
-2.50402675351805,-2.49952764668416,-2.49416346978328,-2.48404860475659,
-2.40844300856654,-2.37315847519949,-2.34923736215947,-2.33873005593193,
-2.33072176651715,-2.32191375841392,-2.30718277846463,-2.25630106598102),
 .UNSPECIFIED.);
#2117=B_SPLINE_CURVE_WITH_KNOTS('',3,(#35091,#35092,#35093,#35094,#35095,
#35096,#35097,#35098,#35099,#35100,#35101,#35102,#35103,#35104,#35105,#35106,
#35107,#35108,#35109,#35110,#35111,#35112,#35113,#35114,#35115,#35116,#35117,
#35118,#35119,#35120,#35121,#35122,#35123,#35124,#35125,#35126,#35127,#35128,
#35129,#35130,#35131,#35132,#35133,#35134,#35135,#35136,#35137,#35138,#35139,
#35140,#35141,#35142,#35143,#35144,#35145,#35146,#35147,#35148,#35149,#35150,
#35151,#35152,#35153,#35154,#35155,#35156,#35157,#35158,#35159,#35160,#35161,
#35162,#35163,#35164,#35165,#35166,#35167,#35168,#35169,#35170,#35171,#35172,
#35173,#35174,#35175,#35176,#35177,#35178,#35179,#35180,#35181,#35182,#35183,
#35184,#35185,#35186,#35187,#35188,#35189,#35190,#35191,#35192,#35193,#35194,
#35195,#35196,#35197,#35198,#35199,#35200,#35201,#35202,#35203,#35204,#35205,
#35206,#35207,#35208,#35209,#35210,#35211,#35212,#35213,#35214,#35215,#35216,
#35217,#35218,#35219,#35220,#35221,#35222,#35223,#35224,#35225,#35226,#35227,
#35228,#35229,#35230,#35231,#35232,#35233,#35234,#35235,#35236,#35237,#35238,
#35239,#35240,#35241,#35242,#35243,#35244,#35245,#35246,#35247,#35248,#35249,
#35250,#35251,#35252,#35253,#35254,#35255,#35256,#35257,#35258,#35259,#35260,
#35261,#35262,#35263,#35264,#35265,#35266,#35267,#35268,#35269,#35270,#35271,
#35272),.UNSPECIFIED.,.F.,.F.,(4,2,2,2,2,2,2,2,2,2,2,2,2,2,2,2,2,2,2,2,
2,2,2,2,2,2,2,2,2,2,2,2,2,2,2,2,2,2,2,2,2,2,2,2,2,2,2,2,2,2,2,2,2,2,2,2,
2,2,2,2,2,2,2,2,2,2,2,2,2,2,2,2,2,2,2,2,2,2,2,2,2,2,2,2,2,2,2,2,2,2,4),
(-2.01540403041363,-1.97105087182943,-1.93084919110475,-1.9224104388942,
-1.91745914148358,-1.91283411580665,-1.90595068542143,-1.88570462132828,
-1.84889588021947,-1.77578571549031,-1.76033977362606,-1.75130039884835,
-1.74413574399215,-1.73444478558129,-1.71525041721242,-1.66580267212204,
-1.60216460957617,-1.58881549615542,-1.58297417643701,-1.57848325181503,
-1.57305659400479,-1.56231314834687,-1.51912740404222,-1.43715435929942,
-1.42262529873154,-1.41385990755967,-1.40584139840264,-1.39524837742795,
-1.37077410014621,-1.33424309267047,-1.27904087477932,-1.25572791374213,
-1.24830390298614,-1.24403896045695,-1.23936025072194,-1.23219942426583,
-1.20942266243595,-1.16409962945601,-1.1035462346794,-1.08761075996848,
-1.07846702204661,-1.07051931868482,-1.06058708637759,-1.04006878571749,
-0.964690282576342,-0.92123806632143,-0.912738303588415,-0.907774032884151,
-0.903156268135697,-0.896311282261529,-0.876388936118637,-0.840560173777627,
-0.765753188958409,-0.750477526058375,-0.741474998318385,-0.733508786457134,
-0.723362210779881,-0.701620321460426,-0.670971413661392,-0.656560136610894,
-0.593750419093718,-0.579860058722233,-0.574276101613057,-0.569739966332332,
-0.564715296331333,-0.555932041671417,-0.544814981055154,-0.519175287262509,
-0.435630593574715,-0.416578711984817,-0.406795181440412,-0.398857230770941,
-0.389602566155293,-0.372666787672479,-0.350990251114021,-0.29308907677258,
-0.248139866157751,-0.239633955500326,-0.23466870949306,-0.230052247722714,
-0.223212344624252,-0.203328493638811,-0.165047205734008,-0.0968343148362305,
-0.0807251579815768,-0.0707223802273352,-0.0627697178572486,-0.0552960657740107,
-0.0463378343276242,-0.0291380055809453,-0.000969506735735101),
 .UNSPECIFIED.);
#2118=B_SPLINE_CURVE_WITH_KNOTS('',3,(#35273,#35274,#35275,#35276,#35277,
#35278,#35279,#35280,#35281,#35282,#35283,#35284,#35285,#35286,#35287,#35288),
 .UNSPECIFIED.,.F.,.F.,(4,2,2,2,2,2,2,4),(-4.27050797530105,-4.20918175648102,
-4.18921511742037,-4.17566477666909,-4.16972660284406,-4.16523563613543,
-4.15980525540617,-4.15027967554863),.UNSPECIFIED.);
#2119=B_SPLINE_CURVE_WITH_KNOTS('',3,(#35289,#35290,#35291,#35292,#35293,
#35294,#35295,#35296,#35297,#35298,#35299,#35300,#35301,#35302,#35303,#35304,
#35305,#35306,#35307,#35308,#35309,#35310,#35311,#35312,#35313,#35314,#35315,
#35316,#35317,#35318,#35319,#35320,#35321,#35322,#35323,#35324,#35325,#35326,
#35327,#35328,#35329,#35330,#35331,#35332,#35333,#35334,#35335,#35336,#35337,
#35338,#35339,#35340,#35341,#35342,#35343,#35344,#35345,#35346,#35347,#35348,
#35349,#35350,#35351,#35352,#35353,#35354,#35355,#35356,#35357,#35358,#35359,
#35360,#35361,#35362,#35363,#35364,#35365,#35366,#35367,#35368,#35369,#35370,
#35371,#35372,#35373,#35374,#35375,#35376,#35377,#35378,#35379,#35380,#35381,
#35382,#35383,#35384,#35385,#35386,#35387,#35388,#35389,#35390,#35391,#35392,
#35393,#35394,#35395,#35396,#35397,#35398,#35399,#35400,#35401,#35402,#35403,
#35404,#35405,#35406,#35407,#35408,#35409,#35410,#35411,#35412,#35413,#35414,
#35415,#35416,#35417,#35418,#35419,#35420,#35421,#35422,#35423,#35424,#35425,
#35426,#35427,#35428,#35429,#35430,#35431,#35432,#35433,#35434,#35435,#35436,
#35437,#35438,#35439,#35440,#35441,#35442,#35443,#35444,#35445,#35446,#35447,
#35448,#35449,#35450,#35451,#35452,#35453,#35454,#35455,#35456,#35457,#35458,
#35459,#35460,#35461,#35462,#35463,#35464,#35465,#35466,#35467,#35468,#35469,
#35470,#35471,#35472,#35473,#35474,#35475,#35476,#35477,#35478,#35479,#35480),
 .UNSPECIFIED.,.F.,.F.,(4,2,2,2,2,2,2,2,2,2,2,2,2,2,2,2,2,2,2,2,2,2,2,2,
2,2,2,2,2,2,2,2,2,2,2,2,2,2,2,2,2,2,2,2,2,2,2,2,2,2,2,2,2,2,2,2,2,2,2,2,
2,2,2,2,2,2,2,2,2,2,2,2,2,2,2,2,2,2,2,2,2,2,2,2,2,2,2,2,2,2,2,2,2,2,2,4),
(-2.25630106598102,-2.22665188879084,-2.17869341128798,-2.17014812749761,
-2.16517353502421,-2.16061327301725,-2.15383763824685,-2.13593453700016,
-2.10493148874884,-2.02461880953053,-2.008489005903,-1.99930281207444,-1.99135738846346,
-1.98147908044215,-1.96126788018294,-1.88643911726412,-1.84194590014947,
-1.83343942038279,-1.82847310019824,-1.82385501306422,-1.81701180837149,
-1.79711164667502,-1.7613539425913,-1.68639388790096,-1.67095006657059,
-1.66199507027169,-1.65401890969819,-1.64378763498014,-1.62155477871562,
-1.58990006365558,-1.55259707823166,-1.50911627441789,-1.49840176846068,
-1.49298032102185,-1.48848819578634,-1.48253724097305,-1.46891237560183,
-1.44878900710068,-1.3645481816212,-1.34022673719909,-1.33043315772026,
-1.32232767956074,-1.31393521513241,-1.30123179687271,-1.25780207293039,
-1.21804096198826,-1.17266992891469,-1.16185205132341,-1.1564106215643,
-1.15196371009145,-1.14606660037006,-1.13275795317811,-1.11328895698438,
-1.03718695050705,-1.00596565688298,-0.994127752130195,-0.98598521223695,
-0.97764232529372,-0.965187474978963,-0.924881387000842,-0.883120502128747,
-0.836029481961262,-0.82525642770728,-0.819823926033665,-0.815333544401949,
-0.809399101155309,-0.795869557094396,-0.775943688955905,-0.694322035280049,
-0.667764199661518,-0.656613205219409,-0.648510217404342,-0.639961900885749,
-0.626486229351708,-0.568080916515301,-0.506404869931409,-0.491201225169912,
-0.484812416709915,-0.4802708344267,-0.475116628138645,-0.465718842718387,
-0.418204251226746,-0.339084702663833,-0.324158143105303,-0.315311005813255,
-0.307314811154912,-0.296892298533253,-0.273490499830659,-0.239348203981405,
-0.169039366723416,-0.154450184279452,-0.148755300277396,-0.144193160304904,
-0.139226329550409,-0.1307130459406,-0.12134621462309),.UNSPECIFIED.);
#2120=B_SPLINE_CURVE_WITH_KNOTS('',3,(#35485,#35486,#35487,#35488,#35489,
#35490,#35491,#35492,#35493,#35494,#35495,#35496,#35497,#35498,#35499,#35500,
#35501,#35502,#35503,#35504,#35505,#35506,#35507,#35508,#35509,#35510,#35511,
#35512,#35513,#35514,#35515,#35516,#35517,#35518,#35519,#35520,#35521,#35522,
#35523,#35524,#35525,#35526,#35527,#35528,#35529,#35530,#35531,#35532,#35533,
#35534,#35535,#35536,#35537,#35538,#35539,#35540,#35541,#35542,#35543,#35544,
#35545,#35546,#35547,#35548,#35549,#35550,#35551,#35552,#35553,#35554,#35555,
#35556,#35557,#35558,#35559,#35560,#35561,#35562,#35563,#35564,#35565,#35566,
#35567,#35568,#35569,#35570,#35571,#35572,#35573,#35574,#35575,#35576,#35577,
#35578,#35579,#35580,#35581,#35582,#35583,#35584,#35585,#35586,#35587,#35588,
#35589,#35590,#35591,#35592,#35593,#35594,#35595,#35596,#35597,#35598,#35599,
#35600,#35601,#35602,#35603,#35604,#35605,#35606,#35607,#35608,#35609,#35610,
#35611,#35612,#35613,#35614,#35615,#35616,#35617,#35618,#35619,#35620,#35621,
#35622,#35623,#35624,#35625,#35626,#35627,#35628,#35629,#35630,#35631,#35632,
#35633,#35634,#35635,#35636,#35637,#35638,#35639,#35640,#35641,#35642,#35643,
#35644,#35645,#35646,#35647,#35648,#35649,#35650,#35651,#35652,#35653,#35654,
#35655,#35656,#35657,#35658,#35659,#35660,#35661,#35662,#35663,#35664,#35665,
#35666,#35667,#35668,#35669,#35670,#35671,#35672,#35673,#35674,#35675,#35676,
#35677,#35678),.UNSPECIFIED.,.F.,.F.,(4,2,2,2,2,2,2,2,2,2,2,2,2,2,2,2,2,
2,2,2,2,2,2,2,2,2,2,2,2,2,2,2,2,2,2,2,2,2,2,2,2,2,2,2,2,2,2,2,2,2,2,2,2,
2,2,2,2,2,2,2,2,2,2,2,2,2,2,2,2,2,2,2,2,2,2,2,2,2,2,2,2,2,2,2,2,2,2,2,2,
2,2,2,2,2,2,2,4),(-4.15012784700328,-4.13768479087268,-4.11856038692716,
-4.10888262908483,-4.10171943274022,-4.09267098242306,-4.07718174678539,
-4.00462979355366,-3.95114543254014,-3.94221997146866,-3.93716484225613,
-3.9325888492165,-3.92702866492889,-3.91328394762036,-3.85029839280303,
-3.83580949968707,-3.80513830683069,-3.78338664403422,-3.77323799165445,
-3.76527125700535,-3.75626931161481,-3.74099745979581,-3.66620715221463,
-3.63040419672153,-3.61048991443097,-3.60364585284258,-3.59902809761266,
-3.59406323625909,-3.58556118908269,-3.54203078285546,-3.46664636078207,
-3.44613911912456,-3.43620860411234,-3.42826082946351,-3.41911543440626,
-3.40317277771717,-3.34494399390341,-3.29792230798571,-3.27469641717895,
-3.26749016680202,-3.2628021815342,-3.2585461780006,-3.25116953473084,-3.22834090593342,
-3.16627705022579,-3.11718274732264,-3.10411091757459,-3.09564516189169,
-3.0875890428566,-3.0762363730723,-3.04850387674872,-2.96840978302202,-2.9486111058567,
-2.93514217874399,-2.92921822140438,-2.92472879498221,-2.91928895502453,
-2.90847736434631,-2.8631834416426,-2.82360754468627,-2.7798968508195,-2.76717310780248,
-2.75877726160425,-2.75067583975485,-2.74089619370489,-2.71665888095593,
-2.63237133622941,-2.61225307828568,-2.59863028859254,-2.59268021320517,
-2.5881886725426,-2.58276792116707,-2.5720546432161,-2.52859810689668,-2.49136551580897,
-2.45962357568752,-2.4373511814138,-2.42711407875539,-2.41913830473275,
-2.41018885156645,-2.39476780294479,-2.31969439184951,-2.28405057724413,
-2.26418949417452,-2.25735177354734,-2.252735174401,-2.24776806466829,-2.23925557601856,
-2.19343191938615,-2.1361209766679,-2.10481334371136,-2.09296558141158,
-2.08556108274967,-2.07735584576061,-2.06562164239614,-2.03261516951048,
-2.01540403041363),.UNSPECIFIED.);
#2121=B_SPLINE_CURVE_WITH_KNOTS('',3,(#35680,#35681,#35682,#35683,#35684,
#35685,#35686,#35687),.UNSPECIFIED.,.F.,.F.,(4,2,2,4),(-0.12134621462309,
-0.0841733796356287,-0.0489133595461245,-0.000970789400192507),
 .UNSPECIFIED.);
#2122=B_SPLINE_CURVE_WITH_KNOTS('',3,(#35688,#35689,#35690,#35691,#35692,
#35693,#35694,#35695,#35696,#35697,#35698,#35699,#35700,#35701,#35702,#35703,
#35704,#35705,#35706,#35707,#35708,#35709,#35710,#35711,#35712,#35713,#35714,
#35715,#35716,#35717,#35718,#35719,#35720,#35721,#35722,#35723,#35724,#35725,
#35726,#35727,#35728,#35729,#35730,#35731,#35732,#35733,#35734,#35735,#35736,
#35737,#35738,#35739,#35740,#35741,#35742,#35743,#35744,#35745,#35746,#35747,
#35748,#35749,#35750,#35751,#35752,#35753,#35754,#35755,#35756,#35757,#35758,
#35759,#35760,#35761,#35762,#35763,#35764,#35765,#35766,#35767,#35768,#35769,
#35770,#35771,#35772,#35773,#35774,#35775,#35776,#35777,#35778,#35779,#35780,
#35781,#35782,#35783,#35784,#35785,#35786,#35787,#35788,#35789,#35790,#35791,
#35792,#35793,#35794,#35795,#35796,#35797,#35798,#35799,#35800,#35801,#35802,
#35803,#35804,#35805,#35806,#35807,#35808,#35809,#35810,#35811,#35812,#35813,
#35814,#35815,#35816,#35817,#35818,#35819,#35820,#35821,#35822,#35823,#35824,
#35825,#35826,#35827,#35828,#35829,#35830,#35831,#35832,#35833,#35834,#35835,
#35836,#35837,#35838,#35839,#35840,#35841,#35842,#35843,#35844,#35845,#35846,
#35847,#35848,#35849,#35850,#35851,#35852,#35853,#35854,#35855,#35856,#35857,
#35858,#35859,#35860,#35861,#35862,#35863,#35864,#35865,#35866,#35867,#35868,
#35869,#35870,#35871,#35872,#35873,#35874,#35875,#35876,#35877,#35878,#35879,
#35880,#35881,#35882,#35883,#35884,#35885,#35886),.UNSPECIFIED.,.F.,.F.,
(4,3,3,3,3,3,3,3,3,3,3,3,3,3,3,3,3,3,3,3,3,3,3,3,3,3,3,3,3,3,3,3,3,3,3,
3,3,3,3,3,3,3,3,3,3,3,3,3,3,3,3,3,3,3,3,3,3,3,3,3,3,3,3,3,3,3,4),(-16.4167960594917,
-16.3231866314087,-16.2295269003941,-16.1346626816157,-16.0407807338294,
-15.9454253795549,-15.8500700252804,-15.7580593289838,-15.666169660585,
-15.5743745685141,-15.4826447769296,-15.3909489474181,-15.2992633109964,
-15.207564113087,-15.1157697354696,-15.0239260396849,-14.9319324031901,
-14.8594406487004,-14.7674298823043,-14.6755401432034,-14.5837449799275,
-14.4920151166801,-14.4003192152502,-14.308633506742,-14.2169342366647,
-14.1251397872016,-14.0332960196421,-13.941302312234,-13.8688112721204,
-13.7768007953962,-13.6849113464236,-13.5931164733523,-13.5013868992429,
-13.4096912862,-13.3180058649905,-13.2263068807854,-13.1345127132284,-13.0426692258026,
-12.9506757927242,-12.8781818955404,-12.7861710643817,-12.6942812623679,
-12.6024860380833,-12.510756116906,-12.4190601594478,-12.3273743968664,
-12.2356750747262,-12.1438805766162,-12.0520367622262,-11.9600430114395,
-11.8875525189603,-11.7955413127616,-11.7036511308559,-11.6118555223852,
-11.5201252122009,-11.4284288629229,-11.3367427061933,-11.245042988059,
-11.1532480935682,-11.0614038819903,-10.9694097368279,-10.8969231423803,
-10.8060917931932,-10.7154014179413,-10.624792371434,-10.5342434733015,
-10.4883010731468),.UNSPECIFIED.);
#2123=B_SPLINE_CURVE_WITH_KNOTS('',3,(#35892,#35893,#35894,#35895,#35896,
#35897,#35898,#35899,#35900,#35901,#35902,#35903,#35904,#35905,#35906,#35907,
#35908,#35909,#35910,#35911,#35912,#35913,#35914,#35915,#35916,#35917,#35918,
#35919,#35920,#35921,#35922,#35923,#35924,#35925,#35926,#35927,#35928,#35929,
#35930,#35931,#35932,#35933,#35934,#35935,#35936,#35937,#35938,#35939,#35940,
#35941,#35942,#35943,#35944,#35945,#35946,#35947,#35948,#35949,#35950,#35951,
#35952,#35953,#35954,#35955,#35956,#35957,#35958,#35959,#35960,#35961,#35962,
#35963,#35964,#35965,#35966,#35967,#35968,#35969,#35970,#35971,#35972,#35973,
#35974,#35975,#35976,#35977,#35978,#35979,#35980,#35981,#35982,#35983,#35984,
#35985,#35986,#35987,#35988,#35989,#35990,#35991,#35992,#35993,#35994,#35995,
#35996,#35997,#35998,#35999,#36000,#36001,#36002,#36003,#36004,#36005,#36006,
#36007,#36008,#36009,#36010,#36011,#36012,#36013,#36014,#36015,#36016,#36017,
#36018,#36019),.UNSPECIFIED.,.F.,.F.,(4,2,2,2,2,2,2,2,2,2,2,2,2,2,2,2,2,
2,2,2,2,2,2,2,2,2,2,2,2,2,2,2,2,2,2,2,2,2,2,2,2,2,2,2,2,2,2,2,2,2,2,2,2,
2,2,2,2,2,2,2,2,2,2,4),(0.000234205929175261,0.00314848603653745,0.0067045111635944,
0.0168739000398768,0.0615307527646696,0.107334776582209,0.134796991517308,
0.146454022578125,0.155357023913133,0.1652275816112,0.182046717494131,0.274726979642122,
0.320861047165836,0.329525968901998,0.334551414402502,0.339045553572495,
0.345512518537176,0.362198977451867,0.422255985535926,0.46061653869019,
0.485633015473455,0.496017784180939,0.503706305636458,0.511933002375833,
0.525114218951138,0.577956322639473,0.637361486507521,0.654976985957441,
0.667261308249631,0.672788245216847,0.677173157397879,0.682612824762992,
0.693104287233814,0.735392797844991,0.810846433052819,0.83035092034576,
0.840176814946397,0.847438120612499,0.856601019533708,0.872291963298752,
0.937037200195196,0.977056452679149,0.998292865919186,1.00537849982969,
1.01011462818581,1.01511874622903,1.02366974728301,1.06906727212008,1.126308523086,
1.14786674619417,1.16474307983491,1.17401558827739,1.18199803909754,1.19187567048779,
1.21191633823506,1.30302015212422,1.32363980923898,1.33751136488475,1.3435116830711,
1.34800515020899,1.35337159037266,1.36388540057331,1.42020101528312,1.42896226070502),
 .UNSPECIFIED.);
#2124=B_SPLINE_CURVE_WITH_KNOTS('',3,(#36022,#36023,#36024,#36025,#36026,
#36027,#36028,#36029,#36030,#36031,#36032,#36033,#36034,#36035,#36036,#36037,
#36038,#36039,#36040,#36041,#36042,#36043,#36044,#36045,#36046,#36047,#36048,
#36049,#36050,#36051,#36052,#36053,#36054,#36055,#36056,#36057,#36058,#36059,
#36060,#36061,#36062,#36063,#36064,#36065,#36066,#36067,#36068,#36069,#36070,
#36071,#36072,#36073,#36074,#36075,#36076,#36077,#36078,#36079,#36080,#36081,
#36082,#36083,#36084,#36085,#36086,#36087,#36088,#36089,#36090,#36091,#36092,
#36093,#36094,#36095,#36096,#36097,#36098,#36099,#36100,#36101,#36102,#36103,
#36104,#36105,#36106,#36107,#36108,#36109,#36110,#36111,#36112,#36113,#36114,
#36115,#36116,#36117,#36118,#36119,#36120,#36121,#36122,#36123,#36124,#36125,
#36126,#36127,#36128,#36129,#36130,#36131,#36132,#36133,#36134,#36135,#36136,
#36137,#36138,#36139,#36140,#36141,#36142,#36143,#36144,#36145,#36146,#36147,
#36148,#36149,#36150,#36151,#36152,#36153,#36154,#36155,#36156,#36157,#36158,
#36159,#36160,#36161,#36162,#36163,#36164,#36165,#36166,#36167,#36168,#36169,
#36170,#36171,#36172,#36173,#36174,#36175,#36176,#36177,#36178,#36179,#36180,
#36181,#36182,#36183,#36184,#36185,#36186,#36187,#36188,#36189,#36190,#36191,
#36192,#36193,#36194,#36195,#36196,#36197,#36198,#36199),.UNSPECIFIED.,
 .F.,.F.,(4,2,2,2,2,2,2,2,2,2,2,2,2,2,2,2,2,2,2,2,2,2,2,2,2,2,2,2,2,2,2,
2,2,2,2,2,2,2,2,2,2,2,2,2,2,2,2,2,2,2,2,2,2,2,2,2,2,2,2,2,2,2,2,2,2,2,2,
2,2,2,2,2,2,2,2,2,2,2,2,2,2,2,2,2,2,2,2,2,4),(-4.02494338810148,-4.02193033969876,
-3.93992493724719,-3.90898528817333,-3.88701568625783,-3.87674877851422,
-3.86867619689505,-3.85953432808841,-3.84394574206266,-3.77645666986379,
-3.73831257456779,-3.7176502615311,-3.710629551744,-3.70590583610625,-3.70087859080669,
-3.69222160968196,-3.643742635999,-3.60482700916446,-3.56046904788309,-3.54766406691828,
-3.53922113783566,-3.53107721596669,-3.52124854456094,-3.49689370347662,
-3.41231019774439,-3.39212798293188,-3.37846348207257,-3.37249735705626,
-3.36800653077206,-3.36261445928767,-3.35229640830421,-3.27786616873493,
-3.24206093108382,-3.2179332598802,-3.20742999625514,-3.1994619848219,-3.19073705975483,
-3.17624657194768,-3.09373918090561,-3.0467226990626,-3.03822771032295,
-3.03328531554629,-3.02873160499058,-3.02305902147951,-3.0086003235589,
-2.94621901314478,-2.90693705366131,-2.88931455408222,-2.87482004812651,
-2.86604936768864,-2.85800870802107,-2.84754196753151,-2.8242333757087,
-2.73879282065517,-2.7186051338215,-2.70494404426304,-2.69897577112925,
-2.6944722943758,-2.6890391924984,-2.67861256474836,-2.62251078304219,-2.57499960297815,
-2.54621023157496,-2.53499083918056,-2.52687249649355,-2.51936057425587,
-2.50690999221778,-2.4695974098945,-2.39985326444936,-2.37200580601915,
-2.36438676671624,-2.35961144442308,-2.35542554360662,-2.34842693245584,
-2.32886154200221,-2.27072975957472,-2.21429030497882,-2.20088224133076,
-2.1923506436553,-2.18424566655486,-2.17306335946067,-2.1462659572014,-2.06490482925812,
-2.04500240947859,-2.03148397396127,-2.02555345366618,-2.0210642215966,
-2.01563046295169,-2.01551729291411),.UNSPECIFIED.);
#2125=B_SPLINE_CURVE_WITH_KNOTS('',3,(#36205,#36206,#36207,#36208,#36209,
#36210,#36211,#36212,#36213,#36214,#36215,#36216,#36217,#36218,#36219,#36220,
#36221,#36222,#36223,#36224,#36225,#36226,#36227,#36228,#36229,#36230,#36231,
#36232,#36233,#36234,#36235,#36236,#36237,#36238,#36239,#36240,#36241,#36242,
#36243,#36244,#36245,#36246,#36247,#36248,#36249,#36250,#36251,#36252,#36253,
#36254,#36255,#36256,#36257,#36258,#36259,#36260,#36261,#36262,#36263,#36264,
#36265,#36266,#36267,#36268,#36269,#36270,#36271,#36272,#36273,#36274,#36275,
#36276,#36277,#36278,#36279,#36280,#36281,#36282,#36283,#36284,#36285,#36286,
#36287,#36288,#36289,#36290,#36291,#36292,#36293,#36294,#36295,#36296,#36297,
#36298,#36299,#36300,#36301,#36302,#36303,#36304,#36305,#36306,#36307,#36308,
#36309,#36310,#36311,#36312,#36313,#36314,#36315,#36316,#36317,#36318,#36319,
#36320,#36321,#36322,#36323,#36324,#36325,#36326,#36327,#36328,#36329,#36330,
#36331,#36332,#36333,#36334,#36335,#36336,#36337,#36338,#36339,#36340,#36341,
#36342,#36343,#36344,#36345,#36346,#36347,#36348,#36349),.UNSPECIFIED.,
 .F.,.F.,(4,3,3,3,3,3,3,3,3,3,3,3,3,3,3,3,3,3,3,3,3,3,3,3,3,3,3,3,3,3,3,
3,3,3,3,3,3,3,3,3,3,3,3,3,3,3,3,3,4),(74.4826090388022,74.5701171009061,
74.6575762790477,74.7450106693487,74.8324410149635,74.9198880511916,75.0074270886218,
75.0950132990107,75.182740727668,75.2578179239381,75.345779870584,75.4336307723664,
75.521393459374,75.612275189517,75.6999372963985,75.7875855042096,75.8752403136858,
75.9629222251375,76.0506985009842,76.1385309892356,76.2264861090207,76.2484473005182,
76.3362729479242,76.4239892867612,76.5116192868255,76.6025514606096,76.6900863685774,
76.7776096198249,76.8651418461542,76.9527036807354,77.0403641770883,77.1280832577018,
77.215929283375,77.2390766770982,77.3262114351889,77.413235203979,77.500171740674,
77.5913635297995,77.6782069848409,77.7650406065135,77.8518857190326,77.9387636512412,
78.0257484601057,78.1127957290388,78.199980961869,78.2297060536782,78.3409616690792,
78.450436080729,78.5398161890327),.UNSPECIFIED.);
#2126=B_SPLINE_CURVE_WITH_KNOTS('',3,(#36351,#36352,#36353,#36354),
 .UNSPECIFIED.,.F.,.F.,(4,4),(78.5398163397448,79.2203354302582),
 .UNSPECIFIED.);
#2127=B_SPLINE_CURVE_WITH_KNOTS('',3,(#36358,#36359,#36360,#36361,#36362,
#36363,#36364,#36365,#36366,#36367,#36368,#36369,#36370,#36371,#36372,#36373,
#36374,#36375,#36376,#36377,#36378,#36379,#36380,#36381,#36382,#36383,#36384,
#36385,#36386,#36387,#36388,#36389,#36390,#36391,#36392,#36393,#36394,#36395,
#36396,#36397,#36398,#36399,#36400),.UNSPECIFIED.,.F.,.F.,(4,3,3,3,3,3,
3,3,3,3,3,3,3,3,4),(78.5398163399585,78.6513084307211,78.7649921971891,
78.7900351244193,78.8773286503125,78.9645131129572,79.0516120919081,79.1386516146217,
79.2256598993982,79.3126581327151,79.3996674889143,79.4867635448239,79.573902644392,
79.6611829276023,79.7442522065205),.UNSPECIFIED.);
#2128=B_SPLINE_CURVE_WITH_KNOTS('',3,(#36401,#36402,#36403,#36404,#36405,
#36406,#36407,#36408,#36409,#36410,#36411,#36412,#36413,#36414,#36415,#36416,
#36417,#36418,#36419,#36420,#36421,#36422,#36423,#36424,#36425,#36426,#36427,
#36428,#36429,#36430,#36431,#36432,#36433,#36434,#36435,#36436,#36437,#36438,
#36439,#36440,#36441,#36442,#36443,#36444,#36445,#36446,#36447,#36448,#36449,
#36450,#36451,#36452,#36453,#36454,#36455,#36456,#36457,#36458,#36459,#36460,
#36461,#36462,#36463,#36464,#36465,#36466,#36467,#36468,#36469,#36470,#36471,
#36472,#36473,#36474,#36475,#36476,#36477,#36478,#36479,#36480,#36481,#36482,
#36483,#36484,#36485,#36486,#36487,#36488,#36489,#36490,#36491,#36492,#36493,
#36494,#36495,#36496,#36497,#36498,#36499,#36500,#36501,#36502,#36503,#36504,
#36505,#36506,#36507,#36508,#36509,#36510,#36511,#36512,#36513,#36514,#36515,
#36516,#36517,#36518,#36519,#36520,#36521,#36522,#36523,#36524,#36525,#36526,
#36527,#36528,#36529,#36530,#36531,#36532,#36533,#36534,#36535,#36536,#36537,
#36538,#36539,#36540,#36541,#36542,#36543,#36544,#36545,#36546,#36547,#36548),
 .UNSPECIFIED.,.F.,.F.,(4,3,3,3,3,3,3,3,3,3,3,3,3,3,3,3,3,3,3,3,3,3,3,3,
3,3,3,3,3,3,3,3,3,3,3,3,3,3,3,3,3,3,3,3,3,3,3,3,3,4),(74.4816274181351,
74.5692304984992,74.656878603019,74.7446691610334,74.8275176180992,74.9153494983652,
75.003070542925,75.0907037356887,75.1816341430626,75.2691684858901,75.3566897930302,
75.4442187036887,75.5317758574419,75.6194296879387,75.7071409396066,75.7949775033597,
75.8181469946792,75.9059726472772,75.9936876684966,76.0813150465029,76.1722477120974,
76.2597767911498,76.3472930457285,76.4348171195448,76.5223696568421,76.6100192180418,
76.697726397457,76.7855592065891,76.8087763712592,76.8965157262234,76.9841440922057,
77.0716845630408,77.1626497111406,77.25009180658,77.3375211983859,77.4249586234669,
77.5124248194916,77.5999889284807,77.6876110719292,77.7753601050296,77.7994057478392,
77.8864292608986,77.9733147168126,78.0601210604153,78.1468698280841,78.2335825041045,
78.3203028169223,78.4070264415887,78.4938091009427,78.5398163397448),
 .UNSPECIFIED.);
#2129=B_SPLINE_CURVE_WITH_KNOTS('',3,(#36554,#36555,#36556,#36557,#36558,
#36559,#36560,#36561,#36562,#36563,#36564,#36565,#36566,#36567,#36568,#36569,
#36570,#36571,#36572,#36573,#36574,#36575,#36576,#36577,#36578,#36579,#36580,
#36581,#36582,#36583,#36584,#36585,#36586,#36587,#36588,#36589,#36590,#36591,
#36592,#36593,#36594,#36595,#36596,#36597,#36598,#36599,#36600,#36601,#36602,
#36603,#36604,#36605,#36606,#36607,#36608,#36609,#36610,#36611,#36612,#36613,
#36614,#36615,#36616,#36617,#36618,#36619,#36620,#36621,#36622,#36623,#36624,
#36625,#36626,#36627,#36628,#36629,#36630,#36631,#36632,#36633,#36634,#36635,
#36636,#36637,#36638,#36639,#36640,#36641,#36642,#36643,#36644,#36645,#36646,
#36647,#36648,#36649,#36650,#36651,#36652,#36653,#36654,#36655,#36656,#36657,
#36658,#36659,#36660,#36661,#36662,#36663,#36664,#36665,#36666,#36667,#36668,
#36669,#36670,#36671,#36672,#36673,#36674,#36675,#36676,#36677,#36678,#36679,
#36680,#36681,#36682,#36683,#36684,#36685,#36686,#36687,#36688,#36689,#36690,
#36691,#36692,#36693,#36694,#36695,#36696,#36697,#36698,#36699,#36700,#36701),
 .UNSPECIFIED.,.F.,.F.,(4,3,3,3,3,3,3,3,3,3,3,3,3,3,3,3,3,3,3,3,3,3,3,3,
3,3,3,3,3,3,3,3,3,3,3,3,3,3,3,3,3,3,3,3,3,3,3,3,3,4),(68.1983639794465,
68.2861814082633,68.3234122878779,68.4112289338761,68.498934783569,68.5865528382251,
68.6774889415042,68.7650083820866,68.8525148993902,68.9400291482807,69.0275717840982,
69.1152113816981,69.2029085498004,69.2907313551699,69.314041664458,69.4018606979925,
69.4895689306246,69.5771893608844,69.6681245709036,69.7556463539722,69.8431551975548,
69.9306717540522,70.0182166763247,70.1058585176953,70.1935579073452,70.2813828848927,
70.304671041038,70.3924904070348,70.4801989962389,70.5678198064247,70.6587548828238,
70.7462771009769,70.8337863991138,70.9213034290419,71.0088488430415,71.0964912005166,
71.1841911210527,71.2720166468968,71.295300417618,71.3826886130108,71.4699662357104,
71.5571567828598,71.6445910640475,71.7316868152726,71.8187708963969,71.9058644037372,
71.9935560608934,72.0807764862596,72.1687037593107,72.2566310323619),
 .UNSPECIFIED.);
#2130=B_SPLINE_CURVE_WITH_KNOTS('',3,(#36702,#36703,#36704,#36705,#36706,
#36707,#36708,#36709,#36710,#36711,#36712,#36713,#36714,#36715,#36716,#36717,
#36718,#36719,#36720,#36721,#36722,#36723,#36724,#36725,#36726,#36727,#36728,
#36729,#36730,#36731,#36732,#36733,#36734,#36735,#36736,#36737,#36738,#36739,
#36740,#36741,#36742,#36743,#36744,#36745,#36746,#36747,#36748,#36749,#36750,
#36751,#36752,#36753,#36754,#36755,#36756,#36757,#36758,#36759,#36760,#36761,
#36762,#36763,#36764,#36765,#36766,#36767,#36768,#36769,#36770,#36771,#36772,
#36773,#36774,#36775,#36776,#36777,#36778,#36779,#36780,#36781,#36782,#36783,
#36784,#36785,#36786),.UNSPECIFIED.,.F.,.F.,(4,3,3,3,3,3,3,3,3,3,3,3,3,
3,3,3,3,3,3,3,3,3,3,3,3,3,3,3,4),(72.2566310325652,72.285929794198,72.3737616617343,
72.46148269366,72.5491158738982,72.6400462860082,72.7275806166556,72.8151019117628,
72.9026308105475,72.9901879525983,73.0778417717025,73.1655530121446,73.2533895649997,
73.2765591707781,73.3643847775249,73.4520997526408,73.5397270843495,73.6306597672255,
73.7181887997928,73.8057050078983,73.8932290353041,73.9807815263042,74.0684310416082,
74.1561381753079,74.2439709393373,74.2671885473581,74.3549358526297,74.4425595257674,
74.4826090388022),.UNSPECIFIED.);
#2131=B_SPLINE_CURVE_WITH_KNOTS('',3,(#36788,#36789,#36790,#36791,#36792,
#36793,#36794,#36795,#36796,#36797,#36798,#36799,#36800,#36801,#36802,#36803,
#36804,#36805,#36806,#36807,#36808,#36809,#36810,#36811,#36812,#36813,#36814,
#36815,#36816,#36817,#36818,#36819,#36820,#36821,#36822,#36823,#36824,#36825,
#36826,#36827,#36828,#36829,#36830,#36831,#36832,#36833,#36834,#36835,#36836,
#36837,#36838,#36839,#36840,#36841,#36842,#36843,#36844,#36845,#36846,#36847,
#36848,#36849,#36850,#36851,#36852,#36853,#36854,#36855,#36856,#36857,#36858,
#36859,#36860,#36861,#36862,#36863,#36864,#36865,#36866,#36867,#36868,#36869),
 .UNSPECIFIED.,.F.,.F.,(4,3,3,3,3,3,3,3,3,3,3,3,3,3,3,3,3,3,3,3,3,3,3,3,
3,3,3,4),(72.2566310325652,72.3454126132022,72.434221928334,72.523077423167,
72.6120589945079,72.701109252016,72.7903164552464,72.8462588649391,72.934078238315,
73.0217868349393,73.1094076525767,73.2003427261945,73.2878649518309,73.3753742574496,
73.4628912948501,73.5504367163045,73.6380790811704,73.7257790090688,73.8136045421773,
73.8368882415191,73.9246814727248,74.0123709463197,74.0999775010394,74.1875219079629,
74.2750312327159,74.362520448007,74.4500269610276,74.4816274181351),
 .UNSPECIFIED.);
#2132=B_SPLINE_CURVE_WITH_KNOTS('',3,(#36870,#36871,#36872,#36873,#36874,
#36875,#36876,#36877,#36878,#36879,#36880,#36881,#36882,#36883,#36884,#36885,
#36886,#36887,#36888,#36889,#36890,#36891,#36892,#36893,#36894,#36895,#36896,
#36897,#36898,#36899,#36900,#36901,#36902,#36903,#36904,#36905,#36906,#36907,
#36908,#36909,#36910,#36911,#36912,#36913,#36914,#36915,#36916,#36917,#36918,
#36919,#36920,#36921,#36922,#36923,#36924,#36925,#36926,#36927,#36928,#36929,
#36930,#36931,#36932,#36933,#36934,#36935,#36936,#36937,#36938,#36939,#36940,
#36941,#36942,#36943,#36944,#36945,#36946,#36947,#36948,#36949,#36950,#36951,
#36952,#36953,#36954,#36955,#36956,#36957,#36958,#36959,#36960,#36961,#36962,
#36963,#36964,#36965,#36966,#36967,#36968,#36969,#36970,#36971,#36972,#36973,
#36974,#36975,#36976,#36977,#36978,#36979,#36980,#36981,#36982,#36983,#36984,
#36985,#36986,#36987,#36988,#36989,#36990,#36991,#36992,#36993,#36994,#36995,
#36996,#36997,#36998,#36999,#37000,#37001,#37002,#37003,#37004,#37005,#37006,
#37007,#37008,#37009,#37010,#37011,#37012,#37013,#37014,#37015,#37016,#37017),
 .UNSPECIFIED.,.F.,.F.,(4,3,3,3,3,3,3,3,3,3,3,3,3,3,3,3,3,3,3,3,3,3,3,3,
3,3,3,3,3,3,3,3,3,3,3,3,3,3,3,3,3,3,3,3,3,3,3,3,3,4),(68.1993401972453,
68.2868763896218,68.3743883605345,68.4618967697717,68.549422269573,68.6370391947937,
68.7247035314655,68.8125067582073,68.883741358619,68.9715591937461,69.0592662329932,
69.1468854762243,69.2378211335961,69.3253417528177,69.4128494430728,69.5003648579722,
69.5879086515959,69.675549389072,69.7632476879449,69.851071602163,69.874370735199,
69.9621887251155,70.0498959219278,70.1375153252757,70.2284509235886,70.3159717082027,
70.4034795654982,70.4909951488949,70.5785391122832,70.6661800205218,70.7538784909369,
70.8417025765127,70.8650001117791,70.9528167547558,71.0405226014255,71.1281406530599,
71.2190767574723,71.3065961950559,71.3941027093744,71.4816169552964,71.569159588166,
71.6567991828616,71.7444963480818,71.8323191506235,71.8556294883591,71.9558798743633,
72.0526975236685,72.1492455697667,72.2453959180088,72.2566310323761),
 .UNSPECIFIED.);
#2133=B_SPLINE_CURVE_WITH_KNOTS('',3,(#37023,#37024,#37025,#37026,#37027,
#37028,#37029,#37030,#37031,#37032,#37033,#37034,#37035,#37036,#37037,#37038,
#37039,#37040,#37041,#37042,#37043,#37044,#37045,#37046,#37047,#37048,#37049,
#37050,#37051,#37052,#37053,#37054,#37055,#37056,#37057,#37058,#37059,#37060,
#37061,#37062,#37063,#37064,#37065,#37066,#37067,#37068,#37069,#37070,#37071,
#37072,#37073,#37074,#37075,#37076,#37077,#37078,#37079,#37080,#37081,#37082,
#37083,#37084,#37085,#37086,#37087,#37088,#37089,#37090,#37091,#37092,#37093,
#37094,#37095,#37096,#37097,#37098,#37099,#37100,#37101,#37102,#37103,#37104,
#37105,#37106,#37107,#37108,#37109,#37110,#37111,#37112,#37113,#37114,#37115,
#37116,#37117,#37118,#37119,#37120,#37121,#37122,#37123,#37124,#37125,#37126,
#37127,#37128,#37129,#37130,#37131,#37132,#37133,#37134,#37135,#37136,#37137,
#37138,#37139,#37140,#37141,#37142,#37143,#37144,#37145,#37146,#37147,#37148,
#37149,#37150,#37151,#37152,#37153,#37154,#37155,#37156,#37157,#37158,#37159,
#37160,#37161,#37162,#37163,#37164,#37165,#37166,#37167,#37168,#37169,#37170),
 .UNSPECIFIED.,.F.,.F.,(4,3,3,3,3,3,3,3,3,3,3,3,3,3,3,3,3,3,3,3,3,3,3,3,
3,3,3,3,3,3,3,3,3,3,3,3,3,3,3,3,3,3,3,3,3,3,3,3,3,4),(61.9155759128088,
62.0030907136044,62.0906332953162,62.178272546237,62.2659688209867,62.3537913858594,
62.3796360283978,62.4674537388885,62.5551606542796,62.6427797745698,62.7337154783708,
62.8212359776857,62.9087435493546,62.9962588471121,63.083802525162,63.1714431499544,
63.2591413376945,63.346965143887,63.3702654049778,63.458083136711,63.5457900732432,
63.6334092145493,63.7243449104253,63.8118654303149,63.8993730223614,63.9868883402774,
64.0744320382452,64.1620726825017,64.2497708894643,64.3375947143806,64.3608947815578,
64.4487125432784,64.5364195101062,64.6240386819771,64.7149743664972,64.80249491742,
64.8900025406175,64.9775178897679,65.0650616190193,65.1527022944715,65.2404005326154,
65.3282243884524,65.3515241581378,65.4399938084303,65.528348931963,65.6166094524169,
65.7058185206591,65.7939460925293,65.8836959089575,65.9734457253856),
 .UNSPECIFIED.);
#2134=B_SPLINE_CURVE_WITH_KNOTS('',3,(#37171,#37172,#37173,#37174,#37175,
#37176,#37177,#37178,#37179,#37180,#37181,#37182,#37183,#37184,#37185,#37186,
#37187,#37188,#37189,#37190,#37191,#37192,#37193,#37194,#37195,#37196,#37197,
#37198,#37199,#37200,#37201,#37202,#37203,#37204,#37205,#37206,#37207,#37208,
#37209,#37210,#37211,#37212,#37213,#37214,#37215,#37216,#37217,#37218,#37219,
#37220,#37221,#37222,#37223,#37224,#37225,#37226,#37227,#37228,#37229,#37230,
#37231,#37232,#37233,#37234,#37235,#37236,#37237,#37238,#37239,#37240,#37241,
#37242,#37243,#37244,#37245,#37246,#37247,#37248,#37249),.UNSPECIFIED.,
 .F.,.F.,(4,3,3,3,3,3,3,3,3,3,3,3,3,3,3,3,3,3,3,3,3,3,3,3,3,3,4),(65.9734457255974,
66.0719666577997,66.1708766451026,66.270310369695,66.3421535347179,66.4299713696735,
66.5176784087517,66.6052976518168,66.6962333092519,66.7837539283157,66.8712616184165,
66.9587770331652,67.0463208266417,67.1339615639766,67.2216598627118,67.3094837767978,
67.3327829112979,67.4206084663604,67.5083214321086,67.5959318428673,67.6834846155375,
67.7710004509517,67.8585000180416,67.9460405103184,68.0335997133571,68.1212547539381,
68.1983639794465),.UNSPECIFIED.);
#2135=B_SPLINE_CURVE_WITH_KNOTS('',3,(#37251,#37252,#37253,#37254,#37255,
#37256,#37257,#37258,#37259,#37260,#37261,#37262,#37263,#37264,#37265,#37266,
#37267,#37268,#37269,#37270,#37271,#37272,#37273,#37274,#37275,#37276,#37277,
#37278,#37279,#37280,#37281,#37282,#37283,#37284,#37285,#37286,#37287,#37288,
#37289,#37290,#37291,#37292,#37293,#37294,#37295,#37296,#37297,#37298,#37299,
#37300,#37301,#37302,#37303,#37304,#37305,#37306,#37307,#37308,#37309,#37310,
#37311,#37312,#37313,#37314,#37315,#37316,#37317,#37318,#37319,#37320,#37321,
#37322,#37323,#37324,#37325,#37326,#37327,#37328,#37329,#37330,#37331,#37332),
 .UNSPECIFIED.,.F.,.F.,(4,3,3,3,3,3,3,3,3,3,3,3,3,3,3,3,3,3,3,3,3,3,3,3,
3,3,3,4),(65.9734457255662,66.0604573171659,66.1473630253195,66.2341866877546,
66.3209558483189,66.4076973522153,66.4944326209674,66.581183066942,66.6680217727115,
66.7549076097825,66.8419276275553,66.9024826054589,66.9903003673624,67.0780073343742,
67.1656265064294,67.2565621908806,67.3440827419878,67.4315903653695,67.5191057147038,
67.6066494441382,67.6942901197717,67.781988358096,67.8698122141105,67.893111982039,
67.9809173627593,68.0686254652694,68.1562390279435,68.1993401972453),
 .UNSPECIFIED.);
#2136=B_SPLINE_CURVE_WITH_KNOTS('',3,(#37333,#37334,#37335,#37336,#37337,
#37338,#37339,#37340,#37341,#37342,#37343,#37344,#37345,#37346,#37347,#37348,
#37349,#37350,#37351,#37352,#37353,#37354,#37355,#37356,#37357,#37358,#37359,
#37360,#37361,#37362,#37363,#37364,#37365,#37366,#37367,#37368,#37369,#37370,
#37371,#37372,#37373,#37374,#37375,#37376,#37377,#37378,#37379,#37380,#37381,
#37382,#37383,#37384,#37385,#37386,#37387,#37388,#37389,#37390,#37391,#37392,
#37393,#37394,#37395,#37396,#37397,#37398,#37399,#37400,#37401,#37402,#37403,
#37404,#37405,#37406,#37407,#37408,#37409,#37410,#37411,#37412,#37413,#37414,
#37415,#37416,#37417,#37418,#37419,#37420,#37421,#37422,#37423,#37424,#37425,
#37426,#37427,#37428,#37429,#37430,#37431,#37432,#37433,#37434,#37435,#37436,
#37437,#37438,#37439,#37440,#37441,#37442,#37443,#37444,#37445,#37446,#37447,
#37448,#37449,#37450,#37451,#37452,#37453,#37454,#37455,#37456,#37457,#37458,
#37459,#37460,#37461,#37462,#37463,#37464,#37465,#37466,#37467,#37468,#37469,
#37470,#37471,#37472,#37473,#37474,#37475,#37476,#37477,#37478,#37479,#37480,
#37481,#37482,#37483),.UNSPECIFIED.,.F.,.F.,(4,3,3,3,3,3,3,3,3,3,3,3,3,
3,3,3,3,3,3,3,3,3,3,3,3,3,3,3,3,3,3,3,3,3,3,3,3,3,3,3,3,3,3,3,3,3,3,3,3,
3,4),(61.9154863939113,61.9493357225588,62.0371534448221,62.1248603719843,
62.21247950403,62.3034152034186,62.3909357143763,62.4784432976267,62.5659586068916,
62.6535022963624,62.7411429323911,62.828841131273,62.9166649483845,62.9399650991388,
63.0277828231757,63.115489752098,63.2031088858884,63.2940445846172,63.3815650972706,
63.4690726821958,63.5565879931129,63.6441316842115,63.731772321824,63.8194705222658,
63.9072943408907,63.9305944757189,64.0184122044976,64.1061191381951,64.1937382767883,
64.2846739737272,64.3721944912207,64.4597020809913,64.5472173967536,64.6347610926922,
64.7224017351121,64.8100999403481,64.8979237637111,64.9212238522989,65.0090415627361,
65.096748478074,65.184367598311,65.275303302132,65.3628238013942,65.4503313730109,
65.5378466707163,65.6253903487142,65.7130309734558,65.8007291611456,65.8885529672889,
65.9118532288789,65.9734457253856),.UNSPECIFIED.);
#2137=B_SPLINE_CURVE_WITH_KNOTS('',3,(#37489,#37490,#37491,#37492,#37493,
#37494,#37495,#37496,#37497,#37498,#37499,#37500,#37501,#37502,#37503,#37504,
#37505,#37506,#37507,#37508,#37509,#37510,#37511,#37512,#37513,#37514,#37515,
#37516,#37517,#37518,#37519,#37520,#37521,#37522,#37523,#37524,#37525,#37526,
#37527,#37528,#37529,#37530,#37531,#37532,#37533,#37534,#37535,#37536,#37537,
#37538,#37539,#37540,#37541,#37542,#37543,#37544,#37545,#37546,#37547,#37548,
#37549,#37550,#37551,#37552,#37553,#37554,#37555,#37556,#37557,#37558,#37559,
#37560,#37561,#37562,#37563,#37564,#37565,#37566,#37567,#37568,#37569,#37570,
#37571,#37572,#37573,#37574,#37575,#37576,#37577,#37578,#37579,#37580,#37581,
#37582,#37583,#37584,#37585,#37586,#37587,#37588,#37589,#37590,#37591,#37592,
#37593,#37594,#37595,#37596,#37597,#37598,#37599,#37600,#37601,#37602,#37603,
#37604,#37605,#37606,#37607,#37608,#37609,#37610,#37611,#37612,#37613,#37614,
#37615,#37616,#37617,#37618,#37619,#37620,#37621,#37622,#37623,#37624,#37625,
#37626,#37627,#37628,#37629,#37630,#37631,#37632,#37633,#37634,#37635,#37636),
 .UNSPECIFIED.,.F.,.F.,(4,3,3,3,3,3,3,3,3,3,3,3,3,3,3,3,3,3,3,3,3,3,3,3,
3,3,3,3,3,3,3,3,3,3,3,3,3,3,3,3,3,3,3,3,3,3,3,3,3,4),(55.6330521101367,
55.7206607613694,55.8100606373129,55.8975784490138,55.9850858701811,56.0726035538017,
56.1634176075807,56.2510662065663,56.3387753439269,56.426606455157,56.4358597689176,
56.5236774924359,56.6113844208518,56.6990035541487,56.7899392530673,56.8774597652619,
56.9649673497418,57.0524826602275,57.1400263509091,57.2276669881277,57.3153651881888,
57.4031890064548,57.4264891454976,57.5143068691385,57.6020137976754,57.6896329310915,
57.7805686299647,57.8680891422732,57.9555967268649,58.0431120374601,58.1306557282489,
58.2182963655708,58.3059945657329,58.393818384096,58.4171185220777,58.5049362463856,
58.5926431755931,58.6802623096824,58.7711980083043,58.8587185212883,58.9462261065552,
59.0337414178245,59.1212851092855,59.2089257472737,59.2966239480993,59.3844477671167,
59.4077478986577,59.5162980940516,59.6233575452028,59.6902604180839),
 .UNSPECIFIED.);
#2138=B_SPLINE_CURVE_WITH_KNOTS('',3,(#37637,#37638,#37639,#37640,#37641,
#37642,#37643,#37644,#37645,#37646,#37647,#37648,#37649,#37650,#37651,#37652,
#37653,#37654,#37655,#37656,#37657,#37658,#37659,#37660,#37661,#37662,#37663,
#37664,#37665,#37666,#37667,#37668,#37669,#37670,#37671,#37672,#37673,#37674,
#37675,#37676,#37677,#37678,#37679,#37680,#37681,#37682,#37683,#37684,#37685,
#37686,#37687,#37688,#37689,#37690,#37691,#37692,#37693,#37694,#37695,#37696,
#37697,#37698,#37699,#37700,#37701,#37702,#37703,#37704,#37705,#37706,#37707,
#37708,#37709,#37710,#37711,#37712,#37713,#37714,#37715),.UNSPECIFIED.,
 .F.,.F.,(4,3,3,3,3,3,3,3,3,3,3,3,3,3,3,3,3,3,3,3,3,3,3,3,3,3,4),(59.6902604182061,
59.7787750253351,59.8656202876032,59.9524524305475,60.0392927619938,60.1290638903048,
60.2160327288235,60.3072050020306,60.3983772752377,60.4861949992756,60.5739019281986,
60.6615210619902,60.7524567607187,60.8399772733732,60.9274848582996,61.015000169218,
61.1025438603181,61.190184497932,61.2778826983752,61.3657065170016,61.3890066518177,
61.476820870378,61.5645289188598,61.6522906673471,61.739842506503,61.8277092096559,
61.9155759128088),.UNSPECIFIED.);
#2139=B_SPLINE_CURVE_WITH_KNOTS('',3,(#37717,#37718,#37719,#37720,#37721,
#37722,#37723,#37724,#37725,#37726,#37727,#37728,#37729,#37730,#37731,#37732,
#37733,#37734,#37735,#37736,#37737,#37738,#37739,#37740,#37741,#37742,#37743,
#37744,#37745,#37746,#37747,#37748,#37749,#37750,#37751,#37752,#37753,#37754,
#37755,#37756,#37757,#37758,#37759,#37760,#37761,#37762,#37763,#37764,#37765,
#37766,#37767,#37768,#37769,#37770,#37771,#37772,#37773,#37774,#37775,#37776,
#37777,#37778,#37779,#37780,#37781,#37782,#37783,#37784,#37785,#37786,#37787,
#37788,#37789,#37790,#37791,#37792,#37793,#37794,#37795),.UNSPECIFIED.,
 .F.,.F.,(4,3,3,3,3,3,3,3,3,3,3,3,3,3,3,3,3,3,3,3,3,3,3,3,3,3,4),(59.69026041843,
59.7976956857359,59.9067549033646,59.9680769693988,60.0558946930393,60.1436016215757,
60.2312207549914,60.3221564538648,60.4096769661728,60.4971845507641,60.5846998613588,
60.6722435521473,60.7598841894687,60.8475823896304,60.935406207993,60.9587063459788,
61.0465260468144,61.1342344663927,61.221854606759,61.309409240327,61.3969287920519,
61.4844339306849,61.5719453095809,61.6595334389219,61.7471595669974,61.8349150953326,
61.9154863939113),.UNSPECIFIED.);
#2140=B_SPLINE_CURVE_WITH_KNOTS('',3,(#37796,#37797,#37798,#37799,#37800,
#37801,#37802,#37803,#37804,#37805,#37806,#37807,#37808,#37809,#37810,#37811,
#37812,#37813,#37814,#37815,#37816,#37817,#37818,#37819,#37820,#37821,#37822,
#37823,#37824,#37825,#37826,#37827,#37828,#37829,#37830,#37831,#37832,#37833,
#37834,#37835,#37836,#37837,#37838,#37839,#37840,#37841,#37842,#37843,#37844,
#37845,#37846,#37847,#37848,#37849,#37850,#37851,#37852,#37853,#37854,#37855,
#37856,#37857,#37858,#37859,#37860,#37861,#37862,#37863,#37864,#37865,#37866,
#37867,#37868,#37869,#37870,#37871,#37872,#37873,#37874,#37875,#37876,#37877,
#37878,#37879,#37880,#37881,#37882,#37883,#37884,#37885,#37886,#37887,#37888,
#37889,#37890,#37891,#37892,#37893,#37894,#37895,#37896,#37897,#37898,#37899,
#37900,#37901,#37902,#37903,#37904,#37905,#37906,#37907,#37908,#37909,#37910,
#37911,#37912,#37913,#37914,#37915,#37916,#37917,#37918,#37919,#37920,#37921,
#37922,#37923,#37924,#37925,#37926,#37927,#37928,#37929,#37930,#37931,#37932,
#37933,#37934,#37935,#37936,#37937,#37938,#37939,#37940,#37941,#37942,#37943,
#37944,#37945,#37946),.UNSPECIFIED.,.F.,.F.,(4,3,3,3,3,3,3,3,3,3,3,3,3,
3,3,3,3,3,3,3,3,3,3,3,3,3,3,3,3,3,3,3,3,3,3,3,3,3,3,3,3,3,3,3,3,3,3,3,3,
3,4),(55.6321400172702,55.719683968197,55.8073249295175,55.8950235783074,
55.9828476904339,56.0055594630786,56.0933771867245,56.1810841152678,56.2687032486918,
56.3596389475627,56.4471594598825,56.5346670444869,56.6221823550959,56.7097260458995,
56.7973666832383,56.8850648834183,56.9728887018007,56.9961888396587,57.0840065633094,
57.1717134918572,57.2593326252853,57.3502683241545,57.4377888364782,57.5252964210861,
57.6128117316991,57.7003554225062,57.7879960598478,57.8756942600309,57.9635180784157,
57.9868182162387,58.0746359399782,58.1623428686151,58.2499620021326,58.3408977009683,
58.4284182133814,58.5159257980787,58.6034411087804,58.6909847996761,58.7786254371054,
58.8663236373754,58.954147455846,58.9774475928187,59.0665491959921,59.1535112710729,
59.2403929922443,59.3272158153765,59.4179769660839,59.5047630081795,59.5915521904117,
59.6783867689608,59.6902604182061),.UNSPECIFIED.);
#2141=B_SPLINE_CURVE_WITH_KNOTS('',3,(#37952,#37953,#37954,#37955,#37956,
#37957,#37958,#37959,#37960,#37961,#37962,#37963,#37964,#37965,#37966,#37967,
#37968,#37969,#37970,#37971,#37972,#37973,#37974,#37975,#37976,#37977,#37978,
#37979,#37980,#37981,#37982,#37983,#37984,#37985,#37986,#37987,#37988,#37989,
#37990,#37991,#37992,#37993,#37994,#37995,#37996,#37997,#37998,#37999,#38000,
#38001,#38002,#38003,#38004,#38005,#38006,#38007,#38008,#38009,#38010,#38011,
#38012,#38013,#38014,#38015,#38016,#38017,#38018,#38019,#38020,#38021,#38022,
#38023,#38024,#38025,#38026,#38027,#38028,#38029,#38030,#38031,#38032,#38033,
#38034,#38035,#38036,#38037,#38038,#38039,#38040,#38041,#38042,#38043,#38044,
#38045,#38046,#38047,#38048,#38049,#38050,#38051,#38052,#38053,#38054,#38055,
#38056,#38057,#38058,#38059,#38060,#38061,#38062,#38063,#38064,#38065,#38066,
#38067,#38068,#38069,#38070,#38071,#38072,#38073,#38074,#38075,#38076,#38077,
#38078,#38079,#38080,#38081,#38082,#38083,#38084,#38085,#38086,#38087,#38088,
#38089,#38090,#38091,#38092,#38093,#38094,#38095,#38096,#38097,#38098,#38099),
 .UNSPECIFIED.,.F.,.F.,(4,3,3,3,3,3,3,3,3,3,3,3,3,3,3,3,3,3,3,3,3,3,3,3,
3,3,3,3,3,3,3,3,3,3,3,3,3,3,3,3,3,3,3,3,3,3,3,3,3,4),(49.3487618639327,
49.4365675238893,49.5014541328574,49.5892718565182,49.6769787850764,49.7645979185152,
49.8555336173805,49.943054129715,50.0305617143338,50.1180770249573,50.2056207157754,
50.293261353128,50.3809595533218,50.4687833717175,50.4920835094374,50.5799012330958,
50.6676081616516,50.755227295088,50.8461629939542,50.9336835062863,51.0211910909028,
51.108706401524,51.1962500923399,51.2838907296903,51.3715889298818,51.4594127482754,
51.4827128860175,51.5705306096755,51.6582375382309,51.7458566716667,51.8367923705331,
51.9243128828646,52.0118204674806,52.0993357781011,52.1868794689165,52.2745201062663,
52.3622183064571,52.4500421248501,52.4733422625975,52.5604221705832,52.6473917778918,
52.7342748965889,52.8210968701783,52.90788700504,52.9946666870674,53.0814572896191,
53.1683305096244,53.2552470964566,53.3422944291719,53.4070751108547),
 .UNSPECIFIED.);
#2142=B_SPLINE_CURVE_WITH_KNOTS('',3,(#38100,#38101,#38102,#38103,#38104,
#38105,#38106,#38107,#38108,#38109,#38110,#38111,#38112,#38113,#38114,#38115,
#38116,#38117,#38118,#38119,#38120,#38121,#38122,#38123,#38124,#38125,#38126,
#38127,#38128,#38129,#38130,#38131,#38132,#38133,#38134,#38135,#38136,#38137,
#38138,#38139,#38140,#38141,#38142,#38143,#38144,#38145,#38146,#38147,#38148,
#38149,#38150,#38151,#38152,#38153,#38154,#38155,#38156,#38157,#38158,#38159,
#38160,#38161,#38162,#38163,#38164,#38165,#38166,#38167,#38168,#38169,#38170,
#38171,#38172,#38173,#38174,#38175,#38176,#38177,#38178,#38179,#38180,#38181,
#38182,#38183,#38184),.UNSPECIFIED.,.F.,.F.,(4,3,3,3,3,3,3,3,3,3,3,3,3,
3,3,3,3,3,3,3,3,3,3,3,3,3,3,3,4),(53.4070751110265,53.4639716391775,53.5517893628234,
53.6394962913667,53.7271154247907,53.8180511236615,53.9055716359814,53.9930792205857,
54.0805945311949,54.1681382219988,54.2557788593375,54.3434770595174,54.4313008778997,
54.4546010157575,54.5424187394083,54.6301256679563,54.7177448013847,54.8086805002538,
54.8962010125776,54.9837085971856,55.0712239077982,55.1587675986054,55.2464082359471,
55.3341064361299,55.4219302545147,55.4452303923376,55.5330632331811,55.6207748462539,
55.6330521101367),.UNSPECIFIED.);
#2143=B_SPLINE_CURVE_WITH_KNOTS('',3,(#38186,#38187,#38188,#38189,#38190,
#38191,#38192,#38193,#38194,#38195,#38196,#38197,#38198,#38199,#38200,#38201,
#38202,#38203,#38204,#38205,#38206,#38207,#38208,#38209,#38210,#38211,#38212,
#38213,#38214,#38215,#38216,#38217,#38218,#38219,#38220,#38221,#38222,#38223,
#38224,#38225,#38226,#38227,#38228,#38229,#38230,#38231,#38232,#38233,#38234,
#38235,#38236,#38237,#38238,#38239,#38240,#38241,#38242,#38243,#38244,#38245,
#38246,#38247,#38248,#38249,#38250,#38251,#38252,#38253,#38254,#38255,#38256,
#38257,#38258,#38259,#38260,#38261,#38262,#38263,#38264),.UNSPECIFIED.,
 .F.,.F.,(4,3,3,3,3,3,3,3,3,3,3,3,3,3,3,3,3,3,3,3,3,3,3,3,3,3,4),(53.4070751110265,
53.495269714547,53.5834738756981,53.6717071431048,53.760051289659,53.8484511190451,
53.9370104138986,54.0243007099186,54.1121184335766,54.1998253621318,54.287444495568,
54.3783801944343,54.4659007067658,54.5534082913818,54.6409236020025,54.7284672928177,
54.8161079301674,54.9038061303583,54.991629948751,55.0149300864986,55.1027351464041,
55.1904358985635,55.2780531741872,55.3665748849579,55.4540908007695,55.5431154090198,
55.6321400172702),.UNSPECIFIED.);
#2144=B_SPLINE_CURVE_WITH_KNOTS('',3,(#38265,#38266,#38267,#38268,#38269,
#38270,#38271,#38272,#38273,#38274,#38275,#38276,#38277,#38278,#38279,#38280,
#38281,#38282,#38283,#38284,#38285,#38286,#38287,#38288,#38289,#38290,#38291,
#38292,#38293,#38294,#38295,#38296,#38297,#38298,#38299,#38300,#38301,#38302,
#38303,#38304,#38305,#38306,#38307,#38308,#38309,#38310,#38311,#38312,#38313,
#38314,#38315,#38316,#38317,#38318,#38319,#38320,#38321,#38322,#38323,#38324,
#38325,#38326,#38327,#38328,#38329,#38330,#38331,#38332,#38333,#38334,#38335,
#38336,#38337,#38338,#38339,#38340,#38341,#38342,#38343,#38344,#38345,#38346,
#38347,#38348,#38349,#38350,#38351,#38352,#38353,#38354,#38355,#38356,#38357,
#38358,#38359,#38360,#38361,#38362,#38363,#38364,#38365,#38366,#38367,#38368,
#38369,#38370,#38371,#38372,#38373,#38374,#38375,#38376,#38377,#38378,#38379,
#38380,#38381,#38382,#38383,#38384,#38385,#38386,#38387,#38388,#38389,#38390,
#38391,#38392,#38393,#38394,#38395,#38396,#38397,#38398,#38399,#38400,#38401,
#38402,#38403,#38404,#38405,#38406,#38407,#38408,#38409),.UNSPECIFIED.,
 .F.,.F.,(4,3,3,3,3,3,3,3,3,3,3,3,3,3,3,3,3,3,3,3,3,3,3,3,3,3,3,3,3,3,3,
3,3,3,3,3,3,3,3,3,3,3,3,3,3,3,3,3,4),(49.349825366214,49.438820095887,49.5263372470124,
49.6138446768933,49.7013630383602,49.7914680796698,49.8791179279186,49.9704505657586,
50.0617832035985,50.1496009272581,50.2373078558151,50.3249269892527,50.4158626881185,
50.5033832004516,50.5908907850692,50.6784060956915,50.7659497865088,50.8535904238602,
50.9412886240528,51.0291124424473,51.0524125801785,51.140230303838,51.227937232395,
51.3155563658324,51.4064920646981,51.4940125770313,51.5815201616488,51.669035472271,
51.7565791630885,51.8442198004398,51.931918000632,52.0197418190264,52.0430419567585,
52.1308596804193,52.2185666089775,52.3061857424157,52.3971214412811,52.4846419536155,
52.5721495382344,52.6596648488578,52.7472085396758,52.8348491770283,52.9225473772215,
53.010371195617,53.0336713333386,53.132711821959,53.2314411214127,53.3295918555023,
53.4070751108162),.UNSPECIFIED.);
#2145=B_SPLINE_CURVE_WITH_KNOTS('',3,(#38415,#38416,#38417,#38418,#38419,
#38420,#38421,#38422,#38423,#38424,#38425,#38426,#38427,#38428,#38429,#38430,
#38431,#38432,#38433,#38434,#38435,#38436,#38437,#38438,#38439,#38440,#38441,
#38442,#38443,#38444,#38445,#38446,#38447,#38448,#38449,#38450,#38451,#38452,
#38453,#38454,#38455,#38456,#38457,#38458,#38459,#38460,#38461,#38462,#38463,
#38464,#38465,#38466,#38467,#38468,#38469,#38470,#38471,#38472,#38473,#38474,
#38475,#38476,#38477,#38478,#38479,#38480,#38481,#38482,#38483,#38484,#38485,
#38486,#38487,#38488,#38489,#38490,#38491,#38492,#38493,#38494,#38495,#38496,
#38497,#38498,#38499,#38500,#38501,#38502,#38503,#38504,#38505,#38506,#38507,
#38508,#38509,#38510,#38511,#38512,#38513,#38514,#38515,#38516,#38517,#38518,
#38519,#38520,#38521,#38522,#38523,#38524,#38525,#38526,#38527,#38528,#38529,
#38530,#38531,#38532,#38533,#38534,#38535,#38536,#38537,#38538,#38539,#38540,
#38541,#38542,#38543,#38544,#38545,#38546,#38547,#38548,#38549,#38550,#38551,
#38552,#38553,#38554,#38555,#38556,#38557,#38558,#38559,#38560,#38561,#38562),
 .UNSPECIFIED.,.F.,.F.,(4,3,3,3,3,3,3,3,3,3,3,3,3,3,3,3,3,3,3,3,3,3,3,3,
3,3,3,3,3,3,3,3,3,3,3,3,3,3,3,3,3,3,3,3,3,3,3,3,3,4),(43.0661023071267,
43.1536126359731,43.2411442504889,43.3287694148403,43.4164457620375,43.5042559154041,
43.5576778733773,43.6454955970373,43.7332025255947,43.8208216590325,43.9117573578981,
43.9992778702315,44.0867854548494,44.1743007654717,44.2618444562881,44.3494850936399,
44.4371832938329,44.5250071122277,44.5483072499573,44.6361249736169,44.7238319021739,
44.8114510356114,44.9023867344772,44.9899072468106,45.0774148314281,45.1649301420503,
45.2524738328671,45.3401144702187,45.4278126704115,45.515636488806,45.5389366265373,
45.6267543501971,45.7144612787543,45.8020804121921,45.8930161110578,45.9805366233911,
46.0680442080088,46.155559518631,46.2431032094478,46.3307438467994,46.4184420469919,
46.5062658653866,46.5295660031173,46.6186563250416,46.7076259258581,46.7964937259127,
46.8852637004615,46.9739759768084,47.0626512944777,47.1238898038469),
 .UNSPECIFIED.);
#2146=B_SPLINE_CURVE_WITH_KNOTS('',3,(#38563,#38564,#38565,#38566,#38567,
#38568,#38569,#38570,#38571,#38572,#38573,#38574,#38575,#38576,#38577,#38578,
#38579,#38580,#38581,#38582,#38583,#38584,#38585,#38586,#38587,#38588,#38589,
#38590,#38591,#38592,#38593,#38594,#38595,#38596,#38597,#38598,#38599,#38600,
#38601,#38602,#38603,#38604,#38605,#38606,#38607,#38608,#38609,#38610,#38611,
#38612,#38613,#38614,#38615,#38616,#38617,#38618,#38619,#38620,#38621,#38622,
#38623,#38624,#38625,#38626,#38627,#38628,#38629,#38630,#38631,#38632,#38633,
#38634,#38635,#38636,#38637,#38638,#38639,#38640,#38641),.UNSPECIFIED.,
 .F.,.F.,(4,3,3,3,3,3,3,3,3,3,3,3,3,3,3,3,3,3,3,3,3,3,3,3,3,3,4),(47.123889804041,
47.2229661979551,47.3199017158515,47.4200485477744,47.5201953796974,47.6080131033571,
47.695720031914,47.7833391653516,47.8742748642173,47.9617953765506,48.0493029611683,
48.1368182717905,48.2243619626075,48.312002599959,48.3997008001517,48.4875246185463,
48.5108247562774,48.5986518170984,48.6863658893996,48.7739762520672,48.8615284126721,
48.9490430731682,49.0365409030645,49.1240737168949,49.2116250160511,49.2992578782112,
49.3487618639327),.UNSPECIFIED.);
#2147=B_SPLINE_CURVE_WITH_KNOTS('',3,(#38643,#38644,#38645,#38646,#38647,
#38648,#38649,#38650,#38651,#38652,#38653,#38654,#38655,#38656,#38657,#38658,
#38659,#38660,#38661,#38662,#38663,#38664,#38665,#38666,#38667,#38668,#38669,
#38670,#38671,#38672,#38673,#38674,#38675,#38676,#38677,#38678,#38679,#38680,
#38681,#38682,#38683,#38684,#38685,#38686,#38687,#38688,#38689,#38690,#38691,
#38692,#38693,#38694,#38695,#38696,#38697,#38698,#38699,#38700,#38701,#38702,
#38703,#38704,#38705,#38706,#38707,#38708,#38709,#38710,#38711,#38712,#38713,
#38714,#38715,#38716,#38717,#38718,#38719,#38720,#38721,#38722,#38723,#38724),
 .UNSPECIFIED.,.F.,.F.,(4,3,3,3,3,3,3,3,3,3,3,3,3,3,3,3,3,3,3,3,3,3,3,3,
3,3,3,4),(47.1238898040779,47.2112205230627,47.2984421477902,47.3855782233591,
47.4726547355854,47.5596998923632,47.6467348498431,47.7337807519317,47.8209134726753,
47.9080890145206,47.9954065966316,48.0805244504384,48.1683421740981,48.2560491026551,
48.3436682360925,48.4346039349582,48.5221244472915,48.6096320319093,48.6971473425316,
48.7846910333487,48.8723316707002,48.960029870893,49.0478536892879,49.0711538270185,
49.1589647615704,49.2466781854555,49.3342970290918,49.349825366214),
 .UNSPECIFIED.);
#2148=B_SPLINE_CURVE_WITH_KNOTS('',3,(#38725,#38726,#38727,#38728,#38729,
#38730,#38731,#38732,#38733,#38734,#38735,#38736,#38737,#38738,#38739,#38740,
#38741,#38742,#38743,#38744,#38745,#38746,#38747,#38748,#38749,#38750,#38751,
#38752,#38753,#38754,#38755,#38756,#38757,#38758,#38759,#38760,#38761,#38762,
#38763,#38764,#38765,#38766,#38767,#38768,#38769,#38770,#38771,#38772,#38773,
#38774,#38775,#38776,#38777,#38778,#38779,#38780,#38781,#38782,#38783,#38784,
#38785,#38786,#38787,#38788,#38789,#38790,#38791,#38792,#38793,#38794,#38795,
#38796,#38797,#38798,#38799,#38800,#38801,#38802,#38803,#38804,#38805,#38806,
#38807,#38808,#38809,#38810,#38811,#38812,#38813,#38814,#38815,#38816,#38817,
#38818,#38819,#38820,#38821,#38822,#38823,#38824,#38825,#38826,#38827,#38828,
#38829,#38830,#38831,#38832,#38833,#38834,#38835,#38836,#38837,#38838,#38839,
#38840,#38841,#38842,#38843,#38844,#38845,#38846,#38847,#38848,#38849,#38850,
#38851,#38852,#38853,#38854,#38855,#38856,#38857,#38858,#38859,#38860,#38861,
#38862,#38863,#38864,#38865,#38866,#38867,#38868,#38869,#38870,#38871,#38872,
#38873,#38874,#38875),.UNSPECIFIED.,.F.,.F.,(4,3,3,3,3,3,3,3,3,3,3,3,3,
3,3,3,3,3,3,3,3,3,3,3,3,3,3,3,3,3,3,3,3,3,3,3,3,3,3,3,3,3,3,3,3,3,3,3,3,
3,4),(43.065809626773,43.1273775675383,43.215195291199,43.3029022197571,
43.3905213531958,43.4814570520611,43.5689775643955,43.6564851490144,43.7440004596378,
43.8315441504559,43.9191847878086,44.0068829880024,44.0947068063982,44.1180069441183,
44.2058246677778,44.2935315963346,44.381150729772,44.4720864286378,44.5596069409709,
44.6471145255884,44.7346298362105,44.8221735270273,44.9098141643786,44.9975123645711,
45.0853361829655,45.1086363206983,45.1964540443579,45.2841609729149,45.3717801063525,
45.4627158052182,45.5502363175514,45.637743902169,45.7252592127913,45.8128029036082,
45.9004435409597,45.9881417411522,46.0759655595468,46.0992656972784,46.1870834209383,
46.2747903494955,46.3624094829334,46.453345181799,46.5408656941325,46.6283732787504,
46.715888589373,46.8034322801902,46.8910729175419,46.9787711177347,47.0665949361295,
47.0898950738584,47.1238898038469),.UNSPECIFIED.);
#2149=B_SPLINE_CURVE_WITH_KNOTS('',3,(#38881,#38882,#38883,#38884,#38885,
#38886,#38887,#38888,#38889,#38890,#38891,#38892,#38893,#38894,#38895,#38896,
#38897,#38898,#38899,#38900,#38901,#38902,#38903,#38904,#38905,#38906,#38907,
#38908,#38909,#38910,#38911,#38912,#38913,#38914,#38915,#38916,#38917,#38918,
#38919,#38920,#38921,#38922,#38923,#38924,#38925,#38926,#38927,#38928,#38929,
#38930,#38931,#38932,#38933,#38934,#38935,#38936,#38937,#38938,#38939,#38940,
#38941,#38942,#38943,#38944,#38945,#38946,#38947,#38948,#38949,#38950,#38951,
#38952,#38953,#38954,#38955,#38956,#38957,#38958,#38959,#38960,#38961,#38962,
#38963,#38964,#38965,#38966,#38967,#38968,#38969,#38970,#38971,#38972,#38973,
#38974,#38975,#38976,#38977,#38978,#38979,#38980,#38981,#38982,#38983,#38984,
#38985,#38986,#38987,#38988,#38989,#38990,#38991,#38992,#38993,#38994,#38995,
#38996,#38997,#38998,#38999,#39000,#39001,#39002,#39003,#39004,#39005,#39006,
#39007,#39008,#39009,#39010,#39011,#39012,#39013,#39014,#39015,#39016,#39017,
#39018,#39019,#39020,#39021,#39022,#39023,#39024,#39025,#39026,#39027,#39028),
 .UNSPECIFIED.,.F.,.F.,(4,3,3,3,3,3,3,3,3,3,3,3,3,3,3,3,3,3,3,3,3,3,3,3,
3,3,3,3,3,3,3,3,3,3,3,3,3,3,3,3,3,3,3,3,3,3,3,3,3,4),(36.7834743460371,
36.8711071696441,36.9586711146396,37.0461970608729,37.1337056705273,37.2212175991222,
37.3087534995119,37.3963842651212,37.4840686289141,37.571883639047,37.6139016138971,
37.7017193375656,37.7894262661317,37.8770453995784,37.9679810984408,38.0555016107834,
38.1430091954105,38.2305245060422,38.3180681968687,38.4057088342297,38.4934070344319,
38.581230852836,38.6045309904771,38.6923487141351,38.7800556426905,38.8676747761264,
38.9586104749927,39.0461309873243,39.1336385719403,39.2211538825609,39.3086975733762,
39.396338210726,39.484036410917,39.57186022931,39.5951603670571,39.6829780907157,
39.7706850192716,39.8583041527081,39.9492398515742,40.0367603639064,40.1242679485229,
40.211783259144,40.2993269499597,40.38696758731,40.4746657875014,40.5624896058948,
40.5857897436372,40.6987530453519,40.8096059142798,40.8407044964449),
 .UNSPECIFIED.);
#2150=B_SPLINE_CURVE_WITH_KNOTS('',3,(#39029,#39030,#39031,#39032,#39033,
#39034,#39035,#39036,#39037,#39038,#39039,#39040,#39041,#39042,#39043,#39044,
#39045,#39046,#39047,#39048,#39049,#39050,#39051,#39052,#39053,#39054,#39055,
#39056,#39057,#39058,#39059,#39060,#39061,#39062,#39063,#39064,#39065,#39066,
#39067,#39068,#39069,#39070,#39071,#39072,#39073,#39074,#39075,#39076,#39077,
#39078,#39079,#39080,#39081,#39082,#39083,#39084,#39085,#39086,#39087,#39088,
#39089,#39090,#39091,#39092,#39093,#39094,#39095,#39096,#39097,#39098,#39099,
#39100,#39101,#39102,#39103,#39104,#39105,#39106,#39107,#39108,#39109,#39110),
 .UNSPECIFIED.,.F.,.F.,(4,3,3,3,3,3,3,3,3,3,3,3,3,3,3,3,3,3,3,3,3,3,3,3,
3,3,3,4),(40.8407044966673,40.9273584362595,41.0139637234755,41.1005454082163,
41.1871250286611,41.2737241172989,41.3604139263639,41.4471549251205,41.5340255171112,
41.5764191202172,41.6642368438766,41.7519437724335,41.8395629058709,41.9304986047367,
42.0180191170698,42.1055267016874,42.1930420123095,42.2805857031267,42.368226340478,
42.4559245406704,42.5437483590649,42.5670484967972,42.654865790963,42.7425763493764,
42.8301869080235,42.9177390606068,43.0052579703391,43.0661023071267),
 .UNSPECIFIED.);
#2151=B_SPLINE_CURVE_WITH_KNOTS('',3,(#39112,#39113,#39114,#39115,#39116,
#39117,#39118,#39119,#39120,#39121,#39122,#39123,#39124,#39125,#39126,#39127,
#39128,#39129,#39130,#39131,#39132,#39133,#39134,#39135,#39136,#39137,#39138,
#39139,#39140,#39141,#39142,#39143,#39144,#39145,#39146,#39147,#39148,#39149,
#39150,#39151,#39152,#39153,#39154,#39155,#39156,#39157,#39158,#39159,#39160,
#39161,#39162,#39163,#39164,#39165,#39166,#39167,#39168,#39169,#39170,#39171,
#39172,#39173,#39174,#39175,#39176,#39177,#39178,#39179,#39180,#39181,#39182,
#39183,#39184,#39185,#39186,#39187,#39188,#39189,#39190),.UNSPECIFIED.,
 .F.,.F.,(4,3,3,3,3,3,3,3,3,3,3,3,3,3,3,3,3,3,3,3,3,3,3,3,3,3,4),(40.8407044968327,
40.9448640922813,41.0502373864982,41.1461188143782,41.233936538036,41.3216434665913,
41.409262600027,41.5001982988934,41.5877188112249,41.6752263958407,41.7627417064611,
41.8502853972763,41.9379260346261,42.0256242348169,42.1134480532097,42.1367481909583,
42.2245695492947,42.3122792282294,42.3999002315174,42.4874540511525,42.5749722257416,
42.6624754241103,42.7499842991578,42.8375628974753,42.925179265463,43.012908479813,
43.065809626773),.UNSPECIFIED.);
#2152=B_SPLINE_CURVE_WITH_KNOTS('',3,(#39191,#39192,#39193,#39194,#39195,
#39196,#39197,#39198,#39199,#39200,#39201,#39202,#39203,#39204,#39205,#39206,
#39207,#39208,#39209,#39210,#39211,#39212,#39213,#39214,#39215,#39216,#39217,
#39218,#39219,#39220,#39221,#39222,#39223,#39224,#39225,#39226,#39227,#39228,
#39229,#39230,#39231,#39232,#39233,#39234,#39235,#39236,#39237,#39238,#39239,
#39240,#39241,#39242,#39243,#39244,#39245,#39246,#39247,#39248,#39249,#39250,
#39251,#39252,#39253,#39254,#39255,#39256,#39257,#39258,#39259,#39260,#39261,
#39262,#39263,#39264,#39265,#39266,#39267,#39268,#39269,#39270,#39271,#39272,
#39273,#39274,#39275,#39276,#39277,#39278,#39279,#39280,#39281,#39282,#39283,
#39284,#39285,#39286,#39287,#39288,#39289,#39290,#39291,#39292,#39293,#39294,
#39295,#39296,#39297,#39298,#39299,#39300,#39301,#39302,#39303,#39304,#39305,
#39306,#39307,#39308,#39309,#39310,#39311,#39312,#39313,#39314,#39315,#39316,
#39317,#39318,#39319,#39320,#39321,#39322,#39323,#39324,#39325,#39326,#39327,
#39328,#39329,#39330,#39331,#39332,#39333,#39334,#39335,#39336,#39337,#39338),
 .UNSPECIFIED.,.F.,.F.,(4,3,3,3,3,3,3,3,3,3,3,3,3,3,3,3,3,3,3,3,3,3,3,3,
3,3,3,3,3,3,3,3,3,3,3,3,3,3,3,3,3,3,3,3,3,3,3,3,3,4),(36.7826549295876,
36.8701876837048,36.95781435167,37.0454928643294,37.1333043100256,37.1836013080581,
37.2714190317937,37.3591259604276,37.4467450939429,37.5376807927798,37.6252013051925,
37.71270888989,37.8002242005926,37.8877678914898,37.9754085289219,38.0631067291953,
38.1509305476702,38.1742306846382,38.2620484082879,38.349755336835,38.4373744702629,
38.5283101691323,38.6158306814557,38.7033382660637,38.7908535766762,38.8783972674836,
38.9660379048257,39.0537361050092,39.1415599233948,39.1648600612182,39.2526777848656,
39.3403847134098,39.4280038468348,39.5189395457052,39.6064600580253,39.6939676426298,
39.7814829532385,39.8690266440419,39.9566672813797,40.0443654815585,40.1321892999391,
40.1554894377982,40.242885923383,40.3301773559143,40.4173849585111,40.5045298834919,
40.5916445938398,40.6787389692797,40.7658659689728,40.8407044966673),
 .UNSPECIFIED.);
#2153=B_SPLINE_CURVE_WITH_KNOTS('',3,(#39344,#39345,#39346,#39347,#39348,
#39349,#39350,#39351,#39352,#39353,#39354,#39355,#39356,#39357,#39358,#39359,
#39360,#39361,#39362,#39363,#39364,#39365,#39366,#39367,#39368,#39369,#39370,
#39371,#39372,#39373,#39374,#39375,#39376,#39377,#39378,#39379,#39380,#39381,
#39382,#39383,#39384,#39385,#39386,#39387,#39388,#39389,#39390,#39391,#39392,
#39393,#39394,#39395,#39396,#39397,#39398,#39399,#39400,#39401,#39402,#39403,
#39404,#39405,#39406,#39407,#39408,#39409,#39410,#39411,#39412,#39413,#39414,
#39415,#39416,#39417,#39418,#39419,#39420,#39421,#39422,#39423,#39424,#39425,
#39426,#39427,#39428,#39429,#39430,#39431,#39432,#39433,#39434,#39435,#39436,
#39437,#39438,#39439,#39440,#39441,#39442,#39443,#39444,#39445,#39446,#39447,
#39448,#39449,#39450,#39451,#39452,#39453,#39454,#39455,#39456,#39457,#39458,
#39459,#39460,#39461,#39462,#39463,#39464,#39465,#39466,#39467,#39468,#39469,
#39470,#39471,#39472,#39473,#39474,#39475,#39476,#39477,#39478,#39479,#39480,
#39481,#39482,#39483,#39484,#39485,#39486,#39487,#39488,#39489,#39490,#39491),
 .UNSPECIFIED.,.F.,.F.,(4,3,3,3,3,3,3,3,3,3,3,3,3,3,3,3,3,3,3,3,3,3,3,3,
3,3,3,3,3,3,3,3,3,3,3,3,3,3,3,3,3,3,3,3,3,3,3,3,3,4),(30.4991791414397,
30.5893375596383,30.6794959778369,30.7673137002237,30.8550206274869,30.9426397596114,
31.0335754589621,31.1210959699427,31.2086035531954,31.2961188624419,31.3836625518737,
31.4713031878329,31.5590013866275,31.6468252036264,31.6701253544169,31.7579430786971,
31.845650007882,31.933269141954,32.0242048405844,32.1117253535643,32.1992329388321,
32.2867482501072,32.3742919415789,32.4619325795848,32.5496307804325,32.637454599478,
32.660754730997,32.7485724546253,32.8362793831521,32.9238985165603,33.0148342154374,
33.1023547277442,33.1898623123364,33.2773776229343,33.364921313728,33.4525619510581,
33.5402601512304,33.6280839696064,33.651384107577,33.7382200973112,33.824945993001,
33.9115858335191,33.9981647381688,34.084712476298,34.1712506300881,34.2578007697322,
34.3444298640565,34.4311037988424,34.5178962961451,34.557519189277),
 .UNSPECIFIED.);
#2154=B_SPLINE_CURVE_WITH_KNOTS('',3,(#39492,#39493,#39494,#39495,#39496,
#39497,#39498,#39499,#39500,#39501,#39502,#39503,#39504,#39505,#39506,#39507,
#39508,#39509,#39510,#39511,#39512,#39513,#39514,#39515,#39516,#39517,#39518,
#39519,#39520,#39521,#39522,#39523,#39524,#39525,#39526,#39527,#39528,#39529,
#39530,#39531,#39532,#39533,#39534,#39535,#39536,#39537,#39538,#39539,#39540,
#39541,#39542,#39543,#39544,#39545,#39546,#39547,#39548,#39549,#39550,#39551,
#39552,#39553,#39554,#39555,#39556,#39557,#39558,#39559,#39560,#39561,#39562,
#39563,#39564,#39565,#39566,#39567,#39568,#39569,#39570,#39571,#39572,#39573),
 .UNSPECIFIED.,.F.,.F.,(4,3,3,3,3,3,3,3,3,3,3,3,3,3,3,3,3,3,3,3,3,3,3,3,
3,3,3,4),(34.5575191894877,34.642013484157,34.7298312078921,34.8175381365255,
34.9051572700406,34.9960929688777,35.0836134812899,35.171121065987,35.2586363766889,
35.3461800675859,35.4338207050176,35.5215189052904,35.6093427237649,35.632642860737,
35.7204605843868,35.8081675129339,35.8957866463617,35.9867223452311,36.0742428575547,
36.1617504421628,36.2492657527756,36.3368094435831,36.4244500809253,36.5121482811088,
36.5999720994945,36.6232722373171,36.7110751645256,36.7834743460371),
 .UNSPECIFIED.);
#2155=B_SPLINE_CURVE_WITH_KNOTS('',3,(#39575,#39576,#39577,#39578,#39579,
#39580,#39581,#39582,#39583,#39584,#39585,#39586,#39587,#39588,#39589,#39590,
#39591,#39592,#39593,#39594,#39595,#39596,#39597,#39598,#39599,#39600,#39601,
#39602,#39603,#39604,#39605,#39606,#39607,#39608,#39609,#39610,#39611,#39612,
#39613,#39614,#39615,#39616,#39617,#39618,#39619,#39620,#39621,#39622,#39623,
#39624,#39625,#39626,#39627,#39628,#39629,#39630,#39631,#39632,#39633,#39634,
#39635,#39636,#39637,#39638,#39639,#39640,#39641,#39642,#39643,#39644,#39645,
#39646,#39647,#39648,#39649,#39650,#39651,#39652,#39653,#39654,#39655,#39656),
 .UNSPECIFIED.,.F.,.F.,(4,3,3,3,3,3,3,3,3,3,3,3,3,3,3,3,3,3,3,3,3,3,3,3,
3,3,3,4),(34.5575191894877,34.6452189793779,34.7329127217085,34.8206207339479,
34.908363338699,34.9962128811091,35.0841246971806,35.1721722031867,35.2023425548981,
35.290160278526,35.3778672070522,35.46548634046,35.5564220393372,35.6439425516434,
35.7314501362353,35.8189654468328,35.9065091376259,35.9941497749554,36.0818479751271,
36.1696717935025,36.1929719314781,36.2807796097185,36.368482414792,36.4561011804981,
36.5436546850546,36.6311690814359,36.7186812679047,36.7826549295876),
 .UNSPECIFIED.);
#2156=B_SPLINE_CURVE_WITH_KNOTS('',3,(#39657,#39658,#39659,#39660,#39661,
#39662,#39663,#39664,#39665,#39666,#39667,#39668,#39669,#39670,#39671,#39672,
#39673,#39674,#39675,#39676,#39677,#39678,#39679,#39680,#39681,#39682,#39683,
#39684,#39685,#39686,#39687,#39688,#39689,#39690,#39691,#39692,#39693,#39694,
#39695,#39696,#39697,#39698,#39699,#39700,#39701,#39702,#39703,#39704,#39705,
#39706,#39707,#39708,#39709,#39710,#39711,#39712,#39713,#39714,#39715,#39716,
#39717,#39718,#39719,#39720,#39721,#39722,#39723,#39724,#39725,#39726,#39727,
#39728,#39729,#39730,#39731,#39732,#39733,#39734,#39735,#39736,#39737,#39738,
#39739,#39740,#39741,#39742,#39743,#39744,#39745,#39746,#39747,#39748,#39749,
#39750,#39751,#39752,#39753,#39754,#39755,#39756,#39757,#39758,#39759,#39760,
#39761,#39762,#39763,#39764,#39765,#39766,#39767,#39768,#39769,#39770,#39771,
#39772,#39773,#39774,#39775,#39776,#39777,#39778,#39779,#39780,#39781,#39782,
#39783,#39784,#39785,#39786,#39787,#39788,#39789,#39790,#39791,#39792,#39793,
#39794,#39795,#39796,#39797,#39798,#39799,#39800,#39801,#39802,#39803,#39804),
 .UNSPECIFIED.,.F.,.F.,(4,3,3,3,3,3,3,3,3,3,3,3,3,3,3,3,3,3,3,3,3,3,3,3,
3,3,3,3,3,3,3,3,3,3,3,3,3,3,3,3,3,3,3,3,3,3,3,3,3,4),(30.5002984457891,
30.5878602511594,30.6753851666878,30.7628935163061,30.8504059551847,30.9379431363765,
31.0255755534935,31.11326226172,31.2010787232516,31.239825048578,31.3276427771878,
31.4153497107485,31.5029688492368,31.5939045462269,31.6814250636965,31.7689326534729,
31.8564479692708,31.9439916652747,32.031632307804,32.119330513175,32.2071543367094,
32.230454425158,32.3182721490478,32.405979077851,32.4935982115503,32.5845339103238,
32.6720544229564,32.7595620078866,32.8470773188349,32.9346210099905,33.0222616476981,
33.1099598482573,33.1977836670317,33.221083801738,33.308901524119,33.3966084513758,
33.4842275834946,33.5751632828475,33.6626837938218,33.7501913770681,33.8377066863083,
33.9252503757335,34.0128910116863,34.1005892104745,34.1884130274668,34.211713178318,
34.3130674744917,34.4140179484278,34.5142334839426,34.5575191892806),
 .UNSPECIFIED.);
#2157=B_SPLINE_CURVE_WITH_KNOTS('',3,(#39810,#39811,#39812,#39813,#39814,
#39815,#39816,#39817,#39818,#39819,#39820,#39821,#39822,#39823,#39824,#39825,
#39826,#39827,#39828,#39829,#39830,#39831,#39832,#39833,#39834,#39835,#39836,
#39837,#39838,#39839,#39840,#39841,#39842,#39843,#39844,#39845,#39846,#39847,
#39848,#39849,#39850,#39851,#39852,#39853,#39854,#39855,#39856,#39857,#39858,
#39859,#39860,#39861,#39862,#39863,#39864,#39865,#39866,#39867,#39868,#39869,
#39870,#39871,#39872,#39873,#39874,#39875,#39876,#39877,#39878,#39879,#39880,
#39881,#39882,#39883,#39884,#39885,#39886,#39887,#39888,#39889,#39890,#39891,
#39892,#39893,#39894,#39895,#39896,#39897,#39898,#39899,#39900,#39901,#39902,
#39903,#39904,#39905,#39906,#39907,#39908,#39909,#39910,#39911,#39912,#39913,
#39914,#39915,#39916,#39917,#39918,#39919,#39920,#39921,#39922,#39923,#39924,
#39925,#39926,#39927,#39928,#39929,#39930,#39931,#39932,#39933,#39934,#39935,
#39936,#39937,#39938,#39939,#39940,#39941,#39942,#39943,#39944,#39945,#39946,
#39947,#39948,#39949,#39950,#39951,#39952,#39953,#39954,#39955,#39956,#39957),
 .UNSPECIFIED.,.F.,.F.,(4,3,3,3,3,3,3,3,3,3,3,3,3,3,3,3,3,3,3,3,3,3,3,3,
3,3,3,3,3,3,3,3,3,3,3,3,3,3,3,3,3,3,3,3,3,3,3,3,3,4),(24.2166288630184,
24.3041368733513,24.3916596764232,24.4792727029618,24.5669310750263,24.6547311942768,
24.7357197183567,24.8235373295578,24.9112441439916,24.9988631617908,25.089798903434,
25.1773192970847,25.2648267621001,25.352341952329,25.4398855220887,25.5275260380041,
25.6152241163975,25.7030478133862,25.7263490949368,25.8141668558993,25.9018738221139,
25.9894929935152,26.0804286782654,26.1679492290807,26.2554568523045,26.3429722016151,
26.4305159311601,26.5181566071029,26.6058548458523,26.6936787024586,26.7169784715168,
26.8047962016812,26.8925031369437,26.9801222772785,27.0710579736308,27.158578493298,
27.2460860853985,27.3336014036452,27.4211451022205,27.5087857474913,27.5964839557064,
27.6843077822142,27.7076078480968,27.7974230850615,27.8871096166733,27.9766849091273,
28.0661443963749,28.1555357322244,28.2448678042523,28.2743338823081),
 .UNSPECIFIED.);
#2158=B_SPLINE_CURVE_WITH_KNOTS('',3,(#39958,#39959,#39960,#39961,#39962,
#39963,#39964,#39965,#39966,#39967,#39968,#39969,#39970,#39971,#39972,#39973,
#39974,#39975,#39976,#39977,#39978,#39979,#39980,#39981,#39982,#39983,#39984,
#39985,#39986,#39987,#39988,#39989,#39990,#39991,#39992,#39993,#39994,#39995,
#39996,#39997,#39998,#39999,#40000,#40001,#40002,#40003,#40004,#40005,#40006,
#40007,#40008,#40009,#40010,#40011,#40012,#40013,#40014,#40015,#40016,#40017,
#40018,#40019,#40020,#40021,#40022,#40023,#40024,#40025,#40026,#40027,#40028,
#40029,#40030,#40031,#40032,#40033,#40034,#40035,#40036,#40037,#40038,#40039),
 .UNSPECIFIED.,.F.,.F.,(4,3,3,3,3,3,3,3,3,3,3,3,3,3,3,3,3,3,3,3,3,3,3,3,
3,3,3,4),(28.2743338824658,28.3691609855058,28.4643913559718,28.5598306988534,
28.6555713105395,28.6982372246768,28.7860549532608,28.8737618867956,28.961381025258,
29.0523167222579,29.1398372397006,29.2273448294501,29.314860145221,29.402403841198,
29.4900444837001,29.5777426890439,29.6655665125512,29.6888666012569,29.7766954671531,
29.8670059264389,29.9546146144252,30.0421651514316,30.1296782391034,30.2171745465378,
30.3047008007868,30.3922458634067,30.4798596305342,30.4991791414397),
 .UNSPECIFIED.);
#2159=B_SPLINE_CURVE_WITH_KNOTS('',3,(#40041,#40042,#40043,#40044,#40045,
#40046,#40047,#40048,#40049,#40050,#40051,#40052,#40053,#40054,#40055,#40056,
#40057,#40058,#40059,#40060,#40061,#40062,#40063,#40064,#40065,#40066,#40067,
#40068,#40069,#40070,#40071,#40072,#40073,#40074,#40075,#40076,#40077,#40078,
#40079,#40080,#40081,#40082,#40083,#40084,#40085,#40086,#40087,#40088,#40089,
#40090,#40091,#40092,#40093,#40094,#40095,#40096,#40097,#40098,#40099,#40100,
#40101,#40102,#40103,#40104,#40105,#40106,#40107,#40108,#40109,#40110,#40111,
#40112,#40113,#40114,#40115,#40116,#40117,#40118,#40119,#40120,#40121,#40122),
 .UNSPECIFIED.,.F.,.F.,(4,3,3,3,3,3,3,3,3,3,3,3,3,3,3,3,3,3,3,3,3,3,3,3,
3,3,3,4),(28.2743338824903,28.3620519963015,28.449659412066,28.5371792512195,
28.6273526317443,28.7147749198788,28.8021846604177,28.8896026158296,28.9770495494742,
29.0645934762563,29.1521957090843,29.2399222133715,29.2585662954179,29.3463840255869,
29.4340909608545,29.5217101011948,29.6126457975452,29.7001663172191,29.7876739093267,
29.8751892275808,29.9627329261642,30.0503735714435,30.1380717796675,30.225895606185,
30.2491956719979,30.3370125939443,30.4247058192211,30.5002984457891),
 .UNSPECIFIED.);
#2160=B_SPLINE_CURVE_WITH_KNOTS('',3,(#40123,#40124,#40125,#40126,#40127,
#40128,#40129,#40130,#40131,#40132,#40133,#40134,#40135,#40136,#40137,#40138,
#40139,#40140,#40141,#40142,#40143,#40144,#40145,#40146,#40147,#40148,#40149,
#40150,#40151,#40152,#40153,#40154,#40155,#40156,#40157,#40158,#40159,#40160,
#40161,#40162,#40163,#40164,#40165,#40166,#40167,#40168,#40169,#40170,#40171,
#40172,#40173,#40174,#40175,#40176,#40177,#40178,#40179,#40180,#40181,#40182,
#40183,#40184,#40185,#40186,#40187,#40188,#40189,#40190,#40191,#40192,#40193,
#40194,#40195,#40196,#40197,#40198,#40199,#40200,#40201,#40202,#40203,#40204,
#40205,#40206,#40207,#40208,#40209,#40210,#40211,#40212,#40213,#40214,#40215,
#40216,#40217,#40218,#40219,#40220,#40221,#40222,#40223,#40224,#40225,#40226,
#40227,#40228,#40229,#40230,#40231,#40232,#40233,#40234,#40235,#40236,#40237,
#40238,#40239,#40240,#40241,#40242,#40243,#40244,#40245,#40246,#40247,#40248,
#40249,#40250,#40251,#40252,#40253,#40254,#40255,#40256,#40257,#40258,#40259,
#40260,#40261,#40262,#40263,#40264,#40265,#40266,#40267,#40268,#40269,#40270,
#40271,#40272,#40273),.UNSPECIFIED.,.F.,.F.,(4,3,3,3,3,3,3,3,3,3,3,3,3,
3,3,3,3,3,3,3,3,3,3,3,3,3,3,3,3,3,3,3,3,3,3,3,3,3,3,3,3,3,3,3,3,3,3,3,3,
3,4),(24.2161577263113,24.3054194125178,24.3932361238663,24.4809420258599,
24.5685601198239,24.6594962034832,24.7470156507643,24.8345221627239,24.9220363942335,
25.0095790006303,25.0972185511234,25.1849156617613,25.2727383949358,25.2960487890978,
25.383866778914,25.471573975645,25.5591933789306,25.650128977274,25.737649761874,
25.8251576191729,25.9126732025909,26.0002171660178,26.0878580743214,26.1755565448169,
26.2633806304946,26.2866781656778,26.3744959848762,26.4622030112343,26.5498222446037,
26.6407579068105,26.7282785237727,26.8157862145775,26.9033016328351,26.9908454326265,
27.0784861804008,27.1661844919903,27.2540084223693,27.2773075422579,27.3651251530745,
27.452831967118,27.5404509845215,27.6313867263111,27.7189071195555,27.8064145841616,
27.8939297739781,27.981473343323,28.0691138588222,28.1568119367978,28.2446356333698,
28.2679369188379,28.2743338823081),.UNSPECIFIED.);
#2161=B_SPLINE_CURVE_WITH_KNOTS('',3,(#40279,#40280,#40281,#40282,#40283,
#40284,#40285,#40286,#40287,#40288,#40289,#40290,#40291,#40292,#40293,#40294,
#40295,#40296,#40297,#40298,#40299,#40300,#40301,#40302,#40303,#40304,#40305,
#40306,#40307,#40308,#40309,#40310,#40311,#40312,#40313,#40314,#40315,#40316,
#40317,#40318,#40319,#40320,#40321,#40322,#40323,#40324,#40325,#40326,#40327,
#40328,#40329,#40330,#40331,#40332,#40333,#40334,#40335,#40336,#40337,#40338,
#40339,#40340,#40341,#40342,#40343,#40344,#40345,#40346,#40347,#40348,#40349,
#40350,#40351,#40352,#40353,#40354,#40355,#40356,#40357,#40358,#40359,#40360),
 .UNSPECIFIED.,.F.,.F.,(4,3,3,3,3,3,3,3,3,3,3,3,3,3,3,3,3,3,3,3,3,3,3,3,
3,3,3,4),(15.7079632679489,15.7948132816696,15.88164133663,15.9684687059855,
16.0553166580006,16.142261568354,16.2292579918144,16.3163972482091,16.3803843998776,
16.468224529064,16.5559526601206,16.6435917732961,16.7345195236913,16.8220568152346,
16.9095799626407,16.9971095978197,17.084666352235,17.1723181077271,17.2600263044656,
17.3478583920922,17.3710137764576,17.4589553673584,17.5467936775551,17.6345493822514,
17.7222396449223,17.8098920264127,17.8975364303658,17.9331346486732),
 .UNSPECIFIED.);
#2162=B_SPLINE_CURVE_WITH_KNOTS('',3,(#40362,#40363,#40364,#40365,#40366),
 .UNSPECIFIED.,.F.,.F.,(4,1,4),(14.3991256467175,15.3897550232975,15.707955107058),
 .UNSPECIFIED.);
#2163=B_SPLINE_CURVE_WITH_KNOTS('',3,(#40370,#40371,#40372,#40373,#40374,
#40375,#40376,#40377,#40378,#40379,#40380,#40381,#40382,#40383,#40384,#40385,
#40386,#40387,#40388,#40389,#40390,#40391,#40392,#40393,#40394,#40395,#40396,
#40397,#40398,#40399,#40400,#40401,#40402,#40403,#40404,#40405,#40406,#40407,
#40408,#40409,#40410,#40411,#40412,#40413,#40414,#40415,#40416,#40417,#40418,
#40419,#40420,#40421,#40422,#40423,#40424,#40425,#40426,#40427,#40428,#40429,
#40430,#40431,#40432,#40433),.UNSPECIFIED.,.F.,.F.,(4,3,3,3,3,3,3,3,3,3,
3,3,3,3,3,3,3,3,3,3,3,4),(13.8752088702144,13.9625085938209,14.0496979618328,
14.1368005596739,14.223841740639,14.3108504907928,14.3978479980121,14.4848554371231,
14.571947709351,14.659082001847,14.7463557856079,14.8294259525565,14.9162035685692,
15.002873174162,15.0910094358584,15.1775356280929,15.2640329140993,15.3505229188245,
15.4398830060516,15.5264646980202,15.6172139828766,15.707963267733),
 .UNSPECIFIED.);
#2164=B_SPLINE_CURVE_WITH_KNOTS('',3,(#40434,#40435,#40436,#40437,#40438,
#40439,#40440,#40441,#40442,#40443,#40444,#40445,#40446,#40447,#40448,#40449,
#40450,#40451,#40452,#40453,#40454,#40455,#40456,#40457,#40458,#40459,#40460,
#40461,#40462,#40463,#40464,#40465,#40466,#40467,#40468,#40469,#40470,#40471,
#40472,#40473,#40474,#40475,#40476,#40477,#40478,#40479,#40480,#40481,#40482,
#40483,#40484,#40485,#40486,#40487,#40488,#40489,#40490,#40491,#40492,#40493,
#40494,#40495,#40496,#40497,#40498,#40499,#40500,#40501,#40502,#40503,#40504,
#40505,#40506,#40507,#40508,#40509,#40510,#40511,#40512,#40513,#40514,#40515),
 .UNSPECIFIED.,.F.,.F.,(4,3,3,3,3,3,3,3,3,3,3,3,3,3,3,3,3,3,3,3,3,3,3,3,
3,3,3,4),(15.7079632679489,15.8200553291365,15.9077986523985,15.9954302534377,
16.0829732289737,16.1739371635665,16.2613799276287,16.3488093099911,16.4362460475909,
16.5237108776269,16.6112726216378,16.6988918158899,16.7866370650151,16.8106847057165,
16.8985113353392,16.9862271381107,17.0738551030503,17.1647874754561,17.2523166530516,
17.3398328257959,17.4273566374916,17.5149087323411,17.6025575862392,17.6902639032282,
17.7780956293868,17.8013140822965,17.8891406021589,17.9338702011125),
 .UNSPECIFIED.);
#2165=B_SPLINE_CURVE_WITH_KNOTS('',3,(#40521,#40522,#40523,#40524,#40525,
#40526,#40527,#40528,#40529,#40530,#40531,#40532,#40533,#40534,#40535,#40536,
#40537,#40538,#40539,#40540,#40541,#40542,#40543,#40544,#40545,#40546,#40547,
#40548,#40549,#40550,#40551,#40552,#40553,#40554,#40555,#40556,#40557,#40558,
#40559,#40560,#40561,#40562,#40563,#40564,#40565,#40566,#40567,#40568,#40569,
#40570,#40571,#40572,#40573,#40574,#40575,#40576,#40577,#40578,#40579,#40580,
#40581,#40582,#40583,#40584,#40585,#40586,#40587,#40588,#40589,#40590,#40591,
#40592,#40593,#40594,#40595,#40596,#40597,#40598,#40599,#40600,#40601,#40602,
#40603,#40604,#40605,#40606,#40607,#40608,#40609,#40610,#40611,#40612,#40613,
#40614,#40615,#40616,#40617),.UNSPECIFIED.,.F.,.F.,(4,3,3,3,3,3,3,3,3,3,
3,3,3,3,3,3,3,3,3,3,3,3,3,3,3,3,3,3,3,3,3,3,4),(64.4958550652426,64.5877404030811,
64.6795364658092,64.7712745072369,64.862983345553,64.954686720116,65.0464083595795,
65.1382289717397,65.2301030353743,65.3221248384973,65.3815388542818,65.4728329308018,
65.5640057866637,65.6550847449215,65.7461022669468,65.8370883287862,65.928067469142,
66.0190642154069,66.1101667576848,66.2013233141153,66.292644913399,66.3721682308618,
66.4665062483791,66.5607062484631,66.6547902335657,66.7487644812764,66.842674877868,
66.936541135683,67.0303829231798,67.1242465059106,67.218119628696,67.3120590157693,
67.3627976074418),.UNSPECIFIED.);
#2166=B_SPLINE_CURVE_WITH_KNOTS('',3,(#40625,#40626,#40627,#40628,#40629,
#40630,#40631,#40632,#40633,#40634,#40635,#40636,#40637,#40638,#40639,#40640,
#40641,#40642,#40643,#40644,#40645,#40646,#40647,#40648,#40649,#40650,#40651,
#40652,#40653,#40654,#40655,#40656,#40657,#40658,#40659,#40660,#40661,#40662,
#40663,#40664,#40665,#40666,#40667,#40668,#40669,#40670,#40671,#40672,#40673,
#40674,#40675,#40676,#40677,#40678,#40679,#40680,#40681,#40682,#40683,#40684,
#40685,#40686,#40687,#40688,#40689,#40690,#40691,#40692,#40693,#40694,#40695,
#40696,#40697,#40698,#40699,#40700,#40701,#40702,#40703,#40704,#40705,#40706,
#40707,#40708,#40709,#40710,#40711,#40712,#40713,#40714,#40715,#40716,#40717,
#40718,#40719,#40720,#40721,#40722,#40723,#40724,#40725,#40726,#40727,#40728,
#40729,#40730,#40731,#40732,#40733,#40734,#40735,#40736,#40737,#40738,#40739,
#40740,#40741,#40742,#40743,#40744,#40745,#40746,#40747,#40748,#40749,#40750,
#40751,#40752,#40753,#40754,#40755,#40756,#40757,#40758,#40759,#40760,#40761,
#40762),.UNSPECIFIED.,.F.,.F.,(4,2,2,2,2,2,2,2,2,2,2,2,2,2,2,2,2,2,2,2,
2,2,2,2,2,2,2,2,2,2,2,2,2,2,2,2,2,2,2,2,2,2,2,2,2,2,2,2,2,2,2,2,2,2,2,2,
2,2,2,2,2,2,2,2,2,2,2,2,4),(-3.81690193809338,-3.80414545028679,-3.74006670025191,
-3.69143912438751,-3.67227555739686,-3.66253149013823,-3.65529778374144,
-3.64612779634758,-3.6303228501089,-3.57080907174332,-3.52674181012936,
-3.50434173804963,-3.49714682080329,-3.49240217095334,-3.48806388982645,
-3.48039696001934,-3.45481822290918,-3.39538903941858,-3.36314194761511,
-3.3406137393263,-3.33029784217486,-3.32227202401578,-3.31327616013516,
-3.2977952451329,-3.22257762170979,-3.18687473232911,-3.1669709983955,-3.16011060326152,
-3.15547992791916,-3.15052693251671,-3.1420346445659,-3.09741113398896,
-3.02265432295446,-3.00243450222272,-2.99258160859251,-2.98467194293698,
-2.97554600821613,-2.95958025925697,-2.90534583632465,-2.85485954733824,
-2.83850678214073,-2.82678223374312,-2.82118593506205,-2.81671656323342,
-2.81101396826663,-2.79881933994248,-2.73399278679964,-2.6738834699548,
-2.66033836246495,-2.65176457330894,-2.64364960445811,-2.63250047144603,
-2.60605909251575,-2.52462372080695,-2.5047252556928,-2.49120335488778,
-2.48526031934081,-2.48075981992556,-2.47531004946878,-2.46447168822773,
-2.41889546612772,-2.3786913472785,-2.33579892213381,-2.32312843674949,
-2.31473721833348,-2.30661779422243,-2.2967885560053,-2.27226928694569,
-2.25645475069973),.UNSPECIFIED.);
#2167=B_SPLINE_CURVE_WITH_KNOTS('',3,(#40768,#40769,#40770,#40771,#40772,
#40773,#40774,#40775,#40776,#40777,#40778,#40779,#40780,#40781,#40782,#40783,
#40784,#40785,#40786,#40787,#40788,#40789,#40790,#40791,#40792,#40793,#40794,
#40795,#40796,#40797,#40798,#40799,#40800,#40801,#40802,#40803,#40804,#40805,
#40806,#40807,#40808,#40809,#40810,#40811,#40812,#40813,#40814,#40815,#40816,
#40817,#40818,#40819,#40820,#40821,#40822,#40823,#40824,#40825,#40826,#40827,
#40828,#40829,#40830,#40831,#40832,#40833,#40834,#40835,#40836,#40837,#40838,
#40839,#40840,#40841,#40842,#40843,#40844,#40845,#40846,#40847,#40848,#40849,
#40850,#40851,#40852,#40853,#40854,#40855,#40856,#40857,#40858,#40859,#40860,
#40861,#40862,#40863,#40864,#40865,#40866,#40867,#40868,#40869,#40870,#40871,
#40872,#40873,#40874,#40875,#40876,#40877,#40878,#40879,#40880,#40881,#40882,
#40883,#40884,#40885,#40886,#40887,#40888,#40889,#40890,#40891,#40892,#40893,
#40894,#40895,#40896,#40897,#40898,#40899,#40900,#40901,#40902,#40903,#40904,
#40905,#40906,#40907,#40908,#40909,#40910,#40911,#40912,#40913,#40914,#40915,
#40916,#40917,#40918,#40919,#40920,#40921,#40922,#40923,#40924,#40925,#40926,
#40927,#40928,#40929,#40930,#40931,#40932,#40933,#40934,#40935,#40936,#40937,
#40938,#40939,#40940,#40941,#40942,#40943,#40944,#40945,#40946,#40947),
 .UNSPECIFIED.,.F.,.F.,(4,2,2,2,2,2,2,2,2,2,2,2,2,2,2,2,2,2,2,2,2,2,2,2,
2,2,2,2,2,2,2,2,2,2,2,2,2,2,2,2,2,2,2,2,2,2,2,2,2,2,2,2,2,2,2,2,2,2,2,2,
2,2,2,2,2,2,2,2,2,2,2,2,2,2,2,2,2,2,2,2,2,2,2,2,2,2,2,2,2,4),(-2.01531234407017,
-1.97096071078704,-1.94756117148109,-1.94012707427523,-1.93585906585756,
-1.93117861938418,-1.92401863266923,-1.90127479300297,-1.85607749715525,
-1.79539326600502,-1.77945841106368,-1.77031199891029,-1.76235999565864,
-1.75241957764504,-1.73187232048903,-1.70360323259721,-1.63827914899585,
-1.61166142695045,-1.60392394047654,-1.59912274772414,-1.59439286442838,
-1.58697925931703,-1.56155110645004,-1.50514337105469,-1.45364312936907,
-1.44026864850318,-1.43174256154302,-1.42363164322879,-1.41242264472587,
-1.38366530533075,-1.3362418665076,-1.280027888161,-1.26961727198234,-1.26419216174676,
-1.25970053465287,-1.25375564008212,-1.24017238688386,-1.22013767941578,
-1.13713900350793,-1.11179980248811,-1.10185975090524,-1.0937148900344,
-1.08536358891572,-1.07288389784815,-1.03232843341363,-0.99073421416931,
-0.940181800771379,-0.931553232076937,-0.926558103314133,-0.921941325626722,
-0.915144016305742,-0.895696934292268,-0.86127186389371,-0.784286112040376,
-0.769119060862726,-0.760213094409259,-0.752213079457205,-0.741854976089624,
-0.718911761965742,-0.685780168885447,-0.621742558040532,-0.601006840376462,
-0.593860350086747,-0.589647664390503,-0.584938237636751,-0.577545741920772,
-0.552096825450915,-0.495596634234857,-0.443744339147798,-0.430383760090047,
-0.421886454731182,-0.413818752528643,-0.402697901897264,-0.374376201577517,
-0.328113283163754,-0.270139775620982,-0.259758510931615,-0.254350155192959,
-0.249854865442335,-0.24389290665396,-0.230278661201946,-0.210200479535493,
-0.130807265518076,-0.102676346592433,-0.0912254172311799,-0.0831179788853059,
-0.0746125335939819,-0.0659661057019032,-0.0534904667728278,-0.00100289086636027),
 .UNSPECIFIED.);
#2168=B_SPLINE_CURVE_WITH_KNOTS('',3,(#40948,#40949,#40950,#40951,#40952,
#40953,#40954,#40955,#40956,#40957,#40958,#40959,#40960,#40961,#40962,#40963),
 .UNSPECIFIED.,.F.,.F.,(4,3,3,3,3,4),(64.1406906932069,64.2575061085724,
64.376659147886,64.3909094777018,64.4829383736409,64.4958550652426),
 .UNSPECIFIED.);
#2169=B_SPLINE_CURVE_WITH_KNOTS('',3,(#40964,#40965,#40966,#40967,#40968,
#40969,#40970,#40971,#40972,#40973,#40974,#40975,#40976,#40977,#40978,#40979,
#40980,#40981,#40982,#40983,#40984,#40985,#40986,#40987,#40988,#40989,#40990,
#40991,#40992,#40993,#40994,#40995,#40996,#40997,#40998,#40999,#41000,#41001,
#41002,#41003,#41004,#41005,#41006,#41007,#41008,#41009,#41010,#41011,#41012,
#41013,#41014,#41015,#41016,#41017,#41018,#41019,#41020,#41021,#41022,#41023,
#41024,#41025,#41026,#41027,#41028,#41029,#41030,#41031,#41032,#41033,#41034,
#41035,#41036,#41037,#41038,#41039,#41040,#41041,#41042,#41043,#41044,#41045,
#41046,#41047,#41048,#41049,#41050,#41051,#41052,#41053,#41054,#41055,#41056,
#41057,#41058,#41059,#41060,#41061,#41062,#41063,#41064,#41065,#41066,#41067,
#41068,#41069,#41070,#41071,#41072,#41073,#41074,#41075,#41076,#41077,#41078,
#41079,#41080,#41081,#41082,#41083,#41084,#41085,#41086,#41087,#41088,#41089,
#41090,#41091,#41092,#41093,#41094,#41095,#41096,#41097,#41098,#41099,#41100,
#41101,#41102,#41103,#41104,#41105,#41106,#41107,#41108,#41109,#41110,#41111,
#41112,#41113,#41114,#41115,#41116,#41117,#41118,#41119,#41120,#41121,#41122,
#41123,#41124,#41125,#41126,#41127,#41128,#41129,#41130,#41131,#41132,#41133,
#41134,#41135,#41136,#41137,#41138,#41139,#41140,#41141,#41142,#41143,#41144,
#41145,#41146,#41147,#41148,#41149,#41150,#41151,#41152,#41153,#41154,#41155),
 .UNSPECIFIED.,.F.,.F.,(4,2,2,2,2,2,2,2,2,2,2,2,2,2,2,2,2,2,2,2,2,2,2,2,
2,2,2,2,2,2,2,2,2,2,2,2,2,2,2,2,2,2,2,2,2,2,2,2,2,2,2,2,2,2,2,2,2,2,2,2,
2,2,2,2,2,2,2,2,2,2,2,2,2,2,2,2,2,2,2,2,2,2,2,2,2,2,2,2,2,2,2,2,2,2,2,4),
(-2.25645475069973,-2.188265448513,-2.16815843609405,-2.15453821968529,
-2.14858587548042,-2.14409225088409,-2.13866927501132,-2.12794687637382,
-2.07587180914517,-2.02572030966631,-1.99603011594337,-1.98469628771983,
-1.97656215447964,-1.96807063594224,-1.95487485215768,-1.90852023295647,
-1.89844238129165,-1.84103080710226,-1.82056959567721,-1.81345690373307,
-1.80924954920082,-1.80450052140059,-1.79701064568396,-1.77076241439251,
-1.71029880931953,-1.66349789525828,-1.65027370516261,-1.64177216833422,
-1.63363400967182,-1.62230330094654,-1.59267139016292,-1.54269769962391,
-1.4904687176247,-1.47975562867317,-1.47433213963494,-1.46983704915597,
-1.46387973493251,-1.45022757179672,-1.43005017310064,-1.34509617745399,
-1.3213205756484,-1.31161009754599,-1.303522105511,-1.29509490721011,-1.28223109408553,
-1.23658046206208,-1.22311545002981,-1.16236323575234,-1.14601326662377,
-1.13947205713935,-1.13490538025649,-1.12981840470572,-1.12074815780125,
-1.06918814745251,-0.994513787886353,-0.97921918350772,-0.970210408231548,
-0.962241540986392,-0.95209543013702,-0.930370163976092,-0.899759061955401,
-0.885554438346332,-0.823229219635458,-0.808794455182487,-0.803121969379304,
-0.798563805297194,-0.79358192782134,-0.78500582672239,-0.73552007182797,
-0.657057653698884,-0.642038768689281,-0.633170033097429,-0.625174299932297,
-0.614780909739931,-0.591576030415419,-0.557865252858062,-0.490267689536701,
-0.47307611811594,-0.466400594942164,-0.461857112838476,-0.45684337744927,
-0.448116895776467,-0.392670159420877,-0.321954874120637,-0.306301508353274,
-0.297216285368031,-0.289334882880902,-0.279349669776681,-0.258543889233515,
-0.229767793039436,-0.189691094015558,-0.14418007717786,-0.133351997982961,
-0.127908072083656,-0.123460552149581,-0.121335708249485),.UNSPECIFIED.);
#2170=B_SPLINE_CURVE_WITH_KNOTS('',3,(#41160,#41161,#41162,#41163,#41164,
#41165,#41166,#41167,#41168,#41169,#41170,#41171,#41172,#41173,#41174,#41175,
#41176,#41177,#41178,#41179,#41180,#41181,#41182,#41183,#41184,#41185,#41186,
#41187,#41188,#41189,#41190,#41191,#41192,#41193,#41194,#41195,#41196,#41197,
#41198,#41199,#41200,#41201,#41202,#41203,#41204,#41205,#41206,#41207,#41208,
#41209,#41210,#41211,#41212,#41213,#41214,#41215,#41216,#41217,#41218,#41219,
#41220,#41221,#41222,#41223,#41224,#41225,#41226,#41227,#41228,#41229,#41230,
#41231,#41232,#41233,#41234,#41235,#41236,#41237,#41238,#41239,#41240,#41241,
#41242,#41243,#41244,#41245,#41246,#41247,#41248,#41249,#41250,#41251,#41252,
#41253,#41254,#41255,#41256,#41257,#41258,#41259,#41260,#41261,#41262,#41263,
#41264,#41265,#41266,#41267,#41268,#41269,#41270,#41271,#41272,#41273,#41274,
#41275,#41276,#41277,#41278,#41279,#41280,#41281,#41282,#41283,#41284,#41285,
#41286,#41287,#41288,#41289,#41290,#41291,#41292,#41293,#41294,#41295,#41296,
#41297,#41298,#41299,#41300,#41301,#41302,#41303,#41304,#41305,#41306,#41307,
#41308,#41309,#41310,#41311,#41312,#41313,#41314,#41315,#41316,#41317,#41318,
#41319,#41320,#41321,#41322,#41323,#41324,#41325,#41326,#41327,#41328,#41329,
#41330,#41331,#41332,#41333,#41334,#41335,#41336,#41337,#41338,#41339,#41340,
#41341,#41342,#41343,#41344,#41345,#41346,#41347,#41348,#41349),
 .UNSPECIFIED.,.F.,.F.,(4,2,2,2,2,2,2,2,2,2,2,2,2,2,2,2,2,2,2,2,2,2,2,2,
2,2,2,2,2,2,2,2,2,2,2,2,2,2,2,2,2,2,2,2,2,2,2,2,2,2,2,2,2,2,2,2,2,2,2,2,
2,2,2,2,2,2,2,2,2,2,2,2,2,2,2,2,2,2,2,2,2,2,2,2,2,2,2,2,2,2,2,2,2,2,4),
(-4.15000030030656,-4.13522595040735,-4.12612224403312,-4.1181680101193,
-4.1081727281752,-4.08730727980301,-4.01243572831013,-3.96889446418885,
-3.96046012439918,-3.95550915659461,-3.95093640263236,-3.94409228744308,
-3.92570181317871,-3.86664531623664,-3.81430169542254,-3.79843147169064,
-3.78938914649105,-3.78142655973881,-3.7713372622721,-3.7499361892784,-3.67564526612205,
-3.63231580287583,-3.62388759687953,-3.61893782158866,-3.61436420297819,
-3.60751588561074,-3.58909591392204,-3.52272747619935,-3.48920904052984,
-3.4660953789852,-3.45571739364971,-3.4477241928364,-3.43884889150076,-3.42379510032387,
-3.3456744712235,-3.31168912620144,-3.29239344926946,-3.2856235084116,-3.28101845485011,
-3.27602503329004,-3.2673929348142,-3.21666315206821,-3.1749022291993,-3.13454329118665,
-3.12208179672211,-3.11373626683079,-3.10559244226796,-3.09375481510775,
-3.06254465986431,-2.98649171791725,-2.96703262970778,-2.95372748759616,
-2.94783027314582,-2.94338237337333,-2.93793840032815,-2.92711147250309,
-2.88161688398382,-2.84160215013881,-2.79846697280289,-2.78578337991619,
-2.77739355973636,-2.76928296414223,-2.75947370479395,-2.73505758917039,
-2.65099955049287,-2.6308964216389,-2.61728003269597,-2.61132989618514,
-2.6068371504258,-2.60141341958735,-2.59101648509901,-2.5344267690082,-2.48719136814472,
-2.45849700874451,-2.44729250972131,-2.43917887915967,-2.43064445830223,
-2.41724457248662,-2.36459922493143,-2.3167899239068,-2.29528969457129,
-2.28101527636916,-2.27495694014567,-2.2704550016318,-2.26510769534646,
-2.25507390069574,-2.19290508873731,-2.13594954400614,-2.11923130021793,
-2.10905678828977,-2.10108571336672,-2.09209547865436,-2.07648200164671,
-2.02609895850442,-2.01531234407017),.UNSPECIFIED.);
#2171=B_SPLINE_CURVE_WITH_KNOTS('',3,(#41351,#41352,#41353,#41354,#41355,
#41356,#41357,#41358,#41359,#41360),.UNSPECIFIED.,.F.,.F.,(4,2,2,2,4),(-0.121335708249485,
-0.117564260348161,-0.104263477214096,-0.0848110634910586,-0.000973465629640573),
 .UNSPECIFIED.);
#2172=B_SPLINE_CURVE_WITH_KNOTS('',3,(#41361,#41362,#41363,#41364,#41365,
#41366,#41367,#41368,#41369,#41370,#41371,#41372,#41373,#41374,#41375,#41376,
#41377,#41378,#41379,#41380,#41381,#41382,#41383,#41384,#41385,#41386,#41387,
#41388,#41389,#41390,#41391,#41392,#41393,#41394,#41395,#41396,#41397,#41398,
#41399,#41400,#41401,#41402,#41403,#41404,#41405,#41406,#41407,#41408,#41409,
#41410,#41411,#41412,#41413,#41414,#41415,#41416,#41417,#41418,#41419,#41420,
#41421,#41422,#41423,#41424,#41425,#41426,#41427,#41428,#41429,#41430,#41431,
#41432,#41433,#41434,#41435,#41436,#41437,#41438,#41439,#41440,#41441,#41442,
#41443,#41444,#41445,#41446,#41447,#41448,#41449,#41450,#41451,#41452,#41453,
#41454,#41455,#41456,#41457,#41458,#41459,#41460,#41461,#41462,#41463,#41464,
#41465,#41466,#41467,#41468,#41469,#41470,#41471,#41472,#41473,#41474,#41475,
#41476,#41477,#41478,#41479,#41480,#41481,#41482,#41483,#41484,#41485,#41486,
#41487,#41488,#41489,#41490,#41491,#41492,#41493,#41494,#41495,#41496,#41497,
#41498,#41499,#41500,#41501,#41502,#41503,#41504,#41505,#41506,#41507,#41508,
#41509,#41510,#41511,#41512,#41513,#41514,#41515,#41516,#41517,#41518,#41519,
#41520,#41521,#41522,#41523,#41524,#41525,#41526,#41527,#41528,#41529,#41530,
#41531,#41532,#41533,#41534,#41535,#41536,#41537,#41538,#41539,#41540,#41541,
#41542,#41543,#41544,#41545,#41546),.UNSPECIFIED.,.F.,.F.,(4,2,2,2,2,2,
2,2,2,2,2,2,2,2,2,2,2,2,2,2,2,2,2,2,2,2,2,2,2,2,2,2,2,2,2,2,2,2,2,2,2,2,
2,2,2,2,2,2,2,2,2,2,2,2,2,2,2,2,2,2,2,2,2,2,2,2,2,2,2,2,2,2,2,2,2,2,2,2,
2,2,2,2,2,2,2,2,2,2,2,2,2,2,4),(-4.27050795113119,-4.25427509224251,-4.24187184123641,
-4.23392038678693,-4.22635788692161,-4.21786888783709,-4.2046916503057,
-4.15667450537091,-4.11270201949893,-4.08562384944383,-4.07412039256904,
-4.06510399142198,-4.06002892635896,-4.0554590881063,-4.04889385528842,
-4.03238977752879,-3.97175555728779,-3.9594578584735,-3.91284132260937,
-3.89991610359644,-3.89147808861424,-3.8834006826038,-3.87372829332611,
-3.85018088847584,-3.77871234957384,-3.74995726080526,-3.73801905846285,
-3.72874440550528,-3.72361487282174,-3.71906372566782,-3.71261803819451,
-3.69689454521145,-3.63559155388604,-3.62185217026508,-3.57615591480885,
-3.56329060002804,-3.55486447135609,-3.54677901353323,-3.53707346595768,
-3.51306677924514,-3.42837831455247,-3.40822977720239,-3.39459162077917,
-3.38863782059636,-3.38414465071832,-3.37872316129739,-3.36801149609525,
-3.32462882414156,-3.28740567162125,-3.25561117235718,-3.23331213371091,
-3.22306855011089,-3.21508981602223,-3.20613910625361,-3.19072098630399,
-3.11559915966695,-3.07998223187042,-3.0601288465694,-3.05329070598799,
-3.04867293115153,-3.04370336182409,-3.03518412404142,-2.9885336060331,
-2.95121881375009,-2.91919561683897,-2.89678677364846,-2.88652468954481,
-2.87854389247775,-2.86960359737184,-2.8542365922706,-2.77865856591189,
-2.72776651118525,-2.71876113431754,-2.71368788927925,-2.70911634267098,
-2.70254397524677,-2.68599921173671,-2.61765484911533,-2.56695345195617,
-2.55379060483459,-2.54530373379731,-2.53725374869916,-2.52595409457097,
-2.49858219706786,-2.41803478742769,-2.39819670598228,-2.38470740196583,
-2.37877838414161,-2.37428671496978,-2.36884589115274,-2.35836939704919,
-2.30339600301409,-2.25596412166985),.UNSPECIFIED.);
#2173=B_SPLINE_CURVE_WITH_KNOTS('',3,(#41552,#41553,#41554,#41555,#41556,
#41557,#41558,#41559,#41560,#41561,#41562,#41563,#41564,#41565,#41566,#41567,
#41568,#41569,#41570,#41571,#41572,#41573,#41574,#41575,#41576,#41577,#41578,
#41579,#41580,#41581,#41582,#41583,#41584,#41585,#41586,#41587,#41588,#41589,
#41590,#41591,#41592,#41593,#41594,#41595,#41596,#41597,#41598,#41599,#41600,
#41601,#41602,#41603,#41604,#41605,#41606,#41607,#41608,#41609,#41610,#41611,
#41612,#41613,#41614,#41615,#41616,#41617,#41618,#41619,#41620,#41621,#41622,
#41623,#41624,#41625,#41626,#41627,#41628,#41629,#41630,#41631,#41632,#41633,
#41634,#41635,#41636,#41637,#41638,#41639,#41640,#41641,#41642,#41643,#41644,
#41645,#41646,#41647,#41648,#41649,#41650,#41651,#41652,#41653,#41654,#41655,
#41656,#41657,#41658,#41659,#41660,#41661,#41662,#41663,#41664,#41665,#41666,
#41667,#41668,#41669,#41670,#41671,#41672,#41673,#41674,#41675,#41676,#41677,
#41678,#41679,#41680,#41681,#41682,#41683,#41684,#41685,#41686,#41687,#41688,
#41689,#41690,#41691,#41692,#41693,#41694,#41695,#41696,#41697,#41698,#41699,
#41700,#41701,#41702,#41703,#41704,#41705,#41706,#41707,#41708,#41709,#41710,
#41711,#41712,#41713,#41714,#41715,#41716,#41717,#41718,#41719,#41720,#41721,
#41722,#41723,#41724,#41725,#41726,#41727,#41728,#41729),.UNSPECIFIED.,
 .F.,.F.,(4,2,2,2,2,2,2,2,2,2,2,2,2,2,2,2,2,2,2,2,2,2,2,2,2,2,2,2,2,2,2,
2,2,2,2,2,2,2,2,2,2,2,2,2,2,2,2,2,2,2,2,2,2,2,2,2,2,2,2,2,2,2,2,2,2,2,2,
2,2,2,2,2,2,2,2,2,2,2,2,2,2,2,2,2,2,2,2,2,4),(-2.01478766729567,-1.98142389693945,
-1.90135735049127,-1.88505447692978,-1.87583124846293,-1.8678881810667,
-1.85805706238154,-1.83810810408146,-1.81098734267399,-1.76932464463373,
-1.71869675514139,-1.71006912025876,-1.7050768304324,-1.70047168013875,
-1.69369987558578,-1.6743878931761,-1.64035314228899,-1.56226691515312,
-1.54720299431889,-1.53832596575697,-1.53033382050518,-1.51996091430828,
-1.49687480223465,-1.46341745743288,-1.39734061014468,-1.37868245833986,
-1.3718019831211,-1.36722274917873,-1.36228461190409,-1.35390908580366,
-1.31220651445861,-1.22724137417402,-1.21151030866746,-1.2024094486579,
-1.19453151211719,-1.18457323705081,-1.16391317723629,-1.13542029563517,
-1.09502048355667,-1.04552330017201,-1.03694835231939,-1.03196772929687,
-1.02735769767903,-1.02055649438021,-1.0009998139111,-0.966252100677531,
-0.889520172021265,-0.874289459176133,-0.865378858957684,-0.857395149079794,
-0.847087909724196,-0.824395548004203,-0.791775153128422,-0.730540570037904,
-0.706878780679631,-0.699421142699084,-0.695149448922323,-0.69047613921818,
-0.683344178148795,-0.660850803202293,-0.616563122089116,-0.554623296238921,
-0.53870543267637,-0.529564798957579,-0.521615667916473,-0.51167611442652,
-0.491120496375201,-0.462830958785143,-0.397318212727982,-0.370912933643943,
-0.363200716833005,-0.358405702039758,-0.353669053240905,-0.346229507236389,
-0.320527900062388,-0.262788045056662,-0.212936707808891,-0.199603655886079,
-0.191083975175575,-0.182964918134244,-0.171721015387564,-0.142716955262853,
-0.0645510868593842,-0.0348535160217683,-0.0269078290753282,-0.0220624077458015,
-0.0178631849065608,-0.0131574246501657,-0.000968296068967554),
 .UNSPECIFIED.);
#2174=B_SPLINE_CURVE_WITH_KNOTS('',3,(#41730,#41731,#41732,#41733,#41734,
#41735,#41736,#41737),.UNSPECIFIED.,.F.,.F.,(4,2,2,4),(-4.27065792886625,
-4.20615549532007,-4.15140004945084,-4.15000030030656),.UNSPECIFIED.);
#2175=B_SPLINE_CURVE_WITH_KNOTS('',3,(#41738,#41739,#41740,#41741,#41742,
#41743,#41744,#41745,#41746,#41747,#41748,#41749,#41750,#41751,#41752,#41753,
#41754,#41755,#41756,#41757,#41758,#41759,#41760,#41761,#41762,#41763,#41764,
#41765,#41766,#41767,#41768,#41769,#41770,#41771,#41772,#41773,#41774,#41775,
#41776,#41777,#41778,#41779,#41780,#41781,#41782,#41783,#41784,#41785,#41786,
#41787,#41788,#41789,#41790,#41791,#41792,#41793,#41794,#41795,#41796,#41797,
#41798,#41799,#41800,#41801,#41802,#41803,#41804,#41805,#41806,#41807,#41808,
#41809,#41810,#41811,#41812,#41813,#41814,#41815,#41816,#41817,#41818,#41819,
#41820,#41821,#41822,#41823,#41824,#41825,#41826,#41827,#41828,#41829,#41830,
#41831,#41832,#41833,#41834,#41835,#41836,#41837,#41838,#41839,#41840,#41841,
#41842,#41843,#41844,#41845,#41846,#41847,#41848,#41849,#41850,#41851,#41852,
#41853,#41854,#41855,#41856,#41857,#41858,#41859,#41860,#41861,#41862,#41863,
#41864,#41865,#41866,#41867,#41868,#41869,#41870,#41871,#41872,#41873,#41874,
#41875,#41876,#41877,#41878,#41879,#41880,#41881,#41882,#41883,#41884,#41885,
#41886,#41887,#41888,#41889,#41890,#41891,#41892,#41893,#41894,#41895,#41896,
#41897,#41898,#41899,#41900,#41901,#41902,#41903,#41904,#41905,#41906,#41907,
#41908,#41909,#41910,#41911,#41912,#41913,#41914,#41915,#41916,#41917,#41918,
#41919,#41920,#41921,#41922,#41923,#41924,#41925,#41926,#41927,#41928,#41929,
#41930,#41931),.UNSPECIFIED.,.F.,.F.,(4,2,2,2,2,2,2,2,2,2,2,2,2,2,2,2,2,
2,2,2,2,2,2,2,2,2,2,2,2,2,2,2,2,2,2,2,2,2,2,2,2,2,2,2,2,2,2,2,2,2,2,2,2,
2,2,2,2,2,2,2,2,2,2,2,2,2,2,2,2,2,2,2,2,2,2,2,2,2,2,2,2,2,2,2,2,2,2,2,2,
2,2,2,2,2,2,2,4),(-2.25596412166985,-2.2551379854961,-2.22608637296791,
-2.21483339454486,-2.20671065979714,-2.19818968427851,-2.18485997948021,
-2.13519491500529,-2.06932410101386,-2.05044322982937,-2.0435315989119,
-2.03894582033343,-2.03401633038426,-2.02568450100034,-1.98523838899684,
-1.8980868588721,-1.88279795745333,-1.87379068302208,-1.86582200203709,
-1.85567453631106,-1.83393945445079,-1.80330724510446,-1.78899408232026,
-1.72640696377141,-1.71227107524586,-1.7066461540982,-1.70209946070938,
-1.69709383233158,-1.68840486469955,-1.63237114707048,-1.56221973169301,
-1.54654398055015,-1.53745411601684,-1.52957353028796,-1.5195957794005,
-1.49883118563971,-1.47013551359376,-1.42996647931124,-1.38441460968031,
-1.37358379276728,-1.368139405013,-1.36369202641143,-1.35779658776674,-1.34450037687088,
-1.32505718286995,-1.2492349082855,-1.21777785050964,-1.20591201062179,
-1.19850358834704,-1.19029985459145,-1.17857926328215,-1.14570108425752,
-1.08463669812455,-1.04382719482968,-1.03537074901929,-1.03041516031307,
-1.02579118732442,-1.01891630498404,-0.998748193815775,-0.962177584793591,
-0.888682651366288,-0.873274256426061,-0.864242062250927,-0.857075087309936,
-0.847370404398088,-0.828107243776125,-0.779058623815314,-0.715933260550799,
-0.70238689527521,-0.696859539065917,-0.692290403115334,-0.687214992189357,
-0.678195560823048,-0.66668565535097,-0.639582154705785,-0.551522355782278,
-0.536256091590146,-0.527338087300591,-0.519355704225066,-0.509061387720614,
-0.486447549114657,-0.453993099161195,-0.393692380463093,-0.369003787485475,
-0.361452964589601,-0.357163310527772,-0.352506372867473,-0.345457394138663,
-0.323745255209453,-0.28220043928023,-0.216426521639242,-0.200578912559654,
-0.191453180469336,-0.183578121966971,-0.173655586895282,-0.153195701320748,
-0.121341169407626),.UNSPECIFIED.);
#2176=B_SPLINE_CURVE_WITH_KNOTS('',3,(#41936,#41937,#41938,#41939,#41940,
#41941,#41942,#41943,#41944,#41945,#41946,#41947,#41948,#41949,#41950,#41951,
#41952,#41953,#41954,#41955,#41956,#41957,#41958,#41959,#41960,#41961,#41962,
#41963,#41964,#41965,#41966,#41967,#41968,#41969,#41970,#41971,#41972,#41973,
#41974,#41975,#41976,#41977,#41978,#41979,#41980,#41981,#41982,#41983,#41984,
#41985,#41986,#41987,#41988,#41989,#41990,#41991,#41992,#41993,#41994,#41995,
#41996,#41997,#41998,#41999,#42000,#42001,#42002,#42003,#42004,#42005,#42006,
#42007,#42008,#42009,#42010,#42011,#42012,#42013,#42014,#42015,#42016,#42017,
#42018,#42019,#42020,#42021,#42022,#42023,#42024,#42025,#42026,#42027,#42028,
#42029,#42030,#42031,#42032,#42033,#42034,#42035,#42036,#42037,#42038,#42039,
#42040,#42041,#42042,#42043,#42044,#42045,#42046,#42047,#42048,#42049,#42050,
#42051,#42052,#42053,#42054,#42055,#42056,#42057,#42058,#42059,#42060,#42061,
#42062,#42063,#42064,#42065,#42066,#42067,#42068,#42069,#42070,#42071,#42072,
#42073,#42074,#42075,#42076,#42077,#42078,#42079,#42080,#42081,#42082,#42083,
#42084,#42085,#42086,#42087,#42088,#42089,#42090,#42091,#42092,#42093,#42094,
#42095,#42096,#42097,#42098,#42099,#42100,#42101,#42102,#42103,#42104,#42105,
#42106,#42107,#42108,#42109,#42110,#42111,#42112,#42113,#42114,#42115,#42116,
#42117,#42118,#42119,#42120,#42121,#42122,#42123,#42124,#42125,#42126,#42127,
#42128,#42129),.UNSPECIFIED.,.F.,.F.,(4,2,2,2,2,2,2,2,2,2,2,2,2,2,2,2,2,
2,2,2,2,2,2,2,2,2,2,2,2,2,2,2,2,2,2,2,2,2,2,2,2,2,2,2,2,2,2,2,2,2,2,2,2,
2,2,2,2,2,2,2,2,2,2,2,2,2,2,2,2,2,2,2,2,2,2,2,2,2,2,2,2,2,2,2,2,2,2,2,2,
2,2,2,2,2,2,2,4),(-4.14944962827019,-4.10272140609561,-4.08258792449977,
-4.06895732269192,-4.0630051093006,-4.0585124126523,-4.05309060779653,-4.04237586294686,
-3.99890483705526,-3.96163290205661,-3.92992911186437,-3.90767433471585,
-3.89743876646285,-3.88946148643534,-3.88050745468491,-3.86507065031023,
-3.79013679466601,-3.75442114178497,-3.7345353890308,-3.72769376701249,
-3.72307564625416,-3.71810795052731,-3.70959615865846,-3.66414295848549,
-3.60656472702333,-3.57461604067516,-3.56300244048753,-3.55481768050234,
-3.54640097371988,-3.53358120895505,-3.49276629443858,-3.42675806024391,
-3.40830696029781,-3.39549868426518,-3.38968768882651,-3.38520352012154,
-3.37966957362805,-3.3683749946506,-3.30267708708476,-3.24218935864597,
-3.2286512886369,-3.22008880150768,-3.21198980315496,-3.2008722298171,-3.17462532518238,
-3.09270988792749,-3.07276761846719,-3.05922882914262,-3.05329210381133,
-3.0488006065242,-3.04336736872438,-3.03259412001313,-2.98793890818088,
-2.94971515760834,-2.91930559132735,-2.89768210045214,-2.88755409757852,
-2.87958772172778,-2.8705693834402,-2.85522732124278,-2.78110857098009,
-2.74493162950937,-2.72489250355291,-2.71803268118483,-2.71341123853565,
-2.70844997079813,-2.69996798124049,-2.65809049066428,-2.59781035034129,
-2.56513156021299,-2.55343296377898,-2.545232876767,-2.53782014683422,-2.52783785220864,
-2.50196522337615,-2.41964289722171,-2.39966921094172,-2.3861151904895,
-2.38017578238232,-2.37568396150665,-2.37025242555052,-2.359818212147,-2.3039562408426,
-2.25627402553365,-2.22742373468864,-2.21619848866257,-2.2080813446159,
-2.19955343348292,-2.18618555700907,-2.13500995014627,-2.06315795336684,
-2.04956370438327,-2.04368051160335,-2.03918507904081,-2.03378726581433,
-2.02319470450396,-2.01478766729567),.UNSPECIFIED.);
#2177=B_SPLINE_CURVE_WITH_KNOTS('',3,(#42131,#42132,#42133,#42134,#42135,
#42136,#42137,#42138,#42139,#42140,#42141,#42142,#42143,#42144,#42145,#42146,
#42147,#42148),.UNSPECIFIED.,.F.,.F.,(4,2,2,2,2,2,2,2,4),(-0.121341169407626,
-0.0779221281061221,-0.0618078642818699,-0.0331277363369873,-0.0252541112093821,
-0.0204242081549965,-0.0162322816208417,-0.0115142974486633,-0.000968280968871609),
 .UNSPECIFIED.);
#2178=B_SPLINE_CURVE_WITH_KNOTS('',3,(#42149,#42150,#42151,#42152,#42153,
#42154,#42155,#42156,#42157,#42158,#42159,#42160,#42161,#42162,#42163,#42164,
#42165,#42166,#42167,#42168,#42169,#42170,#42171,#42172,#42173,#42174,#42175,
#42176,#42177,#42178,#42179,#42180,#42181,#42182,#42183,#42184,#42185,#42186,
#42187,#42188,#42189,#42190,#42191,#42192,#42193,#42194,#42195,#42196,#42197,
#42198,#42199,#42200,#42201,#42202,#42203,#42204,#42205,#42206,#42207,#42208,
#42209,#42210,#42211,#42212,#42213,#42214,#42215,#42216,#42217,#42218,#42219,
#42220,#42221,#42222,#42223,#42224,#42225,#42226,#42227,#42228,#42229,#42230,
#42231,#42232,#42233,#42234,#42235,#42236,#42237,#42238,#42239,#42240,#42241,
#42242,#42243,#42244,#42245,#42246,#42247,#42248,#42249,#42250,#42251,#42252,
#42253,#42254,#42255,#42256,#42257,#42258,#42259,#42260,#42261,#42262,#42263,
#42264,#42265,#42266,#42267,#42268,#42269,#42270,#42271,#42272,#42273,#42274,
#42275,#42276,#42277,#42278,#42279,#42280,#42281,#42282,#42283,#42284,#42285,
#42286,#42287,#42288,#42289,#42290,#42291,#42292,#42293,#42294,#42295,#42296,
#42297,#42298,#42299,#42300,#42301,#42302,#42303,#42304,#42305,#42306,#42307,
#42308,#42309,#42310,#42311,#42312,#42313,#42314,#42315,#42316,#42317,#42318,
#42319,#42320,#42321,#42322,#42323,#42324),.UNSPECIFIED.,.F.,.F.,(4,2,2,
2,2,2,2,2,2,2,2,2,2,2,2,2,2,2,2,2,2,2,2,2,2,2,2,2,2,2,2,2,2,2,2,2,2,2,2,
2,2,2,2,2,2,2,2,2,2,2,2,2,2,2,2,2,2,2,2,2,2,2,2,2,2,2,2,2,2,2,2,2,2,2,2,
2,2,2,2,2,2,2,2,2,2,2,2,4),(-4.27077141273018,-4.20105219826454,-4.14924389285938,
-4.13344224297557,-4.12441342514241,-4.11644815710638,-4.10633566142047,
-4.08480338250272,-3.99625327394331,-3.97584256128733,-3.96207920923777,
-3.95610438645374,-3.95160946410396,-3.94620310348259,-3.93556874363832,
-3.88185273707762,-3.83276997960473,-3.80343763128845,-3.79214828949464,
-3.78401976837386,-3.77551076219949,-3.76223801797066,-3.7142017728616,
-3.65491380183328,-3.628900991073,-3.62143313151392,-3.61668958897118,-3.61189936620572,
-3.60421327101246,-3.5779971029985,-3.51221809101799,-3.4838788400994,-3.46329761859604,
-3.45335178833144,-3.4454003311876,-3.43625997065038,-3.42035022059746,
-3.35781378604334,-3.31398312054217,-3.29161478810358,-3.28449488725363,
-3.27982313319493,-3.27554746804555,-3.26807276610443,-3.24424598363636,
-3.18310022914985,-3.15048040740447,-3.12778803788044,-3.1174791186472,
-3.10949359475921,-3.10058045609086,-3.08534392797141,-3.00867199750743,
-2.97391170144308,-2.95434863372959,-2.94754575748717,-2.94293460850252,
-2.93795287863359,-2.92937606689271,-2.8798590595513,-2.83945987944723,
-2.79681775425765,-2.78417163056702,-2.7757893350776,-2.76767342070266,
-2.75784220126321,-2.73328315891535,-2.66285743987781,-2.62096900211229,
-2.61258682758397,-2.60764673373456,-2.6030674157682,-2.59618922529461,
-2.57755375690348,-2.51139982883573,-2.47791577687259,-2.4548176091818,
-2.44444168628536,-2.43644824230045,-2.42757081793226,-2.41250872731763,
-2.33443976584731,-2.30042262870487,-2.28111540045391,-2.27434372236135,
-2.26973811384994,-2.26474479455262,-2.25633136259072),.UNSPECIFIED.);
#2179=B_SPLINE_CURVE_WITH_KNOTS('',3,(#42330,#42331,#42332,#42333,#42334,
#42335,#42336,#42337,#42338,#42339,#42340,#42341,#42342,#42343,#42344,#42345,
#42346,#42347,#42348,#42349,#42350,#42351,#42352,#42353,#42354,#42355,#42356,
#42357,#42358,#42359,#42360,#42361,#42362,#42363,#42364,#42365,#42366,#42367,
#42368,#42369,#42370,#42371,#42372,#42373,#42374,#42375,#42376,#42377,#42378,
#42379,#42380,#42381,#42382,#42383,#42384,#42385,#42386,#42387,#42388,#42389,
#42390,#42391,#42392,#42393,#42394,#42395,#42396,#42397,#42398,#42399,#42400,
#42401,#42402,#42403,#42404,#42405,#42406,#42407,#42408,#42409,#42410,#42411,
#42412,#42413,#42414,#42415,#42416,#42417,#42418,#42419,#42420,#42421,#42422,
#42423,#42424,#42425,#42426,#42427,#42428,#42429,#42430,#42431,#42432,#42433,
#42434,#42435,#42436,#42437,#42438,#42439,#42440,#42441,#42442,#42443,#42444,
#42445,#42446,#42447,#42448,#42449,#42450,#42451,#42452,#42453,#42454,#42455,
#42456,#42457,#42458,#42459,#42460,#42461,#42462,#42463,#42464,#42465,#42466,
#42467,#42468,#42469,#42470,#42471,#42472,#42473,#42474,#42475,#42476,#42477,
#42478,#42479,#42480,#42481,#42482,#42483,#42484,#42485,#42486,#42487,#42488,
#42489,#42490,#42491,#42492,#42493,#42494,#42495,#42496,#42497,#42498,#42499,
#42500,#42501,#42502,#42503,#42504,#42505,#42506,#42507,#42508,#42509),
 .UNSPECIFIED.,.F.,.F.,(4,2,2,2,2,2,2,2,2,2,2,2,2,2,2,2,2,2,2,2,2,2,2,2,
2,2,2,2,2,2,2,2,2,2,2,2,2,2,2,2,2,2,2,2,2,2,2,2,2,2,2,2,2,2,2,2,2,2,2,2,
2,2,2,2,2,2,2,2,2,2,2,2,2,2,2,2,2,2,2,2,2,2,2,2,2,2,2,2,2,4),(-2.01490391173078,
-2.00684535224932,-1.99090656987869,-1.98176017668548,-1.97380962364891,
-1.96387300794123,-1.94334180002067,-1.86792495598627,-1.82452300238471,
-1.81602166620701,-1.81105598315887,-1.80643634844941,-1.79958754143215,
-1.77964518344978,-1.74376087128699,-1.66904877564289,-1.65376009335782,
-1.64475281449409,-1.63678405031052,-1.62663637114586,-1.60490038662731,
-1.57426647920632,-1.5599476420277,-1.49734608835629,-1.48322500072579,
-1.4776024289568,-1.47305625539427,-1.46804932085783,-1.45935436473628,
-1.44838425205299,-1.42328463243156,-1.34383558802149,-1.32129581333781,
-1.31112254981907,-1.30313330385377,-1.29424076639659,-1.27910275296648,
-1.23217962721677,-1.1635671918925,-1.147320065754,-1.14079681607781,-1.13623381255421,
-1.13114051978483,-1.12203734467052,-1.07003987364534,-0.996017413151274,
-0.980660974733026,-0.971639983970414,-0.963674770547508,-0.953553013990797,
-0.931962159377523,-0.901620565065788,-0.863360154938796,-0.81870850428584,
-0.807936563039386,-0.802503883960917,-0.798012824260372,-0.792076555194154,
-0.778538659530865,-0.758595594619598,-0.676735387771622,-0.650406572167471,
-0.63928109732649,-0.631181493311016,-0.622623022395973,-0.609101340019434,
-0.549122463871583,-0.484447291352478,-0.472190648028661,-0.466478497620411,
-0.461997831358171,-0.456376405049407,-0.444614461941354,-0.428205263096451,
-0.377392401210721,-0.323901138220019,-0.308041959160418,-0.298913584026355,
-0.291038545814011,-0.281119056319411,-0.260677242259078,-0.185436394360557,
-0.141752422474655,-0.133250781584499,-0.128285605539653,-0.123667022012404,
-0.116820600046438,-0.0968914194916686,-0.0610422761434274,-0.000969899208267077),
 .UNSPECIFIED.);
#2180=B_SPLINE_CURVE_WITH_KNOTS('',3,(#42510,#42511,#42512,#42513,#42514,
#42515,#42516,#42517,#42518,#42519,#42520,#42521,#42522,#42523,#42524,#42525,
#42526,#42527),.UNSPECIFIED.,.F.,.F.,(4,2,2,2,2,2,2,2,4),(-4.27012660728948,
-4.25498622149472,-4.2431578084548,-4.2351952117576,-4.22763892455177,-4.21916450486579,
-4.20605940887692,-4.15940214927043,-4.14944962827019),.UNSPECIFIED.);
#2181=B_SPLINE_CURVE_WITH_KNOTS('',3,(#42528,#42529,#42530,#42531,#42532,
#42533,#42534,#42535,#42536,#42537,#42538,#42539,#42540,#42541,#42542,#42543,
#42544,#42545,#42546,#42547,#42548,#42549,#42550,#42551,#42552,#42553,#42554,
#42555,#42556,#42557,#42558,#42559,#42560,#42561,#42562,#42563,#42564,#42565,
#42566,#42567,#42568,#42569,#42570,#42571,#42572,#42573,#42574,#42575,#42576,
#42577,#42578,#42579,#42580,#42581,#42582,#42583,#42584,#42585,#42586,#42587,
#42588,#42589,#42590,#42591,#42592,#42593,#42594,#42595,#42596,#42597,#42598,
#42599,#42600,#42601,#42602,#42603,#42604,#42605,#42606,#42607,#42608,#42609,
#42610,#42611,#42612,#42613,#42614,#42615,#42616,#42617,#42618,#42619,#42620,
#42621,#42622,#42623,#42624,#42625,#42626,#42627,#42628,#42629,#42630,#42631,
#42632,#42633,#42634,#42635,#42636,#42637,#42638,#42639,#42640,#42641,#42642,
#42643,#42644,#42645,#42646,#42647,#42648,#42649,#42650,#42651,#42652,#42653,
#42654,#42655,#42656,#42657,#42658,#42659,#42660,#42661,#42662,#42663,#42664,
#42665,#42666,#42667,#42668,#42669,#42670,#42671,#42672,#42673,#42674,#42675,
#42676,#42677,#42678,#42679,#42680,#42681,#42682,#42683,#42684,#42685,#42686,
#42687,#42688,#42689,#42690,#42691,#42692,#42693,#42694,#42695,#42696,#42697,
#42698,#42699,#42700,#42701,#42702,#42703,#42704,#42705,#42706,#42707,#42708,
#42709,#42710,#42711,#42712,#42713,#42714,#42715),.UNSPECIFIED.,.F.,.F.,
(4,2,2,2,2,2,2,2,2,2,2,2,2,2,2,2,2,2,2,2,2,2,2,2,2,2,2,2,2,2,2,2,2,2,2,
2,2,2,2,2,2,2,2,2,2,2,2,2,2,2,2,2,2,2,2,2,2,2,2,2,2,2,2,2,2,2,2,2,2,2,2,
2,2,2,2,2,2,2,2,2,2,2,2,2,2,2,2,2,2,2,2,2,2,4),(-2.25633136259072,-2.25611420428663,
-2.205423913953,-2.16234303250262,-2.13598465614483,-2.11644008911717,-2.10668226851988,
-2.09874216096065,-2.08945881864354,-2.07239176352989,-2.05049186031272,
-1.99132974510706,-1.94804750420133,-1.93954712231086,-1.93458164623434,
-1.92996190624213,-1.92311251593076,-1.90316522735521,-1.86726606648813,
-1.79258072422572,-1.77728927043214,-1.76828139901652,-1.76031273457428,
-1.75016603562434,-1.72843573570909,-1.69781336398404,-1.68354151740539,
-1.62105706991491,-1.60680803792044,-1.60116500163194,-1.59661402246382,
-1.59161776383681,-1.58297281037486,-1.5273236251959,-1.45664432114345,
-1.44100257420494,-1.43191994530131,-1.4247585915353,-1.41512072864443,
-1.39621673224777,-1.34996760181333,-1.29253993250546,-1.27215969970025,
-1.26505610757361,-1.26084977607255,-1.25609962115271,-1.24859881512431,
-1.22219843646328,-1.16090447572383,-1.11506542301896,-1.10189672705302,
-1.09340962723013,-1.08527027217187,-1.07391304283904,-1.04404545349864,
-0.993345872906739,-0.942091550420042,-0.931425399759648,-0.926013246505853,
-0.921519720914318,-0.915554771644664,-0.901847634071452,-0.881551810127337,
-0.794815563417974,-0.771899977648793,-0.761665833410531,-0.753669663013639,
-0.74481159518382,-0.729838700391571,-0.711437220831915,-0.669050121975928,
-0.604364299781365,-0.594522156343336,-0.58921608361287,-0.585161181357674,
-0.579324383659973,-0.56636677947008,-0.547612743951881,-0.478859343724038,
-0.440657941406307,-0.42811978653128,-0.419759862084431,-0.411533850779681,
-0.399691311011088,-0.365718575283084,-0.30013634393097,-0.264835119969563,
-0.256584954392791,-0.251673787837895,-0.247024098672018,-0.24001355455095,
-0.218655483690113,-0.178302679697445,-0.121704891590291),.UNSPECIFIED.);
#2182=B_SPLINE_CURVE_WITH_KNOTS('',3,(#42720,#42721,#42722,#42723,#42724,
#42725,#42726,#42727,#42728,#42729,#42730,#42731,#42732,#42733,#42734,#42735,
#42736,#42737,#42738,#42739,#42740,#42741,#42742,#42743,#42744,#42745,#42746,
#42747,#42748,#42749,#42750,#42751,#42752,#42753,#42754,#42755,#42756,#42757,
#42758,#42759,#42760,#42761,#42762,#42763,#42764,#42765,#42766,#42767,#42768,
#42769,#42770,#42771,#42772,#42773,#42774,#42775,#42776,#42777,#42778,#42779,
#42780,#42781,#42782,#42783,#42784,#42785,#42786,#42787,#42788,#42789,#42790,
#42791,#42792,#42793,#42794,#42795,#42796,#42797,#42798,#42799,#42800,#42801,
#42802,#42803,#42804,#42805,#42806,#42807,#42808,#42809,#42810,#42811,#42812,
#42813,#42814,#42815,#42816,#42817,#42818,#42819,#42820,#42821,#42822,#42823,
#42824,#42825,#42826,#42827,#42828,#42829,#42830,#42831,#42832,#42833,#42834,
#42835,#42836,#42837,#42838,#42839,#42840,#42841,#42842,#42843,#42844,#42845,
#42846,#42847,#42848,#42849,#42850,#42851,#42852,#42853,#42854,#42855,#42856,
#42857,#42858,#42859,#42860,#42861,#42862,#42863,#42864,#42865,#42866,#42867,
#42868,#42869,#42870,#42871,#42872,#42873,#42874,#42875,#42876,#42877,#42878,
#42879,#42880,#42881,#42882,#42883,#42884,#42885,#42886,#42887,#42888,#42889,
#42890,#42891,#42892,#42893,#42894,#42895,#42896,#42897,#42898,#42899,#42900,
#42901,#42902,#42903),.UNSPECIFIED.,.F.,.F.,(4,2,2,2,2,2,2,2,2,2,2,2,2,
2,2,2,2,2,2,2,2,2,2,2,2,2,2,2,2,2,2,2,2,2,2,2,2,2,2,2,2,2,2,2,2,2,2,2,2,
2,2,2,2,2,2,2,2,2,2,2,2,2,2,2,2,2,2,2,2,2,2,2,2,2,2,2,2,2,2,2,2,2,2,2,2,
2,2,2,2,2,2,4),(-4.14974432138309,-4.14846791814416,-4.1036272995958,-4.06490612048757,
-4.02002009343704,-4.00721019973488,-3.99879533019438,-3.99070270227857,
-3.98096668996061,-3.95676135527686,-3.87233139240616,-3.85220164525164,
-3.8385725713699,-3.83262037532498,-3.82812741643513,-3.82270495771739,
-3.81231492892195,-3.75560081303903,-3.70844624827614,-3.67978042381591,
-3.66857943454785,-3.66046607618611,-3.65192989614318,-3.63852280614711,
-3.58554570844267,-3.53810888423012,-3.51659395565881,-3.5023126293188,
-3.49625301678665,-3.49179090280551,-3.48646252704252,-3.47651771098314,
-3.40002224132401,-3.35174657283295,-3.33641956993802,-3.32748836299764,
-3.31950735118771,-3.3092333136485,-3.28674614761279,-3.19948611351233,
-3.17916142907747,-3.16543945796852,-3.15947192283691,-3.15497800549799,
-3.14956737735978,-3.13890959644952,-3.08732629807925,-3.03780055198441,
-3.01704952850813,-3.00065677860689,-2.9915085673212,-2.98355858826363,
-2.97362552027617,-2.95311262981357,-2.87784506758503,-2.83415859324948,
-2.82571944116168,-2.82076723188937,-2.81619466980269,-2.80935277403457,
-2.79098031407557,-2.73190392937765,-2.6749448647585,-2.66151274274947,
-2.65297151067771,-2.64486094521406,-2.63367614088364,-2.60689082964362,
-2.5255895245627,-2.50569357709456,-2.49217677593529,-2.48624347676095,
-2.4817519106473,-2.47631532209191,-2.46585759553819,-2.41047929418916,
-2.36248768990101,-2.33352931465428,-2.32228939467599,-2.31416948994504,
-2.30564563992768,-2.29229898705041,-2.24199412460632,-2.18466667900874,
-2.15904915059887,-2.15161610823454,-2.14688006467059,-2.1426626170076,
-2.13549867704365,-2.11270638785466,-2.06733228386177,-2.01490391173078),
 .UNSPECIFIED.);
#2183=B_SPLINE_CURVE_WITH_KNOTS('',3,(#42905,#42906,#42907,#42908,#42909,
#42910,#42911,#42912,#42913,#42914,#42915,#42916,#42917,#42918,#42919,#42920,
#42921,#42922),.UNSPECIFIED.,.F.,.F.,(4,2,2,2,2,2,2,2,4),(-0.121704891590291,
-0.11342614004661,-0.0976371836018917,-0.0877231932451925,-0.0797752166259034,
-0.0706147557324629,-0.0609728232183739,-0.0409692035001258,-0.000968868351203119),
 .UNSPECIFIED.);
#2184=B_SPLINE_CURVE_WITH_KNOTS('',3,(#42923,#42924,#42925,#42926,#42927,
#42928,#42929,#42930,#42931,#42932,#42933,#42934,#42935,#42936,#42937,#42938,
#42939,#42940,#42941,#42942,#42943,#42944,#42945,#42946,#42947,#42948,#42949,
#42950,#42951,#42952,#42953,#42954,#42955,#42956,#42957,#42958,#42959,#42960,
#42961,#42962,#42963,#42964,#42965,#42966,#42967,#42968,#42969,#42970,#42971,
#42972,#42973,#42974,#42975,#42976,#42977,#42978,#42979,#42980,#42981,#42982,
#42983,#42984,#42985,#42986,#42987,#42988,#42989,#42990,#42991,#42992,#42993,
#42994,#42995,#42996,#42997,#42998,#42999,#43000,#43001,#43002,#43003,#43004,
#43005,#43006,#43007,#43008,#43009,#43010,#43011,#43012,#43013,#43014,#43015,
#43016,#43017,#43018,#43019,#43020,#43021,#43022,#43023,#43024,#43025,#43026,
#43027,#43028,#43029,#43030,#43031,#43032,#43033,#43034,#43035,#43036,#43037,
#43038,#43039,#43040,#43041,#43042,#43043,#43044,#43045,#43046,#43047,#43048,
#43049,#43050,#43051,#43052,#43053,#43054,#43055,#43056,#43057,#43058,#43059,
#43060,#43061,#43062,#43063,#43064,#43065,#43066,#43067,#43068,#43069,#43070,
#43071,#43072,#43073,#43074,#43075,#43076,#43077,#43078,#43079,#43080,#43081,
#43082,#43083,#43084,#43085,#43086,#43087,#43088,#43089,#43090,#43091,#43092,
#43093,#43094,#43095,#43096,#43097,#43098,#43099,#43100),.UNSPECIFIED.,
 .F.,.F.,(4,2,2,2,2,2,2,2,2,2,2,2,2,2,2,2,2,2,2,2,2,2,2,2,2,2,2,2,2,2,2,
2,2,2,2,2,2,2,2,2,2,2,2,2,2,2,2,2,2,2,2,2,2,2,2,2,2,2,2,2,2,2,2,2,2,2,2,
2,2,2,2,2,2,2,2,2,2,2,2,2,2,2,2,2,2,2,2,2,4),(-4.27047542831303,-4.2028023511958,
-4.19484108710681,-4.1880475844779,-4.18343780883772,-4.17845196673257,
-4.16985735720432,-4.11993171814948,-4.06570981841995,-4.04470792430685,
-4.02816651065322,-4.01898762311436,-4.01103937520636,-4.00114554164588,
-3.9808561284274,-3.89058365570733,-3.87006317533269,-3.85624731979524,
-3.85026343488629,-3.84576741756672,-3.84036672789001,-3.82976259748566,
-3.77483604142693,-3.72654571371871,-3.69748263550418,-3.68622794122822,
-3.67810474517564,-3.66958397342759,-3.65625605077966,-3.60666091536594,
-3.54871575368378,-3.52297016480168,-3.51552516790668,-3.51078619120127,
-3.50656998205983,-3.49941491668109,-3.47861923074858,-3.41460643206202,
-3.38148303174929,-3.35855263437229,-3.34820363271455,-3.34021273237256,
-3.33131969027148,-3.31618422149891,-3.23867249433833,-3.20435376611551,
-3.18494143175752,-3.1781564394202,-3.17354813118027,-3.16855903212778,
-3.1599495016037,-3.10970432333238,-3.06868702967458,-3.02723215719761,
-3.01467854240712,-3.00631391868362,-2.99818297232946,-2.98829361080563,
-2.96335366835513,-2.87994817748842,-2.8598910227536,-2.84629619300653,
-2.84034924079151,-2.83585611403274,-2.8304283907749,-2.82001532402029,
-2.76369406971441,-2.71628420232577,-2.68752692754953,-2.67631270100351,
-2.66819625783259,-2.65966261957234,-2.64627192651873,-2.59416504461488,
-2.54574443551906,-2.52426462729073,-2.50999897537829,-2.50394137708579,
-2.49943884997888,-2.49408948254307,-2.48404809314821,-2.40804882580328,
-2.37293413781144,-2.34908870617247,-2.3385919604751,-2.33058339815916,
-2.32176676297337,-2.30700060463983,-2.25618542829049),.UNSPECIFIED.);
#2185=B_SPLINE_CURVE_WITH_KNOTS('',3,(#43106,#43107,#43108,#43109,#43110,
#43111,#43112,#43113,#43114,#43115,#43116,#43117,#43118,#43119,#43120,#43121,
#43122,#43123,#43124,#43125,#43126,#43127,#43128,#43129,#43130,#43131,#43132,
#43133,#43134,#43135,#43136,#43137,#43138,#43139,#43140,#43141,#43142,#43143,
#43144,#43145,#43146,#43147,#43148,#43149,#43150,#43151,#43152,#43153,#43154,
#43155,#43156,#43157,#43158,#43159,#43160,#43161,#43162,#43163,#43164,#43165,
#43166,#43167,#43168,#43169,#43170,#43171,#43172,#43173,#43174,#43175,#43176,
#43177,#43178,#43179,#43180,#43181,#43182,#43183,#43184,#43185,#43186,#43187,
#43188,#43189,#43190,#43191,#43192,#43193,#43194,#43195,#43196,#43197,#43198,
#43199,#43200,#43201,#43202,#43203,#43204,#43205,#43206,#43207,#43208,#43209,
#43210,#43211,#43212,#43213,#43214,#43215,#43216,#43217,#43218,#43219,#43220,
#43221,#43222,#43223,#43224,#43225,#43226,#43227,#43228,#43229,#43230,#43231,
#43232,#43233,#43234,#43235,#43236,#43237,#43238,#43239,#43240,#43241,#43242,
#43243,#43244,#43245,#43246,#43247,#43248,#43249,#43250,#43251,#43252,#43253,
#43254,#43255,#43256,#43257,#43258,#43259,#43260,#43261,#43262,#43263,#43264,
#43265,#43266,#43267,#43268,#43269,#43270,#43271,#43272,#43273,#43274,#43275,
#43276,#43277,#43278,#43279,#43280,#43281,#43282,#43283,#43284,#43285),
 .UNSPECIFIED.,.F.,.F.,(4,2,2,2,2,2,2,2,2,2,2,2,2,2,2,2,2,2,2,2,2,2,2,2,
2,2,2,2,2,2,2,2,2,2,2,2,2,2,2,2,2,2,2,2,2,2,2,2,2,2,2,2,2,2,2,2,2,2,2,2,
2,2,2,2,2,2,2,2,2,2,2,2,2,2,2,2,2,2,2,2,2,2,2,2,2,2,2,2,2,4),(-2.01554578796151,
-1.97103123005403,-1.93097181759248,-1.92253513746472,-1.91758303054684,
-1.9129553724187,-1.90606508035253,-1.88577498368381,-1.84883727333426,
-1.77593475546572,-1.76046564052153,-1.75141901115537,-1.74425187666022,
-1.73456174434985,-1.71538463815053,-1.66594597785084,-1.60238378534787,
-1.58894412989728,-1.58308620274509,-1.57859231117078,-1.57317410730551,
-1.56248042901183,-1.51978089673919,-1.43700366905451,-1.42258772503365,
-1.41384341047713,-1.40581415108061,-1.39516198893724,-1.37032201041875,
-1.33295478886762,-1.27558186874864,-1.25512205871348,-1.24800824509256,
-1.24379977332218,-1.23905147948378,-1.23156093796387,-1.20528740017942,
-1.14467072668409,-1.09807316746509,-1.0848632965148,-1.07636721830375,
-1.06823170834232,-1.05690056197673,-1.02724233745582,-0.977184103456037,
-0.925077313692892,-0.914361436720255,-0.908939171293729,-0.904446196472628,
-0.898493654406605,-0.884862827502424,-0.864727554532776,-0.780313496705148,
-0.756139403078319,-0.746367819413911,-0.738266688958129,-0.729864493060608,
-0.717117419951956,-0.673105607219358,-0.633796923416527,-0.588642416944584,
-0.577838773629542,-0.572399576055189,-0.567908660094148,-0.561979783383725,
-0.548487716707292,-0.528640596521868,-0.448026995938828,-0.420686381152166,
-0.409393112258311,-0.401345376190143,-0.392858894504195,-0.379692361252308,
-0.328859248556321,-0.259893106967106,-0.243977875884682,-0.237505865760107,
-0.232951017645036,-0.22783466941652,-0.218621332049285,-0.206785395676726,
-0.165911353814076,-0.0971919190351272,-0.0808855130853292,-0.0708260347570257,
-0.0628665444576238,-0.0553961706292034,-0.0464698457397591,-0.0292329749492484,
-0.000968449818818451),.UNSPECIFIED.);
#2186=B_SPLINE_CURVE_WITH_KNOTS('',3,(#43286,#43287,#43288,#43289,#43290,
#43291,#43292,#43293,#43294,#43295,#43296,#43297,#43298,#43299,#43300,#43301),
 .UNSPECIFIED.,.F.,.F.,(4,2,2,2,2,2,2,4),(-4.26995744812625,-4.20854418514327,
-4.18863575523228,-4.17511314825444,-4.16917905860353,-4.16468764681411,
-4.15925216914881,-4.14974432138309),.UNSPECIFIED.);
#2187=B_SPLINE_CURVE_WITH_KNOTS('',3,(#43302,#43303,#43304,#43305,#43306,
#43307,#43308,#43309,#43310,#43311,#43312,#43313,#43314,#43315,#43316,#43317,
#43318,#43319,#43320,#43321,#43322,#43323,#43324,#43325,#43326,#43327,#43328,
#43329,#43330,#43331,#43332,#43333,#43334,#43335,#43336,#43337,#43338,#43339,
#43340,#43341,#43342,#43343,#43344,#43345,#43346,#43347,#43348,#43349,#43350,
#43351,#43352,#43353,#43354,#43355,#43356,#43357,#43358,#43359,#43360,#43361,
#43362,#43363,#43364,#43365,#43366,#43367,#43368,#43369,#43370,#43371,#43372,
#43373,#43374,#43375,#43376,#43377,#43378,#43379,#43380,#43381,#43382,#43383,
#43384,#43385,#43386,#43387,#43388,#43389,#43390,#43391,#43392,#43393,#43394,
#43395,#43396,#43397,#43398,#43399,#43400,#43401,#43402,#43403,#43404,#43405,
#43406,#43407,#43408,#43409,#43410,#43411,#43412,#43413,#43414,#43415,#43416,
#43417,#43418,#43419,#43420,#43421,#43422,#43423,#43424,#43425,#43426,#43427,
#43428,#43429,#43430,#43431,#43432,#43433,#43434,#43435,#43436,#43437,#43438,
#43439,#43440,#43441,#43442,#43443,#43444,#43445,#43446,#43447,#43448,#43449,
#43450,#43451,#43452,#43453,#43454,#43455,#43456,#43457,#43458,#43459,#43460,
#43461,#43462,#43463,#43464,#43465,#43466,#43467,#43468,#43469,#43470,#43471,
#43472,#43473,#43474,#43475,#43476,#43477,#43478,#43479,#43480,#43481,#43482,
#43483,#43484,#43485,#43486,#43487,#43488,#43489,#43490,#43491,#43492,#43493,
#43494,#43495),.UNSPECIFIED.,.F.,.F.,(4,2,2,2,2,2,2,2,2,2,2,2,2,2,2,2,2,
2,2,2,2,2,2,2,2,2,2,2,2,2,2,2,2,2,2,2,2,2,2,2,2,2,2,2,2,2,2,2,2,2,2,2,2,
2,2,2,2,2,2,2,2,2,2,2,2,2,2,2,2,2,2,2,2,2,2,2,2,2,2,2,2,2,2,2,2,2,2,2,2,
2,2,2,2,2,2,2,4),(-2.25618542829049,-2.22672059863037,-2.17859210143867,
-2.17004222970896,-2.1650659111468,-2.16050470499341,-2.1537283333742,-2.13582650511268,
-2.10482854960935,-2.02452735676493,-2.00839162929354,-1.99920282934488,
-1.99125547618372,-1.98137508075322,-1.96116015673039,-1.88631530576674,
-1.84185274236897,-1.83334533127237,-1.82837806589094,-1.82375862046547,
-1.81691246100755,-1.79699563439922,-1.76118995674109,-1.68632661276455,
-1.67087182616814,-1.66191321567541,-1.65393533907042,-1.64370383577268,
-1.62147822395032,-1.58984011650555,-1.55252263692881,-1.50903851142576,
-1.49832301054929,-1.49290059266807,-1.48840728803549,-1.48245404131109,
-1.46882050516715,-1.44868013474766,-1.36420813090703,-1.33999353643743,
-1.33025560499249,-1.32216220690252,-1.31374734055386,-1.30093900636659,
-1.25607154766657,-1.21736994013372,-1.17254908536673,-1.16176587002138,
-1.15633043915348,-1.15183882155036,-1.14590404961739,-1.13237857279693,
-1.11246265301048,-1.0309829314971,-1.00430736412699,-0.993138841805342,
-0.985031121717851,-0.976484888847862,-0.963027568594057,-0.905270167198867,
-0.844756859122124,-0.828154058201975,-0.82157301903771,-0.817000569930036,
-0.811932286096004,-0.802947933605645,-0.79149704777724,-0.764618230914736,
-0.675965070528053,-0.660824581060035,-0.651931904544749,-0.643943374134029,
-0.63360032557256,-0.610695460654489,-0.577625649227347,-0.513832000422512,
-0.492876160719128,-0.485703479298056,-0.481484818892183,-0.476751726807192,
-0.469330506797591,-0.443841535130703,-0.387137730974593,-0.33602256950956,
-0.322670478763516,-0.314146339563308,-0.306028421477061,-0.294794925446189,
-0.265875084129225,-0.21798950604371,-0.162533150278821,-0.152084654529271,
-0.146650504880891,-0.142159549066541,-0.136225133701574,-0.122698376414465,
-0.121351841344903),.UNSPECIFIED.);
#2188=B_SPLINE_CURVE_WITH_KNOTS('',3,(#43500,#43501,#43502,#43503,#43504,
#43505,#43506,#43507,#43508,#43509,#43510,#43511,#43512,#43513,#43514,#43515,
#43516,#43517,#43518,#43519,#43520,#43521,#43522,#43523,#43524,#43525,#43526,
#43527,#43528,#43529,#43530,#43531,#43532,#43533,#43534,#43535,#43536,#43537,
#43538,#43539,#43540,#43541,#43542,#43543,#43544,#43545,#43546,#43547,#43548,
#43549,#43550,#43551,#43552,#43553,#43554,#43555,#43556,#43557,#43558,#43559,
#43560,#43561,#43562,#43563,#43564,#43565,#43566,#43567,#43568,#43569,#43570,
#43571,#43572,#43573,#43574,#43575,#43576,#43577,#43578,#43579,#43580,#43581,
#43582,#43583,#43584,#43585,#43586,#43587,#43588,#43589,#43590,#43591,#43592,
#43593,#43594,#43595,#43596,#43597,#43598,#43599,#43600,#43601,#43602,#43603,
#43604,#43605,#43606,#43607,#43608,#43609,#43610,#43611,#43612,#43613,#43614,
#43615,#43616,#43617,#43618,#43619,#43620,#43621,#43622,#43623,#43624,#43625,
#43626,#43627,#43628,#43629,#43630,#43631,#43632,#43633,#43634,#43635,#43636,
#43637,#43638,#43639,#43640,#43641,#43642,#43643,#43644,#43645,#43646,#43647,
#43648,#43649,#43650,#43651,#43652,#43653,#43654,#43655,#43656,#43657,#43658,
#43659,#43660,#43661,#43662,#43663,#43664,#43665,#43666,#43667,#43668,#43669,
#43670,#43671,#43672,#43673,#43674,#43675,#43676,#43677,#43678,#43679,#43680,
#43681,#43682,#43683,#43684,#43685,#43686,#43687,#43688,#43689,#43690,#43691),
 .UNSPECIFIED.,.F.,.F.,(4,2,2,2,2,2,2,2,2,2,2,2,2,2,2,2,2,2,2,2,2,2,2,2,
2,2,2,2,2,2,2,2,2,2,2,2,2,2,2,2,2,2,2,2,2,2,2,2,2,2,2,2,2,2,2,2,2,2,2,2,
2,2,2,2,2,2,2,2,2,2,2,2,2,2,2,2,2,2,2,2,2,2,2,2,2,2,2,2,2,2,2,2,2,2,2,4),
(-4.15046929847984,-4.13270632885826,-4.11676300793453,-4.10770559221249,
-4.09974473951702,-4.08967792181627,-4.06840763326063,-3.99397118374691,
-3.95398662443728,-3.94359230127021,-3.93823371708984,-3.93373316049068,
-3.92779520758228,-3.91442227744894,-3.85092751156094,-3.83634860473377,
-3.79028711258421,-3.77739761162911,-3.76896663538752,-3.76088437034561,
-3.75119214915331,-3.72727135145519,-3.6561071401658,-3.61720744870898,
-3.60693711676568,-3.6016032777906,-3.59709899907138,-3.59112497792671,
-3.57754808483821,-3.51424339085961,-3.46489198826929,-3.44574486133427,
-3.43606094823155,-3.42889512652169,-3.41984579887042,-3.40436097570136,
-3.33172920355803,-3.27846586088945,-3.26945068362377,-3.26437556346478,
-3.25980512841828,-3.25427457441599,-3.24071306075823,-3.17755239429721,
-3.11833702358862,-3.10483235243416,-3.09627598443772,-3.08817244092739,
-3.07703195171029,-3.05057882524173,-2.96888036571166,-2.94895304253389,
-2.93542094903084,-2.92948489351571,-2.92499293441597,-2.91955794913335,
-2.9087779040026,-2.86402239904391,-2.82553399446278,-2.78035124686849,
-2.76751992338799,-2.75910017209899,-2.75100944876956,-2.74128375303232,
-2.71714947473425,-2.63261651967047,-2.61247798609605,-2.5988443072636,
-2.59289097345053,-2.5883975256516,-2.5829749302194,-2.57225894499987,-2.52879278673367,
-2.49154160446548,-2.45980931837968,-2.43753966588343,-2.42730052285845,
-2.41932172725802,-2.41036730867661,-2.39493327852405,-2.31993857812761,
-2.28424424806978,-2.26436431862397,-2.25752265618995,-2.25290397393512,
-2.24793507666022,-2.23942009929252,-2.19358185224284,-2.13627473018799,
-2.10496524348096,-2.09311431952685,-2.08570710035488,-2.07749817419153,
-2.06575720536979,-2.03271675136986,-2.01554578796151),.UNSPECIFIED.);
#2189=B_SPLINE_CURVE_WITH_KNOTS('',3,(#43693,#43694,#43695,#43696,#43697,
#43698,#43699,#43700),.UNSPECIFIED.,.F.,.F.,(4,2,2,4),(-0.121351841344903,
-0.102778514164449,-0.0579874682746311,-0.00096969038325926),
 .UNSPECIFIED.);
#2190=B_SPLINE_CURVE_WITH_KNOTS('',3,(#43701,#43702,#43703,#43704,#43705,
#43706,#43707,#43708,#43709,#43710,#43711,#43712,#43713,#43714,#43715,#43716,
#43717,#43718,#43719,#43720,#43721,#43722,#43723,#43724,#43725,#43726,#43727,
#43728,#43729,#43730,#43731,#43732,#43733,#43734,#43735,#43736,#43737,#43738,
#43739,#43740,#43741,#43742,#43743,#43744,#43745,#43746,#43747,#43748,#43749,
#43750,#43751,#43752,#43753,#43754,#43755,#43756,#43757,#43758,#43759,#43760,
#43761,#43762,#43763,#43764,#43765,#43766,#43767,#43768,#43769,#43770,#43771,
#43772,#43773,#43774,#43775,#43776,#43777,#43778,#43779,#43780,#43781,#43782,
#43783,#43784,#43785,#43786,#43787,#43788,#43789,#43790,#43791,#43792,#43793,
#43794,#43795,#43796,#43797,#43798,#43799,#43800,#43801,#43802,#43803,#43804,
#43805,#43806,#43807,#43808,#43809,#43810,#43811,#43812,#43813,#43814,#43815,
#43816,#43817,#43818,#43819,#43820,#43821,#43822,#43823,#43824,#43825,#43826,
#43827,#43828,#43829,#43830,#43831,#43832,#43833,#43834,#43835,#43836,#43837,
#43838,#43839,#43840,#43841,#43842,#43843,#43844,#43845,#43846,#43847,#43848,
#43849,#43850,#43851,#43852,#43853,#43854,#43855,#43856,#43857,#43858,#43859,
#43860,#43861,#43862,#43863,#43864,#43865,#43866,#43867,#43868,#43869,#43870,
#43871,#43872,#43873,#43874,#43875,#43876,#43877,#43878,#43879,#43880,#43881,
#43882,#43883,#43884,#43885,#43886,#43887,#43888,#43889,#43890,#43891,#43892,
#43893,#43894,#43895,#43896,#43897,#43898,#43899),.UNSPECIFIED.,.F.,.F.,
(4,3,3,3,3,3,3,3,3,3,3,3,3,3,3,3,3,3,3,3,3,3,3,3,3,3,3,3,3,3,3,3,3,3,3,
3,3,3,3,3,3,3,3,3,3,3,3,3,3,3,3,3,3,3,3,3,3,3,3,3,3,3,3,3,3,3,4),(-16.4167960594917,
-16.3231866235391,-16.229526884803,-16.1346626699223,-16.0407807148777,
-15.945425370079,-15.8500700252804,-15.7580593298291,-15.6661696621795,
-15.5743745707618,-15.4826447796861,-15.3909489505947,-15.2992633145047,
-15.2075641168384,-15.1157697393271,-15.0239260435727,-14.9319324069844,
-14.8594406487004,-14.7674299218298,-14.6755402224228,-14.5837450989567,
-14.4920152755291,-14.400319413912,-14.3086337451621,-14.2169345147419,
-14.1251401045348,-14.0332963760681,-13.941302707081,-13.8688112721204,
-13.7768007117943,-13.6849111792182,-13.5931162226491,-13.5013865655354,
-13.4096908698183,-13.3180053663597,-13.2263063004262,-13.1345120524464,
-13.0426684851999,-12.9506749741105,-12.8781818955404,-12.7861710919384,
-12.6942813168831,-12.602486118933,-12.5107562230586,-12.4190602902644,
-12.3273745516834,-12.2356752528554,-12.1438807768566,-12.0520369839466,
-11.9600432533881,-11.8875525189603,-11.7955415542391,-11.7036516150329,
-11.6118562501565,-11.5201261839085,-11.4284300786933,-11.3367441658633,
-11.2450446911762,-11.1532500379329,-11.0614060667469,-10.9694121580842,
-10.8969231423803,-10.8060912012837,-10.715400234171,-10.6247905958859,
-10.5342411065541,-10.4882942077004),.UNSPECIFIED.);
#2191=B_SPLINE_CURVE_WITH_KNOTS('',3,(#43905,#43906,#43907,#43908,#43909,
#43910,#43911,#43912,#43913,#43914,#43915,#43916,#43917,#43918,#43919,#43920,
#43921,#43922,#43923,#43924,#43925,#43926,#43927,#43928,#43929,#43930,#43931,
#43932,#43933,#43934,#43935,#43936,#43937,#43938,#43939,#43940,#43941,#43942,
#43943,#43944,#43945,#43946,#43947,#43948,#43949,#43950,#43951,#43952,#43953,
#43954,#43955,#43956,#43957,#43958,#43959,#43960,#43961,#43962,#43963,#43964,
#43965,#43966,#43967,#43968,#43969,#43970,#43971,#43972,#43973,#43974,#43975,
#43976,#43977,#43978,#43979,#43980,#43981,#43982,#43983,#43984,#43985,#43986,
#43987,#43988,#43989,#43990,#43991,#43992,#43993,#43994,#43995,#43996,#43997,
#43998,#43999,#44000,#44001,#44002,#44003,#44004,#44005,#44006,#44007,#44008,
#44009,#44010,#44011,#44012,#44013,#44014,#44015,#44016,#44017,#44018,#44019,
#44020,#44021,#44022,#44023,#44024,#44025,#44026,#44027,#44028,#44029,#44030,
#44031,#44032),.UNSPECIFIED.,.F.,.F.,(4,2,2,2,2,2,2,2,2,2,2,2,2,2,2,2,2,
2,2,2,2,2,2,2,2,2,2,2,2,2,2,2,2,2,2,2,2,2,2,2,2,2,2,2,2,2,2,2,2,2,2,2,2,
2,2,2,2,2,2,2,2,2,2,4),(0.000239016707890752,0.00315166214361164,0.00671773766773776,
0.0169827679766186,0.0635487110239646,0.112156318829945,0.129455895946306,
0.143873315375382,0.153203387882427,0.162137432678307,0.17287716353032,
0.194033657182551,0.272985524325323,0.305915699365059,0.325078614379287,
0.331875706730879,0.336498161130002,0.341361930413961,0.349714073947605,
0.393602958573611,0.468743405451748,0.487751158624623,0.497184420264035,
0.504820517838277,0.51368934223756,0.52931039522351,0.619175633277945,0.658185238232473,
0.66828046524847,0.673409994408688,0.677833605850783,0.683613544369486,
0.696660790620161,0.760790654083829,0.81077497077889,0.830124034941486,
0.839900410017414,0.84713465343804,0.856274490851527,0.871948121460915,
0.937828225154308,0.977392726828777,0.998489503837954,1.00554079075414,
1.01025533116603,1.01525251794431,1.02378236126374,1.06622533685266,1.12577146809519,
1.14774179735986,1.16486129990916,1.17418522605343,1.18216887676668,1.19199345952817,
1.21172904406483,1.3030291436912,1.32364860922065,1.3375215734021,1.34352735342838,
1.34802717493649,1.35340521592046,1.36395766346144,1.41960965183253,1.42897696838616),
 .UNSPECIFIED.);
#2192=B_SPLINE_CURVE_WITH_KNOTS('',3,(#44035,#44036,#44037,#44038,#44039,
#44040,#44041,#44042,#44043,#44044,#44045,#44046,#44047,#44048,#44049,#44050,
#44051,#44052,#44053,#44054,#44055,#44056,#44057,#44058,#44059,#44060,#44061,
#44062,#44063,#44064,#44065,#44066,#44067,#44068,#44069,#44070,#44071,#44072,
#44073,#44074,#44075,#44076,#44077,#44078,#44079,#44080,#44081,#44082,#44083,
#44084,#44085,#44086,#44087,#44088,#44089,#44090,#44091,#44092,#44093,#44094,
#44095,#44096,#44097,#44098,#44099,#44100,#44101,#44102,#44103,#44104,#44105,
#44106,#44107,#44108,#44109,#44110,#44111,#44112,#44113,#44114,#44115,#44116,
#44117,#44118,#44119,#44120,#44121,#44122,#44123,#44124,#44125,#44126,#44127,
#44128,#44129,#44130,#44131,#44132,#44133,#44134,#44135,#44136,#44137,#44138,
#44139,#44140,#44141,#44142,#44143,#44144,#44145,#44146,#44147,#44148,#44149,
#44150,#44151,#44152,#44153,#44154,#44155,#44156,#44157,#44158,#44159,#44160,
#44161,#44162,#44163,#44164,#44165,#44166,#44167,#44168,#44169,#44170,#44171,
#44172,#44173,#44174,#44175,#44176,#44177,#44178,#44179,#44180,#44181,#44182,
#44183,#44184,#44185,#44186,#44187,#44188,#44189,#44190,#44191,#44192,#44193,
#44194,#44195,#44196,#44197,#44198,#44199,#44200,#44201,#44202,#44203,#44204,
#44205,#44206,#44207,#44208,#44209,#44210),.UNSPECIFIED.,.F.,.F.,(4,2,2,
2,2,2,2,2,2,2,2,2,2,2,2,2,2,2,2,2,2,2,2,2,2,2,2,2,2,2,2,2,2,2,2,2,2,2,2,
2,2,2,2,2,2,2,2,2,2,2,2,2,2,2,2,2,2,2,2,2,2,2,2,2,2,2,2,2,2,2,2,2,2,2,2,
2,2,2,2,2,2,2,2,2,2,2,2,4),(-4.02414899437559,-4.01725069329091,-3.95119121645565,
-3.91323211790503,-3.88805516392213,-3.8772911778161,-3.86918427641931,
-3.86035722164114,-3.84579108688948,-3.76660016120897,-3.72368939308642,
-3.71292566437222,-3.70743568028743,-3.70287775078405,-3.696902579107,-3.68292552867492,
-3.61991469360162,-3.57106522667542,-3.55179493283753,-3.54205679910813,
-3.5348516529627,-3.52575184739845,-3.51017381466984,-3.4378738824274,-3.40050153883197,
-3.38005104542205,-3.3731274348465,-3.36848553490925,-3.36355630707564,
-3.35517047884301,-3.31607714363579,-3.25353266158283,-3.22030437544304,
-3.20857732616469,-3.2004021206995,-3.19207149277192,-3.17953784307398,
-3.14109450170882,-3.07216486309444,-3.04444276755788,-3.03685934018612,
-3.03210961014489,-3.02792601811024,-3.02094000648734,-3.00149302970198,
-2.94326284724269,-2.89129340084666,-2.87545999123913,-2.86641684277024,
-2.85844052559617,-2.84831529139372,-2.82675364675384,-2.73854237802906,
-2.71816695693039,-2.70441754302905,-2.69843704402835,-2.69393450153278,
-2.6885146518464,-2.67815042909065,-2.62021754296784,-2.57388348214683,
-2.54551001820523,-2.53434543589075,-2.52623522438772,-2.51768143347307,
-2.50420134075086,-2.44897165951614,-2.39572951484344,-2.37098968375173,
-2.36363509616993,-2.35891506173386,-2.35468603588276,-2.34745279183694,
-2.32596393102289,-2.26935087648644,-2.21378315056379,-2.2004061807555,
-2.19187937311335,-2.18376834674631,-2.17256016371868,-2.14563307218365,
-2.0644695723789,-2.04458371551823,-2.03107289414446,-2.02514274496808,
-2.02065276747142,-2.01521677086951,-2.01510602195132),.UNSPECIFIED.);
#2193=B_SPLINE_CURVE_WITH_KNOTS('',3,(#44216,#44217,#44218,#44219,#44220,
#44221,#44222,#44223,#44224,#44225,#44226,#44227,#44228,#44229,#44230,#44231,
#44232,#44233,#44234,#44235,#44236,#44237,#44238,#44239,#44240,#44241,#44242,
#44243,#44244,#44245,#44246,#44247,#44248,#44249,#44250,#44251,#44252,#44253,
#44254,#44255,#44256,#44257,#44258,#44259,#44260,#44261,#44262,#44263,#44264,
#44265,#44266,#44267,#44268,#44269,#44270,#44271,#44272,#44273,#44274,#44275,
#44276,#44277,#44278,#44279,#44280,#44281,#44282,#44283,#44284,#44285,#44286,
#44287,#44288,#44289,#44290,#44291,#44292,#44293,#44294,#44295,#44296,#44297,
#44298,#44299,#44300,#44301,#44302,#44303,#44304,#44305,#44306,#44307,#44308,
#44309,#44310,#44311,#44312,#44313,#44314,#44315,#44316,#44317,#44318,#44319,
#44320,#44321,#44322,#44323,#44324,#44325,#44326,#44327,#44328,#44329,#44330,
#44331,#44332,#44333,#44334,#44335,#44336,#44337,#44338,#44339,#44340,#44341,
#44342,#44343,#44344,#44345,#44346,#44347,#44348,#44349,#44350,#44351,#44352,
#44353,#44354,#44355,#44356,#44357,#44358,#44359,#44360),.UNSPECIFIED.,
 .F.,.F.,(4,3,3,3,3,3,3,3,3,3,3,3,3,3,3,3,3,3,3,3,3,3,3,3,3,3,3,3,3,3,3,
3,3,3,3,3,3,3,3,3,3,3,3,3,3,3,3,3,4),(74.4826134639429,74.5701017210815,
74.6575411968586,74.7449559528723,74.8323667521485,74.9197943499317,75.0073142166116,
75.0948813813697,75.1825901309915,75.2578179239381,75.3457884273519,75.4336478048373,
75.5214188779625,75.612297430782,75.6999676523823,75.78762386132,75.8752865504186,
75.9629762119858,76.0507600100425,76.1385998960894,76.2265621785653,76.2484473005182,
76.3363314594677,76.4241063946703,76.5117950016086,76.6027052110448,76.6902983576817,
76.7778796066848,76.8654695235803,76.9530886749992,77.0408056385432,77.1285807561576,
77.2164817566519,77.2390766770982,77.3260771415733,77.412966501338,77.4997686274976,
77.5910108057702,77.6777204878012,77.7644207287209,77.8511329515665,77.9378785848385,
78.0247325806727,78.1116496986136,78.1987067829138,78.2297060536782,78.3416517190473,
78.4517369676243,78.5398162006367),.UNSPECIFIED.);
#2194=B_SPLINE_CURVE_WITH_KNOTS('',3,(#44362,#44363,#44364,#44365),
 .UNSPECIFIED.,.F.,.F.,(4,4),(78.5398163397448,79.2203354302583),
 .UNSPECIFIED.);
#2195=B_SPLINE_CURVE_WITH_KNOTS('',3,(#44369,#44370,#44371,#44372,#44373,
#44374,#44375,#44376,#44377,#44378,#44379,#44380,#44381,#44382,#44383,#44384,
#44385,#44386,#44387,#44388,#44389,#44390,#44391,#44392,#44393,#44394,#44395,
#44396,#44397,#44398,#44399,#44400,#44401,#44402,#44403,#44404,#44405,#44406,
#44407,#44408,#44409,#44410,#44411),.UNSPECIFIED.,.F.,.F.,(4,3,3,3,3,3,
3,3,3,3,3,3,3,3,4),(78.5398163398759,78.6511924917076,78.7647307704921,
78.7900351244193,78.8773825896874,78.9646210658141,79.0517740756938,79.1388674668699,
79.2259295154673,79.3129813583285,79.4000441200288,79.4871929619449,79.5743845951527,
79.6617164564392,79.7442523245248),.UNSPECIFIED.);
#2196=B_SPLINE_CURVE_WITH_KNOTS('',3,(#44412,#44413,#44414,#44415,#44416,
#44417,#44418,#44419,#44420,#44421,#44422,#44423,#44424,#44425,#44426,#44427,
#44428,#44429,#44430,#44431,#44432,#44433,#44434,#44435,#44436,#44437,#44438,
#44439,#44440,#44441,#44442,#44443,#44444,#44445,#44446,#44447,#44448,#44449,
#44450,#44451,#44452,#44453,#44454,#44455,#44456,#44457,#44458,#44459,#44460,
#44461,#44462,#44463,#44464,#44465,#44466,#44467,#44468,#44469,#44470,#44471,
#44472,#44473,#44474,#44475,#44476,#44477,#44478,#44479,#44480,#44481,#44482,
#44483,#44484,#44485,#44486,#44487,#44488,#44489,#44490,#44491,#44492,#44493,
#44494,#44495,#44496,#44497,#44498,#44499,#44500,#44501,#44502,#44503,#44504,
#44505,#44506,#44507,#44508,#44509,#44510,#44511,#44512,#44513,#44514,#44515,
#44516,#44517,#44518,#44519,#44520,#44521,#44522,#44523,#44524,#44525,#44526,
#44527,#44528,#44529,#44530,#44531,#44532,#44533,#44534,#44535,#44536,#44537,
#44538,#44539,#44540,#44541,#44542,#44543,#44544,#44545,#44546,#44547,#44548,
#44549,#44550,#44551,#44552,#44553,#44554,#44555,#44556,#44557,#44558,#44559),
 .UNSPECIFIED.,.F.,.F.,(4,3,3,3,3,3,3,3,3,3,3,3,3,3,3,3,3,3,3,3,3,3,3,3,
3,3,3,3,3,3,3,3,3,3,3,3,3,3,3,3,3,3,3,3,3,3,3,3,3,4),(74.4816294174661,
74.5692291326888,74.6568738988186,74.7446611805597,74.8275176180992,74.9153515022495,
75.0030745344625,75.0907096966175,75.1816393588752,75.2691756140558,75.3566988094021,
75.4442295822475,75.5317885702762,75.6194441849438,75.7071571937103,75.7949954619019,
75.8181469946792,75.9059803529528,75.9937031226878,76.0813382823747,76.1722680434853,
76.2598049368958,76.3473290042904,76.4348608808726,76.5224212023653,76.6100784810607,
76.6977933481166,76.7856337425876,76.8087763712593,76.8964961427356,76.9841049002744,
77.0716257599405,77.1625982584278,77.2500208544713,77.3374308199701,77.4248489115836,
77.512295886818,77.5998410363746,77.6874443493797,77.7751748842725,77.7994057478393,
77.8864522154222,77.9733604160186,78.0601893663266,78.1469605854896,78.2336955406122,
78.3204377947017,78.4071831868706,78.4939872267225,78.5398163397448),
 .UNSPECIFIED.);
#2197=B_SPLINE_CURVE_WITH_KNOTS('',3,(#44565,#44566,#44567,#44568,#44569,
#44570,#44571,#44572,#44573,#44574,#44575,#44576,#44577,#44578,#44579,#44580,
#44581,#44582,#44583,#44584,#44585,#44586,#44587,#44588,#44589,#44590,#44591,
#44592,#44593,#44594,#44595,#44596,#44597,#44598,#44599,#44600,#44601,#44602,
#44603,#44604,#44605,#44606,#44607,#44608,#44609,#44610,#44611,#44612,#44613,
#44614,#44615,#44616,#44617,#44618,#44619,#44620,#44621,#44622,#44623,#44624,
#44625,#44626,#44627,#44628,#44629,#44630,#44631,#44632,#44633,#44634,#44635,
#44636,#44637,#44638,#44639,#44640,#44641,#44642,#44643,#44644,#44645,#44646,
#44647,#44648,#44649,#44650,#44651,#44652,#44653,#44654,#44655,#44656,#44657,
#44658,#44659,#44660,#44661,#44662,#44663,#44664,#44665,#44666,#44667,#44668,
#44669,#44670,#44671,#44672,#44673,#44674,#44675,#44676,#44677,#44678,#44679,
#44680,#44681,#44682,#44683,#44684,#44685,#44686,#44687,#44688,#44689,#44690,
#44691,#44692,#44693,#44694,#44695,#44696,#44697,#44698,#44699,#44700,#44701,
#44702,#44703,#44704,#44705,#44706,#44707,#44708,#44709,#44710,#44711,#44712),
 .UNSPECIFIED.,.F.,.F.,(4,3,3,3,3,3,3,3,3,3,3,3,3,3,3,3,3,3,3,3,3,3,3,3,
3,3,3,3,3,3,3,3,3,3,3,3,3,3,3,3,3,3,3,3,3,3,3,3,3,4),(68.1983678147316,
68.2861854710949,68.3234122878779,68.4112283810042,68.4989336774631,68.5865511791694,
68.6774874898305,68.7650063816156,68.8525123525859,68.9400260581836,69.0275681543285,
69.1152072202934,69.2029038608162,69.2907261485386,69.314041664458,69.4018609779144,
69.4895694873212,69.5771901909359,69.6681252971987,69.755647343511,69.8431564461835,
69.9306732573624,70.0182184296503,70.1058605129341,70.1935601400665,70.2813853468485,
70.304671041038,70.3924917596528,70.4802017089149,70.5678238849091,70.6587584514977,
70.7462820410624,70.8337927103019,70.9213111095382,71.0088578895641,71.09650160134,
71.1842028709319,71.2720297278734,71.295300417618,71.3826851317177,71.469959269805,
71.5571463325211,71.6445819200016,71.7316742053465,71.8187548325092,71.9058449008842,
71.9935414337543,72.0807584843929,72.1686947583788,72.2566310323648),
 .UNSPECIFIED.);
#2198=B_SPLINE_CURVE_WITH_KNOTS('',3,(#44713,#44714,#44715,#44716,#44717,
#44718,#44719,#44720,#44721,#44722,#44723,#44724,#44725,#44726,#44727,#44728,
#44729,#44730,#44731,#44732,#44733,#44734,#44735,#44736,#44737,#44738,#44739,
#44740,#44741,#44742,#44743,#44744,#44745,#44746,#44747,#44748,#44749,#44750,
#44751,#44752,#44753,#44754,#44755,#44756,#44757,#44758,#44759,#44760,#44761,
#44762,#44763,#44764,#44765,#44766,#44767,#44768,#44769,#44770,#44771,#44772,
#44773,#44774,#44775,#44776,#44777,#44778,#44779,#44780,#44781,#44782,#44783,
#44784,#44785,#44786,#44787,#44788,#44789,#44790,#44791,#44792,#44793,#44794,
#44795,#44796,#44797),.UNSPECIFIED.,.F.,.F.,(4,3,3,3,3,3,3,3,3,3,3,3,3,
3,3,3,3,3,3,3,3,3,3,3,3,3,3,3,4),(72.2566310325652,72.2859297941981,72.3737636821433,
72.4614867181185,72.5491218839988,72.6400515448462,72.7275878036391,72.8151110025499,
72.9026417789087,72.9902007703964,73.0778563884256,73.1655694005009,73.2534076718996,
73.2765591707781,73.3643925445142,73.4521153297987,73.5397505051032,73.6306802603851,
73.7182171694824,73.8057412525619,73.8932731448105,73.9808334819333,74.068490776127,
74.1562056586224,74.2440460683294,74.2671885473581,74.3549161093617,74.4425200092409,
74.4826134639429),.UNSPECIFIED.);
#2199=B_SPLINE_CURVE_WITH_KNOTS('',3,(#44799,#44800,#44801,#44802,#44803,
#44804,#44805,#44806,#44807,#44808,#44809,#44810,#44811,#44812,#44813,#44814,
#44815,#44816,#44817,#44818,#44819,#44820,#44821,#44822,#44823,#44824,#44825,
#44826,#44827,#44828,#44829,#44830,#44831,#44832,#44833,#44834,#44835,#44836,
#44837,#44838,#44839,#44840,#44841,#44842,#44843,#44844,#44845,#44846,#44847,
#44848,#44849,#44850,#44851,#44852,#44853,#44854,#44855,#44856,#44857,#44858,
#44859,#44860,#44861,#44862,#44863,#44864,#44865,#44866,#44867,#44868,#44869,
#44870,#44871,#44872,#44873,#44874,#44875,#44876,#44877,#44878,#44879,#44880),
 .UNSPECIFIED.,.F.,.F.,(4,3,3,3,3,3,3,3,3,3,3,3,3,3,3,3,3,3,3,3,3,3,3,3,
3,3,3,4),(72.2566310325652,72.3454121678946,72.4342210203789,72.5230760362226,
72.6120571070531,72.7011068517644,72.7903135273602,72.8462588649391,72.934079580666,
73.0217895270243,73.1094117001026,73.2003462677797,73.2878698544167,73.3753805207293,
73.4628989170425,73.5504456941521,73.638089403037,73.7257906697492,73.8136175238493,
73.8368882415192,73.924677994041,74.0123639854369,74.0999670580816,74.1875079866763,
74.2750138504675,74.3624996138977,74.4500027036407,74.4816294174661),
 .UNSPECIFIED.);
#2200=B_SPLINE_CURVE_WITH_KNOTS('',3,(#44881,#44882,#44883,#44884,#44885,
#44886,#44887,#44888,#44889,#44890,#44891,#44892,#44893,#44894,#44895,#44896,
#44897,#44898,#44899,#44900,#44901,#44902,#44903,#44904,#44905,#44906,#44907,
#44908,#44909,#44910,#44911,#44912,#44913,#44914,#44915,#44916,#44917,#44918,
#44919,#44920,#44921,#44922,#44923,#44924,#44925,#44926,#44927,#44928,#44929,
#44930,#44931,#44932,#44933,#44934,#44935,#44936,#44937,#44938,#44939,#44940,
#44941,#44942,#44943,#44944,#44945,#44946,#44947,#44948,#44949,#44950,#44951,
#44952,#44953,#44954,#44955,#44956,#44957,#44958,#44959,#44960,#44961,#44962,
#44963,#44964,#44965,#44966,#44967,#44968,#44969,#44970,#44971,#44972,#44973,
#44974,#44975,#44976,#44977,#44978,#44979,#44980,#44981,#44982,#44983,#44984,
#44985,#44986,#44987,#44988,#44989,#44990,#44991,#44992,#44993,#44994,#44995,
#44996,#44997,#44998,#44999,#45000,#45001,#45002,#45003,#45004,#45005,#45006,
#45007,#45008,#45009,#45010,#45011,#45012,#45013,#45014,#45015,#45016,#45017,
#45018,#45019,#45020,#45021,#45022,#45023,#45024,#45025,#45026,#45027,#45028),
 .UNSPECIFIED.,.F.,.F.,(4,3,3,3,3,3,3,3,3,3,3,3,3,3,3,3,3,3,3,3,3,3,3,3,
3,3,3,3,3,3,3,3,3,3,3,3,3,3,3,3,3,3,3,3,3,3,3,3,3,4),(68.1993438798599,
68.2868799916938,68.3743918833257,68.4619002146255,68.5494256379166,68.637042488327,
68.7247067515849,68.8125099054391,68.883741358619,68.971559219945,69.0592662848475,
69.1468855531686,69.2378212009224,69.3253418436864,69.4128495568768,69.500364994083,
69.5879088093621,69.6755495674304,69.7632478863016,69.8510718195009,69.8743707351991,
69.9621889551786,70.0498963831715,70.137516018533,70.2284515301888,70.3159725474149,
70.4034806371411,70.4909964525364,70.5785406472388,70.6661817846189,70.7538804831779,
70.8417047937,70.8650001117791,70.9528162060867,71.0405215037276,71.1281390066153,
71.2190753168333,71.3065942097912,71.394100181929,71.4816138886882,71.5691559859863,
71.6567950530876,71.7444916947385,71.8323139835676,71.8556294883591,71.9558798743625,
72.0526994126788,72.1492492883176,72.2454013625398,72.2566310323726),
 .UNSPECIFIED.);
#2201=B_SPLINE_CURVE_WITH_KNOTS('',3,(#45034,#45035,#45036,#45037,#45038,
#45039,#45040,#45041,#45042,#45043,#45044,#45045,#45046,#45047,#45048,#45049,
#45050,#45051,#45052,#45053,#45054,#45055,#45056,#45057,#45058,#45059,#45060,
#45061,#45062,#45063,#45064,#45065,#45066,#45067,#45068,#45069,#45070,#45071,
#45072,#45073,#45074,#45075,#45076,#45077,#45078,#45079,#45080,#45081,#45082,
#45083,#45084,#45085,#45086,#45087,#45088,#45089,#45090,#45091,#45092,#45093,
#45094,#45095,#45096,#45097,#45098,#45099,#45100,#45101,#45102,#45103,#45104,
#45105,#45106,#45107,#45108,#45109,#45110,#45111,#45112,#45113,#45114,#45115,
#45116,#45117,#45118,#45119,#45120,#45121,#45122,#45123,#45124,#45125,#45126,
#45127,#45128,#45129,#45130,#45131,#45132,#45133,#45134,#45135,#45136,#45137,
#45138,#45139,#45140,#45141,#45142,#45143,#45144,#45145,#45146,#45147,#45148,
#45149,#45150,#45151,#45152,#45153,#45154,#45155,#45156,#45157,#45158,#45159,
#45160,#45161,#45162,#45163,#45164,#45165,#45166,#45167,#45168,#45169,#45170,
#45171,#45172,#45173,#45174,#45175,#45176,#45177,#45178,#45179,#45180,#45181),
 .UNSPECIFIED.,.F.,.F.,(4,3,3,3,3,3,3,3,3,3,3,3,3,3,3,3,3,3,3,3,3,3,3,3,
3,3,3,3,3,3,3,3,3,3,3,3,3,3,3,3,3,3,3,3,3,3,3,3,3,4),(61.9155795994057,
62.0030944068429,62.0906369960354,62.1782762547704,62.2659725380791,62.3537951104487,
62.3796360283978,62.4674537279978,62.5551606325058,62.6427797419325,62.7337154498132,
62.8212359383819,62.9087434993666,62.9962587865121,63.0838024540337,63.1714430684749,
63.2591412459543,63.3469650420966,63.3702654049778,63.4580831375175,63.545790074768,
63.633409216705,63.7243449123116,63.8118654326121,63.8993730249881,63.9868883431528,
64.0744320412883,64.1620726855925,64.2497708925329,64.3375947173261,64.3608947815578,
64.4487125812256,64.5364195861566,64.6240387962398,64.7149744664771,64.8024950556412,
64.8900027170247,64.977518104265,65.0650618714678,65.1527025844783,65.240400859995,
65.3282247526493,65.3515241581379,65.4399937117072,65.5283487386399,65.6166091627478,
65.7058183034073,65.7939457801226,65.8836957527541,65.9734457253856),
 .UNSPECIFIED.);
#2202=B_SPLINE_CURVE_WITH_KNOTS('',3,(#45182,#45183,#45184,#45185,#45186,
#45187,#45188,#45189,#45190,#45191,#45192,#45193,#45194,#45195,#45196,#45197,
#45198,#45199,#45200,#45201,#45202,#45203,#45204,#45205,#45206,#45207,#45208,
#45209,#45210,#45211,#45212,#45213,#45214,#45215,#45216,#45217,#45218,#45219,
#45220,#45221,#45222,#45223,#45224,#45225,#45226,#45227,#45228,#45229,#45230,
#45231,#45232,#45233,#45234,#45235,#45236,#45237,#45238,#45239,#45240,#45241,
#45242,#45243,#45244,#45245,#45246,#45247,#45248,#45249,#45250,#45251,#45252,
#45253,#45254,#45255,#45256,#45257,#45258,#45259,#45260),.UNSPECIFIED.,
 .F.,.F.,(4,3,3,3,3,3,3,3,3,3,3,3,3,3,3,3,3,3,3,3,3,3,3,3,3,3,4),(65.9734457256019,
66.0719665867376,66.1708765057206,66.2703101688383,66.3421535347179,66.4299713960909,
66.5176784610392,66.6052977294049,66.6962333771415,66.7837540199466,66.8712617331766,
66.958777170421,67.0463209857378,67.133961743841,67.2216600627455,67.3094839959762,
67.3327829112979,67.4206086977955,67.5083218961891,67.5959325406812,67.6834855476166,
67.7710016175743,67.8585014192332,67.9460421456659,68.0336015824382,68.1212568561678,
68.1983678147316),.UNSPECIFIED.);
#2203=B_SPLINE_CURVE_WITH_KNOTS('',3,(#45262,#45263,#45264,#45265,#45266,
#45267,#45268,#45269,#45270,#45271,#45272,#45273,#45274,#45275,#45276,#45277,
#45278,#45279,#45280,#45281,#45282,#45283,#45284,#45285,#45286,#45287,#45288,
#45289,#45290,#45291,#45292,#45293,#45294,#45295,#45296,#45297,#45298,#45299,
#45300,#45301,#45302,#45303,#45304,#45305,#45306,#45307,#45308,#45309,#45310,
#45311,#45312,#45313,#45314,#45315,#45316,#45317,#45318,#45319,#45320,#45321,
#45322,#45323,#45324,#45325,#45326,#45327,#45328,#45329,#45330,#45331,#45332,
#45333,#45334,#45335,#45336,#45337,#45338,#45339,#45340,#45341,#45342,#45343),
 .UNSPECIFIED.,.F.,.F.,(4,3,3,3,3,3,3,3,3,3,3,3,3,3,3,3,3,3,3,3,3,3,3,3,
3,3,3,4),(65.9734457255633,66.0604573157294,66.14736302234,66.2341866831258,
66.3209558418872,66.4076973438865,66.4944326106493,66.5811830545443,66.6680217581067,
66.7549075928963,66.8419276082886,66.902482605459,66.990300405037,67.0780074098778,
67.16562661987,67.2565622901411,67.3440828792145,67.4315905405076,67.5191059276573,
67.6066496947706,67.6942904076922,67.7819886831202,67.869812575687,67.893111982039,
67.9809172824462,68.0686253046379,68.1562387872474,68.1993438798599),
 .UNSPECIFIED.);
#2204=B_SPLINE_CURVE_WITH_KNOTS('',3,(#45344,#45345,#45346,#45347,#45348,
#45349,#45350,#45351,#45352,#45353,#45354,#45355,#45356,#45357,#45358,#45359,
#45360,#45361,#45362,#45363,#45364,#45365,#45366,#45367,#45368,#45369,#45370,
#45371,#45372,#45373,#45374,#45375,#45376,#45377,#45378,#45379,#45380,#45381,
#45382,#45383,#45384,#45385,#45386,#45387,#45388,#45389,#45390,#45391,#45392,
#45393,#45394,#45395,#45396,#45397,#45398,#45399,#45400,#45401,#45402,#45403,
#45404,#45405,#45406,#45407,#45408,#45409,#45410,#45411,#45412,#45413,#45414,
#45415,#45416,#45417,#45418,#45419,#45420,#45421,#45422,#45423,#45424,#45425,
#45426,#45427,#45428,#45429,#45430,#45431,#45432,#45433,#45434,#45435,#45436,
#45437,#45438,#45439,#45440,#45441,#45442,#45443,#45444,#45445,#45446,#45447,
#45448,#45449,#45450,#45451,#45452,#45453,#45454,#45455,#45456,#45457,#45458,
#45459,#45460,#45461,#45462,#45463,#45464,#45465,#45466,#45467,#45468,#45469,
#45470,#45471,#45472,#45473,#45474,#45475,#45476,#45477,#45478,#45479,#45480,
#45481,#45482,#45483,#45484,#45485,#45486,#45487,#45488,#45489,#45490,#45491,
#45492,#45493,#45494),.UNSPECIFIED.,.F.,.F.,(4,3,3,3,3,3,3,3,3,3,3,3,3,
3,3,3,3,3,3,3,3,3,3,3,3,3,3,3,3,3,3,3,3,3,3,3,3,3,3,3,3,3,3,3,3,3,3,3,3,
3,4),(61.9154901076124,61.9493357225588,62.0371534434414,62.124860369225,
62.2124794998959,62.3034151998013,62.3909357094019,62.4784432913042,62.5659585992311,
62.6535022873757,62.7411429221022,62.8288411196942,62.9166649355437,62.9399650991389,
63.0277828228076,63.1154897513483,63.2031088847447,63.2940445836165,63.3815650958472,
63.4690726803401,63.5565879908155,63.6441316814639,63.7317723186155,63.8194705185899,
63.9072943367414,63.9305944757189,64.0184122103713,64.1061191499622,64.1937382944615,
64.2846739891911,64.3721945125848,64.4597021082432,64.5472174298747,64.6347611316574,
64.7224017798552,64.8100999908372,64.8979238198559,64.9212238522989,65.0090415519244,
65.0967484564579,65.1843675659104,65.2753032737815,65.3628237623755,65.4503313233851,
65.5378466105556,65.6253902781022,65.7130308925677,65.8007290700712,65.8885528662372,
65.911853228879,65.9734457253856),.UNSPECIFIED.);
#2205=B_SPLINE_CURVE_WITH_KNOTS('',3,(#45500,#45501,#45502,#45503,#45504,
#45505,#45506,#45507,#45508,#45509,#45510,#45511,#45512,#45513,#45514,#45515,
#45516,#45517,#45518,#45519,#45520,#45521,#45522,#45523,#45524,#45525,#45526,
#45527,#45528,#45529,#45530,#45531,#45532,#45533,#45534,#45535,#45536,#45537,
#45538,#45539,#45540,#45541,#45542,#45543,#45544,#45545,#45546,#45547,#45548,
#45549,#45550,#45551,#45552,#45553,#45554,#45555,#45556,#45557,#45558,#45559,
#45560,#45561,#45562,#45563,#45564,#45565,#45566,#45567,#45568,#45569,#45570,
#45571,#45572,#45573,#45574,#45575,#45576,#45577,#45578,#45579,#45580,#45581,
#45582,#45583,#45584,#45585,#45586,#45587,#45588,#45589,#45590,#45591,#45592,
#45593,#45594,#45595,#45596,#45597,#45598,#45599,#45600,#45601,#45602,#45603,
#45604,#45605,#45606,#45607,#45608,#45609,#45610,#45611,#45612,#45613,#45614,
#45615,#45616,#45617,#45618,#45619,#45620,#45621,#45622,#45623,#45624,#45625,
#45626,#45627,#45628,#45629,#45630,#45631,#45632,#45633,#45634,#45635,#45636,
#45637,#45638,#45639,#45640,#45641,#45642,#45643,#45644,#45645,#45646,#45647),
 .UNSPECIFIED.,.F.,.F.,(4,3,3,3,3,3,3,3,3,3,3,3,3,3,3,3,3,3,3,3,3,3,3,3,
3,3,3,3,3,3,3,3,3,3,3,3,3,3,3,3,3,3,3,3,3,3,3,3,3,4),(55.633055807239,55.7206644555141,
55.8100638696896,55.897581680751,55.9850891020412,56.0726067865466,56.1634200321393,
56.2510686326646,56.3387777720785,56.4266088847394,56.4358597689176,56.5236774922691,
56.6113844205186,56.6990035536499,56.7899392526309,56.8774597646623,56.9649673489804,
57.0524826593056,57.1400263498282,57.2276669868911,57.3153651867981,57.4031890049135,
57.4264891454977,57.5143068690169,57.6020137974301,57.6896329307208,57.7805686296404,
57.86808914182,57.9555967262817,58.043112036746,58.1306557274031,58.2182963645929,
58.3059945646225,58.3938183828535,58.4171185220777,58.5049362472664,58.5926431773569,
58.6802623123306,58.7711980106215,58.8587185244875,58.9462261106341,59.0337414227797,
59.1212851151128,59.2089257539622,59.296623955644,59.3844477755035,59.4077478986577,
59.5162980885706,59.6233575347649,59.6902604180773),.UNSPECIFIED.);
#2206=B_SPLINE_CURVE_WITH_KNOTS('',3,(#45648,#45649,#45650,#45651,#45652,
#45653,#45654,#45655,#45656,#45657,#45658,#45659,#45660,#45661,#45662,#45663,
#45664,#45665,#45666,#45667,#45668,#45669,#45670,#45671,#45672,#45673,#45674,
#45675,#45676,#45677,#45678,#45679,#45680,#45681,#45682,#45683,#45684,#45685,
#45686,#45687,#45688,#45689,#45690,#45691,#45692,#45693,#45694,#45695,#45696,
#45697,#45698,#45699,#45700,#45701,#45702,#45703,#45704,#45705,#45706,#45707,
#45708,#45709,#45710,#45711,#45712,#45713,#45714,#45715,#45716,#45717,#45718,
#45719,#45720,#45721,#45722,#45723,#45724,#45725,#45726),.UNSPECIFIED.,
 .F.,.F.,(4,3,3,3,3,3,3,3,3,3,3,3,3,3,3,3,3,3,3,3,3,3,3,3,3,3,4),(59.690260418206,
59.778775025335,59.8656202866756,59.9524524287065,60.0392927592542,60.1290638882501,
60.2160327259131,60.3072050005754,60.3983772752377,60.4861949989052,60.5739019274446,
60.6615210608397,60.7524567597119,60.8399772719413,60.9274848564327,61.0150001669067,
61.1025438575537,61.1901844947038,61.2778826946767,61.3657065128266,61.3890066518178,
61.4768208758908,61.5645289299805,61.6522915973368,61.7398434419403,61.827711520673,
61.9155795994057),.UNSPECIFIED.);
#2207=B_SPLINE_CURVE_WITH_KNOTS('',3,(#45728,#45729,#45730,#45731,#45732,
#45733,#45734,#45735,#45736,#45737,#45738,#45739,#45740,#45741,#45742,#45743,
#45744,#45745,#45746,#45747,#45748,#45749,#45750,#45751,#45752,#45753,#45754,
#45755,#45756,#45757,#45758,#45759,#45760,#45761,#45762,#45763,#45764,#45765,
#45766,#45767,#45768,#45769,#45770,#45771,#45772,#45773,#45774,#45775,#45776,
#45777,#45778,#45779,#45780,#45781,#45782,#45783,#45784,#45785,#45786,#45787,
#45788,#45789,#45790,#45791,#45792,#45793,#45794,#45795,#45796,#45797,#45798,
#45799,#45800,#45801,#45802,#45803,#45804,#45805,#45806),.UNSPECIFIED.,
 .F.,.F.,(4,3,3,3,3,3,3,3,3,3,3,3,3,3,3,3,3,3,3,3,3,3,3,3,3,3,4),(59.6902604184428,
59.7976956859163,59.9067549038113,59.9680769693988,60.0558946929184,60.1436016213319,
60.231220754623,60.3221564535424,60.4096769657224,60.4971845501845,60.5846998606492,
60.6722435513067,60.7598841884968,60.8475823885268,60.9354062067581,60.9587063459788,
61.0465260474693,61.1342344677582,61.2218546088897,61.3094092434533,61.3969287962482,
61.4844339360247,61.5719453161366,61.6595334476544,61.7471595779332,61.8349151107887,
61.9154901076124),.UNSPECIFIED.);
#2208=B_SPLINE_CURVE_WITH_KNOTS('',3,(#45807,#45808,#45809,#45810,#45811,
#45812,#45813,#45814,#45815,#45816,#45817,#45818,#45819,#45820,#45821,#45822,
#45823,#45824,#45825,#45826,#45827,#45828,#45829,#45830,#45831,#45832,#45833,
#45834,#45835,#45836,#45837,#45838,#45839,#45840,#45841,#45842,#45843,#45844,
#45845,#45846,#45847,#45848,#45849,#45850,#45851,#45852,#45853,#45854,#45855,
#45856,#45857,#45858,#45859,#45860,#45861,#45862,#45863,#45864,#45865,#45866,
#45867,#45868,#45869,#45870,#45871,#45872,#45873,#45874,#45875,#45876,#45877,
#45878,#45879,#45880,#45881,#45882,#45883,#45884,#45885,#45886,#45887,#45888,
#45889,#45890,#45891,#45892,#45893,#45894,#45895,#45896,#45897,#45898,#45899,
#45900,#45901,#45902,#45903,#45904,#45905,#45906,#45907,#45908,#45909,#45910,
#45911,#45912,#45913,#45914,#45915,#45916,#45917,#45918,#45919,#45920,#45921,
#45922,#45923,#45924,#45925,#45926,#45927,#45928,#45929,#45930,#45931,#45932,
#45933,#45934,#45935,#45936,#45937,#45938,#45939,#45940,#45941,#45942,#45943,
#45944,#45945,#45946,#45947,#45948,#45949,#45950,#45951,#45952,#45953,#45954,
#45955,#45956,#45957),.UNSPECIFIED.,.F.,.F.,(4,3,3,3,3,3,3,3,3,3,3,3,3,
3,3,3,3,3,3,3,3,3,3,3,3,3,3,3,3,3,3,3,3,3,3,3,3,3,3,3,3,3,3,3,3,3,3,3,3,
3,4),(55.6321437035808,55.719687656161,55.807328619535,55.8950272711616,
55.9828513851517,56.0055594630787,56.0933771867062,56.181084115231,56.2687032486367,
56.3596389475144,56.4471594598163,56.5346670444028,56.6221823549943,56.7097260457809,
56.7973666831025,56.8850648832657,56.9728887016316,56.9961888396587,57.0840065632834,
57.1717134918049,57.2593326252068,57.3502683240858,57.4377888363825,57.5252964209634,
57.6128117315488,57.7003554223288,57.7879960596434,57.875694259799,57.9635180781567,
57.9868182162387,58.0746359401032,58.1623428688656,58.2499620025095,58.3408977012982,
58.4284182138362,58.5159257986579,58.6034411094834,58.6909848005021,58.778625438053,
58.8663236384434,58.954147457033,58.9774475928188,59.0665491959922,59.153511270838,
59.2403929917755,59.3272158146748,59.4179769655576,59.5047630074242,59.5915521894301,
59.6783867677546,59.690260418206),.UNSPECIFIED.);
#2209=B_SPLINE_CURVE_WITH_KNOTS('',3,(#45963,#45964,#45965,#45966,#45967,
#45968,#45969,#45970,#45971,#45972,#45973,#45974,#45975,#45976,#45977,#45978,
#45979,#45980,#45981,#45982,#45983,#45984,#45985,#45986,#45987,#45988,#45989,
#45990,#45991,#45992,#45993,#45994,#45995,#45996,#45997,#45998,#45999,#46000,
#46001,#46002,#46003,#46004,#46005,#46006,#46007,#46008,#46009,#46010,#46011,
#46012,#46013,#46014,#46015,#46016,#46017,#46018,#46019,#46020,#46021,#46022,
#46023,#46024,#46025,#46026,#46027,#46028,#46029,#46030,#46031,#46032,#46033,
#46034,#46035,#46036,#46037,#46038,#46039,#46040,#46041,#46042,#46043,#46044,
#46045,#46046,#46047,#46048,#46049,#46050,#46051,#46052,#46053,#46054,#46055,
#46056,#46057,#46058,#46059,#46060,#46061,#46062,#46063,#46064,#46065,#46066,
#46067,#46068,#46069,#46070,#46071,#46072,#46073,#46074,#46075,#46076,#46077,
#46078,#46079,#46080,#46081,#46082,#46083,#46084,#46085,#46086,#46087,#46088,
#46089,#46090,#46091,#46092,#46093,#46094,#46095,#46096,#46097,#46098,#46099,
#46100,#46101,#46102,#46103,#46104,#46105,#46106,#46107,#46108,#46109,#46110),
 .UNSPECIFIED.,.F.,.F.,(4,3,3,3,3,3,3,3,3,3,3,3,3,3,3,3,3,3,3,3,3,3,3,3,
3,3,3,3,3,3,3,3,3,3,3,3,3,3,3,3,3,3,3,3,3,3,3,3,3,4),(49.3487655641429,
49.4365712254866,49.5014541328574,49.5892718565205,49.676978785081,49.764597918522,
49.8555336173865,49.9430541297232,50.0305617143443,50.11807702497,50.2056207157904,
50.2932613531452,50.3809595533411,50.468783371739,50.4920835094375,50.5799012330941,
50.6676081616481,50.7552272950827,50.8461629939495,50.9336835062799,51.0211910908947,
51.1087064015141,51.1962500923283,51.2838907296771,51.371588929867,51.4594127482591,
51.4827128860175,51.5705306096707,51.6582375382212,51.7458566716522,51.8367923705204,
51.9243128828471,52.0118204674581,52.0993357780737,52.186879468884,52.2745201062289,
52.3622183064147,52.4500421248028,52.4733422625975,52.5604221705999,52.6473917779252,
52.7342748966389,52.8210968702449,52.9078870051233,52.9946666871673,53.0814572897356,
53.1683305097573,53.2552470966057,53.3422944293372,53.4070751108575),
 .UNSPECIFIED.);
#2210=B_SPLINE_CURVE_WITH_KNOTS('',3,(#46111,#46112,#46113,#46114,#46115,
#46116,#46117,#46118,#46119,#46120,#46121,#46122,#46123,#46124,#46125,#46126,
#46127,#46128,#46129,#46130,#46131,#46132,#46133,#46134,#46135,#46136,#46137,
#46138,#46139,#46140,#46141,#46142,#46143,#46144,#46145,#46146,#46147,#46148,
#46149,#46150,#46151,#46152,#46153,#46154,#46155,#46156,#46157,#46158,#46159,
#46160,#46161,#46162,#46163,#46164,#46165,#46166,#46167,#46168,#46169,#46170,
#46171,#46172,#46173,#46174,#46175,#46176,#46177,#46178,#46179,#46180,#46181,
#46182,#46183,#46184,#46185,#46186,#46187,#46188,#46189,#46190,#46191,#46192,
#46193,#46194,#46195),.UNSPECIFIED.,.F.,.F.,(4,3,3,3,3,3,3,3,3,3,3,3,3,
3,3,3,3,3,3,3,3,3,3,3,3,3,3,3,4),(53.4070751110265,53.4639716391775,53.5517893628049,
53.6394962913298,53.7271154247354,53.8180511236132,53.9055716359151,53.9930792205016,
54.080594531093,54.1681382218795,54.2557788592012,54.3434770593642,54.43130087773,
54.4546010157576,54.5424187393821,54.6301256679035,54.7177448013052,54.8086805001843,
54.8962010124809,54.9837085970618,55.0712239076471,55.158767598427,55.2464082357414,
55.3341064358969,55.4219302542547,55.4452303923376,55.533063232291,55.6207748440684,
55.633055807239),.UNSPECIFIED.);
#2211=B_SPLINE_CURVE_WITH_KNOTS('',3,(#46197,#46198,#46199,#46200,#46201,
#46202,#46203,#46204,#46205,#46206,#46207,#46208,#46209,#46210,#46211,#46212,
#46213,#46214,#46215,#46216,#46217,#46218,#46219,#46220,#46221,#46222,#46223,
#46224,#46225,#46226,#46227,#46228,#46229,#46230,#46231,#46232,#46233,#46234,
#46235,#46236,#46237,#46238,#46239,#46240,#46241,#46242,#46243,#46244,#46245,
#46246,#46247,#46248,#46249,#46250,#46251,#46252,#46253,#46254,#46255,#46256,
#46257,#46258,#46259,#46260,#46261,#46262,#46263,#46264,#46265,#46266,#46267,
#46268,#46269,#46270,#46271,#46272,#46273,#46274,#46275),.UNSPECIFIED.,
 .F.,.F.,(4,3,3,3,3,3,3,3,3,3,3,3,3,3,3,3,3,3,3,3,3,3,3,3,3,3,4),(53.4070751110265,
53.4952697145479,53.5834738757,53.6717071431077,53.760051289663,53.8484511190502,
53.937010413905,54.0243007099186,54.1121184335718,54.1998253621224,54.2874444955536,
54.3783801944217,54.4659007067484,54.5534082913595,54.6409236019751,54.7284672927852,
54.8161079301302,54.9038061303163,54.9916299487045,55.0149300864986,55.1027351460802,
55.1904358979913,55.2780531734419,55.3665758059767,55.4540917217808,55.5431177126808,
55.6321437035808),.UNSPECIFIED.);
#2212=B_SPLINE_CURVE_WITH_KNOTS('',3,(#46276,#46277,#46278,#46279,#46280,
#46281,#46282,#46283,#46284,#46285,#46286,#46287,#46288,#46289,#46290,#46291,
#46292,#46293,#46294,#46295,#46296,#46297,#46298,#46299,#46300,#46301,#46302,
#46303,#46304,#46305,#46306,#46307,#46308,#46309,#46310,#46311,#46312,#46313,
#46314,#46315,#46316,#46317,#46318,#46319,#46320,#46321,#46322,#46323,#46324,
#46325,#46326,#46327,#46328,#46329,#46330,#46331,#46332,#46333,#46334,#46335,
#46336,#46337,#46338,#46339,#46340,#46341,#46342,#46343,#46344,#46345,#46346,
#46347,#46348,#46349,#46350,#46351,#46352,#46353,#46354,#46355,#46356,#46357,
#46358,#46359,#46360,#46361,#46362,#46363,#46364,#46365,#46366,#46367,#46368,
#46369,#46370,#46371,#46372,#46373,#46374,#46375,#46376,#46377,#46378,#46379,
#46380,#46381,#46382,#46383,#46384,#46385,#46386,#46387,#46388,#46389,#46390,
#46391,#46392,#46393,#46394,#46395,#46396,#46397,#46398,#46399,#46400,#46401,
#46402,#46403,#46404,#46405,#46406,#46407,#46408,#46409,#46410,#46411,#46412,
#46413,#46414,#46415,#46416,#46417,#46418,#46419,#46420),.UNSPECIFIED.,
 .F.,.F.,(4,3,3,3,3,3,3,3,3,3,3,3,3,3,3,3,3,3,3,3,3,3,3,3,3,3,3,3,3,3,3,
3,3,3,3,3,3,3,3,3,3,3,3,3,3,3,3,3,4),(49.3498290568562,49.4388233251989,
49.5263404755851,49.6138479054887,49.7013662677403,49.7914705017049,49.8791203513828,
49.9704517774906,50.0617832035985,50.149600927258,50.2373078558148,50.324926989252,
50.4158626881178,50.5033832004509,50.5908907850683,50.6784060956903,50.7659497865072,
50.8535904238585,50.9412886240507,51.0291124424452,51.0524125801785,51.1402303038371,
51.227937232393,51.3155563658297,51.4064920646958,51.4940125770281,51.5815201616448,
51.6690354722663,51.7565791630822,51.8442198004329,51.9319180006247,52.0197418190183,
52.0430419567586,52.1308596804217,52.2185666089819,52.3061857424226,52.3971214412871,
52.4846419536239,52.5721495382451,52.6596648488706,52.7472085396905,52.8348491770453,
52.9225473772411,53.0103711956392,53.0336713333386,53.1327118219515,53.2314411213958,
53.3295918554781,53.4070751108119),.UNSPECIFIED.);
#2213=B_SPLINE_CURVE_WITH_KNOTS('',3,(#46426,#46427,#46428,#46429,#46430,
#46431,#46432,#46433,#46434,#46435,#46436,#46437,#46438,#46439,#46440,#46441,
#46442,#46443,#46444,#46445,#46446,#46447,#46448,#46449,#46450,#46451,#46452,
#46453,#46454,#46455,#46456,#46457,#46458,#46459,#46460,#46461,#46462,#46463,
#46464,#46465,#46466,#46467,#46468,#46469,#46470,#46471,#46472,#46473,#46474,
#46475,#46476,#46477,#46478,#46479,#46480,#46481,#46482,#46483,#46484,#46485,
#46486,#46487,#46488,#46489,#46490,#46491,#46492,#46493,#46494,#46495,#46496,
#46497,#46498,#46499,#46500,#46501,#46502,#46503,#46504,#46505,#46506,#46507,
#46508,#46509,#46510,#46511,#46512,#46513,#46514,#46515,#46516,#46517,#46518,
#46519,#46520,#46521,#46522,#46523,#46524,#46525,#46526,#46527,#46528,#46529,
#46530,#46531,#46532,#46533,#46534,#46535,#46536,#46537,#46538,#46539,#46540,
#46541,#46542,#46543,#46544,#46545,#46546,#46547,#46548,#46549,#46550,#46551,
#46552,#46553,#46554,#46555,#46556,#46557,#46558,#46559,#46560,#46561,#46562,
#46563,#46564,#46565,#46566,#46567,#46568,#46569,#46570,#46571,#46572,#46573),
 .UNSPECIFIED.,.F.,.F.,(4,3,3,3,3,3,3,3,3,3,3,3,3,3,3,3,3,3,3,3,3,3,3,3,
3,3,3,3,3,3,3,3,3,3,3,3,3,3,3,3,3,3,3,3,3,3,3,3,3,4),(43.0661059914245,
43.1536163207319,43.2411479365787,43.3287731026926,43.4164494524346,43.5042596073108,
43.5576778733773,43.6454955970374,43.7332025255949,43.8208216590328,43.9117573578984,
43.9992778702322,44.0867854548504,44.1743007654729,44.2618444562906,44.3494850936427,
44.4371832938357,44.5250071122309,44.5483072499573,44.6361249736169,44.7238319021739,
44.8114510356115,44.9023867344772,44.9899072468104,45.077414831428,45.1649301420504,
45.2524738328672,45.3401144702188,45.4278126704114,45.5156364888059,45.5389366265373,
45.6267543501969,45.7144612787539,45.8020804121914,45.8930161110571,45.9805366233903,
46.0680442080077,46.1555595186297,46.2431032094465,46.3307438467979,46.4184420469911,
46.5062658653855,46.5295660031174,46.6186563250424,46.7076259258596,46.7964937259149,
46.8852637004643,46.9739759768119,47.0626512944818,47.1238898038469),
 .UNSPECIFIED.);
#2214=B_SPLINE_CURVE_WITH_KNOTS('',3,(#46574,#46575,#46576,#46577,#46578,
#46579,#46580,#46581,#46582,#46583,#46584,#46585,#46586,#46587,#46588,#46589,
#46590,#46591,#46592,#46593,#46594,#46595,#46596,#46597,#46598,#46599,#46600,
#46601,#46602,#46603,#46604,#46605,#46606,#46607,#46608,#46609,#46610,#46611,
#46612,#46613,#46614,#46615,#46616,#46617,#46618,#46619,#46620,#46621,#46622,
#46623,#46624,#46625,#46626,#46627,#46628,#46629,#46630,#46631,#46632,#46633,
#46634,#46635,#46636,#46637,#46638,#46639,#46640,#46641,#46642,#46643,#46644,
#46645,#46646,#46647,#46648,#46649,#46650,#46651,#46652),.UNSPECIFIED.,
 .F.,.F.,(4,3,3,3,3,3,3,3,3,3,3,3,3,3,3,3,3,3,3,3,3,3,3,3,3,3,4),(47.1238898040446,
47.2229661979578,47.3199017158545,47.420048547776,47.5201953796974,47.6080131033568,
47.6957200319137,47.7833391653511,47.8742748642169,47.96179537655,48.0493029611674,
48.1368182717896,48.2243619626063,48.3120025999576,48.39970080015,48.4875246185445,
48.5108247562774,48.5986518168583,48.6863658889724,48.7739762516002,48.8615284122406,
48.9490430728474,49.0365409029296,49.1240737177127,49.2116250178518,49.2992578827919,
49.3487655641429),.UNSPECIFIED.);
#2215=B_SPLINE_CURVE_WITH_KNOTS('',3,(#46654,#46655,#46656,#46657,#46658,
#46659,#46660,#46661,#46662,#46663,#46664,#46665,#46666,#46667,#46668,#46669,
#46670,#46671,#46672,#46673,#46674,#46675,#46676,#46677,#46678,#46679,#46680,
#46681,#46682,#46683,#46684,#46685,#46686,#46687,#46688,#46689,#46690,#46691,
#46692,#46693,#46694,#46695,#46696,#46697,#46698,#46699,#46700,#46701,#46702,
#46703,#46704,#46705,#46706,#46707,#46708,#46709,#46710,#46711,#46712,#46713,
#46714,#46715,#46716,#46717,#46718,#46719,#46720,#46721,#46722,#46723,#46724,
#46725,#46726,#46727,#46728,#46729,#46730,#46731,#46732,#46733,#46734,#46735),
 .UNSPECIFIED.,.F.,.F.,(4,3,3,3,3,3,3,3,3,3,3,3,3,3,3,3,3,3,3,3,3,3,3,3,
3,3,3,4),(47.1238898040744,47.2112205230592,47.2984421477866,47.3855782233556,
47.4726547355818,47.5596998923596,47.6467348498393,47.7337807519279,47.8209134726714,
47.9080890145168,47.9954065966277,48.0805244504385,48.1683421740981,48.256049102655,
48.3436682360926,48.4346039349583,48.5221244472915,48.6096320319092,48.6971473425314,
48.7846910333482,48.8723316706997,48.9600298708923,49.047853689287,49.0711538270185,
49.1589647608053,49.2466781839562,49.3342970267507,49.3498290568562),
 .UNSPECIFIED.);
#2216=B_SPLINE_CURVE_WITH_KNOTS('',3,(#46736,#46737,#46738,#46739,#46740,
#46741,#46742,#46743,#46744,#46745,#46746,#46747,#46748,#46749,#46750,#46751,
#46752,#46753,#46754,#46755,#46756,#46757,#46758,#46759,#46760,#46761,#46762,
#46763,#46764,#46765,#46766,#46767,#46768,#46769,#46770,#46771,#46772,#46773,
#46774,#46775,#46776,#46777,#46778,#46779,#46780,#46781,#46782,#46783,#46784,
#46785,#46786,#46787,#46788,#46789,#46790,#46791,#46792,#46793,#46794,#46795,
#46796,#46797,#46798,#46799,#46800,#46801,#46802,#46803,#46804,#46805,#46806,
#46807,#46808,#46809,#46810,#46811,#46812,#46813,#46814,#46815,#46816,#46817,
#46818,#46819,#46820,#46821,#46822,#46823,#46824,#46825,#46826,#46827,#46828,
#46829,#46830,#46831,#46832,#46833,#46834,#46835,#46836,#46837,#46838,#46839,
#46840,#46841,#46842,#46843,#46844,#46845,#46846,#46847,#46848,#46849,#46850,
#46851,#46852,#46853,#46854,#46855,#46856,#46857,#46858,#46859,#46860,#46861,
#46862,#46863,#46864,#46865,#46866,#46867,#46868,#46869,#46870,#46871,#46872,
#46873,#46874,#46875,#46876,#46877,#46878,#46879,#46880,#46881,#46882,#46883,
#46884,#46885,#46886),.UNSPECIFIED.,.F.,.F.,(4,3,3,3,3,3,3,3,3,3,3,3,3,
3,3,3,3,3,3,3,3,3,3,3,3,3,3,3,3,3,3,3,3,3,3,3,3,3,3,3,3,3,3,3,3,3,3,3,3,
3,4),(43.0658133366405,43.1273775675383,43.2151952912012,43.3029022197615,
43.3905213532024,43.4814570520669,43.5689775644036,43.6564851490247,43.7440004596504,
43.8315441504708,43.9191847878258,44.0068829880219,44.09470680642,44.1180069441183,
44.205824667777,44.293531596333,44.3811507297696,44.4720864286357,44.559606940968,
44.6471145255847,44.734629836206,44.8221735270219,44.9098141643725,44.9975123645641,
45.0853361829577,45.1086363206984,45.1964540443579,45.2841609729147,45.3717801063521,
45.4627158052179,45.550236317551,45.6377439021685,45.7252592127906,45.8128029036074,
45.9004435409588,45.9881417411512,46.0759655595457,46.0992656972784,46.1870834209386,
46.2747903494961,46.3624094829342,46.4533451817998,46.5408656941336,46.6283732787517,
46.7158885893746,46.8034322801918,46.8910729175439,46.978771117737,47.0665949361321,
47.0898950738584,47.1238898038469),.UNSPECIFIED.);
#2217=B_SPLINE_CURVE_WITH_KNOTS('',3,(#46892,#46893,#46894,#46895,#46896,
#46897,#46898,#46899,#46900,#46901,#46902,#46903,#46904,#46905,#46906,#46907,
#46908,#46909,#46910,#46911,#46912,#46913,#46914,#46915,#46916,#46917,#46918,
#46919,#46920,#46921,#46922,#46923,#46924,#46925,#46926,#46927,#46928,#46929,
#46930,#46931,#46932,#46933,#46934,#46935,#46936,#46937,#46938,#46939,#46940,
#46941,#46942,#46943,#46944,#46945,#46946,#46947,#46948,#46949,#46950,#46951,
#46952,#46953,#46954,#46955,#46956,#46957,#46958,#46959,#46960,#46961,#46962,
#46963,#46964,#46965,#46966,#46967,#46968,#46969,#46970,#46971,#46972,#46973,
#46974,#46975,#46976,#46977,#46978,#46979,#46980,#46981,#46982,#46983,#46984,
#46985,#46986,#46987,#46988,#46989,#46990,#46991,#46992,#46993,#46994,#46995,
#46996,#46997,#46998,#46999,#47000,#47001,#47002,#47003,#47004,#47005,#47006,
#47007,#47008,#47009,#47010,#47011,#47012,#47013,#47014,#47015,#47016,#47017,
#47018,#47019,#47020,#47021,#47022,#47023,#47024,#47025,#47026,#47027,#47028,
#47029,#47030,#47031,#47032,#47033,#47034,#47035,#47036,#47037,#47038,#47039),
 .UNSPECIFIED.,.F.,.F.,(4,3,3,3,3,3,3,3,3,3,3,3,3,3,3,3,3,3,3,3,3,3,3,3,
3,3,3,3,3,3,3,3,3,3,3,3,3,3,3,3,3,3,3,3,3,3,3,3,3,4),(36.7834780455645,
36.8711108657648,36.9586748083193,37.0462007533675,37.1337093627084,37.2212212918609,
37.3087571936796,37.3963879611388,37.4840723275651,37.571887339318,37.6139016138971,
37.7017193375819,37.7894262661645,37.877045399628,37.9679810984841,38.0555016108438,
38.1430091954881,38.2305245061372,38.318068196981,38.4057088343595,38.4934070345791,
38.5812308530006,38.6045309904771,38.6923487141302,38.7800556426807,38.8676747761118,
38.95861047498,39.0461309873066,39.1336385719176,39.2211538825333,39.3086975733436,
39.3963382106886,39.4840364108747,39.5718602292628,39.5951603670572,39.6829780907142,
39.7706850192685,39.8583041527033,39.9492398515701,40.0367603639005,40.1242679485152,
40.2117832591345,40.2993269499484,40.3869675872969,40.4746657874865,40.5624896058781,
40.5857897436372,40.6987530453545,40.809605914287,40.8407044965425),
 .UNSPECIFIED.);
#2218=B_SPLINE_CURVE_WITH_KNOTS('',3,(#47040,#47041,#47042,#47043,#47044,
#47045,#47046,#47047,#47048,#47049,#47050,#47051,#47052,#47053,#47054,#47055,
#47056,#47057,#47058,#47059,#47060,#47061,#47062,#47063,#47064,#47065,#47066,
#47067,#47068,#47069,#47070,#47071,#47072,#47073,#47074,#47075,#47076,#47077,
#47078,#47079,#47080,#47081,#47082,#47083,#47084,#47085,#47086,#47087,#47088,
#47089,#47090,#47091,#47092,#47093,#47094,#47095,#47096,#47097,#47098,#47099,
#47100,#47101,#47102,#47103,#47104,#47105,#47106,#47107,#47108,#47109,#47110,
#47111,#47112,#47113,#47114,#47115,#47116,#47117,#47118,#47119,#47120,#47121),
 .UNSPECIFIED.,.F.,.F.,(4,3,3,3,3,3,3,3,3,3,3,3,3,3,3,3,3,3,3,3,3,3,3,3,
3,3,3,4),(40.8407044966673,40.9273584362615,41.0139637234795,41.1005454082225,
41.1871250286695,41.2737241173095,41.3604139263767,41.4471549251353,41.5340255171282,
41.5764191202172,41.6642368438759,41.7519437724319,41.8395629058685,41.9304986047346,
42.0180191170668,42.1055267016834,42.1930420123047,42.2805857031209,42.3682263404714,
42.4559245406633,42.543748359057,42.5670484967972,42.6548657905408,42.7425763486081,
42.830186907156,42.9177390596702,43.0052579701374,43.0661059914245),
 .UNSPECIFIED.);
#2219=B_SPLINE_CURVE_WITH_KNOTS('',3,(#47123,#47124,#47125,#47126,#47127,
#47128,#47129,#47130,#47131,#47132,#47133,#47134,#47135,#47136,#47137,#47138,
#47139,#47140,#47141,#47142,#47143,#47144,#47145,#47146,#47147,#47148,#47149,
#47150,#47151,#47152,#47153,#47154,#47155,#47156,#47157,#47158,#47159,#47160,
#47161,#47162,#47163,#47164,#47165,#47166,#47167,#47168,#47169,#47170,#47171,
#47172,#47173,#47174,#47175,#47176,#47177,#47178,#47179,#47180,#47181,#47182,
#47183,#47184,#47185,#47186,#47187,#47188,#47189,#47190,#47191,#47192,#47193,
#47194,#47195,#47196,#47197,#47198,#47199,#47200,#47201),.UNSPECIFIED.,
 .F.,.F.,(4,3,3,3,3,3,3,3,3,3,3,3,3,3,3,3,3,3,3,3,3,3,3,3,3,3,4),(40.8407044968387,
40.9448640923073,41.0502373865446,41.1461188143783,41.2339365380315,41.3216434665819,
41.4092626000131,41.5001982988812,41.5877188112079,41.6752263958189,41.7627417064345,
41.8502853972449,41.9379260345899,42.0256242347759,42.1134480531641,42.1367481909583,
42.2245695490687,42.3122792278308,42.3999002309991,42.4874540507318,42.5749722254939,
42.6624754241108,42.7499842994818,42.8375628990347,42.9251792682886,43.012908486006,
43.0658133366405),.UNSPECIFIED.);
#2220=B_SPLINE_CURVE_WITH_KNOTS('',3,(#47202,#47203,#47204,#47205,#47206,
#47207,#47208,#47209,#47210,#47211,#47212,#47213,#47214,#47215,#47216,#47217,
#47218,#47219,#47220,#47221,#47222,#47223,#47224,#47225,#47226,#47227,#47228,
#47229,#47230,#47231,#47232,#47233,#47234,#47235,#47236,#47237,#47238,#47239,
#47240,#47241,#47242,#47243,#47244,#47245,#47246,#47247,#47248,#47249,#47250,
#47251,#47252,#47253,#47254,#47255,#47256,#47257,#47258,#47259,#47260,#47261,
#47262,#47263,#47264,#47265,#47266,#47267,#47268,#47269,#47270,#47271,#47272,
#47273,#47274,#47275,#47276,#47277,#47278,#47279,#47280,#47281,#47282,#47283,
#47284,#47285,#47286,#47287,#47288,#47289,#47290,#47291,#47292,#47293,#47294,
#47295,#47296,#47297,#47298,#47299,#47300,#47301,#47302,#47303,#47304,#47305,
#47306,#47307,#47308,#47309,#47310,#47311,#47312,#47313,#47314,#47315,#47316,
#47317,#47318,#47319,#47320,#47321,#47322,#47323,#47324,#47325,#47326,#47327,
#47328,#47329,#47330,#47331,#47332,#47333,#47334,#47335,#47336,#47337,#47338,
#47339,#47340,#47341,#47342,#47343,#47344,#47345,#47346,#47347,#47348,#47349),
 .UNSPECIFIED.,.F.,.F.,(4,3,3,3,3,3,3,3,3,3,3,3,3,3,3,3,3,3,3,3,3,3,3,3,
3,3,3,3,3,3,3,3,3,3,3,3,3,3,3,3,3,3,3,3,3,3,3,3,3,4),(36.7826586151206,
36.870191370437,36.9578180400284,37.0454965550951,37.1333080021703,37.1836013080582,
37.271419031912,37.3591259606657,37.4467450943021,37.5376807930941,37.6252013056306,
37.7127088904528,37.8002242012807,37.887767892304,37.9754085298621,38.0631067302617,
38.1509305488621,38.1742306846382,38.2620484082612,38.3497553367814,38.4373744701818,
38.5283101690614,38.6158306813579,38.7033382659388,38.7908535765245,38.8783972673053,
38.9660379046209,39.0537361047776,39.1415599231371,39.1648600612182,39.2526777848493,
39.3403847133773,39.4280038467852,39.5189395456618,39.6064600579642,39.6939676425507,
39.7814829531414,39.8690266439265,39.9566672812459,40.0443654814061,40.1321892997682,
40.1554894377982,40.2428859234006,40.3301773559497,40.417384958565,40.5045298835639,
40.5916445939303,40.6787389693886,40.7658659691,40.8407044966673),
 .UNSPECIFIED.);
#2221=B_SPLINE_CURVE_WITH_KNOTS('',3,(#47355,#47356,#47357,#47358,#47359,
#47360,#47361,#47362,#47363,#47364,#47365,#47366,#47367,#47368,#47369,#47370,
#47371,#47372,#47373,#47374,#47375,#47376,#47377,#47378,#47379,#47380,#47381,
#47382,#47383,#47384,#47385,#47386,#47387,#47388,#47389,#47390,#47391,#47392,
#47393,#47394,#47395,#47396,#47397,#47398,#47399,#47400,#47401,#47402,#47403,
#47404,#47405,#47406,#47407,#47408,#47409,#47410,#47411,#47412,#47413,#47414,
#47415,#47416,#47417,#47418,#47419,#47420,#47421,#47422,#47423,#47424,#47425,
#47426,#47427,#47428,#47429,#47430,#47431,#47432,#47433,#47434,#47435,#47436,
#47437,#47438,#47439,#47440,#47441,#47442,#47443,#47444,#47445,#47446,#47447,
#47448,#47449,#47450,#47451,#47452,#47453,#47454,#47455,#47456,#47457,#47458,
#47459,#47460,#47461,#47462,#47463,#47464,#47465,#47466,#47467,#47468,#47469,
#47470,#47471,#47472,#47473,#47474,#47475,#47476,#47477,#47478,#47479,#47480,
#47481,#47482,#47483,#47484,#47485,#47486,#47487,#47488,#47489,#47490,#47491,
#47492,#47493,#47494,#47495,#47496,#47497,#47498,#47499,#47500,#47501,#47502),
 .UNSPECIFIED.,.F.,.F.,(4,3,3,3,3,3,3,3,3,3,3,3,3,3,3,3,3,3,3,3,3,3,3,3,
3,3,3,3,3,3,3,3,3,3,3,3,3,3,3,3,3,3,3,3,3,3,3,3,3,4),(30.4991828394597,
30.5893394086483,30.6794959778369,30.7673136989568,30.8550206249318,30.9426397557483,
31.0335754555819,31.1210959652133,31.208603547104,31.2961188549769,31.383662543025,
31.4713031775926,31.5590013749893,31.6468251905915,31.6701253544169,31.7579430795362,
31.8456500095705,31.9332691445012,32.0242048428132,32.1117253566694,32.1992329428183,
32.2867482549787,32.3742919473387,32.4619325862332,32.5496307879704,32.6374546079003,
32.660754730997,32.7485724544937,32.8362793828887,32.9238985161654,33.0148342150918,
33.1023547272682,33.1898623117308,33.2773776221998,33.3649213128656,33.4525619500699,
33.5402601501174,33.6280839683712,33.651384107577,33.7382200971852,33.8249459927466,
33.9115858331337,33.9981647376494,34.0847124756428,34.1712506292952,34.2578007687998,
34.3444298629828,34.431103797626,34.517896294785,34.5575191892807),
 .UNSPECIFIED.);
#2222=B_SPLINE_CURVE_WITH_KNOTS('',3,(#47503,#47504,#47505,#47506,#47507,
#47508,#47509,#47510,#47511,#47512,#47513,#47514,#47515,#47516,#47517,#47518,
#47519,#47520,#47521,#47522,#47523,#47524,#47525,#47526,#47527,#47528,#47529,
#47530,#47531,#47532,#47533,#47534,#47535,#47536,#47537,#47538,#47539,#47540,
#47541,#47542,#47543,#47544,#47545,#47546,#47547,#47548,#47549,#47550,#47551,
#47552,#47553,#47554,#47555,#47556,#47557,#47558,#47559,#47560,#47561,#47562,
#47563,#47564,#47565,#47566,#47567,#47568,#47569,#47570,#47571,#47572,#47573,
#47574,#47575,#47576,#47577,#47578,#47579,#47580,#47581,#47582,#47583,#47584),
 .UNSPECIFIED.,.F.,.F.,(4,3,3,3,3,3,3,3,3,3,3,3,3,3,3,3,3,3,3,3,3,3,3,3,
3,3,3,4),(34.5575191894877,34.642013484157,34.7298312080111,34.8175381367651,
34.905157270402,34.9960929691939,35.0836134817308,35.1711210665532,35.2586363773814,
35.3461800684051,35.4338207059635,35.5215189063633,35.6093427249641,35.6326428607371,
35.72046058436,35.8081675128802,35.8957866462808,35.9867223451604,36.0742428574568,
36.1617504420376,36.2492657526232,36.3368094434037,36.4244500807191,36.5121482808759,
36.5999720992353,36.6232722373171,36.7110751632043,36.7834780455645),
 .UNSPECIFIED.);
#2223=B_SPLINE_CURVE_WITH_KNOTS('',3,(#47586,#47587,#47588,#47589,#47590,
#47591,#47592,#47593,#47594,#47595,#47596,#47597,#47598,#47599,#47600,#47601,
#47602,#47603,#47604,#47605,#47606,#47607,#47608,#47609,#47610,#47611,#47612,
#47613,#47614,#47615,#47616,#47617,#47618,#47619,#47620,#47621,#47622,#47623,
#47624,#47625,#47626,#47627,#47628,#47629,#47630,#47631,#47632,#47633,#47634,
#47635,#47636,#47637,#47638,#47639,#47640,#47641,#47642,#47643,#47644,#47645,
#47646,#47647,#47648,#47649,#47650,#47651,#47652,#47653,#47654,#47655,#47656,
#47657,#47658,#47659,#47660,#47661,#47662,#47663,#47664,#47665,#47666,#47667),
 .UNSPECIFIED.,.F.,.F.,(4,3,3,3,3,3,3,3,3,3,3,3,3,3,3,3,3,3,3,3,3,3,3,3,
3,3,3,4),(34.5575191894877,34.6452189800071,34.7329127229688,34.8206207358406,
34.9083633412251,34.9962128842659,35.0841247009675,35.1721722075983,35.2023425548981,
35.2901602783952,35.3778672067906,35.4654863400676,35.5564220389939,35.6439425511707,
35.7314501356336,35.818965446103,35.9065091367695,35.9941497739741,36.081847974022,
36.1696717922762,36.1929719314781,36.2807796092091,36.3684824138462,36.4561011791891,
36.5436546837677,36.6311690801989,36.7186812678158,36.7826586151206),
 .UNSPECIFIED.);
#2224=B_SPLINE_CURVE_WITH_KNOTS('',3,(#47668,#47669,#47670,#47671,#47672,
#47673,#47674,#47675,#47676,#47677,#47678,#47679,#47680,#47681,#47682,#47683,
#47684,#47685,#47686,#47687,#47688,#47689,#47690,#47691,#47692,#47693,#47694,
#47695,#47696,#47697,#47698,#47699,#47700,#47701,#47702,#47703,#47704,#47705,
#47706,#47707,#47708,#47709,#47710,#47711,#47712,#47713,#47714,#47715,#47716,
#47717,#47718,#47719,#47720,#47721,#47722,#47723,#47724,#47725,#47726,#47727,
#47728,#47729,#47730,#47731,#47732,#47733,#47734,#47735,#47736,#47737,#47738,
#47739,#47740,#47741,#47742,#47743,#47744,#47745,#47746,#47747,#47748,#47749,
#47750,#47751,#47752,#47753,#47754,#47755,#47756,#47757,#47758,#47759,#47760,
#47761,#47762,#47763,#47764,#47765,#47766,#47767,#47768,#47769,#47770,#47771,
#47772,#47773,#47774,#47775,#47776,#47777,#47778,#47779,#47780,#47781,#47782,
#47783,#47784,#47785,#47786,#47787,#47788,#47789,#47790,#47791,#47792,#47793,
#47794,#47795,#47796,#47797,#47798,#47799,#47800,#47801,#47802,#47803,#47804,
#47805,#47806,#47807,#47808,#47809,#47810,#47811,#47812,#47813,#47814,#47815),
 .UNSPECIFIED.,.F.,.F.,(4,3,3,3,3,3,3,3,3,3,3,3,3,3,3,3,3,3,3,3,3,3,3,3,
3,3,3,3,3,3,3,3,3,3,3,3,3,3,3,3,3,3,3,3,3,3,3,3,3,4),(30.5003021439847,
30.5878639365854,30.6753888404462,30.7628971791787,30.8504096079639,30.9379467798666,
31.0255791880603,31.1132658881075,31.2010823404694,31.239825048578,31.3276427828231,
31.4153497220844,31.5029688663314,31.5939045611847,31.6814250845207,31.7689326801932,
31.8564480019105,31.9439917038511,32.0316323523121,32.1193305636194,32.2071543930516,
32.230454425158,32.3182721485766,32.405979076915,32.4935982101567,32.5845339091044,
32.6720544212997,32.7595620058012,32.8470773163295,32.9346210070747,33.022261644388,
33.1099598445619,33.1977836629669,33.221083801738,33.3089015228609,33.3966084488389,
33.4842275796583,33.5751632794908,33.6626837891255,33.7501913710195,33.8377066788955,
33.9252503669469,34.0128910015178,34.1005891989182,34.1884130145237,34.2117131783181,
34.3130674767607,34.4140179529609,34.5142334906665,34.5575191892756),
 .UNSPECIFIED.);
#2225=B_SPLINE_CURVE_WITH_KNOTS('',3,(#47821,#47822,#47823,#47824,#47825,
#47826,#47827,#47828,#47829,#47830,#47831,#47832,#47833,#47834,#47835,#47836,
#47837,#47838,#47839,#47840,#47841,#47842,#47843,#47844,#47845,#47846,#47847,
#47848,#47849,#47850,#47851,#47852,#47853,#47854,#47855,#47856,#47857,#47858,
#47859,#47860,#47861,#47862,#47863,#47864,#47865,#47866,#47867,#47868,#47869,
#47870,#47871,#47872,#47873,#47874,#47875,#47876,#47877,#47878,#47879,#47880,
#47881,#47882,#47883,#47884,#47885,#47886,#47887,#47888,#47889,#47890,#47891,
#47892,#47893,#47894,#47895,#47896,#47897,#47898,#47899,#47900,#47901,#47902,
#47903,#47904,#47905,#47906,#47907,#47908,#47909,#47910,#47911,#47912,#47913,
#47914,#47915,#47916,#47917,#47918,#47919,#47920,#47921,#47922,#47923,#47924,
#47925,#47926,#47927,#47928,#47929,#47930,#47931,#47932,#47933,#47934,#47935,
#47936,#47937,#47938,#47939,#47940,#47941,#47942,#47943,#47944,#47945,#47946,
#47947,#47948,#47949,#47950,#47951,#47952,#47953,#47954,#47955,#47956,#47957,
#47958,#47959,#47960,#47961,#47962,#47963,#47964,#47965,#47966,#47967,#47968),
 .UNSPECIFIED.,.F.,.F.,(4,3,3,3,3,3,3,3,3,3,3,3,3,3,3,3,3,3,3,3,3,3,3,3,
3,3,3,3,3,3,3,3,3,3,3,3,3,3,3,3,3,3,3,3,3,3,3,3,3,4),(24.2166325387365,
24.3041405728609,24.3916634012199,24.4792764543864,24.5669348543629,24.6547350011096,
24.7357197183568,24.8235372551853,24.9112439941232,24.9988629354017,25.0897987053436,
25.1773190203967,25.2648264061816,25.3523415166308,25.4398850061448,25.5275254415223,
25.6152234391129,25.7030470555221,25.7263490949368,25.8141668925815,25.9018738958755,
25.9894931047059,26.0804287755572,26.1679493644343,26.2554570258878,26.3429724135546,
26.4305161815409,26.5181568958598,26.6058551729917,26.6936790676986,26.7169784715168,
26.8047962015636,26.8925031367968,26.9801222771902,27.0710579735536,27.1585784935006,
27.2460860859628,27.333601404653,27.4211451037538,27.5087857496696,27.5964839586007,
27.6843077859232,27.7076078480968,27.7974230784913,27.8871096033198,27.9766848887918,
28.0661443688007,28.1555356972699,28.2448677617403,28.2743338823081),
 .UNSPECIFIED.);
#2226=B_SPLINE_CURVE_WITH_KNOTS('',3,(#47969,#47970,#47971,#47972,#47973,
#47974,#47975,#47976,#47977,#47978,#47979,#47980,#47981,#47982,#47983,#47984,
#47985,#47986,#47987,#47988,#47989,#47990,#47991,#47992,#47993,#47994,#47995,
#47996,#47997,#47998,#47999,#48000,#48001,#48002,#48003,#48004,#48005,#48006,
#48007,#48008,#48009,#48010,#48011,#48012,#48013,#48014,#48015,#48016,#48017,
#48018,#48019,#48020,#48021,#48022,#48023,#48024,#48025,#48026,#48027,#48028,
#48029,#48030,#48031,#48032,#48033,#48034,#48035,#48036,#48037,#48038,#48039,
#48040,#48041,#48042,#48043,#48044,#48045,#48046,#48047,#48048,#48049,#48050),
 .UNSPECIFIED.,.F.,.F.,(4,3,3,3,3,3,3,3,3,3,3,3,3,3,3,3,3,3,3,3,3,3,3,3,
3,3,3,4),(28.2743338824685,28.3691609662208,28.464391316564,28.5598306389529,
28.6555712299543,28.6982372246769,28.786054958936,28.8737618982115,28.9613810424729,
29.0523167373209,29.1398372606714,29.2273448563586,29.3148601780908,29.4024038800461,
29.4900445285221,29.5777427398441,29.6655665692908,29.6888666012569,29.7766954664342,
29.8670063880624,29.9546150751734,30.0421656114966,30.1296786986772,30.2171750058131,
30.3047012605698,30.3922463238332,30.479860093122,30.4991828394597),
 .UNSPECIFIED.);
#2227=B_SPLINE_CURVE_WITH_KNOTS('',3,(#48052,#48053,#48054,#48055,#48056,
#48057,#48058,#48059,#48060,#48061,#48062,#48063,#48064,#48065,#48066,#48067,
#48068,#48069,#48070,#48071,#48072,#48073,#48074,#48075,#48076,#48077,#48078,
#48079,#48080,#48081,#48082,#48083,#48084,#48085,#48086,#48087,#48088,#48089,
#48090,#48091,#48092,#48093,#48094,#48095,#48096,#48097,#48098,#48099,#48100,
#48101,#48102,#48103,#48104,#48105,#48106,#48107,#48108,#48109,#48110,#48111,
#48112,#48113,#48114,#48115,#48116,#48117,#48118,#48119,#48120,#48121,#48122,
#48123,#48124,#48125,#48126,#48127,#48128,#48129,#48130,#48131,#48132,#48133),
 .UNSPECIFIED.,.F.,.F.,(4,3,3,3,3,3,3,3,3,3,3,3,3,3,3,3,3,3,3,3,3,3,3,3,
3,3,3,4),(28.2743338824878,28.3620520323679,28.4496594845734,28.5371793604949,
28.6273527273603,28.7147750528498,28.8021848308995,28.8896028239389,28.9770497952893,
29.0645937597082,29.1521960301773,29.2399225718329,29.2585662954179,29.3463840254668,
29.434090960702,29.5217101010972,29.6126457974598,29.7001663174082,29.7876739098713,
29.8751892285622,29.9627329276637,30.0503735735801,30.1380717825111,30.2258956098337,
30.249195671998,30.3370125831573,30.4247057975662,30.5003021439847),
 .UNSPECIFIED.);
#2228=B_SPLINE_CURVE_WITH_KNOTS('',3,(#48134,#48135,#48136,#48137,#48138,
#48139,#48140,#48141,#48142,#48143,#48144,#48145,#48146,#48147,#48148,#48149,
#48150,#48151,#48152,#48153,#48154,#48155,#48156,#48157,#48158,#48159,#48160,
#48161,#48162,#48163,#48164,#48165,#48166,#48167,#48168,#48169,#48170,#48171,
#48172,#48173,#48174,#48175,#48176,#48177,#48178,#48179,#48180,#48181,#48182,
#48183,#48184,#48185,#48186,#48187,#48188,#48189,#48190,#48191,#48192,#48193,
#48194,#48195,#48196,#48197,#48198,#48199,#48200,#48201,#48202,#48203,#48204,
#48205,#48206,#48207,#48208,#48209,#48210,#48211,#48212,#48213,#48214,#48215,
#48216,#48217,#48218,#48219,#48220,#48221,#48222,#48223,#48224,#48225,#48226,
#48227,#48228,#48229,#48230,#48231,#48232,#48233,#48234,#48235,#48236,#48237,
#48238,#48239,#48240,#48241,#48242,#48243,#48244,#48245,#48246,#48247,#48248,
#48249,#48250,#48251,#48252,#48253,#48254,#48255,#48256,#48257,#48258,#48259,
#48260,#48261,#48262,#48263,#48264,#48265,#48266,#48267,#48268,#48269,#48270,
#48271,#48272,#48273,#48274,#48275,#48276,#48277,#48278,#48279,#48280,#48281,
#48282,#48283,#48284),.UNSPECIFIED.,.F.,.F.,(4,3,3,3,3,3,3,3,3,3,3,3,3,
3,3,3,3,3,3,3,3,3,3,3,3,3,3,3,3,3,3,3,3,3,3,3,3,3,3,3,3,3,3,3,3,3,3,3,3,
3,4),(24.21616161747,24.3054194125178,24.393235611936,24.4809409946289,
24.5685585625919,24.6594948409052,24.7470137487717,24.8345197172836,24.9220334018862,
25.0095754584884,25.0972144576362,25.1849110153759,25.2727331975642,25.2960487890978,
25.3838670030276,25.4715744261254,25.5591940577416,25.6501295712336,25.7376505876018,
25.8251586775367,25.9126744942071,26.000218691252,26.0878598325432,26.1755585359319,
26.2633828525917,26.2866781656779,26.3744960038223,26.4622030499671,26.5498223039364,
26.6407579587266,26.7282785982027,26.8157863121929,26.9033017542858,26.9908455785413,
27.0784863515969,27.1661846889744,27.254008645693,27.2773075422579,27.3651250792531,
27.4528318183603,27.5404507598101,27.6313865296886,27.7189068449178,27.8064142308805,
27.8939293415086,27.9814728312022,28.0691132667604,28.1568112645317,28.2446348811215,
28.2679369188379,28.2743338823081),.UNSPECIFIED.);
#2229=B_SPLINE_CURVE_WITH_KNOTS('',3,(#48290,#48291,#48292,#48293,#48294,
#48295,#48296,#48297,#48298,#48299,#48300,#48301,#48302,#48303,#48304,#48305,
#48306,#48307,#48308,#48309,#48310,#48311,#48312,#48313,#48314,#48315,#48316,
#48317,#48318,#48319,#48320,#48321,#48322,#48323,#48324,#48325,#48326,#48327,
#48328,#48329,#48330,#48331,#48332,#48333,#48334,#48335,#48336,#48337,#48338,
#48339,#48340,#48341,#48342,#48343,#48344,#48345,#48346,#48347,#48348,#48349,
#48350,#48351,#48352,#48353,#48354,#48355,#48356,#48357,#48358,#48359,#48360,
#48361,#48362,#48363,#48364,#48365,#48366,#48367,#48368,#48369,#48370,#48371),
 .UNSPECIFIED.,.F.,.F.,(4,3,3,3,3,3,3,3,3,3,3,3,3,3,3,3,3,3,3,3,3,3,3,3,
3,3,3,4),(15.7079632679489,15.7946698168415,15.8813534775319,15.9680356344082,
16.0547376665272,16.1415361894612,16.2283857888847,16.3153785783739,16.3803843998776,
16.4682788564933,16.5560621028591,16.6437570426224,16.7346641343518,16.8222586496917,
16.9098394322283,16.9974270480132,17.0850420628687,17.1727521940932,17.2605188998545,
17.3484092437941,17.3710137764576,17.4589624658426,17.5468080500348,17.6345711957375,
17.7222691239434,17.8099293002927,17.8975816624113,17.9331385422654),
 .UNSPECIFIED.);
#2230=B_SPLINE_CURVE_WITH_KNOTS('',3,(#48373,#48374,#48375,#48376,#48377),
 .UNSPECIFIED.,.F.,.F.,(4,1,4),(14.3991256467175,15.3897550232976,15.7079550217499),
 .UNSPECIFIED.);
#2231=B_SPLINE_CURVE_WITH_KNOTS('',3,(#48381,#48382,#48383,#48384,#48385,
#48386,#48387,#48388,#48389,#48390,#48391,#48392,#48393,#48394,#48395,#48396,
#48397,#48398,#48399,#48400,#48401,#48402,#48403,#48404,#48405,#48406,#48407,
#48408,#48409,#48410,#48411,#48412,#48413,#48414,#48415,#48416,#48417,#48418,
#48419,#48420,#48421,#48422,#48423,#48424,#48425,#48426,#48427,#48428,#48429,
#48430,#48431,#48432,#48433,#48434,#48435,#48436,#48437,#48438,#48439,#48440,
#48441,#48442,#48443,#48444),.UNSPECIFIED.,.F.,.F.,(4,3,3,3,3,3,3,3,3,3,
3,3,3,3,3,3,3,3,3,3,3,4),(13.8752087520864,13.9625601789458,14.0498018549144,
14.1369573059842,14.2240519813441,14.3111146099278,14.3981663291118,14.4852282634698,
14.5723751741815,14.6595642711191,14.7468925938367,14.8294259525565,14.9162044274587,
15.0028750659864,15.0910110912051,15.1775387458644,15.2640376537039,15.3505294393131,
15.439887896419,15.5264717573148,15.6172175125258,15.7079632677367),
 .UNSPECIFIED.);
#2232=B_SPLINE_CURVE_WITH_KNOTS('',3,(#48445,#48446,#48447,#48448,#48449,
#48450,#48451,#48452,#48453,#48454,#48455,#48456,#48457,#48458,#48459,#48460,
#48461,#48462,#48463,#48464,#48465,#48466,#48467,#48468,#48469,#48470,#48471,
#48472,#48473,#48474,#48475,#48476,#48477,#48478,#48479,#48480,#48481,#48482,
#48483,#48484,#48485,#48486,#48487,#48488,#48489,#48490,#48491,#48492,#48493,
#48494,#48495,#48496,#48497,#48498,#48499,#48500,#48501,#48502,#48503,#48504,
#48505,#48506,#48507,#48508,#48509,#48510,#48511,#48512,#48513,#48514,#48515,
#48516,#48517,#48518,#48519,#48520,#48521,#48522,#48523,#48524,#48525,#48526),
 .UNSPECIFIED.,.F.,.F.,(4,3,3,3,3,3,3,3,3,3,3,3,3,3,3,3,3,3,3,3,3,3,3,3,
3,3,3,4),(15.7079632679489,15.8200553291365,15.9077800709228,15.9953928439823,
16.082916768368,16.1738877605365,16.2613110318231,16.3487207906136,16.436137793803,
16.523582798485,16.6111246793828,16.6987239645013,16.7864493875845,16.8106847057165,
16.8985189524792,16.9862424441556,17.0738781598958,17.1648076501959,17.2523446830397,
17.3398687358889,17.4274004439648,17.5149604428944,17.6026171724979,17.6903313578386,
17.7781708816529,17.8013140822966,17.8891423167076,17.9338728886362),
 .UNSPECIFIED.);
#2233=B_SPLINE_CURVE_WITH_KNOTS('',3,(#48532,#48533,#48534,#48535,#48536,
#48537,#48538,#48539,#48540,#48541,#48542,#48543,#48544,#48545,#48546,#48547,
#48548,#48549,#48550,#48551,#48552,#48553,#48554,#48555,#48556,#48557,#48558,
#48559,#48560,#48561,#48562,#48563,#48564,#48565,#48566,#48567,#48568,#48569,
#48570,#48571,#48572,#48573,#48574,#48575,#48576,#48577,#48578,#48579,#48580,
#48581,#48582,#48583,#48584,#48585,#48586,#48587,#48588,#48589,#48590,#48591,
#48592,#48593,#48594,#48595,#48596,#48597,#48598,#48599,#48600,#48601,#48602,
#48603,#48604,#48605,#48606,#48607,#48608,#48609,#48610,#48611,#48612,#48613,
#48614,#48615,#48616,#48617,#48618,#48619,#48620,#48621,#48622,#48623,#48624,
#48625,#48626,#48627,#48628),.UNSPECIFIED.,.F.,.F.,(4,3,3,3,3,3,3,3,3,3,
3,3,3,3,3,3,3,3,3,3,3,3,3,3,3,3,3,3,3,3,3,3,4),(64.4958654892591,64.5878117777329,
64.6796687687264,64.7714674489333,64.8632367224699,64.9550002532635,65.0467816942969,
65.1386612087587,65.230593746165,65.32267279102,65.3815388542818,65.4726934888845,
65.5637267792503,65.65466617812,65.7455446050282,65.8363918516251,65.9272325688873,
66.0180913969724,66.1090575805604,66.2000783819247,66.2912666572051,66.3721682308618,
66.4666159606274,66.5609259986622,66.655120074501,66.7492038319741,66.8432231820123,
66.9371975924462,67.0311464863855,67.1251148440193,67.2190914006473,67.3131312555883,
67.3627976074418),.UNSPECIFIED.);
#2234=B_SPLINE_CURVE_WITH_KNOTS('',3,(#48636,#48637,#48638,#48639,#48640,
#48641,#48642,#48643,#48644,#48645,#48646,#48647,#48648,#48649,#48650,#48651,
#48652,#48653,#48654,#48655,#48656,#48657,#48658,#48659,#48660,#48661,#48662,
#48663,#48664,#48665,#48666,#48667,#48668,#48669,#48670,#48671,#48672,#48673,
#48674,#48675,#48676,#48677,#48678,#48679,#48680,#48681,#48682,#48683,#48684,
#48685,#48686,#48687,#48688,#48689,#48690,#48691,#48692,#48693,#48694,#48695,
#48696,#48697,#48698,#48699,#48700,#48701,#48702,#48703,#48704,#48705,#48706,
#48707,#48708,#48709,#48710,#48711,#48712,#48713,#48714,#48715,#48716,#48717,
#48718,#48719,#48720,#48721,#48722,#48723,#48724,#48725,#48726,#48727,#48728,
#48729,#48730,#48731,#48732,#48733,#48734,#48735,#48736,#48737,#48738,#48739,
#48740,#48741,#48742,#48743,#48744,#48745,#48746,#48747,#48748,#48749,#48750,
#48751,#48752,#48753,#48754,#48755,#48756,#48757,#48758,#48759,#48760,#48761,
#48762,#48763,#48764,#48765,#48766,#48767,#48768,#48769,#48770,#48771,#48772,
#48773),.UNSPECIFIED.,.F.,.F.,(4,2,2,2,2,2,2,2,2,2,2,2,2,2,2,2,2,2,2,2,
2,2,2,2,2,2,2,2,2,2,2,2,2,2,2,2,2,2,2,2,2,2,2,2,2,2,2,2,2,2,2,2,2,2,2,2,
2,2,2,2,2,2,2,2,2,2,2,2,4),(-3.8159802817818,-3.80236928524017,-3.75530370914742,
-3.70539731607039,-3.67564854302536,-3.6642164672265,-3.65598257013116,
-3.64735517776101,-3.63386237542377,-3.5789052995534,-3.53734500310367,
-3.51562868770045,-3.50122878070881,-3.49507048308581,-3.49052592416303,
-3.48509252990008,-3.47446797917823,-3.41948587521002,-3.37154346450627,
-3.34261109281059,-3.33134419424982,-3.32318920456458,-3.31461302861812,
-3.30114856638697,-3.24798780205897,-3.19268324308138,-3.17557277292305,
-3.16343646290805,-3.15773838047819,-3.15369957451371,-3.14830620227463,
-3.13797979421403,-3.08043879953883,-3.03375250468406,-3.00528314402067,
-2.99414913468061,-2.98608602511283,-2.97760658199937,-2.96430289364066,
-2.9143495461893,-2.84003610723327,-2.82685565896935,-2.82100429808657,
-2.81657562389555,-2.81113520453627,-2.80065823852271,-2.74667311239221,
-2.69768131291251,-2.66836269863596,-2.65706395587901,-2.64892354714072,
-2.64039685966665,-2.62708318745669,-2.57794967788699,-2.51997090039894,
-2.49423218958418,-2.48677658100827,-2.48202656404952,-2.47722287235016,
-2.46948479101221,-2.44309613626079,-2.37758240781103,-2.33531134436267,
-2.32269382308117,-2.31431656263378,-2.30619527608143,-2.29634492992303,
-2.27167043501862,-2.25604913488483),.UNSPECIFIED.);
#2235=B_SPLINE_CURVE_WITH_KNOTS('',3,(#48779,#48780,#48781,#48782,#48783,
#48784,#48785,#48786,#48787,#48788,#48789,#48790,#48791,#48792,#48793,#48794,
#48795,#48796,#48797,#48798,#48799,#48800,#48801,#48802,#48803,#48804,#48805,
#48806,#48807,#48808,#48809,#48810,#48811,#48812,#48813,#48814,#48815,#48816,
#48817,#48818,#48819,#48820,#48821,#48822,#48823,#48824,#48825,#48826,#48827,
#48828,#48829,#48830,#48831,#48832,#48833,#48834,#48835,#48836,#48837,#48838,
#48839,#48840,#48841,#48842,#48843,#48844,#48845,#48846,#48847,#48848,#48849,
#48850,#48851,#48852,#48853,#48854,#48855,#48856,#48857,#48858,#48859,#48860,
#48861,#48862,#48863,#48864,#48865,#48866,#48867,#48868,#48869,#48870,#48871,
#48872,#48873,#48874,#48875,#48876,#48877,#48878,#48879,#48880,#48881,#48882,
#48883,#48884,#48885,#48886,#48887,#48888,#48889,#48890,#48891,#48892,#48893,
#48894,#48895,#48896,#48897,#48898,#48899,#48900,#48901,#48902,#48903,#48904,
#48905,#48906,#48907,#48908,#48909,#48910,#48911,#48912,#48913,#48914,#48915,
#48916,#48917,#48918,#48919,#48920,#48921,#48922,#48923,#48924,#48925,#48926,
#48927,#48928,#48929,#48930,#48931,#48932,#48933,#48934,#48935,#48936,#48937,
#48938,#48939,#48940,#48941,#48942,#48943,#48944,#48945,#48946,#48947,#48948,
#48949,#48950,#48951,#48952,#48953,#48954,#48955,#48956),.UNSPECIFIED.,
 .F.,.F.,(4,2,2,2,2,2,2,2,2,2,2,2,2,2,2,2,2,2,2,2,2,2,2,2,2,2,2,2,2,2,2,
2,2,2,2,2,2,2,2,2,2,2,2,2,2,2,2,2,2,2,2,2,2,2,2,2,2,2,2,2,2,2,2,2,2,2,2,
2,2,2,2,2,2,2,2,2,2,2,2,2,2,2,2,2,2,2,2,2,4),(-2.01524637946625,-1.97117235359194,
-1.94754198410681,-1.94008740470034,-1.93581638535977,-1.9311412347247,
-1.9240042022512,-1.90147334034537,-1.85704954887112,-1.79532974948722,
-1.7794104985436,-1.77026883070907,-1.76231858115783,-1.75237729671238,
-1.7318167846165,-1.70352017593473,-1.6379760780529,-1.61157416540518,-1.60386591515836,
-1.599071971706,-1.59433952209767,-1.58690611473692,-1.56122832853527,-1.50360611181347,
-1.45354024952445,-1.44020574428231,-1.43169081758819,-1.42358066511926,
-1.41235683362176,-1.38346177215334,-1.33563610667739,-1.28006147076001,
-1.26962145811798,-1.26419190422336,-1.25970354180774,-1.25377248259357,
-1.24026025600279,-1.2203710498627,-1.13927393268819,-1.11223801117913,
-1.10100549967706,-1.09296737951648,-1.08446141052123,-1.07120127978754,
-1.0184293339982,-0.942861807503496,-0.932758346196491,-0.927394150303743,
-0.922883724142963,-0.916822306019369,-0.902590749912535,-0.881187682739607,
-0.831583136723827,-0.780875674958192,-0.767517114608159,-0.758981876333513,
-0.750847493623583,-0.739580408237012,-0.710495026366432,-0.66218164615411,
-0.607297393457773,-0.596820714586557,-0.591380744981763,-0.58695263940325,
-0.58110226227966,-0.567925162310321,-0.493673847496277,-0.443617250335225,
-0.430310419772939,-0.421831183565596,-0.41376984617743,-0.40264082068429,
-0.374198582348755,-0.327584026627377,-0.270017981651149,-0.259699110258334,
-0.25430785025771,-0.250269655836963,-0.244571093057724,-0.232428975475039,
-0.215304479889232,-0.159910383024156,-0.106818477230286,-0.0933557651507457,
-0.0847809752165488,-0.0766275291918341,-0.0685599868093,-0.0576300795599785,
-0.00100809160743357),.UNSPECIFIED.);
#2236=B_SPLINE_CURVE_WITH_KNOTS('',3,(#48957,#48958,#48959,#48960,#48961,
#48962,#48963,#48964,#48965,#48966,#48967,#48968,#48969,#48970,#48971,#48972),
 .UNSPECIFIED.,.F.,.F.,(4,3,3,3,3,4),(64.1406906932476,64.2573846340332,
64.3763846980835,64.3909094777018,64.4829991505123,64.4958654892591),
 .UNSPECIFIED.);
#2237=B_SPLINE_CURVE_WITH_KNOTS('',3,(#48973,#48974,#48975,#48976,#48977,
#48978,#48979,#48980,#48981,#48982,#48983,#48984,#48985,#48986,#48987,#48988,
#48989,#48990,#48991,#48992,#48993,#48994,#48995,#48996,#48997,#48998,#48999,
#49000,#49001,#49002,#49003,#49004,#49005,#49006,#49007,#49008,#49009,#49010,
#49011,#49012,#49013,#49014,#49015,#49016,#49017,#49018,#49019,#49020,#49021,
#49022,#49023,#49024,#49025,#49026,#49027,#49028,#49029,#49030,#49031,#49032,
#49033,#49034,#49035,#49036,#49037,#49038,#49039,#49040,#49041,#49042,#49043,
#49044,#49045,#49046,#49047,#49048,#49049,#49050,#49051,#49052,#49053,#49054,
#49055,#49056,#49057,#49058,#49059,#49060,#49061,#49062,#49063,#49064,#49065,
#49066,#49067,#49068,#49069,#49070,#49071,#49072,#49073,#49074,#49075,#49076,
#49077,#49078,#49079,#49080,#49081,#49082,#49083,#49084,#49085,#49086,#49087,
#49088,#49089,#49090,#49091,#49092,#49093,#49094,#49095,#49096,#49097,#49098,
#49099,#49100,#49101,#49102,#49103,#49104,#49105,#49106,#49107,#49108,#49109,
#49110,#49111,#49112,#49113,#49114,#49115,#49116,#49117,#49118,#49119,#49120,
#49121,#49122,#49123,#49124,#49125,#49126,#49127,#49128,#49129,#49130,#49131,
#49132,#49133,#49134,#49135,#49136,#49137,#49138,#49139,#49140,#49141,#49142,
#49143,#49144,#49145,#49146,#49147,#49148,#49149,#49150,#49151,#49152,#49153,
#49154,#49155,#49156,#49157,#49158,#49159,#49160,#49161,#49162),
 .UNSPECIFIED.,.F.,.F.,(4,2,2,2,2,2,2,2,2,2,2,2,2,2,2,2,2,2,2,2,2,2,2,2,
2,2,2,2,2,2,2,2,2,2,2,2,2,2,2,2,2,2,2,2,2,2,2,2,2,2,2,2,2,2,2,2,2,2,2,2,
2,2,2,2,2,2,2,2,2,2,2,2,2,2,2,2,2,2,2,2,2,2,2,2,2,2,2,2,2,2,2,2,2,2,4),
(-2.25604913488483,-2.18785682196863,-2.1677665984532,-2.15415633770891,
-2.14820831459379,-2.14371811797818,-2.13829994497247,-2.12758962218332,
-2.07535601862155,-2.02532397048771,-1.99567874743702,-1.9843558171834,
-1.9762281176329,-1.96774225382847,-1.95455337705862,-1.90821016361135,
-1.89800167760216,-1.84039253906393,-1.82020439264348,-1.81312844983984,
-1.8089297603779,-1.80417554470848,-1.79665363768787,-1.76999657250674,
-1.70731917786023,-1.66295132923247,-1.64987267443735,-1.6414034449495,
-1.63325244010934,-1.62183055829978,-1.59145440354981,-1.51186515502239,
-1.4850327587046,-1.47727675810207,-1.47247099490959,-1.46774153435521,
-1.46033774641746,-1.43504432541337,-1.37927263921278,-1.32705473382731,
-1.31366328842835,-1.30513166470767,-1.29701900053342,-1.28581315536973,
-1.2570980580444,-1.20980433332651,-1.15335997391034,-1.14295942718709,
-1.1375357734097,-1.13304479263005,-1.12709928463253,-1.11350267226373,
-1.09343690594463,-1.00996122365891,-0.985048121694844,-0.97516537845347,
-0.96703905858256,-0.958678447450702,-0.946129553874666,-0.904674580323758,
-0.863705539291906,-0.813492846415116,-0.80488680199612,-0.79990010068119,
-0.795294144258878,-0.788513475771654,-0.769122775692711,-0.734859512674769,
-0.657191088238776,-0.642073170891989,-0.633186072483549,-0.625198026828659,
-0.614849270916213,-0.591903637284072,-0.558745703553591,-0.494445285291431,
-0.474004190800517,-0.466894047003265,-0.462687188973309,-0.457940424847267,
-0.450451651684341,-0.42417839347516,-0.363549730670916,-0.316901444116721,
-0.303730372528516,-0.295244402092222,-0.287108117489695,-0.275758635725873,
-0.245937237329409,-0.195376087353446,-0.143900431522099,-0.133244640209012,
-0.127835451999951,-0.123343133097485,-0.121334274483195),.UNSPECIFIED.);
#2238=B_SPLINE_CURVE_WITH_KNOTS('',3,(#49167,#49168,#49169,#49170,#49171,
#49172,#49173,#49174,#49175,#49176,#49177,#49178,#49179,#49180,#49181,#49182,
#49183,#49184,#49185,#49186,#49187,#49188,#49189,#49190,#49191,#49192,#49193,
#49194,#49195,#49196,#49197,#49198,#49199,#49200,#49201,#49202,#49203,#49204,
#49205,#49206,#49207,#49208,#49209,#49210,#49211,#49212,#49213,#49214,#49215,
#49216,#49217,#49218,#49219,#49220,#49221,#49222,#49223,#49224,#49225,#49226,
#49227,#49228,#49229,#49230,#49231,#49232,#49233,#49234,#49235,#49236,#49237,
#49238,#49239,#49240,#49241,#49242,#49243,#49244,#49245,#49246,#49247,#49248,
#49249,#49250,#49251,#49252,#49253,#49254,#49255,#49256,#49257,#49258,#49259,
#49260,#49261,#49262,#49263,#49264,#49265,#49266,#49267,#49268,#49269,#49270,
#49271,#49272,#49273,#49274,#49275,#49276,#49277,#49278,#49279,#49280,#49281,
#49282,#49283,#49284,#49285,#49286,#49287,#49288,#49289,#49290,#49291,#49292,
#49293,#49294,#49295,#49296,#49297,#49298,#49299,#49300,#49301,#49302,#49303,
#49304,#49305,#49306,#49307,#49308,#49309,#49310,#49311,#49312,#49313,#49314,
#49315,#49316,#49317,#49318,#49319,#49320,#49321,#49322,#49323,#49324,#49325,
#49326,#49327,#49328,#49329,#49330,#49331,#49332,#49333,#49334,#49335,#49336,
#49337,#49338,#49339,#49340,#49341,#49342,#49343,#49344,#49345,#49346,#49347,
#49348,#49349,#49350,#49351,#49352,#49353,#49354,#49355,#49356,#49357,#49358,
#49359,#49360),.UNSPECIFIED.,.F.,.F.,(4,2,2,2,2,2,2,2,2,2,2,2,2,2,2,2,2,
2,2,2,2,2,2,2,2,2,2,2,2,2,2,2,2,2,2,2,2,2,2,2,2,2,2,2,2,2,2,2,2,2,2,2,2,
2,2,2,2,2,2,2,2,2,2,2,2,2,2,2,2,2,2,2,2,2,2,2,2,2,2,2,2,2,2,2,2,2,2,2,2,
2,2,2,2,2,2,2,4),(-4.14968971221015,-4.14613951770191,-4.13262163571353,
-4.12406566573447,-4.11596862875263,-4.10484711285268,-4.07852895524875,
-3.99670216147919,-3.97676939988255,-3.96323638410418,-3.95730208629117,
-3.95281245028536,-3.94738170196693,-3.93661443909146,-3.89098960514216,
-3.85089696882983,-3.82210862915545,-3.80129997335259,-3.7913166767727,
-3.78343838033831,-3.7743585808226,-3.75871950313345,-3.68813361491474,
-3.63256265076525,-3.62386903190368,-3.61886365513924,-3.61431976026846,
-3.60870090187122,-3.59459458900767,-3.53195385063498,-3.51759732217433,
-3.48696491482241,-3.46523327149188,-3.45508900339031,-3.4471237372455,
-3.43812138120597,-3.42284367255486,-3.34813929946971,-3.31229871400597,
-3.29237302873156,-3.28552826973011,-3.28091088650699,-3.27594737989848,
-3.26744946343817,-3.22429086396982,-3.16499709098304,-3.13258183956557,
-3.12091628752857,-3.11272446056812,-3.10530952507597,-3.09530962117868,
-3.06916829712429,-2.98922582993614,-2.96803754036205,-2.95390921989029,
-2.94787581874199,-2.94337753239159,-2.9380166087374,-2.92791376940292,
-2.86711668424234,-2.8224084221447,-2.79463084720547,-2.78355320158664,
-2.77546252641307,-2.76689014345078,-2.75329564111982,-2.69304424079818,
-2.64395541033935,-2.62020570696751,-2.61294807566401,-2.6082498829655,
-2.60400461130362,-2.59668223221427,-2.57437218158575,-2.51182753723812,
-2.47896322475052,-2.45615794159679,-2.44583366787227,-2.43785007869641,
-2.4289533173454,-2.41378162372494,-2.33662853949002,-2.28623673404108,
-2.27765066894587,-2.27266847580768,-2.26811427010957,-2.26136667566018,
-2.24365075162703,-2.18403519633135,-2.13587825420236,-2.11915654499046,
-2.10898295059721,-2.10101446510982,-2.09202920817599,-2.07643016420023,
-2.02613671851317,-2.01524637946625),.UNSPECIFIED.);
#2239=B_SPLINE_CURVE_WITH_KNOTS('',3,(#49362,#49363,#49364,#49365,#49366,
#49367,#49368,#49369,#49370,#49371),.UNSPECIFIED.,.F.,.F.,(4,2,2,2,4),(-0.121334274483195,
-0.117378401436383,-0.103666538849867,-0.0833593375923389,-0.000975325102178241),
 .UNSPECIFIED.);
#2240=B_SPLINE_CURVE_WITH_KNOTS('',3,(#49372,#49373,#49374,#49375,#49376,
#49377,#49378,#49379,#49380,#49381,#49382,#49383,#49384,#49385,#49386,#49387,
#49388,#49389,#49390,#49391,#49392,#49393,#49394,#49395,#49396,#49397,#49398,
#49399,#49400,#49401,#49402,#49403,#49404,#49405,#49406,#49407,#49408,#49409,
#49410,#49411,#49412,#49413,#49414,#49415,#49416,#49417,#49418,#49419,#49420,
#49421,#49422,#49423,#49424,#49425,#49426,#49427,#49428,#49429,#49430,#49431,
#49432,#49433,#49434,#49435,#49436,#49437,#49438,#49439,#49440,#49441,#49442,
#49443,#49444,#49445,#49446,#49447,#49448,#49449,#49450,#49451,#49452,#49453,
#49454,#49455,#49456,#49457,#49458,#49459,#49460,#49461,#49462,#49463,#49464,
#49465,#49466,#49467,#49468,#49469,#49470,#49471,#49472,#49473,#49474,#49475,
#49476,#49477,#49478,#49479,#49480,#49481,#49482,#49483,#49484,#49485,#49486,
#49487,#49488,#49489,#49490,#49491,#49492,#49493,#49494,#49495,#49496,#49497,
#49498,#49499,#49500,#49501,#49502,#49503,#49504,#49505,#49506,#49507,#49508,
#49509,#49510,#49511,#49512,#49513,#49514,#49515,#49516,#49517,#49518,#49519,
#49520,#49521,#49522,#49523,#49524,#49525,#49526,#49527,#49528,#49529,#49530,
#49531,#49532,#49533,#49534,#49535,#49536,#49537,#49538,#49539,#49540,#49541,
#49542,#49543,#49544,#49545,#49546,#49547,#49548,#49549),.UNSPECIFIED.,
 .F.,.F.,(4,2,2,2,2,2,2,2,2,2,2,2,2,2,2,2,2,2,2,2,2,2,2,2,2,2,2,2,2,2,2,
2,2,2,2,2,2,2,2,2,2,2,2,2,2,2,2,2,2,2,2,2,2,2,2,2,2,2,2,2,2,2,2,2,2,2,2,
2,2,2,2,2,2,2,2,2,2,2,2,2,2,2,2,2,2,2,2,2,4),(-4.27069253146465,-4.25382227564401,
-4.2410426801416,-4.23324808460416,-4.22556529108036,-4.21681634818942,
-4.20237008358997,-4.1342605407797,-4.0923109481809,-4.07047931789365,-4.06341753057571,
-4.05875809547891,-4.05447147190329,-4.04693624734976,-4.0224311118733,
-3.96189731402034,-3.91320956523195,-3.90015976209251,-3.89169779047831,
-3.88363791998101,-3.87226738797422,-3.84442414769242,-3.76445167164648,
-3.74466127208302,-3.73119589173919,-3.72527210468108,-3.72078221765012,
-3.71534109709162,-3.70452486961746,-3.6591753402215,-3.61948628985693,
-3.57591319779884,-3.56319850511883,-3.55480381666027,-3.5467000203529,
-3.53691322525324,-3.51263421085097,-3.42838703269747,-3.40827009117478,
-3.39464748699942,-3.38869703966519,-3.38420502666613,-3.37878347287155,
-3.36806797283986,-3.32458313858687,-3.2872941225708,-3.2555937538825,-3.23334059738502,
-3.22310601583075,-3.21512974845548,-3.20617720020493,-3.19074416813872,
-3.11575537148139,-3.08005534121769,-3.06017455323844,-3.05333398191888,
-3.04871648592878,-3.04374955702078,-3.0352395509004,-2.99017113554231,
-2.91447268163651,-2.89515239069106,-2.8854374846631,-2.87827014713962,
-2.86924687178384,-2.85387762247084,-2.78001722702751,-2.72705236436821,
-2.71843083651246,-2.71344005991677,-2.70888778972161,-2.70215684585707,
-2.68456422902658,-2.61732795283435,-2.5668973474104,-2.55375073916023,
-2.54526876573048,-2.53721964486301,-2.52591494163477,-2.49849966893336,
-2.41799983763994,-2.39816635687508,-2.38467993045638,-2.37875235869401,
-2.37426194619358,-2.36882306565325,-2.35835171448144,-2.30327850121938,
-2.25593923477587),.UNSPECIFIED.);
#2241=B_SPLINE_CURVE_WITH_KNOTS('',3,(#49555,#49556,#49557,#49558,#49559,
#49560,#49561,#49562,#49563,#49564,#49565,#49566,#49567,#49568,#49569,#49570,
#49571,#49572,#49573,#49574,#49575,#49576,#49577,#49578,#49579,#49580,#49581,
#49582,#49583,#49584,#49585,#49586,#49587,#49588,#49589,#49590,#49591,#49592,
#49593,#49594,#49595,#49596,#49597,#49598,#49599,#49600,#49601,#49602,#49603,
#49604,#49605,#49606,#49607,#49608,#49609,#49610,#49611,#49612,#49613,#49614,
#49615,#49616,#49617,#49618,#49619,#49620,#49621,#49622,#49623,#49624,#49625,
#49626,#49627,#49628,#49629,#49630,#49631,#49632,#49633,#49634,#49635,#49636,
#49637,#49638,#49639,#49640,#49641,#49642,#49643,#49644,#49645,#49646,#49647,
#49648,#49649,#49650,#49651,#49652,#49653,#49654,#49655,#49656,#49657,#49658,
#49659,#49660,#49661,#49662,#49663,#49664,#49665,#49666,#49667,#49668,#49669,
#49670,#49671,#49672,#49673,#49674,#49675,#49676,#49677,#49678,#49679,#49680,
#49681,#49682,#49683,#49684,#49685,#49686,#49687,#49688,#49689,#49690,#49691,
#49692,#49693,#49694,#49695,#49696,#49697,#49698,#49699,#49700,#49701,#49702,
#49703,#49704,#49705,#49706,#49707,#49708,#49709,#49710,#49711,#49712,#49713,
#49714,#49715,#49716,#49717,#49718,#49719,#49720,#49721,#49722,#49723,#49724,
#49725,#49726,#49727,#49728,#49729,#49730,#49731,#49732),.UNSPECIFIED.,
 .F.,.F.,(4,2,2,2,2,2,2,2,2,2,2,2,2,2,2,2,2,2,2,2,2,2,2,2,2,2,2,2,2,2,2,
2,2,2,2,2,2,2,2,2,2,2,2,2,2,2,2,2,2,2,2,2,2,2,2,2,2,2,2,2,2,2,2,2,2,2,2,
2,2,2,2,2,2,2,2,2,2,2,2,2,2,2,2,2,2,2,2,2,4),(-2.01502246037067,-1.98169731450777,
-1.90173558673302,-1.88534179650667,-1.87610017858487,-1.86815977443268,
-1.8583557727864,-1.83855078644552,-1.81170282860945,-1.76948827394314,
-1.71888939864403,-1.71026383110115,-1.70527244185678,-1.70066801345141,
-1.69389737184125,-1.67459033691109,-1.64056994241434,-1.56243214447281,
-1.54737291312349,-1.53849769038798,-1.53050669467853,-1.52013472071676,
-1.49704903882493,-1.46359242696767,-1.39754179029721,-1.37884478289928,
-1.37195955880564,-1.36737994953238,-1.36244468686577,-1.35408040494002,
-1.31268467923658,-1.22717780313807,-1.21155281906764,-1.20247550035619,
-1.19531609855523,-1.18567806575067,-1.16676364345449,-1.12027345163667,
-1.06242059062369,-1.04258023954654,-1.03554531205344,-1.0313521582367,
-1.02658668181786,-1.01900971328711,-0.991672189360913,-0.925070766363241,
-0.88479634268939,-0.872029014353895,-0.863624830605795,-0.85543617843434,
-0.843789291295884,-0.811533743398526,-0.752825065341529,-0.708952106137622,
-0.700450621704578,-0.695486224320385,-0.690869081385854,-0.684026076462995,
-0.66411747655555,-0.628328069107437,-0.553461921603732,-0.538014259570234,
-0.529060042405756,-0.521086336756685,-0.510860659524785,-0.488650609722859,
-0.457039276156101,-0.419706029191237,-0.376226435046764,-0.365509402071225,
-0.360088356969347,-0.355597561360689,-0.349649667012437,-0.336037089967,
-0.315937113439235,-0.231966595891586,-0.207458658425235,-0.197637940992484,
-0.189527377553755,-0.181147286875157,-0.168497956766223,-0.125752974196045,
-0.0645402929535018,-0.034851635230439,-0.026907861210298,-0.0220637319845611,
-0.0178656474137155,-0.0131614607899771,-0.000969412843418152),
 .UNSPECIFIED.);
#2242=B_SPLINE_CURVE_WITH_KNOTS('',3,(#49733,#49734,#49735,#49736,#49737,
#49738),.UNSPECIFIED.,.F.,.F.,(4,2,4),(-4.27034593055923,-4.20600833774116,
-4.14968971221015),.UNSPECIFIED.);
#2243=B_SPLINE_CURVE_WITH_KNOTS('',3,(#49739,#49740,#49741,#49742,#49743,
#49744,#49745,#49746,#49747,#49748,#49749,#49750,#49751,#49752,#49753,#49754,
#49755,#49756,#49757,#49758,#49759,#49760,#49761,#49762,#49763,#49764,#49765,
#49766,#49767,#49768,#49769,#49770,#49771,#49772,#49773,#49774,#49775,#49776,
#49777,#49778,#49779,#49780,#49781,#49782,#49783,#49784,#49785,#49786,#49787,
#49788,#49789,#49790,#49791,#49792,#49793,#49794,#49795,#49796,#49797,#49798,
#49799,#49800,#49801,#49802,#49803,#49804,#49805,#49806,#49807,#49808,#49809,
#49810,#49811,#49812,#49813,#49814,#49815,#49816,#49817,#49818,#49819,#49820,
#49821,#49822,#49823,#49824,#49825,#49826,#49827,#49828,#49829,#49830,#49831,
#49832,#49833,#49834,#49835,#49836,#49837,#49838,#49839,#49840,#49841,#49842,
#49843,#49844,#49845,#49846,#49847,#49848,#49849,#49850,#49851,#49852,#49853,
#49854,#49855,#49856,#49857,#49858,#49859,#49860,#49861,#49862,#49863,#49864,
#49865,#49866,#49867,#49868,#49869,#49870,#49871,#49872,#49873,#49874,#49875,
#49876,#49877,#49878,#49879,#49880,#49881,#49882,#49883,#49884,#49885,#49886,
#49887,#49888,#49889,#49890,#49891,#49892,#49893,#49894,#49895,#49896,#49897,
#49898,#49899,#49900,#49901,#49902,#49903,#49904,#49905,#49906,#49907,#49908,
#49909,#49910,#49911,#49912,#49913,#49914,#49915,#49916,#49917,#49918,#49919,
#49920,#49921,#49922,#49923,#49924,#49925,#49926,#49927,#49928,#49929,#49930),
 .UNSPECIFIED.,.F.,.F.,(4,2,2,2,2,2,2,2,2,2,2,2,2,2,2,2,2,2,2,2,2,2,2,2,
2,2,2,2,2,2,2,2,2,2,2,2,2,2,2,2,2,2,2,2,2,2,2,2,2,2,2,2,2,2,2,2,2,2,2,2,
2,2,2,2,2,2,2,2,2,2,2,2,2,2,2,2,2,2,2,2,2,2,2,2,2,2,2,2,2,2,2,2,2,2,2,4),
(-2.25593923477587,-2.2550800414557,-2.22605005401396,-2.21480174339244,
-2.20668152750578,-2.19816253331147,-2.18483473372666,-2.13516675811743,
-2.06929076115446,-2.05041220285426,-2.04350196827854,-2.03891736272286,
-2.03398959635608,-2.02566181201838,-1.98528561620682,-1.89800555339563,
-1.88256410357354,-1.87361036234211,-1.86563524958772,-1.85540522181267,
-1.83317465503591,-1.80152277322564,-1.76422626907087,-1.72075189506879,
-1.71003883794084,-1.70461811566501,-1.70012658756494,-1.69417641947781,
-1.68055333710693,-1.66043258711796,-1.57620231475946,-1.55188450553228,
-1.54209229075394,-1.53398790637176,-1.52559653843235,-1.51289470815902,
-1.46946940876894,-1.42971453814165,-1.38434994422378,-1.37353353023355,
-1.36809282923244,-1.36360363996874,-1.35768114283175,-1.34422045505091,
-1.32443675254983,-1.2445998529737,-1.21661712545391,-1.20522620707125,
-1.19716382796879,-1.18870956817852,-1.1756931807367,-1.12753268451687,
-1.06887401673824,-1.0423783162708,-1.03465305628698,-1.02985577760556,
-1.0251228962551,-1.01769861701944,-0.992161626551961,-0.935222833816181,
-0.884409072451034,-0.871050988798573,-0.862527190624263,-0.854412603354564,
-0.843188781145115,-0.814328499114182,-0.766611290749401,-0.71088080989809,
-0.700446240037341,-0.695015849579098,-0.690525947368874,-0.684590488731045,
-0.671051976519683,-0.651106350960472,-0.569203907306135,-0.542906860628762,
-0.531786573129396,-0.523689487113011,-0.515132634773628,-0.501611462487577,
-0.441578622240588,-0.376801212678062,-0.364645841538989,-0.358952947263029,
-0.354473714820259,-0.348837072030278,-0.336988373591138,-0.32041252621164,
-0.26853063150797,-0.211863930273245,-0.19824643768441,-0.189669715927705,
-0.181581929282899,-0.170519406312706,-0.142846285350935,-0.121312221259422),
 .UNSPECIFIED.);
#2244=B_SPLINE_CURVE_WITH_KNOTS('',3,(#49935,#49936,#49937,#49938,#49939,
#49940,#49941,#49942,#49943,#49944,#49945,#49946,#49947,#49948,#49949,#49950,
#49951,#49952,#49953,#49954,#49955,#49956,#49957,#49958,#49959,#49960,#49961,
#49962,#49963,#49964,#49965,#49966,#49967,#49968,#49969,#49970,#49971,#49972,
#49973,#49974,#49975,#49976,#49977,#49978,#49979,#49980,#49981,#49982,#49983,
#49984,#49985,#49986,#49987,#49988,#49989,#49990,#49991,#49992,#49993,#49994,
#49995,#49996,#49997,#49998,#49999,#50000,#50001,#50002,#50003,#50004,#50005,
#50006,#50007,#50008,#50009,#50010,#50011,#50012,#50013,#50014,#50015,#50016,
#50017,#50018,#50019,#50020,#50021,#50022,#50023,#50024,#50025,#50026,#50027,
#50028,#50029,#50030,#50031,#50032,#50033,#50034,#50035,#50036,#50037,#50038,
#50039,#50040,#50041,#50042,#50043,#50044,#50045,#50046,#50047,#50048,#50049,
#50050,#50051,#50052,#50053,#50054,#50055,#50056,#50057,#50058,#50059,#50060,
#50061,#50062,#50063,#50064,#50065,#50066,#50067,#50068,#50069,#50070,#50071,
#50072,#50073,#50074,#50075,#50076,#50077,#50078,#50079,#50080,#50081,#50082,
#50083,#50084,#50085,#50086,#50087,#50088,#50089,#50090,#50091,#50092,#50093,
#50094,#50095,#50096,#50097,#50098,#50099,#50100,#50101,#50102,#50103,#50104,
#50105,#50106,#50107,#50108,#50109,#50110,#50111,#50112,#50113,#50114,#50115,
#50116,#50117,#50118,#50119,#50120,#50121,#50122,#50123,#50124,#50125,#50126,
#50127,#50128,#50129,#50130),.UNSPECIFIED.,.F.,.F.,(4,2,2,2,2,2,2,2,2,2,
2,2,2,2,2,2,2,2,2,2,2,2,2,2,2,2,2,2,2,2,2,2,2,2,2,2,2,2,2,2,2,2,2,2,2,2,
2,2,2,2,2,2,2,2,2,2,2,2,2,2,2,2,2,2,2,2,2,2,2,2,2,2,2,2,2,2,2,2,2,2,2,2,
2,2,2,2,2,2,2,2,2,2,2,2,2,2,2,4),(-4.14991050821145,-4.10258403056536,-4.08280372408018,
-4.06934364215264,-4.06342116292215,-4.05893181733817,-4.05349079841364,
-4.04267327848696,-3.99729287255898,-3.95753145847438,-3.91406325561467,
-3.90135730538617,-3.89296497549934,-3.88486097738506,-3.87507089466387,
-3.85076662092273,-3.7665644894935,-3.74645229828964,-3.73283238898894,
-3.72688277390483,-3.72239124293459,-3.71697008987701,-3.70625487088741,
-3.6553904889722,-3.60542183439986,-3.5845761651439,-3.56812811842537,-3.55897012962597,
-3.55102326351955,-3.54110940847704,-3.52069606524622,-3.44531330018553,
-3.41554115104302,-3.40334758723133,-3.39392310798449,-3.38876305627559,
-3.38422271837605,-3.3778441766149,-3.36276784594267,-3.3009533336059,-3.25231306484021,
-3.23325322223389,-3.22358713789573,-3.2164245835296,-3.20736645766327,
-3.19183390654462,-3.11977135048715,-3.06533941999265,-3.05670486852015,
-3.05171144694938,-3.04716069726048,-3.04043765779841,-3.02289843783961,
-2.96312970168028,-2.95016545104569,-2.91969943144597,-2.89804824697386,
-2.88791634043941,-2.87995067691451,-2.87093722765783,-2.85561402224077,
-2.78129575563538,-2.74521932994297,-2.72521343008392,-2.71835811146044,
-2.713738011316,-2.70877648959731,-2.70029116682257,-2.65820686740767,-2.59807079980261,
-2.56542875111248,-2.55373527283697,-2.54553704070586,-2.53812492514167,
-2.52814193969286,-2.50224684150195,-2.41992891809295,-2.39995469690588,
-2.38640058933983,-2.38046166899047,-2.37597052381414,-2.37054040170487,
-2.36011074480476,-2.30414385396667,-2.25651314094471,-2.22768040864393,
-2.21645838219754,-2.20834273065099,-2.19981573612492,-2.18644811597091,
-2.13526330321036,-2.06339574347577,-2.0498034354368,-2.04392106431644,
-2.03942633111184,-2.034029665389,-2.02344052083963,-2.01502246037067),
 .UNSPECIFIED.);
#2245=B_SPLINE_CURVE_WITH_KNOTS('',3,(#50132,#50133,#50134,#50135,#50136,
#50137,#50138,#50139,#50140,#50141,#50142,#50143,#50144,#50145,#50146,#50147,
#50148,#50149),.UNSPECIFIED.,.F.,.F.,(4,2,2,2,2,2,2,2,4),(-0.121312221259422,
-0.0984195014592903,-0.0617965384739233,-0.0331257004132508,-0.0252540589033955,
-0.0204254706852453,-0.016234698007148,-0.0115182919411119,-0.000969387966873082),
 .UNSPECIFIED.);
#2246=B_SPLINE_CURVE_WITH_KNOTS('',3,(#50150,#50151,#50152,#50153,#50154,
#50155,#50156,#50157,#50158,#50159,#50160,#50161,#50162,#50163,#50164,#50165,
#50166,#50167,#50168,#50169,#50170,#50171,#50172,#50173,#50174,#50175,#50176,
#50177,#50178,#50179,#50180,#50181,#50182,#50183,#50184,#50185,#50186,#50187,
#50188,#50189,#50190,#50191,#50192,#50193,#50194,#50195,#50196,#50197,#50198,
#50199,#50200,#50201,#50202,#50203,#50204,#50205,#50206,#50207,#50208,#50209,
#50210,#50211,#50212,#50213,#50214,#50215,#50216,#50217,#50218,#50219,#50220,
#50221,#50222,#50223,#50224,#50225,#50226,#50227,#50228,#50229,#50230,#50231,
#50232,#50233,#50234,#50235,#50236,#50237,#50238,#50239,#50240,#50241,#50242,
#50243,#50244,#50245,#50246,#50247,#50248,#50249,#50250,#50251,#50252,#50253,
#50254,#50255,#50256,#50257,#50258,#50259,#50260,#50261,#50262,#50263,#50264,
#50265,#50266,#50267,#50268,#50269,#50270,#50271,#50272,#50273,#50274,#50275,
#50276,#50277,#50278,#50279,#50280,#50281,#50282,#50283,#50284,#50285,#50286,
#50287,#50288,#50289,#50290,#50291,#50292,#50293,#50294,#50295,#50296,#50297,
#50298,#50299,#50300,#50301,#50302,#50303,#50304,#50305,#50306,#50307,#50308,
#50309,#50310,#50311,#50312,#50313,#50314,#50315,#50316,#50317,#50318,#50319,
#50320,#50321,#50322,#50323),.UNSPECIFIED.,.F.,.F.,(4,2,2,2,2,2,2,2,2,2,
2,2,2,2,2,2,2,2,2,2,2,2,2,2,2,2,2,2,2,2,2,2,2,2,2,2,2,2,2,2,2,2,2,2,2,2,
2,2,2,2,2,2,2,2,2,2,2,2,2,2,2,2,2,2,2,2,2,2,2,2,2,2,2,2,2,2,2,2,2,2,2,2,
2,2,2,2,4),(-4.27179890156562,-4.23186784878015,-4.15611311581933,-4.13679228513219,
-4.12707638101779,-4.1199080341674,-4.11088313381104,-4.09551022507233,
-4.02165293833365,-3.98530180834149,-3.96520398302602,-3.95833718332906,
-3.95371451219657,-3.94875599018934,-3.94028658401118,-3.89907062209992,
-3.83824534133803,-3.80542158098759,-3.79370621401721,-3.7855031905106,
-3.77809361624191,-3.76622196597541,-3.73471554955944,-3.65895662485527,
-3.63952164967748,-3.6262280356811,-3.62033293713632,-3.61588548764024,
-3.61044090738187,-3.59960963313656,-3.55406154891125,-3.51395291467636,
-3.48515232452518,-3.46433494081551,-3.4543475771836,-3.4464661252529,-3.43738275109183,
-3.42173768346061,-3.35111860148115,-3.29562793963435,-3.28687623499795,
-3.28185720778926,-3.27731648857647,-3.27065589280916,-3.25355938436952,
-3.18579393001903,-3.13522756519233,-3.12207225016118,-3.1135876300787,
-3.10553806195894,-3.0942362276997,-3.06684610115723,-2.98629851768257,
-2.96645922108836,-2.9529693977907,-2.94704070025515,-2.94254959277758,
-2.9371100642068,-2.92663796449747,-2.87196021014954,-2.80132245417822,
-2.78673624097538,-2.77795728893227,-2.76993950532062,-2.75954708739381,
-2.73661473129622,-2.66422909172293,-2.62159778033585,-2.61319078998254,
-2.60824548722877,-2.60366940403785,-2.5968080752331,-2.57829534358584,
-2.51199366845522,-2.47847884305241,-2.45536562328426,-2.44498738862789,
-2.43699398049138,-2.42811852458821,-2.41306494152108,-2.33489345590886,
-2.30090909812101,-2.28161240347054,-2.27484210241728,-2.27023688857187,
-2.26524358446378,-2.25682980023252),.UNSPECIFIED.);
#2247=B_SPLINE_CURVE_WITH_KNOTS('',3,(#50329,#50330,#50331,#50332,#50333,
#50334,#50335,#50336,#50337,#50338,#50339,#50340,#50341,#50342,#50343,#50344,
#50345,#50346,#50347,#50348,#50349,#50350,#50351,#50352,#50353,#50354,#50355,
#50356,#50357,#50358,#50359,#50360,#50361,#50362,#50363,#50364,#50365,#50366,
#50367,#50368,#50369,#50370,#50371,#50372,#50373,#50374,#50375,#50376,#50377,
#50378,#50379,#50380,#50381,#50382,#50383,#50384,#50385,#50386,#50387,#50388,
#50389,#50390,#50391,#50392,#50393,#50394,#50395,#50396,#50397,#50398,#50399,
#50400,#50401,#50402,#50403,#50404,#50405,#50406,#50407,#50408,#50409,#50410,
#50411,#50412,#50413,#50414,#50415,#50416,#50417,#50418,#50419,#50420,#50421,
#50422,#50423,#50424,#50425,#50426,#50427,#50428,#50429,#50430,#50431,#50432,
#50433,#50434,#50435,#50436,#50437,#50438,#50439,#50440,#50441,#50442,#50443,
#50444,#50445,#50446,#50447,#50448,#50449,#50450,#50451,#50452,#50453,#50454,
#50455,#50456,#50457,#50458,#50459,#50460,#50461,#50462,#50463,#50464,#50465,
#50466,#50467,#50468,#50469,#50470,#50471,#50472,#50473,#50474,#50475,#50476,
#50477,#50478,#50479,#50480,#50481,#50482,#50483,#50484,#50485,#50486,#50487,
#50488,#50489,#50490,#50491,#50492,#50493,#50494,#50495,#50496,#50497,#50498,
#50499,#50500,#50501,#50502,#50503,#50504,#50505,#50506,#50507,#50508,#50509,
#50510,#50511,#50512),.UNSPECIFIED.,.F.,.F.,(4,2,2,2,2,2,2,2,2,2,2,2,2,
2,2,2,2,2,2,2,2,2,2,2,2,2,2,2,2,2,2,2,2,2,2,2,2,2,2,2,2,2,2,2,2,2,2,2,2,
2,2,2,2,2,2,2,2,2,2,2,2,2,2,2,2,2,2,2,2,2,2,2,2,2,2,2,2,2,2,2,2,2,2,2,2,
2,2,2,2,2,2,4),(-2.01495508295737,-2.00689615841809,-1.99095787635076,-1.98181283293574,
-1.97386417025694,-1.96393096995103,-1.94341156801903,-1.86802652050232,
-1.82456397519696,-1.81606312892168,-1.81109823935513,-1.8064799111471,
-1.79963410833907,-1.77970952549718,-1.74387700955012,-1.66905952164474,
-1.65378210197524,-1.64477849293584,-1.63681129693617,-1.62666343070455,
-1.60491862225422,-1.57426545218282,-1.55985073881598,-1.49702891170059,
-1.4831414982134,-1.4775576181753,-1.47302109882991,-1.46799539337194,-1.45920909748763,
-1.44808742164175,-1.42243265291249,-1.33878525297366,-1.31979995593782,
-1.31002880612164,-1.30209056293848,-1.29282388104751,-1.27583124811816,
-1.25405780599962,-1.19561454389183,-1.15137606520766,-1.14287218231421,
-1.13790698348621,-1.13328960556872,-1.12644697680209,-1.10654491983909,
-1.07077727665911,-0.995859699638924,-0.980415474630749,-0.971461436046849,
-0.963486827109749,-0.953258514592142,-0.931036323348952,-0.899401132689867,
-0.862088773811877,-0.818608594539454,-0.807895692988189,-0.802475156607295,
-0.797983845401291,-0.792034046590277,-0.778412144371624,-0.758293468483079,
-0.674082771065319,-0.649753962210217,-0.639960324206288,-0.631855859419937,
-0.623465525661463,-0.610767508812456,-0.567387632567234,-0.527601526817668,
-0.482223677970243,-0.47140670302522,-0.465966047675366,-0.46151995392572,
-0.455624168672415,-0.442319466311555,-0.422857163337568,-0.346804907095297,
-0.315556429021794,-0.303716815498926,-0.296314528806867,-0.288109423296191,
-0.276370796192306,-0.243314325268445,-0.181541391456794,-0.141617731666903,
-0.133188731148189,-0.128240014992132,-0.123614708489622,-0.116727004986083,
-0.0964384694353698,-0.0594955002376233,-0.000970997524927105),
 .UNSPECIFIED.);
#2248=B_SPLINE_CURVE_WITH_KNOTS('',3,(#50513,#50514,#50515,#50516,#50517,
#50518,#50519,#50520,#50521,#50522,#50523,#50524,#50525,#50526,#50527,#50528,
#50529,#50530),.UNSPECIFIED.,.F.,.F.,(4,2,2,2,2,2,2,2,4),(-4.27059030084637,
-4.25544757169058,-4.24361540156102,-4.23565536546824,-4.22810109817617,
-4.21962878643441,-4.20652603409915,-4.15987520303184,-4.14991050821145),
 .UNSPECIFIED.);
#2249=B_SPLINE_CURVE_WITH_KNOTS('',3,(#50531,#50532,#50533,#50534,#50535,
#50536,#50537,#50538,#50539,#50540,#50541,#50542,#50543,#50544,#50545,#50546,
#50547,#50548,#50549,#50550,#50551,#50552,#50553,#50554,#50555,#50556,#50557,
#50558,#50559,#50560,#50561,#50562,#50563,#50564,#50565,#50566,#50567,#50568,
#50569,#50570,#50571,#50572,#50573,#50574,#50575,#50576,#50577,#50578,#50579,
#50580,#50581,#50582,#50583,#50584,#50585,#50586,#50587,#50588,#50589,#50590,
#50591,#50592,#50593,#50594,#50595,#50596,#50597,#50598,#50599,#50600,#50601,
#50602,#50603,#50604,#50605,#50606,#50607,#50608,#50609,#50610,#50611,#50612,
#50613,#50614,#50615,#50616,#50617,#50618,#50619,#50620,#50621,#50622,#50623,
#50624,#50625,#50626,#50627,#50628,#50629,#50630,#50631,#50632,#50633,#50634,
#50635,#50636,#50637,#50638,#50639,#50640,#50641,#50642,#50643,#50644,#50645,
#50646,#50647,#50648,#50649,#50650,#50651,#50652,#50653,#50654,#50655,#50656,
#50657,#50658,#50659,#50660,#50661,#50662,#50663,#50664,#50665,#50666,#50667,
#50668,#50669,#50670,#50671,#50672,#50673,#50674,#50675,#50676,#50677,#50678,
#50679,#50680,#50681,#50682,#50683,#50684,#50685,#50686,#50687,#50688,#50689,
#50690,#50691,#50692,#50693,#50694,#50695,#50696,#50697,#50698,#50699,#50700,
#50701,#50702,#50703,#50704,#50705,#50706,#50707,#50708,#50709,#50710,#50711,
#50712,#50713,#50714,#50715,#50716,#50717,#50718),.UNSPECIFIED.,.F.,.F.,
(4,2,2,2,2,2,2,2,2,2,2,2,2,2,2,2,2,2,2,2,2,2,2,2,2,2,2,2,2,2,2,2,2,2,2,
2,2,2,2,2,2,2,2,2,2,2,2,2,2,2,2,2,2,2,2,2,2,2,2,2,2,2,2,2,2,2,2,2,2,2,2,
2,2,2,2,2,2,2,2,2,2,2,2,2,2,2,2,2,2,2,2,2,2,4),(-2.25682980023252,-2.25661250994356,
-2.20591257576506,-2.16281917118168,-2.13645165548217,-2.1169018521095,
-2.10714324506673,-2.09920344941743,-2.08992165103755,-2.07286138092067,
-2.05097351320595,-1.99189112121632,-1.94846836710502,-1.93996632939605,
-1.93500061792971,-1.93038141875548,-1.92353417342988,-1.90360425218822,
-1.86776004680764,-1.79293828114798,-1.7776571174334,-1.76865167205481,
-1.76068307377045,-1.75053372660918,-1.7287870318966,-1.69813247594623,
-1.6837292262318,-1.62093360426141,-1.60700311727575,-1.60141158179645,
-1.59687272734449,-1.5918497418494,-1.58307889778798,-1.52849127241406,
-1.4568114331574,-1.44123923617918,-1.43217172506076,-1.42500902950786,
-1.41535226570942,-1.39634664209088,-1.34840773421741,-1.28791964058421,
-1.27126858243578,-1.26468001100106,-1.26010659180953,-1.25504232594926,
-1.24607590567697,-1.23465494675142,-1.2078893145758,-1.11890400261765,
-1.10382968798458,-1.09495104026401,-1.08696025643398,-1.07659325769416,
-1.05354021592884,-1.0201545541671,-0.954535073066022,-0.935406972779673,
-0.928463685195102,-0.92387308407564,-0.918956447793143,-0.910679620498813,
-0.871583711698889,-0.78201784921328,-0.767075074254779,-0.758224156700196,
-0.750228098639219,-0.739810878433548,-0.716444905435652,-0.682381818962293,
-0.612588687674437,-0.597492388887194,-0.591112830477054,-0.586572586060987,
-0.581413763313979,-0.571993817454269,-0.517287834361057,-0.447099468186158,
-0.431428251344811,-0.422341143590254,-0.414463128361396,-0.404488982464491,
-0.383733974638334,-0.355054707383274,-0.314847093571687,-0.269304023175076,
-0.258475328608771,-0.253032386465008,-0.248586505264217,-0.242693697072303,
-0.229406404558046,-0.209979860025607,-0.134328372818447,-0.121726265633444),
 .UNSPECIFIED.);
#2250=B_SPLINE_CURVE_WITH_KNOTS('',3,(#50723,#50724,#50725,#50726,#50727,
#50728,#50729,#50730,#50731,#50732,#50733,#50734,#50735,#50736,#50737,#50738,
#50739,#50740,#50741,#50742,#50743,#50744,#50745,#50746,#50747,#50748,#50749,
#50750,#50751,#50752,#50753,#50754,#50755,#50756,#50757,#50758,#50759,#50760,
#50761,#50762,#50763,#50764,#50765,#50766,#50767,#50768,#50769,#50770,#50771,
#50772,#50773,#50774,#50775,#50776,#50777,#50778,#50779,#50780,#50781,#50782,
#50783,#50784,#50785,#50786,#50787,#50788,#50789,#50790,#50791,#50792,#50793,
#50794,#50795,#50796,#50797,#50798,#50799,#50800,#50801,#50802,#50803,#50804,
#50805,#50806,#50807,#50808,#50809,#50810,#50811,#50812,#50813,#50814,#50815,
#50816,#50817,#50818,#50819,#50820,#50821,#50822,#50823,#50824,#50825,#50826,
#50827,#50828,#50829,#50830,#50831,#50832,#50833,#50834,#50835,#50836,#50837,
#50838,#50839,#50840,#50841,#50842,#50843,#50844,#50845,#50846,#50847,#50848,
#50849,#50850,#50851,#50852,#50853,#50854,#50855,#50856,#50857,#50858,#50859,
#50860,#50861,#50862,#50863,#50864,#50865,#50866,#50867,#50868,#50869,#50870,
#50871,#50872,#50873,#50874,#50875,#50876,#50877,#50878,#50879,#50880,#50881,
#50882,#50883,#50884,#50885,#50886,#50887,#50888,#50889,#50890,#50891,#50892,
#50893,#50894,#50895,#50896,#50897,#50898,#50899,#50900,#50901,#50902,#50903,
#50904),.UNSPECIFIED.,.F.,.F.,(4,2,2,2,2,2,2,2,2,2,2,2,2,2,2,2,2,2,2,2,
2,2,2,2,2,2,2,2,2,2,2,2,2,2,2,2,2,2,2,2,2,2,2,2,2,2,2,2,2,2,2,2,2,2,2,2,
2,2,2,2,2,2,2,2,2,2,2,2,2,2,2,2,2,2,2,2,2,2,2,2,2,2,2,2,2,2,2,2,2,2,4),
(-4.14982650109305,-4.1082873562313,-4.03324515804132,-4.01292358148232,
-4.00302634855727,-3.99508089494166,-3.98591142787804,-3.96985567421038,
-3.91185516252669,-3.8648129285416,-3.84158169981968,-3.83437491440773,
-3.82968682075502,-3.82543092738862,-3.81805484803389,-3.7952317618859,
-3.73316273078659,-3.6840670492864,-3.67099515387706,-3.66252939411821,
-3.65447329869181,-3.64312071007598,-3.61538867767319,-3.53529391966009,
-3.51549518972057,-3.50202624071291,-3.49610228589735,-3.4916128655996,
-3.48617303864717,-3.47536149953984,-3.43006828533371,-3.39049394461776,
-3.34678119115582,-3.33405730208145,-3.32566143067199,-3.31756003629561,
-3.30778048711826,-3.28354377230916,-3.19925548416821,-3.1791371768581,
-3.16551436513755,-3.159564287869,-3.15507274944567,-3.14965200580156,-3.13893875631023,
-3.09548280903759,-3.05825154495698,-3.0265084516441,-3.00423550502694,
-2.99399831377212,-2.98602253535218,-2.9770731443316,-2.96165237912129,
-2.88657642140549,-2.83541038289319,-2.82633734706489,-2.82125087459975,
-2.81668653397386,-2.81015123254805,-2.7938288120438,-2.73302986116154,
-2.67510130030553,-2.6616381434093,-2.65309183599168,-2.64498669158846,
-2.63382611939545,-2.60719732470529,-2.52569662487933,-2.50578533783049,
-2.49226160437534,-2.48632789952198,-2.48183723769271,-2.4764034512305,
-2.46595582275543,-2.41036452589907,-2.36249942517703,-2.33358539067036,
-2.32235276123421,-2.31423548341687,-2.30571214072808,-2.29236169239625,
-2.24186162469394,-2.18468907522819,-2.15910380673045,-2.15167458095321,
-2.1469400423572,-2.1427233022465,-2.13555968771329,-2.11276153245501,-2.06736403238497,
-2.01495508295737),.UNSPECIFIED.);
#2251=B_SPLINE_CURVE_WITH_KNOTS('',3,(#50906,#50907,#50908,#50909,#50910,
#50911,#50912,#50913,#50914,#50915,#50916,#50917,#50918,#50919,#50920,#50921),
 .UNSPECIFIED.,.F.,.F.,(4,2,2,2,2,2,2,4),(-0.121726265633444,-0.102713804360095,
-0.0908325869755382,-0.0834232988331032,-0.0752256878954314,-0.0670488432893421,
-0.0557586804094333,-0.000969944449356401),.UNSPECIFIED.);
#2252=B_SPLINE_CURVE_WITH_KNOTS('',3,(#50922,#50923,#50924,#50925,#50926,
#50927,#50928,#50929,#50930,#50931,#50932,#50933,#50934,#50935,#50936,#50937,
#50938,#50939,#50940,#50941,#50942,#50943,#50944,#50945,#50946,#50947,#50948,
#50949,#50950,#50951,#50952,#50953,#50954,#50955,#50956,#50957,#50958,#50959,
#50960,#50961,#50962,#50963,#50964,#50965,#50966,#50967,#50968,#50969,#50970,
#50971,#50972,#50973,#50974,#50975,#50976,#50977,#50978,#50979,#50980,#50981,
#50982,#50983,#50984,#50985,#50986,#50987,#50988,#50989,#50990,#50991,#50992,
#50993,#50994,#50995,#50996,#50997,#50998,#50999,#51000,#51001,#51002,#51003,
#51004,#51005,#51006,#51007,#51008,#51009,#51010,#51011,#51012,#51013,#51014,
#51015,#51016,#51017,#51018,#51019,#51020,#51021,#51022,#51023,#51024,#51025,
#51026,#51027,#51028,#51029,#51030,#51031,#51032,#51033,#51034,#51035,#51036,
#51037,#51038,#51039,#51040,#51041,#51042,#51043,#51044,#51045,#51046,#51047,
#51048,#51049,#51050,#51051,#51052,#51053,#51054,#51055,#51056,#51057,#51058,
#51059,#51060,#51061,#51062,#51063,#51064,#51065,#51066,#51067,#51068,#51069,
#51070,#51071,#51072,#51073,#51074,#51075,#51076,#51077,#51078,#51079,#51080,
#51081,#51082,#51083,#51084,#51085,#51086,#51087,#51088,#51089,#51090,#51091,
#51092,#51093,#51094,#51095,#51096,#51097,#51098,#51099,#51100,#51101),
 .UNSPECIFIED.,.F.,.F.,(4,2,2,2,2,2,2,2,2,2,2,2,2,2,2,2,2,2,2,2,2,2,2,2,
2,2,2,2,2,2,2,2,2,2,2,2,2,2,2,2,2,2,2,2,2,2,2,2,2,2,2,2,2,2,2,2,2,2,2,2,
2,2,2,2,2,2,2,2,2,2,2,2,2,2,2,2,2,2,2,2,2,2,2,2,2,2,2,2,2,4),(-4.27066642005769,
-4.20450669432558,-4.19591865740787,-4.18871611366403,-4.18402833466105,
-4.17917337930773,-4.17118368822046,-4.14103271644137,-4.07807885739943,
-4.03719297500419,-4.02468825619013,-4.01633511798358,-4.00819979996669,
-3.99828582349113,-3.97314189738097,-3.88998252595607,-3.86994487373079,
-3.85636020284215,-3.85041604760643,-3.84592441665616,-3.84049796566513,
-3.82975788290823,-3.76345750597047,-3.72287200729123,-3.70492262509248,
-3.69023113630502,-3.68143124171302,-3.67342075096437,-3.66307499420352,
-3.63946209474127,-3.56748834589091,-3.53859744257702,-3.52662489882081,
-3.51733016194855,-3.51219688443914,-3.50764792098268,-3.50121313539205,
-3.48556689753791,-3.42418867343737,-3.36593649721675,-3.35246218155466,
-3.34391317329678,-3.33580849643624,-3.32465347500487,-3.29807095676384,
-3.21650779525402,-3.19659069829215,-3.18306388503558,-3.17712939848285,
-3.17263838888996,-3.1672044812344,-3.1564267122281,-3.11170137393137,-3.07330764627421,
-3.02799881035847,-3.01516017231304,-3.00674010509332,-2.99865238218313,
-2.9889344048032,-2.9648433797927,-2.88024096795973,-2.86009721401144,-2.8464613928347,
-2.84050837578946,-2.83601577966916,-2.8305951826985,-2.82021266003633,
-2.76333596297476,-2.7162634462516,-2.68762556427817,-2.67642881459227,
-2.66831679128014,-2.65978055953677,-2.64637047528827,-2.59326002313963,
-2.54532916737113,-2.52417745267427,-2.5100650394432,-2.50403322216664,
-2.4995340983232,-2.49416983757404,-2.48405465993704,-2.40844992956381,
-2.37316459242375,-2.3492430700218,-2.33873566156012,-2.33072732260278,
-2.32191928835796,-2.30718833518643,-2.25630608464035),.UNSPECIFIED.);
#2253=B_SPLINE_CURVE_WITH_KNOTS('',3,(#51107,#51108,#51109,#51110,#51111,
#51112,#51113,#51114,#51115,#51116,#51117,#51118,#51119,#51120,#51121,#51122,
#51123,#51124,#51125,#51126,#51127,#51128,#51129,#51130,#51131,#51132,#51133,
#51134,#51135,#51136,#51137,#51138,#51139,#51140,#51141,#51142,#51143,#51144,
#51145,#51146,#51147,#51148,#51149,#51150,#51151,#51152,#51153,#51154,#51155,
#51156,#51157,#51158,#51159,#51160,#51161,#51162,#51163,#51164,#51165,#51166,
#51167,#51168,#51169,#51170,#51171,#51172,#51173,#51174,#51175,#51176,#51177,
#51178,#51179,#51180,#51181,#51182,#51183,#51184,#51185,#51186,#51187,#51188,
#51189,#51190,#51191,#51192,#51193,#51194,#51195,#51196,#51197,#51198,#51199,
#51200,#51201,#51202,#51203,#51204,#51205,#51206,#51207,#51208,#51209,#51210,
#51211,#51212,#51213,#51214,#51215,#51216,#51217,#51218,#51219,#51220,#51221,
#51222,#51223,#51224,#51225,#51226,#51227,#51228,#51229,#51230,#51231,#51232,
#51233,#51234,#51235,#51236,#51237,#51238,#51239,#51240,#51241,#51242,#51243,
#51244,#51245,#51246,#51247,#51248,#51249,#51250,#51251,#51252,#51253,#51254,
#51255,#51256,#51257,#51258,#51259,#51260,#51261,#51262,#51263,#51264,#51265,
#51266,#51267,#51268,#51269,#51270,#51271,#51272,#51273,#51274,#51275,#51276,
#51277,#51278,#51279,#51280,#51281,#51282,#51283,#51284,#51285,#51286,#51287,
#51288),.UNSPECIFIED.,.F.,.F.,(4,2,2,2,2,2,2,2,2,2,2,2,2,2,2,2,2,2,2,2,
2,2,2,2,2,2,2,2,2,2,2,2,2,2,2,2,2,2,2,2,2,2,2,2,2,2,2,2,2,2,2,2,2,2,2,2,
2,2,2,2,2,2,2,2,2,2,2,2,2,2,2,2,2,2,2,2,2,2,2,2,2,2,2,2,2,2,2,2,2,2,4),
(-2.01540403112139,-1.97105136948028,-1.93084922841608,-1.92241046674066,
-1.91745917003503,-1.9128341508167,-1.90595073915008,-1.88570480379444,
-1.84889644755654,-1.77578561155131,-1.76033973643343,-1.75130038095629,
-1.74413573114024,-1.73444476642549,-1.71525033646811,-1.66580262697228,
-1.60216445243628,-1.58881545732867,-1.58297416056085,-1.57848324138124,
-1.5730565755451,-1.56231307435975,-1.51912676950302,-1.43715461635382,
-1.42262543062796,-1.41386001862441,-1.40584152515428,-1.39524857680718,
-1.37077473063976,-1.33424469865971,-1.27904499091919,-1.25572860599391,
-1.24830426835741,-1.2440392661089,-1.23936062382481,-1.23220011854312,
-1.20942644959956,-1.1641148584887,-1.10354597476904,-1.08761064848205,
-1.07846694715354,-1.07051924808615,-1.06058698533554,-1.04006848479775,
-0.964689634107515,-0.921238054893156,-0.91273830108402,-0.907774035032211,
-0.903156274572745,-0.896311295802245,-0.876388979019519,-0.84056029548628,
-0.765753154174027,-0.750477512485586,-0.741474994270852,-0.733508789374499,
-0.72336222092219,-0.701620342579102,-0.670971450466201,-0.656560122439426,
-0.593750375264972,-0.57986004552223,-0.574276096265196,-0.569739965685457,
-0.564715299207513,-0.555932048192157,-0.54481499123808,-0.519175302046611,
-0.435630653447615,-0.416578735157652,-0.406795202486274,-0.398857258392173,
-0.389602611106648,-0.37266689432786,-0.350990459195165,-0.293089836872497,
-0.248139868711028,-0.239633959232288,-0.234668716220123,-0.230052259616926,
-0.223212368372139,-0.203328586427172,-0.165047175600778,-0.0968343570779647,
-0.0807251782686702,-0.0707223989749149,-0.0627697428924434,-0.0552960986842517,
-0.0463378825376443,-0.0291380428848708,-0.000969509926115122),
 .UNSPECIFIED.);
#2254=B_SPLINE_CURVE_WITH_KNOTS('',3,(#51289,#51290,#51291,#51292,#51293,
#51294,#51295,#51296,#51297,#51298,#51299,#51300,#51301,#51302,#51303,#51304),
 .UNSPECIFIED.,.F.,.F.,(4,2,2,2,2,2,2,4),(-4.2700769044163,-4.19726735642565,
-4.17736906543256,-4.17052691070852,-4.16590950518612,-4.16094397358122,
-4.152438800623,-4.14982650109305),.UNSPECIFIED.);
#2255=B_SPLINE_CURVE_WITH_KNOTS('',3,(#51305,#51306,#51307,#51308,#51309,
#51310,#51311,#51312,#51313,#51314,#51315,#51316,#51317,#51318,#51319,#51320,
#51321,#51322,#51323,#51324,#51325,#51326,#51327,#51328,#51329,#51330,#51331,
#51332,#51333,#51334,#51335,#51336,#51337,#51338,#51339,#51340,#51341,#51342,
#51343,#51344,#51345,#51346,#51347,#51348,#51349,#51350,#51351,#51352,#51353,
#51354,#51355,#51356,#51357,#51358,#51359,#51360,#51361,#51362,#51363,#51364,
#51365,#51366,#51367,#51368,#51369,#51370,#51371,#51372,#51373,#51374,#51375,
#51376,#51377,#51378,#51379,#51380,#51381,#51382,#51383,#51384,#51385,#51386,
#51387,#51388,#51389,#51390,#51391,#51392,#51393,#51394,#51395,#51396,#51397,
#51398,#51399,#51400,#51401,#51402,#51403,#51404,#51405,#51406,#51407,#51408,
#51409,#51410,#51411,#51412,#51413,#51414,#51415,#51416,#51417,#51418,#51419,
#51420,#51421,#51422,#51423,#51424,#51425,#51426,#51427,#51428,#51429,#51430,
#51431,#51432,#51433,#51434,#51435,#51436,#51437,#51438,#51439,#51440,#51441,
#51442,#51443,#51444,#51445,#51446,#51447,#51448,#51449,#51450,#51451,#51452,
#51453,#51454,#51455,#51456,#51457,#51458,#51459,#51460,#51461,#51462,#51463,
#51464,#51465,#51466,#51467,#51468,#51469,#51470,#51471,#51472,#51473,#51474,
#51475,#51476,#51477,#51478,#51479,#51480,#51481,#51482,#51483,#51484,#51485,
#51486,#51487,#51488,#51489,#51490,#51491,#51492,#51493,#51494,#51495,#51496,
#51497,#51498),.UNSPECIFIED.,.F.,.F.,(4,2,2,2,2,2,2,2,2,2,2,2,2,2,2,2,2,
2,2,2,2,2,2,2,2,2,2,2,2,2,2,2,2,2,2,2,2,2,2,2,2,2,2,2,2,2,2,2,2,2,2,2,2,
2,2,2,2,2,2,2,2,2,2,2,2,2,2,2,2,2,2,2,2,2,2,2,2,2,2,2,2,2,2,2,2,2,2,2,2,
2,2,2,2,2,2,2,4),(-2.25630608464035,-2.22665608863465,-2.17869788383292,
-2.17015256186819,-2.16517794394682,-2.16061765643055,-2.15384198147782,
-2.13593876315631,-2.10493550210421,-2.02462227724864,-2.00849239269026,
-1.99930614997329,-1.99136068286754,-1.9814823195733,-1.96127100384044,
-1.88644182286149,-1.84194822390737,-1.83344169373867,-1.82847534548915,
-1.82385723388452,-1.81701399612784,-1.79711376566932,-1.76135599915273,
-1.68639514367998,-1.67095126243185,-1.66199622203288,-1.65402001705065,
-1.64378867863304,-1.62155565749395,-1.58990068614956,-1.55259751550503,
-1.5091164493172,-1.49840187926288,-1.49298040097717,-1.48848825145647,
-1.48253726694896,-1.4689123452172,-1.44878890771564,-1.36454833446142,
-1.34022610404596,-1.33043236932,-1.32232682201949,-1.3139343467314,-1.30123103488885,
-1.25780347391481,-1.21804023857895,-1.17266803485197,-1.16185003086918,
-1.15640855809648,-1.15196162368115,-1.14606450014982,-1.13275588923714,
-1.11328701361728,-1.03718725397823,-1.00596326367933,-0.994124996952157,
-0.985982358008743,-0.977639492242221,-0.965184913902923,-0.924882635268002,
-0.883119213883946,-0.836025355105792,-0.825252215367661,-0.819819678630679,
-0.815329273066339,-0.809394805584559,-0.795865237590222,-0.775939367664903,
-0.69431878705586,-0.667759389674627,-0.656608154368171,-0.648505092507639,
-0.639956788739636,-0.626481334627401,-0.568085212898543,-0.506426166795781,
-0.491199464899958,-0.484808698147212,-0.480266811200401,-0.475113532638111,
-0.465720282655782,-0.453578513085589,-0.424013595510056,-0.349463049411302,
-0.328263161010679,-0.318210567271455,-0.310253382564873,-0.301192145033339,
-0.285220312656599,-0.2320659815783,-0.171333807383222,-0.154989143431792,
-0.148450884418965,-0.143886597679154,-0.138802702872771,-0.129739418416578,
-0.121361672833077),.UNSPECIFIED.);
#2256=B_SPLINE_CURVE_WITH_KNOTS('',3,(#51503,#51504,#51505,#51506,#51507,
#51508,#51509,#51510,#51511,#51512,#51513,#51514,#51515,#51516,#51517,#51518,
#51519,#51520,#51521,#51522,#51523,#51524,#51525,#51526,#51527,#51528,#51529,
#51530,#51531,#51532,#51533,#51534,#51535,#51536,#51537,#51538,#51539,#51540,
#51541,#51542,#51543,#51544,#51545,#51546,#51547,#51548,#51549,#51550,#51551,
#51552,#51553,#51554,#51555,#51556,#51557,#51558,#51559,#51560,#51561,#51562,
#51563,#51564,#51565,#51566,#51567,#51568,#51569,#51570,#51571,#51572,#51573,
#51574,#51575,#51576,#51577,#51578,#51579,#51580,#51581,#51582,#51583,#51584,
#51585,#51586,#51587,#51588,#51589,#51590,#51591,#51592,#51593,#51594,#51595,
#51596,#51597,#51598,#51599,#51600,#51601,#51602,#51603,#51604,#51605,#51606,
#51607,#51608,#51609,#51610,#51611,#51612,#51613,#51614,#51615,#51616,#51617,
#51618,#51619,#51620,#51621,#51622,#51623,#51624,#51625,#51626,#51627,#51628,
#51629,#51630,#51631,#51632,#51633,#51634,#51635,#51636,#51637,#51638,#51639,
#51640,#51641,#51642,#51643,#51644,#51645,#51646,#51647,#51648,#51649,#51650,
#51651,#51652,#51653,#51654,#51655,#51656,#51657,#51658,#51659,#51660,#51661,
#51662,#51663,#51664,#51665,#51666,#51667,#51668,#51669,#51670,#51671,#51672,
#51673,#51674,#51675,#51676,#51677,#51678,#51679,#51680,#51681,#51682,#51683,
#51684,#51685,#51686,#51687,#51688,#51689,#51690,#51691,#51692,#51693,#51694,
#51695,#51696),.UNSPECIFIED.,.F.,.F.,(4,2,2,2,2,2,2,2,2,2,2,2,2,2,2,2,2,
2,2,2,2,2,2,2,2,2,2,2,2,2,2,2,2,2,2,2,2,2,2,2,2,2,2,2,2,2,2,2,2,2,2,2,2,
2,2,2,2,2,2,2,2,2,2,2,2,2,2,2,2,2,2,2,2,2,2,2,2,2,2,2,2,2,2,2,2,2,2,2,2,
2,2,2,2,2,2,2,4),(-4.15012799910223,-4.13770291279851,-4.11856720368116,
-4.10888734005964,-4.10172395829129,-4.09267707088321,-4.07719508535689,
-4.00456088298881,-3.95114469027171,-3.94221968518544,-3.93716465558241,
-3.93258862930004,-3.92702828456003,-3.91328258296434,-3.85029795249565,
-3.83580935355281,-3.80513828910692,-3.78338669329017,-3.77323805832315,
-3.76527133227511,-3.75626939157692,-3.74099753609209,-3.66620732335969,
-3.63040431130387,-3.61049001390752,-3.60364595454235,-3.5990282030219,
-3.59406334872494,-3.58556132032129,-3.54203293479802,-3.46664739859655,
-3.44613955153438,-3.43620893417147,-3.42826115932338,-3.41911585377816,
-3.40317359139517,-3.34475719783788,-3.29787751298955,-3.27468857687821,
-3.26748603690984,-3.26279880766999,-3.25854208311828,-3.25116161400311,
-3.22829489262859,-3.16626651847937,-3.11718164650289,-3.10411035642869,
-3.09564471523164,-3.08758854087377,-3.07623551312685,-3.04850065947577,
-2.96840940456376,-2.94861095795744,-2.93514214427853,-2.92921820920294,
-2.92472878803074,-2.91928894084348,-2.90847729856123,-2.86318255149109,
-2.8236048949081,-2.77989650195236,-2.76717293403115,-2.75877712798345,
-2.75067569051386,-2.74089595926649,-2.71665806699367,-2.6323712564819,
-2.61225305439068,-2.5986302936305,-2.59268022619285,-2.58818868980108,
-2.58276794214718,-2.57205466861945,-2.52859814615984,-2.49136559965593,
-2.45962361679968,-2.43735120527208,-2.42711410508525,-2.41913833749668,
-2.41018889650569,-2.39476788277872,-2.31969419661528,-2.28405052658235,
-2.26418949498752,-2.25735178411163,-2.25273518973789,-2.24776808371841,
-2.23925559963183,-2.19343197119745,-2.13612099482066,-2.10481335580357,
-2.09296559891226,-2.0855611059612,-2.07735587741152,-2.06562169077769,
-2.03261531170587,-2.01540403112139),.UNSPECIFIED.);
#2257=B_SPLINE_CURVE_WITH_KNOTS('',3,(#51698,#51699,#51700,#51701,#51702,
#51703,#51704,#51705),.UNSPECIFIED.,.F.,.F.,(4,2,2,4),(-0.121361672833077,
-0.0788430327264066,-0.0196534734691905,-0.000970778274795699),
 .UNSPECIFIED.);
#2258=B_SPLINE_CURVE_WITH_KNOTS('',3,(#51706,#51707,#51708,#51709,#51710,
#51711,#51712,#51713,#51714,#51715,#51716,#51717,#51718,#51719,#51720,#51721,
#51722,#51723,#51724,#51725,#51726,#51727,#51728,#51729,#51730,#51731,#51732,
#51733,#51734,#51735,#51736,#51737,#51738,#51739,#51740,#51741,#51742,#51743,
#51744,#51745,#51746,#51747,#51748,#51749,#51750,#51751,#51752,#51753,#51754,
#51755,#51756,#51757,#51758,#51759,#51760,#51761,#51762,#51763,#51764,#51765,
#51766,#51767,#51768,#51769,#51770,#51771,#51772,#51773,#51774,#51775,#51776,
#51777,#51778,#51779,#51780,#51781,#51782,#51783,#51784,#51785,#51786,#51787,
#51788,#51789,#51790,#51791,#51792,#51793,#51794,#51795,#51796,#51797,#51798,
#51799,#51800,#51801,#51802,#51803,#51804,#51805,#51806,#51807,#51808,#51809,
#51810,#51811,#51812,#51813,#51814,#51815,#51816,#51817,#51818,#51819,#51820,
#51821,#51822,#51823,#51824,#51825,#51826,#51827,#51828,#51829,#51830,#51831,
#51832,#51833,#51834,#51835,#51836,#51837,#51838,#51839,#51840,#51841,#51842,
#51843,#51844,#51845,#51846,#51847,#51848,#51849,#51850,#51851,#51852,#51853,
#51854,#51855,#51856,#51857,#51858,#51859,#51860,#51861,#51862,#51863,#51864,
#51865,#51866,#51867,#51868,#51869,#51870,#51871,#51872,#51873,#51874,#51875,
#51876,#51877,#51878,#51879,#51880,#51881,#51882,#51883,#51884,#51885,#51886,
#51887,#51888,#51889,#51890,#51891,#51892,#51893,#51894,#51895,#51896,#51897,
#51898,#51899,#51900,#51901,#51902,#51903,#51904),.UNSPECIFIED.,.F.,.F.,
(4,3,3,3,3,3,3,3,3,3,3,3,3,3,3,3,3,3,3,3,3,3,3,3,3,3,3,3,3,3,3,3,3,3,3,
3,3,3,3,3,3,3,3,3,3,3,3,3,3,3,3,3,3,3,3,3,3,3,3,3,3,3,3,3,3,3,4),(-16.4167960594917,
-16.3231866314518,-16.2295269004793,-16.1346626816796,-16.0407807339324,
-15.9454253796064,-15.8500700252804,-15.7580593289842,-15.6661696605864,
-15.5743745685169,-15.4826447769347,-15.3909489474259,-15.2992633110076,
-15.2075641131019,-15.1157697354889,-15.0239260397092,-14.93193240322,-14.8594406487004,
-14.7674298820707,-14.675540142735,-14.5837449792239,-14.4920151157411,
-14.4003192140759,-14.3086335053328,-14.2169342350209,-14.1251397853258,
-14.0332960175352,-13.9413023098999,-13.8688112721204,-13.7768007958635,
-13.684911347358,-13.5931164747535,-13.5013869011079,-13.4096912885271,
-13.3180058677772,-13.2263068840292,-13.1345127169216,-13.0426692299422,
-12.9506757972999,-12.8781818955404,-12.7861710642596,-12.6942812621272,
-12.6024860377262,-12.5107561164391,-12.4190601588747,-12.3273743961905,
-12.2356750739514,-12.1438805757485,-12.0520367612691,-11.9600430103993,
-11.8875525189603,-11.7955413114026,-11.7036511281309,-11.6118555182898,
-11.5201252067329,-11.4284288560818,-11.3367426979798,-11.2450429784762,
-11.1532480826281,-11.0614038696983,-10.9694097232057,-10.8969231423803,
-10.8060917963888,-10.7154014243328,-10.6247923810207,-10.5342434860829,
-10.4883011219526),.UNSPECIFIED.);
#2259=B_SPLINE_CURVE_WITH_KNOTS('',3,(#51910,#51911,#51912,#51913,#51914,
#51915,#51916,#51917,#51918,#51919,#51920,#51921,#51922,#51923,#51924,#51925,
#51926,#51927,#51928,#51929,#51930,#51931,#51932,#51933,#51934,#51935,#51936,
#51937,#51938,#51939,#51940,#51941,#51942,#51943,#51944,#51945,#51946,#51947,
#51948,#51949,#51950,#51951,#51952,#51953,#51954,#51955,#51956,#51957,#51958,
#51959,#51960,#51961,#51962,#51963,#51964,#51965,#51966,#51967,#51968,#51969,
#51970,#51971,#51972,#51973,#51974,#51975,#51976,#51977,#51978,#51979,#51980,
#51981,#51982,#51983,#51984,#51985,#51986,#51987,#51988,#51989,#51990,#51991,
#51992,#51993,#51994,#51995,#51996,#51997,#51998,#51999,#52000,#52001,#52002,
#52003,#52004,#52005,#52006,#52007,#52008,#52009,#52010,#52011,#52012,#52013,
#52014,#52015,#52016,#52017,#52018,#52019,#52020,#52021,#52022,#52023,#52024,
#52025,#52026,#52027,#52028,#52029,#52030,#52031,#52032,#52033,#52034,#52035,
#52036,#52037),.UNSPECIFIED.,.F.,.F.,(4,2,2,2,2,2,2,2,2,2,2,2,2,2,2,2,2,
2,2,2,2,2,2,2,2,2,2,2,2,2,2,2,2,2,2,2,2,2,2,2,2,2,2,2,2,2,2,2,2,2,2,2,2,
2,2,2,2,2,2,2,2,2,2,4),(0.00023418752938069,0.00315081488393006,0.00670998306291529,
0.0168928125761018,0.0617594987574512,0.107919044930031,0.13495437600853,
0.146551589240641,0.155447730774231,0.165349469766094,0.182321728836201,
0.274969220724888,0.320871474826383,0.329529544441537,0.334553533174522,
0.339048055301246,0.345518406077316,0.362224844207103,0.422266001158218,
0.460621487816279,0.485635852341467,0.496020108702134,0.503708340411375,
0.511934797877298,0.525115762712998,0.577959271430399,0.637362858857812,
0.654978060519609,0.667262186287639,0.672789027783616,0.677173957550166,
0.682613655152971,0.693105144563507,0.735404306501783,0.810846805884277,
0.830352008521856,0.840178129618988,0.847439558359909,0.856602561112202,
0.872293580606378,0.937032602343338,0.977054528538225,0.998291751472804,
1.0053775651737,1.01011380108815,1.01511794681386,1.02366902545801,1.06908163979997,
1.12631128277454,1.14786738106989,1.1647424587352,1.17401470273502,1.1819971517978,
1.19187506987937,1.21191738201843,1.30301994754333,1.32363958307489,1.33751112151411,
1.34351141290234,1.34800485063959,1.35337123845478,1.36388487750363,1.4202032623988,
1.42896198809384),.UNSPECIFIED.);
#2260=B_SPLINE_CURVE_WITH_KNOTS('',3,(#52040,#52041,#52042,#52043,#52044,
#52045,#52046,#52047,#52048,#52049,#52050,#52051,#52052,#52053,#52054,#52055,
#52056,#52057,#52058,#52059,#52060,#52061,#52062,#52063,#52064,#52065,#52066,
#52067,#52068,#52069,#52070,#52071,#52072,#52073,#52074,#52075,#52076,#52077,
#52078,#52079,#52080,#52081,#52082,#52083,#52084,#52085,#52086,#52087,#52088,
#52089,#52090,#52091,#52092,#52093,#52094,#52095,#52096,#52097,#52098,#52099,
#52100,#52101,#52102,#52103,#52104,#52105,#52106,#52107,#52108,#52109,#52110,
#52111,#52112,#52113,#52114,#52115,#52116,#52117,#52118,#52119,#52120,#52121,
#52122,#52123,#52124,#52125,#52126,#52127,#52128,#52129,#52130,#52131,#52132,
#52133,#52134,#52135,#52136,#52137,#52138,#52139,#52140,#52141,#52142,#52143,
#52144,#52145,#52146,#52147,#52148,#52149,#52150,#52151,#52152,#52153,#52154,
#52155,#52156,#52157,#52158,#52159,#52160,#52161,#52162,#52163,#52164,#52165,
#52166,#52167,#52168,#52169,#52170,#52171,#52172,#52173,#52174,#52175,#52176,
#52177,#52178,#52179,#52180,#52181,#52182,#52183,#52184,#52185,#52186,#52187,
#52188,#52189,#52190,#52191,#52192,#52193,#52194,#52195,#52196,#52197,#52198,
#52199,#52200,#52201,#52202,#52203,#52204,#52205,#52206,#52207,#52208,#52209,
#52210,#52211,#52212,#52213,#52214,#52215,#52216,#52217,#52218,#52219),
 .UNSPECIFIED.,.F.,.F.,(4,2,2,2,2,2,2,2,2,2,2,2,2,2,2,2,2,2,2,2,2,2,2,2,
2,2,2,2,2,2,2,2,2,2,2,2,2,2,2,2,2,2,2,2,2,2,2,2,2,2,2,2,2,2,2,2,2,2,2,2,
2,2,2,2,2,2,2,2,2,2,2,2,2,2,2,2,2,2,2,2,2,2,2,2,2,2,2,2,2,4),(-4.02402267163659,
-4.01660595258704,-3.95364176009931,-3.90430146731395,-3.88483392599072,
-3.87501536411647,-3.86775531655484,-3.85858850312061,-3.84287671102708,
-3.77920201461287,-3.73848912010533,-3.7170474773943,-3.70993954359626,
-3.705199173783,-3.7002031284654,-3.69168818039025,-3.65041139171089,-3.59001474375477,
-3.56790954289913,-3.55071788283664,-3.54138346606413,-3.5334060536903,
-3.52360876674235,-3.50832050943198,-3.41269493655136,-3.39182620271596,
-3.37783653980434,-3.3718171792667,-3.36736237564828,-3.36202916308435,
-3.35198712933449,-3.29045477172602,-3.24614198279102,-3.2185400092547,
-3.20752498482568,-3.19948208104683,-3.19096441943396,-3.17747171542151,
-3.11821642741899,-3.06778904700215,-3.05145196237189,-3.03973923673363,
-3.03415037267497,-3.02968538196736,-3.02398781229025,-3.0118123363106,
-2.94698203397978,-2.93186411164734,-2.88560078676851,-2.87268493316162,
-2.86423951203056,-2.85614471713959,-2.84643799289944,-2.82247190522749,
-2.73812598012657,-2.71801934401764,-2.70439812184665,-2.6984375285932,
-2.69393573458594,-2.68849957327305,-2.67805405001853,-2.62240817981378,
-2.5746329162323,-2.54575474923565,-2.53452556263767,-2.52640726863891,
-2.51890030133127,-2.50646958836968,-2.46934448982591,-2.39943761366767,
-2.37156973861686,-2.36395056390614,-2.35917606270683,-2.35499160524717,
-2.34799665369331,-2.3284502377363,-2.27032315783059,-2.21389269381728,
-2.20048802607827,-2.19195869010734,-2.18385593227559,-2.17267680296184,
-2.14588753507544,-2.06454709742011,-2.04464994359441,-2.03113510631806,
-2.02520618075471,-2.02071816153257,-2.01528587790108,-2.01517272200403),
 .UNSPECIFIED.);
#2261=B_SPLINE_CURVE_WITH_KNOTS('',3,(#52222,#52223,#52224,#52225,#52226,
#52227,#52228,#52229,#52230,#52231,#52232,#52233,#52234,#52235,#52236,#52237,
#52238,#52239,#52240,#52241,#52242,#52243,#52244,#52245,#52246,#52247,#52248,
#52249,#52250,#52251,#52252,#52253,#52254,#52255,#52256,#52257,#52258,#52259,
#52260,#52261,#52262,#52263,#52264,#52265,#52266,#52267,#52268,#52269,#52270,
#52271,#52272,#52273,#52274,#52275,#52276,#52277,#52278,#52279,#52280,#52281,
#52282,#52283,#52284,#52285,#52286,#52287,#52288,#52289,#52290,#52291,#52292,
#52293,#52294,#52295,#52296,#52297,#52298,#52299,#52300,#52301,#52302,#52303,
#52304,#52305,#52306,#52307,#52308,#52309,#52310,#52311,#52312,#52313,#52314,
#52315,#52316,#52317,#52318,#52319,#52320,#52321,#52322,#52323,#52324,#52325,
#52326,#52327,#52328,#52329,#52330,#52331,#52332,#52333,#52334,#52335,#52336,
#52337,#52338,#52339,#52340,#52341,#52342,#52343,#52344,#52345,#52346,#52347,
#52348,#52349,#52350,#52351,#52352,#52353,#52354,#52355,#52356,#52357,#52358,
#52359,#52360,#52361,#52362,#52363,#52364,#52365,#52366,#52367,#52368,#52369,
#52370,#52371,#52372,#52373,#52374,#52375,#52376,#52377,#52378,#52379,#52380,
#52381,#52382,#52383,#52384,#52385,#52386,#52387,#52388,#52389,#52390,#52391,
#52392,#52393,#52394,#52395,#52396,#52397),.UNSPECIFIED.,.F.,.F.,(4,2,2,
2,2,2,2,2,2,2,2,2,2,2,2,2,2,2,2,2,2,2,2,2,2,2,2,2,2,2,2,2,2,2,2,2,2,2,2,
2,2,2,2,2,2,2,2,2,2,2,2,2,2,2,2,2,2,2,2,2,2,2,2,2,2,2,2,2,2,2,2,2,2,2,2,
2,2,2,2,2,2,2,2,2,2,2,2,4),(-2.01517272200403,-2.00451421475811,-1.96106213155183,
-1.87951619754589,-1.86492309862471,-1.85614311422181,-1.84812622090925,
-1.83755726436441,-1.81324564606162,-1.77708203346033,-1.70369549294232,
-1.69307996863779,-1.68767734350376,-1.68318290544184,-1.67720460568732,
-1.66341335324765,-1.64293966426981,-1.55346008976567,-1.53259330238081,
-1.52259968181013,-1.5146479566336,-1.50554850677165,-1.48938602999012,
-1.4347071153928,-1.37072646907013,-1.35774588054285,-1.35196797134065,
-1.34748247238081,-1.34200777300546,-1.3310132088857,-1.31603793420628,
-1.27348537786853,-1.20912347912388,-1.19324792318433,-1.18411814316633,
-1.17617086320738,-1.16622377577733,-1.1456150627671,-1.11722019791397,
-1.05093302106982,-1.02531256885602,-1.01768284795244,-1.01290659752773,
-1.0081551939923,-1.00064276234197,-0.974082766992665,-0.911915808755105,
-0.86703122091171,-0.853922549591104,-0.845449779320622,-0.837306845451479,
-0.825915741171162,-0.79576116729459,-0.695354578463866,-0.683865194435322,
-0.678295195949978,-0.673813967315783,-0.668047991095213,-0.655488413935762,
-0.63752948906932,-0.575701553691541,-0.530441315366723,-0.51730861014069,
-0.508830588232313,-0.500689966397516,-0.489314451871821,-0.4592873642273,
-0.408092241917568,-0.357558247253426,-0.346880926698242,-0.341467588406309,
-0.336975847578333,-0.331017140459763,-0.317340732788108,-0.297107608098964,
-0.211268921629903,-0.187660629047367,-0.17731726515844,-0.169308914596127,
-0.160511666378622,-0.145825197766476,-0.127884076061152,-0.0873207091797893,
-0.0200345644038687,-0.0101360220370331,-0.00509855288362194,-0.00252798223428485,
-0.000974350499079791),.UNSPECIFIED.);
#2262=B_SPLINE_CURVE_WITH_KNOTS('',3,(#52398,#52399,#52400,#52401,#52402,
#52403,#52404,#52405,#52406,#52407,#52408,#52409),.UNSPECIFIED.,.F.,.F.,
(4,2,2,2,2,4),(-4.27068267614152,-4.26906071683224,-4.26567284309363,-4.25534850711771,
-4.18701167929227,-4.15012799910223),.UNSPECIFIED.);
#2263=B_SPLINE_CURVE_WITH_KNOTS('',3,(#52411,#52412,#52413,#52414,#52415,
#52416,#52417,#52418,#52419,#52420,#52421,#52422,#52423),.UNSPECIFIED.,
 .F.,.F.,(4,3,3,3,4),(-10.4883011219526,-10.3977630967638,-10.3072244319694,
-10.2166042167435,-10.133610752539),.UNSPECIFIED.);
#2264=B_SPLINE_CURVE_WITH_KNOTS('',3,(#52424,#52425,#52426,#52427,#52428,
#52429,#52430,#52431,#52432,#52433,#52434,#52435,#52436,#52437,#52438,#52439,
#52440,#52441,#52442,#52443,#52444,#52445,#52446,#52447,#52448,#52449,#52450,
#52451,#52452,#52453,#52454,#52455,#52456,#52457,#52458,#52459,#52460,#52461,
#52462,#52463,#52464,#52465,#52466,#52467,#52468,#52469,#52470,#52471,#52472,
#52473,#52474,#52475,#52476,#52477,#52478,#52479,#52480,#52481,#52482,#52483,
#52484,#52485,#52486,#52487,#52488,#52489,#52490,#52491,#52492,#52493,#52494,
#52495,#52496,#52497,#52498,#52499,#52500,#52501,#52502,#52503,#52504,#52505,
#52506,#52507,#52508,#52509,#52510,#52511,#52512,#52513,#52514,#52515,#52516,
#52517,#52518,#52519,#52520,#52521,#52522,#52523,#52524,#52525,#52526,#52527,
#52528,#52529,#52530,#52531,#52532,#52533,#52534,#52535,#52536,#52537,#52538,
#52539,#52540,#52541,#52542,#52543,#52544,#52545,#52546,#52547,#52548,#52549,
#52550,#52551,#52552,#52553,#52554,#52555,#52556,#52557,#52558,#52559,#52560,
#52561,#52562,#52563,#52564,#52565,#52566,#52567,#52568,#52569,#52570,#52571,
#52572,#52573,#52574,#52575,#52576,#52577,#52578,#52579,#52580,#52581,#52582,
#52583,#52584,#52585,#52586,#52587,#52588,#52589,#52590,#52591,#52592,#52593,
#52594,#52595,#52596,#52597,#52598,#52599,#52600,#52601),.UNSPECIFIED.,
 .F.,.F.,(4,2,2,2,2,2,2,2,2,2,2,2,2,2,2,2,2,2,2,2,2,2,2,2,2,2,2,2,2,2,2,
2,2,2,2,2,2,2,2,2,2,2,2,2,2,2,2,2,2,2,2,2,2,2,2,2,2,2,2,2,2,2,2,2,2,2,2,
2,2,2,2,2,2,2,2,2,2,2,2,2,2,2,2,2,2,2,2,2,4),(1.42896198809384,1.4676069046044,
1.49633027241518,1.50749827636214,1.5155673490849,1.5240365280871,1.53728877174833,
1.5856502766483,1.64518673674128,1.6712521509008,1.6786940485876,1.68341067942742,
1.68819090857537,1.69583141257155,1.72154466244348,1.78102387516357,1.82893164231001,
1.84221479084182,1.85073553946781,1.85887953677657,1.87019885072875,1.89969164795299,
1.94930827429658,2.00173039829016,2.0124269241899,2.01785490779613,2.02235727248275,
2.02833362993651,2.04209051972532,2.06248418843395,2.15077369753267,2.1724548842877,
2.18259358848788,2.19056211931748,2.19957632750544,2.21530288889363,2.26651687946367,
2.32322707232744,2.34464354272712,2.35186934148753,2.35609705492575,2.36081358114991,
2.36816706397028,2.39294998783131,2.44641636492676,2.50135512008876,2.51480899963436,
2.52334897391691,2.53144756370541,2.54259774884853,2.57093333455923,2.61716552701576,
2.67527627765604,2.68567969679657,2.69110154802672,2.69559135910075,2.70153415836735,
2.71511130517783,2.73513362263386,2.8180962147721,2.843405383942,2.85333937569815,
2.86148077414723,2.86982992057021,2.88230887593711,2.9228780881293,2.96449929249285,
3.01508129559219,3.02370613434759,3.02869859883741,3.03330426787174,3.04007886361942,
3.05941690492843,3.09352562777417,3.17153224569895,3.18654898104897,3.19541532466561,
3.20340816947816,3.21379660117432,3.23698277850097,3.27065804936337,3.32737136699031,
3.35346761275655,3.36114044099337,3.36592658200327,3.37066988522707,3.37814303984516,
3.38715189303689,3.44292570109838),.UNSPECIFIED.);
#2265=B_SPLINE_CURVE_WITH_KNOTS('',3,(#52604,#52605,#52606,#52607,#52608,
#52609,#52610,#52611,#52612,#52613,#52614,#52615,#52616,#52617,#52618,#52619,
#52620,#52621,#52622,#52623,#52624,#52625,#52626,#52627,#52628,#52629,#52630,
#52631,#52632,#52633,#52634,#52635,#52636,#52637,#52638,#52639,#52640,#52641,
#52642,#52643,#52644,#52645,#52646,#52647,#52648,#52649,#52650,#52651,#52652,
#52653,#52654,#52655,#52656,#52657,#52658,#52659,#52660,#52661,#52662,#52663,
#52664,#52665,#52666,#52667,#52668,#52669,#52670,#52671,#52672,#52673,#52674,
#52675,#52676,#52677,#52678,#52679,#52680,#52681,#52682,#52683,#52684,#52685,
#52686,#52687,#52688,#52689,#52690,#52691,#52692,#52693,#52694,#52695,#52696,
#52697,#52698,#52699,#52700,#52701,#52702,#52703,#52704,#52705,#52706,#52707,
#52708,#52709,#52710,#52711,#52712,#52713,#52714,#52715,#52716,#52717,#52718,
#52719,#52720,#52721,#52722,#52723,#52724,#52725,#52726,#52727,#52728,#52729,
#52730,#52731,#52732,#52733,#52734,#52735,#52736,#52737,#52738,#52739,#52740,
#52741,#52742,#52743,#52744,#52745,#52746,#52747,#52748),.UNSPECIFIED.,
 .F.,.F.,(4,3,3,3,3,3,3,3,3,3,3,3,3,3,3,3,3,3,3,3,3,3,3,3,3,3,3,3,3,3,3,
3,3,3,3,3,3,3,3,3,3,3,3,3,3,3,3,3,4),(17.9338728886362,18.0215470171645,
18.109145290346,18.1966963826855,18.2842238107557,18.3717482174281,18.4592902384062,
18.5469240273282,18.6346056657183,18.7224257637154,18.7919434588766,18.8797490912985,
18.9674437658401,19.0550504983712,19.1459907905069,19.233498614164,19.3209934256709,
19.4084958923916,19.4960266821179,19.5836543980516,19.6713396497812,19.7591505784758,
19.7825728354566,19.8703935858385,19.9581035608051,20.045725756466,20.1366603134123,
20.2241839074821,20.3116945756246,20.3992129681634,20.4867597358884,20.5744034271253,
20.6621046713552,20.7499314960658,20.7732022120367,20.8610213198291,20.9487296628209,
21.0363502391096,21.127285407798,21.2148074249428,21.3023165347146,21.3898333892518,
21.4773786411749,21.5650208574271,21.6527206487517,21.740546064198,21.7638315886167,
21.8810147460357,21.9911485751285),.UNSPECIFIED.);
#2266=B_SPLINE_CURVE_WITH_KNOTS('',3,(#52749,#52750,#52751,#52752,#52753,
#52754,#52755,#52756,#52757,#52758,#52759,#52760,#52761,#52762,#52763,#52764,
#52765,#52766,#52767,#52768,#52769,#52770,#52771,#52772,#52773,#52774,#52775,
#52776,#52777,#52778,#52779,#52780,#52781,#52782,#52783,#52784,#52785,#52786,
#52787,#52788,#52789,#52790,#52791,#52792,#52793,#52794,#52795,#52796,#52797,
#52798,#52799,#52800,#52801,#52802,#52803,#52804,#52805,#52806,#52807,#52808,
#52809,#52810,#52811,#52812,#52813,#52814,#52815,#52816,#52817,#52818,#52819,
#52820,#52821,#52822,#52823,#52824,#52825,#52826,#52827,#52828,#52829,#52830),
 .UNSPECIFIED.,.F.,.F.,(4,3,3,3,3,3,3,3,3,3,3,3,3,3,3,3,3,3,3,3,3,3,3,3,
3,3,3,4),(21.9911485753198,22.0776479350916,22.1640847934423,22.2504889236019,
22.3368820188365,22.4232857594527,22.5097743554891,22.5963065092834,22.6829750966663,
22.7544609651967,22.842279179636,22.9299866032483,23.0176062353834,23.1085417486826,
23.1960627655776,23.2835708560414,23.3710866732419,23.4586308708177,23.5462720126386,
23.6339707165569,23.7217950337417,23.7450903417767,23.8329109711975,23.9206243020769,
24.0082360027158,24.0957890755062,24.1833037493284,24.2166325387365),
 .UNSPECIFIED.);
#2267=B_SPLINE_CURVE_WITH_KNOTS('',3,(#52832,#52833,#52834,#52835,#52836,
#52837,#52838,#52839,#52840,#52841,#52842,#52843,#52844,#52845,#52846,#52847,
#52848,#52849,#52850,#52851,#52852,#52853,#52854,#52855,#52856,#52857,#52858,
#52859,#52860,#52861,#52862,#52863,#52864,#52865,#52866,#52867,#52868,#52869,
#52870,#52871,#52872,#52873,#52874,#52875,#52876,#52877,#52878,#52879,#52880,
#52881,#52882,#52883,#52884,#52885,#52886,#52887,#52888,#52889,#52890,#52891,
#52892,#52893,#52894,#52895,#52896,#52897,#52898,#52899,#52900,#52901,#52902,
#52903,#52904,#52905,#52906,#52907,#52908,#52909,#52910,#52911,#52912,#52913),
 .UNSPECIFIED.,.F.,.F.,(4,3,3,3,3,3,3,3,3,3,3,3,3,3,3,3,3,3,3,3,3,3,3,3,
3,3,3,4),(21.9911485753334,22.0925692444526,22.1945700829516,22.2972271432548,
22.3241606593577,22.4119814069087,22.4996913790177,22.5873135717981,22.6782481298156,
22.7657717209657,22.8532823861793,22.9408007757831,23.0283475405699,23.1159912288789,
23.2036924701836,23.2915192919947,23.3147900359378,23.4026144680511,23.4903268534229,
23.5810561989288,23.6686091896034,23.75612672866,23.8436294826255,23.9311381021069,
24.0187103272813,24.1063207651217,24.1940286371691,24.21616161747),
 .UNSPECIFIED.);
#2268=B_SPLINE_CURVE_WITH_KNOTS('',3,(#52914,#52915,#52916,#52917,#52918,
#52919,#52920,#52921,#52922,#52923,#52924,#52925,#52926,#52927,#52928,#52929,
#52930,#52931,#52932,#52933,#52934,#52935,#52936,#52937,#52938,#52939,#52940,
#52941,#52942,#52943,#52944,#52945,#52946,#52947,#52948,#52949,#52950,#52951,
#52952,#52953,#52954,#52955,#52956,#52957,#52958,#52959,#52960,#52961,#52962,
#52963,#52964,#52965,#52966,#52967,#52968,#52969,#52970,#52971,#52972,#52973,
#52974,#52975,#52976,#52977,#52978,#52979,#52980,#52981,#52982,#52983,#52984,
#52985,#52986,#52987,#52988,#52989,#52990,#52991,#52992,#52993,#52994,#52995,
#52996,#52997,#52998,#52999,#53000,#53001,#53002,#53003,#53004,#53005,#53006,
#53007,#53008,#53009,#53010,#53011,#53012,#53013,#53014,#53015,#53016,#53017,
#53018,#53019,#53020,#53021,#53022,#53023,#53024,#53025,#53026,#53027,#53028,
#53029,#53030,#53031,#53032,#53033,#53034,#53035,#53036,#53037,#53038,#53039,
#53040,#53041,#53042,#53043,#53044,#53045,#53046,#53047,#53048,#53049,#53050,
#53051,#53052,#53053,#53054,#53055,#53056,#53057,#53058,#53059,#53060,#53061),
 .UNSPECIFIED.,.F.,.F.,(4,3,3,3,3,3,3,3,3,3,3,3,3,3,3,3,3,3,3,3,3,3,3,3,
3,3,3,3,3,3,3,3,3,3,3,3,3,3,3,3,3,3,3,3,3,3,3,3,3,4),(17.9331385422654,
18.0208128771327,18.1085789253771,18.1963916734127,18.2843454815269,18.3616431530376,
18.449367930366,18.5369807394303,18.6245047002394,18.7154756789117,18.8028989874472,
18.8903087837302,18.9777258246176,19.0651708671648,19.152712785992,19.2403121091229,
19.3280375700532,19.3522725296177,19.4401067612013,19.5278302375573,19.6154659378553,
19.7063954338981,19.7939324510954,19.8814564882501,19.9689881806001,20.0565481637901,
20.1442048777122,20.2319190473871,20.3197585556779,20.3429019061977,20.4307340335604,
20.5184556443017,20.6060897189339,20.6970199144144,20.784555920573,20.8720791767411,
20.9596103201831,21.047169988739,21.1348267395123,21.2225411511409,21.3103812019963,
21.3335312827777,21.421325086341,21.5090102364101,21.5966075330255,21.6841377047948,
21.7716264493274,21.8590906176265,21.9465691639125,21.9911485751285),
 .UNSPECIFIED.);
#2269=B_SPLINE_CURVE_WITH_KNOTS('',3,(#53064,#53065,#53066,#53067,#53068,
#53069,#53070,#53071,#53072,#53073,#53074,#53075,#53076,#53077,#53078,#53079,
#53080,#53081,#53082,#53083,#53084,#53085,#53086,#53087,#53088,#53089,#53090,
#53091,#53092,#53093,#53094,#53095,#53096,#53097,#53098,#53099,#53100,#53101,
#53102,#53103,#53104,#53105,#53106,#53107,#53108,#53109,#53110,#53111,#53112,
#53113,#53114,#53115,#53116,#53117,#53118,#53119,#53120,#53121,#53122,#53123,
#53124,#53125,#53126,#53127,#53128,#53129,#53130,#53131,#53132,#53133,#53134,
#53135,#53136,#53137,#53138,#53139,#53140,#53141,#53142,#53143,#53144,#53145,
#53146,#53147,#53148,#53149,#53150,#53151,#53152,#53153,#53154,#53155,#53156,
#53157,#53158,#53159,#53160,#53161,#53162,#53163,#53164,#53165,#53166,#53167,
#53168,#53169,#53170,#53171,#53172,#53173,#53174,#53175,#53176,#53177,#53178,
#53179,#53180,#53181,#53182,#53183,#53184,#53185,#53186,#53187,#53188,#53189,
#53190,#53191,#53192,#53193,#53194,#53195,#53196,#53197,#53198,#53199,#53200,
#53201,#53202,#53203,#53204,#53205,#53206,#53207,#53208,#53209,#53210,#53211,
#53212,#53213,#53214,#53215,#53216,#53217,#53218,#53219,#53220,#53221,#53222,
#53223,#53224,#53225,#53226,#53227,#53228,#53229,#53230,#53231,#53232,#53233,
#53234,#53235,#53236,#53237,#53238,#53239,#53240,#53241),.UNSPECIFIED.,
 .F.,.F.,(4,2,2,2,2,2,2,2,2,2,2,2,2,2,2,2,2,2,2,2,2,2,2,2,2,2,2,2,2,2,2,
2,2,2,2,2,2,2,2,2,2,2,2,2,2,2,2,2,2,2,2,2,2,2,2,2,2,2,2,2,2,2,2,2,2,2,2,
2,2,2,2,2,2,2,2,2,2,2,2,2,2,2,2,2,2,2,2,2,4),(-2.01510602195132,-2.0044317114712,
-1.96086731396523,-1.87949599766812,-1.86487540474218,-1.85608815869749,
-1.84807038027914,-1.83750866339353,-1.81325484667234,-1.77722657183864,
-1.70350257554885,-1.69306672196303,-1.68763383237778,-1.68314108510995,
-1.6772000959313,-1.6636390055709,-1.64364926666656,-1.56120372012365,-1.53540663865066,
-1.52542898772208,-1.51801717690807,-1.50981563675015,-1.49810995219668,
-1.46536847004356,-1.40484166951035,-1.36333421682153,-1.3548606689335,
-1.34990125877571,-1.34527920866447,-1.33841487704988,-1.31833650282153,
-1.28203942000067,-1.20806208840535,-1.1926999558903,-1.18367771130796,
-1.17571266540575,-1.16559288782027,-1.14401382787951,-1.11369663955315,
-1.07539876741578,-1.03073039487558,-1.01995710283299,-1.01452415556432,
-1.01003293556814,-1.00409665429345,-0.99056026333586,-0.970620902600873,
-0.888820995130883,-0.862431544129402,-0.851298906545881,-0.843197568132834,
-0.834640384824886,-0.821127484121622,-0.761499315502669,-0.697519577552796,
-0.684544058961901,-0.67876561523136,-0.67427829789425,-0.668799256910654,
-0.65778942132117,-0.64278773401885,-0.600103559402819,-0.535928015486579,
-0.52004600642507,-0.510912491352526,-0.502961801435924,-0.493010086867018,
-0.472389476168545,-0.443974486443278,-0.37757160740112,-0.352080491709411,
-0.344459917436211,-0.339684332581721,-0.334928725731316,-0.327401144965952,
-0.300677559471162,-0.237623252380554,-0.193682918097719,-0.180635753336664,
-0.17217381440158,-0.164020425050653,-0.152579434675949,-0.122043130566837,
-0.0710903605481419,-0.021239433825702,-0.0106102094200809,-0.00529049879569223,
-0.00261560889277293,-0.000972523347507427),.UNSPECIFIED.);
#2270=B_SPLINE_CURVE_WITH_KNOTS('',3,(#53242,#53243,#53244,#53245,#53246,
#53247,#53248,#53249,#53250,#53251,#53252,#53253),.UNSPECIFIED.,.F.,.F.,
(4,2,2,2,2,4),(-4.2710288732429,-4.26942616966666,-4.26606147541147,-4.25584756501187,
-4.18561723202379,-4.15046929847984),.UNSPECIFIED.);
#2271=B_SPLINE_CURVE_WITH_KNOTS('',3,(#53255,#53256,#53257,#53258,#53259,
#53260,#53261,#53262,#53263,#53264,#53265,#53266,#53267),.UNSPECIFIED.,
 .F.,.F.,(4,3,3,3,4),(-10.4882942077004,-10.3977555936811,-10.3072163406073,
-10.2165955445259,-10.1336107524811),.UNSPECIFIED.);
#2272=B_SPLINE_CURVE_WITH_KNOTS('',3,(#53268,#53269,#53270,#53271,#53272,
#53273,#53274,#53275,#53276,#53277,#53278,#53279,#53280,#53281,#53282,#53283,
#53284,#53285,#53286,#53287,#53288,#53289,#53290,#53291,#53292,#53293,#53294,
#53295,#53296,#53297,#53298,#53299,#53300,#53301,#53302,#53303,#53304,#53305,
#53306,#53307,#53308,#53309,#53310,#53311,#53312,#53313,#53314,#53315,#53316,
#53317,#53318,#53319,#53320,#53321,#53322,#53323,#53324,#53325,#53326,#53327,
#53328,#53329,#53330,#53331,#53332,#53333,#53334,#53335,#53336,#53337,#53338,
#53339,#53340,#53341,#53342,#53343,#53344,#53345,#53346,#53347,#53348,#53349,
#53350,#53351,#53352,#53353,#53354,#53355,#53356,#53357,#53358,#53359,#53360,
#53361,#53362,#53363,#53364,#53365,#53366,#53367,#53368,#53369,#53370,#53371,
#53372,#53373,#53374,#53375,#53376,#53377,#53378,#53379,#53380,#53381,#53382,
#53383,#53384,#53385,#53386,#53387,#53388,#53389,#53390,#53391,#53392,#53393,
#53394,#53395,#53396,#53397,#53398,#53399,#53400,#53401,#53402,#53403,#53404,
#53405,#53406,#53407,#53408,#53409,#53410,#53411,#53412,#53413,#53414,#53415,
#53416,#53417,#53418,#53419,#53420,#53421,#53422,#53423,#53424,#53425,#53426,
#53427,#53428,#53429,#53430,#53431,#53432,#53433,#53434,#53435,#53436,#53437,
#53438,#53439,#53440,#53441,#53442,#53443),.UNSPECIFIED.,.F.,.F.,(4,2,2,
2,2,2,2,2,2,2,2,2,2,2,2,2,2,2,2,2,2,2,2,2,2,2,2,2,2,2,2,2,2,2,2,2,2,2,2,
2,2,2,2,2,2,2,2,2,2,2,2,2,2,2,2,2,2,2,2,2,2,2,2,2,2,2,2,2,2,2,2,2,2,2,2,
2,2,2,2,2,2,2,2,2,2,2,2,4),(1.42897696838616,1.46741399900062,1.4962817479625,
1.50747664149338,1.51555765934761,1.52403315896472,1.53728303602105,1.58537646119945,
1.64510865215483,1.67121576218021,1.67866660797506,1.68338860514827,1.68816973070354,
1.69581320288804,1.72155830573022,1.78120631517213,1.82889207245565,1.84216294039551,
1.85067949012597,1.85882195563953,1.87014297564165,1.89966061686505,1.94933774210726,
2.00176272089881,2.01246140564018,2.01788787305856,2.02238900944671,2.02836248149229,
2.04210041037211,2.06245363617006,2.15010509400306,2.17227445881266,2.18249818450072,
2.19047736960002,2.19944523199193,2.21493670413336,2.26438130308697,2.33884697895409,
2.34917345804516,2.35458322536127,2.35907669657421,2.365044492506,2.37877582324682,
2.39912186739911,2.48670846944777,2.50678412169201,2.51674076021563,2.52414497203279,
2.53234581491239,2.54406530112091,2.57695399226888,2.63803562873668,2.67894607028684,
2.68740441471095,2.69235881500317,2.69698225534397,2.70385339807908,2.72398463101445,
2.76043868950381,2.83408916429931,2.84948139257655,2.85851191435645,2.86568181947272,
2.87539621406065,2.89470112244532,2.97069396812108,3.01544306822901,3.02395342326548,
3.02892203382812,3.0335418016751,3.04038829051741,3.06030844694979,3.09612412908314,
3.17102746566376,3.18640753138475,3.19535063730725,3.20333113420022,3.21358891054149,
3.23597107785262,3.26793788023563,3.32626235462994,3.35340566644226,3.36119484109002,
3.36600727683016,3.37073089151171,3.37810455280796,3.3869574035366,3.44309910570526),
 .UNSPECIFIED.);
#2273=B_SPLINE_CURVE_WITH_KNOTS('',3,(#53446,#53447,#53448,#53449,#53450,
#53451,#53452,#53453,#53454,#53455,#53456,#53457,#53458,#53459,#53460,#53461,
#53462,#53463,#53464,#53465,#53466,#53467,#53468,#53469,#53470,#53471,#53472,
#53473,#53474,#53475,#53476,#53477,#53478,#53479,#53480,#53481,#53482,#53483,
#53484,#53485,#53486,#53487,#53488,#53489,#53490,#53491,#53492,#53493,#53494,
#53495,#53496,#53497,#53498,#53499,#53500,#53501,#53502,#53503,#53504,#53505,
#53506,#53507,#53508,#53509,#53510,#53511,#53512,#53513,#53514,#53515,#53516,
#53517,#53518,#53519,#53520,#53521,#53522,#53523,#53524,#53525,#53526,#53527,
#53528,#53529,#53530,#53531,#53532,#53533,#53534,#53535,#53536,#53537,#53538,
#53539,#53540,#53541,#53542,#53543,#53544,#53545,#53546,#53547,#53548,#53549,
#53550,#53551,#53552,#53553,#53554,#53555,#53556,#53557,#53558,#53559,#53560,
#53561,#53562,#53563,#53564,#53565,#53566,#53567,#53568,#53569,#53570,#53571,
#53572,#53573,#53574,#53575,#53576,#53577,#53578,#53579,#53580,#53581,#53582,
#53583,#53584,#53585,#53586,#53587,#53588,#53589,#53590),.UNSPECIFIED.,
 .F.,.F.,(4,3,3,3,3,3,3,3,3,3,3,3,3,3,3,3,3,3,3,3,3,3,3,3,3,3,3,3,3,3,3,
3,3,3,3,3,3,3,3,3,3,3,3,3,3,3,3,3,4),(17.9338702011125,18.0215425533029,
18.1091390113459,18.1966882365676,18.2842137661014,18.37173624473,18.4592763100473,
18.5469081112597,18.6345877412305,18.7224058161635,18.7919434588766,18.8797523806305,
18.9674503898695,19.0550604981952,19.1459995403529,19.2335108212493,19.3210091141967,
19.4085150829,19.4960493915041,19.5836806339246,19.6713694207407,19.7591838703614,
19.7825728354566,19.8703922597118,19.9581008960562,20.0457217423095,20.1366568010254,
20.2241790274407,20.3116883235665,20.3992053412126,20.4867507326539,20.574393052463,
20.6620929264883,20.749918393224,20.7732022120366,20.8610210912083,20.948729198936,
21.0363495336298,21.1272847905032,21.2148065516797,21.3023154005905,21.3898319896304,
21.4773769716732,21.565018912844,21.6527184257294,21.7405435598915,21.7638315886167,
21.8810158240277,21.9911485751285),.UNSPECIFIED.);
#2274=B_SPLINE_CURVE_WITH_KNOTS('',3,(#53591,#53592,#53593,#53594,#53595,
#53596,#53597,#53598,#53599,#53600,#53601,#53602,#53603,#53604,#53605,#53606,
#53607,#53608,#53609,#53610,#53611,#53612,#53613,#53614,#53615,#53616,#53617,
#53618,#53619,#53620,#53621,#53622,#53623,#53624,#53625,#53626,#53627,#53628,
#53629,#53630,#53631,#53632,#53633,#53634,#53635,#53636,#53637,#53638,#53639,
#53640,#53641,#53642,#53643,#53644,#53645,#53646,#53647,#53648,#53649,#53650,
#53651,#53652,#53653,#53654,#53655,#53656,#53657,#53658,#53659,#53660,#53661,
#53662,#53663,#53664,#53665,#53666,#53667,#53668,#53669,#53670,#53671,#53672),
 .UNSPECIFIED.,.F.,.F.,(4,3,3,3,3,3,3,3,3,3,3,3,3,3,3,3,3,3,3,3,3,3,3,3,
3,3,3,4),(21.991148575271,22.0776484880045,22.1640859049774,22.2504905972469,
22.3368842576987,22.4232885662622,22.5097777320238,22.5963104573412,22.6829796147006,
22.7544609651967,22.8422789538582,22.9299861494228,23.0176055515318,23.1085411503124,
23.1960619337185,23.2835697898192,23.3710853720355,23.4586293342593,23.5462702413632,
23.6339687106596,23.7217927951481,23.7450903417767,23.8329109525581,23.9206242639271,
24.0082359437503,24.0957889950546,24.183303645942,24.2166288630184),
 .UNSPECIFIED.);
#2275=B_SPLINE_CURVE_WITH_KNOTS('',3,(#53674,#53675,#53676,#53677,#53678,
#53679,#53680,#53681,#53682,#53683,#53684,#53685,#53686,#53687,#53688,#53689,
#53690,#53691,#53692,#53693,#53694,#53695,#53696,#53697,#53698,#53699,#53700,
#53701,#53702,#53703,#53704,#53705,#53706,#53707,#53708,#53709,#53710,#53711,
#53712,#53713,#53714,#53715,#53716,#53717,#53718,#53719,#53720,#53721,#53722,
#53723,#53724,#53725,#53726,#53727,#53728,#53729,#53730,#53731,#53732,#53733,
#53734,#53735,#53736,#53737,#53738,#53739,#53740,#53741,#53742,#53743,#53744,
#53745,#53746,#53747,#53748,#53749,#53750,#53751,#53752,#53753,#53754,#53755),
 .UNSPECIFIED.,.F.,.F.,(4,3,3,3,3,3,3,3,3,3,3,3,3,3,3,3,3,3,3,3,3,3,3,3,
3,3,3,4),(21.991148575328,22.0925750235656,22.1945818624572,22.297244987739,
22.3241606593577,22.4119800908502,22.4996887345,22.5873095881174,22.6782446440949,
22.7657668779734,22.8532761815859,22.940793206734,23.0283386056848,23.1159809329764,
23.2036808144772,23.2915062886212,23.3147900359377,23.4026142419743,23.4903263946006,
23.5810553110645,23.6686080538086,23.756125339587,23.8436278351851,23.931136191465,
24.0187081467531,24.1063183109976,24.1940259041244,24.2161577263113),
 .UNSPECIFIED.);
#2276=B_SPLINE_CURVE_WITH_KNOTS('',3,(#53756,#53757,#53758,#53759,#53760,
#53761,#53762,#53763,#53764,#53765,#53766,#53767,#53768,#53769,#53770,#53771,
#53772,#53773,#53774,#53775,#53776,#53777,#53778,#53779,#53780,#53781,#53782,
#53783,#53784,#53785,#53786,#53787,#53788,#53789,#53790,#53791,#53792,#53793,
#53794,#53795,#53796,#53797,#53798,#53799,#53800,#53801,#53802,#53803,#53804,
#53805,#53806,#53807,#53808,#53809,#53810,#53811,#53812,#53813,#53814,#53815,
#53816,#53817,#53818,#53819,#53820,#53821,#53822,#53823,#53824,#53825,#53826,
#53827,#53828,#53829,#53830,#53831,#53832,#53833,#53834,#53835,#53836,#53837,
#53838,#53839,#53840,#53841,#53842,#53843,#53844,#53845,#53846,#53847,#53848,
#53849,#53850,#53851,#53852,#53853,#53854,#53855,#53856,#53857,#53858,#53859,
#53860,#53861,#53862,#53863,#53864,#53865,#53866,#53867,#53868,#53869,#53870,
#53871,#53872,#53873,#53874,#53875,#53876,#53877,#53878,#53879,#53880,#53881,
#53882,#53883,#53884,#53885,#53886,#53887,#53888,#53889,#53890,#53891,#53892,
#53893,#53894,#53895,#53896,#53897,#53898,#53899,#53900,#53901,#53902,#53903),
 .UNSPECIFIED.,.F.,.F.,(4,3,3,3,3,3,3,3,3,3,3,3,3,3,3,3,3,3,3,3,3,3,3,3,
3,3,3,3,3,3,3,3,3,3,3,3,3,3,3,3,3,3,3,3,3,3,3,3,3,4),(17.9331346486732,
18.0208008418309,18.1085586009925,18.1963629732292,18.2843083139475,18.3616431530376,
18.449386361552,18.5370178462857,18.6245607041036,18.7155246822929,18.8029673258297,
18.8903965868309,18.9778332023575,19.0652979097325,19.1528595308134,19.2404786018306,
19.3282237282067,19.3522725296176,19.4400992041747,19.5278150523077,19.6154430629779,
19.7063754183804,19.7939046423309,19.8814208615799,19.9689447198792,20.0564968613797,
20.1441457617657,20.2318521252015,20.3196838973925,20.3429019061977,20.4307323340458,
20.5184522034034,20.6060844970501,20.6970153452661,20.7845494822013,20.8720708396058,
20.9596000566279,21.0471577729739,21.1348125427106,21.2225249541539,21.3103629916908,
21.3335312827777,21.4213282095817,21.5090165240303,21.5966170225215,21.6841504300686,
21.771642449676,21.8591099162917,21.9465917807573,21.9911485751285),
 .UNSPECIFIED.);
#2277=B_SPLINE_CURVE_WITH_KNOTS('',3,(#53906,#53907,#53908,#53909,#53910,
#53911,#53912,#53913,#53914,#53915,#53916,#53917,#53918,#53919,#53920,#53921,
#53922,#53923,#53924,#53925,#53926,#53927,#53928,#53929,#53930,#53931,#53932,
#53933,#53934,#53935,#53936,#53937,#53938,#53939,#53940,#53941,#53942,#53943,
#53944,#53945,#53946,#53947,#53948,#53949,#53950,#53951,#53952,#53953,#53954,
#53955,#53956,#53957,#53958,#53959,#53960,#53961,#53962,#53963,#53964,#53965,
#53966,#53967,#53968,#53969,#53970,#53971,#53972,#53973,#53974,#53975,#53976,
#53977,#53978,#53979,#53980,#53981,#53982,#53983,#53984,#53985,#53986,#53987,
#53988,#53989,#53990,#53991,#53992,#53993,#53994,#53995,#53996,#53997,#53998,
#53999,#54000,#54001,#54002,#54003,#54004,#54005,#54006,#54007,#54008,#54009,
#54010,#54011,#54012,#54013,#54014,#54015,#54016,#54017,#54018,#54019,#54020,
#54021,#54022,#54023,#54024,#54025,#54026,#54027,#54028,#54029,#54030,#54031,
#54032,#54033,#54034,#54035,#54036,#54037,#54038,#54039,#54040,#54041,#54042,
#54043,#54044,#54045,#54046,#54047,#54048,#54049,#54050,#54051,#54052,#54053,
#54054,#54055,#54056,#54057,#54058,#54059,#54060,#54061,#54062,#54063,#54064,
#54065,#54066,#54067,#54068,#54069,#54070,#54071,#54072,#54073,#54074,#54075,
#54076,#54077),.UNSPECIFIED.,.F.,.F.,(4,2,2,2,2,2,2,2,2,2,2,2,2,2,2,2,2,
2,2,2,2,2,2,2,2,2,2,2,2,2,2,2,2,2,2,2,2,2,2,2,2,2,2,2,2,2,2,2,2,2,2,2,2,
2,2,2,2,2,2,2,2,2,2,2,2,2,2,2,2,2,2,2,2,2,2,2,2,2,2,2,2,2,2,2,2,4),(-2.01551729291411,
-2.00485584560195,-1.9613915699149,-1.87982452303997,-1.86522737907853,
-1.85644500508538,-1.84842595738612,-1.83785420115296,-1.81353634332151,
-1.77736369470597,-1.70395574528014,-1.69333764465119,-1.68793362022894,
-1.68343796383025,-1.67745797292388,-1.6636625306281,-1.64318232872964,
-1.55366278916108,-1.53280190555801,-1.52280762463715,-1.51485391558332,
-1.50575061817829,-1.48957690053267,-1.43482754925375,-1.3707039488082,
-1.35908927001258,-1.35340586146658,-1.34884603156413,-1.34387258184106,
-1.33533020945826,-1.28751745267307,-1.20672559278948,-1.19202597681336,
-1.18322540000485,-1.17521692252114,-1.16469923606476,-1.14070480745836,
-1.10525773627288,-1.03012385305295,-1.01993357496737,-1.01455413556473,
-1.01005787674292,-1.00405044403608,-0.990084278654935,-0.969241387422245,
-0.873420503508213,-0.857034650446284,-0.847795136008765,-0.839855203327756,
-0.830050051574538,-0.810236190278846,-0.783370261830456,-0.741177824036141,
-0.69061076330626,-0.681987282930691,-0.676996515365108,-0.672392333456984,
-0.665621325643081,-0.646307595833169,-0.612265525127834,-0.534186499210383,
-0.51912275174109,-0.510247270411892,-0.502257491914246,-0.491889169034531,
-0.468821161619825,-0.435400792448215,-0.369554225159334,-0.350664203474423,
-0.343753450025736,-0.339169526250929,-0.334243640603721,-0.325921163238598,
-0.285642987253449,-0.198226315501195,-0.182821766418207,-0.173876946954676,
-0.165902457938223,-0.155663032031858,-0.133367585790185,-0.101577600200077,
-0.0380060262036244,-0.0150834299228487,-0.00785356191111222,-0.00370416980883594,
-0.000974342611802808),.UNSPECIFIED.);
#2278=B_SPLINE_CURVE_WITH_KNOTS('',3,(#54078,#54079,#54080,#54081,#54082,
#54083,#54084,#54085,#54086,#54087,#54088,#54089),.UNSPECIFIED.,.F.,.F.,
(4,2,2,2,2,4),(-4.27068267975062,-4.26906145758045,-4.26567463808812,-4.25535529738831,
-4.18692414937688,-4.15012784700328),.UNSPECIFIED.);
#2279=B_SPLINE_CURVE_WITH_KNOTS('',3,(#54091,#54092,#54093,#54094,#54095,
#54096,#54097,#54098,#54099,#54100,#54101,#54102,#54103),.UNSPECIFIED.,
 .F.,.F.,(4,3,3,3,4),(-10.4883010731468,-10.397763044796,-10.3072243768395,
-10.216604158493,-10.1336107525393),.UNSPECIFIED.);
#2280=B_SPLINE_CURVE_WITH_KNOTS('',3,(#54104,#54105,#54106,#54107,#54108,
#54109,#54110,#54111,#54112,#54113,#54114,#54115,#54116,#54117,#54118,#54119,
#54120,#54121,#54122,#54123,#54124,#54125,#54126,#54127,#54128,#54129,#54130,
#54131,#54132,#54133,#54134,#54135,#54136,#54137,#54138,#54139,#54140,#54141,
#54142,#54143,#54144,#54145,#54146,#54147,#54148,#54149,#54150,#54151,#54152,
#54153,#54154,#54155,#54156,#54157,#54158,#54159,#54160,#54161,#54162,#54163,
#54164,#54165,#54166,#54167,#54168,#54169,#54170,#54171,#54172,#54173,#54174,
#54175,#54176,#54177,#54178,#54179,#54180,#54181,#54182,#54183,#54184,#54185,
#54186,#54187,#54188,#54189,#54190,#54191,#54192,#54193,#54194,#54195,#54196,
#54197,#54198,#54199,#54200,#54201,#54202,#54203,#54204,#54205,#54206,#54207,
#54208,#54209,#54210,#54211,#54212,#54213,#54214,#54215,#54216,#54217,#54218,
#54219,#54220,#54221,#54222,#54223,#54224,#54225,#54226,#54227,#54228,#54229,
#54230,#54231,#54232,#54233,#54234,#54235,#54236,#54237,#54238,#54239,#54240,
#54241,#54242,#54243,#54244,#54245,#54246,#54247,#54248,#54249,#54250,#54251,
#54252,#54253,#54254,#54255,#54256,#54257,#54258,#54259,#54260,#54261,#54262,
#54263,#54264,#54265,#54266,#54267,#54268,#54269,#54270,#54271,#54272,#54273,
#54274,#54275,#54276,#54277,#54278,#54279,#54280,#54281),.UNSPECIFIED.,
 .F.,.F.,(4,2,2,2,2,2,2,2,2,2,2,2,2,2,2,2,2,2,2,2,2,2,2,2,2,2,2,2,2,2,2,
2,2,2,2,2,2,2,2,2,2,2,2,2,2,2,2,2,2,2,2,2,2,2,2,2,2,2,2,2,2,2,2,2,2,2,2,
2,2,2,2,2,2,2,2,2,2,2,2,2,2,2,2,2,2,2,2,2,4),(1.42896226070502,1.46760630807409,
1.49633027514612,1.50749839411284,1.51556752003582,1.52403673018617,1.53728897428289,
1.5856494956979,1.64518666713393,1.67125223828278,1.67869417368618,1.68341082794888,
1.68819106050374,1.69583157802488,1.72154498345669,1.78102501648932,1.82893172626393,
1.84221481544433,1.85073554231687,1.85887952965337,1.87019884611771,1.89969173097079,
1.94930855097605,2.00173087151417,2.01242740034867,2.01785537427144,2.02235773171005,
2.02833407399051,2.04209087049889,2.0624843409397,2.15077067139438,2.17245429937023,
2.18259343056372,2.19056201115673,2.19957597506071,2.21530130486682,2.26650589711478,
2.32319739803509,2.34463814477,2.3518667079049,2.35609493908851,2.36081086712881,
2.36816144281155,2.39291279821649,2.44623889947685,2.50134065548667,2.51480195401738,
2.52334346069836,2.53144130861827,2.54258691783137,2.57088859138895,2.61702655972888,
2.67526013133429,2.68567373581047,2.69109771876124,2.69558732092313,2.70152728280376,
2.71508756196999,2.73507475771854,2.81756899567094,2.84329917656217,2.85327126333096,
2.86068193557275,2.86888518304589,2.8805991291241,2.91341048992409,2.97421532664369,
3.01538147111956,3.023848666603,3.02880742911736,3.03343054553154,3.0403003236911,
3.06042763051094,3.09687264547184,3.17066339032726,3.18597708686976,3.19498813737077,
3.20295360792355,3.21308789873877,3.23475506836586,3.26525360577859,3.32507674682859,
3.35312000980341,3.36097522902233,3.36580074958091,3.37051004368903,3.37782039401938,
3.38657571455232,3.44294074553524),.UNSPECIFIED.);
#2281=B_SPLINE_CURVE_WITH_KNOTS('',3,(#54284,#54285,#54286,#54287,#54288,
#54289,#54290,#54291,#54292,#54293,#54294,#54295,#54296,#54297,#54298,#54299,
#54300,#54301,#54302,#54303,#54304,#54305,#54306,#54307,#54308,#54309,#54310,
#54311,#54312,#54313,#54314,#54315,#54316,#54317,#54318,#54319,#54320,#54321,
#54322,#54323,#54324,#54325,#54326,#54327,#54328,#54329,#54330,#54331,#54332,
#54333,#54334,#54335,#54336,#54337,#54338,#54339,#54340,#54341,#54342,#54343,
#54344,#54345,#54346,#54347,#54348,#54349,#54350,#54351,#54352,#54353,#54354,
#54355,#54356,#54357,#54358,#54359,#54360,#54361,#54362,#54363,#54364,#54365,
#54366,#54367,#54368,#54369,#54370,#54371,#54372,#54373,#54374,#54375,#54376,
#54377,#54378,#54379,#54380,#54381,#54382,#54383,#54384,#54385,#54386,#54387,
#54388,#54389,#54390,#54391,#54392,#54393,#54394,#54395,#54396,#54397,#54398,
#54399,#54400,#54401,#54402,#54403,#54404,#54405,#54406,#54407,#54408,#54409,
#54410,#54411,#54412,#54413,#54414,#54415,#54416,#54417,#54418,#54419,#54420,
#54421,#54422,#54423,#54424,#54425,#54426,#54427,#54428),.UNSPECIFIED.,
 .F.,.F.,(4,3,3,3,3,3,3,3,3,3,3,3,3,3,3,3,3,3,3,3,3,3,3,3,3,3,3,3,3,3,3,
3,3,3,3,3,3,3,3,3,3,3,3,3,3,3,3,3,4),(17.9338728552279,18.0215469755457,
18.1091452403261,18.1966963240079,18.2842237432648,18.3717481409769,18.4592901528567,
18.5469239325214,18.6346055615492,18.7224256501151,18.7919434588766,18.8797491078548,
18.9674437991789,19.0550505486975,19.1459908345424,19.2334986755925,19.3209935046125,
19.4084959889484,19.4960267963733,19.583654530042,19.6713397995486,19.7591507459476,
19.7825728354566,19.870393578819,19.9581035467,20.0457257352183,20.1366602948206,
20.2241838816509,20.3116945425309,20.3992129277918,20.4867596882313,20.5744033722082,
20.6621046091846,20.749931426706,20.7732022120367,20.8610213187728,20.9487296606754,
21.0363502358434,21.1272854049401,21.2148074208924,21.302316529447,21.3898333827436,
21.4773786334039,21.5650208483663,21.6527206383839,21.7405460525077,21.7638315886167,
21.8810147511443,21.9911485751285),.UNSPECIFIED.);
#2282=B_SPLINE_CURVE_WITH_KNOTS('',3,(#54429,#54430,#54431,#54432,#54433,
#54434,#54435,#54436,#54437,#54438,#54439,#54440,#54441,#54442,#54443,#54444,
#54445,#54446,#54447,#54448,#54449,#54450,#54451,#54452,#54453,#54454,#54455,
#54456,#54457,#54458,#54459,#54460,#54461,#54462,#54463,#54464,#54465,#54466,
#54467,#54468,#54469,#54470,#54471,#54472,#54473,#54474,#54475,#54476,#54477,
#54478,#54479,#54480,#54481,#54482,#54483,#54484,#54485,#54486,#54487,#54488,
#54489,#54490,#54491,#54492,#54493,#54494,#54495,#54496,#54497,#54498,#54499,
#54500,#54501,#54502,#54503,#54504,#54505,#54506,#54507,#54508,#54509,#54510),
 .UNSPECIFIED.,.F.,.F.,(4,3,3,3,3,3,3,3,3,3,3,3,3,3,3,3,3,3,3,3,3,3,3,3,
3,3,3,4),(21.9911485753201,22.0776479380628,22.1640847994147,22.2504889325943,
22.3368820308656,22.4232857745334,22.5097743736308,22.5963065304959,22.6829751209414,
22.7544609651967,22.842279178373,22.9299866007098,23.0176062315584,23.1085417453356,
23.1960627609244,23.283570850077,23.3710866659631,23.4586308622222,23.5462720027297,
23.6339707053352,23.721795021218,23.7450903417767,23.8329109711241,23.9206243019256,
24.0082360024787,24.0957890751796,24.1833037489021,24.2166325011217),
 .UNSPECIFIED.);
#2283=B_SPLINE_CURVE_WITH_KNOTS('',3,(#54512,#54513,#54514,#54515,#54516,
#54517,#54518,#54519,#54520,#54521,#54522,#54523,#54524,#54525,#54526,#54527,
#54528,#54529,#54530,#54531,#54532,#54533,#54534,#54535,#54536,#54537,#54538,
#54539,#54540,#54541,#54542,#54543,#54544,#54545,#54546,#54547,#54548,#54549,
#54550,#54551,#54552,#54553,#54554,#54555,#54556,#54557,#54558,#54559,#54560,
#54561,#54562,#54563,#54564,#54565,#54566,#54567,#54568,#54569,#54570,#54571,
#54572,#54573,#54574,#54575,#54576,#54577,#54578,#54579,#54580,#54581,#54582,
#54583,#54584,#54585,#54586,#54587,#54588,#54589,#54590,#54591,#54592,#54593),
 .UNSPECIFIED.,.F.,.F.,(4,3,3,3,3,3,3,3,3,3,3,3,3,3,3,3,3,3,3,3,3,3,3,3,
3,3,3,4),(21.9911485753333,22.0925692721343,22.1945701393998,22.2972272288129,
22.3241606593577,22.4119814005141,22.4996913661684,22.587313552442,22.678248112879,
22.7657716974341,22.8532823560317,22.9408007390053,23.0283474971554,23.1159911788507,
23.2036924135476,23.2915192288096,23.3147900359378,23.4026144670927,23.4903268514756,
23.5810561923767,23.6686091819928,23.7561267199653,23.8436294728221,23.9311380911715,
24.0187103151771,24.1063207518307,24.1940286226559,24.2161615786844),
 .UNSPECIFIED.);
#2284=B_SPLINE_CURVE_WITH_KNOTS('',3,(#54594,#54595,#54596,#54597,#54598,
#54599,#54600,#54601,#54602,#54603,#54604,#54605,#54606,#54607,#54608,#54609,
#54610,#54611,#54612,#54613,#54614,#54615,#54616,#54617,#54618,#54619,#54620,
#54621,#54622,#54623,#54624,#54625,#54626,#54627,#54628,#54629,#54630,#54631,
#54632,#54633,#54634,#54635,#54636,#54637,#54638,#54639,#54640,#54641,#54642,
#54643,#54644,#54645,#54646,#54647,#54648,#54649,#54650,#54651,#54652,#54653,
#54654,#54655,#54656,#54657,#54658,#54659,#54660,#54661,#54662,#54663,#54664,
#54665,#54666,#54667,#54668,#54669,#54670,#54671,#54672,#54673,#54674,#54675,
#54676,#54677,#54678,#54679,#54680,#54681,#54682,#54683,#54684,#54685,#54686,
#54687,#54688,#54689,#54690,#54691,#54692,#54693,#54694,#54695,#54696,#54697,
#54698,#54699,#54700,#54701,#54702,#54703,#54704,#54705,#54706,#54707,#54708,
#54709,#54710,#54711,#54712,#54713,#54714,#54715,#54716,#54717,#54718,#54719,
#54720,#54721,#54722,#54723,#54724,#54725,#54726,#54727,#54728,#54729,#54730,
#54731,#54732,#54733,#54734,#54735,#54736,#54737,#54738,#54739,#54740,#54741),
 .UNSPECIFIED.,.F.,.F.,(4,3,3,3,3,3,3,3,3,3,3,3,3,3,3,3,3,3,3,3,3,3,3,3,
3,3,3,3,3,3,3,3,3,3,3,3,3,3,3,3,3,3,3,3,3,3,3,3,3,4),(17.933138501431,18.0208128037283,
18.1085788187915,18.1963915332837,18.2843453074777,18.3616431530376,18.4493680107016,
18.5369809011481,18.6245049442856,18.7154758924521,18.8028992851819,18.8903091662094,
18.9777262923058,19.0651714204417,19.1527134250011,19.2403128340521,19.328038380529,
19.3522725296177,19.4401067268995,19.5278301686341,19.6154658340362,19.7063953430564,
19.7939323248959,19.881456326584,19.9689879833974,20.0565479310192,20.1442046095046,
20.2319187437788,20.31975821699,20.3429019061977,20.4307340263315,20.5184556296605,
20.6060896967071,20.697019894966,20.7845558931506,20.8720791412141,20.959610276429,
21.0471699366439,21.1348266789459,21.2225410820182,21.3103811242552,21.3335312827777,
21.4213251004975,21.509010264913,21.596607576048,21.6841377624944,21.7716265218872,
21.8590907051537,21.946569266503,21.9911485751285),.UNSPECIFIED.);
#2285=B_SPLINE_CURVE_WITH_KNOTS('',3,(#54744,#54745,#54746,#54747,#54748,
#54749,#54750,#54751,#54752,#54753,#54754,#54755,#54756,#54757,#54758,#54759,
#54760,#54761,#54762,#54763,#54764,#54765,#54766,#54767,#54768,#54769,#54770,
#54771,#54772,#54773,#54774,#54775,#54776,#54777,#54778,#54779,#54780,#54781,
#54782,#54783,#54784,#54785,#54786,#54787,#54788,#54789,#54790,#54791,#54792,
#54793,#54794,#54795,#54796,#54797,#54798,#54799,#54800,#54801,#54802,#54803,
#54804,#54805,#54806,#54807,#54808,#54809,#54810,#54811,#54812,#54813,#54814,
#54815,#54816,#54817,#54818,#54819,#54820,#54821,#54822,#54823,#54824,#54825,
#54826,#54827,#54828,#54829,#54830,#54831,#54832,#54833,#54834,#54835,#54836,
#54837,#54838,#54839,#54840,#54841,#54842,#54843,#54844,#54845,#54846,#54847,
#54848,#54849,#54850,#54851,#54852,#54853,#54854,#54855,#54856,#54857,#54858,
#54859,#54860,#54861,#54862,#54863,#54864,#54865,#54866,#54867,#54868,#54869,
#54870,#54871,#54872,#54873,#54874,#54875,#54876,#54877,#54878,#54879,#54880,
#54881,#54882,#54883,#54884,#54885,#54886,#54887,#54888,#54889,#54890,#54891,
#54892,#54893,#54894,#54895,#54896,#54897,#54898,#54899,#54900,#54901,#54902,
#54903,#54904,#54905,#54906,#54907,#54908,#54909,#54910,#54911,#54912,#54913,
#54914,#54915,#54916,#54917,#54918,#54919,#54920,#54921),.UNSPECIFIED.,
 .F.,.F.,(4,2,2,2,2,2,2,2,2,2,2,2,2,2,2,2,2,2,2,2,2,2,2,2,2,2,2,2,2,2,2,
2,2,2,2,2,2,2,2,2,2,2,2,2,2,2,2,2,2,2,2,2,2,2,2,2,2,2,2,2,2,2,2,2,2,2,2,
2,2,2,2,2,2,2,2,2,2,2,2,2,2,2,2,2,2,2,2,2,4),(-2.01509656764977,-2.00442233309338,
-1.9608583577495,-1.87948704543101,-1.86486657550063,-1.85607938554859,
-1.84806164739386,-1.83749996772665,-1.81324616040176,-1.77721781116714,
-1.70349473386971,-1.69305883332441,-1.68762595096638,-1.68313323006403,
-1.67719230258546,-1.66363146043247,-1.64364219553089,-1.56120202888727,
-1.53540039744752,-1.52542244956876,-1.51801059822966,-1.50980918998896,
-1.49810404406586,-1.46536688483646,-1.4048564047723,-1.36332861833298,
-1.35485467935966,-1.34989520288803,-1.34527322972197,-1.33840921159076,
-1.31833327766372,-1.2820434608007,-1.20805411918878,-1.19269330151755,
-1.18367137174265,-1.17570633079864,-1.16558618798958,-1.14400480293205,
-1.11368284458367,-1.07539126960149,-1.03072531611218,-1.01995220604332,
-1.01451931294949,-1.01002811585744,-1.00409183718097,-0.990555342435218,
-0.970615723187036,-0.888811585450084,-0.862426344445932,-0.85129421014968,
-0.843192989048181,-0.834635706030987,-0.821122162907508,-0.761468710728449,
-0.697439338488143,-0.684516130021924,-0.678746703584717,-0.674259955026725,
-0.668773483690929,-0.657725090667497,-0.642652460849895,-0.599590832733255,
-0.535943149624645,-0.520051552054786,-0.510916016790236,-0.502965578788175,
-0.493016829977024,-0.47241272073589,-0.444029850769972,-0.37785629362894,
-0.352121194415033,-0.344479781412078,-0.339699733192449,-0.334948449595917,
-0.327441082075921,-0.300958007167124,-0.239215749908723,-0.193873240375049,
-0.180734101219078,-0.172253508725591,-0.164111456249471,-0.152735532858041,
-0.122716224619186,-0.0713397715117924,-0.0212389669004389,-0.0106100332438987,
-0.00529042794641405,-0.00261557680526768,-0.000972528424130169),
 .UNSPECIFIED.);
#2286=B_SPLINE_CURVE_WITH_KNOTS('',3,(#54922,#54923,#54924,#54925,#54926,
#54927,#54928,#54929,#54930,#54931,#54932,#54933),.UNSPECIFIED.,.F.,.F.,
(4,2,2,2,2,4),(-4.27097705097338,-4.26723027831455,-4.26003241710359,-4.23690981860426,
-4.17261700115569,-4.15043685499169),.UNSPECIFIED.);
#2287=B_SPLINE_CURVE_WITH_KNOTS('',3,(#54935,#54936,#54937,#54938,#54939,
#54940,#54941,#54942,#54943,#54944,#54945,#54946,#54947),.UNSPECIFIED.,
 .F.,.F.,(4,3,3,3,4),(-10.4882942057671,-10.3977555924899,-10.3072163401549,
-10.2165955448043,-10.1336107524809),.UNSPECIFIED.);
#2288=B_SPLINE_CURVE_WITH_KNOTS('',3,(#54948,#54949,#54950,#54951,#54952,
#54953,#54954,#54955,#54956,#54957,#54958,#54959,#54960,#54961,#54962,#54963,
#54964,#54965,#54966,#54967,#54968,#54969,#54970,#54971,#54972,#54973,#54974,
#54975,#54976,#54977,#54978,#54979,#54980,#54981,#54982,#54983,#54984,#54985,
#54986,#54987,#54988,#54989,#54990,#54991,#54992,#54993,#54994,#54995,#54996,
#54997,#54998,#54999,#55000,#55001,#55002,#55003,#55004,#55005,#55006,#55007,
#55008,#55009,#55010,#55011,#55012,#55013,#55014,#55015,#55016,#55017,#55018,
#55019,#55020,#55021,#55022,#55023,#55024,#55025,#55026,#55027,#55028,#55029,
#55030,#55031,#55032,#55033,#55034,#55035,#55036,#55037,#55038,#55039,#55040,
#55041,#55042,#55043,#55044,#55045,#55046,#55047,#55048,#55049,#55050,#55051,
#55052,#55053,#55054,#55055,#55056,#55057,#55058,#55059,#55060,#55061,#55062,
#55063,#55064,#55065,#55066,#55067,#55068,#55069,#55070,#55071,#55072,#55073,
#55074,#55075,#55076,#55077,#55078,#55079,#55080,#55081,#55082,#55083,#55084,
#55085,#55086,#55087,#55088,#55089,#55090,#55091,#55092,#55093,#55094,#55095,
#55096,#55097,#55098,#55099,#55100,#55101,#55102,#55103,#55104,#55105,#55106,
#55107,#55108,#55109,#55110,#55111,#55112,#55113,#55114,#55115,#55116,#55117,
#55118,#55119,#55120,#55121,#55122,#55123),.UNSPECIFIED.,.F.,.F.,(4,2,2,
2,2,2,2,2,2,2,2,2,2,2,2,2,2,2,2,2,2,2,2,2,2,2,2,2,2,2,2,2,2,2,2,2,2,2,2,
2,2,2,2,2,2,2,2,2,2,2,2,2,2,2,2,2,2,2,2,2,2,2,2,2,2,2,2,2,2,2,2,2,2,2,2,
2,2,2,2,2,2,2,2,2,2,2,2,4),(1.42898336541552,1.46742042112348,1.49628767324879,
1.50748242560879,1.51556335490523,1.52403877281142,1.53728854434148,1.58538207353613,
1.64511336640643,1.67122017213511,1.67867093854414,1.68339288630674,1.68817396892759,
1.69581737063309,1.7215622074559,1.78120946774099,1.82889513342733,1.84216590412159,
1.85068238563881,1.8588247819375,1.87014569937684,1.89966303694102,1.94933960584668,
2.00176420693129,2.0124627931025,2.01788921483925,2.02239031356692,2.02836373761618,
2.04210157404567,2.0624546801884,2.15010624733382,2.17227476486632,2.18249828827888,
2.19047738888946,2.19944523224858,2.21493687033016,2.26438326886928,2.33884446341765,
2.34917154282268,2.35458140550876,2.35907481829952,2.36504235539273,2.37877234152408,
2.39911564013077,2.48666264161458,2.50894350254305,2.51918007663318,2.52715367372913,
2.53609874002411,2.55150650100293,2.60038497279164,2.67585417911298,2.68599672903178,
2.69136531045916,2.69586331645455,2.70188621777872,2.71593968890811,2.73696465367393,
2.82131097911041,2.84470522745123,2.85517774105293,2.86320851512811,2.87195340468667,
2.88636803507151,2.94862908948105,3.0128998568419,3.02278794986426,3.02810540927959,
3.03257077225844,3.03865180033539,3.05306208137573,3.07485511640371,3.12305130328204,
3.17486450111713,3.18824825716846,3.19678029661692,3.20489719519077,3.21611528228411,
3.24467251611403,3.29167571826644,3.34865407437406,3.35903110763528,3.36445108845531,
3.36894453296996,3.37490069007886,3.38161060650366,3.3934525021966,3.44312968008527),
 .UNSPECIFIED.);
#2289=B_SPLINE_CURVE_WITH_KNOTS('',3,(#55126,#55127,#55128,#55129,#55130,
#55131,#55132,#55133,#55134,#55135,#55136,#55137,#55138,#55139,#55140,#55141,
#55142,#55143,#55144,#55145,#55146,#55147,#55148,#55149,#55150,#55151,#55152,
#55153,#55154,#55155,#55156,#55157,#55158,#55159,#55160,#55161,#55162,#55163,
#55164,#55165,#55166,#55167,#55168,#55169,#55170,#55171,#55172,#55173,#55174,
#55175,#55176,#55177,#55178,#55179,#55180,#55181,#55182,#55183,#55184,#55185,
#55186,#55187,#55188,#55189,#55190,#55191,#55192,#55193,#55194,#55195,#55196,
#55197,#55198,#55199,#55200,#55201,#55202,#55203,#55204,#55205,#55206,#55207,
#55208,#55209,#55210,#55211,#55212,#55213,#55214,#55215,#55216,#55217,#55218,
#55219,#55220,#55221,#55222,#55223,#55224,#55225,#55226,#55227,#55228,#55229,
#55230,#55231,#55232,#55233,#55234,#55235,#55236,#55237,#55238,#55239,#55240,
#55241,#55242,#55243,#55244,#55245,#55246,#55247,#55248,#55249,#55250,#55251,
#55252,#55253,#55254,#55255,#55256,#55257,#55258,#55259,#55260,#55261,#55262,
#55263,#55264,#55265,#55266,#55267,#55268,#55269,#55270),.UNSPECIFIED.,
 .F.,.F.,(4,3,3,3,3,3,3,3,3,3,3,3,3,3,3,3,3,3,3,3,3,3,3,3,3,3,3,3,3,3,3,
3,3,3,3,3,3,3,3,3,3,3,3,3,3,3,3,3,4),(17.9338701936111,18.0215425484498,
18.1091390091939,18.1966882371871,18.2842137695347,18.3717362510166,18.4592763192238,
18.5469081233696,18.6345877563007,18.7224058342168,18.7919434588766,18.8797523761682,
18.9674503808827,19.0550604846278,19.1459995284814,19.2335108046853,19.3210090929069,
19.4085150568561,19.4960493606828,19.583680598315,19.6713693803307,19.7591838251699,
19.7825728354566,19.8703922614065,19.9581008994616,20.0457217474393,20.136656805514,
20.2241790336769,20.3116883315558,20.3992053509585,20.4867507441582,20.5743930657194,
20.6620929414952,20.7499184099657,20.7732022120367,20.8610210915467,20.948729199622,
21.0363495346721,21.1272847914152,21.2148065529677,21.302315402261,21.3898319916896,
21.4773769741273,21.5650189156996,21.652718428991,21.7405435635626,21.7638315886167,
21.8810158224684,21.9911485751285),.UNSPECIFIED.);
#2290=B_SPLINE_CURVE_WITH_KNOTS('',3,(#55271,#55272,#55273,#55274,#55275,
#55276,#55277,#55278,#55279,#55280,#55281,#55282,#55283,#55284,#55285,#55286,
#55287,#55288,#55289,#55290,#55291,#55292,#55293,#55294,#55295,#55296,#55297,
#55298,#55299,#55300,#55301,#55302,#55303,#55304,#55305,#55306,#55307,#55308,
#55309,#55310,#55311,#55312,#55313,#55314,#55315,#55316,#55317,#55318,#55319,
#55320,#55321,#55322,#55323,#55324,#55325,#55326,#55327,#55328,#55329,#55330,
#55331,#55332,#55333,#55334,#55335,#55336,#55337,#55338,#55339,#55340,#55341,
#55342,#55343,#55344,#55345,#55346,#55347,#55348,#55349,#55350,#55351,#55352),
 .UNSPECIFIED.,.F.,.F.,(4,3,3,3,3,3,3,3,3,3,3,3,3,3,3,3,3,3,3,3,3,3,3,3,
3,3,3,4),(21.9911485752709,22.0776484873086,22.1640859035787,22.2504905951409,
22.3368842548815,22.4232885627304,22.5097777277752,22.5963104523736,22.682979609016,
22.7544609651967,22.8422789541284,22.9299861499661,23.0176055523507,23.108541151029,
23.1960619347146,23.2835697910957,23.3710853735935,23.4586293360987,23.5462702434834,
23.6339687130605,23.7217927978273,23.7450903417767,23.8329109525895,23.9206242639913,
24.0082359438482,24.0957889951867,24.1833036461088,24.2166288571228),
 .UNSPECIFIED.);
#2291=B_SPLINE_CURVE_WITH_KNOTS('',3,(#55354,#55355,#55356,#55357,#55358,
#55359,#55360,#55361,#55362,#55363,#55364,#55365,#55366,#55367,#55368,#55369,
#55370,#55371,#55372,#55373,#55374,#55375,#55376,#55377,#55378,#55379,#55380,
#55381,#55382,#55383,#55384,#55385,#55386,#55387,#55388,#55389,#55390,#55391,
#55392,#55393,#55394,#55395,#55396,#55397,#55398,#55399,#55400,#55401,#55402,
#55403,#55404,#55405,#55406,#55407,#55408,#55409,#55410,#55411,#55412,#55413,
#55414,#55415,#55416,#55417,#55418,#55419,#55420,#55421,#55422,#55423,#55424,
#55425,#55426,#55427,#55428,#55429,#55430,#55431,#55432,#55433,#55434,#55435),
 .UNSPECIFIED.,.F.,.F.,(4,3,3,3,3,3,3,3,3,3,3,3,3,3,3,3,3,3,3,3,3,3,3,3,
3,3,3,4),(21.991148575328,22.0925750122967,22.1945818395017,22.2972449529874,
22.3241606593577,22.4119800933751,22.4996887395737,22.5873095957602,22.6782446507824,
22.7657668872646,22.853276193489,22.9407932212544,23.0283386228251,23.1159809527272,
23.203680836836,23.2915063135646,23.3147900359378,23.4026142424768,23.4903263956193,
23.5810553112597,23.6686080545512,23.7561253408872,23.8436278370528,23.9311361939092,
24.0187081497838,24.106318314622,24.1940259083462,24.2161577207422),
 .UNSPECIFIED.);
#2292=B_SPLINE_CURVE_WITH_KNOTS('',3,(#55436,#55437,#55438,#55439,#55440,
#55441,#55442,#55443,#55444,#55445,#55446,#55447,#55448,#55449,#55450,#55451,
#55452,#55453,#55454,#55455,#55456,#55457,#55458,#55459,#55460,#55461,#55462,
#55463,#55464,#55465,#55466,#55467,#55468,#55469,#55470,#55471,#55472,#55473,
#55474,#55475,#55476,#55477,#55478,#55479,#55480,#55481,#55482,#55483,#55484,
#55485,#55486,#55487,#55488,#55489,#55490,#55491,#55492,#55493,#55494,#55495,
#55496,#55497,#55498,#55499,#55500,#55501,#55502,#55503,#55504,#55505,#55506,
#55507,#55508,#55509,#55510,#55511,#55512,#55513,#55514,#55515,#55516,#55517,
#55518,#55519,#55520,#55521,#55522,#55523,#55524,#55525,#55526,#55527,#55528,
#55529,#55530,#55531,#55532,#55533,#55534,#55535,#55536,#55537,#55538,#55539,
#55540,#55541,#55542,#55543,#55544,#55545,#55546,#55547,#55548,#55549,#55550,
#55551,#55552,#55553,#55554,#55555,#55556,#55557,#55558,#55559,#55560,#55561,
#55562,#55563,#55564,#55565,#55566,#55567,#55568,#55569,#55570,#55571,#55572,
#55573,#55574,#55575,#55576,#55577,#55578,#55579,#55580,#55581,#55582,#55583),
 .UNSPECIFIED.,.F.,.F.,(4,3,3,3,3,3,3,3,3,3,3,3,3,3,3,3,3,3,3,3,3,3,3,3,
3,3,3,3,3,3,3,3,3,3,3,3,3,3,3,3,3,3,3,3,3,3,3,3,3,4),(17.9331346413009,
18.0208008549548,18.1085586349722,18.1963630282738,18.2843083902826,18.3616431530376,
18.4493863215626,18.5370177657643,18.6245605825582,18.7155245759407,18.8029671774752,
18.8903963961828,18.9778329691677,19.0652976337961,19.1528592120373,19.2404782401086,
19.328223323708,19.3522725296177,19.4400992198406,19.5278150837884,19.6154431104019,
19.7063754598764,19.7939046999881,19.8814209354505,19.9689448099973,20.0564969677625,
20.144145884356,20.2318522639848,20.3196840522245,20.3429019061977,20.4307323378319,
20.5184522110659,20.6060845086748,20.6970153554376,20.7845494965245,20.8720708581442,
20.9596000794408,21.047157800116,21.1348125742423,21.222524990115,21.3103630321082,
21.3335312827777,21.421328203082,21.5090165109469,21.5966170027785,21.6841504035972,
21.7716424163973,21.8591098761587,21.9465917337312,21.9911485751285),
 .UNSPECIFIED.);
#2293=B_SPLINE_CURVE_WITH_KNOTS('',3,(#55585,#55586,#55587,#55588,#55589,
#55590,#55591,#55592,#55593,#55594,#55595,#55596,#55597,#55598,#55599,#55600,
#55601,#55602,#55603,#55604,#55605,#55606,#55607,#55608,#55609,#55610,#55611,
#55612,#55613,#55614,#55615,#55616,#55617,#55618,#55619,#55620,#55621,#55622,
#55623,#55624,#55625,#55626,#55627,#55628,#55629,#55630,#55631,#55632,#55633,
#55634,#55635,#55636,#55637,#55638,#55639,#55640,#55641,#55642,#55643,#55644,
#55645,#55646,#55647,#55648,#55649,#55650,#55651,#55652,#55653,#55654,#55655,
#55656,#55657,#55658,#55659,#55660,#55661,#55662,#55663,#55664,#55665,#55666,
#55667,#55668,#55669,#55670,#55671,#55672,#55673,#55674,#55675,#55676,#55677,
#55678,#55679,#55680,#55681),.UNSPECIFIED.,.F.,.F.,(4,3,3,3,3,3,3,3,3,3,
3,3,3,3,3,3,3,3,3,3,3,3,3,3,3,3,3,3,3,3,3,3,4),(-0.760759816994444,-0.728264991811328,
-0.695770166628212,-0.679277258312604,-0.673133552693547,-0.639296875083126,
-0.609964780509387,-0.599335840102474,-0.591522810183719,-0.556929583326479,
-0.521819327675206,-0.48700557018393,-0.46641420726125,-0.455506208456746,
-0.450683812595539,-0.414689753833517,-0.404640118493211,-0.369640440894481,
-0.33464076329575,-0.314658074377986,-0.309087722362195,-0.304655337289647,
-0.268706903554133,-0.232146738196951,-0.195137918029292,-0.172257529468521,
-0.161271461718819,-0.155984382027272,-0.118128117568438,-0.0801985115663637,
-0.0429532259117857,-0.0149177406115184,-7.75271862796333E-5),
 .UNSPECIFIED.);
#2294=B_SPLINE_CURVE_WITH_KNOTS('',3,(#55682,#55683,#55684,#55685,#55686,
#55687,#55688,#55689,#55690,#55691,#55692,#55693,#55694,#55695,#55696,#55697,
#55698,#55699,#55700,#55701,#55702,#55703,#55704,#55705,#55706,#55707,#55708,
#55709,#55710,#55711,#55712,#55713,#55714,#55715,#55716,#55717,#55718,#55719,
#55720,#55721,#55722,#55723,#55724,#55725,#55726,#55727,#55728,#55729,#55730,
#55731,#55732,#55733,#55734,#55735,#55736,#55737,#55738,#55739,#55740,#55741,
#55742,#55743,#55744,#55745,#55746,#55747,#55748,#55749,#55750,#55751,#55752,
#55753,#55754,#55755,#55756,#55757,#55758,#55759,#55760,#55761,#55762,#55763,
#55764,#55765,#55766,#55767,#55768,#55769,#55770,#55771,#55772,#55773,#55774,
#55775,#55776,#55777,#55778,#55779,#55780,#55781),.UNSPECIFIED.,.F.,.F.,
(4,3,3,3,3,3,3,3,3,3,3,3,3,3,3,3,3,3,3,3,3,3,3,3,3,3,3,3,3,3,3,3,3,4),(-0.757763664684544,
-0.720381973657696,-0.682469288080949,-0.665926778923518,-0.657236479192177,
-0.619823586647078,-0.58844849796256,-0.574621441004157,-0.568708672760664,
-0.563214615962493,-0.526686992270663,-0.490320816525781,-0.45498363839703,
-0.433443448090507,-0.420354083330733,-0.414509335427944,-0.379623925576214,
-0.368822877170939,-0.33339680623558,-0.297701811576582,-0.279872858492725,
-0.274338169979935,-0.269571988414296,-0.234853323947987,-0.200243129273121,
-0.165977491882068,-0.146785125676167,-0.136607374511969,-0.130842930290342,
-0.0974426608405007,-0.0645413522423534,-0.0326213770037655,-0.0124385622348649,
0.),.UNSPECIFIED.);
#2295=B_SPLINE_CURVE_WITH_KNOTS('',3,(#56066,#56067,#56068,#56069,#56070,
#56071,#56072,#56073,#56074,#56075,#56076,#56077,#56078,#56079,#56080,#56081,
#56082,#56083,#56084,#56085,#56086,#56087,#56088,#56089,#56090,#56091,#56092,
#56093,#56094,#56095,#56096,#56097,#56098,#56099,#56100,#56101,#56102,#56103,
#56104,#56105,#56106,#56107,#56108,#56109,#56110,#56111,#56112,#56113,#56114,
#56115,#56116,#56117,#56118,#56119,#56120,#56121,#56122,#56123,#56124,#56125,
#56126,#56127,#56128,#56129,#56130,#56131,#56132,#56133,#56134,#56135,#56136,
#56137,#56138,#56139,#56140,#56141,#56142,#56143,#56144,#56145,#56146,#56147,
#56148,#56149,#56150,#56151,#56152,#56153,#56154,#56155,#56156,#56157,#56158,
#56159,#56160,#56161,#56162),.UNSPECIFIED.,.F.,.F.,(4,3,3,3,3,3,3,3,3,3,
3,3,3,3,3,3,3,3,3,3,3,3,3,3,3,3,3,3,3,3,3,3,4),(0.,0.0317312806353046,0.0642559409710066,
0.0977155979249547,0.129677601589085,0.134721269266439,0.168713657830876,
0.203412250787311,0.238085926099261,0.267345190569703,0.27293511481588,
0.277770698819479,0.313396265799393,0.348890032601819,0.355122983981029,
0.389870418620742,0.41193498250944,0.417350288416101,0.422249312177161,
0.457204205816802,0.493397395543351,0.529989879387874,0.55660407456938,
0.565580838002556,0.571298452925119,0.608611867141919,0.64218476056642,
0.656270742946784,0.66268483640152,0.700540820507026,0.7381751635799,0.742903440839923,
0.757686396975181),.UNSPECIFIED.);
#2296=B_SPLINE_CURVE_WITH_KNOTS('',3,(#56448,#56449,#56450,#56451),
 .UNSPECIFIED.,.F.,.F.,(4,4),(-0.0163901208212989,0.),.UNSPECIFIED.);
#2297=B_SPLINE_CURVE_WITH_KNOTS('',3,(#56452,#56453,#56454,#56455,#56456,
#56457,#56458,#56459,#56460,#56461,#56462,#56463,#56464,#56465,#56466,#56467,
#56468,#56469,#56470,#56471,#56472,#56473,#56474,#56475,#56476,#56477,#56478,
#56479,#56480,#56481,#56482,#56483,#56484,#56485,#56486,#56487,#56488,#56489,
#56490,#56491,#56492,#56493,#56494,#56495,#56496,#56497,#56498,#56499,#56500,
#56501,#56502,#56503,#56504,#56505,#56506,#56507,#56508,#56509,#56510,#56511,
#56512,#56513,#56514,#56515,#56516,#56517,#56518,#56519,#56520,#56521,#56522,
#56523,#56524,#56525,#56526,#56527,#56528,#56529,#56530,#56531,#56532,#56533,
#56534,#56535,#56536,#56537,#56538,#56539,#56540,#56541,#56542,#56543,#56544,
#56545,#56546,#56547,#56548),.UNSPECIFIED.,.F.,.F.,(4,3,3,3,3,3,3,3,3,3,
3,3,3,3,3,3,3,3,3,3,3,3,3,3,3,3,3,3,3,3,3,3,4),(0.,0.0369273503214421,0.075453949697969,
0.113980549074496,0.148593722241587,0.155414829285566,0.15991268003852,
0.196868730101154,0.233511857819008,0.269948573766588,0.300182913927748,
0.30668030757842,0.311558445745243,0.346837776429413,0.381907055493282,
0.390885934411227,0.426888021696901,0.446975199311113,0.453110029126761,
0.457477086043627,0.492330531618533,0.527975345133486,0.56362015864844,
0.586702996757923,0.593773585511785,0.59917438939843,0.633033686297888,
0.662014224183436,0.675195718914722,0.683250103205775,0.715766483365038,
0.7482828635243,0.760759816994426),.UNSPECIFIED.);
#2298=B_SPLINE_CURVE_WITH_KNOTS('',3,(#56550,#56551,#56552,#56553,#56554,
#56555,#56556,#56557,#56558,#56559,#56560,#56561,#56562,#56563,#56564,#56565,
#56566,#56567,#56568,#56569,#56570,#56571,#56572,#56573,#56574,#56575,#56576,
#56577,#56578,#56579,#56580,#56581,#56582,#56583,#56584,#56585,#56586,#56587,
#56588,#56589,#56590,#56591,#56592,#56593,#56594,#56595,#56596,#56597,#56598,
#56599,#56600,#56601,#56602,#56603,#56604,#56605,#56606,#56607,#56608,#56609,
#56610,#56611,#56612,#56613,#56614,#56615,#56616,#56617,#56618,#56619,#56620,
#56621,#56622,#56623,#56624,#56625,#56626,#56627,#56628,#56629,#56630,#56631,
#56632,#56633,#56634,#56635,#56636,#56637,#56638,#56639,#56640,#56641,#56642,
#56643,#56644,#56645,#56646),.UNSPECIFIED.,.F.,.F.,(4,3,3,3,3,3,3,3,3,3,
3,3,3,3,3,3,3,3,3,3,3,3,3,3,3,3,3,3,3,3,3,3,4),(-0.760759816994476,-0.72867719727751,
-0.695709509772144,-0.679296483390001,-0.67313674552237,-0.639623085494667,
-0.605457437465359,-0.599329771118666,-0.591523612514049,-0.556772239761969,
-0.521698252355195,-0.486799294770719,-0.466411345045984,-0.455503194092392,
-0.450680887225085,-0.414687271005122,-0.404640118493233,-0.369644644590622,
-0.334649170688011,-0.31466595630823,-0.309139237774412,-0.304706649237392,
-0.26876366107657,-0.23220698919768,-0.195198522951163,-0.172299540947597,
-0.161302847522944,-0.15637940503376,-0.118526813930542,-0.0805957826481643,
-0.0433462769323225,-0.0149177406115232,-7.70745645911542E-5),
 .UNSPECIFIED.);
#2299=B_SPLINE_CURVE_WITH_KNOTS('',3,(#56647,#56648,#56649,#56650,#56651,
#56652,#56653,#56654,#56655,#56656,#56657,#56658,#56659,#56660,#56661,#56662,
#56663,#56664,#56665,#56666,#56667,#56668,#56669,#56670,#56671,#56672,#56673,
#56674,#56675,#56676,#56677,#56678,#56679,#56680,#56681,#56682,#56683,#56684,
#56685,#56686,#56687,#56688,#56689,#56690,#56691,#56692,#56693,#56694,#56695,
#56696,#56697,#56698,#56699,#56700,#56701,#56702,#56703,#56704,#56705,#56706,
#56707,#56708,#56709,#56710,#56711,#56712,#56713,#56714,#56715,#56716,#56717,
#56718,#56719,#56720,#56721,#56722,#56723,#56724,#56725,#56726,#56727,#56728,
#56729,#56730,#56731,#56732,#56733,#56734,#56735,#56736,#56737,#56738,#56739,
#56740,#56741,#56742,#56743,#56744,#56745,#56746),.UNSPECIFIED.,.F.,.F.,
(4,3,3,3,3,3,3,3,3,3,3,3,3,3,3,3,3,3,3,3,3,3,3,3,3,3,3,3,3,3,3,3,3,4),(-0.757763664684541,
-0.720112840922623,-0.682462017160704,-0.665890632802888,-0.657236256652766,
-0.619823116120217,-0.588448296754926,-0.57462061065214,-0.568701943316166,
-0.563203084666934,-0.526652622723307,-0.490393340155699,-0.455008271985665,
-0.433438531484178,-0.420355266574036,-0.414509519578869,-0.379626370547332,
-0.368822877170946,-0.333397756276839,-0.297724697737825,-0.279872859743228,
-0.274339772740684,-0.269574604924806,-0.234866697539682,-0.200136844250274,
-0.166019399733717,-0.146788550715945,-0.136613171362025,-0.130388812283381,
-0.0969950806536839,-0.0641041103661313,-0.0321947839414556,-0.0124385622348649,
0.),.UNSPECIFIED.);
#2300=B_SPLINE_CURVE_WITH_KNOTS('',3,(#57031,#57032,#57033,#57034,#57035,
#57036,#57037,#57038,#57039,#57040,#57041,#57042,#57043,#57044,#57045,#57046,
#57047,#57048,#57049,#57050,#57051,#57052,#57053,#57054,#57055,#57056,#57057,
#57058,#57059,#57060,#57061,#57062,#57063,#57064,#57065,#57066,#57067,#57068,
#57069,#57070,#57071,#57072,#57073,#57074,#57075,#57076,#57077,#57078,#57079,
#57080,#57081,#57082,#57083,#57084,#57085,#57086,#57087,#57088,#57089,#57090,
#57091,#57092,#57093,#57094,#57095,#57096,#57097,#57098,#57099,#57100,#57101,
#57102,#57103,#57104,#57105,#57106,#57107,#57108,#57109,#57110,#57111,#57112,
#57113,#57114,#57115,#57116,#57117,#57118,#57119,#57120,#57121,#57122,#57123,
#57124),.UNSPECIFIED.,.F.,.F.,(4,3,3,3,3,3,3,3,3,3,3,3,3,3,3,3,3,3,3,3,
3,3,3,3,3,3,3,3,3,3,3,4),(7.37877496047656E-15,0.0324242548762023,0.0650764812389879,
0.0985463434422195,0.129697019504787,0.134733032820196,0.169300198334513,
0.203925126369526,0.238560097109361,0.273001694877465,0.278364300420405,
0.314020733983785,0.349481131532155,0.355122983981017,0.389954438528394,
0.411931265454395,0.417329657811387,0.422220055612132,0.457543827286333,
0.493520000679641,0.53011436736757,0.556569343667961,0.565759141712967,
0.571513495091189,0.608852677501213,0.637578888089422,0.651941993383527,
0.660700630375842,0.666305098677632,0.704604269758768,0.742903440839903,
0.757686857130631),.UNSPECIFIED.);
#2301=B_SPLINE_CURVE_WITH_KNOTS('',3,(#57410,#57411,#57412,#57413),
 .UNSPECIFIED.,.F.,.F.,(4,4),(-0.0162873320748038,0.),.UNSPECIFIED.);
#2302=B_SPLINE_CURVE_WITH_KNOTS('',3,(#57414,#57415,#57416,#57417,#57418,
#57419,#57420,#57421,#57422,#57423,#57424,#57425,#57426,#57427,#57428,#57429,
#57430,#57431,#57432,#57433,#57434,#57435,#57436,#57437,#57438,#57439,#57440,
#57441,#57442,#57443,#57444,#57445,#57446,#57447,#57448,#57449,#57450,#57451,
#57452,#57453,#57454,#57455,#57456,#57457,#57458,#57459,#57460,#57461,#57462,
#57463,#57464,#57465,#57466,#57467,#57468,#57469,#57470,#57471,#57472,#57473,
#57474,#57475,#57476,#57477,#57478,#57479,#57480,#57481,#57482,#57483,#57484,
#57485,#57486,#57487,#57488,#57489,#57490,#57491,#57492,#57493,#57494,#57495,
#57496,#57497,#57498,#57499,#57500,#57501,#57502,#57503,#57504,#57505,#57506,
#57507,#57508,#57509,#57510,#57511,#57512,#57513),.UNSPECIFIED.,.F.,.F.,
(4,3,3,3,3,3,3,3,3,3,3,3,3,3,3,3,3,3,3,3,3,3,3,3,3,3,3,3,3,3,3,3,3,4),(8.40311229217861E-15,
0.037154906704243,0.0748575402003926,0.112713526298086,0.148602209914868,
0.155563216342729,0.160137581649395,0.197101195136362,0.233889668479667,
0.269838109891337,0.300344302506693,0.307574466956952,0.312824195400226,
0.348077394899254,0.383139909542925,0.390885934411227,0.426911554808929,
0.446975445769724,0.453109734545746,0.457476473349302,0.492419953500651,
0.527549736956349,0.562225774259029,0.586701706612183,0.593769976980005,
0.599171096269385,0.633029003473375,0.662011207283425,0.673224422339548,
0.681404190977219,0.683249578743692,0.715766221134031,0.74828286352437,
0.7607598169945),.UNSPECIFIED.);
#2303=B_SPLINE_CURVE_WITH_KNOTS('',3,(#57515,#57516,#57517,#57518,#57519,
#57520,#57521,#57522,#57523,#57524,#57525,#57526,#57527,#57528,#57529,#57530,
#57531,#57532,#57533,#57534,#57535,#57536,#57537,#57538,#57539,#57540,#57541,
#57542,#57543,#57544,#57545,#57546,#57547,#57548,#57549,#57550,#57551,#57552,
#57553,#57554,#57555,#57556,#57557,#57558,#57559,#57560,#57561,#57562,#57563,
#57564,#57565,#57566,#57567,#57568,#57569,#57570,#57571,#57572,#57573,#57574,
#57575,#57576,#57577,#57578,#57579,#57580,#57581,#57582,#57583,#57584,#57585,
#57586,#57587,#57588,#57589,#57590,#57591,#57592,#57593,#57594,#57595,#57596,
#57597,#57598,#57599,#57600,#57601,#57602,#57603,#57604,#57605,#57606,#57607,
#57608,#57609,#57610,#57611),.UNSPECIFIED.,.F.,.F.,(4,3,3,3,3,3,3,3,3,3,
3,3,3,3,3,3,3,3,3,3,3,3,3,3,3,3,3,3,3,3,3,3,4),(-0.760759816994569,-0.728265012223969,
-0.695770207453369,-0.679277205036654,-0.673133543750063,-0.639296880860471,
-0.60996478556457,-0.599335856776469,-0.591522808027896,-0.556929595372945,
-0.521884160161627,-0.486981466865639,-0.466414215846013,-0.455506217424483,
-0.450683821468725,-0.414689761897011,-0.404640118493263,-0.369640429831607,
-0.334640741169951,-0.314658053635049,-0.309087585707408,-0.304655192905571,
-0.268706744459819,-0.232146569596101,-0.19513774849793,-0.17225741155648,
-0.161271373612937,-0.155984378195552,-0.118128111533916,-0.080198505595755,
-0.0429532188256224,-0.0149177406115174,-7.75300628616282E-5),
 .UNSPECIFIED.);
#2304=B_SPLINE_CURVE_WITH_KNOTS('',3,(#57612,#57613,#57614,#57615,#57616,
#57617,#57618,#57619,#57620,#57621,#57622,#57623,#57624,#57625,#57626,#57627,
#57628,#57629,#57630,#57631,#57632,#57633,#57634,#57635,#57636,#57637,#57638,
#57639,#57640,#57641,#57642,#57643,#57644,#57645,#57646,#57647,#57648,#57649,
#57650,#57651,#57652,#57653,#57654,#57655,#57656,#57657,#57658,#57659,#57660,
#57661,#57662,#57663,#57664,#57665,#57666,#57667,#57668,#57669,#57670,#57671,
#57672,#57673,#57674,#57675,#57676,#57677,#57678,#57679,#57680,#57681,#57682,
#57683,#57684,#57685,#57686,#57687,#57688,#57689,#57690,#57691,#57692,#57693,
#57694,#57695,#57696,#57697,#57698,#57699,#57700,#57701,#57702,#57703,#57704,
#57705,#57706,#57707,#57708,#57709,#57710,#57711),.UNSPECIFIED.,.F.,.F.,
(4,3,3,3,3,3,3,3,3,3,3,3,3,3,3,3,3,3,3,3,3,3,3,3,3,3,3,3,3,3,3,3,3,4),(-0.757763664684454,
-0.720381983678288,-0.682469301582833,-0.665926845916897,-0.657236479144063,
-0.619823586771666,-0.588448498071578,-0.574621442191374,-0.568708683306026,
-0.563214634116051,-0.526663060420545,-0.490401464824994,-0.455014148149494,
-0.433443455337693,-0.420354081977822,-0.414509335454218,-0.379623921634209,
-0.36882287717096,-0.333396805704032,-0.29770181177085,-0.279872858674851,
-0.274338167969609,-0.269571984980098,-0.234909244560119,-0.200298697723679,
-0.165977486809442,-0.14678512123762,-0.136607366744964,-0.130842926885658,
-0.0973672231254303,-0.0647374859486738,-0.0326213606334859,-0.0124385622348654,
0.),.UNSPECIFIED.);
#2305=B_SPLINE_CURVE_WITH_KNOTS('',3,(#57996,#57997,#57998,#57999,#58000,
#58001,#58002,#58003,#58004,#58005,#58006,#58007,#58008,#58009,#58010,#58011,
#58012,#58013,#58014,#58015,#58016,#58017,#58018,#58019,#58020,#58021,#58022,
#58023,#58024,#58025,#58026,#58027,#58028,#58029,#58030,#58031,#58032,#58033,
#58034,#58035,#58036,#58037,#58038,#58039,#58040,#58041,#58042,#58043,#58044,
#58045,#58046,#58047,#58048,#58049,#58050,#58051,#58052,#58053,#58054,#58055,
#58056,#58057,#58058,#58059,#58060,#58061,#58062,#58063,#58064,#58065,#58066,
#58067,#58068,#58069,#58070,#58071,#58072,#58073,#58074,#58075,#58076,#58077,
#58078,#58079,#58080,#58081,#58082,#58083,#58084,#58085,#58086,#58087,#58088,
#58089,#58090,#58091,#58092),.UNSPECIFIED.,.F.,.F.,(4,3,3,3,3,3,3,3,3,3,
3,3,3,3,3,3,3,3,3,3,3,3,3,3,3,3,3,3,3,3,3,3,4),(0.,0.0317312649685969,0.0642559110632862,
0.0974710776091265,0.12967756590561,0.134721247960768,0.168753867071307,
0.20335447753473,0.238023614120417,0.267345161024578,0.27293499338489,0.277770512668279,
0.3133960762696,0.348889848578609,0.355122983980998,0.389870425600039,0.411934989052527,
0.417350324507801,0.422249364155745,0.457397349687017,0.493693649725071,
0.529989949763124,0.556604136147715,0.56558068166977,0.571298424882708,
0.608725571359697,0.642184740832426,0.65627071778627,0.66268481658205,0.700540800689733,
0.738175144334356,0.74290344083985,0.757686395020893),.UNSPECIFIED.);
#2306=B_SPLINE_CURVE_WITH_KNOTS('',3,(#58378,#58379,#58380,#58381),
 .UNSPECIFIED.,.F.,.F.,(4,4),(-0.0163907070131913,0.),.UNSPECIFIED.);
#2307=B_SPLINE_CURVE_WITH_KNOTS('',3,(#58382,#58383,#58384,#58385,#58386,
#58387,#58388,#58389,#58390,#58391,#58392,#58393,#58394,#58395,#58396,#58397,
#58398,#58399,#58400,#58401,#58402,#58403,#58404,#58405,#58406,#58407,#58408,
#58409,#58410,#58411,#58412,#58413,#58414,#58415,#58416,#58417,#58418,#58419,
#58420,#58421,#58422,#58423,#58424,#58425,#58426,#58427,#58428,#58429,#58430,
#58431,#58432,#58433,#58434,#58435,#58436,#58437,#58438,#58439,#58440,#58441,
#58442,#58443,#58444,#58445,#58446,#58447,#58448,#58449,#58450,#58451,#58452,
#58453,#58454,#58455,#58456,#58457,#58458,#58459,#58460,#58461,#58462,#58463,
#58464,#58465,#58466,#58467,#58468,#58469,#58470,#58471,#58472,#58473,#58474,
#58475,#58476,#58477,#58478),.UNSPECIFIED.,.F.,.F.,(4,3,3,3,3,3,3,3,3,3,
3,3,3,3,3,3,3,3,3,3,3,3,3,3,3,3,3,3,3,3,3,3,4),(0.,0.0371488255941907,0.0748481542789714,
0.112705168174495,0.148593698835094,0.15541443824774,0.159912176538531,
0.196868224356431,0.233511365402667,0.269948093072399,0.300182553407106,
0.306678475117778,0.311556542095174,0.347097110787367,0.381905205719197,
0.39088593441123,0.426888020859033,0.446975198525616,0.453110029188261,
0.457477086646452,0.492330532691639,0.527975346805991,0.563620160920343,
0.586702998745845,0.593773594183896,0.599174397431784,0.633258020605501,
0.662014231335216,0.675195728621906,0.683250104575177,0.715766484049769,
0.74828286352436,0.760759816994485),.UNSPECIFIED.);
#2308=B_SPLINE_CURVE_WITH_KNOTS('',3,(#58480,#58481,#58482,#58483,#58484,
#58485,#58486,#58487,#58488,#58489,#58490,#58491,#58492,#58493,#58494,#58495,
#58496,#58497,#58498,#58499,#58500,#58501,#58502,#58503,#58504,#58505,#58506,
#58507,#58508,#58509,#58510,#58511,#58512,#58513,#58514,#58515,#58516,#58517,
#58518,#58519,#58520,#58521,#58522,#58523,#58524,#58525,#58526,#58527,#58528,
#58529,#58530,#58531,#58532,#58533,#58534,#58535,#58536,#58537,#58538,#58539,
#58540,#58541,#58542,#58543,#58544,#58545,#58546,#58547,#58548,#58549,#58550,
#58551,#58552,#58553,#58554,#58555,#58556,#58557,#58558,#58559,#58560,#58561,
#58562,#58563,#58564,#58565,#58566,#58567,#58568,#58569,#58570,#58571,#58572,
#58573,#58574,#58575,#58576),.UNSPECIFIED.,.F.,.F.,(4,3,3,3,3,3,3,3,3,3,
3,3,3,3,3,3,3,3,3,3,3,3,3,3,3,3,3,3,3,3,3,3,4),(-0.760759816994486,-0.728677168897516,
-0.695709459409064,-0.679296550858681,-0.673136756605015,-0.639623073529853,
-0.605457412994165,-0.599329749581528,-0.591523615338422,-0.5567722273375,
-0.52169823453926,-0.486799286134059,-0.466411335710125,-0.455503184191866,
-0.450680877744631,-0.414687263581558,-0.404640118493239,-0.370062588212486,
-0.334594449163023,-0.314665985300723,-0.309139425335693,-0.304706824750879,
-0.268763856298477,-0.232207196979931,-0.195198731916467,-0.17229968507175,
-0.161302955218476,-0.156379428357842,-0.118526840186713,-0.0805958087489636,
-0.0433463054005835,-0.0149177406115234,-7.70748816987286E-5),
 .UNSPECIFIED.);
#2309=B_SPLINE_CURVE_WITH_KNOTS('',3,(#58577,#58578,#58579,#58580,#58581,
#58582,#58583,#58584,#58585,#58586,#58587,#58588,#58589,#58590,#58591,#58592,
#58593,#58594,#58595,#58596,#58597,#58598,#58599,#58600,#58601,#58602,#58603,
#58604,#58605,#58606,#58607,#58608,#58609,#58610,#58611,#58612,#58613,#58614,
#58615,#58616,#58617,#58618,#58619,#58620,#58621,#58622,#58623,#58624,#58625,
#58626,#58627,#58628,#58629,#58630,#58631,#58632,#58633,#58634,#58635,#58636,
#58637,#58638,#58639,#58640,#58641,#58642,#58643,#58644,#58645,#58646,#58647,
#58648,#58649,#58650,#58651,#58652,#58653,#58654,#58655,#58656,#58657,#58658,
#58659,#58660,#58661,#58662,#58663,#58664,#58665,#58666,#58667,#58668,#58669,
#58670,#58671,#58672,#58673,#58674,#58675,#58676),.UNSPECIFIED.,.F.,.F.,
(4,3,3,3,3,3,3,3,3,3,3,3,3,3,3,3,3,3,3,3,3,3,3,3,3,3,3,3,3,3,3,3,3,4),(-0.75776366468452,
-0.72011282712767,-0.68246198957082,-0.665890495352086,-0.657236255224794,
-0.61982311437852,-0.588448295761168,-0.574620607209714,-0.568701916322679,
-0.563203038262648,-0.5266525809423,-0.490393307629812,-0.455008248392471,
-0.433438511839063,-0.420355271578355,-0.414509520573623,-0.379626380580655,
-0.368822877170925,-0.333217025002694,-0.297701813310625,-0.27987286011839,
-0.274339780902846,-0.26957461784756,-0.234866709644299,-0.200136856371557,
-0.166019419234261,-0.146788567732903,-0.136613199619544,-0.130845342725424,
-0.0974461208295118,-0.0645472684616144,-0.0326317837335634,-0.0124385622348647,
0.),.UNSPECIFIED.);
#2310=B_SPLINE_CURVE_WITH_KNOTS('',3,(#58961,#58962,#58963,#58964,#58965,
#58966,#58967,#58968,#58969,#58970,#58971,#58972,#58973,#58974,#58975,#58976,
#58977,#58978,#58979,#58980,#58981,#58982,#58983,#58984,#58985,#58986,#58987,
#58988,#58989,#58990,#58991,#58992,#58993,#58994,#58995,#58996,#58997,#58998,
#58999,#59000,#59001,#59002,#59003,#59004,#59005,#59006,#59007,#59008,#59009,
#59010,#59011,#59012,#59013,#59014,#59015,#59016,#59017,#59018,#59019,#59020,
#59021,#59022,#59023,#59024,#59025,#59026,#59027,#59028,#59029,#59030,#59031,
#59032,#59033,#59034,#59035,#59036,#59037,#59038,#59039,#59040,#59041,#59042,
#59043,#59044,#59045,#59046,#59047,#59048,#59049,#59050,#59051,#59052,#59053,
#59054),.UNSPECIFIED.,.F.,.F.,(4,3,3,3,3,3,3,3,3,3,3,3,3,3,3,3,3,3,3,3,
3,3,3,3,3,3,3,3,3,3,3,4),(7.37877496047521E-15,0.0324242735236978,0.0650765288202324,
0.0985464079585014,0.129697094094769,0.134733078671135,0.168898023091528,
0.203503086561803,0.238170057614052,0.267361263736785,0.273576206797938,
0.27836433821044,0.314020768760248,0.349481163000816,0.355122983981023,
0.3899544235958,0.411931250623808,0.417329575041924,0.42221994011044,0.457543689126243,
0.493519846720045,0.530114209763389,0.556569206240022,0.564438243045673,
0.572420851034514,0.609740985058124,0.647119750965754,0.656486576561947,
0.666305087445587,0.704604264142757,0.742903440839926,0.757686856778839),
 .UNSPECIFIED.);
#2311=B_SPLINE_CURVE_WITH_KNOTS('',3,(#59340,#59341,#59342,#59343),
 .UNSPECIFIED.,.F.,.F.,(4,4),(-0.0162873178926763,0.),.UNSPECIFIED.);
#2312=B_SPLINE_CURVE_WITH_KNOTS('',3,(#59344,#59345,#59346,#59347,#59348,
#59349,#59350,#59351,#59352,#59353,#59354,#59355,#59356,#59357,#59358,#59359,
#59360,#59361,#59362,#59363,#59364,#59365,#59366,#59367,#59368,#59369,#59370,
#59371,#59372,#59373,#59374,#59375,#59376,#59377,#59378,#59379,#59380,#59381,
#59382,#59383,#59384,#59385,#59386,#59387,#59388,#59389,#59390,#59391,#59392,
#59393,#59394,#59395,#59396,#59397,#59398,#59399,#59400,#59401,#59402,#59403,
#59404,#59405,#59406,#59407,#59408,#59409,#59410,#59411,#59412,#59413,#59414,
#59415,#59416,#59417,#59418,#59419,#59420,#59421,#59422,#59423,#59424,#59425,
#59426,#59427,#59428,#59429,#59430,#59431,#59432,#59433,#59434,#59435,#59436,
#59437,#59438,#59439,#59440),.UNSPECIFIED.,.F.,.F.,(4,3,3,3,3,3,3,3,3,3,
3,3,3,3,3,3,3,3,3,3,3,3,3,3,3,3,3,3,3,3,3,3,4),(8.4031122921758E-15,0.0371549281743425,
0.0748575730861908,0.11271355525129,0.148602239855083,0.155563764461372,
0.1601385507907,0.197102163001497,0.233890618711408,0.269839031867023,0.300344999315642,
0.307576069988628,0.312824559625132,0.34807774400219,0.383140250103658,
0.39088593441124,0.426911555703311,0.446975446515054,0.453109732596831,
0.457476469900029,0.492419949903742,0.527549734179228,0.562225766766138,
0.586701700129649,0.593769962691508,0.599171083400769,0.633028984861318,
0.662011195208229,0.675191763445889,0.683249576797649,0.715766220161021,
0.748282863524393,0.760759816994521),.UNSPECIFIED.);
#2313=B_SPLINE_CURVE_WITH_KNOTS('',3,(#59501,#59502,#59503,#59504),
 .UNSPECIFIED.,.F.,.F.,(4,4),(112.182489743597,112.611961982353),
 .UNSPECIFIED.);
#2314=B_SPLINE_CURVE_WITH_KNOTS('',3,(#59507,#59508,#59509,#59510,#59511,
#59512,#59513,#59514,#59515,#59516,#59517,#59518,#59519,#59520,#59521,#59522,
#59523,#59524,#59525,#59526,#59527,#59528,#59529,#59530,#59531,#59532,#59533,
#59534,#59535,#59536,#59537),.UNSPECIFIED.,.F.,.F.,(4,3,3,3,3,3,3,3,3,3,
4),(112.181968556931,112.285773472651,112.391790544659,112.495346156522,
112.59884907986,112.702334544286,112.810228420394,112.91385103149,113.017546973854,
113.121410915295,113.133910048719),.UNSPECIFIED.);
#2315=B_SPLINE_CURVE_WITH_KNOTS('',3,(#59543,#59544,#59545,#59546,#59547,
#59548,#59549,#59550,#59551,#59552,#59553,#59554,#59555,#59556,#59557,#59558,
#59559,#59560,#59561,#59562,#59563,#59564,#59565,#59566,#59567,#59568,#59569,
#59570,#59571,#59572,#59573,#59574,#59575,#59576,#59577,#59578,#59579,#59580,
#59581,#59582,#59583,#59584,#59585,#59586,#59587,#59588,#59589,#59590,#59591,
#59592,#59593,#59594,#59595,#59596,#59597,#59598,#59599,#59600,#59601,#59602,
#59603,#59604,#59605,#59606,#59607,#59608,#59609,#59610,#59611,#59612,#59613,
#59614,#59615,#59616,#59617,#59618,#59619,#59620,#59621,#59622,#59623,#59624,
#59625,#59626,#59627,#59628,#59629,#59630,#59631,#59632,#59633,#59634,#59635,
#59636,#59637,#59638,#59639,#59640,#59641,#59642,#59643,#59644,#59645,#59646,
#59647,#59648,#59649,#59650,#59651,#59652,#59653,#59654,#59655,#59656,#59657,
#59658,#59659,#59660,#59661,#59662,#59663),.UNSPECIFIED.,.F.,.F.,(4,3,3,
3,3,3,3,3,3,3,3,3,3,3,3,3,3,3,3,3,3,3,3,3,3,3,3,3,3,3,3,3,3,3,3,3,3,3,3,
3,4),(105.899140451686,106.003024815435,106.106864212787,106.210693366653,
106.314717718923,106.418692007997,106.522861281791,106.626790775734,106.730987263758,
106.835028766578,106.93894855402,107.042803073214,107.146627085189,107.250455307722,
107.354392349897,107.458388337965,107.562566286003,107.62431931017,107.728406127187,
107.832337435927,107.936146784475,108.039890771643,108.143604319905,108.24732230847,
108.351150224774,108.455037544721,108.55910873153,108.621847844607,108.726214065306,
108.830424643138,108.934511720786,109.038532332813,109.142520999285,109.246512195638,
109.350608540247,109.454761991411,109.559092813096,109.619376379044,109.740298293392,
109.860139275301,109.955742676499),.UNSPECIFIED.);
#2316=B_SPLINE_CURVE_WITH_KNOTS('',3,(#59664,#59665,#59666,#59667,#59668,
#59669),.UNSPECIFIED.,.F.,.F.,(4,1,1,4),(109.955742875643,110.61690491348,
111.614433447917,112.182489743597),.UNSPECIFIED.);
#2317=B_SPLINE_CURVE_WITH_KNOTS('',3,(#59671,#59672,#59673,#59674,#59675,
#59676,#59677,#59678,#59679,#59680,#59681,#59682,#59683,#59684,#59685,#59686,
#59687,#59688,#59689,#59690,#59691,#59692,#59693,#59694,#59695,#59696,#59697,
#59698,#59699,#59700,#59701,#59702,#59703,#59704,#59705,#59706,#59707,#59708,
#59709,#59710,#59711,#59712,#59713,#59714,#59715,#59716,#59717,#59718,#59719,
#59720,#59721,#59722,#59723,#59724,#59725,#59726,#59727,#59728,#59729,#59730,
#59731,#59732,#59733,#59734,#59735,#59736,#59737,#59738,#59739,#59740),
 .UNSPECIFIED.,.F.,.F.,(4,3,3,3,3,3,3,3,3,3,3,3,3,3,3,3,3,3,3,3,3,3,3,4),
(109.955742875643,110.103310972773,110.160880318691,110.264967062808,110.368898298551,
110.472707574298,110.576451488819,110.68016496469,110.783882881219,110.887710726514,
110.991597975919,111.095669093687,111.158408853127,111.262775109417,111.366985722483,
111.47107283468,111.575093480817,111.679082180912,111.783073410354,111.887169787029,
111.991323269728,112.095654121783,112.155937387564,112.181968556931),
 .UNSPECIFIED.);
#2318=B_SPLINE_CURVE_WITH_KNOTS('',3,(#59741,#59742,#59743,#59744,#59745,
#59746,#59747,#59748,#59749,#59750,#59751,#59752,#59753,#59754,#59755,#59756,
#59757,#59758,#59759,#59760,#59761,#59762,#59763,#59764,#59765,#59766,#59767,
#59768,#59769,#59770,#59771,#59772,#59773,#59774,#59775,#59776,#59777,#59778,
#59779,#59780,#59781,#59782,#59783,#59784,#59785,#59786,#59787,#59788,#59789,
#59790,#59791,#59792,#59793,#59794,#59795,#59796,#59797,#59798,#59799,#59800,
#59801,#59802,#59803,#59804,#59805,#59806,#59807,#59808,#59809,#59810,#59811,
#59812,#59813,#59814,#59815,#59816,#59817,#59818,#59819,#59820,#59821,#59822,
#59823,#59824,#59825,#59826,#59827,#59828,#59829,#59830,#59831,#59832,#59833,
#59834,#59835,#59836,#59837,#59838,#59839,#59840,#59841,#59842,#59843,#59844,
#59845,#59846,#59847,#59848,#59849,#59850,#59851,#59852,#59853,#59854,#59855,
#59856,#59857,#59858,#59859,#59860,#59861,#59862,#59863,#59864),
 .UNSPECIFIED.,.F.,.F.,(4,3,3,3,3,3,3,3,3,3,3,3,3,3,3,3,3,3,3,3,3,3,3,3,
3,3,3,3,3,3,3,3,3,3,3,3,3,3,3,3,3,4),(105.898025478301,106.00200980369,
106.106176851874,106.170766180944,106.274954662883,106.378987940918,106.482899222427,
106.586745067332,106.690560250991,106.794379505344,106.89830743079,107.002294204721,
107.106462887271,107.168294715381,107.27246889799,107.376487822855,107.480384740769,
107.584216223424,107.688017067289,107.791822025433,107.895735819492,107.999708533646,
108.10386342229,108.165823249817,108.270028204319,108.37407786237,108.478005309915,
108.581867180328,108.685698226556,108.78953315797,108.893476372029,108.997478238522,
109.101661542088,109.163351784254,109.266012649306,109.368536778223,109.470960989788,
109.57332195874,109.675698114947,109.778078147715,109.88056957456,109.955742875311),
 .UNSPECIFIED.);
#2319=B_SPLINE_CURVE_WITH_KNOTS('',3,(#59870,#59871,#59872,#59873,#59874,
#59875,#59876,#59877,#59878,#59879,#59880,#59881,#59882,#59883,#59884,#59885,
#59886,#59887,#59888,#59889,#59890,#59891,#59892,#59893,#59894,#59895,#59896,
#59897,#59898,#59899,#59900,#59901,#59902,#59903,#59904,#59905,#59906,#59907,
#59908,#59909,#59910,#59911,#59912,#59913,#59914,#59915,#59916,#59917,#59918,
#59919,#59920,#59921,#59922,#59923,#59924,#59925,#59926,#59927,#59928,#59929,
#59930,#59931,#59932,#59933,#59934,#59935,#59936,#59937,#59938,#59939,#59940,
#59941,#59942,#59943,#59944,#59945,#59946,#59947,#59948,#59949,#59950,#59951,
#59952,#59953,#59954,#59955,#59956,#59957,#59958,#59959,#59960,#59961,#59962,
#59963,#59964,#59965,#59966,#59967,#59968,#59969,#59970,#59971,#59972,#59973,
#59974,#59975,#59976,#59977,#59978,#59979,#59980,#59981,#59982,#59983,#59984,
#59985,#59986,#59987,#59988,#59989,#59990,#59991,#59992,#59993,#59994,#59995,
#59996),.UNSPECIFIED.,.F.,.F.,(4,3,3,3,3,3,3,3,3,3,3,3,3,3,3,3,3,3,3,3,
3,3,3,3,3,3,3,3,3,3,3,3,3,3,3,3,3,3,3,3,3,3,4),(99.6152316573692,99.6440910346775,
99.7482776242847,99.852308980079,99.9562183047007,100.060062172463,100.163875361819,
100.267692607789,100.371618517559,100.475603268673,100.579769939392,100.641619569114,
100.745806326648,100.849837854855,100.953747357642,101.057591407011,101.161404781119,
101.265222214687,101.369148315049,101.473133258728,101.577300122986,101.639148103551,
101.743333059736,101.847362781364,101.951270478531,102.055112723852,102.158924298124,
102.262739938717,102.366664268879,102.470647452536,102.574812591943,102.636676637987,
102.740864888504,102.8448978973,102.948808855441,103.052654343846,103.156469138697,
103.260287972727,103.36421543326,103.468201716448,103.572369873255,103.634205172424,
103.672557568463),.UNSPECIFIED.);
#2320=B_SPLINE_CURVE_WITH_KNOTS('',3,(#59997,#59998,#59999,#60000,#60001,
#60002,#60003,#60004,#60005,#60006,#60007,#60008,#60009,#60010,#60011,#60012,
#60013,#60014,#60015,#60016,#60017,#60018,#60019,#60020,#60021,#60022,#60023,
#60024,#60025,#60026,#60027,#60028,#60029,#60030,#60031,#60032,#60033,#60034,
#60035,#60036,#60037,#60038,#60039,#60040,#60041,#60042,#60043,#60044,#60045,
#60046,#60047,#60048,#60049,#60050,#60051,#60052,#60053,#60054,#60055,#60056,
#60057,#60058,#60059,#60060,#60061,#60062,#60063,#60064,#60065,#60066),
 .UNSPECIFIED.,.F.,.F.,(4,3,3,3,3,3,3,3,3,3,3,3,3,3,3,3,3,3,3,3,3,3,3,4),
(103.672557568736,103.776099131449,103.883053453376,103.986323984164,104.089534941353,
104.192721969991,104.295920677775,104.399231122839,104.502608908511,104.606156363019,
104.631733706861,104.735907902116,104.839926839642,104.943823770182,105.047655265435,
105.151456121852,105.255261092482,105.359174898845,105.463147625218,105.567302525815,
105.629262241297,105.73346168362,105.837495278037,105.899140451686),
 .UNSPECIFIED.);
#2321=B_SPLINE_CURVE_WITH_KNOTS('',3,(#60068,#60069,#60070,#60071,#60072,
#60073,#60074,#60075,#60076,#60077,#60078,#60079,#60080,#60081,#60082,#60083,
#60084,#60085,#60086,#60087,#60088,#60089,#60090,#60091,#60092,#60093,#60094,
#60095,#60096,#60097,#60098,#60099,#60100,#60101,#60102,#60103,#60104,#60105,
#60106,#60107,#60108,#60109,#60110,#60111,#60112,#60113,#60114,#60115,#60116,
#60117,#60118,#60119,#60120,#60121,#60122,#60123,#60124,#60125,#60126,#60127,
#60128,#60129,#60130,#60131,#60132,#60133,#60134),.UNSPECIFIED.,.F.,.F.,
(4,3,3,3,3,3,3,3,3,3,3,3,3,3,3,3,3,3,3,3,3,3,4),(103.672557568463,103.781092798507,
103.889920271511,103.998901190727,104.108175816525,104.175709112071,104.279894066294,
104.383923785958,104.487831481169,104.591673724538,104.695485296866,104.799300935527,
104.903225263787,105.007208445554,105.111373583115,105.173237646508,105.277400211582,
105.381419534253,105.485330617835,105.58918653948,105.69300465016,105.796876384297,
105.898025478301),.UNSPECIFIED.);
#2322=B_SPLINE_CURVE_WITH_KNOTS('',3,(#60135,#60136,#60137,#60138,#60139,
#60140,#60141,#60142,#60143,#60144,#60145,#60146,#60147,#60148,#60149,#60150,
#60151,#60152,#60153,#60154,#60155,#60156,#60157,#60158,#60159,#60160,#60161,
#60162,#60163,#60164,#60165,#60166,#60167,#60168,#60169,#60170,#60171,#60172,
#60173,#60174,#60175,#60176,#60177,#60178,#60179,#60180,#60181,#60182,#60183,
#60184,#60185,#60186,#60187,#60188,#60189,#60190,#60191,#60192,#60193,#60194,
#60195,#60196,#60197,#60198,#60199,#60200,#60201,#60202,#60203,#60204,#60205,
#60206,#60207,#60208,#60209,#60210,#60211,#60212,#60213,#60214,#60215,#60216,
#60217,#60218,#60219,#60220,#60221,#60222,#60223,#60224,#60225,#60226,#60227,
#60228,#60229,#60230,#60231,#60232,#60233,#60234,#60235,#60236,#60237,#60238,
#60239,#60240,#60241,#60242,#60243,#60244,#60245,#60246,#60247,#60248,#60249,
#60250,#60251,#60252,#60253,#60254,#60255,#60256,#60257,#60258),
 .UNSPECIFIED.,.F.,.F.,(4,3,3,3,3,3,3,3,3,3,3,3,3,3,3,3,3,3,3,3,3,3,3,3,
3,3,3,3,3,3,3,3,3,3,3,3,3,3,3,3,3,4),(99.6156110735334,99.7194228461579,
99.8232425484925,99.9271733249442,100.031166423026,100.135337924969,100.185594974325,
100.289781443786,100.393812681037,100.497721890031,100.601565644022,100.705378721615,
100.809195857982,100.913121662166,101.0171063098,101.121272881461,101.183123508761,
101.287309756554,101.391340771663,101.49524975888,101.599093291441,101.70290614827,
101.806723064866,101.910648652299,102.014633084558,102.118799445352,102.180652043198,
102.284838632953,102.388869988893,102.492779313656,102.596623181558,102.700436371051,
102.804253617154,102.908179527053,103.012164278294,103.116330949132,103.178180577634,
103.287930451885,103.397356063251,103.506584798371,103.615565394141,103.672557568099),
 .UNSPECIFIED.);
#2323=B_SPLINE_CURVE_WITH_KNOTS('',3,(#60264,#60265,#60266,#60267,#60268,
#60269,#60270,#60271,#60272,#60273,#60274,#60275,#60276,#60277,#60278,#60279,
#60280,#60281,#60282,#60283,#60284,#60285,#60286,#60287,#60288,#60289,#60290,
#60291,#60292,#60293,#60294,#60295,#60296,#60297,#60298,#60299,#60300,#60301,
#60302,#60303,#60304,#60305,#60306,#60307,#60308,#60309,#60310,#60311,#60312,
#60313,#60314,#60315,#60316,#60317,#60318,#60319,#60320,#60321,#60322,#60323,
#60324,#60325,#60326,#60327,#60328,#60329,#60330,#60331,#60332,#60333,#60334,
#60335,#60336,#60337,#60338,#60339,#60340,#60341,#60342,#60343,#60344,#60345,
#60346,#60347,#60348,#60349,#60350,#60351,#60352,#60353,#60354,#60355,#60356,
#60357,#60358,#60359,#60360,#60361,#60362,#60363,#60364,#60365,#60366,#60367,
#60368,#60369,#60370,#60371,#60372,#60373,#60374,#60375,#60376,#60377,#60378,
#60379,#60380,#60381,#60382,#60383,#60384,#60385,#60386,#60387,#60388,#60389,
#60390),.UNSPECIFIED.,.F.,.F.,(4,3,3,3,3,3,3,3,3,3,3,3,3,3,3,3,3,3,3,3,
3,3,3,3,3,3,3,3,3,3,3,3,3,3,3,3,3,3,3,3,3,3,4),(93.3317416570353,93.4356900182446,
93.5397112732845,93.6439007855695,93.6589198280579,93.7631062483201,93.867137435993,
93.9710465950891,94.0748902990129,94.1787033264439,94.2825204126295,94.3864461669513,
94.4904307648283,94.5945972874407,94.6564483624945,94.7606347887181,94.8646659824113,
94.9685751475859,95.0724188576205,95.1762318911854,95.2800489835188,95.3839747439665,
95.4879593479663,95.5921258766296,95.6539768969311,95.7581632966126,95.8621944637261,
95.9661036023919,96.069947285976,96.1737602931869,96.2775773593012,96.3815030939157,
96.4854876722607,96.589654175829,96.6515054313677,96.7545601138384,96.8574737137944,
96.960282655331,97.0675550568191,97.1702894267118,97.2730248740603,97.3758310709248,
97.3893722612835),.UNSPECIFIED.);
#2324=B_SPLINE_CURVE_WITH_KNOTS('',3,(#60391,#60392,#60393,#60394,#60395,
#60396,#60397,#60398,#60399,#60400,#60401,#60402,#60403,#60404,#60405,#60406,
#60407,#60408,#60409,#60410,#60411,#60412,#60413,#60414,#60415,#60416,#60417,
#60418,#60419,#60420,#60421,#60422,#60423,#60424,#60425,#60426,#60427,#60428,
#60429,#60430,#60431,#60432,#60433,#60434,#60435,#60436,#60437,#60438,#60439,
#60440,#60441,#60442,#60443,#60444,#60445,#60446,#60447,#60448,#60449,#60450,
#60451,#60452,#60453,#60454,#60455,#60456,#60457),.UNSPECIFIED.,.F.,.F.,
(4,3,3,3,3,3,3,3,3,3,3,3,3,3,3,3,3,3,3,3,3,3,4),(97.3893722615608,97.5221133461261,
97.6490339658043,97.7532204351495,97.8572516722844,97.961160881162,98.0650046350367,
98.1688177125131,98.2726348487633,98.3765606528317,98.4805453003508,98.5847118718985,
98.6465625002409,98.750750772808,98.8588108833781,98.9627158777204,99.0665559339843,
99.170365829249,99.274180297392,99.3780947560921,99.4820689269285,99.5862024311775,
99.6152316573692),.UNSPECIFIED.);
#2325=B_SPLINE_CURVE_WITH_KNOTS('',3,(#60459,#60460,#60461,#60462,#60463,
#60464,#60465,#60466,#60467,#60468,#60469,#60470,#60471,#60472,#60473,#60474,
#60475,#60476,#60477,#60478,#60479,#60480,#60481,#60482,#60483,#60484,#60485,
#60486,#60487,#60488,#60489,#60490,#60491,#60492,#60493,#60494,#60495,#60496,
#60497,#60498,#60499,#60500,#60501,#60502,#60503,#60504,#60505,#60506,#60507,
#60508,#60509,#60510,#60511,#60512,#60513,#60514,#60515,#60516,#60517,#60518,
#60519,#60520,#60521,#60522,#60523,#60524,#60525),.UNSPECIFIED.,.F.,.F.,
(4,3,3,3,3,3,3,3,3,3,3,3,3,3,3,3,3,3,3,3,3,3,4),(97.389372261676,97.4918503890655,
97.5942398116576,97.6965771922798,97.7988991181241,97.9013122938342,98.0037702233957,
98.1064116155926,98.1905379054514,98.2947243050946,98.3987554721697,98.5026646107974,
98.6065082943435,98.7103213015167,98.8141383675937,98.9180641021713,99.0220486804797,
99.1262151840124,99.1880664398879,99.2949525982993,99.3989655196461,99.5072882965898,
99.6156110735334),.UNSPECIFIED.);
#2326=B_SPLINE_CURVE_WITH_KNOTS('',3,(#60526,#60527,#60528,#60529,#60530,
#60531,#60532,#60533,#60534,#60535,#60536,#60537,#60538,#60539,#60540,#60541,
#60542,#60543,#60544,#60545,#60546,#60547,#60548,#60549,#60550,#60551,#60552,
#60553,#60554,#60555,#60556,#60557,#60558,#60559,#60560,#60561,#60562,#60563,
#60564,#60565,#60566,#60567,#60568,#60569,#60570,#60571,#60572,#60573,#60574,
#60575,#60576,#60577,#60578,#60579,#60580,#60581,#60582,#60583,#60584,#60585,
#60586,#60587,#60588,#60589,#60590,#60591,#60592,#60593,#60594,#60595,#60596,
#60597,#60598,#60599,#60600,#60601,#60602,#60603,#60604,#60605,#60606,#60607,
#60608,#60609,#60610,#60611,#60612,#60613,#60614,#60615,#60616,#60617,#60618,
#60619,#60620,#60621,#60622,#60623,#60624,#60625,#60626,#60627,#60628,#60629,
#60630,#60631,#60632,#60633,#60634,#60635,#60636,#60637,#60638,#60639,#60640,
#60641,#60642,#60643,#60644,#60645,#60646,#60647,#60648,#60649),
 .UNSPECIFIED.,.F.,.F.,(4,3,3,3,3,3,3,3,3,3,3,3,3,3,3,3,3,3,3,3,3,3,3,3,
3,3,3,3,3,3,3,3,3,3,3,3,3,3,3,3,3,4),(93.3327269072094,93.4411890147714,
93.545075652954,93.6489069061472,93.7527175368652,93.8565422742999,93.9604818343983,
94.0644892674887,94.1686696731495,94.2004237677049,94.3046101878998,94.40864137553,
94.5125505346197,94.6163942385596,94.7202072660287,94.8240243522744,94.9279501066888,
95.0319347046769,95.1361012274282,95.1979523021416,95.302138719216,95.4061699037234,
95.5100790597019,95.6139227605392,95.7177357849191,95.8215528680932,95.9254786194841,
96.0294632144714,96.1336297342899,96.1954808365782,96.2996672568408,96.403698444514,
96.5076076036104,96.6114513075345,96.7152643349658,96.8190814211517,96.9230071754736,
97.0269917733508,97.1311582959633,97.1930093710148,97.3433995555629,97.3893722612835),
 .UNSPECIFIED.);
#2327=B_SPLINE_CURVE_WITH_KNOTS('',3,(#60655,#60656,#60657,#60658,#60659,
#60660,#60661,#60662,#60663,#60664,#60665,#60666,#60667,#60668,#60669,#60670,
#60671,#60672,#60673,#60674,#60675,#60676,#60677,#60678,#60679,#60680,#60681,
#60682,#60683,#60684,#60685,#60686,#60687,#60688,#60689,#60690,#60691,#60692,
#60693,#60694,#60695,#60696,#60697,#60698,#60699,#60700,#60701,#60702,#60703,
#60704,#60705,#60706,#60707,#60708,#60709,#60710,#60711,#60712,#60713,#60714,
#60715,#60716,#60717,#60718,#60719,#60720,#60721,#60722,#60723,#60724,#60725,
#60726,#60727,#60728,#60729,#60730,#60731,#60732,#60733,#60734,#60735,#60736,
#60737,#60738,#60739,#60740,#60741,#60742,#60743,#60744,#60745,#60746,#60747,
#60748,#60749,#60750,#60751,#60752,#60753,#60754,#60755,#60756,#60757,#60758,
#60759,#60760,#60761,#60762,#60763,#60764,#60765,#60766,#60767,#60768,#60769,
#60770,#60771,#60772,#60773,#60774,#60775),.UNSPECIFIED.,.F.,.F.,(4,3,3,
3,3,3,3,3,3,3,3,3,3,3,3,3,3,3,3,3,3,3,3,3,3,3,3,3,3,3,3,3,3,3,3,3,3,3,3,
3,4),(87.0493885881288,87.1532100506506,87.2570212560048,87.3612030973632,
87.4651598347553,87.5694542280968,87.6737486214383,87.7779350407011,87.881966227395,
87.9858753855465,88.0897190885474,88.1935321150783,88.297349200388,88.4012749538761,
88.505259550942,88.6094260727875,88.6712771558749,88.775463575262,88.8794947620805,
88.9834039203575,89.0872476234842,89.1910606501409,89.2948777355758,89.3988034891882,
89.502788086378,89.6069546083453,89.6688056903115,89.7729921093415,89.8770232958033,
89.9809324537247,90.0847761564972,90.1885891828012,90.2924062678863,90.3963320211544,
90.5003166180026,90.6044831396363,90.6663342247481,90.7790776483305,90.8915379903017,
91.0035447872594,91.1061869538188),.UNSPECIFIED.);
#2328=B_SPLINE_CURVE_WITH_KNOTS('',3,(#60776,#60777,#60778,#60779,#60780,
#60781,#60782,#60783,#60784,#60785,#60786,#60787,#60788,#60789,#60790,#60791,
#60792,#60793,#60794,#60795,#60796,#60797,#60798,#60799,#60800,#60801,#60802,
#60803,#60804,#60805,#60806,#60807,#60808,#60809,#60810,#60811,#60812,#60813,
#60814,#60815,#60816,#60817,#60818,#60819,#60820,#60821,#60822,#60823,#60824,
#60825,#60826,#60827,#60828,#60829,#60830,#60831,#60832,#60833,#60834,#60835,
#60836,#60837,#60838,#60839,#60840,#60841,#60842,#60843,#60844,#60845),
 .UNSPECIFIED.,.F.,.F.,(4,3,3,3,3,3,3,3,3,3,3,3,3,3,3,3,3,3,3,3,3,3,3,4),
(91.106186954104,91.2126211265272,91.3191385231278,91.425852667608,91.5326811228738,
91.6397298025484,91.6638627591847,91.768049179377,91.8720803670044,91.9759895260916,
92.0798332300288,92.1836462574954,92.2874633437386,92.3913890981505,92.495373696136,
92.5995402188847,92.6613912936213,92.7655571769376,92.8695782420305,92.9734895025858,
93.0773351539117,93.1811423844798,93.28497571317,93.3317416570353),
 .UNSPECIFIED.);
#2329=B_SPLINE_CURVE_WITH_KNOTS('',3,(#60847,#60848,#60849,#60850,#60851,
#60852,#60853,#60854,#60855,#60856,#60857,#60858,#60859,#60860,#60861,#60862,
#60863,#60864,#60865,#60866,#60867,#60868,#60869,#60870,#60871,#60872,#60873,
#60874,#60875,#60876,#60877,#60878,#60879,#60880,#60881,#60882,#60883,#60884,
#60885,#60886,#60887,#60888,#60889,#60890,#60891,#60892,#60893,#60894,#60895,
#60896,#60897,#60898,#60899,#60900,#60901,#60902,#60903,#60904,#60905,#60906,
#60907,#60908,#60909,#60910,#60911,#60912,#60913,#60914,#60915,#60916),
 .UNSPECIFIED.,.F.,.F.,(4,3,3,3,3,3,3,3,3,3,3,3,3,3,3,3,3,3,3,3,3,3,3,4),
(91.106186954104,91.2078381643952,91.3120245837827,91.4160557706019,91.5199649288792,
91.6238086320062,91.7276216586632,91.8314387440987,91.9353644977115,92.0393490949017,
92.1435156168694,92.2053666988318,92.3095531178613,92.4135843043225,92.5174934622435,
92.6213371650153,92.725150191319,92.8289672764033,92.9328930296709,93.0368776265185,
93.1410441481518,93.2028952332684,93.3070788474263,93.3327269072094),
 .UNSPECIFIED.);
#2330=B_SPLINE_CURVE_WITH_KNOTS('',3,(#60917,#60918,#60919,#60920,#60921,
#60922,#60923,#60924,#60925,#60926,#60927,#60928,#60929,#60930,#60931,#60932,
#60933,#60934,#60935,#60936,#60937,#60938,#60939,#60940,#60941,#60942,#60943,
#60944,#60945,#60946,#60947,#60948,#60949,#60950,#60951,#60952,#60953,#60954,
#60955,#60956,#60957,#60958,#60959,#60960,#60961,#60962,#60963,#60964,#60965,
#60966,#60967,#60968,#60969,#60970,#60971,#60972,#60973,#60974,#60975,#60976,
#60977,#60978,#60979,#60980,#60981,#60982,#60983,#60984,#60985,#60986,#60987,
#60988,#60989,#60990,#60991,#60992,#60993,#60994,#60995,#60996,#60997,#60998,
#60999,#61000,#61001,#61002,#61003,#61004,#61005,#61006,#61007,#61008,#61009,
#61010,#61011,#61012,#61013,#61014,#61015,#61016,#61017,#61018,#61019,#61020,
#61021,#61022,#61023,#61024,#61025,#61026,#61027,#61028,#61029,#61030,#61031,
#61032,#61033,#61034,#61035,#61036,#61037,#61038,#61039,#61040),
 .UNSPECIFIED.,.F.,.F.,(4,3,3,3,3,3,3,3,3,3,3,3,3,3,3,3,3,3,3,3,3,3,3,3,
3,3,3,3,3,3,3,3,3,3,3,3,3,3,3,3,3,4),(87.0484498294534,87.1526150410913,
87.2177240266488,87.3219104459156,87.4259416326137,87.5298507907699,87.6336944937756,
87.7375075203117,87.8413246056266,87.9452503591202,88.0492349561918,88.1534014780432,
88.2152525610854,88.3194389803689,88.4234701670837,88.5273793252565,88.631223028279,
88.7350360548318,88.8388531401634,88.9427788936735,89.0467634907616,89.1509300126291,
89.212781095522,89.3169675147653,89.4209987014401,89.5249078595731,89.6287515625559,
89.7325645890692,89.8363816743616,89.9403074278333,90.0442920248832,90.1484585467135,
90.2103096299586,90.3131827203157,90.4158805807014,90.5184806860294,90.621019531032,
90.7235335248247,90.8261208448599,90.9287446854245,91.0315305435812,91.1061869536406),
 .UNSPECIFIED.);
#2331=B_SPLINE_CURVE_WITH_KNOTS('',3,(#61046,#61047,#61048,#61049,#61050,
#61051,#61052,#61053,#61054,#61055,#61056,#61057,#61058,#61059,#61060,#61061,
#61062,#61063,#61064,#61065,#61066,#61067,#61068,#61069,#61070,#61071,#61072,
#61073,#61074,#61075,#61076,#61077,#61078,#61079,#61080,#61081,#61082,#61083,
#61084,#61085,#61086,#61087,#61088,#61089,#61090,#61091,#61092,#61093,#61094,
#61095,#61096,#61097,#61098,#61099,#61100,#61101,#61102,#61103,#61104,#61105,
#61106,#61107,#61108,#61109,#61110,#61111,#61112,#61113,#61114,#61115,#61116,
#61117,#61118,#61119,#61120,#61121,#61122,#61123,#61124,#61125,#61126,#61127,
#61128,#61129,#61130,#61131,#61132,#61133,#61134,#61135,#61136,#61137,#61138,
#61139,#61140,#61141,#61142,#61143,#61144,#61145,#61146,#61147,#61148,#61149,
#61150,#61151,#61152,#61153,#61154,#61155,#61156,#61157,#61158,#61159,#61160,
#61161,#61162,#61163,#61164,#61165,#61166),.UNSPECIFIED.,.F.,.F.,(4,3,3,
3,3,3,3,3,3,3,3,3,3,3,3,3,3,3,3,3,3,3,3,3,3,3,3,3,3,3,3,3,3,3,3,3,3,3,3,
3,4),(80.7662045556485,80.8702751267713,80.9742087479646,81.0780672034999,
81.1818852904301,81.2856977526014,81.3896126700318,81.4935777329238,81.5977339187956,
81.6885774148187,81.792763834087,81.8967950207866,82.0007041789443,82.1045478819516,
82.2083609084893,82.3121779938057,82.416103747301,82.5200883443742,82.6242548662273,
82.6861059492553,82.7902923685257,82.8943235552275,82.9982327133873,83.1020764163968,
83.2058894429367,83.3097065282554,83.4136322817528,83.5176168788281,83.6217834006832,
83.6836344836919,83.787820902958,83.8918520896554,83.9957612478108,84.099604950816,
84.2034179773515,84.3072350626659,84.4111608161591,84.5151454132304,84.6193119350814,
84.6811630181285,84.8230016469244),.UNSPECIFIED.);
#2332=B_SPLINE_CURVE_WITH_KNOTS('',3,(#61167,#61168,#61169,#61170,#61171,
#61172,#61173,#61174,#61175,#61176,#61177,#61178,#61179,#61180,#61181,#61182,
#61183,#61184,#61185,#61186,#61187,#61188,#61189,#61190,#61191,#61192,#61193,
#61194,#61195,#61196,#61197,#61198,#61199,#61200,#61201,#61202,#61203,#61204,
#61205,#61206,#61207,#61208,#61209,#61210,#61211,#61212,#61213,#61214,#61215,
#61216,#61217,#61218,#61219,#61220,#61221,#61222,#61223,#61224,#61225,#61226,
#61227,#61228,#61229,#61230,#61231,#61232,#61233,#61234,#61235,#61236),
 .UNSPECIFIED.,.F.,.F.,(4,3,3,3,3,3,3,3,3,3,3,3,3,3,3,3,3,3,3,3,3,3,3,4),
(84.8230016473368,84.9299628854903,85.0323879596833,85.1347430254586,85.2370647046657,
85.3393895675522,85.4418181479453,85.544308232961,85.6469663801133,85.6786915525651,
85.7828779718485,85.8869091585633,85.9908183167361,86.0946620197585,86.1984750463114,
86.3022921316428,86.4062178851529,86.510202482241,86.6143690041085,86.6762200870017,
86.7803789666152,86.8844021488389,86.9883093146419,87.0493885881288),
 .UNSPECIFIED.);
#2333=B_SPLINE_CURVE_WITH_KNOTS('',3,(#61238,#61239,#61240,#61241,#61242,
#61243,#61244,#61245,#61246,#61247,#61248,#61249,#61250,#61251,#61252,#61253,
#61254,#61255,#61256,#61257,#61258,#61259,#61260,#61261,#61262,#61263,#61264,
#61265,#61266,#61267,#61268,#61269,#61270,#61271,#61272,#61273,#61274,#61275,
#61276,#61277,#61278,#61279,#61280,#61281,#61282,#61283,#61284,#61285,#61286,
#61287,#61288,#61289,#61290,#61291,#61292,#61293,#61294,#61295,#61296,#61297,
#61298,#61299,#61300,#61301,#61302,#61303,#61304),.UNSPECIFIED.,.F.,.F.,
(4,3,3,3,3,3,3,3,3,3,3,3,3,3,3,3,3,3,3,3,3,3,4),(84.8230016473359,84.9377580239963,
85.0529300598084,85.1686593350748,85.2226669577756,85.3268533770461,85.4308845637479,
85.5347937219076,85.6386374249172,85.742450451457,85.8462675367755,85.9501932902729,
86.0541778873482,86.1583444092033,86.2201954922122,86.3243482554789,86.4283607948039,
86.5322681022207,86.6361050469233,86.739945971975,86.8437814338426,86.947723902542,
87.0484498294534),.UNSPECIFIED.);
#2334=B_SPLINE_CURVE_WITH_KNOTS('',3,(#61305,#61306,#61307,#61308,#61309,
#61310,#61311,#61312,#61313,#61314,#61315,#61316,#61317,#61318,#61319,#61320,
#61321,#61322,#61323,#61324,#61325,#61326,#61327,#61328,#61329,#61330,#61331,
#61332,#61333,#61334,#61335,#61336,#61337,#61338,#61339,#61340,#61341,#61342,
#61343,#61344,#61345,#61346,#61347,#61348,#61349,#61350,#61351,#61352,#61353,
#61354,#61355,#61356,#61357,#61358,#61359,#61360,#61361,#61362,#61363,#61364,
#61365,#61366,#61367,#61368,#61369,#61370,#61371,#61372,#61373,#61374,#61375,
#61376,#61377,#61378,#61379,#61380,#61381,#61382,#61383,#61384,#61385,#61386,
#61387,#61388,#61389,#61390,#61391,#61392,#61393,#61394,#61395,#61396,#61397,
#61398,#61399,#61400,#61401,#61402,#61403,#61404,#61405,#61406,#61407,#61408,
#61409,#61410,#61411,#61412,#61413,#61414,#61415,#61416,#61417,#61418,#61419,
#61420,#61421,#61422,#61423,#61424,#61425,#61426,#61427,#61428),
 .UNSPECIFIED.,.F.,.F.,(4,3,3,3,3,3,3,3,3,3,3,3,3,3,3,3,3,3,3,3,3,3,3,3,
3,3,3,3,3,3,3,3,3,3,3,3,3,3,3,3,3,4),(80.76574074697,80.8695602808333,80.9734907573594,
81.0774833634171,81.1816545661312,81.2325528200292,81.3367392392979,81.4407704259977,
81.5446795841557,81.6485232871634,81.7523363137014,81.8561533990182,81.9600791525138,
82.0640637495873,82.1682302714407,82.2300813544658,82.3342677737346,82.438298960435,
82.5422081185932,82.6460518216011,82.7498648481394,82.8536819334565,82.9576076869522,
83.0615922840261,83.1657588058797,83.2276098889024,83.3317963081708,83.4358274948703,
83.539736653028,83.6435803560355,83.7473933825735,83.8512104678899,83.9551362213854,
84.0591208184588,84.1632873403121,84.225138423339,84.3308712802875,84.4364337114794,
84.5418329411289,84.6471360606506,84.7523779621414,84.8230016469245),
 .UNSPECIFIED.);
#2335=B_SPLINE_CURVE_WITH_KNOTS('',3,(#61434,#61435,#61436,#61437,#61438,
#61439,#61440,#61441,#61442,#61443,#61444,#61445,#61446,#61447,#61448,#61449,
#61450,#61451,#61452,#61453,#61454,#61455,#61456,#61457,#61458,#61459,#61460,
#61461,#61462,#61463,#61464,#61465,#61466,#61467,#61468,#61469,#61470,#61471,
#61472,#61473,#61474,#61475,#61476,#61477,#61478,#61479,#61480,#61481,#61482,
#61483,#61484,#61485,#61486,#61487,#61488,#61489,#61490,#61491,#61492,#61493,
#61494,#61495,#61496,#61497,#61498,#61499,#61500,#61501,#61502,#61503,#61504,
#61505,#61506,#61507,#61508,#61509,#61510,#61511,#61512,#61513,#61514,#61515,
#61516,#61517,#61518,#61519,#61520,#61521,#61522,#61523,#61524,#61525,#61526,
#61527,#61528,#61529,#61530,#61531,#61532,#61533,#61534,#61535,#61536,#61537,
#61538,#61539,#61540,#61541,#61542,#61543,#61544,#61545,#61546,#61547,#61548,
#61549,#61550,#61551,#61552,#61553,#61554,#61555,#61556,#61557,#61558,#61559,
#61560),.UNSPECIFIED.,.F.,.F.,(4,3,3,3,3,3,3,3,3,3,3,3,3,3,3,3,3,3,3,3,
3,3,3,3,3,3,3,3,3,3,3,3,3,3,3,3,3,3,3,3,3,3,4),(74.482061581652,74.5860823401427,
74.6902715180945,74.7058776737625,74.8100640930311,74.9140952797311,75.0180044378891,
75.1218481408968,75.2256611674348,75.3294782527516,75.4334040062472,75.5373886033208,
75.6415551251742,75.7034062081991,75.8075926274677,75.9116238141677,76.0155329723257,
76.1193766753334,76.2231897018714,76.3270067871883,76.4309325406839,76.5349171377575,
76.6390836596109,76.7009347426357,76.8051211619044,76.9091523486044,77.0130615067624,
77.1169052097702,77.2207182363082,77.3245353216251,77.4284610751208,77.5324456721944,
77.6366121940478,77.6984632770723,77.8036324098607,77.9060965907541,78.0084634414062,
78.1107696824821,78.2180313467064,78.3203753326912,78.4227592903787,78.5252692706971,
78.5398163393791),.UNSPECIFIED.);
#2336=B_SPLINE_CURVE_WITH_KNOTS('',3,(#61561,#61562,#61563,#61564,#61565,
#61566,#61567,#61568,#61569,#61570,#61571,#61572,#61573,#61574,#61575,#61576,
#61577,#61578,#61579,#61580,#61581,#61582,#61583,#61584,#61585,#61586,#61587,
#61588,#61589,#61590,#61591,#61592,#61593,#61594,#61595,#61596,#61597,#61598,
#61599,#61600,#61601,#61602,#61603,#61604,#61605,#61606,#61607,#61608,#61609,
#61610,#61611,#61612,#61613,#61614,#61615,#61616,#61617,#61618,#61619,#61620,
#61621,#61622,#61623,#61624,#61625,#61626,#61627),.UNSPECIFIED.,.F.,.F.,
(4,3,3,3,3,3,3,3,3,3,3,3,3,3,3,3,3,3,3,3,3,3,4),(78.5398163397449,78.6959918115089,
78.8001782307774,78.9042094174774,79.0081185756353,79.111962278643,79.2157753051809,
79.3195923904978,79.4235181439933,79.5275027410669,79.6316692629202,79.6935203459455,
79.7977067652144,79.9017379519145,80.0056471100728,80.1094908130807,80.2133038396189,
80.317120924936,80.4210466784318,80.5250312755056,80.6291977973592,80.6910488803821,
80.7662045556485),.UNSPECIFIED.);
#2337=B_SPLINE_CURVE_WITH_KNOTS('',3,(#61629,#61630,#61631,#61632,#61633,
#61634,#61635,#61636,#61637,#61638,#61639,#61640,#61641,#61642,#61643,#61644,
#61645,#61646,#61647,#61648,#61649,#61650,#61651,#61652,#61653,#61654,#61655,
#61656,#61657,#61658,#61659,#61660,#61661,#61662,#61663,#61664,#61665,#61666,
#61667,#61668,#61669,#61670,#61671,#61672,#61673,#61674,#61675,#61676,#61677,
#61678,#61679,#61680,#61681,#61682,#61683,#61684,#61685,#61686,#61687,#61688,
#61689,#61690,#61691,#61692,#61693,#61694,#61695),.UNSPECIFIED.,.F.,.F.,
(4,3,3,3,3,3,3,3,3,3,3,3,3,3,3,3,3,3,3,3,3,3,4),(78.5398163397448,78.6430648259428,
78.7462751676037,78.8494829022752,78.9527963206924,79.0561639752372,79.1597213368926,
79.237495751156,79.3416821704247,79.4457133571247,79.5496225152827,79.6534662182905,
79.7572792448284,79.8610963301453,79.9650220836409,80.0690066807144,80.1731732025678,
80.2350242855926,80.3392063862691,80.4458399764443,80.5497449585483,80.6577428527591,
80.76574074697),.UNSPECIFIED.);
#2338=B_SPLINE_CURVE_WITH_KNOTS('',3,(#61696,#61697,#61698,#61699,#61700,
#61701,#61702,#61703,#61704,#61705,#61706,#61707,#61708,#61709,#61710,#61711,
#61712,#61713,#61714,#61715,#61716,#61717,#61718,#61719,#61720,#61721,#61722,
#61723,#61724,#61725,#61726,#61727,#61728,#61729,#61730,#61731,#61732,#61733,
#61734,#61735,#61736,#61737,#61738,#61739,#61740,#61741,#61742,#61743,#61744,
#61745,#61746,#61747,#61748,#61749,#61750,#61751,#61752,#61753,#61754,#61755,
#61756,#61757,#61758,#61759,#61760,#61761,#61762,#61763,#61764,#61765,#61766,
#61767,#61768,#61769,#61770,#61771,#61772,#61773,#61774,#61775,#61776,#61777,
#61778,#61779,#61780,#61781,#61782,#61783,#61784,#61785,#61786,#61787,#61788,
#61789,#61790,#61791,#61792,#61793,#61794,#61795,#61796,#61797,#61798,#61799,
#61800,#61801,#61802,#61803,#61804,#61805,#61806,#61807,#61808,#61809,#61810,
#61811,#61812,#61813,#61814,#61815,#61816,#61817,#61818,#61819),
 .UNSPECIFIED.,.F.,.F.,(4,3,3,3,3,3,3,3,3,3,3,3,3,3,3,3,3,3,3,3,3,3,3,3,
3,3,3,3,3,3,3,3,3,3,3,3,3,3,3,3,3,4),(74.4832427137469,74.5871328253029,
74.6909659100892,74.7947767330557,74.898600024183,75.0025371546479,75.1065406853698,
75.2107186073821,75.2473816134096,75.3515680326783,75.4555992193782,75.5595083775362,
75.663352080544,75.7671651070821,75.8709821923987,75.9749079458944,76.0788925429681,
76.1830590648215,76.2449101478462,76.3490965671148,76.453127753815,76.557036911973,
76.6608806149807,76.7646936415184,76.8685107268352,76.9724364803309,77.0764210774044,
77.1805875992577,77.2424386822828,77.3466251015514,77.4506562882513,77.5545654464092,
77.658409149417,77.7622221759551,77.866039261272,77.9699650147675,78.0739496118412,
78.1781161336946,78.2399672167194,78.3667743014798,78.4918646575237,78.5398163394183),
 .UNSPECIFIED.);
#2339=B_SPLINE_CURVE_WITH_KNOTS('',3,(#61825,#61826,#61827,#61828,#61829,
#61830,#61831,#61832,#61833,#61834,#61835,#61836,#61837,#61838,#61839,#61840,
#61841,#61842,#61843,#61844,#61845,#61846,#61847,#61848,#61849,#61850,#61851,
#61852,#61853,#61854,#61855,#61856,#61857,#61858,#61859,#61860,#61861,#61862,
#61863,#61864,#61865,#61866,#61867,#61868,#61869,#61870,#61871,#61872,#61873,
#61874,#61875,#61876,#61877,#61878,#61879,#61880,#61881,#61882,#61883,#61884,
#61885,#61886,#61887,#61888,#61889,#61890,#61891,#61892,#61893,#61894,#61895,
#61896,#61897,#61898,#61899,#61900,#61901,#61902,#61903,#61904,#61905,#61906,
#61907,#61908,#61909,#61910,#61911,#61912,#61913,#61914,#61915,#61916,#61917,
#61918,#61919,#61920,#61921,#61922,#61923,#61924,#61925,#61926,#61927,#61928,
#61929,#61930,#61931,#61932,#61933,#61934,#61935,#61936,#61937,#61938,#61939,
#61940,#61941,#61942,#61943,#61944,#61945),.UNSPECIFIED.,.F.,.F.,(4,3,3,
3,3,3,3,3,3,3,3,3,3,3,3,3,3,3,3,3,3,3,3,3,3,3,3,3,3,3,3,3,3,3,3,3,3,3,3,
3,4),(68.1995378123589,68.303348975242,68.4076883482173,68.5116448055075,
68.6161756363252,68.7207064671429,68.8248928864116,68.9289240731113,69.0328332312694,
69.1366769342771,69.2404899608151,69.3443070461318,69.4482327996275,69.5522173967011,
69.6563839185545,69.7182350015795,69.8224214208481,69.9264526075479,70.0303617657059,
70.1342054687136,70.2380184952514,70.3418355805683,70.4457613340638,70.5497459311376,
70.653912452991,70.7157635360161,70.8199499552846,70.9239811419846,71.0278903001425,
71.1317340031501,71.2355470296882,71.339364115005,71.4432898685007,71.5472744655741,
71.6514409874275,71.7132920704527,71.8208733890792,71.9298127999507,72.0369795361949,
72.1468052843801,72.2566310325652),.UNSPECIFIED.);
#2340=B_SPLINE_CURVE_WITH_KNOTS('',3,(#61946,#61947,#61948,#61949,#61950,
#61951,#61952,#61953,#61954,#61955,#61956,#61957,#61958,#61959,#61960,#61961,
#61962,#61963,#61964,#61965,#61966,#61967,#61968,#61969,#61970,#61971,#61972,
#61973,#61974,#61975,#61976,#61977,#61978,#61979,#61980,#61981,#61982,#61983,
#61984,#61985,#61986,#61987,#61988,#61989,#61990,#61991,#61992,#61993,#61994,
#61995,#61996,#61997,#61998,#61999,#62000,#62001,#62002,#62003,#62004,#62005,
#62006,#62007,#62008,#62009,#62010,#62011,#62012),.UNSPECIFIED.,.F.,.F.,
(4,3,3,3,3,3,3,3,3,3,3,3,3,3,3,3,3,3,3,3,3,3,4),(72.2566310330111,72.3701784259807,
72.4815873942032,72.5962039995462,72.7108206048893,72.8150070241579,72.9190382108579,
73.022947369016,73.1267910720237,73.2306040985618,73.3344211838786,73.4383469373742,
73.5423315344479,73.6464980563013,73.7083491393259,73.8125058091446,73.9165206688818,
74.0204287176382,74.1242648292319,74.2280916123974,74.3319123054245,74.4358068055344,
74.482061581652),.UNSPECIFIED.);
#2341=B_SPLINE_CURVE_WITH_KNOTS('',3,(#62014,#62015,#62016,#62017,#62018,
#62019,#62020,#62021,#62022,#62023,#62024,#62025,#62026,#62027,#62028,#62029,
#62030,#62031,#62032,#62033,#62034,#62035,#62036,#62037,#62038,#62039,#62040,
#62041,#62042,#62043,#62044,#62045,#62046,#62047,#62048,#62049,#62050,#62051,
#62052,#62053,#62054,#62055,#62056,#62057,#62058,#62059,#62060,#62061,#62062,
#62063,#62064,#62065,#62066,#62067,#62068,#62069,#62070,#62071,#62072,#62073,
#62074,#62075,#62076,#62077,#62078,#62079,#62080,#62081,#62082,#62083),
 .UNSPECIFIED.,.F.,.F.,(4,3,3,3,3,3,3,3,3,3,3,3,3,3,3,3,3,3,3,3,3,3,3,4),
(72.2566310325652,72.3607828828408,72.4647795326403,72.5686542861375,72.6724637223968,
72.7762426721719,72.880025922937,72.9839179050169,73.0878690474532,73.1920015684937,
73.2523245445364,73.3565109638049,73.4605421505048,73.5644513086627,73.6682950116704,
73.7721080382084,73.8759251235251,73.9798508770207,74.0838354740943,74.1880019959476,
74.249853078973,74.3540440480012,74.4580688912286,74.4832427137469),
 .UNSPECIFIED.);
#2342=B_SPLINE_CURVE_WITH_KNOTS('',3,(#62084,#62085,#62086,#62087,#62088,
#62089,#62090,#62091,#62092,#62093,#62094,#62095,#62096,#62097,#62098,#62099,
#62100,#62101,#62102,#62103,#62104,#62105,#62106,#62107,#62108,#62109,#62110,
#62111,#62112,#62113,#62114,#62115,#62116,#62117,#62118,#62119,#62120,#62121,
#62122,#62123,#62124,#62125,#62126,#62127,#62128,#62129,#62130,#62131,#62132,
#62133,#62134,#62135,#62136,#62137,#62138,#62139,#62140,#62141,#62142,#62143,
#62144,#62145,#62146,#62147,#62148,#62149,#62150,#62151,#62152,#62153,#62154,
#62155,#62156,#62157,#62158,#62159,#62160,#62161,#62162,#62163,#62164,#62165,
#62166,#62167,#62168,#62169,#62170,#62171,#62172,#62173,#62174,#62175,#62176,
#62177,#62178,#62179,#62180,#62181,#62182,#62183,#62184,#62185,#62186,#62187,
#62188,#62189,#62190,#62191,#62192,#62193,#62194,#62195,#62196,#62197,#62198,
#62199,#62200,#62201,#62202,#62203,#62204,#62205,#62206,#62207,#62208,#62209,
#62210),.UNSPECIFIED.,.F.,.F.,(4,3,3,3,3,3,3,3,3,3,3,3,3,3,3,3,3,3,3,3,
3,3,3,3,3,3,3,3,3,3,3,3,3,3,3,3,3,3,3,3,3,3,4),(68.1991393899546,68.2646818723534,
68.368868291622,68.4728994783219,68.5768086364799,68.6806523394876,68.7844653660256,
68.8882824513424,68.992208204838,69.0961928019116,69.200359323765,69.26221040679,
69.3663968260586,69.4704280127586,69.5743371709166,69.6781808739243,69.7819939004623,
69.8858109857791,69.9897367392748,70.0937213363484,70.1978878582018,70.2597389412266,
70.3639253604953,70.4679565471953,70.5718657053533,70.675709408361,70.779522434899,
70.8833395202159,70.9872652737115,71.0912498707852,71.1954163926385,71.2572674756632,
71.3614538949318,71.4654850816318,71.5693942397898,71.6732379427976,71.7770509693356,
71.8808680546524,71.9847938081481,72.0887784052216,72.192944927075,72.2547960100998,
72.256631032138),.UNSPECIFIED.);
#2343=B_SPLINE_CURVE_WITH_KNOTS('',3,(#62216,#62217,#62218,#62219,#62220,
#62221,#62222,#62223,#62224,#62225,#62226,#62227,#62228,#62229,#62230,#62231,
#62232,#62233,#62234,#62235,#62236,#62237,#62238,#62239,#62240,#62241,#62242,
#62243,#62244,#62245,#62246,#62247,#62248,#62249,#62250,#62251,#62252,#62253,
#62254,#62255,#62256,#62257,#62258,#62259,#62260,#62261,#62262,#62263,#62264,
#62265,#62266,#62267,#62268,#62269,#62270,#62271,#62272,#62273,#62274,#62275,
#62276,#62277,#62278,#62279,#62280,#62281,#62282,#62283,#62284,#62285,#62286,
#62287,#62288,#62289,#62290,#62291,#62292,#62293,#62294,#62295,#62296,#62297,
#62298,#62299,#62300,#62301,#62302,#62303,#62304,#62305,#62306,#62307,#62308,
#62309,#62310,#62311,#62312,#62313,#62314,#62315,#62316,#62317,#62318,#62319,
#62320,#62321,#62322,#62323,#62324,#62325,#62326,#62327,#62328,#62329,#62330,
#62331,#62332,#62333,#62334,#62335,#62336),.UNSPECIFIED.,.F.,.F.,(4,3,3,
3,3,3,3,3,3,3,3,3,3,3,3,3,3,3,3,3,3,3,3,3,3,3,3,3,3,3,3,3,3,3,3,3,3,3,3,
3,4),(61.916866067234,62.0208000153523,62.1246586748948,62.2284768431646,
62.332289264134,62.436204059969,62.5401688912189,62.6443249654368,62.7355352605233,
62.8397216797919,62.9437528664919,63.0476620246499,63.1515057276576,63.2553187541956,
63.3591358395125,63.4630615930081,63.5670461900817,63.6712127119351,63.7330637949599,
63.8372502142285,63.9412814009285,64.0451905590865,64.1490342620942,64.2528472886322,
64.3566643739491,64.4605901274447,64.5645747245183,64.6687412463717,64.7305923293965,
64.8347787486651,64.9388099353651,65.0427190935231,65.1465627965308,65.2503758230689,
65.3541929083857,65.4581186618813,65.5621032589549,65.6662697808083,65.7281208638331,
65.8639211020862,65.9734457249235),.UNSPECIFIED.);
#2344=B_SPLINE_CURVE_WITH_KNOTS('',3,(#62337,#62338,#62339,#62340,#62341,
#62342,#62343,#62344,#62345,#62346,#62347,#62348,#62349,#62350,#62351,#62352,
#62353,#62354,#62355,#62356,#62357,#62358,#62359,#62360,#62361,#62362,#62363,
#62364,#62365,#62366,#62367,#62368,#62369,#62370,#62371,#62372,#62373,#62374,
#62375,#62376,#62377,#62378,#62379,#62380,#62381,#62382,#62383,#62384,#62385,
#62386,#62387,#62388,#62389,#62390,#62391,#62392,#62393,#62394,#62395,#62396,
#62397,#62398,#62399,#62400,#62401,#62402,#62403,#62404,#62405,#62406),
 .UNSPECIFIED.,.F.,.F.,(4,3,3,3,3,3,3,3,3,3,3,3,3,3,3,3,3,3,3,3,3,3,3,4),
(65.9734457253856,66.0761394376291,66.1787659097615,66.2813614741682,66.3839624163265,
66.4866699517349,66.5894404069822,66.6923813783738,66.7256493982697,66.8298358175384,
66.9338670042384,67.0377761623964,67.1416198654042,67.2454328919421,67.3492499772588,
67.4531757307544,67.557160327828,67.6613268496814,67.7231779327063,67.8273675151293,
67.9313793154479,68.0352880094723,68.1391301362491,68.1995378123589),
 .UNSPECIFIED.);
#2345=B_SPLINE_CURVE_WITH_KNOTS('',3,(#62408,#62409,#62410,#62411,#62412,
#62413,#62414,#62415,#62416,#62417,#62418,#62419,#62420,#62421,#62422,#62423,
#62424,#62425,#62426,#62427,#62428,#62429,#62430,#62431,#62432,#62433,#62434,
#62435,#62436,#62437,#62438,#62439,#62440,#62441,#62442,#62443,#62444,#62445,
#62446,#62447,#62448,#62449,#62450,#62451,#62452,#62453,#62454,#62455,#62456,
#62457,#62458,#62459,#62460,#62461,#62462,#62463,#62464,#62465,#62466,#62467,
#62468,#62469,#62470,#62471,#62472,#62473,#62474),.UNSPECIFIED.,.F.,.F.,
(4,3,3,3,3,3,3,3,3,3,3,3,3,3,3,3,3,3,3,3,3,3,4),(65.973445725698,66.0988776153497,
66.226129946551,66.2696248034802,66.3738112227488,66.4778424094487,66.5817515676067,
66.6855952706144,66.7894082971523,66.8932253824693,66.9971511359649,67.1011357330385,
67.2053022548918,67.2671533379168,67.3713444216424,67.4753543191426,67.5792620015281,
67.6831023303074,67.7869100855494,67.8907809267929,67.9946786620491,68.0987368470952,
68.1991393899546),.UNSPECIFIED.);
#2346=B_SPLINE_CURVE_WITH_KNOTS('',3,(#62475,#62476,#62477,#62478,#62479,
#62480,#62481,#62482,#62483,#62484,#62485,#62486,#62487,#62488,#62489,#62490,
#62491,#62492,#62493,#62494,#62495,#62496,#62497,#62498,#62499,#62500,#62501,
#62502,#62503,#62504,#62505,#62506,#62507,#62508,#62509,#62510,#62511,#62512,
#62513,#62514,#62515,#62516,#62517,#62518,#62519,#62520,#62521,#62522,#62523,
#62524,#62525,#62526,#62527,#62528,#62529,#62530,#62531,#62532,#62533,#62534,
#62535,#62536,#62537,#62538,#62539,#62540,#62541,#62542,#62543,#62544,#62545,
#62546,#62547,#62548,#62549,#62550,#62551,#62552,#62553,#62554,#62555,#62556,
#62557,#62558,#62559,#62560,#62561,#62562,#62563,#62564,#62565,#62566,#62567,
#62568,#62569,#62570,#62571,#62572,#62573,#62574,#62575,#62576,#62577,#62578,
#62579,#62580,#62581,#62582,#62583,#62584,#62585,#62586,#62587,#62588,#62589,
#62590,#62591,#62592,#62593,#62594,#62595,#62596,#62597,#62598),
 .UNSPECIFIED.,.F.,.F.,(4,3,3,3,3,3,3,3,3,3,3,3,3,3,3,3,3,3,3,3,3,3,3,3,
3,3,3,3,3,3,3,3,3,3,3,3,3,3,3,3,3,4),(61.9158957506032,62.0198259490519,
62.1238180900071,62.2279890148855,62.2795106657338,62.3836970850024,62.4877282717021,
62.5916374298601,62.6954811328678,62.7992941594057,62.9031112447225,63.0070369982182,
63.1110215952918,63.2151881171452,63.2770392001704,63.3812256194391,63.4852568061391,
63.5891659642971,63.6930096673048,63.7968226938427,63.9006397791598,64.0045655326555,
64.1085501297291,64.2127166515826,64.274567734607,64.3787541538756,64.4827853405758,
64.5866944987338,64.6905382017415,64.7943512282798,64.8981683135967,65.0020940670924,
65.1060786641661,65.2102451860196,65.2720962690436,65.3756018854378,65.4789620265338,
65.5822125841125,65.6854054642092,65.7885610860738,65.8917634870123,65.9734457253856),
 .UNSPECIFIED.);
#2347=B_SPLINE_CURVE_WITH_KNOTS('',3,(#62604,#62605,#62606,#62607,#62608,
#62609,#62610,#62611,#62612,#62613,#62614,#62615,#62616,#62617,#62618,#62619,
#62620,#62621,#62622,#62623,#62624,#62625,#62626,#62627,#62628,#62629,#62630,
#62631,#62632,#62633,#62634,#62635,#62636,#62637,#62638,#62639,#62640,#62641,
#62642,#62643,#62644,#62645,#62646,#62647,#62648,#62649,#62650,#62651,#62652,
#62653,#62654,#62655,#62656,#62657,#62658,#62659,#62660,#62661,#62662,#62663,
#62664,#62665,#62666,#62667,#62668,#62669,#62670,#62671,#62672,#62673,#62674,
#62675,#62676,#62677,#62678,#62679,#62680,#62681,#62682,#62683,#62684,#62685,
#62686,#62687,#62688,#62689,#62690,#62691,#62692,#62693,#62694,#62695,#62696,
#62697,#62698,#62699,#62700,#62701,#62702,#62703,#62704,#62705,#62706,#62707,
#62708,#62709,#62710,#62711,#62712,#62713,#62714,#62715,#62716,#62717,#62718,
#62719,#62720,#62721,#62722,#62723,#62724,#62725,#62726,#62727,#62728,#62729,
#62730),.UNSPECIFIED.,.F.,.F.,(4,3,3,3,3,3,3,3,3,3,3,3,3,3,3,3,3,3,3,3,
3,3,3,3,3,3,3,3,3,3,3,3,3,3,3,3,3,3,3,3,3,3,4),(55.6326012668771,55.7367901940337,
55.7528355194671,55.8570219387357,55.9610531254356,56.0649622835936,56.1688059866013,
56.2726190131393,56.3764360984561,56.4803618519517,56.5843464490253,56.6885129708787,
56.7503640539037,56.8545504731724,56.9585816598724,57.0624908180304,57.1663345210382,
57.2701475475762,57.3739646328931,57.4778903863887,57.5818749834624,57.6860415053158,
57.7478925883403,57.8520790076089,57.9561101943089,58.0600193524668,58.1638630554745,
58.2676760820125,58.3714931673293,58.4754189208249,58.5794035178985,58.6835700397519,
58.7454211227769,58.8487780338705,58.95396333187,59.0570447634803,59.160064366593,
59.2630580262836,59.3698586241792,59.4729706208884,59.5761501528113,59.679489744252,
59.6902604178662),.UNSPECIFIED.);
#2348=B_SPLINE_CURVE_WITH_KNOTS('',3,(#62731,#62732,#62733,#62734,#62735,
#62736,#62737,#62738,#62739,#62740,#62741,#62742,#62743,#62744,#62745,#62746,
#62747,#62748,#62749,#62750,#62751,#62752,#62753,#62754,#62755,#62756,#62757,
#62758,#62759,#62760,#62761,#62762,#62763,#62764,#62765,#62766,#62767,#62768,
#62769,#62770,#62771,#62772,#62773,#62774,#62775,#62776,#62777,#62778,#62779,
#62780,#62781,#62782,#62783,#62784,#62785,#62786,#62787,#62788,#62789,#62790,
#62791,#62792,#62793,#62794,#62795,#62796,#62797,#62798,#62799,#62800),
 .UNSPECIFIED.,.F.,.F.,(4,3,3,3,3,3,3,3,3,3,3,3,3,3,3,3,3,3,3,3,3,3,3,4),
(59.690260418206,59.7429496572135,59.8471360764822,59.9511672631822,60.0550764213402,
60.1589201243479,60.2627331508859,60.3665502362028,60.4704759896984,60.574460586772,
60.6786271086254,60.7404781916501,60.8446646109187,60.9486957976186,61.0526049557766,
61.1564486587843,61.2602616853224,61.3640787706392,61.4680045241348,61.5719891212084,
61.6761556430618,61.7380067260867,61.8421682999702,61.916866067234),
 .UNSPECIFIED.);
#2349=B_SPLINE_CURVE_WITH_KNOTS('',3,(#62802,#62803,#62804,#62805,#62806,
#62807,#62808,#62809,#62810,#62811,#62812,#62813,#62814,#62815,#62816,#62817,
#62818,#62819,#62820,#62821,#62822,#62823,#62824,#62825,#62826,#62827,#62828,
#62829,#62830,#62831,#62832,#62833,#62834,#62835,#62836,#62837,#62838,#62839,
#62840,#62841,#62842,#62843,#62844,#62845,#62846,#62847,#62848,#62849,#62850,
#62851,#62852,#62853,#62854,#62855,#62856,#62857,#62858,#62859,#62860,#62861,
#62862,#62863,#62864,#62865,#62866,#62867,#62868),.UNSPECIFIED.,.F.,.F.,
(4,3,3,3,3,3,3,3,3,3,3,3,3,3,3,3,3,3,3,3,3,3,4),(59.690260418206,59.7955870148004,
59.900955252961,60.0064809160437,60.1120913042759,60.2179183210518,60.2844535968606,
60.3886400161293,60.4926712028292,60.5965803609872,60.7004240639949,60.804237090533,
60.9080541758499,61.0119799293455,61.115964526419,61.2201310482724,61.2819821312972,
61.3861518308917,61.4901756511522,61.5966056760149,61.7004458108553,61.8081707807292,
61.9158957506032),.UNSPECIFIED.);
#2350=B_SPLINE_CURVE_WITH_KNOTS('',3,(#62869,#62870,#62871,#62872,#62873,
#62874,#62875,#62876,#62877,#62878,#62879,#62880,#62881,#62882,#62883,#62884,
#62885,#62886,#62887,#62888,#62889,#62890,#62891,#62892,#62893,#62894,#62895,
#62896,#62897,#62898,#62899,#62900,#62901,#62902,#62903,#62904,#62905,#62906,
#62907,#62908,#62909,#62910,#62911,#62912,#62913,#62914,#62915,#62916,#62917,
#62918,#62919,#62920,#62921,#62922,#62923,#62924,#62925,#62926,#62927,#62928,
#62929,#62930,#62931,#62932,#62933,#62934,#62935,#62936,#62937,#62938,#62939,
#62940,#62941,#62942,#62943,#62944,#62945,#62946,#62947,#62948,#62949,#62950,
#62951,#62952,#62953,#62954,#62955,#62956,#62957,#62958,#62959,#62960,#62961,
#62962,#62963,#62964,#62965,#62966,#62967,#62968,#62969,#62970,#62971,#62972,
#62973,#62974,#62975,#62976,#62977,#62978,#62979,#62980,#62981,#62982,#62983,
#62984,#62985,#62986,#62987,#62988,#62989,#62990,#62991,#62992),
 .UNSPECIFIED.,.F.,.F.,(4,3,3,3,3,3,3,3,3,3,3,3,3,3,3,3,3,3,3,3,3,3,3,3,
3,3,3,3,3,3,3,3,3,3,3,3,3,3,3,3,3,4),(55.6335465335838,55.7373798265119,
55.841190675596,55.9450138109094,56.0489506758914,56.1529537776165,56.2571314291437,
56.2943394591142,56.3985258783828,56.5025570650831,56.606466223241,56.7103099262487,
56.8141229527868,56.9179400381039,57.0218657915995,57.1258503886731,57.2300169105264,
57.2918679935508,57.3960544128195,57.5000855995193,57.6039947576773,57.7078384606851,
57.8116514872232,57.9154685725402,58.0193943260358,58.1233789231093,58.2275454449626,
58.2893965279874,58.3935829472562,58.4976141339562,58.6015232921141,58.7053669951219,
58.80918002166,58.9129971069773,59.0169228604729,59.1209074575463,59.2250739793998,
59.286925062424,59.4023023747485,59.517314278657,59.6317214277123,59.6902604178031),
 .UNSPECIFIED.);
#2351=B_SPLINE_CURVE_WITH_KNOTS('',3,(#62998,#62999,#63000,#63001,#63002,
#63003,#63004,#63005,#63006,#63007,#63008,#63009,#63010,#63011,#63012,#63013,
#63014,#63015,#63016,#63017,#63018,#63019,#63020,#63021,#63022,#63023,#63024,
#63025,#63026,#63027,#63028,#63029,#63030,#63031,#63032,#63033,#63034,#63035,
#63036,#63037,#63038,#63039,#63040,#63041,#63042,#63043,#63044,#63045,#63046,
#63047,#63048,#63049,#63050,#63051,#63052,#63053,#63054,#63055,#63056,#63057,
#63058,#63059,#63060,#63061,#63062,#63063,#63064,#63065,#63066,#63067,#63068,
#63069,#63070,#63071,#63072,#63073,#63074,#63075,#63076,#63077,#63078,#63079,
#63080,#63081,#63082,#63083,#63084,#63085,#63086,#63087,#63088,#63089,#63090,
#63091,#63092,#63093,#63094,#63095,#63096,#63097,#63098,#63099,#63100,#63101,
#63102,#63103,#63104,#63105,#63106,#63107,#63108,#63109,#63110,#63111,#63112,
#63113,#63114,#63115,#63116,#63117,#63118,#63119,#63120,#63121),
 .UNSPECIFIED.,.F.,.F.,(4,3,3,3,3,3,3,3,3,3,3,3,3,3,3,3,3,3,3,3,3,3,3,3,
3,3,3,3,3,3,3,3,3,3,3,3,3,3,3,3,3,4),(49.3496692790113,49.4541680374703,
49.5581242119948,49.6628942624211,49.7676643128475,49.8718507321162,49.975881918816,
50.079791076974,50.1836347799817,50.2874478065198,50.3912648918367,50.4951906453324,
50.5991752424061,50.7033417642595,50.7651928472842,50.8693792665528,50.9734104532528,
51.0773196114108,51.1811633144184,51.2849763409564,51.3887934262732,51.4927191797688,
51.5967037768424,51.7008702986958,51.7627213817208,51.8669078009894,51.9709389876895,
52.0748481458475,52.1786918488552,52.2825048753932,52.3863219607103,52.4902477142059,
52.5942323112796,52.6983988331331,52.7602499161573,52.8647413337414,52.9690770723351,
53.0785765820079,53.1827008676145,53.2867777522309,53.39085559745,53.4070751110264),
 .UNSPECIFIED.);
#2352=B_SPLINE_CURVE_WITH_KNOTS('',3,(#63122,#63123,#63124,#63125,#63126,
#63127,#63128,#63129,#63130,#63131,#63132,#63133,#63134,#63135,#63136,#63137,
#63138,#63139,#63140,#63141,#63142,#63143,#63144,#63145,#63146,#63147,#63148,
#63149,#63150,#63151,#63152,#63153,#63154,#63155,#63156,#63157,#63158,#63159,
#63160,#63161,#63162,#63163,#63164,#63165,#63166,#63167,#63168,#63169,#63170,
#63171,#63172,#63173,#63174,#63175,#63176,#63177,#63178,#63179,#63180,#63181,
#63182,#63183,#63184,#63185,#63186,#63187,#63188),.UNSPECIFIED.,.F.,.F.,
(4,3,3,3,3,3,3,3,3,3,3,3,3,3,3,3,3,3,3,3,3,3,4),(53.4070751114695,53.5260746317928,
53.646159585465,53.7577784505939,53.8619648698625,53.9659960565624,54.0699052147203,
54.173748917728,54.277561944266,54.3813790295827,54.4853047830783,54.5892893801519,
54.6934559020053,54.7553069850305,54.8649687702613,54.9689734123707,55.0728760912958,
55.1767116670854,55.2805149180024,55.3843665183207,55.4882460132565,55.592246094713,
55.6326012668771),.UNSPECIFIED.);
#2353=B_SPLINE_CURVE_WITH_KNOTS('',3,(#63190,#63191,#63192,#63193,#63194,
#63195,#63196,#63197,#63198,#63199,#63200,#63201,#63202,#63203,#63204,#63205,
#63206,#63207,#63208,#63209,#63210,#63211,#63212,#63213,#63214,#63215,#63216,
#63217,#63218,#63219,#63220,#63221,#63222,#63223,#63224,#63225,#63226,#63227,
#63228,#63229,#63230,#63231,#63232,#63233,#63234,#63235,#63236,#63237,#63238,
#63239,#63240,#63241,#63242,#63243,#63244,#63245,#63246,#63247,#63248,#63249,
#63250,#63251,#63252,#63253,#63254,#63255,#63256,#63257,#63258,#63259),
 .UNSPECIFIED.,.F.,.F.,(4,3,3,3,3,3,3,3,3,3,3,3,3,3,3,3,3,3,3,3,3,3,3,4),
(53.407075111485,53.5098558320716,53.6124863111895,53.7150344153237,53.8175366234483,
53.9200293486254,54.0226180274753,54.1252565130567,54.2280753277761,54.299282390241,
54.4034688095096,54.5074999962097,54.6114091543677,54.7152528573754,54.8190658839134,
54.9228829692301,55.0268087227257,55.1307933197994,55.2349598416528,55.2968109246776,
55.4009764972008,55.505005936927,55.6089152722148,55.6335465335838),
 .UNSPECIFIED.);
#2354=B_SPLINE_CURVE_WITH_KNOTS('',3,(#63260,#63261,#63262,#63263,#63264,
#63265,#63266,#63267,#63268,#63269,#63270,#63271,#63272,#63273,#63274,#63275,
#63276,#63277,#63278,#63279,#63280,#63281,#63282,#63283,#63284,#63285,#63286,
#63287,#63288,#63289,#63290,#63291,#63292,#63293,#63294,#63295,#63296,#63297,
#63298,#63299,#63300,#63301,#63302,#63303,#63304,#63305,#63306,#63307,#63308,
#63309,#63310,#63311,#63312,#63313,#63314,#63315,#63316,#63317,#63318,#63319,
#63320,#63321,#63322,#63323,#63324,#63325,#63326,#63327,#63328,#63329,#63330,
#63331,#63332,#63333,#63334,#63335,#63336,#63337,#63338,#63339,#63340,#63341,
#63342,#63343,#63344,#63345,#63346,#63347,#63348,#63349,#63350,#63351,#63352,
#63353,#63354,#63355,#63356,#63357,#63358,#63359,#63360,#63361,#63362,#63363,
#63364,#63365,#63366,#63367,#63368,#63369,#63370,#63371,#63372,#63373,#63374,
#63375,#63376,#63377,#63378,#63379,#63380,#63381,#63382,#63383),
 .UNSPECIFIED.,.F.,.F.,(4,3,3,3,3,3,3,3,3,3,3,3,3,3,3,3,3,3,3,3,3,3,3,3,
3,3,3,3,3,3,3,3,3,3,3,3,3,3,3,3,3,4),(49.350124038248,49.4542486334836,
49.56111358586,49.6649925950448,49.7688199617351,49.8726304431839,49.9817648955116,
50.0857131347655,50.1897342001324,50.2939235850304,50.3091682524946,50.4133546717632,
50.5173858584632,50.6212950166212,50.725138719629,50.828951746167,50.9327688314839,
51.0366945849795,51.1406791820532,51.2448457039066,51.3066967869312,51.4108832061998,
51.5149143928998,51.6188235510578,51.7226672540655,51.8264802806035,51.9302973659203,
52.0342231194159,52.1382077164896,52.2423742383429,52.3042253213678,52.4084117406365,
52.5124429273365,52.6163520854945,52.7201957885023,52.8240088150403,52.9278259003573,
53.0317516538529,53.1357362509266,53.23990277278,53.3017538558044,53.4070751110264),
 .UNSPECIFIED.);
#2355=B_SPLINE_CURVE_WITH_KNOTS('',3,(#63389,#63390,#63391,#63392,#63393,
#63394,#63395,#63396,#63397,#63398,#63399,#63400,#63401,#63402,#63403,#63404,
#63405,#63406,#63407,#63408,#63409,#63410,#63411,#63412,#63413,#63414,#63415,
#63416,#63417,#63418,#63419,#63420,#63421,#63422,#63423,#63424,#63425,#63426,
#63427,#63428,#63429,#63430,#63431,#63432,#63433,#63434,#63435,#63436,#63437,
#63438,#63439,#63440,#63441,#63442,#63443,#63444,#63445,#63446,#63447,#63448,
#63449,#63450,#63451,#63452,#63453,#63454,#63455,#63456,#63457,#63458,#63459,
#63460,#63461,#63462,#63463,#63464,#63465,#63466,#63467,#63468,#63469,#63470,
#63471,#63472,#63473,#63474,#63475,#63476,#63477,#63478,#63479,#63480,#63481,
#63482,#63483,#63484,#63485,#63486,#63487,#63488,#63489,#63490,#63491,#63492,
#63493,#63494,#63495,#63496,#63497,#63498,#63499,#63500,#63501,#63502,#63503,
#63504,#63505,#63506,#63507,#63508,#63509),.UNSPECIFIED.,.F.,.F.,(4,3,3,
3,3,3,3,3,3,3,3,3,3,3,3,3,3,3,3,3,3,3,3,3,3,3,3,3,3,3,3,3,3,3,3,3,3,3,3,
3,4),(43.0672711160795,43.171130047172,43.2749483241126,43.3787606910417,
43.4826753260211,43.5866398502954,43.6907957769975,43.782493106228,43.8866795254969,
43.9907107121971,44.0946198703554,44.1984635733632,44.3022765999014,44.4060936852183,
44.5100194387141,44.614004035788,44.7181705576416,44.7800216406646,44.8842080599332,
44.9882392466327,45.0921484047906,45.1959921077983,45.299805134336,45.4036222196529,
45.5075479731484,45.6115325702219,45.7156990920752,45.7775501751012,45.8817365943696,
45.9857677810696,46.0896769392276,46.1935206422352,46.2973336687731,46.4011507540897,
46.5050765075852,46.6090611046589,46.7132276265123,46.7750787095378,46.8955468165434,
47.0149579004648,47.1238898034052),.UNSPECIFIED.);
#2356=B_SPLINE_CURVE_WITH_KNOTS('',3,(#63510,#63511,#63512,#63513,#63514,
#63515,#63516,#63517,#63518,#63519,#63520,#63521,#63522,#63523,#63524,#63525,
#63526,#63527,#63528,#63529,#63530,#63531,#63532,#63533,#63534,#63535,#63536,
#63537,#63538,#63539,#63540,#63541,#63542,#63543,#63544,#63545,#63546,#63547,
#63548,#63549,#63550,#63551,#63552,#63553,#63554,#63555,#63556,#63557,#63558,
#63559,#63560,#63561,#63562,#63563,#63564,#63565,#63566,#63567,#63568,#63569,
#63570,#63571,#63572,#63573,#63574,#63575,#63576,#63577,#63578,#63579),
 .UNSPECIFIED.,.F.,.F.,(4,3,3,3,3,3,3,3,3,3,3,3,3,3,3,3,3,3,3,3,3,3,3,4),
(47.1238898038468,47.2279417400956,47.3319880830487,47.4360629830603,47.5402700680329,
47.6445565808272,47.749025499834,47.7726072439743,47.8767936632429,47.9808248499428,
48.0847340081008,48.1885777111084,48.2923907376463,48.396207822963,48.5001335764586,
48.6041181735321,48.7082846953855,48.7701357784109,48.8743117183295,48.9783401946021,
49.0822482051315,49.1860855662751,49.2899055677676,49.3496692790113),
 .UNSPECIFIED.);
#2357=B_SPLINE_CURVE_WITH_KNOTS('',3,(#63581,#63582,#63583,#63584,#63585,
#63586,#63587,#63588,#63589,#63590,#63591,#63592,#63593,#63594,#63595,#63596,
#63597,#63598,#63599,#63600,#63601,#63602,#63603,#63604,#63605,#63606,#63607,
#63608,#63609,#63610,#63611,#63612,#63613,#63614,#63615,#63616,#63617,#63618,
#63619,#63620,#63621,#63622,#63623,#63624,#63625,#63626,#63627,#63628,#63629,
#63630,#63631,#63632,#63633,#63634,#63635,#63636,#63637,#63638,#63639,#63640,
#63641,#63642,#63643,#63644,#63645,#63646,#63647,#63648,#63649,#63650),
 .UNSPECIFIED.,.F.,.F.,(4,3,3,3,3,3,3,3,3,3,3,3,3,3,3,3,3,3,3,3,3,3,3,4),
(47.1238898038468,47.2757519674211,47.3165826491848,47.4207690684534,47.5248002551535,
47.6287094133114,47.7325531163191,47.8363661428571,47.9401832281739,48.0441089816695,
48.1480935787431,48.2522601005964,48.3141111836214,48.41829760289,48.52232878959,
48.626237947748,48.7300816507557,48.8338946772937,48.9377117626105,49.0416375161061,
49.1456221131797,49.249788635033,49.311639718058,49.350124038248),
 .UNSPECIFIED.);
#2358=B_SPLINE_CURVE_WITH_KNOTS('',3,(#63651,#63652,#63653,#63654,#63655,
#63656,#63657,#63658,#63659,#63660,#63661,#63662,#63663,#63664,#63665,#63666,
#63667,#63668,#63669,#63670,#63671,#63672,#63673,#63674,#63675,#63676,#63677,
#63678,#63679,#63680,#63681,#63682,#63683,#63684,#63685,#63686,#63687,#63688,
#63689,#63690,#63691,#63692,#63693,#63694,#63695,#63696,#63697,#63698,#63699,
#63700,#63701,#63702,#63703,#63704,#63705,#63706,#63707,#63708,#63709,#63710,
#63711,#63712,#63713,#63714,#63715,#63716,#63717,#63718,#63719,#63720,#63721,
#63722,#63723,#63724,#63725,#63726,#63727,#63728,#63729,#63730,#63731,#63732,
#63733,#63734,#63735,#63736,#63737,#63738,#63739,#63740,#63741,#63742,#63743,
#63744,#63745,#63746,#63747,#63748,#63749,#63750,#63751,#63752,#63753,#63754,
#63755,#63756,#63757,#63758,#63759,#63760,#63761,#63762,#63763,#63764,#63765,
#63766,#63767,#63768,#63769,#63770,#63771,#63772,#63773,#63774),
 .UNSPECIFIED.,.F.,.F.,(4,3,3,3,3,3,3,3,3,3,3,3,3,3,3,3,3,3,3,3,3,3,3,3,
3,3,3,3,3,3,3,3,3,3,3,3,3,3,3,3,3,4),(43.0661580857027,43.1701497603984,
43.2743204074643,43.3264685114384,43.4306549307087,43.5346861174104,43.6385952755701,
43.7424389785796,43.8462520051194,43.950069090438,44.0539948439354,44.1579794410109,
44.262145962866,44.323997045875,44.4281834651433,44.5322146518429,44.6361238100006,
44.7399675130079,44.8437805395456,44.9475976248621,45.0515233783574,45.1555079754306,
45.2596744972837,45.3215255803116,45.42571199958,45.5297431862797,45.6336523444374,
45.7374960474449,45.8413090739826,45.9451261592993,46.0490519127946,46.153036509868,
46.2572030317211,46.3190541147482,46.4216814718161,46.5241724459798,46.6265638875465,
46.728892502623,46.831240038188,46.9335916782507,47.0360639088855,47.1238898034172),
 .UNSPECIFIED.);
#2359=B_SPLINE_CURVE_WITH_KNOTS('',3,(#63780,#63781,#63782,#63783,#63784,
#63785,#63786,#63787,#63788,#63789,#63790,#63791,#63792,#63793,#63794,#63795,
#63796,#63797,#63798,#63799,#63800,#63801,#63802,#63803,#63804,#63805,#63806,
#63807,#63808,#63809,#63810,#63811,#63812,#63813,#63814,#63815,#63816,#63817,
#63818,#63819,#63820,#63821,#63822,#63823,#63824,#63825,#63826,#63827,#63828,
#63829,#63830,#63831,#63832,#63833,#63834,#63835,#63836,#63837,#63838,#63839,
#63840,#63841,#63842,#63843,#63844,#63845,#63846,#63847,#63848,#63849,#63850,
#63851,#63852,#63853,#63854,#63855,#63856,#63857,#63858,#63859,#63860,#63861,
#63862,#63863,#63864,#63865,#63866,#63867,#63868,#63869,#63870,#63871,#63872,
#63873,#63874,#63875,#63876,#63877,#63878,#63879,#63880,#63881,#63882,#63883,
#63884,#63885,#63886,#63887,#63888,#63889,#63890,#63891,#63892,#63893,#63894,
#63895,#63896,#63897,#63898,#63899,#63900,#63901,#63902,#63903,#63904,#63905,
#63906),.UNSPECIFIED.,.F.,.F.,(4,3,3,3,3,3,3,3,3,3,3,3,3,3,3,3,3,3,3,3,
3,3,3,3,3,3,3,3,3,3,3,3,3,3,3,3,3,3,3,3,3,3,4),(36.78344581208,36.7997933651718,
36.9039797844176,37.0080109710943,37.1119201292284,37.2157638322118,37.3195768587253,
37.4233939440173,37.5273196974879,37.6313042945363,37.7354708163644,37.7973218996084,
37.9015083188911,38.0055395056052,38.1094486637777,38.2132923668,38.3171053933527,
38.4209224786844,38.5248482321949,38.6288328292834,38.7329993511516,38.794850434045,
38.8990368533117,39.0030680400096,39.1069771981657,39.2108209011714,39.3146339277075,
39.4184510130225,39.5223767665163,39.626361363588,39.7305278854396,39.7923789684816,
39.8965653877479,40.0005965744455,40.1045057326011,40.2083494356064,40.3121624621419,
40.4159795474563,40.5199053009494,40.6238898980205,40.7280564198712,40.7899075029182,
40.8407044966672),.UNSPECIFIED.);
#2360=B_SPLINE_CURVE_WITH_KNOTS('',3,(#63907,#63908,#63909,#63910,#63911,
#63912,#63913,#63914,#63915,#63916,#63917,#63918,#63919,#63920,#63921,#63922,
#63923,#63924,#63925,#63926,#63927,#63928,#63929,#63930,#63931,#63932,#63933,
#63934,#63935,#63936,#63937,#63938,#63939,#63940,#63941,#63942,#63943,#63944,
#63945,#63946,#63947,#63948,#63949,#63950,#63951,#63952,#63953,#63954,#63955,
#63956,#63957,#63958,#63959,#63960,#63961,#63962,#63963,#63964,#63965,#63966,
#63967,#63968,#63969,#63970,#63971,#63972,#63973,#63974,#63975,#63976),
 .UNSPECIFIED.,.F.,.F.,(4,3,3,3,3,3,3,3,3,3,3,3,3,3,3,3,3,3,3,3,3,3,3,4),
(40.8407044970057,40.9440672893056,41.0494883828117,41.152586115044,41.2556259852181,
41.3586438439567,41.4658418923063,41.5689883265361,41.672205701304,41.7755885097155,
41.7874360373548,41.8916224566231,41.9956536433224,42.09956280148,42.2034065044874,
42.3072195310251,42.4110366163415,42.5149623698368,42.61894696691,42.723113488763,
42.7849645717913,42.889142338587,42.993155286009,43.0672711160795),
 .UNSPECIFIED.);
#2361=B_SPLINE_CURVE_WITH_KNOTS('',3,(#63978,#63979,#63980,#63981,#63982,
#63983,#63984,#63985,#63986,#63987,#63988,#63989,#63990,#63991,#63992,#63993,
#63994,#63995,#63996,#63997,#63998,#63999,#64000,#64001,#64002,#64003,#64004,
#64005,#64006,#64007,#64008,#64009,#64010,#64011,#64012,#64013,#64014,#64015,
#64016,#64017,#64018,#64019,#64020,#64021,#64022,#64023,#64024,#64025,#64026,
#64027,#64028,#64029,#64030,#64031,#64032,#64033,#64034,#64035,#64036,#64037,
#64038,#64039,#64040,#64041,#64042,#64043,#64044),.UNSPECIFIED.,.F.,.F.,
(4,3,3,3,3,3,3,3,3,3,3,3,3,3,3,3,3,3,3,3,3,3,4),(40.8407044970049,40.9498036597885,
41.059225021957,41.1688181464335,41.2787131705263,41.3314114425652,41.4355978618318,
41.5396290485299,41.6435382066859,41.7473819096916,41.8511949362276,41.9550120215426,
42.0589377750363,42.162922372108,42.2670888939596,42.3289399770018,42.4330996296936,
42.537116410545,42.6410253236269,42.7473085141458,42.8511267993879,42.9586424425453,
43.0661580857027),.UNSPECIFIED.);
#2362=B_SPLINE_CURVE_WITH_KNOTS('',3,(#64045,#64046,#64047,#64048,#64049,
#64050,#64051,#64052,#64053,#64054,#64055,#64056,#64057,#64058,#64059,#64060,
#64061,#64062,#64063,#64064,#64065,#64066,#64067,#64068,#64069,#64070,#64071,
#64072,#64073,#64074,#64075,#64076,#64077,#64078,#64079,#64080,#64081,#64082,
#64083,#64084,#64085,#64086,#64087,#64088,#64089,#64090,#64091,#64092,#64093,
#64094,#64095,#64096,#64097,#64098,#64099,#64100,#64101,#64102,#64103,#64104,
#64105,#64106,#64107,#64108,#64109,#64110,#64111,#64112,#64113,#64114,#64115,
#64116,#64117,#64118,#64119,#64120,#64121,#64122,#64123,#64124,#64125,#64126,
#64127,#64128,#64129,#64130,#64131,#64132,#64133,#64134,#64135,#64136,#64137,
#64138,#64139,#64140,#64141,#64142,#64143,#64144,#64145,#64146,#64147,#64148,
#64149,#64150,#64151,#64152,#64153,#64154,#64155,#64156,#64157,#64158,#64159,
#64160,#64161,#64162,#64163,#64164,#64165,#64166,#64167,#64168),
 .UNSPECIFIED.,.F.,.F.,(4,3,3,3,3,3,3,3,3,3,3,3,3,3,3,3,3,3,3,3,3,3,3,3,
3,3,3,3,3,3,3,3,3,3,3,3,3,3,3,3,3,4),(36.7837215602892,36.8875324398736,
36.9913553996099,37.0952919646733,37.1992945812679,37.3034719274497,37.3412973048188,
37.4454837242011,37.5495149110163,37.6534240692914,37.7572677724171,37.861080799074,
37.9648978845105,38.068823638126,38.1728082353197,38.2769747572924,38.3388258392554,
38.443012258516,38.5470434452082,38.6509526033586,38.7547963063589,38.8586093328897,
38.9624264181996,39.0663521716886,39.170336768756,39.2745032906034,39.336354373692,
39.4405407929378,39.5445719796144,39.6484811377484,39.7523248407317,39.8561378672449,
39.9599549525368,40.0638807060072,40.1678653030555,40.2720318248834,40.3338829081286,
40.4430298277098,40.5518710894771,40.6605292198773,40.7689635848472,40.8407044966672),
 .UNSPECIFIED.);
#2363=B_SPLINE_CURVE_WITH_KNOTS('',3,(#64174,#64175,#64176,#64177,#64178,
#64179,#64180,#64181,#64182,#64183,#64184,#64185,#64186,#64187,#64188,#64189,
#64190,#64191,#64192,#64193,#64194,#64195,#64196,#64197,#64198,#64199,#64200,
#64201,#64202,#64203,#64204,#64205,#64206,#64207,#64208,#64209,#64210,#64211,
#64212,#64213,#64214,#64215,#64216,#64217,#64218,#64219,#64220,#64221,#64222,
#64223,#64224,#64225,#64226,#64227,#64228,#64229,#64230,#64231,#64232,#64233,
#64234,#64235,#64236,#64237,#64238,#64239,#64240,#64241,#64242,#64243,#64244,
#64245,#64246,#64247,#64248,#64249,#64250,#64251,#64252,#64253,#64254,#64255,
#64256,#64257,#64258,#64259,#64260,#64261,#64262,#64263,#64264,#64265,#64266,
#64267,#64268,#64269,#64270,#64271,#64272,#64273,#64274,#64275,#64276,#64277,
#64278,#64279,#64280,#64281,#64282,#64283,#64284,#64285,#64286,#64287,#64288,
#64289,#64290,#64291,#64292,#64293,#64294,#64295,#64296,#64297),
 .UNSPECIFIED.,.F.,.F.,(4,3,3,3,3,3,3,3,3,3,3,3,3,3,3,3,3,3,3,3,3,3,3,3,
3,3,3,3,3,3,3,3,3,3,3,3,3,3,3,3,3,4),(30.4998648058973,30.6038202387868,
30.7092211986695,30.8146221585522,30.9188085758045,31.0228397604511,31.1267489165103,
31.2305926173923,31.3344056417809,31.438222724928,31.5421484762373,31.6461330711119,
31.7502995907701,31.8121506929888,31.9163371131478,32.0203683007497,32.1242774598222,
32.2281211637518,32.3319341912178,32.4357512774668,32.5396770318953,32.6436616299036,
32.7478281526841,32.8096792274254,32.9138656467037,33.0178968334161,33.1218059915907,
33.2256496946177,33.3294627211775,33.4332798065179,33.5372055600414,33.6411901571448,
33.7453566790312,33.807207761862,33.9101447146387,34.0129417465494,34.1156354071316,
34.2182621038502,34.3208882127981,34.4235151981878,34.5262219085223,34.5575191894877),
 .UNSPECIFIED.);
#2364=B_SPLINE_CURVE_WITH_KNOTS('',3,(#64298,#64299,#64300,#64301,#64302,
#64303,#64304,#64305,#64306,#64307,#64308,#64309,#64310,#64311,#64312,#64313,
#64314,#64315,#64316,#64317,#64318,#64319,#64320,#64321,#64322,#64323,#64324,
#64325,#64326,#64327,#64328,#64329,#64330,#64331,#64332,#64333,#64334,#64335,
#64336,#64337,#64338,#64339,#64340,#64341,#64342,#64343,#64344,#64345,#64346,
#64347,#64348,#64349,#64350,#64351,#64352,#64353,#64354,#64355,#64356,#64357,
#64358,#64359,#64360,#64361,#64362,#64363,#64364),.UNSPECIFIED.,.F.,.F.,
(4,3,3,3,3,3,3,3,3,3,3,3,3,3,3,3,3,3,3,3,3,3,4),(34.5575191897626,34.6928922558157,
34.8047362962986,34.9089227156805,35.0129539024955,35.1168630607702,35.2207067638956,
35.3245197905522,35.4283368759883,35.5322626296034,35.6362472267968,35.7404137487692,
35.8022648307352,35.9064523911116,36.0104843860351,36.1143930817558,36.2182358509204,
36.3220474724968,36.4258626813829,36.5297810858963,36.6337581406846,36.7379046401028,
36.78344581208),.UNSPECIFIED.);
#2365=B_SPLINE_CURVE_WITH_KNOTS('',3,(#64366,#64367,#64368,#64369,#64370,
#64371,#64372,#64373,#64374,#64375,#64376,#64377,#64378,#64379,#64380,#64381,
#64382,#64383,#64384,#64385,#64386,#64387,#64388,#64389,#64390,#64391,#64392,
#64393,#64394,#64395,#64396,#64397,#64398,#64399,#64400,#64401,#64402,#64403,
#64404,#64405,#64406,#64407,#64408,#64409,#64410,#64411,#64412,#64413,#64414,
#64415,#64416,#64417,#64418,#64419,#64420,#64421,#64422,#64423,#64424,#64425,
#64426,#64427,#64428,#64429,#64430,#64431,#64432,#64433,#64434,#64435),
 .UNSPECIFIED.,.F.,.F.,(4,3,3,3,3,3,3,3,3,3,3,3,3,3,3,3,3,3,3,3,3,3,3,4),
(34.5575191897576,34.6600276231159,34.7624524447675,34.8648302599766,34.9671976054275,
35.0696598596247,35.1721712597452,35.2748625288751,35.3462402359456,35.4504266552239,
35.5544578419364,35.658367000111,35.7622107031378,35.8660237296973,35.9698408150383,
36.0737665685617,36.1777511656652,36.2819176875515,36.3437687703822,36.4479637300609,
36.5519784470328,36.6558896321121,36.7597264522879,36.7837215602892),
 .UNSPECIFIED.);
#2366=B_SPLINE_CURVE_WITH_KNOTS('',3,(#64436,#64437,#64438,#64439,#64440,
#64441,#64442,#64443,#64444,#64445,#64446,#64447,#64448,#64449,#64450,#64451,
#64452,#64453,#64454,#64455,#64456,#64457,#64458,#64459,#64460,#64461,#64462,
#64463,#64464,#64465,#64466,#64467,#64468,#64469,#64470,#64471,#64472,#64473,
#64474,#64475,#64476,#64477,#64478,#64479,#64480,#64481,#64482,#64483,#64484,
#64485,#64486,#64487,#64488,#64489,#64490,#64491,#64492,#64493,#64494,#64495,
#64496,#64497,#64498,#64499,#64500,#64501,#64502,#64503,#64504,#64505,#64506,
#64507,#64508,#64509,#64510,#64511,#64512,#64513,#64514,#64515,#64516,#64517,
#64518,#64519,#64520,#64521,#64522,#64523,#64524,#64525,#64526,#64527,#64528,
#64529,#64530,#64531,#64532,#64533,#64534,#64535,#64536,#64537,#64538,#64539,
#64540,#64541,#64542,#64543,#64544,#64545,#64546,#64547,#64548,#64549,#64550,
#64551,#64552,#64553,#64554,#64555,#64556,#64557,#64558,#64559),
 .UNSPECIFIED.,.F.,.F.,(4,3,3,3,3,3,3,3,3,3,3,3,3,3,3,3,3,3,3,3,3,3,3,3,
3,3,3,3,3,3,3,3,3,3,3,3,3,3,3,3,3,4),(30.5008964778001,30.60780018035,30.7116793508395,
30.8155067878367,30.9193172487462,31.0285194611095,31.1324675689032,31.2364884416467,
31.3406776902349,31.3561260981992,31.4603125242579,31.5643437178277,31.66825288294,
31.7720965929505,31.8759096265291,31.9797267189139,32.0836524794704,32.1876370836113,
32.2918036124655,32.3536546326358,32.4578410526536,32.5618722401372,32.6657813991263,
32.769625102994,32.8734381304197,32.9772552166506,33.0811809710948,33.1851655691379,
33.2893320919833,33.3511831670724,33.4553695843202,33.5594007689621,33.6633099250166,
33.7671536258938,33.8709666502777,33.9747837334197,34.078709484724,34.1826940795938,
34.2868605992471,34.348711701509,34.4945927534407,34.5575191894877),
 .UNSPECIFIED.);
#2367=B_SPLINE_CURVE_WITH_KNOTS('',3,(#64565,#64566,#64567,#64568,#64569,
#64570,#64571,#64572,#64573,#64574,#64575,#64576,#64577,#64578,#64579,#64580,
#64581,#64582,#64583,#64584,#64585,#64586,#64587,#64588,#64589,#64590,#64591,
#64592,#64593,#64594,#64595,#64596,#64597,#64598,#64599,#64600,#64601,#64602,
#64603,#64604,#64605,#64606,#64607,#64608,#64609,#64610,#64611,#64612,#64613,
#64614,#64615,#64616,#64617,#64618,#64619,#64620,#64621,#64622,#64623,#64624,
#64625,#64626,#64627,#64628,#64629,#64630,#64631,#64632,#64633,#64634,#64635,
#64636,#64637,#64638,#64639,#64640,#64641,#64642,#64643,#64644,#64645,#64646,
#64647,#64648,#64649,#64650,#64651,#64652,#64653,#64654,#64655,#64656,#64657,
#64658,#64659,#64660,#64661,#64662,#64663,#64664,#64665,#64666,#64667,#64668,
#64669,#64670,#64671,#64672,#64673,#64674,#64675,#64676,#64677,#64678,#64679,
#64680,#64681,#64682,#64683,#64684,#64685),.UNSPECIFIED.,.F.,.F.,(4,3,3,
3,3,3,3,3,3,3,3,3,3,3,3,3,3,3,3,3,3,3,3,3,3,3,3,3,3,3,3,3,3,3,3,3,3,3,3,
3,4),(24.217503635835,24.3213222059318,24.425134673036,24.5290492826193,
24.6330136077226,24.7371695283197,24.8294509519326,24.9336372114634,25.0376682357345,
25.1415772282558,25.2454207637364,25.3492336211072,25.4530505358651,25.5569761178482,
25.6609605426126,25.765126892764,25.8269794863692,25.9311659550804,26.0351971917238,
26.1391064003233,26.2429501540519,26.3467632315137,26.450580367881,26.554506172266,
26.6584908202149,26.7626573923662,26.8245080208058,26.9286944520351,27.0327256510729,
27.1366348220718,27.2404785382244,27.3442915781914,27.4481086772032,27.5520344447068,
27.6560190559863,27.7601855922066,27.8220365552424,27.935110886893,28.0468017146134,
28.1605677982292,28.274333881845),.UNSPECIFIED.);
#2368=B_SPLINE_CURVE_WITH_KNOTS('',3,(#64686,#64687,#64688,#64689,#64690,
#64691,#64692,#64693,#64694,#64695,#64696,#64697,#64698,#64699,#64700,#64701,
#64702,#64703,#64704,#64705,#64706,#64707,#64708,#64709,#64710,#64711,#64712,
#64713,#64714,#64715,#64716,#64717,#64718,#64719,#64720,#64721,#64722,#64723,
#64724,#64725,#64726,#64727,#64728,#64729,#64730,#64731,#64732,#64733,#64734,
#64735,#64736,#64737,#64738,#64739,#64740,#64741,#64742,#64743,#64744,#64745,
#64746,#64747,#64748,#64749,#64750,#64751,#64752),.UNSPECIFIED.,.F.,.F.,
(4,3,3,3,3,3,3,3,3,3,3,3,3,3,3,3,3,3,3,3,3,3,4),(28.2743338823081,28.3811973776,
28.4907893056198,28.5979678654125,28.7087664775457,28.819565089679,28.9237515157207,
29.0277827092731,29.131691874368,29.2355355843608,29.3393486179216,29.4431657102888,
29.5470914708273,29.6510760749505,29.755242603787,29.8170936241156,29.9212582775509,
30.0252784744297,30.1291892265987,30.23303658542,30.3368456659329,30.440686438367,
30.4998648058973),.UNSPECIFIED.);
#2369=B_SPLINE_CURVE_WITH_KNOTS('',3,(#64754,#64755,#64756,#64757,#64758,
#64759,#64760,#64761,#64762,#64763,#64764,#64765,#64766,#64767,#64768,#64769,
#64770,#64771,#64772,#64773,#64774,#64775,#64776,#64777,#64778,#64779,#64780,
#64781,#64782,#64783,#64784,#64785,#64786,#64787,#64788,#64789,#64790,#64791,
#64792,#64793,#64794,#64795,#64796,#64797,#64798,#64799,#64800,#64801,#64802,
#64803,#64804,#64805,#64806,#64807,#64808,#64809,#64810,#64811,#64812,#64813,
#64814,#64815,#64816,#64817,#64818,#64819,#64820,#64821,#64822,#64823),
 .UNSPECIFIED.,.F.,.F.,(4,3,3,3,3,3,3,3,3,3,3,3,3,3,3,3,3,3,3,3,3,3,3,4),
(28.2743338823081,28.3635404948894,28.4677269637131,28.5717582004703,28.6756674091851,
28.7795111630297,28.8833242406082,28.9871413770926,29.0910671815947,29.1950518296606,
29.299218401928,29.361069029326,29.4652554605646,29.5692866596124,29.6731958306218,
29.777039546785,29.8808525867634,29.9846696857866,30.0885954533024,30.1925800645945,
30.2967466008277,30.3585975637626,30.4627747459839,30.5008964778001),
 .UNSPECIFIED.);
#2370=B_SPLINE_CURVE_WITH_KNOTS('',3,(#64824,#64825,#64826,#64827,#64828,
#64829,#64830,#64831,#64832,#64833,#64834,#64835,#64836,#64837,#64838,#64839,
#64840,#64841,#64842,#64843,#64844,#64845,#64846,#64847,#64848,#64849,#64850,
#64851,#64852,#64853,#64854,#64855,#64856,#64857,#64858,#64859,#64860,#64861,
#64862,#64863,#64864,#64865,#64866,#64867,#64868,#64869,#64870,#64871,#64872,
#64873,#64874,#64875,#64876,#64877,#64878,#64879,#64880,#64881,#64882,#64883,
#64884,#64885,#64886,#64887,#64888,#64889,#64890,#64891,#64892,#64893,#64894,
#64895,#64896,#64897,#64898,#64899,#64900,#64901,#64902,#64903,#64904,#64905,
#64906,#64907,#64908,#64909,#64910,#64911,#64912,#64913,#64914,#64915,#64916,
#64917,#64918,#64919,#64920,#64921,#64922,#64923,#64924,#64925,#64926,#64927,
#64928,#64929,#64930,#64931,#64932,#64933,#64934,#64935,#64936,#64937,#64938,
#64939,#64940,#64941,#64942,#64943,#64944,#64945,#64946,#64947),
 .UNSPECIFIED.,.F.,.F.,(4,3,3,3,3,3,3,3,3,3,3,3,3,3,3,3,3,3,3,3,3,3,3,3,
3,3,3,3,3,3,3,3,3,3,3,3,3,3,3,3,3,4),(24.216610822454,24.3207830806826,
24.373426357143,24.4776114009861,24.5816411901214,24.6855489246265,24.7893911886519,
24.8932027630289,24.9970183851422,25.1009426686368,25.2049257896555,25.3090908418869,
25.3709548915796,25.4751416524088,25.5791731833385,25.683082687985,25.7869267386815,
25.8907401135825,25.9945575474114,26.0984836472173,26.2024685898807,26.3066354524068,
26.3684834260162,26.4726699929772,26.5767013312479,26.6806106460173,26.7844545086655,
26.8882676976377,26.9920849479502,27.0960108692345,27.1999956359264,27.3041623284679,
27.3660119604528,27.4689825722287,27.5717780278883,27.6744756345683,27.7771117866933,
27.8797227943392,27.9824096578291,28.0851324769858,28.1880251700446,28.2743338818544),
 .UNSPECIFIED.);
#2371=B_SPLINE_CURVE_WITH_KNOTS('',3,(#64953,#64954,#64955,#64956,#64957,
#64958,#64959,#64960,#64961,#64962,#64963,#64964,#64965,#64966,#64967,#64968,
#64969,#64970,#64971,#64972,#64973,#64974,#64975,#64976,#64977,#64978,#64979,
#64980,#64981,#64982,#64983,#64984,#64985,#64986,#64987,#64988,#64989,#64990,
#64991,#64992,#64993,#64994,#64995,#64996,#64997,#64998,#64999,#65000,#65001,
#65002,#65003,#65004,#65005,#65006,#65007,#65008,#65009,#65010,#65011,#65012,
#65013,#65014,#65015,#65016,#65017,#65018,#65019,#65020,#65021,#65022),
 .UNSPECIFIED.,.F.,.F.,(4,3,3,3,3,3,3,3,3,3,3,3,3,3,3,3,3,3,3,3,3,3,3,4),
(15.7079632679489,15.8108075207976,15.9136176294312,16.0164295592376,16.1193522355562,
16.2223337901453,16.3255055953843,16.3931980816502,16.4974234526802,16.601492102817,
16.7054363083021,16.8093135437171,16.913158532871,17.0170059545467,17.1209593297386,
17.2249700571636,17.3291600474277,17.3907266160868,17.4950704177087,17.5992688449958,
17.7033463481182,17.8073550286743,17.9113372683337,17.9338028151035),
 .UNSPECIFIED.);
#2372=B_SPLINE_CURVE_WITH_KNOTS('',3,(#65024,#65025,#65026,#65027,#65028),
 .UNSPECIFIED.,.F.,.F.,(4,1,4),(14.398141012777,15.3956695472136,15.7079548703062),
 .UNSPECIFIED.);
#2373=B_SPLINE_CURVE_WITH_KNOTS('',3,(#65032,#65033,#65034,#65035,#65036,
#65037,#65038,#65039,#65040,#65041,#65042,#65043,#65044,#65045,#65046,#65047,
#65048,#65049,#65050,#65051,#65052,#65053,#65054,#65055,#65056,#65057,#65058,
#65059,#65060,#65061,#65062,#65063,#65064,#65065,#65066,#65067,#65068,#65069,
#65070,#65071,#65072,#65073,#65074,#65075,#65076,#65077,#65078,#65079,#65080,
#65081,#65082,#65083,#65084,#65085,#65086,#65087,#65088,#65089),
 .UNSPECIFIED.,.F.,.F.,(4,3,3,3,3,3,3,3,3,3,3,3,3,3,3,3,3,3,3,4),(13.8761929464654,
13.9800533101315,14.0837576809506,14.1873395169571,14.2908561363859,14.3943427883844,
14.4978346788727,14.6014334411966,14.7050930721393,14.808926366747,14.8541656075666,
14.9608903150643,15.0635179860614,15.1660515649805,15.2685276082899,15.3709825899125,
15.4735044952598,15.5760669075167,15.6787650973359,15.7079632675479),
 .UNSPECIFIED.);
#2374=B_SPLINE_CURVE_WITH_KNOTS('',3,(#65090,#65091,#65092,#65093,#65094,
#65095,#65096,#65097,#65098,#65099,#65100,#65101,#65102,#65103,#65104,#65105,
#65106,#65107,#65108,#65109,#65110,#65111,#65112,#65113,#65114,#65115,#65116,
#65117,#65118,#65119,#65120,#65121,#65122,#65123,#65124,#65125,#65126,#65127,
#65128,#65129,#65130,#65131,#65132,#65133,#65134,#65135,#65136,#65137,#65138,
#65139,#65140,#65141,#65142,#65143,#65144,#65145,#65146,#65147,#65148,#65149,
#65150,#65151,#65152,#65153,#65154,#65155,#65156),.UNSPECIFIED.,.F.,.F.,
(4,3,3,3,3,3,3,3,3,3,3,3,3,3,3,3,3,3,3,3,3,3,4),(15.7079632679489,15.8516941420032,
15.9557858042368,16.0597208697947,16.1635323445499,16.2672774512289,16.3709911139846,
16.4747082126587,16.5785337136997,16.6824177550802,16.7864843330176,16.8492226764398,
16.9534205021522,17.0574630418792,17.1613834157788,17.2652382431943,17.3690622856147,
17.4728902609929,17.576826634821,17.6808217159442,17.7849983901856,17.8467512108764,
17.9343860548896),.UNSPECIFIED.);
#2375=B_SPLINE_CURVE_WITH_KNOTS('',3,(#65162,#65163,#65164,#65165,#65166,
#65167,#65168,#65169,#65170,#65171,#65172,#65173,#65174,#65175,#65176,#65177,
#65178,#65179,#65180,#65181,#65182,#65183,#65184,#65185,#65186,#65187,#65188,
#65189,#65190,#65191,#65192,#65193,#65194,#65195,#65196,#65197,#65198,#65199,
#65200,#65201,#65202,#65203,#65204,#65205,#65206,#65207,#65208,#65209,#65210,
#65211,#65212,#65213,#65214,#65215,#65216,#65217,#65218,#65219,#65220,#65221,
#65222,#65223,#65224,#65225,#65226,#65227,#65228,#65229,#65230,#65231,#65232,
#65233,#65234,#65235,#65236,#65237,#65238,#65239,#65240,#65241,#65242,#65243,
#65244,#65245,#65246,#65247,#65248,#65249,#65250,#65251,#65252,#65253,#65254,
#65255,#65256,#65257,#65258,#65259,#65260,#65261,#65262,#65263,#65264,#65265,
#65266,#65267,#65268,#65269,#65270,#65271,#65272,#65273,#65274,#65275,#65276,
#65277,#65278,#65279,#65280,#65281,#65282,#65283,#65284,#65285,#65286,#65287,
#65288,#65289,#65290,#65291,#65292,#65293,#65294,#65295,#65296,#65297,#65298,
#65299,#65300,#65301,#65302,#65303,#65304,#65305,#65306,#65307,#65308,#65309,
#65310,#65311,#65312,#65313,#65314,#65315,#65316,#65317,#65318,#65319,#65320,
#65321),.UNSPECIFIED.,.F.,.F.,(4,2,2,2,2,2,2,2,2,2,2,2,2,2,2,2,2,2,2,2,
2,2,2,2,2,2,2,2,2,2,2,2,2,2,2,2,2,2,2,2,2,2,2,2,2,2,2,2,2,2,2,2,2,2,2,2,
2,2,2,2,2,2,2,2,2,2,2,2,2,2,2,2,2,2,2,2,2,2,2,4),(-0.808582055129663,-0.803750614026372,
-0.763920330281699,-0.755667253465798,-0.75190245147688,-0.748972613107904,
-0.745765373766368,-0.740511450747678,-0.719053209338083,-0.69846875698509,
-0.691967490889064,-0.672374345367434,-0.668941281667516,-0.667023789605648,
-0.665537186039255,-0.663440027933879,-0.659063955571724,-0.641129598341453,
-0.609238275446381,-0.591965953341908,-0.586791614385876,-0.583578500081481,
-0.580606426328198,-0.576666530975811,-0.567786478554396,-0.555350320334861,
-0.532819209479985,-0.507841520573553,-0.503028370410831,-0.500866708614739,
-0.499194069315333,-0.497221158872559,-0.493559031526201,-0.488855239769308,
-0.477797381356973,-0.456889776921505,-0.42796240650032,-0.422295505956326,
-0.418967878059288,-0.41600699396248,-0.412244951825184,-0.404420493997271,
-0.393962716344978,-0.367392978153513,-0.342227285733235,-0.337519719142119,
-0.33535920705291,-0.333720165398493,-0.331917713334656,-0.328671763421213,
-0.310469465232343,-0.274328821835838,-0.257188434838968,-0.252160474892508,
-0.249075844823561,-0.246251013205195,-0.242552244870408,-0.234440828804303,
-0.215769155900156,-0.187732945517661,-0.171746381145023,-0.168478623810818,
-0.16662470038414,-0.164968853319369,-0.163325419308313,-0.159701628571505,
-0.154862417972763,-0.143393153682017,-0.108931284928433,-0.0861875646209558,
-0.0802886329468558,-0.0767063052521176,-0.0734367767388694,-0.0691524045541401,
-0.0595712385022908,-0.0329949355909643,-0.00749774509555919,-0.00328704030493268,
-0.00149795699922902,-5.90725362616208E-5),.UNSPECIFIED.);
#2376=B_SPLINE_CURVE_WITH_KNOTS('',3,(#65325,#65326,#65327,#65328,#65329,
#65330,#65331,#65332,#65333,#65334),.UNSPECIFIED.,.F.,.F.,(4,2,2,2,4),(-1.15749276218983,
-1.15572035722263,-1.15208331877872,-1.12811344528877,-1.10921379458959),
 .UNSPECIFIED.);
#2377=B_SPLINE_CURVE_WITH_KNOTS('',3,(#65338,#65339,#65340,#65341,#65342,
#65343,#65344,#65345,#65346,#65347,#65348,#65349,#65350,#65351,#65352,#65353,
#65354,#65355,#65356,#65357,#65358,#65359,#65360,#65361,#65362,#65363,#65364,
#65365,#65366,#65367,#65368,#65369,#65370,#65371,#65372,#65373,#65374,#65375,
#65376,#65377,#65378,#65379,#65380,#65381,#65382,#65383,#65384,#65385,#65386,
#65387,#65388,#65389,#65390,#65391,#65392,#65393,#65394,#65395,#65396,#65397,
#65398,#65399,#65400,#65401,#65402,#65403,#65404,#65405,#65406,#65407,#65408,
#65409,#65410,#65411,#65412,#65413,#65414,#65415,#65416,#65417,#65418,#65419,
#65420,#65421,#65422,#65423,#65424,#65425,#65426,#65427,#65428,#65429,#65430,
#65431,#65432,#65433,#65434,#65435,#65436,#65437,#65438,#65439,#65440,#65441,
#65442,#65443,#65444,#65445,#65446,#65447,#65448,#65449,#65450,#65451,#65452,
#65453,#65454,#65455,#65456,#65457,#65458,#65459,#65460,#65461,#65462,#65463,
#65464,#65465,#65466,#65467,#65468,#65469,#65470,#65471,#65472,#65473,#65474,
#65475,#65476,#65477,#65478,#65479,#65480,#65481,#65482,#65483,#65484,#65485,
#65486,#65487,#65488,#65489,#65490,#65491,#65492,#65493,#65494,#65495,#65496,
#65497,#65498,#65499,#65500,#65501,#65502,#65503,#65504,#65505,#65506,#65507,
#65508,#65509,#65510,#65511,#65512,#65513,#65514,#65515,#65516,#65517,#65518,
#65519,#65520,#65521,#65522,#65523,#65524,#65525,#65526,#65527,#65528,#65529,
#65530,#65531,#65532,#65533,#65534,#65535,#65536,#65537,#65538,#65539,#65540,
#65541,#65542,#65543,#65544,#65545,#65546,#65547,#65548,#65549,#65550,#65551,
#65552,#65553,#65554,#65555,#65556,#65557,#65558,#65559,#65560,#65561,#65562,
#65563,#65564,#65565,#65566,#65567,#65568,#65569,#65570,#65571,#65572,#65573,
#65574,#65575,#65576,#65577,#65578,#65579,#65580,#65581,#65582,#65583),
 .UNSPECIFIED.,.F.,.F.,(4,2,2,2,2,2,2,2,2,2,2,2,2,2,2,2,2,2,2,2,2,2,2,2,
2,2,2,2,2,2,2,2,2,2,2,2,2,2,2,2,2,2,2,2,2,2,2,2,2,2,2,2,2,2,2,2,2,2,2,2,
2,2,2,2,2,2,2,2,2,2,2,2,2,2,2,2,2,2,2,2,2,2,2,2,2,2,2,2,2,2,2,2,2,2,2,2,
2,2,2,2,2,2,2,2,2,2,2,2,2,2,2,2,2,2,2,2,2,2,2,2,2,2,4),(-1.10921379458959,
-1.1076622373938,-1.08543029392662,-1.08007660077131,-1.07681618900784,
-1.07384144573965,-1.07002200227276,-1.06362969737749,-1.03625654951167,
-1.01337557673973,-1.00413366587587,-0.998062465708908,-0.995654503029387,
-0.995584277422565,-0.995514581954951,-0.994634984079058,-0.992976116028102,
-0.990699970051695,-0.986534035181013,-0.95638691292609,-0.932673550488202,
-0.918981357511638,-0.914363492443028,-0.911268149014135,-0.908270632900765,
-0.903997613306416,-0.893720029061984,-0.856272923844288,-0.840725640414238,
-0.834891118125428,-0.830578552244249,-0.828493879803355,-0.827008934693503,
-0.825083117447351,-0.821611454849291,-0.800373373787523,-0.795878501794505,
-0.775697105914707,-0.75357378904031,-0.748280596185468,-0.745065450117817,
-0.742138744625703,-0.738392298060851,-0.732156623046581,-0.694465634680216,
-0.666738258049506,-0.663195678002921,-0.661278515404786,-0.65963265045503,
-0.657494032312746,-0.652918871567297,-0.623432265430871,-0.59912137250215,
-0.589806414114396,-0.582658273763377,-0.579044736771133,-0.576119956577928,
-0.572745584710808,-0.566772416941517,-0.53448537490031,-0.501621091196771,
-0.497196429139702,-0.49509160053332,-0.493444676853058,-0.491454876526423,
-0.487604356959964,-0.482567470634422,-0.470231421438504,-0.433118198255328,
-0.419075378204661,-0.414291071255023,-0.411172166491054,-0.408181866721782,
-0.40405128380816,-0.393914186715727,-0.378950192964909,-0.359038211076391,
-0.356823833118952,-0.333520724434363,-0.33002920063043,-0.32809416072214,
-0.32644584832746,-0.324277862816438,-0.319490470960679,-0.297575056806468,
-0.256724250613953,-0.24961066582482,-0.245962076794916,-0.243040707618046,
-0.239705129944953,-0.233893905956809,-0.226762494548428,-0.211069025012032,
-0.181557437977702,-0.16648146851152,-0.163191867885106,-0.161303248197036,
-0.159692646635295,-0.159675204713457,-0.159658113308516,-0.15964134997403,
-0.159624893753413,-0.159608725047098,-0.159592825484932,-0.159577177801894,
-0.159561765764004,-0.159546574017785,-0.159531588127396,-0.15951679434262,
-0.159502179667159,-0.159487731745921,-0.159473438765623,-0.157288660723066,
-0.154702145306918,-0.150102155419665,-0.106320137254155,-0.0867330356464405,
-0.0814335128342001,-0.0782058172347371,-0.0752616337348794,-0.0714195197704843,
-0.0630253608599946,-0.0594837367698858),.UNSPECIFIED.);
#2378=B_SPLINE_CURVE_WITH_KNOTS('',3,(#65588,#65589,#65590,#65591,#65592,
#65593,#65594,#65595,#65596,#65597,#65598,#65599,#65600,#65601,#65602,#65603,
#65604,#65605,#65606,#65607,#65608,#65609,#65610,#65611,#65612,#65613,#65614,
#65615,#65616,#65617,#65618,#65619,#65620,#65621,#65622,#65623,#65624,#65625,
#65626,#65627,#65628,#65629,#65630,#65631,#65632,#65633,#65634,#65635,#65636,
#65637,#65638,#65639,#65640,#65641,#65642,#65643,#65644,#65645,#65646,#65647,
#65648,#65649,#65650,#65651,#65652,#65653,#65654,#65655,#65656,#65657,#65658,
#65659,#65660,#65661,#65662,#65663,#65664,#65665,#65666,#65667,#65668,#65669,
#65670,#65671,#65672,#65673,#65674,#65675,#65676,#65677,#65678,#65679,#65680,
#65681,#65682,#65683,#65684,#65685,#65686,#65687,#65688,#65689,#65690,#65691,
#65692,#65693,#65694,#65695,#65696,#65697,#65698,#65699,#65700,#65701,#65702,
#65703,#65704,#65705,#65706,#65707,#65708,#65709,#65710,#65711,#65712,#65713,
#65714,#65715,#65716,#65717,#65718,#65719,#65720,#65721,#65722,#65723,#65724,
#65725,#65726,#65727,#65728,#65729,#65730,#65731,#65732,#65733,#65734,#65735,
#65736,#65737,#65738,#65739,#65740,#65741,#65742,#65743,#65744,#65745,#65746,
#65747,#65748,#65749,#65750,#65751,#65752,#65753,#65754,#65755,#65756,#65757,
#65758,#65759,#65760,#65761,#65762,#65763,#65764,#65765,#65766,#65767,#65768,
#65769,#65770,#65771,#65772,#65773,#65774,#65775,#65776,#65777,#65778,#65779,
#65780,#65781,#65782,#65783,#65784,#65785,#65786,#65787,#65788,#65789,#65790,
#65791,#65792,#65793),.UNSPECIFIED.,.F.,.F.,(4,2,2,2,2,2,2,2,2,2,2,2,2,
2,2,2,2,2,2,2,2,2,2,2,2,2,2,2,2,2,2,2,2,2,2,2,2,2,2,2,2,2,2,2,2,2,2,2,2,
2,2,2,2,2,2,2,2,2,2,2,2,2,2,2,2,2,2,2,2,2,2,2,2,2,2,2,2,2,2,2,2,2,2,2,2,
2,2,2,2,2,2,2,2,2,2,2,2,2,2,2,2,2,4),(-1.85846886095936,-1.83940746062439,
-1.83584410856664,-1.83391468281092,-1.83226448898463,-1.83012226369945,
-1.82535591730456,-1.80035676732322,-1.77297800175295,-1.76304851740448,
-1.75554658385211,-1.75259517608712,-1.74960920593114,-1.74648440515245,
-1.74166992480376,-1.72733708559932,-1.69375758835966,-1.67430341423461,
-1.6697663072851,-1.66764318548338,-1.66615436934787,-1.66425192801052,
-1.66090687750724,-1.64486336622851,-1.61437034361168,-1.59258605810712,
-1.58729403195599,-1.58406722219309,-1.58112146812251,-1.57733837612187,
-1.57101172952175,-1.53487894154682,-1.51483572827075,-1.50806052845142,
-1.50323563971223,-1.50105966179817,-1.49942416983499,-1.49749802835678,
-1.49404903860049,-1.47439651711881,-1.46756476285612,-1.44599525673569,
-1.42575798766076,-1.4205649458911,-1.41735896958992,-1.41440623622628,
-1.41057755467444,-1.40203015604819,-1.36270968135944,-1.34127876933968,
-1.33653713800039,-1.33437620702495,-1.33274284051056,-1.33080884318828,
-1.32731946098936,-1.30448740517577,-1.30173400770234,-1.28561352722048,
-1.25963283693165,-1.25413250054938,-1.25086226218927,-1.24792908125744,
-1.24417130761191,-1.23807099264858,-1.19226636828357,-1.1740287969165,
-1.1696260424052,-1.16752863401233,-1.16604278240289,-1.16412267488346,
-1.1607005570197,-1.14311944415211,-1.09804721401168,-1.08934483797966,
-1.08544687611174,-1.08249299916335,-1.07928692081737,-1.07409623560765,
-1.05598913768461,-1.02459976863163,-1.01174140477052,-1.00656771909017,
-1.00263635224312,-1.00062973789446,-0.998983142740153,-0.996896518036183,
-0.992569302577529,-0.958661620705056,-0.926714198535095,-0.921025586144166,
-0.9177109377958,-0.915071589931665,-0.911511887496554,-0.904639540027466,
-0.879761342924638,-0.862527715430148,-0.839367465758799,-0.835876498401726,
-0.833941437923539,-0.832298862120824,-0.830144346188354,-0.825392157409788,
-0.808582055129663),.UNSPECIFIED.);
#2379=B_SPLINE_CURVE_WITH_KNOTS('',3,(#65795,#65796,#65797,#65798,#65799,
#65800,#65801,#65802),.UNSPECIFIED.,.F.,.F.,(4,2,2,4),(-0.0594837367698858,
-0.0402893593164964,-0.00570478766600024,-0.000519914712907845),
 .UNSPECIFIED.);
#2380=B_SPLINE_CURVE_WITH_KNOTS('',3,(#65803,#65804,#65805,#65806,#65807,
#65808,#65809,#65810,#65811,#65812,#65813),.UNSPECIFIED.,.F.,.F.,(4,2,1,
1,1,1,1,4),(-91.8109775642064,-91.7726251681672,-90.7750966337306,-89.777568099294,
-88.7800395648573,-87.7825110304207,-86.7849824959842,-85.8810481711785),
 .UNSPECIFIED.);
#2381=B_SPLINE_CURVE_WITH_KNOTS('',3,(#65819,#65820,#65821,#65822,#65823,
#65824,#65825,#65826,#65827,#65828,#65829,#65830,#65831,#65832,#65833,#65834,
#65835,#65836,#65837,#65838,#65839,#65840,#65841,#65842,#65843,#65844,#65845,
#65846,#65847,#65848,#65849,#65850,#65851,#65852,#65853,#65854,#65855,#65856,
#65857,#65858,#65859,#65860,#65861,#65862,#65863,#65864,#65865,#65866,#65867,
#65868,#65869,#65870,#65871,#65872,#65873,#65874,#65875,#65876,#65877,#65878,
#65879,#65880,#65881,#65882,#65883,#65884,#65885,#65886,#65887,#65888,#65889,
#65890,#65891,#65892,#65893,#65894,#65895,#65896,#65897,#65898,#65899,#65900,
#65901,#65902,#65903,#65904,#65905,#65906,#65907,#65908,#65909,#65910,#65911,
#65912,#65913,#65914,#65915,#65916,#65917,#65918,#65919,#65920,#65921,#65922,
#65923,#65924,#65925,#65926,#65927,#65928,#65929,#65930,#65931,#65932,#65933,
#65934,#65935,#65936,#65937,#65938,#65939,#65940,#65941,#65942,#65943,#65944,
#65945,#65946,#65947,#65948,#65949,#65950,#65951,#65952,#65953,#65954,#65955,
#65956,#65957,#65958,#65959,#65960,#65961,#65962,#65963,#65964,#65965,#65966,
#65967,#65968,#65969,#65970,#65971,#65972,#65973,#65974,#65975,#65976,#65977,
#65978,#65979,#65980,#65981,#65982,#65983,#65984,#65985,#65986,#65987,#65988,
#65989,#65990,#65991,#65992,#65993,#65994,#65995,#65996,#65997,#65998,#65999,
#66000,#66001,#66002,#66003,#66004,#66005,#66006,#66007,#66008,#66009,#66010),
 .UNSPECIFIED.,.F.,.F.,(4,2,2,2,2,2,2,2,2,2,2,2,2,2,2,2,2,2,2,2,2,2,2,2,
2,2,2,2,2,2,2,2,2,2,2,2,2,2,2,2,2,2,2,2,2,2,2,2,2,2,2,2,2,2,2,2,2,2,2,2,
2,2,2,2,2,2,2,2,2,2,2,2,2,2,2,2,2,2,2,2,2,2,2,2,2,2,2,2,2,2,2,2,2,2,2,4),
(-0.991262637114908,-0.990030252789208,-0.964527390077046,-0.944362212569878,
-0.922374036844681,-0.918886818977652,-0.916952565365279,-0.91531878672021,
-0.913156466960908,-0.908406383444986,-0.886886962178832,-0.847304463235204,
-0.838984566926019,-0.835196135180223,-0.832249899261719,-0.829026281497939,
-0.823748072949235,-0.80217954981134,-0.781695306292921,-0.775418038969063,
-0.755652765737664,-0.752201922684275,-0.750275855961832,-0.74864097689561,
-0.746466720698178,-0.741650014618699,-0.734888983996405,-0.714919338689796,
-0.678641842268481,-0.672321416351242,-0.668540371424746,-0.665595239400699,
-0.662368125913504,-0.657073298748417,-0.635227958438309,-0.604487035879512,
-0.588763616771329,-0.585445145543287,-0.583548821242408,-0.581892680820745,
-0.579660050052783,-0.574510941017902,-0.567116707527369,-0.543611162637253,
-0.512259918175071,-0.505168607929871,-0.501522597149624,-0.498598920688561,
-0.495255888335385,-0.489418751926246,-0.454493428867502,-0.42414295424235,
-0.419520884632951,-0.417404696033666,-0.415757055510615,-0.413809412693716,
-0.410158687053075,-0.40545650268177,-0.394352189656478,-0.372833388782713,
-0.343029282271306,-0.337355579530089,-0.334047276832857,-0.331411905411525,
-0.327856286025243,-0.320987859283398,-0.296099589263666,-0.278896086712574,
-0.255762494913994,-0.252271942542737,-0.25033702846841,-0.248703473997468,
-0.246542473035566,-0.24179918967524,-0.220346644129287,-0.1809766917338,
-0.172464914557856,-0.168643181998464,-0.165692330929846,-0.162957682269341,
-0.158213118362014,-0.143229348464024,-0.115398714033831,-0.108393955572286,
-0.0890224012168137,-0.0855820925314036,-0.0836584253521946,-0.0821731792243276,
-0.0800811858767538,-0.0757086538011402,-0.0577400170824042,-0.020644334918703,
-0.00771115206037433,-0.00324887219255287,-0.00155419658315507,-0.000491736839017494),
 .UNSPECIFIED.);
#2382=B_SPLINE_CURVE_WITH_KNOTS('',3,(#66011,#66012,#66013,#66014,#66015,
#66016,#66017,#66018,#66019,#66020,#66021,#66022,#66023,#66024),
 .UNSPECIFIED.,.F.,.F.,(4,2,2,2,2,2,4),(-1.91741114141026,-1.91639157322029,
-1.91462258465228,-1.91113044186193,-1.90404850449963,-1.8694194204246,
-1.85846886095936),.UNSPECIFIED.);
#2383=B_SPLINE_CURVE_WITH_KNOTS('',3,(#66026,#66027,#66028,#66029,#66030),
 .UNSPECIFIED.,.F.,.F.,(4,1,4),(-85.8810481711785,-85.7874539615476,-85.5277944653042),
 .UNSPECIFIED.);
#2384=B_SPLINE_CURVE_WITH_KNOTS('',3,(#66031,#66032,#66033,#66034,#66035,
#66036,#66037,#66038,#66039,#66040,#66041,#66042,#66043,#66044,#66045,#66046,
#66047,#66048,#66049,#66050,#66051,#66052,#66053,#66054,#66055,#66056,#66057,
#66058,#66059,#66060,#66061,#66062,#66063,#66064,#66065,#66066,#66067,#66068,
#66069,#66070,#66071,#66072,#66073,#66074,#66075,#66076,#66077,#66078,#66079,
#66080,#66081,#66082,#66083,#66084,#66085,#66086,#66087,#66088,#66089,#66090,
#66091,#66092,#66093,#66094,#66095,#66096,#66097,#66098,#66099,#66100,#66101,
#66102,#66103,#66104,#66105,#66106,#66107,#66108,#66109,#66110,#66111,#66112,
#66113,#66114,#66115,#66116,#66117,#66118,#66119,#66120,#66121,#66122,#66123,
#66124,#66125,#66126,#66127,#66128,#66129,#66130,#66131,#66132,#66133,#66134,
#66135,#66136,#66137,#66138,#66139,#66140,#66141,#66142,#66143,#66144,#66145,
#66146,#66147,#66148,#66149,#66150,#66151,#66152,#66153,#66154,#66155,#66156,
#66157,#66158,#66159,#66160,#66161,#66162,#66163,#66164,#66165,#66166,#66167,
#66168,#66169,#66170,#66171,#66172,#66173,#66174,#66175,#66176,#66177,#66178,
#66179,#66180,#66181,#66182,#66183,#66184,#66185,#66186,#66187,#66188,#66189,
#66190,#66191,#66192,#66193,#66194,#66195,#66196,#66197,#66198,#66199,#66200,
#66201,#66202,#66203,#66204,#66205,#66206,#66207,#66208,#66209,#66210,#66211,
#66212,#66213,#66214,#66215,#66216,#66217,#66218,#66219,#66220,#66221,#66222,
#66223,#66224,#66225,#66226),.UNSPECIFIED.,.F.,.F.,(4,2,2,2,2,2,2,2,2,2,
2,2,2,2,2,2,2,2,2,2,2,2,2,2,2,2,2,2,2,2,2,2,2,2,2,2,2,2,2,2,2,2,2,2,2,2,
2,2,2,2,2,2,2,2,2,2,2,2,2,2,2,2,2,2,2,2,2,2,2,2,2,2,2,2,2,2,2,2,2,2,2,2,
2,2,2,2,2,2,2,2,2,2,2,2,2,2,2,4),(-2.10008743950006,-2.07854758539132,-2.06877862930352,
-2.06503838939257,-2.06216829021424,-2.05922429423112,-2.05599570021913,
-2.05069216043087,-2.03102510249862,-2.00168280493975,-1.98255848273885,
-1.9792220524613,-1.97728355240748,-1.97563519043276,-1.97350747600006,
-1.96898873895325,-1.93818697272705,-1.90358154539059,-1.8977555977107,
-1.89441544227115,-1.89149226372879,-1.88784424526438,-1.88074062426806,
-1.84985466702855,-1.82603089322516,-1.81858514856592,-1.81340927420629,
-1.81117240061264,-1.80951606479392,-1.80762300535485,-1.80431769066657,
-1.7888211309634,-1.75993741222275,-1.74412320851496,-1.73695564665984,
-1.73112123017635,-1.72777932196644,-1.72485640810646,-1.72121107940999,
-1.71412029633266,-1.68295169443865,-1.65933233966515,-1.65192035299934,
-1.64676189882025,-1.64452803392657,-1.64287210544079,-1.64097741210199,
-1.6376647637853,-1.62201995662916,-1.59123768309075,-1.56931402662564,
-1.56401518113037,-1.56078779532817,-1.5578438456884,-1.55406632578062,
-1.54775647857148,-1.51134486933854,-1.49148906085177,-1.48475078730921,
-1.47994609221674,-1.47777436960016,-1.47614015179838,-1.47421345641829,
-1.4707582897344,-1.45080620780897,-1.44422628400323,-1.42257348373837,
-1.40244782344601,-1.39726429089917,-1.39406159600309,-1.39111021501586,
-1.38728096677913,-1.3787223542671,-1.33942298786977,-1.31799890436937,
-1.31325885529179,-1.31109876033984,-1.30946563868309,-1.30753101246325,
-1.30404046854004,-1.2809101718976,-1.26371676454656,-1.23878206653153,
-1.2319085560276,-1.22835246299673,-1.22571764938885,-1.22241122638425,
-1.21674379980181,-1.1859481371649,-1.16109781882375,-1.15268110023202,
-1.14701778961442,-1.14470027386306,-1.14303250902419,-1.14118049436591,
-1.13797580709458,-1.12495134819297,-1.10916695937962),.UNSPECIFIED.);
#2385=B_SPLINE_CURVE_WITH_KNOTS('',3,(#66231,#66232,#66233,#66234,#66235,
#66236,#66237,#66238,#66239,#66240,#66241,#66242,#66243,#66244,#66245,#66246,
#66247,#66248,#66249,#66250,#66251,#66252,#66253,#66254,#66255,#66256,#66257,
#66258,#66259,#66260,#66261,#66262,#66263,#66264,#66265,#66266,#66267,#66268,
#66269,#66270,#66271,#66272,#66273,#66274,#66275,#66276,#66277,#66278,#66279,
#66280,#66281,#66282,#66283,#66284,#66285,#66286,#66287,#66288,#66289,#66290,
#66291,#66292,#66293,#66294,#66295,#66296,#66297,#66298,#66299,#66300,#66301,
#66302,#66303,#66304,#66305,#66306,#66307,#66308,#66309,#66310,#66311,#66312,
#66313,#66314,#66315,#66316,#66317,#66318,#66319,#66320,#66321,#66322,#66323,
#66324,#66325,#66326,#66327,#66328,#66329,#66330,#66331,#66332,#66333,#66334,
#66335,#66336,#66337,#66338,#66339,#66340,#66341,#66342,#66343,#66344,#66345,
#66346,#66347,#66348,#66349,#66350,#66351,#66352,#66353,#66354,#66355,#66356,
#66357,#66358,#66359,#66360,#66361,#66362,#66363,#66364,#66365,#66366,#66367,
#66368,#66369,#66370,#66371,#66372,#66373,#66374,#66375,#66376,#66377,#66378,
#66379,#66380,#66381,#66382,#66383,#66384,#66385,#66386,#66387,#66388,#66389,
#66390,#66391,#66392,#66393,#66394,#66395,#66396,#66397,#66398,#66399,#66400,
#66401,#66402,#66403,#66404,#66405,#66406,#66407,#66408,#66409,#66410,#66411,
#66412,#66413,#66414,#66415,#66416,#66417,#66418,#66419,#66420,#66421,#66422,
#66423,#66424,#66425,#66426,#66427,#66428,#66429,#66430,#66431,#66432,#66433,
#66434),.UNSPECIFIED.,.F.,.F.,(4,2,2,2,2,2,2,2,2,2,2,2,2,2,2,2,2,2,2,2,
2,2,2,2,2,2,2,2,2,2,2,2,2,2,2,2,2,2,2,2,2,2,2,2,2,2,2,2,2,2,2,2,2,2,2,2,
2,2,2,2,2,2,2,2,2,2,2,2,2,2,2,2,2,2,2,2,2,2,2,2,2,2,2,2,2,2,2,2,2,2,2,2,
2,2,2,2,2,2,2,2,2,4),(-2.04109563196961,-2.03715166773698,-2.01184485869293,
-2.00492313862756,-2.00135674269587,-1.99872014403853,-1.99541903998376,
-1.98977977271561,-1.9625587603051,-1.94281058529977,-1.92394171208846,
-1.91946817563695,-1.91735695221755,-1.91586952367419,-1.91395912560044,
-1.91057850924682,-1.89356466756653,-1.86496597641253,-1.84241737865986,
-1.83708119169235,-1.83384507126245,-1.8309021145354,-1.82713819870818,
-1.82087882015238,-1.78367129416691,-1.75594594539535,-1.75229721405626,
-1.75034989376827,-1.74870208936822,-1.74658510843154,-1.74195918188692,
-1.70306723415312,-1.68077297087022,-1.67238655265899,-1.66854520687439,
-1.66560053599183,-1.66237124360447,-1.65706660533259,-1.6373914453673,
-1.593689662428,-1.58911259941301,-1.5855370929312,-1.58360513725545,-1.58195527996346,
-1.57981668163954,-1.57507102486309,-1.54946079707402,-1.52714225126485,
-1.51476112371381,-1.50591628141653,-1.50199508401009,-1.49903907249871,
-1.49584558576601,-1.49070872035556,-1.47365075930622,-1.44171997951546,
-1.42375032635273,-1.41937730102091,-1.41728507992514,-1.41579964612381,
-1.41387572895629,-1.41043498620636,-1.39107237832122,-1.38403770584597,
-1.36305971324366,-1.34919519049433,-1.33959438691019,-1.33554818274283,
-1.33257256844589,-1.3294269142354,-1.32451446334915,-1.30929130373869,
-1.27648270213017,-1.25730678594088,-1.2527995987844,-1.25068199203506,
-1.24919377127372,-1.24728753521754,-1.24392567755249,-1.2274651145437,
-1.19771105536898,-1.17567014700486,-1.17036299720748,-1.16713301119125,
-1.16418825384889,-1.16041184023517,-1.15216101112613,-1.11252226898492,
-1.09098941404171,-1.08623779520677,-1.08407512288789,-1.08244121292983,
-1.08050699739299,-1.07702023269248,-1.05524045376991,-1.05036481417599,
-1.0116168663927,-1.00548338386893,-1.00171495280942,-0.998779155699581,
-0.995511802796277,-0.991262637114908),.UNSPECIFIED.);
#2386=B_SPLINE_CURVE_WITH_KNOTS('',3,(#66435,#66436,#66437,#66438,#66439,
#66440,#66441,#66442,#66443,#66444,#66445,#66446,#66447,#66448,#66449,#66450,
#66451,#66452,#66453,#66454,#66455,#66456,#66457,#66458,#66459,#66460,#66461,
#66462,#66463,#66464,#66465,#66466,#66467,#66468,#66469,#66470,#66471,#66472,
#66473,#66474,#66475,#66476,#66477,#66478,#66479,#66480,#66481,#66482,#66483,
#66484,#66485,#66486,#66487,#66488,#66489,#66490,#66491,#66492,#66493,#66494,
#66495,#66496,#66497,#66498,#66499,#66500,#66501,#66502,#66503,#66504,#66505,
#66506,#66507,#66508,#66509,#66510,#66511,#66512,#66513,#66514,#66515,#66516,
#66517,#66518,#66519,#66520,#66521,#66522,#66523,#66524,#66525,#66526,#66527,
#66528,#66529,#66530,#66531,#66532,#66533,#66534,#66535,#66536,#66537,#66538,
#66539,#66540,#66541,#66542,#66543,#66544,#66545,#66546,#66547,#66548,#66549,
#66550,#66551,#66552,#66553,#66554,#66555,#66556,#66557,#66558,#66559,#66560,
#66561,#66562,#66563,#66564,#66565,#66566,#66567,#66568,#66569,#66570,#66571,
#66572,#66573,#66574,#66575,#66576,#66577,#66578,#66579,#66580,#66581,#66582,
#66583,#66584,#66585,#66586,#66587,#66588,#66589,#66590,#66591,#66592,#66593,
#66594,#66595,#66596,#66597,#66598,#66599,#66600,#66601,#66602,#66603,#66604,
#66605,#66606,#66607,#66608,#66609,#66610,#66611,#66612,#66613,#66614,#66615,
#66616,#66617,#66618,#66619,#66620,#66621,#66622,#66623,#66624,#66625,#66626,
#66627,#66628,#66629,#66630,#66631,#66632,#66633,#66634,#66635,#66636,#66637,
#66638,#66639,#66640,#66641,#66642,#66643,#66644,#66645,#66646,#66647,#66648,
#66649,#66650,#66651,#66652,#66653,#66654,#66655,#66656,#66657,#66658,#66659,
#66660,#66661,#66662,#66663,#66664,#66665,#66666,#66667,#66668,#66669,#66670,
#66671,#66672),.UNSPECIFIED.,.F.,.F.,(4,2,2,2,2,2,2,2,2,2,2,2,2,2,2,2,2,
2,2,2,2,2,2,2,2,2,2,2,2,2,2,2,2,2,2,2,2,2,2,2,2,2,2,2,2,2,2,2,2,2,2,2,2,
2,2,2,2,2,2,2,2,2,2,2,2,2,2,2,2,2,2,2,2,2,2,2,2,2,2,2,2,2,2,2,2,2,2,2,2,
2,2,2,2,2,2,2,2,2,2,2,2,2,2,2,2,2,2,2,2,2,2,2,2,2,2,2,2,2,4),(-1.10916695937962,
-1.09785195841207,-1.07226864233564,-1.06531323034322,-1.06174092605676,
-1.05910454465279,-1.0558096438895,-1.05019595022401,-1.02083592305063,
-0.991387429212326,-0.981669540765042,-0.978749037959597,-0.97695925254149,
-0.975263122680412,-0.9727837578719,-0.966034814558207,-0.922226828297954,
-0.902675719034099,-0.897378507909132,-0.89415160224643,-0.891207758227922,
-0.887365563769124,-0.878969252877936,-0.85619628815039,-0.830091811939781,
-0.815697950286459,-0.812447122794245,-0.810566532129448,-0.808907449766328,
-0.806648381931185,-0.801340698496335,-0.79363595111145,-0.76818292718107,
-0.73937940400311,-0.732254783421282,-0.72860268913279,-0.725679490342722,
-0.722342831441816,-0.716532187548575,-0.682184275913402,-0.651090204741507,
-0.646551180600829,-0.6444281909992,-0.642783289586587,-0.640815528728321,
-0.637066012409968,-0.63219831607411,-0.620489823571801,-0.599279371849155,
-0.570182032143738,-0.564536252593569,-0.561202930568941,-0.558307094544375,
-0.554663791565358,-0.547344301304792,-0.537731571237426,-0.511962107665647,
-0.484744484464426,-0.480019022507963,-0.477884616107571,-0.476235812879305,
-0.474302546218574,-0.470718319451695,-0.442099374994455,-0.405754974018102,
-0.39943990984595,-0.395661162926829,-0.392717324841462,-0.38949114357372,
-0.384196767274576,-0.362335538446676,-0.331560175530213,-0.315888801721569,
-0.312575041309464,-0.31068023933258,-0.309024620880329,-0.306791669882353,
-0.301637556163642,-0.294232777094044,-0.270658540912069,-0.239402364645259,
-0.232311699916303,-0.228666690483956,-0.225744166606889,-0.222402851162856,
-0.216569825877009,-0.209404896987984,-0.193599036620314,-0.165317328395053,
-0.14932369071598,-0.145982141213971,-0.144081071524549,-0.142592923032059,
-0.142579128536054,-0.142565964393677,-0.142553393344733,-0.142541380979266,
-0.142529895482768,-0.142509885233177,-0.142490030749955,-0.142470325188627,
-0.14245076194988,-0.142431334553265,-0.142412036723164,-0.142392862367559,
-0.142373805566179,-0.142354860503376,-0.142336021523246,-0.142317283109273,
-0.142298639845394,-0.142280086458585,-0.140162043029368,-0.135247659671907,
-0.128141754728387,-0.106305341310492,-0.072704223676547,-0.0656632114127612,
-0.0620284846312131,-0.0595287291512849),.UNSPECIFIED.);
#2387=B_SPLINE_CURVE_WITH_KNOTS('',3,(#66678,#66679,#66680,#66681,#66682,
#66683,#66684,#66685,#66686,#66687,#66688,#66689,#66690,#66691,#66692,#66693,
#66694,#66695,#66696,#66697,#66698,#66699,#66700,#66701,#66702,#66703,#66704,
#66705,#66706,#66707,#66708,#66709,#66710,#66711,#66712,#66713,#66714,#66715,
#66716,#66717,#66718,#66719,#66720,#66721,#66722,#66723,#66724,#66725,#66726,
#66727,#66728,#66729,#66730,#66731,#66732,#66733,#66734,#66735,#66736,#66737,
#66738,#66739,#66740,#66741,#66742,#66743,#66744,#66745,#66746,#66747,#66748,
#66749,#66750,#66751,#66752,#66753,#66754,#66755,#66756,#66757,#66758,#66759,
#66760,#66761,#66762,#66763,#66764,#66765,#66766,#66767,#66768,#66769,#66770,
#66771,#66772,#66773,#66774,#66775,#66776,#66777,#66778,#66779,#66780,#66781,
#66782,#66783,#66784,#66785,#66786,#66787,#66788,#66789,#66790,#66791,#66792,
#66793,#66794,#66795,#66796,#66797,#66798,#66799,#66800,#66801,#66802,#66803,
#66804,#66805,#66806,#66807,#66808,#66809,#66810,#66811,#66812,#66813,#66814,
#66815,#66816,#66817,#66818,#66819,#66820,#66821,#66822,#66823,#66824,#66825,
#66826,#66827,#66828,#66829,#66830,#66831,#66832,#66833,#66834,#66835,#66836,
#66837,#66838,#66839,#66840,#66841,#66842,#66843,#66844,#66845,#66846,#66847,
#66848,#66849,#66850,#66851,#66852,#66853,#66854,#66855,#66856,#66857,#66858,
#66859,#66860,#66861,#66862,#66863,#66864,#66865,#66866,#66867,#66868,#66869,
#66870,#66871,#66872,#66873,#66874,#66875,#66876,#66877,#66878,#66879,#66880,
#66881,#66882,#66883,#66884,#66885,#66886,#66887,#66888,#66889,#66890,#66891,
#66892,#66893,#66894,#66895,#66896,#66897,#66898,#66899,#66900,#66901,#66902,
#66903),.UNSPECIFIED.,.F.,.F.,(4,2,2,2,2,2,2,2,2,2,2,2,2,2,2,2,2,2,2,2,
2,2,2,2,2,2,2,2,2,2,2,2,2,2,2,2,2,2,2,2,2,2,2,2,2,2,2,2,2,2,2,2,2,2,2,2,
2,2,2,2,2,2,2,2,2,2,2,2,2,2,2,2,2,2,2,2,2,2,2,2,2,2,2,2,2,2,2,2,2,2,2,2,
2,2,2,2,2,2,2,2,2,2,2,2,2,2,2,2,2,2,2,2,4),(-0.991194904658961,-0.989058491626383,
-0.985746034335273,-0.983851197030988,-0.982194965446795,-0.979960349182465,
-0.974798752808426,-0.967380016124243,-0.943724386415452,-0.912576510451123,
-0.90548403672454,-0.901838034646032,-0.89891465974563,-0.895572292867348,
-0.889737164279442,-0.882569425933697,-0.866755685093601,-0.837909878960278,
-0.822426100828139,-0.819121429452957,-0.817228355206994,-0.815571733408831,
-0.813334003219074,-0.808154192747193,-0.800700081459465,-0.77682948391001,
-0.745962654520282,-0.738867704777704,-0.735221196377737,-0.732297786767454,
-0.728955783804222,-0.72312235362758,-0.715957282228572,-0.700152639618032,
-0.671304545212078,-0.655809351069932,-0.652504140663196,-0.650610946596399,
-0.648954355676494,-0.64671684902612,-0.641538331851979,-0.634086729332441,
-0.610231397602398,-0.579344742099706,-0.57224998935752,-0.568603525612343,
-0.565680124390798,-0.562338101220941,-0.556504557299234,-0.549339303327267,
-0.533534020766918,-0.504686172267139,-0.489191833461697,-0.485886668598096,
-0.483993486958045,-0.482336897099563,-0.480099378739821,-0.47492077839181,
-0.467469009380936,-0.443612622131685,-0.412727460531904,-0.405632707781558,
-0.401986248085462,-0.399062852073509,-0.395720836993071,-0.389887312809662,
-0.382722086150404,-0.366916880819668,-0.338069072199305,-0.322574702883354,
-0.319269541326764,-0.317376362560824,-0.315719775922348,-0.313482262853182,
-0.308303678767825,-0.300851936514463,-0.27699567239423,-0.246110465049564,
-0.23901572641041,-0.235369273677834,-0.232445883108845,-0.229103874098857,
-0.223270360112144,-0.216105145760034,-0.200299966375875,-0.171802739950951,
-0.156005557003889,-0.152674181454946,-0.150775084015369,-0.149175409652698,
-0.149155773580123,-0.149136266281287,-0.149116881360587,-0.14909761257984,
-0.149078453872716,-0.149059399305514,-0.149040443054649,-0.14902157946385,
-0.14900280305385,-0.148984108405387,-0.14686707330857,-0.144354652225158,
-0.13994845932989,-0.129882787025892,-0.0914884568668121,-0.0755866350468697,
-0.07060407606162,-0.0674441109984219,-0.0644762356056652,-0.0604736220423971,
-0.0511374369443929,-0.0378016688393984,-0.000492023165766259),
 .UNSPECIFIED.);
#2388=B_SPLINE_CURVE_WITH_KNOTS('',3,(#66904,#66905,#66906,#66907,#66908,
#66909,#66910,#66911,#66912,#66913,#66914,#66915,#66916,#66917,#66918,#66919,
#66920,#66921,#66922,#66923),.UNSPECIFIED.,.F.,.F.,(4,2,2,2,2,2,2,2,2,4),
(-2.09991839469697,-2.0886857961363,-2.08627102604875,-2.08454940902833,
-2.08301335512356,-2.08147524148558,-2.07935219203929,-2.0739136789937,
-2.059231498808,-2.04109563196961),.UNSPECIFIED.);
#2389=B_SPLINE_CURVE_WITH_KNOTS('',3,(#66925,#66926,#66927,#66928,#66929,
#66930,#66931,#66932,#66933,#66934,#66935,#66936),.UNSPECIFIED.,.F.,.F.,
(4,2,2,2,2,4),(-0.0595287291512849,-0.059106780442287,-0.0557582976601512,
-0.0498913034740727,-0.016627889067852,-0.00049195452369095),
 .UNSPECIFIED.);
#2390=B_SPLINE_CURVE_WITH_KNOTS('',3,(#66937,#66938,#66939,#66940,#66941,
#66942,#66943,#66944,#66945,#66946,#66947,#66948,#66949,#66950,#66951,#66952,
#66953,#66954,#66955,#66956,#66957,#66958,#66959,#66960,#66961,#66962,#66963,
#66964,#66965,#66966,#66967,#66968,#66969,#66970,#66971,#66972,#66973,#66974,
#66975,#66976,#66977,#66978,#66979,#66980,#66981,#66982,#66983,#66984,#66985,
#66986,#66987,#66988,#66989,#66990,#66991,#66992,#66993,#66994,#66995,#66996,
#66997,#66998,#66999,#67000,#67001,#67002,#67003,#67004,#67005,#67006,#67007,
#67008,#67009,#67010,#67011,#67012,#67013,#67014,#67015,#67016,#67017,#67018,
#67019,#67020,#67021,#67022,#67023,#67024,#67025,#67026,#67027,#67028,#67029,
#67030,#67031,#67032,#67033,#67034,#67035,#67036,#67037,#67038,#67039,#67040,
#67041,#67042,#67043,#67044,#67045,#67046,#67047,#67048,#67049,#67050,#67051,
#67052,#67053,#67054,#67055,#67056,#67057,#67058,#67059,#67060,#67061,#67062,
#67063,#67064,#67065,#67066,#67067,#67068,#67069,#67070,#67071,#67072,#67073,
#67074,#67075,#67076,#67077,#67078,#67079,#67080,#67081,#67082,#67083,#67084,
#67085,#67086,#67087,#67088,#67089,#67090,#67091,#67092,#67093,#67094,#67095,
#67096,#67097,#67098,#67099,#67100,#67101,#67102,#67103,#67104,#67105,#67106,
#67107,#67108,#67109,#67110,#67111,#67112,#67113,#67114,#67115,#67116,#67117,
#67118,#67119,#67120,#67121,#67122,#67123,#67124,#67125,#67126,#67127,#67128),
 .UNSPECIFIED.,.F.,.F.,(4,2,2,2,2,2,2,2,2,2,2,2,2,2,2,2,2,2,2,2,2,2,2,2,
2,2,2,2,2,2,2,2,2,2,2,2,2,2,2,2,2,2,2,2,2,2,2,2,2,2,2,2,2,2,2,2,2,2,2,2,
2,2,2,2,2,2,2,2,2,2,2,2,2,2,2,2,2,2,2,2,2,2,2,2,2,2,2,2,2,2,2,2,2,2,2,4),
(-2.09972951695153,-2.08762494873157,-2.08160922163102,-2.07926464619698,
-2.07756995289858,-2.07588864726461,-2.07407041354946,-2.0710206138509,
-2.0599397817213,-2.04192034850692,-2.01035678597967,-1.99976485160584,
-1.99556694831247,-1.99256567514997,-1.98983237580441,-1.98544641751165,
-1.97436485107193,-1.93166229369477,-1.92046297263968,-1.91573442843177,
-1.91206766930225,-1.91011685239375,-1.90846990090058,-1.90635882692954,
-1.90176372976302,-1.86272928461758,-1.83584647360384,-1.83031075555954,
-1.82703240618409,-1.82409985914047,-1.82035378996897,-1.81429550014344,
-1.77483027179431,-1.74914995239231,-1.74540675712624,-1.74344009580529,
-1.74179479404348,-1.7396695685506,-1.73511973418902,-1.7040896211669,-1.66971564387023,
-1.66386534967124,-1.66051996650054,-1.65759726293833,-1.65395645029617,
-1.64688811049169,-1.6142995184733,-1.59174317797869,-1.58099321034783,
-1.57807440153557,-1.57628491885698,-1.57460818384061,-1.57253670508038,
-1.56841806937079,-1.53751669813052,-1.50300585905392,-1.49717290596144,
-1.49383125417834,-1.49090822736861,-1.48726231554419,-1.4801689744172,
-1.44927314347284,-1.42544383362372,-1.41799716422669,-1.41282080725194,
-1.41058384417993,-1.40892749041593,-1.4070344668602,-1.40372933182265,
-1.38823677207131,-1.35935394998613,-1.34353633706865,-1.336367767452,-1.3305327051611,
-1.32719065175309,-1.32426774116309,-1.32062258740339,-1.31353269480601,
-1.28226643076721,-1.25872134993977,-1.2513216573233,-1.24616953939659,
-1.24393675552747,-1.24228095677482,-1.24038563639913,-1.23707023673077,
-1.22138033464888,-1.19067429075411,-1.16872688871161,-1.16342661352892,
-1.16019891038352,-1.15725502804261,-1.15347808863828,-1.14717033205657,
-1.11072211711538,-1.10894444197162),.UNSPECIFIED.);
#2391=B_SPLINE_CURVE_WITH_KNOTS('',3,(#67133,#67134,#67135,#67136,#67137,
#67138,#67139,#67140,#67141,#67142,#67143,#67144,#67145,#67146,#67147,#67148,
#67149,#67150,#67151,#67152,#67153,#67154,#67155,#67156,#67157,#67158,#67159,
#67160,#67161,#67162,#67163,#67164,#67165,#67166,#67167,#67168,#67169,#67170,
#67171,#67172,#67173,#67174,#67175,#67176,#67177,#67178,#67179,#67180,#67181,
#67182,#67183,#67184,#67185,#67186,#67187,#67188,#67189,#67190,#67191,#67192,
#67193,#67194,#67195,#67196,#67197,#67198,#67199,#67200,#67201,#67202,#67203,
#67204,#67205,#67206,#67207,#67208,#67209,#67210,#67211,#67212,#67213,#67214,
#67215,#67216,#67217,#67218,#67219,#67220,#67221,#67222,#67223,#67224,#67225,
#67226,#67227,#67228,#67229,#67230,#67231,#67232,#67233,#67234,#67235,#67236,
#67237,#67238,#67239,#67240,#67241,#67242,#67243,#67244,#67245,#67246,#67247,
#67248,#67249,#67250,#67251,#67252,#67253,#67254,#67255,#67256,#67257,#67258,
#67259,#67260,#67261,#67262,#67263,#67264,#67265,#67266,#67267,#67268,#67269,
#67270,#67271,#67272,#67273,#67274,#67275,#67276,#67277,#67278,#67279,#67280,
#67281,#67282,#67283,#67284,#67285,#67286,#67287,#67288,#67289,#67290,#67291,
#67292,#67293,#67294,#67295,#67296,#67297,#67298,#67299,#67300,#67301,#67302,
#67303,#67304,#67305,#67306,#67307,#67308,#67309,#67310,#67311,#67312,#67313,
#67314,#67315,#67316,#67317,#67318,#67319,#67320,#67321,#67322,#67323,#67324,
#67325,#67326,#67327,#67328,#67329,#67330,#67331,#67332,#67333,#67334),
 .UNSPECIFIED.,.F.,.F.,(4,2,2,2,2,2,2,2,2,2,2,2,2,2,2,2,2,2,2,2,2,2,2,2,
2,2,2,2,2,2,2,2,2,2,2,2,2,2,2,2,2,2,2,2,2,2,2,2,2,2,2,2,2,2,2,2,2,2,2,2,
2,2,2,2,2,2,2,2,2,2,2,2,2,2,2,2,2,2,2,2,2,2,2,2,2,2,2,2,2,2,2,2,2,2,2,2,
2,2,2,2,4),(-2.04074305503047,-2.02176080152629,-1.99384987027655,-1.98710611557191,
-1.98462713436291,-1.98293077150667,-1.98114019282429,-1.97821731248195,
-1.96848114424382,-1.9329647641981,-1.91720136870814,-1.91004840441284,
-1.9042230673634,-1.90088266277738,-1.89795889794749,-1.89430964280617,
-1.88720188374861,-1.85636083673836,-1.83251384732456,-1.82506419838601,
-1.81988617265438,-1.81764869367751,-1.81599202616616,-1.81409867224156,
-1.81079296270405,-1.79529482930241,-1.7664215516926,-1.75060743488931,
-1.74343967161567,-1.73760494974324,-1.734262600938,-1.73133912750374,-1.72769285124944,
-1.72059932197814,-1.68974702487582,-1.66589205386159,-1.65844117369326,
-1.65326254347845,-1.65102499052903,-1.64936834343959,-1.64747509951189,
-1.64416976632013,-1.62867836833479,-1.59980717527062,-1.5839882391475,
-1.57681912105258,-1.5709835654804,-1.56764108564395,-1.56471769844216,
-1.56107179312776,-1.55397983344114,-1.5229640496197,-1.49923529656856,
-1.49180522827657,-1.48663734319411,-1.48440165718248,-1.4827452756282,
-1.48085104734367,-1.47754125304301,-1.46195639825263,-1.43191758295835,
-1.41687236308896,-1.40669916778648,-1.40256401223938,-1.39957377750021,
-1.39645793794689,-1.39168439733425,-1.37773034360203,-1.34383483598883,
-1.32426896056079,-1.31972036402197,-1.31759532801764,-1.31610652886066,
-1.31420602388915,-1.31086836948689,-1.29499934795618,-1.26456344967935,
-1.24258072683854,-1.23727798761749,-1.23404945875012,-1.23110523923404,
-1.22732842082489,-1.2210220479472,-1.18455963312416,-1.15609582848917,
-1.15250324513326,-1.15056793435959,-1.1489189499622,-1.14678618252229,
-1.14207156602555,-1.11468307184424,-1.08900037948016,-1.07466390661277,
-1.06998852261704,-1.0668931076755,-1.06392412876924,-1.05974129419506,
-1.05002072744021,-1.03548481317483,-1.00469839400656,-0.991194904658961),
 .UNSPECIFIED.);
#2392=B_SPLINE_CURVE_WITH_KNOTS('',3,(#67335,#67336,#67337,#67338,#67339,
#67340,#67341,#67342,#67343,#67344,#67345,#67346,#67347,#67348,#67349,#67350,
#67351,#67352,#67353,#67354,#67355,#67356,#67357,#67358,#67359,#67360,#67361,
#67362,#67363,#67364,#67365,#67366,#67367,#67368,#67369,#67370,#67371,#67372,
#67373,#67374,#67375,#67376,#67377,#67378,#67379,#67380,#67381,#67382,#67383,
#67384,#67385,#67386,#67387,#67388,#67389,#67390,#67391,#67392,#67393,#67394,
#67395,#67396,#67397,#67398,#67399,#67400,#67401,#67402,#67403,#67404,#67405,
#67406,#67407,#67408,#67409,#67410,#67411,#67412,#67413,#67414,#67415,#67416,
#67417,#67418,#67419,#67420,#67421,#67422,#67423,#67424,#67425,#67426,#67427,
#67428,#67429,#67430,#67431,#67432,#67433,#67434,#67435,#67436,#67437,#67438,
#67439,#67440,#67441,#67442,#67443,#67444,#67445,#67446,#67447,#67448,#67449,
#67450,#67451,#67452,#67453,#67454,#67455,#67456,#67457,#67458,#67459,#67460,
#67461,#67462,#67463,#67464,#67465,#67466,#67467,#67468,#67469,#67470,#67471,
#67472,#67473,#67474,#67475,#67476,#67477,#67478,#67479,#67480,#67481,#67482,
#67483,#67484,#67485,#67486,#67487,#67488,#67489,#67490,#67491,#67492,#67493,
#67494,#67495,#67496,#67497,#67498,#67499,#67500,#67501,#67502,#67503,#67504,
#67505,#67506,#67507,#67508,#67509,#67510,#67511,#67512,#67513,#67514,#67515,
#67516,#67517,#67518,#67519,#67520,#67521,#67522,#67523,#67524,#67525,#67526,
#67527,#67528,#67529,#67530,#67531,#67532,#67533,#67534,#67535,#67536,#67537,
#67538,#67539,#67540,#67541,#67542,#67543,#67544,#67545,#67546,#67547,#67548,
#67549,#67550,#67551,#67552,#67553,#67554,#67555,#67556,#67557,#67558,#67559,
#67560),.UNSPECIFIED.,.F.,.F.,(4,2,2,2,2,2,2,2,2,2,2,2,2,2,2,2,2,2,2,2,
2,2,2,2,2,2,2,2,2,2,2,2,2,2,2,2,2,2,2,2,2,2,2,2,2,2,2,2,2,2,2,2,2,2,2,2,
2,2,2,2,2,2,2,2,2,2,2,2,2,2,2,2,2,2,2,2,2,2,2,2,2,2,2,2,2,2,2,2,2,2,2,2,
2,2,2,2,2,2,2,2,2,2,2,2,2,2,2,2,2,2,2,2,4),(-1.10894444197162,-1.09089037655592,
-1.08415673956179,-1.07935451739902,-1.07718323275036,-1.0755490522122,
-1.07362205003105,-1.07016553621993,-1.05015894330672,-1.00482988921112,
-0.9986247928755,-0.994877149968059,-0.991937411299972,-0.988695082365399,
-0.98332570959186,-0.960135671977726,-0.928328678479021,-0.914931135687885,
-0.911703892112214,-0.909847096522318,-0.908181184114637,-0.90587463306034,
-0.900278591256796,-0.891997440140209,-0.862453253489691,-0.836016300195138,
-0.830390634826198,-0.827093385934435,-0.824457656189739,-0.82088957566476,
-0.813954305730896,-0.788529788800003,-0.761746855292337,-0.748309387119202,
-0.745079594319196,-0.743222243293156,-0.74155650652568,-0.739251122986672,
-0.733662316760718,-0.725395842303092,-0.695965248052592,-0.669394038897802,
-0.663766083718624,-0.660468342903045,-0.657832680934087,-0.654265296671087,
-0.647333552011604,-0.621937100275696,-0.595212690067308,-0.581701278464992,
-0.57846136206839,-0.576601810292879,-0.574936768258777,-0.572636000128682,
-0.56707569812071,-0.558866924475694,-0.52987746694275,-0.502782721339736,
-0.497146456614218,-0.493846937544746,-0.491211528055736,-0.487646677809804,
-0.480727720528842,-0.455432768920035,-0.428921743268478,-0.41509896592003,
-0.411845751260955,-0.409983311383686,-0.408319160044401,-0.406024373637239,
-0.400500848305203,-0.392366270165909,-0.363931998791517,-0.336176653628017,
-0.330529219537321,-0.327227312306831,-0.324592238284008,-0.321030774621129,
-0.314128881203692,-0.288968850040101,-0.262745703274513,-0.24852090429876,
-0.24524096413246,-0.243372730086959,-0.241710296067741,-0.239427261335879,
-0.233975446541185,-0.225984731803385,-0.198590728969246,-0.169517932224578,
-0.163887738783788,-0.160589509162061,-0.157732828173098,-0.157546413679192,
-0.157380327295911,-0.157228306947839,-0.157086037941978,-0.156950352757707,
-0.15681878652873,-0.156689310236186,-0.156560158753731,-0.156429711576455,
-0.152313747556579,-0.140655079980355,-0.122288555785325,-0.0959586558801422,
-0.0818862949928874,-0.0786145565632204,-0.0767481097014717,-0.075085175726414,
-0.0727986058168453,-0.0673252172130096,-0.0593761644650439),
 .UNSPECIFIED.);
#2393=B_SPLINE_CURVE_WITH_KNOTS('',3,(#67566,#67567,#67568,#67569,#67570,
#67571,#67572,#67573,#67574,#67575,#67576,#67577,#67578,#67579,#67580,#67581,
#67582,#67583,#67584,#67585,#67586,#67587,#67588,#67589,#67590,#67591,#67592,
#67593,#67594,#67595,#67596,#67597,#67598,#67599,#67600,#67601,#67602,#67603,
#67604,#67605,#67606,#67607,#67608,#67609,#67610,#67611,#67612,#67613,#67614,
#67615,#67616,#67617,#67618,#67619,#67620,#67621,#67622,#67623,#67624,#67625,
#67626,#67627,#67628,#67629,#67630,#67631,#67632,#67633,#67634,#67635,#67636,
#67637,#67638,#67639,#67640,#67641,#67642,#67643,#67644,#67645,#67646,#67647,
#67648,#67649,#67650,#67651,#67652,#67653,#67654,#67655,#67656,#67657,#67658,
#67659,#67660,#67661,#67662,#67663,#67664,#67665,#67666,#67667,#67668,#67669,
#67670,#67671,#67672,#67673,#67674,#67675,#67676,#67677,#67678,#67679,#67680,
#67681,#67682,#67683,#67684,#67685,#67686,#67687,#67688,#67689,#67690,#67691,
#67692,#67693,#67694,#67695,#67696,#67697,#67698,#67699,#67700,#67701,#67702,
#67703,#67704,#67705,#67706,#67707,#67708,#67709,#67710,#67711,#67712,#67713,
#67714,#67715,#67716,#67717,#67718,#67719,#67720,#67721,#67722,#67723,#67724,
#67725,#67726,#67727,#67728,#67729,#67730,#67731,#67732,#67733,#67734,#67735,
#67736,#67737,#67738,#67739,#67740,#67741,#67742,#67743,#67744,#67745,#67746,
#67747,#67748,#67749,#67750,#67751,#67752,#67753,#67754,#67755,#67756,#67757,
#67758,#67759,#67760,#67761,#67762,#67763,#67764,#67765,#67766,#67767,#67768,
#67769,#67770,#67771,#67772,#67773),.UNSPECIFIED.,.F.,.F.,(4,2,2,2,2,2,
2,2,2,2,2,2,2,2,2,2,2,2,2,2,2,2,2,2,2,2,2,2,2,2,2,2,2,2,2,2,2,2,2,2,2,2,
2,2,2,2,2,2,2,2,2,2,2,2,2,2,2,2,2,2,2,2,2,2,2,2,2,2,2,2,2,2,2,2,2,2,2,2,
2,2,2,2,2,2,2,2,2,2,2,2,2,2,2,2,2,2,2,2,2,2,2,2,2,4),(-0.991238213430677,
-0.976641098909451,-0.971230807864263,-0.967978531114308,-0.965039079154578,
-0.961241742758999,-0.953103229758448,-0.925083580910352,-0.891127935454698,
-0.886797858173586,-0.884713751144305,-0.883070102675632,-0.881068500737586,
-0.877156636841558,-0.872014680897714,-0.859274844728248,-0.828002733313391,
-0.809602906575744,-0.804375953569787,-0.801163009680009,-0.798213051105526,
-0.794335341475655,-0.785743700959912,-0.758090115601303,-0.72450349102752,
-0.720134861275554,-0.71804337759993,-0.716399431371068,-0.714404184847302,
-0.710523612973384,-0.705435001796337,-0.692899901914688,-0.654316896289965,
-0.641653679920653,-0.637036579568481,-0.634260816191678,-0.631290139889179,
-0.627274387086287,-0.617862219996585,-0.604377302909968,-0.582858406290926,
-0.576004895198285,-0.556406456687993,-0.552959641722108,-0.551034353252153,
-0.549399146856339,-0.54722316280081,-0.542397598994321,-0.535620209360751,
-0.51556697007537,-0.479407361604222,-0.473079687412401,-0.469296387173338,
-0.466350689785722,-0.463124164445328,-0.457833101308611,-0.436057485466618,
-0.405583031730287,-0.389553840963494,-0.386209695742535,-0.384307459223142,
-0.382818572822939,-0.380695026841,-0.376155991265821,-0.356683892684253,
-0.323061797240769,-0.308751121174757,-0.303938737272029,-0.300814288931752,
-0.297827927808991,-0.29371776307728,-0.283710276033602,-0.269014953284204,
-0.248834278459128,-0.244849051881725,-0.223158171046896,-0.219672848435838,
-0.217739029785914,-0.216105209456666,-0.213942302507689,-0.209188904993565,
-0.18763574474434,-0.147983885056826,-0.139736774480289,-0.135961189517189,
-0.133016750198675,-0.131759432379266,-0.131703476977391,-0.13157000340885,
-0.131441985762563,-0.131318625722611,-0.131199224891469,-0.13108316602606,
-0.127592372240812,-0.119051126452774,-0.107127561791166,-0.0807651978249793,
-0.0565214939093335,-0.0530212881142028,-0.0510842239026097,-0.0494352662233957,
-0.0472681091763347,-0.0424908150203636,-0.000491816551951527),
 .UNSPECIFIED.);
#2394=B_SPLINE_CURVE_WITH_KNOTS('',3,(#67774,#67775,#67776,#67777,#67778,
#67779,#67780,#67781,#67782,#67783,#67784,#67785,#67786,#67787,#67788,#67789,
#67790,#67791),.UNSPECIFIED.,.F.,.F.,(4,2,2,2,2,2,2,2,4),(-2.09980330258049,
-2.07619390304051,-2.07214372682003,-2.06916417689941,-2.06616224626754,
-2.06306409603706,-2.05837678839064,-2.04518472895466,-2.04074305503047),
 .UNSPECIFIED.);
#2395=B_SPLINE_CURVE_WITH_KNOTS('',3,(#67793,#67794,#67795,#67796,#67797,
#67798,#67799,#67800,#67801,#67802),.UNSPECIFIED.,.F.,.F.,(4,2,2,2,4),(-0.0593761644650439,
-0.0592913074490973,-0.0342070986254461,-0.00945211975966167,-0.00049169905348269),
 .UNSPECIFIED.);
#2396=B_SPLINE_CURVE_WITH_KNOTS('',3,(#67803,#67804,#67805,#67806,#67807,
#67808,#67809,#67810,#67811,#67812,#67813,#67814,#67815,#67816,#67817,#67818,
#67819,#67820,#67821,#67822,#67823,#67824,#67825,#67826,#67827,#67828,#67829,
#67830,#67831,#67832,#67833,#67834,#67835,#67836,#67837,#67838,#67839,#67840,
#67841,#67842,#67843,#67844,#67845,#67846,#67847,#67848,#67849,#67850,#67851,
#67852,#67853,#67854,#67855,#67856,#67857,#67858,#67859,#67860,#67861,#67862,
#67863,#67864,#67865,#67866,#67867,#67868,#67869,#67870,#67871,#67872,#67873,
#67874,#67875,#67876,#67877,#67878,#67879,#67880,#67881,#67882,#67883,#67884,
#67885,#67886,#67887,#67888,#67889,#67890,#67891,#67892,#67893,#67894,#67895,
#67896,#67897,#67898,#67899,#67900,#67901,#67902,#67903,#67904,#67905,#67906,
#67907,#67908,#67909,#67910,#67911,#67912,#67913,#67914,#67915,#67916,#67917,
#67918,#67919,#67920,#67921,#67922,#67923,#67924,#67925,#67926,#67927,#67928,
#67929,#67930,#67931,#67932,#67933,#67934,#67935,#67936,#67937,#67938,#67939,
#67940,#67941,#67942,#67943,#67944,#67945,#67946,#67947,#67948,#67949,#67950,
#67951,#67952,#67953,#67954,#67955,#67956,#67957,#67958,#67959,#67960,#67961,
#67962,#67963,#67964,#67965,#67966,#67967,#67968,#67969,#67970,#67971,#67972,
#67973,#67974,#67975,#67976,#67977,#67978,#67979,#67980,#67981,#67982,#67983,
#67984,#67985,#67986,#67987,#67988,#67989,#67990,#67991,#67992),
 .UNSPECIFIED.,.F.,.F.,(4,2,2,2,2,2,2,2,2,2,2,2,2,2,2,2,2,2,2,2,2,2,2,2,
2,2,2,2,2,2,2,2,2,2,2,2,2,2,2,2,2,2,2,2,2,2,2,2,2,2,2,2,2,2,2,2,2,2,2,2,
2,2,2,2,2,2,2,2,2,2,2,2,2,2,2,2,2,2,2,2,2,2,2,2,2,2,2,2,2,2,2,2,2,2,4),
(-2.10024504072334,-2.09787273841388,-2.09523860874424,-2.09246330528043,
-2.08935977733162,-2.08464641798153,-2.07112934357474,-2.04408003428377,
-2.01566772564429,-2.01200283565764,-2.01005224938009,-2.00840502045651,
-2.00629300155547,-2.00169366717601,-1.97108418808107,-1.93630774981785,
-1.93048139131627,-1.92714074190697,-1.92421698095752,-1.92056803847037,
-1.91346198160399,-1.88096440418894,-1.85837622794891,-1.84761720780912,
-1.8446972972018,-1.8429073874589,-1.84123046149147,-1.83915896107834,-1.83504093330713,
-1.80412213877854,-1.76961599056957,-1.76378213197677,-1.76043994885644,
-1.75751644997828,-1.75386993977086,-1.74677540363776,-1.71588047192911,
-1.6920428168382,-1.68459420820755,-1.67941663649243,-1.67717924779383,
-1.67552261877299,-1.67362932661174,-1.6703238203993,-1.65483216059785,
-1.62594546978692,-1.61012255769803,-1.60295202816064,-1.5971155138448,
-1.59377281327351,-1.59084944358724,-1.58720385745557,-1.58011357497684,
-1.54876799246582,-1.52527567895461,-1.51788419285912,-1.51273609566101,
-1.51050378408327,-1.50884782213758,-1.50695172217838,-1.5036336910992,
-1.48791320988004,-1.45713439125066,-1.43527278329857,-1.42997697129172,
-1.4267498888739,-1.42380521958709,-1.42002539514928,-1.41370856253163,
-1.37739504125981,-1.35746665629243,-1.35071390093406,-1.3459012665092,
-1.34372789953177,-1.34209327888696,-1.34016710917275,-1.33671515486238,
-1.31691095177069,-1.31065234924921,-1.29014526813032,-1.26856989282184,
-1.26329131237934,-1.26006788303582,-1.25712211529855,-1.25333472147441,
-1.24699120920666,-1.21118885186706,-1.18240397849715,-1.17863478312334,
-1.17666264847304,-1.17501765314872,-1.17289908874325,-1.16838552857327,
-1.13691431709602,-1.10919217566827),.UNSPECIFIED.);
#2397=B_SPLINE_CURVE_WITH_KNOTS('',3,(#67997,#67998,#67999,#68000,#68001,
#68002,#68003,#68004,#68005,#68006,#68007,#68008,#68009,#68010,#68011,#68012,
#68013,#68014,#68015,#68016,#68017,#68018,#68019,#68020,#68021,#68022,#68023,
#68024,#68025,#68026,#68027,#68028,#68029,#68030,#68031,#68032,#68033,#68034,
#68035,#68036,#68037,#68038,#68039,#68040,#68041,#68042,#68043,#68044,#68045,
#68046,#68047,#68048,#68049,#68050,#68051,#68052,#68053,#68054,#68055,#68056,
#68057,#68058,#68059,#68060,#68061,#68062,#68063,#68064,#68065,#68066,#68067,
#68068,#68069,#68070,#68071,#68072,#68073,#68074,#68075,#68076,#68077,#68078,
#68079,#68080,#68081,#68082,#68083,#68084,#68085,#68086,#68087,#68088,#68089,
#68090,#68091,#68092,#68093,#68094,#68095,#68096,#68097,#68098,#68099,#68100,
#68101,#68102,#68103,#68104,#68105,#68106,#68107,#68108,#68109,#68110,#68111,
#68112,#68113,#68114,#68115,#68116,#68117,#68118,#68119,#68120,#68121,#68122,
#68123,#68124,#68125,#68126,#68127,#68128,#68129,#68130,#68131,#68132,#68133,
#68134,#68135,#68136,#68137,#68138,#68139,#68140,#68141,#68142,#68143,#68144,
#68145,#68146,#68147,#68148,#68149,#68150,#68151,#68152,#68153,#68154,#68155,
#68156,#68157,#68158,#68159,#68160,#68161,#68162,#68163,#68164,#68165,#68166,
#68167,#68168,#68169,#68170,#68171,#68172,#68173,#68174,#68175,#68176,#68177,
#68178,#68179,#68180,#68181,#68182,#68183,#68184,#68185,#68186,#68187,#68188,
#68189,#68190,#68191,#68192),.UNSPECIFIED.,.F.,.F.,(4,2,2,2,2,2,2,2,2,2,
2,2,2,2,2,2,2,2,2,2,2,2,2,2,2,2,2,2,2,2,2,2,2,2,2,2,2,2,2,2,2,2,2,2,2,2,
2,2,2,2,2,2,2,2,2,2,2,2,2,2,2,2,2,2,2,2,2,2,2,2,2,2,2,2,2,2,2,2,2,2,2,2,
2,2,2,2,2,2,2,2,2,2,2,2,2,2,2,4),(-2.0412663643322,-2.01060717261452,-1.98828790130411,
-1.97511847098684,-1.97112742661626,-1.96803319828237,-1.96508135997042,
-1.9612574310206,-1.95273657878317,-1.91339267278809,-1.89194377310661,
-1.88720010779772,-1.8850386909596,-1.88340469790752,-1.88146914146686,
-1.87797709584422,-1.8548274488637,-1.83760928190919,-1.81269888917485,
-1.80582684315187,-1.80226992237025,-1.79963383762293,-1.79632494669173,
-1.79065101663131,-1.76084503878615,-1.73931689071548,-1.7282336780585,
-1.72353686181082,-1.71988887908675,-1.71794149996365,-1.71629336048578,
-1.71417559231816,-1.70954661352483,-1.67065837436693,-1.64367872984786,
-1.63813790037239,-1.63485759808724,-1.63192394379233,-1.62817732016164,
-1.6203166952437,-1.58023817567784,-1.5585658093168,-1.55380013103779,-1.55163477525613,
-1.55000045310844,-1.54806769301185,-1.54458801201727,-1.5234848008202,
-1.5187966136912,-1.4987575837135,-1.47655718878509,-1.47124012733842,-1.46800770745067,
-1.46506304478681,-1.46128994989667,-1.45499950750342,-1.41822384803917,
-1.39859794336622,-1.38865786258578,-1.38581134779563,-1.384037184282,-1.38234962929046,
-1.379830723386,-1.37332386187274,-1.34126769928369,-1.31543259691161,-1.3067129472373,
-1.30281286390363,-1.29985957088073,-1.29665627485738,-1.29147502602385,
-1.27349368529231,-1.24202474900111,-1.22910099098222,-1.22391134039225,
-1.21997121665099,-1.21796381967116,-1.21632029735965,-1.21424250100709,
-1.20994565330823,-1.17565638974526,-1.1487627648545,-1.14002778855009,
-1.13612517425918,-1.13317162651532,-1.12996966128824,-1.12479418140525,
-1.10689369033933,-1.06939817794942,-1.06025456089091,-1.05424110806619,
-1.05186817121142,-1.05019077942413,-1.04836130290588,-1.04526232091129,
-1.03215413643346,-0.998040183333568,-0.991238213430677),.UNSPECIFIED.);
#2398=B_SPLINE_CURVE_WITH_KNOTS('',3,(#68193,#68194,#68195,#68196,#68197,
#68198,#68199,#68200,#68201,#68202,#68203,#68204,#68205,#68206,#68207,#68208,
#68209,#68210,#68211,#68212,#68213,#68214,#68215,#68216,#68217,#68218,#68219,
#68220,#68221,#68222,#68223,#68224,#68225,#68226,#68227,#68228,#68229,#68230,
#68231,#68232,#68233,#68234,#68235,#68236,#68237,#68238,#68239,#68240,#68241,
#68242,#68243,#68244,#68245,#68246,#68247,#68248,#68249,#68250,#68251,#68252,
#68253,#68254,#68255,#68256,#68257,#68258,#68259,#68260,#68261,#68262,#68263,
#68264,#68265,#68266,#68267,#68268,#68269,#68270,#68271,#68272,#68273,#68274,
#68275,#68276,#68277,#68278,#68279,#68280,#68281,#68282,#68283,#68284,#68285,
#68286,#68287,#68288,#68289,#68290,#68291,#68292,#68293,#68294,#68295,#68296,
#68297,#68298,#68299,#68300,#68301,#68302,#68303,#68304,#68305,#68306,#68307,
#68308,#68309,#68310,#68311,#68312,#68313,#68314,#68315,#68316,#68317,#68318,
#68319,#68320,#68321,#68322,#68323,#68324,#68325,#68326,#68327,#68328,#68329,
#68330,#68331,#68332,#68333,#68334,#68335,#68336,#68337,#68338,#68339,#68340,
#68341,#68342,#68343,#68344,#68345,#68346,#68347,#68348,#68349,#68350,#68351,
#68352,#68353,#68354,#68355,#68356,#68357,#68358,#68359,#68360,#68361,#68362,
#68363,#68364,#68365,#68366,#68367,#68368,#68369,#68370,#68371,#68372,#68373,
#68374,#68375,#68376,#68377,#68378,#68379,#68380,#68381,#68382,#68383,#68384,
#68385,#68386,#68387,#68388,#68389,#68390,#68391,#68392),.UNSPECIFIED.,
 .F.,.F.,(4,2,2,2,2,2,2,2,2,2,2,2,2,2,2,2,2,2,2,2,2,2,2,2,2,2,2,2,2,2,2,
2,2,2,2,2,2,2,2,2,2,2,2,2,2,2,2,2,2,2,2,2,2,2,2,2,2,2,2,2,2,2,2,2,2,2,2,
2,2,2,2,2,2,2,2,2,2,2,2,2,2,2,2,2,2,2,2,2,2,2,2,2,2,2,2,2,2,2,2,4),(-1.10919217566827,
-1.10285109736999,-1.09703854338629,-1.09370097916952,-1.09077710882766,
-1.08712433418365,-1.0799988642058,-1.05011741528275,-1.016673667526,-1.01229135522323,
-1.01019762194584,-1.00855403458269,-1.00656186397993,-1.00269470075188,
-0.997628539458234,-0.985177693009459,-0.947242927744185,-0.933976867973413,
-0.929280727424155,-0.926181092711504,-0.923180991732553,-0.918990174932144,
-0.908446744395041,-0.892613381054371,-0.863756518159548,-0.848295087897,
-0.844991443623137,-0.84309864886408,-0.841442073412207,-0.839204199365472,
-0.834023256276718,-0.826567030450243,-0.802685929930445,-0.771815824415442,
-0.764719877234269,-0.761073243945101,-0.758149946739275,-0.75480832178638,
-0.748976269457675,-0.714573756006922,-0.683572745356013,-0.679022836427378,
-0.676897560246747,-0.675252201047247,-0.673285470285616,-0.669542102515961,
-0.642615199985557,-0.604620306015733,-0.598419830165685,-0.594632581617534,
-0.591695266433446,-0.588439619122877,-0.583010017818449,-0.558639141554511,
-0.547105513424786,-0.517020980839767,-0.512442047091056,-0.510302697376582,
-0.50865319759588,-0.506722874304056,-0.503153394592692,-0.498585490451799,
-0.454907512380181,-0.435164561979905,-0.429857209668909,-0.426628074085135,
-0.42368473772664,-0.419846870705144,-0.411475346106364,-0.389611885824379,
-0.350104274878984,-0.345668989673887,-0.343557720325191,-0.341910995435389,
-0.339960935820364,-0.336296810781593,-0.308459750706929,-0.271382650059542,
-0.265113250095761,-0.261347333872226,-0.258405141660985,-0.255172255417685,
-0.249847029937188,-0.227459982195111,-0.207626394063551,-0.183840506494559,
-0.17909860665286,-0.176961315837899,-0.175312293245642,-0.173381190221304,
-0.169806965046338,-0.14118435153848,-0.104828648157685,-0.0985146312613983,
-0.0947362774301334,-0.0917926116789703,-0.0885664833990601,-0.0832718787415284,
-0.0614035604514639,-0.0593668323253494),.UNSPECIFIED.);
#2399=B_SPLINE_CURVE_WITH_KNOTS('',3,(#68398,#68399,#68400,#68401,#68402,
#68403,#68404,#68405,#68406,#68407,#68408,#68409,#68410,#68411,#68412,#68413,
#68414,#68415,#68416,#68417,#68418,#68419,#68420,#68421,#68422,#68423,#68424,
#68425,#68426,#68427,#68428,#68429,#68430,#68431,#68432,#68433,#68434,#68435,
#68436,#68437,#68438,#68439,#68440,#68441,#68442,#68443,#68444,#68445,#68446,
#68447,#68448,#68449,#68450,#68451,#68452,#68453,#68454,#68455,#68456,#68457,
#68458,#68459,#68460,#68461,#68462,#68463,#68464,#68465,#68466,#68467,#68468,
#68469,#68470,#68471,#68472,#68473,#68474,#68475,#68476,#68477,#68478,#68479,
#68480,#68481,#68482,#68483,#68484,#68485,#68486,#68487,#68488,#68489,#68490,
#68491,#68492,#68493,#68494,#68495,#68496,#68497,#68498,#68499,#68500,#68501,
#68502,#68503,#68504,#68505,#68506,#68507,#68508,#68509,#68510,#68511,#68512,
#68513,#68514,#68515,#68516,#68517,#68518,#68519,#68520,#68521,#68522,#68523,
#68524,#68525,#68526,#68527,#68528,#68529,#68530,#68531,#68532,#68533,#68534,
#68535,#68536,#68537,#68538,#68539,#68540,#68541,#68542,#68543,#68544,#68545,
#68546,#68547,#68548,#68549,#68550,#68551,#68552,#68553,#68554,#68555,#68556,
#68557,#68558,#68559,#68560,#68561,#68562,#68563,#68564,#68565,#68566,#68567,
#68568,#68569,#68570,#68571,#68572,#68573,#68574,#68575,#68576,#68577,#68578,
#68579,#68580,#68581,#68582,#68583,#68584,#68585,#68586,#68587,#68588,#68589,
#68590,#68591,#68592,#68593,#68594,#68595),.UNSPECIFIED.,.F.,.F.,(4,2,2,
2,2,2,2,2,2,2,2,2,2,2,2,2,2,2,2,2,2,2,2,2,2,2,2,2,2,2,2,2,2,2,2,2,2,2,2,
2,2,2,2,2,2,2,2,2,2,2,2,2,2,2,2,2,2,2,2,2,2,2,2,2,2,2,2,2,2,2,2,2,2,2,2,
2,2,2,2,2,2,2,2,2,2,2,2,2,2,2,2,2,2,2,2,2,2,2,4),(-0.991317167272335,-0.971269366237599,
-0.956601880946314,-0.953336414956754,-0.951452096944215,-0.949793172520064,
-0.947538903310674,-0.942262563977142,-0.934620200965425,-0.909575086141311,
-0.8776750491207,-0.87204184857997,-0.868710676257753,-0.865813490371843,
-0.86216424209734,-0.854817562117453,-0.84515866654821,-0.81916330323871,
-0.81766818945004,-0.79230722832396,-0.787549888779139,-0.785409366960424,
-0.783759480653418,-0.781829275791654,-0.778261359027506,-0.749637794469464,
-0.713265210641895,-0.706950799053849,-0.703171613546739,-0.700226932995384,
-0.696999302507008,-0.691701278980093,-0.669796948385164,-0.639023568800072,
-0.623392855537778,-0.62008083009688,-0.618186055919584,-0.616529747807254,
-0.61429485201946,-0.609131861330975,-0.601710497585804,-0.578039612039028,
-0.546909828799278,-0.539816970239891,-0.536170823043493,-0.533247357323859,
-0.529904914376362,-0.524069726140404,-0.516901954488812,-0.501088361452861,
-0.472241543781939,-0.456756494487105,-0.453451685267782,-0.451558545332174,
-0.449901875585303,-0.44766409340259,-0.442484217105164,-0.435030056613093,
-0.411159810067018,-0.380290652944542,-0.373195502510553,-0.3695488869495,
-0.366625389483783,-0.363283283971826,-0.357449669232071,-0.350284368098833,
-0.334479201918933,-0.305630252231526,-0.290134649832783,-0.286829342649177,
-0.284936092182368,-0.283279451215878,-0.281041876037474,-0.275863196291234,
-0.268411356523578,-0.24455522826089,-0.213690410647705,-0.206581480733163,
-0.202932030775213,-0.20000831507877,-0.196668190564797,-0.190843899976307,
-0.157099963228134,-0.125363236630374,-0.120921297079108,-0.118808420797331,
-0.117161188585463,-0.11521138282097,-0.111549863208933,-0.0816363119513023,
-0.0570291304981712,-0.0427557720175263,-0.0379479202928798,-0.0348247944232061,
-0.0318385255683217,-0.028886410225576,-0.0249107123818784,-0.016294700971784,
-0.000491204019444046),.UNSPECIFIED.);
#2400=B_SPLINE_CURVE_WITH_KNOTS('',3,(#68596,#68597,#68598,#68599,#68600,
#68601,#68602,#68603,#68604,#68605,#68606,#68607,#68608,#68609,#68610,#68611,
#68612,#68613),.UNSPECIFIED.,.F.,.F.,(4,2,2,2,2,2,2,2,4),(-2.10008377485422,
-2.05932312996458,-2.05571269775278,-2.05274146765247,-2.05093995362208,
-2.04926853040962,-2.04722042808529,-2.04319839434716,-2.0412663643322),
 .UNSPECIFIED.);
#2401=B_SPLINE_CURVE_WITH_KNOTS('',3,(#68615,#68616,#68617,#68618,#68619,
#68620,#68621,#68622,#68623,#68624,#68625,#68626,#68627,#68628,#68629,#68630,
#68631,#68632),.UNSPECIFIED.,.F.,.F.,(4,2,2,2,2,2,2,2,4),(-0.0593668323253494,
-0.0244934904075403,-0.0142512542297031,-0.0112790705132887,-0.00947813354296127,
-0.00791635031254044,-0.00623769422981492,-0.00362381055065628,-0.000491106187273373),
 .UNSPECIFIED.);
#2402=B_SPLINE_CURVE_WITH_KNOTS('',3,(#68633,#68634,#68635,#68636,#68637,
#68638,#68639,#68640,#68641,#68642,#68643,#68644,#68645,#68646,#68647,#68648,
#68649,#68650,#68651,#68652,#68653,#68654,#68655,#68656,#68657,#68658,#68659,
#68660,#68661,#68662,#68663,#68664,#68665,#68666,#68667,#68668,#68669,#68670,
#68671,#68672,#68673,#68674,#68675,#68676,#68677,#68678,#68679,#68680,#68681,
#68682,#68683,#68684,#68685,#68686,#68687,#68688,#68689,#68690,#68691,#68692,
#68693,#68694,#68695,#68696,#68697,#68698,#68699,#68700,#68701,#68702,#68703,
#68704,#68705,#68706,#68707,#68708,#68709,#68710,#68711,#68712,#68713,#68714,
#68715,#68716,#68717,#68718,#68719,#68720,#68721,#68722,#68723,#68724,#68725,
#68726,#68727,#68728,#68729,#68730,#68731,#68732,#68733,#68734,#68735,#68736,
#68737,#68738,#68739,#68740,#68741,#68742,#68743,#68744,#68745,#68746,#68747,
#68748,#68749,#68750,#68751,#68752,#68753,#68754,#68755,#68756,#68757,#68758,
#68759,#68760,#68761,#68762,#68763,#68764,#68765,#68766,#68767,#68768,#68769,
#68770,#68771,#68772,#68773,#68774,#68775,#68776,#68777,#68778,#68779,#68780,
#68781,#68782,#68783,#68784,#68785,#68786,#68787,#68788,#68789,#68790,#68791,
#68792,#68793,#68794,#68795,#68796,#68797,#68798,#68799,#68800,#68801,#68802,
#68803,#68804,#68805,#68806,#68807,#68808,#68809,#68810,#68811,#68812,#68813,
#68814,#68815,#68816,#68817,#68818,#68819,#68820,#68821,#68822,#68823,#68824,
#68825,#68826,#68827,#68828,#68829,#68830,#68831,#68832,#68833,#68834,#68835,
#68836,#68837,#68838,#68839,#68840,#68841,#68842,#68843,#68844,#68845,#68846),
 .UNSPECIFIED.,.F.,.F.,(4,2,2,2,2,2,2,2,2,2,2,2,2,2,2,2,2,2,2,2,2,2,2,2,
2,2,2,2,2,2,2,2,2,2,2,2,2,2,2,2,2,2,2,2,2,2,2,2,2,2,2,2,2,2,2,2,2,2,2,2,
2,2,2,2,2,2,2,2,2,2,2,2,2,2,2,2,2,2,2,2,2,2,2,2,2,2,2,2,2,2,2,2,2,2,2,2,
2,2,2,2,2,2,2,2,2,2,4),(-2.10004855717667,-2.05968761413315,-2.03975706519315,
-2.03143220897157,-2.02760249894487,-2.0246601144664,-2.02142674536316,
-2.01610008933595,-1.99598846901806,-1.95258145943588,-1.94809650511923,
-1.9455538598408,-1.94340707952417,-1.9433868459708,-1.94336657917876,-1.94334627310399,
-1.94332592166687,-1.94330551860702,-1.94329463534735,-1.94328348333027,
-1.9432720490865,-1.94326031831007,-1.94324827571214,-1.94323590498146,
-1.94322318859647,-1.94321010778596,-1.94160157551812,-1.9397063782228,
-1.93639165246691,-1.92091182682553,-1.89202782939398,-1.87621349707516,
-1.86904587472698,-1.86321140840924,-1.85986947092063,-1.85694653106624,
-1.85330116949128,-1.84621032123755,-1.81504121816665,-1.79142177788148,
-1.78400974459386,-1.77885125434831,-1.77661737146842,-1.77496142847113,
-1.7730667168685,-1.7697540346938,-1.7541090257833,-1.72332658729998,-1.70140266668787,
-1.69610376797199,-1.69287635112243,-1.68993237403934,-1.68615482012498,
-1.67984491880162,-1.64343290472883,-1.62357696288477,-1.61683863647587,
-1.61203390181177,-1.60986215968526,-1.60822792651323,-1.60630121216711,
-1.60284600940396,-1.58289359533735,-1.57631373898952,-1.5546607004643,
-1.53453490564711,-1.52935132810845,-1.52614860385069,-1.5231971947656,
-1.51936790859076,-1.51080920467632,-1.47150948359011,-1.45008520417026,
-1.44534511109266,-1.44318499591757,-1.44155185895655,-1.43961721464028,
-1.43612663783686,-1.4129960351218,-1.39580234125571,-1.37086758946653,
-1.36399403779003,-1.36043791624384,-1.35780307860567,-1.35449662167666,
-1.34882912739601,-1.31805963838061,-1.29321564236277,-1.28477925339823,
-1.27910630227377,-1.27678723158176,-1.27511921296331,-1.27326788565249,
-1.27006640430231,-1.25709197869054,-1.22995706084433,-1.20196211208017,
-1.19638823425894,-1.19310183322284,-1.19017096081421,-1.1864392185505,
-1.18042976981119,-1.13421948993561,-1.11619276436942,-1.11181376051969,
-1.10972075181354,-1.10913504811783),.UNSPECIFIED.);
#2403=B_SPLINE_CURVE_WITH_KNOTS('',3,(#68851,#68852,#68853,#68854,#68855,
#68856,#68857,#68858,#68859,#68860,#68861,#68862,#68863,#68864,#68865,#68866,
#68867,#68868,#68869,#68870,#68871,#68872,#68873,#68874,#68875,#68876,#68877,
#68878,#68879,#68880,#68881,#68882,#68883,#68884,#68885,#68886,#68887,#68888,
#68889,#68890,#68891,#68892,#68893,#68894,#68895,#68896,#68897,#68898,#68899,
#68900,#68901,#68902,#68903,#68904,#68905,#68906,#68907,#68908,#68909,#68910,
#68911,#68912,#68913,#68914,#68915,#68916,#68917,#68918,#68919,#68920,#68921,
#68922,#68923,#68924,#68925,#68926,#68927,#68928,#68929,#68930,#68931,#68932,
#68933,#68934,#68935,#68936,#68937,#68938,#68939,#68940,#68941,#68942,#68943,
#68944,#68945,#68946,#68947,#68948,#68949,#68950,#68951,#68952,#68953,#68954,
#68955,#68956,#68957,#68958,#68959,#68960,#68961,#68962,#68963,#68964,#68965,
#68966,#68967,#68968,#68969,#68970,#68971,#68972,#68973,#68974,#68975,#68976,
#68977,#68978,#68979,#68980,#68981,#68982,#68983,#68984,#68985,#68986,#68987,
#68988,#68989,#68990,#68991,#68992,#68993,#68994,#68995,#68996,#68997,#68998,
#68999,#69000,#69001,#69002,#69003,#69004,#69005,#69006,#69007,#69008,#69009,
#69010,#69011,#69012,#69013,#69014,#69015,#69016,#69017,#69018,#69019,#69020,
#69021,#69022,#69023,#69024,#69025,#69026,#69027,#69028,#69029,#69030,#69031,
#69032,#69033,#69034,#69035,#69036,#69037,#69038,#69039,#69040,#69041,#69042,
#69043,#69044,#69045,#69046,#69047,#69048,#69049,#69050,#69051,#69052,#69053,
#69054,#69055,#69056,#69057,#69058,#69059,#69060,#69061,#69062,#69063,#69064,
#69065,#69066,#69067,#69068,#69069,#69070,#69071,#69072),.UNSPECIFIED.,
 .F.,.F.,(4,2,2,2,2,2,2,2,2,2,2,2,2,2,2,2,2,2,2,2,2,2,2,2,2,2,2,2,2,2,2,
2,2,2,2,2,2,2,2,2,2,2,2,2,2,2,2,2,2,2,2,2,2,2,2,2,2,2,2,2,2,2,2,2,2,2,2,
2,2,2,2,2,2,2,2,2,2,2,2,2,2,2,2,2,2,2,2,2,2,2,2,2,2,2,2,2,2,2,2,2,2,2,2,
2,2,2,2,2,2,2,4),(-2.04101140854792,-2.04046337870567,-2.03653625905841,
-2.03357960775552,-2.03038909176893,-2.02526514219354,-2.00834243620288,
-1.97136839202077,-1.9612482612546,-1.9568258979117,-1.95430708832056,-1.95218567019774,
-1.95216703017222,-1.95214830931894,-1.9521295023838,-1.95211060384299,
-1.95209160806915,-1.95207250935541,-1.95046480157463,-1.94859516110489,
-1.94531075704223,-1.93108870305978,-1.90488147509855,-1.87967340979029,
-1.87276446354262,-1.8692007754161,-1.8665646254764,-1.86326207227536,-1.85761525405566,
-1.82993192835102,-1.80146430773374,-1.79332570216422,-1.78779927473401,
-1.78550352819917,-1.78383873054021,-1.78197561983068,-1.77872121911457,
-1.76497882626153,-1.73366860665032,-1.71034598777799,-1.70496803706325,
-1.7017231267894,-1.69878268551681,-1.69503636317025,-1.68695308718502,
-1.64713531104907,-1.6255469237547,-1.62079014296674,-1.6186267004731,-1.6169928963441,
-1.61505963420629,-1.61157649017881,-1.59014769302804,-1.58584023140218,
-1.56599649612362,-1.54359177332018,-1.53826389971339,-1.53502964742402,
-1.53208635606883,-1.52831921112367,-1.52204815025309,-1.48501177542775,
-1.4573154741099,-1.45356216169409,-1.45159316073597,-1.44994766514024,
-1.44782439748652,-1.44328647981571,-1.4121377777625,-1.37785279325446,
-1.37201179059481,-1.36866793711337,-1.3657443598411,-1.36209954296318,
-1.35501396406215,-1.32333438623621,-1.30010544265524,-1.29275819707013,
-1.28763293603589,-1.2854044257926,-1.28374879282641,-1.28185013881087,
-1.27852129110098,-1.26271797510652,-1.23202119299304,-1.21019098936377,
-1.20489685657338,-1.2016699283642,-1.1987248198463,-1.19494360491054,-1.1886224959578,
-1.15240226435025,-1.13242106683317,-1.12565825687406,-1.12084021722084,
-1.11866575663189,-1.11703087675297,-1.11510502490475,-1.11165499438319,
-1.09192898410201,-1.08515634493058,-1.06398241637997,-1.05030761329503,
-1.04100698586047,-1.03730468635691,-1.03456653400743,-1.03156857619638,
-1.02739150479001,-1.01694276714278,-1.00131402756476,-0.991317167272335),
 .UNSPECIFIED.);
#2404=B_SPLINE_CURVE_WITH_KNOTS('',3,(#69073,#69074,#69075,#69076,#69077,
#69078,#69079,#69080,#69081,#69082,#69083,#69084,#69085,#69086,#69087,#69088,
#69089,#69090,#69091,#69092,#69093,#69094,#69095,#69096,#69097,#69098,#69099,
#69100,#69101,#69102,#69103,#69104,#69105,#69106,#69107,#69108,#69109,#69110,
#69111,#69112,#69113,#69114,#69115,#69116,#69117,#69118,#69119,#69120,#69121,
#69122,#69123,#69124,#69125,#69126,#69127,#69128,#69129,#69130,#69131,#69132,
#69133,#69134,#69135,#69136,#69137,#69138,#69139,#69140,#69141,#69142,#69143,
#69144,#69145,#69146,#69147,#69148,#69149,#69150,#69151,#69152,#69153,#69154,
#69155,#69156,#69157,#69158,#69159,#69160,#69161,#69162,#69163,#69164,#69165,
#69166,#69167,#69168,#69169,#69170,#69171,#69172,#69173,#69174,#69175,#69176,
#69177,#69178,#69179,#69180,#69181,#69182,#69183,#69184,#69185,#69186,#69187,
#69188,#69189,#69190,#69191,#69192,#69193,#69194,#69195,#69196,#69197,#69198,
#69199,#69200,#69201,#69202,#69203,#69204,#69205,#69206,#69207,#69208,#69209,
#69210,#69211,#69212,#69213,#69214,#69215,#69216,#69217,#69218,#69219,#69220,
#69221,#69222,#69223,#69224,#69225,#69226,#69227,#69228,#69229,#69230,#69231,
#69232,#69233,#69234,#69235,#69236,#69237,#69238,#69239,#69240,#69241,#69242,
#69243,#69244,#69245,#69246,#69247,#69248,#69249,#69250,#69251,#69252,#69253,
#69254,#69255,#69256,#69257,#69258,#69259,#69260,#69261,#69262,#69263,#69264,
#69265,#69266,#69267,#69268,#69269,#69270,#69271,#69272,#69273,#69274,#69275,
#69276,#69277,#69278,#69279,#69280,#69281,#69282),.UNSPECIFIED.,.F.,.F.,
(4,2,2,2,2,2,2,2,2,2,2,2,2,2,2,2,2,2,2,2,2,2,2,2,2,2,2,2,2,2,2,2,2,2,2,
2,2,2,2,2,2,2,2,2,2,2,2,2,2,2,2,2,2,2,2,2,2,2,2,2,2,2,2,2,2,2,2,2,2,2,2,
2,2,2,2,2,2,2,2,2,2,2,2,2,2,2,2,2,2,2,2,2,2,2,2,2,2,2,2,2,2,2,2,2,4),(-1.10913504811783,
-1.10823560503746,-1.10631330339019,-1.10287832932864,-1.08370403298245,
-1.05030685623411,-1.03416536900961,-1.02915549735935,-1.02598982139593,
-1.02302460379695,-1.01903794937058,-1.0097982501277,-0.996652896361306,
-0.974781043006941,-0.969710435674911,-0.948164892381695,-0.94468152465253,
-0.942748483825111,-0.941115138832031,-0.938952681783957,-0.934199661955977,
-0.912644467143313,-0.872950197330228,-0.864733254059146,-0.860963676975315,
-0.858020786486407,-0.854789336661378,-0.849471623255825,-0.827221407080959,
-0.807213264855721,-0.802961309911672,-0.781508944026267,-0.778026731674855,
-0.776094023368769,-0.774460754865315,-0.772298132842778,-0.76754373499156,
-0.74597288823947,-0.706227413696758,-0.698866794604389,-0.695167444018825,
-0.692430646405077,-0.689433383240041,-0.685255826313089,-0.674798033122222,
-0.659148240024944,-0.629313387590438,-0.614488009316962,-0.611215445706952,
-0.609329912615716,-0.607672042447271,-0.605422123259851,-0.600168787258228,
-0.592570798251011,-0.567803909265849,-0.538167540447757,-0.531018828690988,
-0.527361765927307,-0.524438140402175,-0.521104833478843,-0.515310066090627,
-0.508205327189741,-0.492604851163101,-0.462266997689265,-0.447827701524631,
-0.44453646012659,-0.442665759508467,-0.441003990244195,-0.438725754101463,
-0.433303165466993,-0.425370829025148,-0.398386656774325,-0.36888498189887,
-0.363210094915109,-0.3599022908539,-0.3572679728734,-0.353714645907345,
-0.346853825140484,-0.322016627510291,-0.304779644281041,-0.281622361172221,
-0.278132616732218,-0.27619829662491,-0.274549670659312,-0.272380386757878,
-0.267588715152776,-0.260873851115541,-0.241139611040287,-0.204522650875372,
-0.19821743862134,-0.194441404982222,-0.191497854760682,-0.188270134535489,
-0.182968924783193,-0.160995004480972,-0.130535732850021,-0.123177334826571,
-0.113800611199239,-0.110916416949167,-0.109134732495719,-0.107433892212634,
-0.104929514194292,-0.0979968478002638,-0.0868051149359963,-0.0595087853850942),
 .UNSPECIFIED.);
#2405=B_SPLINE_CURVE_WITH_KNOTS('',3,(#69288,#69289,#69290,#69291,#69292,
#69293,#69294,#69295,#69296,#69297,#69298,#69299,#69300,#69301,#69302,#69303,
#69304,#69305,#69306,#69307,#69308,#69309,#69310,#69311,#69312,#69313,#69314,
#69315,#69316,#69317,#69318,#69319,#69320,#69321,#69322,#69323,#69324,#69325,
#69326,#69327,#69328,#69329,#69330,#69331,#69332,#69333,#69334,#69335,#69336,
#69337,#69338,#69339,#69340,#69341,#69342,#69343,#69344,#69345,#69346,#69347,
#69348,#69349,#69350,#69351,#69352,#69353,#69354,#69355,#69356,#69357,#69358,
#69359,#69360,#69361,#69362,#69363,#69364,#69365,#69366,#69367,#69368,#69369,
#69370,#69371,#69372,#69373,#69374,#69375,#69376,#69377,#69378,#69379,#69380,
#69381,#69382,#69383,#69384,#69385,#69386,#69387,#69388,#69389,#69390,#69391,
#69392,#69393,#69394,#69395,#69396,#69397,#69398,#69399,#69400,#69401,#69402,
#69403,#69404,#69405,#69406,#69407,#69408,#69409,#69410,#69411,#69412,#69413,
#69414,#69415,#69416,#69417,#69418,#69419,#69420,#69421,#69422,#69423,#69424,
#69425,#69426,#69427,#69428,#69429,#69430,#69431,#69432,#69433,#69434,#69435,
#69436,#69437,#69438,#69439,#69440,#69441,#69442,#69443,#69444,#69445,#69446,
#69447,#69448,#69449,#69450,#69451,#69452,#69453,#69454,#69455,#69456,#69457,
#69458,#69459,#69460,#69461,#69462,#69463,#69464,#69465,#69466,#69467,#69468,
#69469,#69470,#69471,#69472,#69473,#69474,#69475,#69476,#69477,#69478,#69479),
 .UNSPECIFIED.,.F.,.F.,(4,2,2,2,2,2,2,2,2,2,2,2,2,2,2,2,2,2,2,2,2,2,2,2,
2,2,2,2,2,2,2,2,2,2,2,2,2,2,2,2,2,2,2,2,2,2,2,2,2,2,2,2,2,2,2,2,2,2,2,2,
2,2,2,2,2,2,2,2,2,2,2,2,2,2,2,2,2,2,2,2,2,2,2,2,2,2,2,2,2,2,2,2,2,2,2,4),
(-0.991163524485056,-0.983026878049841,-0.946840881123856,-0.940514739899372,
-0.936731902269777,-0.933786305147567,-0.930559626163103,-0.925267700523123,
-0.903476746194706,-0.872928633379073,-0.85698523250164,-0.853644440917111,
-0.851742977510495,-0.850253978123014,-0.848129332477108,-0.843584299672713,
-0.824055904383233,-0.790277106245328,-0.7761488197356,-0.771355848435598,
-0.768235512862652,-0.765246922322243,-0.761123713198903,-0.75103148423286,
-0.736159374155473,-0.716318227516734,-0.711906048239111,-0.690591657393007,
-0.687110183998657,-0.685177241068084,-0.683543325407487,-0.681379204472702,
-0.676618987639848,-0.654996410856421,-0.61508748628777,-0.607064295570715,
-0.603288286669525,-0.600351826229788,-0.597089090892841,-0.591628249201624,
-0.566591761526637,-0.545401491976722,-0.52393317807978,-0.520450148231912,
-0.518516925855081,-0.516883161525052,-0.514719745650531,-0.50996300585608,
-0.488374089218609,-0.448570204691978,-0.44045511065525,-0.43670314900139,
-0.433762050818472,-0.430520289160432,-0.425156685979125,-0.402095391058122,
-0.369991487142957,-0.356731237735257,-0.353512132287395,-0.351656734925377,
-0.349989612670611,-0.347677940578411,-0.342052879929887,-0.333713513013906,
-0.307620851035729,-0.277916229645545,-0.272241940121711,-0.268933628690639,
-0.266298428938596,-0.26274327309274,-0.255876562220893,-0.231000047624151,
-0.213789577352936,-0.190640688277787,-0.187157545067066,-0.185224344104027,
-0.183590653753023,-0.181427408603687,-0.176671321802497,-0.155087942023666,
-0.11530042288264,-0.107172335637809,-0.103418147571817,-0.100476855747706,
-0.0972364734954749,-0.0918789076298382,-0.0689263607924405,-0.0424639151764528,
-0.0276457662303507,-0.0218131531556057,-0.0194033301914297,-0.0177365551928999,
-0.0162021746202994,-0.0143991140069215,-0.0117759024763317,-0.000490981604578286),
 .UNSPECIFIED.);
#2406=B_SPLINE_CURVE_WITH_KNOTS('',3,(#69480,#69481,#69482,#69483,#69484,
#69485,#69486,#69487),.UNSPECIFIED.,.F.,.F.,(4,2,2,4),(-2.10006443375851,
-2.06179515910853,-2.04934439557115,-2.04101140854792),.UNSPECIFIED.);
#2407=B_SPLINE_CURVE_WITH_KNOTS('',3,(#69489,#69490,#69491,#69492,#69493,
#69494,#69495,#69496,#69497,#69498,#69499,#69500,#69501,#69502,#69503,#69504,
#69505,#69506,#69507,#69508),.UNSPECIFIED.,.F.,.F.,(4,2,2,2,2,2,2,2,2,4),
(-0.0595087853850942,-0.058697510888168,-0.0373425346330193,-0.0313459871363057,
-0.0276182118008791,-0.0246879939402665,-0.0219472169507867,-0.0187144205006066,
-0.0116643663455923,-0.000491076436926665),.UNSPECIFIED.);
#2408=B_SPLINE_CURVE_WITH_KNOTS('',3,(#69509,#69510,#69511,#69512,#69513,
#69514,#69515,#69516,#69517,#69518,#69519,#69520,#69521,#69522,#69523,#69524,
#69525,#69526,#69527,#69528,#69529,#69530,#69531,#69532,#69533,#69534,#69535,
#69536,#69537,#69538,#69539,#69540,#69541,#69542,#69543,#69544,#69545,#69546,
#69547,#69548,#69549,#69550,#69551,#69552,#69553,#69554,#69555,#69556,#69557,
#69558,#69559,#69560,#69561,#69562,#69563,#69564,#69565,#69566,#69567,#69568,
#69569,#69570,#69571,#69572,#69573,#69574,#69575,#69576,#69577,#69578,#69579,
#69580,#69581,#69582,#69583,#69584,#69585,#69586,#69587,#69588,#69589,#69590,
#69591,#69592,#69593,#69594,#69595,#69596,#69597,#69598,#69599,#69600,#69601,
#69602,#69603,#69604,#69605,#69606,#69607,#69608,#69609,#69610,#69611,#69612,
#69613,#69614,#69615,#69616,#69617,#69618,#69619,#69620,#69621,#69622,#69623,
#69624,#69625,#69626,#69627,#69628,#69629,#69630,#69631,#69632,#69633,#69634,
#69635,#69636,#69637,#69638,#69639,#69640,#69641,#69642,#69643,#69644,#69645,
#69646,#69647,#69648,#69649,#69650,#69651,#69652,#69653,#69654,#69655,#69656,
#69657,#69658,#69659,#69660,#69661,#69662,#69663,#69664,#69665,#69666,#69667,
#69668,#69669,#69670,#69671,#69672,#69673,#69674,#69675,#69676,#69677,#69678,
#69679,#69680,#69681,#69682,#69683,#69684,#69685,#69686,#69687,#69688,#69689,
#69690,#69691,#69692,#69693,#69694,#69695,#69696,#69697,#69698,#69699,#69700,
#69701,#69702,#69703,#69704,#69705,#69706,#69707,#69708,#69709,#69710),
 .UNSPECIFIED.,.F.,.F.,(4,2,2,2,2,2,2,2,2,2,2,2,2,2,2,2,2,2,2,2,2,2,2,2,
2,2,2,2,2,2,2,2,2,2,2,2,2,2,2,2,2,2,2,2,2,2,2,2,2,2,2,2,2,2,2,2,2,2,2,2,
2,2,2,2,2,2,2,2,2,2,2,2,2,2,2,2,2,2,2,2,2,2,2,2,2,2,2,2,2,2,2,2,2,2,2,2,
2,2,2,2,4),(-2.0999449091563,-2.07666843174284,-2.05663022798428,-2.04985598714527,
-2.04503172429198,-2.04285609986559,-2.04122106328592,-2.03929593936723,
-2.03584933571057,-2.0162658540418,-2.00970872068847,-1.98894044934525,
-1.97479736590467,-1.9681325953507,-1.96270191399168,-1.95952553435962,
-1.95660082664708,-1.95294252311187,-1.9457917166481,-1.91498654752645,
-1.89114436075095,-1.88369465537011,-1.87851638492341,-1.87627874169996,
-1.87462194326698,-1.87272847944043,-1.86942272020192,-1.85393113535256,
-1.82504191296418,-1.80921612105338,-1.80204449518046,-1.79620715621365,
-1.79286407052072,-1.78994041453539,-1.78629453759939,-1.77920390264542,
-1.74782168489845,-1.72435250645261,-1.71696452366693,-1.71181810224293,
-1.70958594355634,-1.70792986295426,-1.70603335916057,-1.70271404796654,
-1.68698096982917,-1.65632445893487,-1.63435970241686,-1.62905735206147,
-1.62582865660556,-1.62288404414013,-1.61910641025159,-1.61279804328298,
-1.57632257064629,-1.55649737904291,-1.5497642500766,-1.54496198523726,
-1.54279035075285,-1.54115576473028,-1.53922811379701,-1.53577004856255,
-1.51573153165179,-1.50922182889146,-1.48754394320841,-1.46744096082619,
-1.46225798541871,-1.4590548516825,-1.45610254825058,-1.45227136855492,
-1.44370518965421,-1.40440103426611,-1.3829730660501,-1.37823193432449,
-1.37607129600652,-1.3744377417672,-1.37250257691791,-1.36901100049347,
-1.34584796857757,-1.3286126925848,-1.30372432040562,-1.29685574863177,
-1.29330005676774,-1.29066467190686,-1.28735640231491,-1.28168294109517,
-1.2519057211615,-1.23044639716875,-1.21929854323627,-1.21458402175456,
-1.2109255560697,-1.20897628078701,-1.20732885317225,-1.20521494849235,
-1.20060545823935,-1.17008388438205,-1.1352766573348,-1.12942594440636,
-1.12608007836878,-1.12315681226014,-1.11951511480466,-1.11244446697478,
-1.10905562449139),.UNSPECIFIED.);
#2409=B_SPLINE_CURVE_WITH_KNOTS('',3,(#69715,#69716,#69717,#69718,#69719,
#69720,#69721,#69722,#69723,#69724,#69725,#69726,#69727,#69728,#69729,#69730,
#69731,#69732,#69733,#69734,#69735,#69736,#69737,#69738,#69739,#69740,#69741,
#69742,#69743,#69744,#69745,#69746,#69747,#69748,#69749,#69750,#69751,#69752,
#69753,#69754,#69755,#69756,#69757,#69758,#69759,#69760,#69761,#69762,#69763,
#69764,#69765,#69766,#69767,#69768,#69769,#69770,#69771,#69772,#69773,#69774,
#69775,#69776,#69777,#69778,#69779,#69780,#69781,#69782,#69783,#69784,#69785,
#69786,#69787,#69788,#69789,#69790,#69791,#69792,#69793,#69794,#69795,#69796,
#69797,#69798,#69799,#69800,#69801,#69802,#69803,#69804,#69805,#69806,#69807,
#69808,#69809,#69810,#69811,#69812,#69813,#69814,#69815,#69816,#69817,#69818,
#69819,#69820,#69821,#69822,#69823,#69824,#69825,#69826,#69827,#69828,#69829,
#69830,#69831,#69832,#69833,#69834,#69835,#69836,#69837,#69838,#69839,#69840,
#69841,#69842,#69843,#69844,#69845,#69846,#69847,#69848,#69849,#69850,#69851,
#69852,#69853,#69854,#69855,#69856,#69857,#69858,#69859,#69860,#69861,#69862,
#69863,#69864,#69865,#69866,#69867,#69868,#69869,#69870,#69871,#69872,#69873,
#69874,#69875,#69876,#69877,#69878,#69879,#69880,#69881,#69882,#69883,#69884,
#69885,#69886,#69887,#69888,#69889,#69890,#69891,#69892,#69893,#69894,#69895,
#69896,#69897,#69898,#69899,#69900,#69901,#69902,#69903,#69904,#69905,#69906,
#69907,#69908,#69909,#69910,#69911,#69912,#69913,#69914,#69915,#69916,#69917,
#69918,#69919,#69920,#69921,#69922),.UNSPECIFIED.,.F.,.F.,(4,2,2,2,2,2,
2,2,2,2,2,2,2,2,2,2,2,2,2,2,2,2,2,2,2,2,2,2,2,2,2,2,2,2,2,2,2,2,2,2,2,2,
2,2,2,2,2,2,2,2,2,2,2,2,2,2,2,2,2,2,2,2,2,2,2,2,2,2,2,2,2,2,2,2,2,2,2,2,
2,2,2,2,2,2,2,2,2,2,2,2,2,2,2,2,2,2,2,2,2,2,2,2,2,4),(-2.04100968074023,
-2.03439341721675,-2.02297208680151,-2.01999681466115,-2.01819454724547,
-2.01652381416569,-2.01409361028992,-2.00813160460378,-1.97558280665141,
-1.94549964499961,-1.93931383584393,-1.93648730330084,-1.93361592778463,
-1.93031666442807,-1.92468625636374,-1.89486258036765,-1.87346874408809,
-1.86226766895491,-1.85753836365978,-1.853870983418,-1.8519197458714,-1.85027236297233,
-1.84816058519643,-1.84356332864188,-1.81294426093334,-1.77816547431661,
-1.77235132864021,-1.76901303600551,-1.76608861529528,-1.76243524726692,
-1.7553088240529,-1.72544357404806,-1.70085180256665,-1.69328148741012,
-1.68804138603088,-1.68579317299043,-1.68413495334223,-1.68224716875178,
-1.67896667939265,-1.66400272486342,-1.63388848960519,-1.61069216619181,
-1.6053206322687,-1.60207697036066,-1.59913599462872,-1.59538671563614,
-1.58728770367076,-1.54748442042224,-1.52590005392727,-1.52114350990261,
-1.51898003055573,-1.51734613570246,-1.51541269050827,-1.51192904273728,
-1.49047240580192,-1.48619489444995,-1.46600864759744,-1.44390691087414,
-1.4385962932408,-1.43536561622489,-1.43242114244946,-1.42864635593185,
-1.42234871711739,-1.38571080260644,-1.36600217559981,-1.35929174677412,
-1.35450159301531,-1.35233201506896,-1.35068270295506,-1.3487470087112,
-1.34525335447357,-1.32166210329583,-1.31974023549024,-1.2997534085865,
-1.27728565163176,-1.27195389524837,-1.26871865536853,-1.26577534259461,
-1.26200937866661,-1.25574300697643,-1.21862978724824,-1.19081885319169,
-1.18717087943119,-1.18522367818891,-1.18357579699012,-1.1814584954005,
-1.17683103946109,-1.13794450673776,-1.11097149976371,-1.10543158939837,
-1.10215179506053,-1.09921857283084,-1.09547247037635,-1.08941581554992,
-1.04993129528466,-1.04347828010905,-1.02384316590393,-1.02039543059192,
-1.01846995372311,-1.0168348062201,-1.01465918681382,-1.00983554628724,
-1.00306172752569,-0.991163524485056),.UNSPECIFIED.);
#2410=B_SPLINE_CURVE_WITH_KNOTS('',3,(#69923,#69924,#69925,#69926,#69927,
#69928,#69929,#69930,#69931,#69932,#69933,#69934,#69935,#69936,#69937,#69938,
#69939,#69940,#69941,#69942,#69943,#69944,#69945,#69946,#69947,#69948,#69949,
#69950,#69951,#69952,#69953,#69954,#69955,#69956,#69957,#69958,#69959,#69960,
#69961,#69962,#69963,#69964,#69965,#69966,#69967,#69968,#69969,#69970,#69971,
#69972,#69973,#69974,#69975,#69976,#69977,#69978,#69979,#69980,#69981,#69982,
#69983,#69984,#69985,#69986,#69987,#69988,#69989,#69990,#69991,#69992,#69993,
#69994,#69995,#69996,#69997,#69998,#69999,#70000,#70001,#70002,#70003,#70004,
#70005,#70006,#70007,#70008,#70009,#70010,#70011,#70012,#70013,#70014,#70015,
#70016,#70017,#70018,#70019,#70020,#70021,#70022,#70023,#70024,#70025,#70026,
#70027,#70028,#70029,#70030,#70031,#70032,#70033,#70034,#70035,#70036,#70037,
#70038,#70039,#70040,#70041,#70042,#70043,#70044,#70045,#70046,#70047,#70048,
#70049,#70050,#70051,#70052,#70053,#70054,#70055,#70056,#70057,#70058,#70059,
#70060,#70061,#70062,#70063,#70064,#70065,#70066,#70067,#70068,#70069,#70070,
#70071,#70072,#70073,#70074,#70075,#70076,#70077,#70078,#70079,#70080,#70081,
#70082,#70083,#70084,#70085,#70086,#70087,#70088,#70089,#70090,#70091,#70092,
#70093,#70094,#70095,#70096,#70097,#70098,#70099,#70100,#70101,#70102,#70103,
#70104,#70105,#70106,#70107,#70108,#70109,#70110,#70111,#70112,#70113,#70114,
#70115,#70116,#70117,#70118,#70119,#70120,#70121,#70122),.UNSPECIFIED.,
 .F.,.F.,(4,2,2,2,2,2,2,2,2,2,2,2,2,2,2,2,2,2,2,2,2,2,2,2,2,2,2,2,2,2,2,
2,2,2,2,2,2,2,2,2,2,2,2,2,2,2,2,2,2,2,2,2,2,2,2,2,2,2,2,2,2,2,2,2,2,2,2,
2,2,2,2,2,2,2,2,2,2,2,2,2,2,2,2,2,2,2,2,2,2,2,2,2,2,2,2,2,2,2,2,4),(-1.10905562449139,
-1.07989244897315,-1.05730042595185,-1.05006129332725,-1.04499207021526,
-1.04279696482964,-1.04114070610046,-1.03924522530671,-1.03584062890829,
-1.0163425517279,-0.984420591344482,-0.967263607724238,-0.962117959284015,
-0.958922924628183,-0.955968117583588,-0.952052472653241,-0.943237867116354,
-0.930915726366584,-0.908812842023499,-0.882916425894852,-0.878169764964598,
-0.876031218996987,-0.874381621456611,-0.872450319227578,-0.868876896109351,
-0.864302653965787,-0.820600428693777,-0.800882681570439,-0.795576107638928,
-0.792346877254098,-0.789403088582272,-0.785564104439011,-0.777187939684759,
-0.755187724277675,-0.715881435606778,-0.711346817088701,-0.709224458103667,
-0.707579373329921,-0.705610585271609,-0.701856962634299,-0.69698258240651,
-0.685250360640255,-0.664060526454366,-0.634967456491648,-0.629321590846922,
-0.625987938810331,-0.623091647262524,-0.619447549811745,-0.612125676554942,
-0.602509287955301,-0.576724986844258,-0.549531944393667,-0.544796766739653,
-0.542660424558333,-0.541011212689661,-0.539078777207386,-0.535499337812354,
-0.50710062650664,-0.470489299967225,-0.464188636666517,-0.460413659685079,
-0.457469975402225,-0.454241134674979,-0.448935820559023,-0.426900089951852,
-0.39720995078659,-0.380724528236157,-0.377362509239088,-0.375456655652501,
-0.373969076554226,-0.371852839288409,-0.367350471909351,-0.348211383825908,
-0.315511320694204,-0.300136343144856,-0.295209195026829,-0.292061234930895,
-0.28908845702985,-0.285054003249958,-0.275520291811714,-0.261790984403908,
-0.240704888547187,-0.233880753958874,-0.214246581124304,-0.210799804236854,
-0.208874988957851,-0.207240509976586,-0.205065977117349,-0.200245586322434,
-0.193477133505267,-0.173466367316549,-0.137203133275546,-0.130905950455872,
-0.127132055051805,-0.124188637422674,-0.120959502684205,-0.116856108227694,
-0.10229688074443,-0.0758263288672487,-0.0592761367658359),
 .UNSPECIFIED.);
#2411=B_SPLINE_CURVE_WITH_KNOTS('',3,(#70128,#70129,#70130,#70131,#70132,
#70133,#70134,#70135,#70136,#70137,#70138,#70139,#70140,#70141,#70142,#70143,
#70144,#70145,#70146,#70147,#70148,#70149,#70150,#70151,#70152,#70153,#70154,
#70155,#70156,#70157,#70158,#70159,#70160,#70161,#70162,#70163,#70164,#70165,
#70166,#70167,#70168,#70169,#70170,#70171,#70172,#70173,#70174,#70175,#70176,
#70177,#70178,#70179,#70180,#70181,#70182,#70183,#70184,#70185,#70186,#70187,
#70188,#70189,#70190,#70191,#70192,#70193,#70194,#70195,#70196,#70197,#70198,
#70199,#70200,#70201,#70202,#70203,#70204,#70205,#70206,#70207,#70208,#70209,
#70210,#70211,#70212,#70213,#70214,#70215,#70216,#70217,#70218,#70219,#70220,
#70221,#70222,#70223,#70224,#70225,#70226,#70227,#70228,#70229,#70230,#70231,
#70232,#70233,#70234,#70235,#70236,#70237,#70238,#70239,#70240,#70241,#70242,
#70243,#70244,#70245,#70246,#70247,#70248,#70249,#70250,#70251,#70252,#70253,
#70254,#70255,#70256,#70257,#70258,#70259,#70260,#70261,#70262,#70263,#70264,
#70265,#70266,#70267,#70268,#70269,#70270,#70271,#70272,#70273,#70274,#70275,
#70276,#70277,#70278,#70279,#70280,#70281,#70282,#70283,#70284,#70285,#70286,
#70287,#70288,#70289,#70290,#70291,#70292,#70293,#70294,#70295,#70296,#70297,
#70298,#70299,#70300,#70301,#70302,#70303,#70304,#70305,#70306,#70307,#70308,
#70309,#70310,#70311,#70312,#70313,#70314,#70315,#70316,#70317,#70318,#70319,
#70320,#70321,#70322,#70323,#70324,#70325,#70326,#70327),.UNSPECIFIED.,
 .F.,.F.,(4,2,2,2,2,2,2,2,2,2,2,2,2,2,2,2,2,2,2,2,2,2,2,2,2,2,2,2,2,2,2,
2,2,2,2,2,2,2,2,2,2,2,2,2,2,2,2,2,2,2,2,2,2,2,2,2,2,2,2,2,2,2,2,2,2,2,2,
2,2,2,2,2,2,2,2,2,2,2,2,2,2,2,2,2,2,2,2,2,2,2,2,2,2,2,2,2,2,2,2,4),(-0.99120270234892,
-0.97052252555347,-0.939735350119543,-0.924083754505977,-0.920770361811558,
-0.9188751846278,-0.917218795782781,-0.914984154366355,-0.909823293709255,
-0.902406274798288,-0.878763406618566,-0.847591871469973,-0.840498787049143,
-0.836852414567577,-0.833928715320508,-0.830585947864055,-0.824750041580279,
-0.817581305133379,-0.801765125299225,-0.772916237343243,-0.757431589785655,
-0.754126589546358,-0.752233312669292,-0.75057650330905,-0.748338506059432,
-0.743158018947439,-0.735702885127382,-0.71182846794561,-0.680959680363722,
-0.673863922219174,-0.67021700265696,-0.667293265511549,-0.663950890391726,
-0.658116816619414,-0.650950957983923,-0.635144597049421,-0.606293257588039,
-0.590796265317911,-0.587490681830606,-0.585597275112588,-0.58394049885595,
-0.581702742875006,-0.576523652940169,-0.569071229829163,-0.54521331101059,
-0.514323087469682,-0.507227541313684,-0.503580669463235,-0.500656940906681,
-0.49731454335963,-0.491480345509626,-0.484314288078922,-0.468507231841814,
-0.439656154821301,-0.424160086011945,-0.420854551289094,-0.418961157710516,
-0.4173043823476,-0.415066613351608,-0.409887432561786,-0.402434828022451,
-0.378575762536819,-0.347687151906452,-0.340591604679309,-0.336944736677004,
-0.334021013336721,-0.330678624071017,-0.324844446784518,-0.317678417953824,
-0.301871443319617,-0.273020404257259,-0.257524299505362,-0.2542187678492,
-0.252325377102621,-0.250668604979746,-0.248430841390909,-0.243251677543792,
-0.235799101082807,-0.211940166784878,-0.181091284246506,-0.173971234913882,
-0.170319325609872,-0.167395208383418,-0.164646527632672,-0.159497944058016,
-0.139876590636164,-0.117778313715728,-0.112151457641064,-0.0911956300773815,
-0.0877194391207717,-0.0857877493419125,-0.0841537775195616,-0.0819881285101866,
-0.077218988696509,-0.0555040962299258,-0.0133614193897104,-0.00693652874026658,
-0.0034762226063785,-0.00170446823000911,-0.000491451950976528),
 .UNSPECIFIED.);
#2412=B_SPLINE_CURVE_WITH_KNOTS('',3,(#70328,#70329,#70330,#70331,#70332,
#70333,#70334,#70335,#70336,#70337,#70338,#70339),.UNSPECIFIED.,.F.,.F.,
(4,2,2,2,2,4),(-2.09993530652335,-2.09836798240351,-2.09573911449367,-2.0897004343036,
-2.05968687098578,-2.04100968074023),.UNSPECIFIED.);
#2413=B_SPLINE_CURVE_WITH_KNOTS('',3,(#70341,#70342,#70343,#70344,#70345,
#70346,#70347,#70348,#70349,#70350,#70351,#70352,#70353,#70354,#70355,#70356,
#70357,#70358),.UNSPECIFIED.,.F.,.F.,(4,2,2,2,2,2,2,2,4),(-0.0592761367658359,
-0.0496220222850414,-0.0448654569977602,-0.0427254520128323,-0.0410760525436666,
-0.0391465757575324,-0.0370769471246982,-0.0337915651063874,-0.000491569424012399),
 .UNSPECIFIED.);
#2414=B_SPLINE_CURVE_WITH_KNOTS('',3,(#70359,#70360,#70361,#70362,#70363,
#70364,#70365,#70366,#70367,#70368,#70369,#70370,#70371,#70372,#70373,#70374,
#70375,#70376,#70377,#70378,#70379,#70380,#70381,#70382,#70383,#70384,#70385,
#70386,#70387,#70388,#70389,#70390,#70391,#70392,#70393,#70394,#70395,#70396,
#70397,#70398,#70399,#70400,#70401,#70402,#70403,#70404,#70405,#70406,#70407,
#70408,#70409,#70410,#70411,#70412,#70413,#70414,#70415,#70416,#70417,#70418,
#70419,#70420,#70421,#70422,#70423,#70424,#70425,#70426,#70427,#70428,#70429,
#70430,#70431,#70432,#70433,#70434,#70435,#70436,#70437,#70438,#70439,#70440,
#70441,#70442,#70443,#70444,#70445,#70446,#70447,#70448,#70449,#70450,#70451,
#70452,#70453,#70454,#70455,#70456,#70457,#70458,#70459,#70460,#70461,#70462,
#70463,#70464,#70465,#70466,#70467,#70468,#70469,#70470,#70471,#70472,#70473,
#70474,#70475,#70476,#70477,#70478,#70479,#70480,#70481,#70482,#70483,#70484,
#70485,#70486,#70487,#70488,#70489,#70490,#70491,#70492,#70493,#70494,#70495,
#70496,#70497,#70498,#70499,#70500,#70501,#70502,#70503,#70504,#70505,#70506,
#70507,#70508,#70509,#70510,#70511,#70512,#70513,#70514,#70515,#70516,#70517,
#70518,#70519,#70520,#70521,#70522,#70523,#70524,#70525,#70526,#70527,#70528,
#70529,#70530,#70531,#70532,#70533,#70534,#70535,#70536,#70537,#70538,#70539,
#70540,#70541,#70542,#70543,#70544,#70545,#70546,#70547,#70548,#70549,#70550),
 .UNSPECIFIED.,.F.,.F.,(4,2,2,2,2,2,2,2,2,2,2,2,2,2,2,2,2,2,2,2,2,2,2,2,
2,2,2,2,2,2,2,2,2,2,2,2,2,2,2,2,2,2,2,2,2,2,2,2,2,2,2,2,2,2,2,2,2,2,2,2,
2,2,2,2,2,2,2,2,2,2,2,2,2,2,2,2,2,2,2,2,2,2,2,2,2,2,2,2,2,2,2,2,2,2,2,4),
(-3.79226700229728,-3.76869309243093,-3.75873057225281,-3.75503207360883,
-3.75217532363195,-3.74923690382806,-3.74598349774788,-3.7405659291042,
-3.71904230119387,-3.6861177964198,-3.67290152969814,-3.66940475781104,
-3.66743175262454,-3.66578672717982,-3.66366901637314,-3.65916039317879,
-3.62759765040527,-3.59368461298066,-3.58783286893347,-3.58448687771056,
-3.58156377063674,-3.57792262239557,-3.57085416670093,-3.54294319709848,
-3.51990632971899,-3.51017510517246,-3.50388851079092,-3.50147502727588,
-3.49979093442464,-3.4979780454196,-3.49495313928996,-3.48415790858637,
-3.45546593040333,-3.42655658270721,-3.42095409978053,-3.41766127227018,
-3.41473100106272,-3.41100867096407,-3.4032750674506,-3.36305414166583,
-3.34133723487464,-3.33656779911085,-3.33440216903122,-3.33275347136614,
-3.3308157274676,-3.32731200828443,-3.30286778409506,-3.29864108845374,
-3.28401949248064,-3.25954979435285,-3.25411463701085,-3.25085755282036,
-3.24792013742936,-3.24413443934036,-3.23794020488466,-3.19989419800612,
-3.17306207259627,-3.16930240833762,-3.16733219363184,-3.16568696971176,
-3.16356576112158,-3.15903832496542,-3.12775840538289,-3.09355822524701,
-3.08772545474756,-3.08438352009275,-3.08146002118793,-3.07781322579846,
-3.07071721640639,-3.03998361348104,-3.01602287067233,-3.00855415536765,
-3.00336625129351,-3.00112710906581,-2.99947026858237,-2.99757798606214,
-2.99427690186518,-2.9788781286353,-2.94974049468255,-2.93400996604774,
-2.92686653039648,-2.92104726342291,-2.91770824027695,-2.91478448473236,
-2.91113368530306,-2.90401799207782,-2.87398594511903,-2.8495040927997,
-2.84195134189891,-2.83672035646905,-2.83447391380086,-2.8328161651913,
-2.83092800895798,-2.82764501847077,-2.81262343738359,-2.8011229575537),
 .UNSPECIFIED.);
#2415=B_SPLINE_CURVE_WITH_KNOTS('',3,(#70555,#70556,#70557,#70558,#70559,
#70560,#70561,#70562,#70563,#70564,#70565,#70566,#70567,#70568,#70569,#70570,
#70571,#70572,#70573,#70574,#70575,#70576,#70577,#70578,#70579,#70580,#70581,
#70582,#70583,#70584,#70585,#70586,#70587,#70588,#70589,#70590,#70591,#70592,
#70593,#70594,#70595,#70596,#70597,#70598,#70599,#70600,#70601,#70602,#70603,
#70604,#70605,#70606,#70607,#70608,#70609,#70610,#70611,#70612,#70613,#70614,
#70615,#70616,#70617,#70618,#70619,#70620,#70621,#70622,#70623,#70624,#70625,
#70626,#70627,#70628,#70629,#70630,#70631,#70632,#70633,#70634,#70635,#70636,
#70637,#70638,#70639,#70640,#70641,#70642,#70643,#70644,#70645,#70646,#70647,
#70648,#70649,#70650,#70651,#70652,#70653,#70654,#70655,#70656,#70657,#70658,
#70659,#70660,#70661,#70662,#70663,#70664,#70665,#70666,#70667,#70668,#70669,
#70670,#70671,#70672,#70673,#70674,#70675,#70676,#70677,#70678,#70679,#70680,
#70681,#70682,#70683,#70684,#70685,#70686,#70687,#70688,#70689,#70690,#70691,
#70692,#70693,#70694,#70695,#70696,#70697,#70698,#70699,#70700,#70701,#70702,
#70703,#70704,#70705,#70706,#70707,#70708,#70709,#70710,#70711,#70712,#70713,
#70714,#70715,#70716,#70717,#70718,#70719,#70720,#70721,#70722,#70723,#70724,
#70725,#70726,#70727,#70728,#70729,#70730,#70731,#70732,#70733,#70734,#70735,
#70736,#70737,#70738,#70739,#70740,#70741,#70742,#70743,#70744,#70745,#70746,
#70747,#70748,#70749,#70750,#70751,#70752,#70753,#70754,#70755,#70756,#70757,
#70758,#70759,#70760,#70761,#70762),.UNSPECIFIED.,.F.,.F.,(4,2,2,2,2,2,
2,2,2,2,2,2,2,2,2,2,2,2,2,2,2,2,2,2,2,2,2,2,2,2,2,2,2,2,2,2,2,2,2,2,2,2,
2,2,2,2,2,2,2,2,2,2,2,2,2,2,2,2,2,2,2,2,2,2,2,2,2,2,2,2,2,2,2,2,2,2,2,2,
2,2,2,2,2,2,2,2,2,2,2,2,2,2,2,2,2,2,2,2,2,2,2,2,2,4),(-2.04091635741276,
-2.01188440141379,-2.00604604582115,-2.0027028119587,-1.99977925725802,
-1.99613378764944,-1.98904474763334,-1.95766446818376,-1.93421060428989,
-1.92682581712301,-1.92168118733302,-1.91944938286909,-1.91779338148413,
-1.9158967080275,-1.91257647188455,-1.8968382004011,-1.8662062219757,-1.84424795757977,
-1.83894632433521,-1.8357178542413,-1.83277329220927,-1.82899548590859,
-1.82268621963769,-1.78626073551712,-1.76641764465789,-1.75968154248347,
-1.75487781196599,-1.75270596542566,-1.75107139944688,-1.74914393610478,
-1.74568652200117,-1.72566178062299,-1.71914866046625,-1.6978608478062,
-1.67742568669057,-1.67222031391028,-1.66901245037617,-1.66606177377225,
-1.66224114435686,-1.65373551905202,-1.61438138215118,-1.592940603598,-1.58819848549181,
-1.58603771825878,-1.58440419154811,-1.58246915722536,-1.57897798674924,
-1.55580604680546,-1.53855216395096,-1.51370641022303,-1.50684367675923,
-1.50328923016203,-1.5006540324295,-1.49734502271663,-1.49166775627426,
-1.463070649468,-1.43539023864011,-1.42735975105312,-1.42188719356276,-1.41960028864593,
-1.41793681308113,-1.41606941644598,-1.41279514919074,-1.39869421968225,
-1.3723603288208,-1.3494621286389,-1.34105924791458,-1.33721511682368,-1.33427020961318,
-1.33104253967295,-1.32574493653194,-1.30619974878455,-1.26241174157648,
-1.25566851990902,-1.25318956160024,-1.25149316267505,-1.24970249091616,
-1.2467793601807,-1.2370413872218,-1.22916886224959,-1.19970539116409,-1.17765134840756,
-1.17234377523831,-1.16911388030224,-1.16616943053372,-1.16239372201584,
-1.15609238692101,-1.11952338704043,-1.09977209988514,-1.09305356543346,
-1.08825914618606,-1.08608888036663,-1.08445437127228,-1.08252561457446,
-1.07906278484435,-1.05881614755769,-1.05029467111737,-1.01396627163369,
-1.00764867838686,-1.003868430845,-1.00092340556157,-0.997695887130462,
-0.992399184576247,-0.99120270234892),.UNSPECIFIED.);
#2416=B_SPLINE_CURVE_WITH_KNOTS('',3,(#70763,#70764,#70765,#70766,#70767,
#70768,#70769,#70770,#70771,#70772,#70773,#70774,#70775,#70776,#70777,#70778,
#70779,#70780,#70781,#70782,#70783,#70784,#70785,#70786,#70787,#70788,#70789,
#70790,#70791,#70792,#70793,#70794,#70795,#70796,#70797,#70798,#70799,#70800,
#70801,#70802,#70803,#70804,#70805,#70806,#70807,#70808,#70809,#70810,#70811,
#70812,#70813,#70814,#70815,#70816,#70817,#70818,#70819,#70820,#70821,#70822,
#70823,#70824,#70825,#70826,#70827,#70828,#70829,#70830,#70831,#70832,#70833,
#70834,#70835,#70836,#70837,#70838,#70839,#70840,#70841,#70842,#70843,#70844,
#70845,#70846,#70847,#70848,#70849,#70850,#70851,#70852,#70853,#70854,#70855,
#70856,#70857,#70858,#70859,#70860,#70861,#70862,#70863,#70864,#70865,#70866,
#70867,#70868,#70869,#70870,#70871,#70872,#70873,#70874,#70875,#70876,#70877,
#70878,#70879,#70880,#70881,#70882,#70883,#70884,#70885,#70886,#70887,#70888,
#70889,#70890,#70891,#70892,#70893,#70894,#70895,#70896,#70897,#70898,#70899,
#70900,#70901,#70902,#70903,#70904,#70905,#70906,#70907,#70908,#70909,#70910,
#70911,#70912,#70913,#70914,#70915,#70916,#70917,#70918,#70919,#70920,#70921,
#70922,#70923,#70924,#70925,#70926,#70927,#70928,#70929,#70930,#70931,#70932,
#70933,#70934,#70935,#70936,#70937,#70938,#70939,#70940,#70941,#70942,#70943,
#70944,#70945,#70946,#70947,#70948,#70949,#70950,#70951,#70952,#70953,#70954,
#70955,#70956,#70957,#70958,#70959,#70960,#70961,#70962,#70963,#70964,#70965,
#70966),.UNSPECIFIED.,.F.,.F.,(4,2,2,2,2,2,2,2,2,2,2,2,2,2,2,2,2,2,2,2,
2,2,2,2,2,2,2,2,2,2,2,2,2,2,2,2,2,2,2,2,2,2,2,2,2,2,2,2,2,2,2,2,2,2,2,2,
2,2,2,2,2,2,2,2,2,2,2,2,2,2,2,2,2,2,2,2,2,2,2,2,2,2,2,2,2,2,2,2,2,2,2,2,
2,2,2,2,2,2,2,2,2,4),(-2.8011229575537,-2.78201200322399,-2.75931380357193,
-2.75396983018629,-2.7507324431721,-2.74779056166631,-2.74403110375789,
-2.73778613865376,-2.7003798056338,-2.67286380037986,-2.66918924645564,
-2.66723676339263,-2.66558993475131,-2.66348092555206,-2.65889735871189,
-2.62816051076856,-2.59350948324537,-2.58767554299368,-2.58433349504516,
-2.5814102199381,-2.57776412729436,-2.57067084939012,-2.53969193573025,
-2.5159220617994,-2.50848483988439,-2.50331322692069,-2.50107695364546,
-2.49942056148905,-2.4975268568489,-2.49421918710097,-2.47867860536094,
-2.44977528617931,-2.43399856307833,-2.42684173657609,-2.4210140261735,
-2.41767333674605,-2.41474996701798,-2.41110207207943,-2.40399985778457,
-2.37365955652556,-2.34940500599255,-2.34188894447155,-2.33667684138815,
-2.33443368952596,-2.33277645504829,-2.3308866901916,-2.32759625015505,
-2.31241645765007,-2.28346467734357,-2.26747742931689,-2.25686425335046,
-2.25266320235526,-2.24966134668931,-2.24692864066463,-2.24254611002863,
-2.23148686410769,-2.1949111663011,-2.17252573584712,-2.16904399777374,
-2.16713220022499,-2.16547953798074,-2.16331186084413,-2.15858497934311,
-2.13261461629105,-2.11057936863224,-2.09827401605867,-2.08946926238429,
-2.0855554898841,-2.08260116725428,-2.07940576609371,-2.07425752039094,
-2.05706600201563,-2.0252071235108,-2.00730754564543,-2.00294293579344,
-2.00085262050588,-1.99936767593071,-1.99744320189741,-1.99399889126439,
-1.9744865486143,-1.96754022107747,-1.94602522857578,-1.93251513734213,
-1.92309164822183,-1.91907459867671,-1.91610427769247,-1.91332981030916,
-1.90871713231743,-1.89608118171501,-1.87465946199703,-1.84057714992198,
-1.8362615595842,-1.83418062354002,-1.83253765966788,-1.83053475220116,
-1.82661407884321,-1.82145657163933,-1.80865474801016,-1.77730579185153,
-1.75902463604075,-1.75382443359162,-1.75130590682506),.UNSPECIFIED.);
#2417=B_SPLINE_CURVE_WITH_KNOTS('',3,(#70972,#70973,#70974,#70975,#70976,
#70977,#70978,#70979,#70980,#70981,#70982,#70983,#70984,#70985,#70986,#70987,
#70988,#70989,#70990,#70991,#70992,#70993,#70994,#70995,#70996,#70997,#70998,
#70999,#71000,#71001,#71002,#71003,#71004,#71005,#71006,#71007,#71008,#71009,
#71010,#71011,#71012,#71013,#71014,#71015,#71016,#71017,#71018,#71019,#71020,
#71021,#71022,#71023,#71024,#71025,#71026,#71027,#71028,#71029,#71030,#71031,
#71032,#71033,#71034,#71035,#71036,#71037,#71038,#71039,#71040,#71041,#71042,
#71043,#71044,#71045,#71046,#71047,#71048,#71049,#71050,#71051,#71052,#71053,
#71054,#71055,#71056,#71057,#71058,#71059,#71060,#71061,#71062,#71063,#71064,
#71065,#71066,#71067,#71068,#71069,#71070,#71071,#71072,#71073,#71074,#71075,
#71076,#71077,#71078,#71079,#71080,#71081,#71082,#71083,#71084,#71085,#71086,
#71087,#71088,#71089,#71090,#71091,#71092,#71093,#71094,#71095,#71096,#71097,
#71098,#71099,#71100,#71101,#71102,#71103,#71104,#71105),.UNSPECIFIED.,
 .F.,.F.,(4,2,2,2,2,2,2,2,2,2,2,2,2,2,2,2,2,2,2,2,2,2,2,2,2,2,2,2,2,2,2,
2,2,2,2,2,2,2,2,2,2,2,2,2,2,2,2,2,2,2,2,2,2,2,2,2,2,2,2,2,2,2,2,2,2,2,4),
(-0.70148998943205,-0.674345982124341,-0.669634945455482,-0.667508045624986,
-0.665860654918974,-0.66392105878315,-0.660327484968321,-0.631872921662852,
-0.595208727900692,-0.588883875984432,-0.585091036444246,-0.582131102575772,
-0.578881721765312,-0.573535203379432,-0.551080372117306,-0.522334388217699,
-0.507846378871563,-0.503479856208418,-0.501339156663809,-0.499631792915702,
-0.497824610182475,-0.494927290037092,-0.484780961145284,-0.464415855447431,
-0.43024241330435,-0.423924288357904,-0.42012594748679,-0.417154262742281,
-0.413883542885037,-0.408480900672828,-0.385371235409442,-0.353258122573531,
-0.339703210370992,-0.33650341488823,-0.334637737794428,-0.333038569022195,
-0.330913764757876,-0.325971684055829,-0.318891048670801,-0.296964711156488,
-0.260800289639285,-0.253654577622875,-0.250133257313443,-0.247329437297859,
-0.244147924441893,-0.238664866797341,-0.20809129696095,-0.176127965725983,
-0.169958056443735,-0.167532591865511,-0.165880672760035,-0.164092500729214,
-0.161545039821543,-0.153204821355754,-0.138616386182872,-0.106317607615673,
-0.0858385280892805,-0.080091366127395,-0.0765419995099983,-0.0732636428181496,
-0.0689097683989476,-0.0588996440771098,-0.0327532108786773,-0.00751310391364335,
-0.0032923198447157,-0.00149869915253042,-2.71738506628892E-6),
 .UNSPECIFIED.);
#2418=B_SPLINE_CURVE_WITH_KNOTS('',3,(#71108,#71109,#71110,#71111,#71112,
#71113,#71114,#71115,#71116,#71117,#71118,#71119,#71120,#71121,#71122,#71123,
#71124,#71125,#71126,#71127,#71128,#71129,#71130,#71131,#71132,#71133,#71134,
#71135,#71136,#71137,#71138,#71139,#71140,#71141,#71142,#71143,#71144,#71145,
#71146,#71147,#71148,#71149,#71150,#71151,#71152,#71153,#71154,#71155,#71156,
#71157,#71158,#71159,#71160,#71161,#71162,#71163,#71164,#71165,#71166,#71167,
#71168,#71169,#71170,#71171,#71172,#71173,#71174,#71175,#71176,#71177,#71178,
#71179,#71180,#71181,#71182,#71183,#71184,#71185,#71186,#71187,#71188,#71189,
#71190,#71191,#71192,#71193,#71194,#71195,#71196,#71197,#71198,#71199,#71200,
#71201,#71202,#71203,#71204,#71205,#71206,#71207,#71208,#71209,#71210,#71211,
#71212,#71213,#71214,#71215,#71216,#71217,#71218,#71219,#71220,#71221,#71222,
#71223,#71224,#71225,#71226,#71227,#71228,#71229,#71230,#71231,#71232,#71233,
#71234,#71235,#71236,#71237,#71238,#71239,#71240,#71241,#71242,#71243,#71244,
#71245,#71246,#71247,#71248,#71249,#71250,#71251,#71252,#71253,#71254,#71255,
#71256,#71257,#71258,#71259,#71260,#71261,#71262,#71263,#71264,#71265,#71266,
#71267,#71268,#71269,#71270,#71271,#71272,#71273,#71274,#71275,#71276,#71277,
#71278,#71279,#71280,#71281,#71282,#71283,#71284,#71285,#71286,#71287,#71288,
#71289,#71290,#71291,#71292,#71293,#71294,#71295,#71296,#71297,#71298,#71299,
#71300,#71301,#71302,#71303,#71304,#71305,#71306,#71307,#71308,#71309),
 .UNSPECIFIED.,.F.,.F.,(4,2,2,2,2,2,2,2,2,2,2,2,2,2,2,2,2,2,2,2,2,2,2,2,
2,2,2,2,2,2,2,2,2,2,2,2,2,2,2,2,2,2,2,2,2,2,2,2,2,2,2,2,2,2,2,2,2,2,2,2,
2,2,2,2,2,2,2,2,2,2,2,2,2,2,2,2,2,2,2,2,2,2,2,2,2,2,2,2,2,2,2,2,2,2,2,2,
2,2,2,2,4),(-1.97976470944902,-1.9789712957795,-1.97074210865653,-1.93649408360935,
-1.91058676406563,-1.90504851710588,-1.90174802558588,-1.89878194842719,
-1.89497249570069,-1.88876114646882,-1.84487804431934,-1.82653872045245,
-1.82209852679182,-1.82038768953402,-1.82033407244368,-1.82028049490831,
-1.8202261642487,-1.8201701514512,-1.82011129453788,-1.82004803697691,-1.8199781321918,
-1.8198980424709,-1.81980152783548,-1.81967551012305,-1.81957959146175,
-1.81797039159875,-1.81583786265784,-1.81107867663494,-1.78734873691932,
-1.76750359022668,-1.74521560180538,-1.73987704677321,-1.73662860265687,
-1.73366700024715,-1.72986851373612,-1.72352627521349,-1.68717785705456,
-1.65852384971955,-1.65489808386762,-1.65295131809612,-1.65130413467331,
-1.64918560379227,-1.64469069652582,-1.61372580922956,-1.57916926509896,
-1.57340079941526,-1.57008337888019,-1.56717457013396,-1.56353770564219,
-1.5564364795931,-1.52588130075209,-1.50157454603749,-1.49405384932749,
-1.48884432047777,-1.48660977662906,-1.48495885435688,-1.48307271734828,
-1.47979937055345,-1.46498187316288,-1.43913539251414,-1.41412704498556,
-1.40723837650883,-1.40367550035633,-1.40103594761735,-1.39772381672729,
-1.39204657758675,-1.36003638674829,-1.33522098697313,-1.32391346182469,
-1.32094309913931,-1.31913907659717,-1.31746480371394,-1.31541036793998,
-1.3113658157162,-1.27921958619855,-1.25664684563837,-1.24335503377768,
-1.23879707130675,-1.23572440008365,-1.23273601301409,-1.22845400895434,
-1.21805065760952,-1.18081533402403,-1.15817687343832,-1.15468855825223,
-1.15277487992886,-1.15112250965675,-1.14895719108698,-1.14424089400683,
-1.11903185060416,-1.09613103324159,-1.08387831592845,-1.0751019600958,
-1.07119397330868,-1.06824145213024,-1.06504555872083,-1.05989114519951,
-1.0423194907008,-1.01063738401214,-0.991343892686251,-0.991336294305795),
 .UNSPECIFIED.);
#2419=B_SPLINE_CURVE_WITH_KNOTS('',3,(#71315,#71316,#71317,#71318),
 .UNSPECIFIED.,.F.,.F.,(4,4),(112.182489717842,112.611961982353),
 .UNSPECIFIED.);
#2420=B_SPLINE_CURVE_WITH_KNOTS('',3,(#71321,#71322,#71323,#71324,#71325,
#71326,#71327,#71328,#71329,#71330,#71331,#71332,#71333,#71334,#71335,#71336,
#71337,#71338,#71339,#71340,#71341,#71342,#71343,#71344,#71345,#71346,#71347,
#71348,#71349,#71350,#71351),.UNSPECIFIED.,.F.,.F.,(4,3,3,3,3,3,3,3,3,3,
4),(112.181968561873,112.285773547054,112.391790609764,112.495346290868,
112.598849283204,112.70233481629,112.810228624402,112.913851302595,113.017547311481,
113.121411318193,113.133910048737),.UNSPECIFIED.);
#2421=B_SPLINE_CURVE_WITH_KNOTS('',3,(#71357,#71358,#71359,#71360,#71361,
#71362,#71363,#71364,#71365,#71366,#71367,#71368,#71369,#71370,#71371,#71372,
#71373,#71374,#71375,#71376,#71377,#71378,#71379,#71380,#71381,#71382,#71383,
#71384,#71385,#71386,#71387,#71388,#71389,#71390,#71391,#71392,#71393,#71394,
#71395,#71396,#71397,#71398,#71399,#71400,#71401,#71402,#71403,#71404,#71405,
#71406,#71407,#71408,#71409,#71410,#71411,#71412,#71413,#71414,#71415,#71416,
#71417,#71418,#71419,#71420,#71421,#71422,#71423,#71424,#71425,#71426,#71427,
#71428,#71429,#71430,#71431,#71432,#71433,#71434,#71435,#71436,#71437,#71438,
#71439,#71440,#71441,#71442,#71443,#71444,#71445,#71446,#71447,#71448,#71449,
#71450,#71451,#71452,#71453,#71454,#71455,#71456,#71457,#71458,#71459,#71460,
#71461,#71462,#71463,#71464,#71465,#71466,#71467,#71468,#71469,#71470,#71471,
#71472,#71473,#71474,#71475,#71476,#71477),.UNSPECIFIED.,.F.,.F.,(4,3,3,
3,3,3,3,3,3,3,3,3,3,3,3,3,3,3,3,3,3,3,3,3,3,3,3,3,3,3,3,3,3,3,3,3,3,3,3,
3,4),(105.89914045238,106.003024818123,106.106864217443,106.21069337325,
106.314717723871,106.4186920148,106.522861290385,106.626790775734,106.730987270237,
106.835028779578,106.938948573574,107.042803099337,107.146627117888,107.250455346994,
107.354392395691,107.458388390263,107.562566344703,107.62431931017,107.728406109515,
107.832337400558,107.936146731458,108.039890701015,108.143604231727,108.24732220283,
108.351150101919,108.455037404766,108.559108574838,108.621847844607,108.726214073937,
108.830424660313,108.934511746338,109.038532366638,109.142521041264,109.24651224564,
109.350608598025,109.454762056837,109.559092885886,109.619376379043,109.74029827114,
109.860139236864,109.955742676496),.UNSPECIFIED.);
#2422=B_SPLINE_CURVE_WITH_KNOTS('',3,(#71478,#71479,#71480,#71481,#71482,
#71483),.UNSPECIFIED.,.F.,.F.,(4,1,1,4),(109.955742875643,110.61690491348,
111.614433447917,112.182489717842),.UNSPECIFIED.);
#2423=B_SPLINE_CURVE_WITH_KNOTS('',3,(#71485,#71486,#71487,#71488,#71489,
#71490,#71491,#71492,#71493,#71494,#71495,#71496,#71497,#71498,#71499,#71500,
#71501,#71502,#71503,#71504,#71505,#71506,#71507,#71508,#71509,#71510,#71511,
#71512,#71513,#71514,#71515,#71516,#71517,#71518,#71519,#71520,#71521,#71522,
#71523,#71524,#71525,#71526,#71527,#71528,#71529,#71530,#71531,#71532,#71533,
#71534,#71535,#71536,#71537,#71538,#71539,#71540,#71541,#71542,#71543,#71544,
#71545,#71546,#71547,#71548,#71549,#71550,#71551,#71552,#71553,#71554),
 .UNSPECIFIED.,.F.,.F.,(4,3,3,3,3,3,3,3,3,3,3,3,3,3,3,3,3,3,3,3,3,3,3,4),
(109.955742875643,110.103311094288,110.16088031869,110.264967038889,110.368898250683,
110.472707502544,110.576451393231,110.680164845351,110.783882738247,110.887710560244,
110.991597786505,111.095668881621,111.158408853127,111.262775121087,111.366985745707,
111.471072869233,111.575093526554,111.679082237674,111.783073477966,111.887169865156,
111.991323358195,112.095654220209,112.155937387564,112.181968561873),
 .UNSPECIFIED.);
#2424=B_SPLINE_CURVE_WITH_KNOTS('',3,(#71555,#71556,#71557,#71558,#71559,
#71560,#71561,#71562,#71563,#71564,#71565,#71566,#71567,#71568,#71569,#71570,
#71571,#71572,#71573,#71574,#71575,#71576,#71577,#71578,#71579,#71580,#71581,
#71582,#71583,#71584,#71585,#71586,#71587,#71588,#71589,#71590,#71591,#71592,
#71593,#71594,#71595,#71596,#71597,#71598,#71599,#71600,#71601,#71602,#71603,
#71604,#71605,#71606,#71607,#71608,#71609,#71610,#71611,#71612,#71613,#71614,
#71615,#71616,#71617,#71618,#71619,#71620,#71621,#71622,#71623,#71624,#71625,
#71626,#71627,#71628,#71629,#71630,#71631,#71632,#71633,#71634,#71635,#71636,
#71637,#71638,#71639,#71640,#71641,#71642,#71643,#71644,#71645,#71646,#71647,
#71648,#71649,#71650,#71651,#71652,#71653,#71654,#71655,#71656,#71657,#71658,
#71659,#71660,#71661,#71662,#71663,#71664,#71665,#71666,#71667,#71668,#71669,
#71670,#71671,#71672,#71673,#71674,#71675,#71676,#71677,#71678),
 .UNSPECIFIED.,.F.,.F.,(4,3,3,3,3,3,3,3,3,3,3,3,3,3,3,3,3,3,3,3,3,3,3,3,
3,3,3,3,3,3,3,3,3,3,3,3,3,3,3,3,3,4),(105.898025479477,106.002009805234,
106.106176853772,106.170766180944,106.274954664328,106.378987943816,106.482899226787,
106.586745073159,106.690560258285,106.794379514107,106.89830744101,107.002294216394,
107.106462900374,107.168294715381,107.27246889384,107.37648781455,107.48038472832,
107.584216206841,107.688017046587,107.791822000632,107.895735790654,107.999708500798,
108.103863385519,108.165823249817,108.270028207098,108.374077867905,108.478005318162,
108.581867191257,108.685698240133,108.789533174159,108.893476390757,108.997478259752,
109.101661565735,109.163351784254,109.266012653708,109.368536787086,109.470961003165,
109.573321976682,109.675698137509,109.778078174934,109.88056960646,109.955742875311),
 .UNSPECIFIED.);
#2425=B_SPLINE_CURVE_WITH_KNOTS('',3,(#71684,#71685,#71686,#71687,#71688,
#71689,#71690,#71691,#71692,#71693,#71694,#71695,#71696,#71697,#71698,#71699,
#71700,#71701,#71702,#71703,#71704,#71705,#71706,#71707,#71708,#71709,#71710,
#71711,#71712,#71713,#71714,#71715,#71716,#71717,#71718,#71719,#71720,#71721,
#71722,#71723,#71724,#71725,#71726,#71727,#71728,#71729,#71730,#71731,#71732,
#71733,#71734,#71735,#71736,#71737,#71738,#71739,#71740,#71741,#71742,#71743,
#71744,#71745,#71746,#71747,#71748,#71749,#71750,#71751,#71752,#71753,#71754,
#71755,#71756,#71757,#71758,#71759,#71760,#71761,#71762,#71763,#71764,#71765,
#71766,#71767,#71768,#71769,#71770,#71771,#71772,#71773,#71774,#71775,#71776,
#71777,#71778,#71779,#71780,#71781,#71782,#71783,#71784,#71785,#71786,#71787,
#71788,#71789,#71790,#71791,#71792,#71793,#71794,#71795,#71796,#71797,#71798,
#71799,#71800,#71801,#71802,#71803,#71804,#71805,#71806,#71807,#71808,#71809,
#71810),.UNSPECIFIED.,.F.,.F.,(4,3,3,3,3,3,3,3,3,3,3,3,3,3,3,3,3,3,3,3,
3,3,3,3,3,3,3,3,3,3,3,3,3,3,3,3,3,3,3,3,3,3,4),(99.6152316583351,99.6440910346774,
99.7482776243203,99.8523089801499,99.956218304806,100.060062172602,100.163875361992,
100.267692607994,100.371618517795,100.47560326894,100.579769939687,100.641619569114,
100.745806326823,100.849837855208,100.953747358172,101.05759140772,101.161404782005,
101.265222215752,101.36914831629,101.473133260145,101.577300124576,101.639148103551,
101.743333059261,101.847362780412,101.951270477105,102.055112721953,102.158924295754,
102.262739935879,102.366664265581,102.470647448779,102.574812587739,102.636676637987,
102.740864888811,102.844897897912,102.948808856351,103.052654345051,103.156469140193,
103.260287974509,103.36421543532,103.46820171878,103.57236987585,103.634205172424,
103.672557568463),.UNSPECIFIED.);
#2426=B_SPLINE_CURVE_WITH_KNOTS('',3,(#71811,#71812,#71813,#71814,#71815,
#71816,#71817,#71818,#71819,#71820,#71821,#71822,#71823,#71824,#71825,#71826,
#71827,#71828,#71829,#71830,#71831,#71832,#71833,#71834,#71835,#71836,#71837,
#71838,#71839,#71840,#71841,#71842,#71843,#71844,#71845,#71846,#71847,#71848,
#71849,#71850,#71851,#71852,#71853,#71854,#71855,#71856,#71857,#71858,#71859,
#71860,#71861,#71862,#71863,#71864,#71865,#71866,#71867,#71868,#71869,#71870,
#71871,#71872,#71873,#71874,#71875,#71876,#71877,#71878,#71879,#71880),
 .UNSPECIFIED.,.F.,.F.,(4,3,3,3,3,3,3,3,3,3,3,3,3,3,3,3,3,3,3,3,3,3,3,4),
(103.672557568736,103.776099132589,103.883053454373,103.986323986313,104.089534944656,
104.192721974449,104.295920683386,104.399231129595,104.502608916411,104.606156372049,
104.63173370686,104.73590789905,104.839926833507,104.943823760987,105.047655253186,
105.151456106561,105.255261074165,105.359174877546,105.463147600957,105.567302498657,
105.629262241297,105.733461685671,105.837495282119,105.89914045238),
 .UNSPECIFIED.);
#2427=B_SPLINE_CURVE_WITH_KNOTS('',3,(#71882,#71883,#71884,#71885,#71886,
#71887,#71888,#71889,#71890,#71891,#71892,#71893,#71894,#71895,#71896,#71897,
#71898,#71899,#71900,#71901,#71902,#71903,#71904,#71905,#71906,#71907,#71908,
#71909,#71910,#71911,#71912,#71913,#71914,#71915,#71916,#71917,#71918,#71919,
#71920,#71921,#71922,#71923,#71924,#71925,#71926,#71927,#71928,#71929,#71930,
#71931,#71932,#71933,#71934,#71935,#71936,#71937,#71938,#71939,#71940,#71941,
#71942,#71943,#71944,#71945,#71946,#71947,#71948),.UNSPECIFIED.,.F.,.F.,
(4,3,3,3,3,3,3,3,3,3,3,3,3,3,3,3,3,3,3,3,3,3,4),(103.672557568463,103.781092799078,
103.889920272668,103.998901192476,104.108175818866,104.175709112071,104.27989406565,
104.38392378467,104.487831479238,104.591673721967,104.695485293658,104.799300931684,
104.903225259319,105.007208440466,105.111373577421,105.173237646507,105.277400211996,
105.381419535078,105.485330619066,105.589186541108,105.693004652181,105.796876386701,
105.898025479477),.UNSPECIFIED.);
#2428=B_SPLINE_CURVE_WITH_KNOTS('',3,(#71949,#71950,#71951,#71952,#71953,
#71954,#71955,#71956,#71957,#71958,#71959,#71960,#71961,#71962,#71963,#71964,
#71965,#71966,#71967,#71968,#71969,#71970,#71971,#71972,#71973,#71974,#71975,
#71976,#71977,#71978,#71979,#71980,#71981,#71982,#71983,#71984,#71985,#71986,
#71987,#71988,#71989,#71990,#71991,#71992,#71993,#71994,#71995,#71996,#71997,
#71998,#71999,#72000,#72001,#72002,#72003,#72004,#72005,#72006,#72007,#72008,
#72009,#72010,#72011,#72012,#72013,#72014,#72015,#72016,#72017,#72018,#72019,
#72020,#72021,#72022,#72023,#72024,#72025,#72026,#72027,#72028,#72029,#72030,
#72031,#72032,#72033,#72034,#72035,#72036,#72037,#72038,#72039,#72040,#72041,
#72042,#72043,#72044,#72045,#72046,#72047,#72048,#72049,#72050,#72051,#72052,
#72053,#72054,#72055,#72056,#72057,#72058,#72059,#72060,#72061,#72062,#72063,
#72064,#72065,#72066,#72067,#72068,#72069,#72070,#72071,#72072),
 .UNSPECIFIED.,.F.,.F.,(4,3,3,3,3,3,3,3,3,3,3,3,3,3,3,3,3,3,3,3,3,3,3,3,
3,3,3,3,3,3,3,3,3,3,3,3,3,3,3,3,3,4),(99.6156110745197,99.7194228471478,
99.8232425494864,99.9271733259419,100.031166424027,100.135337925974,100.185594974324,
100.289781443823,100.393812681112,100.497721890145,100.601565644175,100.705378721806,
100.809195858211,100.913121662433,101.017106310105,101.121272881802,101.183123508761,
101.287309756461,101.391340771478,101.495249758603,101.599093291071,101.70290614781,
101.806723064315,101.910648651658,102.014633083828,102.118799444536,102.180652043198,
102.284838633001,102.388869988989,102.492779313799,102.596623181746,102.700436371284,
102.804253617431,102.908179527372,103.012164278654,103.116330949532,103.178180577634,
103.287930451836,103.397356063165,103.506584798252,103.615565393999,103.672557568099),
 .UNSPECIFIED.);
#2429=B_SPLINE_CURVE_WITH_KNOTS('',3,(#72078,#72079,#72080,#72081,#72082,
#72083,#72084,#72085,#72086,#72087,#72088,#72089,#72090,#72091,#72092,#72093,
#72094,#72095,#72096,#72097,#72098,#72099,#72100,#72101,#72102,#72103,#72104,
#72105,#72106,#72107,#72108,#72109,#72110,#72111,#72112,#72113,#72114,#72115,
#72116,#72117,#72118,#72119,#72120,#72121,#72122,#72123,#72124,#72125,#72126,
#72127,#72128,#72129,#72130,#72131,#72132,#72133,#72134,#72135,#72136,#72137,
#72138,#72139,#72140,#72141,#72142,#72143,#72144,#72145,#72146,#72147,#72148,
#72149,#72150,#72151,#72152,#72153,#72154,#72155,#72156,#72157,#72158,#72159,
#72160,#72161,#72162,#72163,#72164,#72165,#72166,#72167,#72168,#72169,#72170,
#72171,#72172,#72173,#72174,#72175,#72176,#72177,#72178,#72179,#72180,#72181,
#72182,#72183,#72184,#72185,#72186,#72187,#72188,#72189,#72190,#72191,#72192,
#72193,#72194,#72195,#72196,#72197,#72198,#72199,#72200,#72201,#72202,#72203,
#72204),.UNSPECIFIED.,.F.,.F.,(4,3,3,3,3,3,3,3,3,3,3,3,3,3,3,3,3,3,3,3,
3,3,3,3,3,3,3,3,3,3,3,3,3,3,3,3,3,3,3,3,3,3,4),(93.3317416580215,93.4356900192302,
93.5397112742701,93.643900786555,93.6589198280578,93.7631062483201,93.867137435993,
93.9710465950891,94.0748902990131,94.1787033264443,94.2825204126297,94.3864461669516,
94.4904307648287,94.5945972874411,94.6564483624944,94.7606347887222,94.8646659824197,
94.9685751475987,95.0724188576377,95.1762318912073,95.2800489835447,95.3839747439967,
95.4879593480006,95.5921258766681,95.653976896931,95.7581632966032,95.862194463707,
95.9661036023635,96.0699472859383,96.1737602931401,96.2775773592453,96.3815030938508,
96.4854876721868,96.5896541757464,96.6515054313676,96.7545601138494,96.8574737138164,
96.9602826553637,97.0675550568436,97.1702894267471,97.2730248741062,97.3758310709812,
97.3893722612835),.UNSPECIFIED.);
#2430=B_SPLINE_CURVE_WITH_KNOTS('',3,(#72205,#72206,#72207,#72208,#72209,
#72210,#72211,#72212,#72213,#72214,#72215,#72216,#72217,#72218,#72219,#72220,
#72221,#72222,#72223,#72224,#72225,#72226,#72227,#72228,#72229,#72230,#72231,
#72232,#72233,#72234,#72235,#72236,#72237,#72238,#72239,#72240,#72241,#72242,
#72243,#72244,#72245,#72246,#72247,#72248,#72249,#72250,#72251,#72252,#72253,
#72254,#72255,#72256,#72257,#72258,#72259,#72260,#72261,#72262,#72263,#72264,
#72265,#72266,#72267,#72268,#72269,#72270,#72271),.UNSPECIFIED.,.F.,.F.,
(4,3,3,3,3,3,3,3,3,3,3,3,3,3,3,3,3,3,3,3,3,3,4),(97.3893722615608,97.5221133460531,
97.6490339658042,97.7532204351774,97.8572516723404,97.9611608812461,98.0650046351491,
98.1688177126537,98.2726348489321,98.3765606530284,98.4805453005753,98.5847118721504,
98.6465625002408,98.7507507727395,98.8588108834389,98.9627158777129,99.0665559339089,
99.170365829106,99.2741802971821,99.3780947558165,99.4820689265879,99.5862024307738,
99.6152316583351),.UNSPECIFIED.);
#2431=B_SPLINE_CURVE_WITH_KNOTS('',3,(#72273,#72274,#72275,#72276,#72277,
#72278,#72279,#72280,#72281,#72282,#72283,#72284,#72285,#72286,#72287,#72288,
#72289,#72290,#72291,#72292,#72293,#72294,#72295,#72296,#72297,#72298,#72299,
#72300,#72301,#72302,#72303,#72304,#72305,#72306,#72307,#72308,#72309,#72310,
#72311,#72312,#72313,#72314,#72315,#72316,#72317,#72318,#72319,#72320,#72321,
#72322,#72323,#72324,#72325,#72326,#72327,#72328,#72329,#72330,#72331,#72332,
#72333,#72334,#72335,#72336,#72337,#72338,#72339),.UNSPECIFIED.,.F.,.F.,
(4,3,3,3,3,3,3,3,3,3,3,3,3,3,3,3,3,3,3,3,3,3,4),(97.389372261676,97.4918503890726,
97.5942398116719,97.6965771923013,97.7988991181528,97.9013122938702,98.0037702234387,
98.1064116156427,98.1905379054512,98.2947243050817,98.3987554721441,98.5026646107592,
98.6065082942927,98.7103213014536,98.8141383675183,98.9180641020837,99.0220486803801,
99.1262151839011,99.1880664398878,99.2949525985458,99.3989655198962,99.507288297208,
99.6156110745197),.UNSPECIFIED.);
#2432=B_SPLINE_CURVE_WITH_KNOTS('',3,(#72340,#72341,#72342,#72343,#72344,
#72345,#72346,#72347,#72348,#72349,#72350,#72351,#72352,#72353,#72354,#72355,
#72356,#72357,#72358,#72359,#72360,#72361,#72362,#72363,#72364,#72365,#72366,
#72367,#72368,#72369,#72370,#72371,#72372,#72373,#72374,#72375,#72376,#72377,
#72378,#72379,#72380,#72381,#72382,#72383,#72384,#72385,#72386,#72387,#72388,
#72389,#72390,#72391,#72392,#72393,#72394,#72395,#72396,#72397,#72398,#72399,
#72400,#72401,#72402,#72403,#72404,#72405,#72406,#72407,#72408,#72409,#72410,
#72411,#72412,#72413,#72414,#72415,#72416,#72417,#72418,#72419,#72420,#72421,
#72422,#72423,#72424,#72425,#72426,#72427,#72428,#72429,#72430,#72431,#72432,
#72433,#72434,#72435,#72436,#72437,#72438,#72439,#72440,#72441,#72442,#72443,
#72444,#72445,#72446,#72447,#72448,#72449,#72450,#72451,#72452,#72453,#72454,
#72455,#72456,#72457,#72458,#72459,#72460,#72461,#72462,#72463),
 .UNSPECIFIED.,.F.,.F.,(4,3,3,3,3,3,3,3,3,3,3,3,3,3,3,3,3,3,3,3,3,3,3,3,
3,3,3,3,3,3,3,3,3,3,3,3,3,3,3,3,3,4),(93.3327269082001,93.4411890156382,
93.5450756538202,93.648906907013,93.7527175377309,93.8565422751658,93.9604818352646,
94.0644892683557,94.1686696740169,94.2004237677048,94.3046101879005,94.4086413755316,
94.5125505346222,94.6163942385629,94.7202072660329,94.8240243522793,94.9279501066946,
95.0319347046836,95.1361012274356,95.1979523021414,95.3021387192142,95.40616990372,
95.5100790596968,95.6139227605325,95.7177357849108,95.8215528680832,95.9254786194727,
96.0294632144584,96.1336297342753,96.195480836578,96.2996672568408,96.4036984445142,
96.5076076036108,96.6114513075351,96.7152643349665,96.8190814211525,96.9230071754745,
97.0269917733517,97.1311582959642,97.1930093710146,97.3433995555511,97.3893722612835),
 .UNSPECIFIED.);
#2433=B_SPLINE_CURVE_WITH_KNOTS('',3,(#72469,#72470,#72471,#72472,#72473,
#72474,#72475,#72476,#72477,#72478,#72479,#72480,#72481,#72482,#72483,#72484,
#72485,#72486,#72487,#72488,#72489,#72490,#72491,#72492,#72493,#72494,#72495,
#72496,#72497,#72498,#72499,#72500,#72501,#72502,#72503,#72504,#72505,#72506,
#72507,#72508,#72509,#72510,#72511,#72512,#72513,#72514,#72515,#72516,#72517,
#72518,#72519,#72520,#72521,#72522,#72523,#72524,#72525,#72526,#72527,#72528,
#72529,#72530,#72531,#72532,#72533,#72534,#72535,#72536,#72537,#72538,#72539,
#72540,#72541,#72542,#72543,#72544,#72545,#72546,#72547,#72548,#72549,#72550,
#72551,#72552,#72553,#72554,#72555,#72556,#72557,#72558,#72559,#72560,#72561,
#72562,#72563,#72564,#72565,#72566,#72567,#72568,#72569,#72570,#72571,#72572,
#72573,#72574,#72575,#72576,#72577,#72578,#72579,#72580,#72581,#72582,#72583,
#72584,#72585,#72586,#72587,#72588,#72589),.UNSPECIFIED.,.F.,.F.,(4,3,3,
3,3,3,3,3,3,3,3,3,3,3,3,3,3,3,3,3,3,3,3,3,3,3,3,3,3,3,3,3,3,3,3,3,3,3,3,
3,4),(87.0493885891151,87.1532100516366,87.2570212569905,87.3612030981024,
87.465159835495,87.5694542284666,87.6737486214382,87.777935040701,87.8819662273946,
87.985875385546,88.0897190885468,88.1935321150776,88.297349200387,88.401274953875,
88.505259550941,88.6094260727864,88.6712771558748,88.7754635752621,88.879494762081,
88.983403920358,89.0872476234846,89.1910606501414,89.2948777355764,89.3988034891889,
89.5027880863789,89.6069546083463,89.6688056903114,89.7729921093414,89.8770232958027,
89.9809324537241,90.0847761564964,90.1885891828006,90.2924062678855,90.3963320211534,
90.5003166180017,90.6044831396355,90.666334224748,90.7790776483314,90.8915379903038,
91.003544787262,91.1061869538187),.UNSPECIFIED.);
#2434=B_SPLINE_CURVE_WITH_KNOTS('',3,(#72590,#72591,#72592,#72593,#72594,
#72595,#72596,#72597,#72598,#72599,#72600,#72601,#72602,#72603,#72604,#72605,
#72606,#72607,#72608,#72609,#72610,#72611,#72612,#72613,#72614,#72615,#72616,
#72617,#72618,#72619,#72620,#72621,#72622,#72623,#72624,#72625,#72626,#72627,
#72628,#72629,#72630,#72631,#72632,#72633,#72634,#72635,#72636,#72637,#72638,
#72639,#72640,#72641,#72642,#72643,#72644,#72645,#72646,#72647,#72648,#72649,
#72650,#72651,#72652,#72653,#72654,#72655,#72656,#72657,#72658,#72659),
 .UNSPECIFIED.,.F.,.F.,(4,3,3,3,3,3,3,3,3,3,3,3,3,3,3,3,3,3,3,3,3,3,3,4),
(91.1061869541039,91.2126211265267,91.3191385231275,91.4258526676074,91.5326811228729,
91.639729802547,91.6638627591846,91.7680491793775,91.872080367006,91.9759895260938,
92.0798332300317,92.1836462574988,92.2874633437425,92.391389098155,92.4953736961413,
92.5995402188908,92.6613912936212,92.7655571769362,92.8695782420278,92.9734895025819,
93.0773351539067,93.1811423844738,93.2849757131635,93.3317416580215),
 .UNSPECIFIED.);
#2435=B_SPLINE_CURVE_WITH_KNOTS('',3,(#72661,#72662,#72663,#72664,#72665,
#72666,#72667,#72668,#72669,#72670,#72671,#72672,#72673,#72674,#72675,#72676,
#72677,#72678,#72679,#72680,#72681,#72682,#72683,#72684,#72685,#72686,#72687,
#72688,#72689,#72690,#72691,#72692,#72693,#72694,#72695,#72696,#72697,#72698,
#72699,#72700,#72701,#72702,#72703,#72704,#72705,#72706,#72707,#72708,#72709,
#72710,#72711,#72712,#72713,#72714,#72715,#72716,#72717,#72718,#72719,#72720,
#72721,#72722,#72723,#72724,#72725,#72726,#72727,#72728,#72729,#72730),
 .UNSPECIFIED.,.F.,.F.,(4,3,3,3,3,3,3,3,3,3,3,3,3,3,3,3,3,3,3,3,3,3,3,4),
(91.1061869541039,91.207838164395,91.3120245837827,91.4160557706021,91.5199649288795,
91.6238086320066,91.7276216586639,91.8314387440995,91.9353644977125,92.0393490949027,
92.1435156168706,92.2053666988316,92.3095531178609,92.4135843043219,92.5174934622426,
92.6213371650143,92.7251501913177,92.8289672764019,92.9328930296692,93.0368776265167,
93.1410441481497,93.2028952332682,93.3070788474255,93.3327269082001),
 .UNSPECIFIED.);
#2436=B_SPLINE_CURVE_WITH_KNOTS('',3,(#72731,#72732,#72733,#72734,#72735,
#72736,#72737,#72738,#72739,#72740,#72741,#72742,#72743,#72744,#72745,#72746,
#72747,#72748,#72749,#72750,#72751,#72752,#72753,#72754,#72755,#72756,#72757,
#72758,#72759,#72760,#72761,#72762,#72763,#72764,#72765,#72766,#72767,#72768,
#72769,#72770,#72771,#72772,#72773,#72774,#72775,#72776,#72777,#72778,#72779,
#72780,#72781,#72782,#72783,#72784,#72785,#72786,#72787,#72788,#72789,#72790,
#72791,#72792,#72793,#72794,#72795,#72796,#72797,#72798,#72799,#72800,#72801,
#72802,#72803,#72804,#72805,#72806,#72807,#72808,#72809,#72810,#72811,#72812,
#72813,#72814,#72815,#72816,#72817,#72818,#72819,#72820,#72821,#72822,#72823,
#72824,#72825,#72826,#72827,#72828,#72829,#72830,#72831,#72832,#72833,#72834,
#72835,#72836,#72837,#72838,#72839,#72840,#72841,#72842,#72843,#72844,#72845,
#72846,#72847,#72848,#72849,#72850,#72851,#72852,#72853,#72854),
 .UNSPECIFIED.,.F.,.F.,(4,3,3,3,3,3,3,3,3,3,3,3,3,3,3,3,3,3,3,3,3,3,3,3,
3,3,3,3,3,3,3,3,3,3,3,3,3,3,3,3,3,4),(87.048449830443,87.1526150420814,
87.2177240266486,87.3219104459154,87.4259416326135,87.5298507907696,87.6336944937754,
87.7375075203115,87.8413246056263,87.94525035912,88.0492349561916,88.153401478043,
88.2152525610852,88.3194389803687,88.4234701670835,88.5273793252564,88.631223028279,
88.7350360548318,88.8388531401634,88.9427788936735,89.0467634907616,89.1509300126291,
89.2127810955218,89.3169675147651,89.4209987014398,89.5249078595728,89.6287515625556,
89.7325645890689,89.8363816743613,89.9403074278329,90.0442920248827,90.148458546713,
90.2103096299584,90.3131827203155,90.4158805807012,90.5184806860292,90.6210195310318,
90.7235335248246,90.8261208448598,90.9287446854243,91.031530543581,91.1061869536405),
 .UNSPECIFIED.);
#2437=B_SPLINE_CURVE_WITH_KNOTS('',3,(#72860,#72861,#72862,#72863,#72864,
#72865,#72866,#72867,#72868,#72869,#72870,#72871,#72872,#72873,#72874,#72875,
#72876,#72877,#72878,#72879,#72880,#72881,#72882,#72883,#72884,#72885,#72886,
#72887,#72888,#72889,#72890,#72891,#72892,#72893,#72894,#72895,#72896,#72897,
#72898,#72899,#72900,#72901,#72902,#72903,#72904,#72905,#72906,#72907,#72908,
#72909,#72910,#72911,#72912,#72913,#72914,#72915,#72916,#72917,#72918,#72919,
#72920,#72921,#72922,#72923,#72924,#72925,#72926,#72927,#72928,#72929,#72930,
#72931,#72932,#72933,#72934,#72935,#72936,#72937,#72938,#72939,#72940,#72941,
#72942,#72943,#72944,#72945,#72946,#72947,#72948,#72949,#72950,#72951,#72952,
#72953,#72954,#72955,#72956,#72957,#72958,#72959,#72960,#72961,#72962,#72963,
#72964,#72965,#72966,#72967,#72968,#72969,#72970,#72971,#72972,#72973,#72974,
#72975,#72976,#72977,#72978,#72979,#72980),.UNSPECIFIED.,.F.,.F.,(4,3,3,
3,3,3,3,3,3,3,3,3,3,3,3,3,3,3,3,3,3,3,3,3,3,3,3,3,3,3,3,3,3,3,3,3,3,3,3,
3,4),(80.7662045566408,80.8702751277622,80.9742087489547,81.0780672044894,
81.1818852914194,81.2856977535908,81.3896126710214,81.4935777339141,81.5977339197861,
81.6885774148186,81.7927638340869,81.8967950207865,82.0007041789442,82.1045478819516,
82.2083609084892,82.3121779938057,82.416103747301,82.5200883443743,82.6242548662274,
82.6861059492552,82.7902923685257,82.8943235552275,82.9982327133873,83.1020764163968,
83.2058894429366,83.3097065282552,83.4136322817526,83.517616878828,83.6217834006831,
83.6836344836918,83.7878209029578,83.8918520896552,83.9957612478106,84.0996049508158,
84.2034179773513,84.3072350626658,84.4111608161589,84.5151454132301,84.6193119350812,
84.6811630181284,84.8230016469245),.UNSPECIFIED.);
#2438=B_SPLINE_CURVE_WITH_KNOTS('',3,(#72981,#72982,#72983,#72984,#72985,
#72986,#72987,#72988,#72989,#72990,#72991,#72992,#72993,#72994,#72995,#72996,
#72997,#72998,#72999,#73000,#73001,#73002,#73003,#73004,#73005,#73006,#73007,
#73008,#73009,#73010,#73011,#73012,#73013,#73014,#73015,#73016,#73017,#73018,
#73019,#73020,#73021,#73022,#73023,#73024,#73025,#73026,#73027,#73028,#73029,
#73030,#73031,#73032,#73033,#73034,#73035,#73036,#73037,#73038,#73039,#73040,
#73041,#73042,#73043,#73044,#73045,#73046,#73047,#73048,#73049,#73050),
 .UNSPECIFIED.,.F.,.F.,(4,3,3,3,3,3,3,3,3,3,3,3,3,3,3,3,3,3,3,3,3,3,3,4),
(84.8230016473369,84.9299628854904,85.0323879596834,85.1347430254586,85.2370647046656,
85.3393895675522,85.4418181479453,85.5443082329609,85.6469663801132,85.678691552565,
85.7828779718483,85.8869091585631,85.9908183167359,86.0946620197583,86.1984750463112,
86.3022921316428,86.4062178851529,86.5102024822409,86.6143690041083,86.6762200870016,
86.7803789666147,86.8844021488383,86.9883093146412,87.0493885891151),
 .UNSPECIFIED.);
#2439=B_SPLINE_CURVE_WITH_KNOTS('',3,(#73052,#73053,#73054,#73055,#73056,
#73057,#73058,#73059,#73060,#73061,#73062,#73063,#73064,#73065,#73066,#73067,
#73068,#73069,#73070,#73071,#73072,#73073,#73074,#73075,#73076,#73077,#73078,
#73079,#73080,#73081,#73082,#73083,#73084,#73085,#73086,#73087,#73088,#73089,
#73090,#73091,#73092,#73093,#73094,#73095,#73096,#73097,#73098,#73099,#73100,
#73101,#73102,#73103,#73104,#73105,#73106,#73107,#73108,#73109,#73110,#73111,
#73112,#73113,#73114,#73115,#73116,#73117,#73118),.UNSPECIFIED.,.F.,.F.,
(4,3,3,3,3,3,3,3,3,3,3,3,3,3,3,3,3,3,3,3,3,3,4),(84.8230016473359,84.9377580239967,
85.0529300598089,85.1686593350758,85.2226669577754,85.3268533770458,85.4308845637476,
85.5347937219074,85.6386374249169,85.7424504514566,85.8462675367751,85.9501932902725,
86.0541778873479,86.1583444092029,86.220195492212,86.3243482554787,86.4283607948036,
86.5322681022204,86.6361050469229,86.739945971975,86.8437814338429,86.9477239025433,
87.048449830443),.UNSPECIFIED.);
#2440=B_SPLINE_CURVE_WITH_KNOTS('',3,(#73119,#73120,#73121,#73122,#73123,
#73124,#73125,#73126,#73127,#73128,#73129,#73130,#73131,#73132,#73133,#73134,
#73135,#73136,#73137,#73138,#73139,#73140,#73141,#73142,#73143,#73144,#73145,
#73146,#73147,#73148,#73149,#73150,#73151,#73152,#73153,#73154,#73155,#73156,
#73157,#73158,#73159,#73160,#73161,#73162,#73163,#73164,#73165,#73166,#73167,
#73168,#73169,#73170,#73171,#73172,#73173,#73174,#73175,#73176,#73177,#73178,
#73179,#73180,#73181,#73182,#73183,#73184,#73185,#73186,#73187,#73188,#73189,
#73190,#73191,#73192,#73193,#73194,#73195,#73196,#73197,#73198,#73199,#73200,
#73201,#73202,#73203,#73204,#73205,#73206,#73207,#73208,#73209,#73210,#73211,
#73212,#73213,#73214,#73215,#73216,#73217,#73218,#73219,#73220,#73221,#73222,
#73223,#73224,#73225,#73226,#73227,#73228,#73229,#73230,#73231,#73232,#73233,
#73234,#73235,#73236,#73237,#73238,#73239,#73240,#73241,#73242),
 .UNSPECIFIED.,.F.,.F.,(4,3,3,3,3,3,3,3,3,3,3,3,3,3,3,3,3,3,3,3,3,3,3,3,
3,3,3,3,3,3,3,3,3,3,3,3,3,3,3,3,3,4),(80.7657407479557,80.8695602818193,
80.9734907583458,81.077483364404,81.1816545671184,81.232552820029,81.3367392392976,
81.4407704259972,81.5446795841552,81.6485232871629,81.7523363137008,81.8561533990176,
81.9600791525132,82.0640637495867,82.1682302714401,82.2300813544656,82.3342677737345,
82.4382989604349,82.5422081185931,82.646051821601,82.7498648481392,82.8536819334563,
82.9576076869522,83.061592284026,83.1657588058796,83.2276098889022,83.3317963081706,
83.4358274948705,83.5397366530282,83.6435803560358,83.7473933825737,83.8512104678904,
83.9551362213858,84.0591208184592,84.1632873403125,84.2251384233388,84.3308712802876,
84.43643371148,84.5418329411296,84.6471360606518,84.7523779621428,84.8230016469245),
 .UNSPECIFIED.);
#2441=B_SPLINE_CURVE_WITH_KNOTS('',3,(#73248,#73249,#73250,#73251,#73252,
#73253,#73254,#73255,#73256,#73257,#73258,#73259,#73260,#73261,#73262,#73263,
#73264,#73265,#73266,#73267,#73268,#73269,#73270,#73271,#73272,#73273,#73274,
#73275,#73276,#73277,#73278,#73279,#73280,#73281,#73282,#73283,#73284,#73285,
#73286,#73287,#73288,#73289,#73290,#73291,#73292,#73293,#73294,#73295,#73296,
#73297,#73298,#73299,#73300,#73301,#73302,#73303,#73304,#73305,#73306,#73307,
#73308,#73309,#73310,#73311,#73312,#73313,#73314,#73315,#73316,#73317,#73318,
#73319,#73320,#73321,#73322,#73323,#73324,#73325,#73326,#73327,#73328,#73329,
#73330,#73331,#73332,#73333,#73334,#73335,#73336,#73337,#73338,#73339,#73340,
#73341,#73342,#73343,#73344,#73345,#73346,#73347,#73348,#73349,#73350,#73351,
#73352,#73353,#73354,#73355,#73356,#73357,#73358,#73359,#73360,#73361,#73362,
#73363,#73364,#73365,#73366,#73367,#73368,#73369,#73370,#73371,#73372,#73373,
#73374),.UNSPECIFIED.,.F.,.F.,(4,3,3,3,3,3,3,3,3,3,3,3,3,3,3,3,3,3,3,3,
3,3,3,3,3,3,3,3,3,3,3,3,3,3,3,3,3,3,3,3,3,3,4),(74.4820615826405,74.586082341132,
74.6902715190842,74.7058776737624,74.810064093031,74.914095279731,75.018004437889,
75.1218481408967,75.2256611674347,75.3294782527516,75.4334040062472,75.5373886033208,
75.6415551251742,75.703406208199,75.8075926274676,75.9116238141675,76.0155329723255,
76.1193766753332,76.2231897018712,76.327006787188,76.4309325406836,76.5349171377572,
76.6390836596106,76.7009347426356,76.8051211619043,76.9091523486042,77.0130615067623,
77.11690520977,77.220718236308,77.3245353216249,77.4284610751206,77.5324456721942,
77.6366121940476,77.6984632770722,77.8036324098605,77.906096590754,78.008463441406,
78.1107696824819,78.2180313467062,78.320375332691,78.4227592903783,78.5252692706967,
78.539816339379),.UNSPECIFIED.);
#2442=B_SPLINE_CURVE_WITH_KNOTS('',3,(#73375,#73376,#73377,#73378,#73379,
#73380,#73381,#73382,#73383,#73384,#73385,#73386,#73387,#73388,#73389,#73390,
#73391,#73392,#73393,#73394,#73395,#73396,#73397,#73398,#73399,#73400,#73401,
#73402,#73403,#73404,#73405,#73406,#73407,#73408,#73409,#73410,#73411,#73412,
#73413,#73414,#73415,#73416,#73417,#73418,#73419,#73420,#73421,#73422,#73423,
#73424,#73425,#73426,#73427,#73428,#73429,#73430,#73431,#73432,#73433,#73434,
#73435,#73436,#73437,#73438,#73439,#73440,#73441),.UNSPECIFIED.,.F.,.F.,
(4,3,3,3,3,3,3,3,3,3,3,3,3,3,3,3,3,3,3,3,3,3,4),(78.5398163397448,78.6959918115088,
78.8001782307773,78.9042094174771,79.008118575635,79.1119622786427,79.2157753051806,
79.3195923904974,79.4235181439929,79.5275027410665,79.6316692629198,79.6935203459454,
79.7977067652143,79.9017379519144,80.0056471100727,80.1094908130806,80.2133038396189,
80.317120924936,80.4210466784319,80.5250312755058,80.6291977973594,80.691048880382,
80.7662045566408),.UNSPECIFIED.);
#2443=B_SPLINE_CURVE_WITH_KNOTS('',3,(#73443,#73444,#73445,#73446,#73447,
#73448,#73449,#73450,#73451,#73452,#73453,#73454,#73455,#73456,#73457,#73458,
#73459,#73460,#73461,#73462,#73463,#73464,#73465,#73466,#73467,#73468,#73469,
#73470,#73471,#73472,#73473,#73474,#73475,#73476,#73477,#73478,#73479,#73480,
#73481,#73482,#73483,#73484,#73485,#73486,#73487,#73488,#73489,#73490,#73491,
#73492,#73493,#73494,#73495,#73496,#73497,#73498,#73499,#73500,#73501,#73502,
#73503,#73504,#73505,#73506,#73507,#73508,#73509),.UNSPECIFIED.,.F.,.F.,
(4,3,3,3,3,3,3,3,3,3,3,3,3,3,3,3,3,3,3,3,3,3,4),(78.5398163397448,78.6430648259427,
78.7462751676035,78.849482902275,78.9527963206921,79.0561639752369,79.1597213368922,
79.2374957511558,79.3416821704245,79.4457133571245,79.5496225152826,79.6534662182904,
79.7572792448286,79.8610963301457,79.9650220836414,80.0690066807151,80.1731732025685,
80.2350242855924,80.3392063862685,80.4458399766903,80.5497449587941,80.6577428533749,
80.7657407479557),.UNSPECIFIED.);
#2444=B_SPLINE_CURVE_WITH_KNOTS('',3,(#73510,#73511,#73512,#73513,#73514,
#73515,#73516,#73517,#73518,#73519,#73520,#73521,#73522,#73523,#73524,#73525,
#73526,#73527,#73528,#73529,#73530,#73531,#73532,#73533,#73534,#73535,#73536,
#73537,#73538,#73539,#73540,#73541,#73542,#73543,#73544,#73545,#73546,#73547,
#73548,#73549,#73550,#73551,#73552,#73553,#73554,#73555,#73556,#73557,#73558,
#73559,#73560,#73561,#73562,#73563,#73564,#73565,#73566,#73567,#73568,#73569,
#73570,#73571,#73572,#73573,#73574,#73575,#73576,#73577,#73578,#73579,#73580,
#73581,#73582,#73583,#73584,#73585,#73586,#73587,#73588,#73589,#73590,#73591,
#73592,#73593,#73594,#73595,#73596,#73597,#73598,#73599,#73600,#73601,#73602,
#73603,#73604,#73605,#73606,#73607,#73608,#73609,#73610,#73611,#73612,#73613,
#73614,#73615,#73616,#73617,#73618,#73619,#73620,#73621,#73622,#73623,#73624,
#73625,#73626,#73627,#73628,#73629,#73630,#73631,#73632,#73633),
 .UNSPECIFIED.,.F.,.F.,(4,3,3,3,3,3,3,3,3,3,3,3,3,3,3,3,3,3,3,3,3,3,3,3,
3,3,3,3,3,3,3,3,3,3,3,3,3,3,3,3,3,4),(74.4832427147351,74.5871328262904,
74.6909659110764,74.7947767340429,74.8986000251703,75.0025371556357,75.1065406863584,
75.2107186083713,75.2473816134094,75.351568032678,75.4555992193779,75.5595083775359,
75.6633520805436,75.7671651070816,75.8709821923983,75.974907945894,76.0788925429675,
76.1830590648209,76.244910147846,76.3490965671146,76.4531277538149,76.5570369119729,
76.6608806149806,76.7646936415186,76.8685107268354,76.972436480331,77.0764210774045,
77.1805875992579,77.2424386822826,77.3466251015511,77.4506562882511,77.5545654464091,
77.6584091494169,77.7622221759549,77.8660392612711,77.9699650147667,78.0739496118403,
78.1781161336937,78.2399672167192,78.3667743014806,78.4918646575244,78.5398163394183),
 .UNSPECIFIED.);
#2445=B_SPLINE_CURVE_WITH_KNOTS('',3,(#73639,#73640,#73641,#73642,#73643,
#73644,#73645,#73646,#73647,#73648,#73649,#73650,#73651,#73652,#73653,#73654,
#73655,#73656,#73657,#73658,#73659,#73660,#73661,#73662,#73663,#73664,#73665,
#73666,#73667,#73668,#73669,#73670,#73671,#73672,#73673,#73674,#73675,#73676,
#73677,#73678,#73679,#73680,#73681,#73682,#73683,#73684,#73685,#73686,#73687,
#73688,#73689,#73690,#73691,#73692,#73693,#73694,#73695,#73696,#73697,#73698,
#73699,#73700,#73701,#73702,#73703,#73704,#73705,#73706,#73707,#73708,#73709,
#73710,#73711,#73712,#73713,#73714,#73715,#73716,#73717,#73718,#73719,#73720,
#73721,#73722,#73723,#73724,#73725,#73726,#73727,#73728,#73729,#73730,#73731,
#73732,#73733,#73734,#73735,#73736,#73737,#73738,#73739,#73740,#73741,#73742,
#73743,#73744,#73745,#73746,#73747,#73748,#73749,#73750,#73751,#73752,#73753,
#73754,#73755,#73756,#73757,#73758,#73759),.UNSPECIFIED.,.F.,.F.,(4,3,3,
3,3,3,3,3,3,3,3,3,3,3,3,3,3,3,3,3,3,3,3,3,3,3,3,3,3,3,3,3,3,3,3,3,3,3,3,
3,4),(68.1995378133446,68.3033489762282,68.4076883489568,68.5116448062476,
68.6161756366952,68.7207064671428,68.8248928864114,68.9289240731113,69.0328332312693,
69.1366769342769,69.240489960815,69.3443070461318,69.4482327996275,69.5522173967011,
69.6563839185545,69.7182350015794,69.822421420848,69.9264526075478,70.0303617657057,
70.1342054687134,70.2380184952513,70.341835580568,70.4457613340636,70.5497459311372,
70.6539124529906,70.715763536016,70.8199499552846,70.9239811419848,71.0278903001428,
71.1317340031507,71.2355470296887,71.3393641150054,71.4432898685011,71.5472744655748,
71.6514409874282,71.7132920704526,71.820873389079,71.9298127999506,72.0369795361944,
72.1468052843798,72.2566310325652),.UNSPECIFIED.);
#2446=B_SPLINE_CURVE_WITH_KNOTS('',3,(#73760,#73761,#73762,#73763,#73764,
#73765,#73766,#73767,#73768,#73769,#73770,#73771,#73772,#73773,#73774,#73775,
#73776,#73777,#73778,#73779,#73780,#73781,#73782,#73783,#73784,#73785,#73786,
#73787,#73788,#73789,#73790,#73791,#73792,#73793,#73794,#73795,#73796,#73797,
#73798,#73799,#73800,#73801,#73802,#73803,#73804,#73805,#73806,#73807,#73808,
#73809,#73810,#73811,#73812,#73813,#73814,#73815,#73816,#73817,#73818,#73819,
#73820,#73821,#73822,#73823,#73824,#73825,#73826),.UNSPECIFIED.,.F.,.F.,
(4,3,3,3,3,3,3,3,3,3,3,3,3,3,3,3,3,3,3,3,3,3,4),(72.2566310330111,72.3701784259806,
72.4815873942033,72.5962039995462,72.7108206048892,72.8150070241578,72.9190382108577,
73.0229473690157,73.1267910720234,73.2306040985614,73.3344211838782,73.4383469373738,
73.5423315344474,73.6464980563008,73.7083491393258,73.8125058091445,73.9165206688817,
74.020428717638,74.1242648292318,74.2280916123976,74.3319123054249,74.4358068055356,
74.4820615826405),.UNSPECIFIED.);
#2447=B_SPLINE_CURVE_WITH_KNOTS('',3,(#73828,#73829,#73830,#73831,#73832,
#73833,#73834,#73835,#73836,#73837,#73838,#73839,#73840,#73841,#73842,#73843,
#73844,#73845,#73846,#73847,#73848,#73849,#73850,#73851,#73852,#73853,#73854,
#73855,#73856,#73857,#73858,#73859,#73860,#73861,#73862,#73863,#73864,#73865,
#73866,#73867,#73868,#73869,#73870,#73871,#73872,#73873,#73874,#73875,#73876,
#73877,#73878,#73879,#73880,#73881,#73882,#73883,#73884,#73885,#73886,#73887,
#73888,#73889,#73890,#73891,#73892,#73893,#73894,#73895,#73896,#73897),
 .UNSPECIFIED.,.F.,.F.,(4,3,3,3,3,3,3,3,3,3,3,3,3,3,3,3,3,3,3,3,3,3,3,4),
(72.2566310325652,72.3607828828408,72.4647795326403,72.5686542861374,72.6724637223968,
72.7762426721719,72.880025922937,72.983917905017,73.0878690474532,73.1920015684936,
73.2523245445362,73.3565109638048,73.460542150505,73.5644513086631,73.6682950116708,
73.7721080382089,73.8759251235256,73.9798508770212,74.0838354740948,74.1880019959482,
74.2498530789728,74.3540440480005,74.4580688912275,74.4832427147351),
 .UNSPECIFIED.);
#2448=B_SPLINE_CURVE_WITH_KNOTS('',3,(#73898,#73899,#73900,#73901,#73902,
#73903,#73904,#73905,#73906,#73907,#73908,#73909,#73910,#73911,#73912,#73913,
#73914,#73915,#73916,#73917,#73918,#73919,#73920,#73921,#73922,#73923,#73924,
#73925,#73926,#73927,#73928,#73929,#73930,#73931,#73932,#73933,#73934,#73935,
#73936,#73937,#73938,#73939,#73940,#73941,#73942,#73943,#73944,#73945,#73946,
#73947,#73948,#73949,#73950,#73951,#73952,#73953,#73954,#73955,#73956,#73957,
#73958,#73959,#73960,#73961,#73962,#73963,#73964,#73965,#73966,#73967,#73968,
#73969,#73970,#73971,#73972,#73973,#73974,#73975,#73976,#73977,#73978,#73979,
#73980,#73981,#73982,#73983,#73984,#73985,#73986,#73987,#73988,#73989,#73990,
#73991,#73992,#73993,#73994,#73995,#73996,#73997,#73998,#73999,#74000,#74001,
#74002,#74003,#74004,#74005,#74006,#74007,#74008,#74009,#74010,#74011,#74012,
#74013,#74014,#74015,#74016,#74017,#74018,#74019,#74020,#74021,#74022,#74023,
#74024),.UNSPECIFIED.,.F.,.F.,(4,3,3,3,3,3,3,3,3,3,3,3,3,3,3,3,3,3,3,3,
3,3,3,3,3,3,3,3,3,3,3,3,3,3,3,3,3,3,3,3,3,3,4),(68.1991393909471,68.2646818723532,
68.3688682916219,68.4728994783218,68.5768086364799,68.6806523394876,68.7844653660257,
68.8882824513425,68.9922082048382,69.0961928019119,69.2003593237653,69.2622104067898,
69.3663968260585,69.4704280127584,69.5743371709164,69.6781808739241,69.7819939004622,
69.885810985779,69.9897367392746,70.0937213363482,70.1978878582016,70.2597389412264,
70.3639253604951,70.467956547195,70.571865705353,70.6757094083608,70.7795224348988,
70.8833395202156,70.9872652737112,71.0912498707849,71.1954163926383,71.257267475663,
71.3614538949317,71.4654850816316,71.5693942397896,71.6732379427972,71.7770509693352,
71.880868054652,71.9847938081477,72.0887784052212,72.1929449270746,72.2547960100996,
72.256631032138),.UNSPECIFIED.);
#2449=B_SPLINE_CURVE_WITH_KNOTS('',3,(#74030,#74031,#74032,#74033,#74034,
#74035,#74036,#74037,#74038,#74039,#74040,#74041,#74042,#74043,#74044,#74045,
#74046,#74047,#74048,#74049,#74050,#74051,#74052,#74053,#74054,#74055,#74056,
#74057,#74058,#74059,#74060,#74061,#74062,#74063,#74064,#74065,#74066,#74067,
#74068,#74069,#74070,#74071,#74072,#74073,#74074,#74075,#74076,#74077,#74078,
#74079,#74080,#74081,#74082,#74083,#74084,#74085,#74086,#74087,#74088,#74089,
#74090,#74091,#74092,#74093,#74094,#74095,#74096,#74097,#74098,#74099,#74100,
#74101,#74102,#74103,#74104,#74105,#74106,#74107,#74108,#74109,#74110,#74111,
#74112,#74113,#74114,#74115,#74116,#74117,#74118,#74119,#74120,#74121,#74122,
#74123,#74124,#74125,#74126,#74127,#74128,#74129,#74130,#74131,#74132,#74133,
#74134,#74135,#74136,#74137,#74138,#74139,#74140,#74141,#74142,#74143,#74144,
#74145,#74146,#74147,#74148,#74149,#74150),.UNSPECIFIED.,.F.,.F.,(4,3,3,
3,3,3,3,3,3,3,3,3,3,3,3,3,3,3,3,3,3,3,3,3,3,3,3,3,3,3,3,3,3,3,3,3,3,3,3,
3,4),(61.9168660682235,62.020800016341,62.1246586758828,62.2284768441524,
62.332289265122,62.4362040609573,62.5401688922078,62.644324966426,62.7355352605232,
62.8397216797919,62.9437528664918,63.0476620246499,63.1515057276576,63.2553187541956,
63.3591358395125,63.4630615930081,63.5670461900818,63.6712127119352,63.7330637949598,
63.8372502142284,63.9412814009284,64.0451905590864,64.149034262094,64.252847288632,
64.3566643739488,64.4605901274444,64.5645747245179,64.6687412463713,64.7305923293964,
64.8347787486651,64.9388099353651,65.0427190935232,65.1465627965309,65.250375823069,
65.354192908386,65.4581186618817,65.5621032589553,65.6662697808087,65.728120863833,
65.8639211020867,65.9734457249234),.UNSPECIFIED.);
#2450=B_SPLINE_CURVE_WITH_KNOTS('',3,(#74151,#74152,#74153,#74154,#74155,
#74156,#74157,#74158,#74159,#74160,#74161,#74162,#74163,#74164,#74165,#74166,
#74167,#74168,#74169,#74170,#74171,#74172,#74173,#74174,#74175,#74176,#74177,
#74178,#74179,#74180,#74181,#74182,#74183,#74184,#74185,#74186,#74187,#74188,
#74189,#74190,#74191,#74192,#74193,#74194,#74195,#74196,#74197,#74198,#74199,
#74200,#74201,#74202,#74203,#74204,#74205,#74206,#74207,#74208,#74209,#74210,
#74211,#74212,#74213,#74214,#74215,#74216,#74217,#74218,#74219,#74220),
 .UNSPECIFIED.,.F.,.F.,(4,3,3,3,3,3,3,3,3,3,3,3,3,3,3,3,3,3,3,3,3,3,3,4),
(65.9734457253856,66.0761394376291,66.1787659097615,66.2813614741681,66.3839624163262,
66.4866699517346,66.5894404069818,66.6923813783733,66.7256493982696,66.8298358175382,
66.9338670042381,67.0377761623961,67.1416198654038,67.2454328919417,67.3492499772587,
67.4531757307542,67.5571603278279,67.6613268496813,67.7231779327062,67.8273675151291,
67.9313793154477,68.035288009472,68.1391301362488,68.1995378133446),
 .UNSPECIFIED.);
#2451=B_SPLINE_CURVE_WITH_KNOTS('',3,(#74222,#74223,#74224,#74225,#74226,
#74227,#74228,#74229,#74230,#74231,#74232,#74233,#74234,#74235,#74236,#74237,
#74238,#74239,#74240,#74241,#74242,#74243,#74244,#74245,#74246,#74247,#74248,
#74249,#74250,#74251,#74252,#74253,#74254,#74255,#74256,#74257,#74258,#74259,
#74260,#74261,#74262,#74263,#74264,#74265,#74266,#74267,#74268,#74269,#74270,
#74271,#74272,#74273,#74274,#74275,#74276,#74277,#74278,#74279,#74280,#74281,
#74282,#74283,#74284,#74285,#74286,#74287,#74288),.UNSPECIFIED.,.F.,.F.,
(4,3,3,3,3,3,3,3,3,3,3,3,3,3,3,3,3,3,3,3,3,3,4),(65.973445725698,66.0988776153487,
66.2261299465501,66.26962480348,66.3738112227487,66.4778424094486,66.5817515676066,
66.6855952706143,66.7894082971523,66.8932253824692,66.9971511359649,67.1011357330385,
67.2053022548919,67.2671533379166,67.3713444216421,67.4753543191422,67.5792620015276,
67.683102330307,67.786910085549,67.8907809267929,67.9946786620494,68.0987368470966,
68.1991393909471),.UNSPECIFIED.);
#2452=B_SPLINE_CURVE_WITH_KNOTS('',3,(#74289,#74290,#74291,#74292,#74293,
#74294,#74295,#74296,#74297,#74298,#74299,#74300,#74301,#74302,#74303,#74304,
#74305,#74306,#74307,#74308,#74309,#74310,#74311,#74312,#74313,#74314,#74315,
#74316,#74317,#74318,#74319,#74320,#74321,#74322,#74323,#74324,#74325,#74326,
#74327,#74328,#74329,#74330,#74331,#74332,#74333,#74334,#74335,#74336,#74337,
#74338,#74339,#74340,#74341,#74342,#74343,#74344,#74345,#74346,#74347,#74348,
#74349,#74350,#74351,#74352,#74353,#74354,#74355,#74356,#74357,#74358,#74359,
#74360,#74361,#74362,#74363,#74364,#74365,#74366,#74367,#74368,#74369,#74370,
#74371,#74372,#74373,#74374,#74375,#74376,#74377,#74378,#74379,#74380,#74381,
#74382,#74383,#74384,#74385,#74386,#74387,#74388,#74389,#74390,#74391,#74392,
#74393,#74394,#74395,#74396,#74397,#74398,#74399,#74400,#74401,#74402,#74403,
#74404,#74405,#74406,#74407,#74408,#74409,#74410,#74411,#74412),
 .UNSPECIFIED.,.F.,.F.,(4,3,3,3,3,3,3,3,3,3,3,3,3,3,3,3,3,3,3,3,3,3,3,3,
3,3,3,3,3,3,3,3,3,3,3,3,3,3,3,3,3,4),(61.9158957515895,62.0198259500386,
62.1238180909945,62.2279890158734,62.2795106657336,62.3836970850022,62.4877282717022,
62.5916374298602,62.6954811328679,62.7992941594058,62.9031112447227,63.0070369982183,
63.1110215952918,63.2151881171452,63.2770392001702,63.3812256194389,63.4852568061389,
63.589165964297,63.6930096673046,63.7968226938427,63.9006397791592,64.0045655326549,
64.1085501297284,64.2127166515818,64.2745677346068,64.3787541538753,64.4827853405749,
64.5866944987329,64.6905382017405,64.7943512282787,64.8981683135958,65.0020940670913,
65.1060786641648,65.2102451860182,65.2720962690434,65.3756018854376,65.4789620265334,
65.5822125841115,65.6854054642083,65.7885610860729,65.8917634870112,65.9734457253856),
 .UNSPECIFIED.);
#2453=B_SPLINE_CURVE_WITH_KNOTS('',3,(#74418,#74419,#74420,#74421,#74422,
#74423,#74424,#74425,#74426,#74427,#74428,#74429,#74430,#74431,#74432,#74433,
#74434,#74435,#74436,#74437,#74438,#74439,#74440,#74441,#74442,#74443,#74444,
#74445,#74446,#74447,#74448,#74449,#74450,#74451,#74452,#74453,#74454,#74455,
#74456,#74457,#74458,#74459,#74460,#74461,#74462,#74463,#74464,#74465,#74466,
#74467,#74468,#74469,#74470,#74471,#74472,#74473,#74474,#74475,#74476,#74477,
#74478,#74479,#74480,#74481,#74482,#74483,#74484,#74485,#74486,#74487,#74488,
#74489,#74490,#74491,#74492,#74493,#74494,#74495,#74496,#74497,#74498,#74499,
#74500,#74501,#74502,#74503,#74504,#74505,#74506,#74507,#74508,#74509,#74510,
#74511,#74512,#74513,#74514,#74515,#74516,#74517,#74518,#74519,#74520,#74521,
#74522,#74523,#74524,#74525,#74526,#74527,#74528,#74529,#74530,#74531,#74532,
#74533,#74534,#74535,#74536,#74537,#74538,#74539,#74540,#74541,#74542,#74543,
#74544),.UNSPECIFIED.,.F.,.F.,(4,3,3,3,3,3,3,3,3,3,3,3,3,3,3,3,3,3,3,3,
3,3,3,3,3,3,3,3,3,3,3,3,3,3,3,3,3,3,3,3,3,3,4),(55.632601267868,55.7367901950251,
55.752835519467,55.8570219387357,55.9610531254356,56.0649622835936,56.1688059866013,
56.2726190131393,56.3764360984562,56.4803618519518,56.5843464490254,56.6885129708788,
56.7503640539036,56.8545504731722,56.9585816598722,57.0624908180302,57.1663345210379,
57.270147547576,57.3739646328928,57.4778903863884,57.581874983462,57.6860415053154,
57.7478925883402,57.8520790076088,57.9561101943088,58.0600193524668,58.1638630554745,
58.2676760820125,58.3714931673294,58.475418920825,58.5794035178986,58.683570039752,
58.7454211227768,58.8487780338704,58.9539633318698,59.0570447634801,59.1600643665929,
59.2630580262833,59.369858624179,59.4729706208883,59.5761501528112,59.6794897442517,
59.6902604178662),.UNSPECIFIED.);
#2454=B_SPLINE_CURVE_WITH_KNOTS('',3,(#74545,#74546,#74547,#74548,#74549,
#74550,#74551,#74552,#74553,#74554,#74555,#74556,#74557,#74558,#74559,#74560,
#74561,#74562,#74563,#74564,#74565,#74566,#74567,#74568,#74569,#74570,#74571,
#74572,#74573,#74574,#74575,#74576,#74577,#74578,#74579,#74580,#74581,#74582,
#74583,#74584,#74585,#74586,#74587,#74588,#74589,#74590,#74591,#74592,#74593,
#74594,#74595,#74596,#74597,#74598,#74599,#74600,#74601,#74602,#74603,#74604,
#74605,#74606,#74607,#74608,#74609,#74610,#74611,#74612,#74613,#74614),
 .UNSPECIFIED.,.F.,.F.,(4,3,3,3,3,3,3,3,3,3,3,3,3,3,3,3,3,3,3,3,3,3,3,4),
(59.690260418206,59.7429496572134,59.847136076482,59.9511672631821,60.0550764213401,
60.1589201243478,60.2627331508858,60.3665502362027,60.4704759896983,60.5744605867719,
60.6786271086253,60.74047819165,60.8446646109187,60.9486957976187,61.0526049557767,
61.1564486587844,61.2602616853225,61.3640787706394,61.468004524135,61.5719891212086,
61.676155643062,61.7380067260866,61.8421682999697,61.9168660682235),
 .UNSPECIFIED.);
#2455=B_SPLINE_CURVE_WITH_KNOTS('',3,(#74616,#74617,#74618,#74619,#74620,
#74621,#74622,#74623,#74624,#74625,#74626,#74627,#74628,#74629,#74630,#74631,
#74632,#74633,#74634,#74635,#74636,#74637,#74638,#74639,#74640,#74641,#74642,
#74643,#74644,#74645,#74646,#74647,#74648,#74649,#74650,#74651,#74652,#74653,
#74654,#74655,#74656,#74657,#74658,#74659,#74660,#74661,#74662,#74663,#74664,
#74665,#74666,#74667,#74668,#74669,#74670,#74671,#74672,#74673,#74674,#74675,
#74676,#74677,#74678,#74679,#74680,#74681,#74682),.UNSPECIFIED.,.F.,.F.,
(4,3,3,3,3,3,3,3,3,3,3,3,3,3,3,3,3,3,3,3,3,3,4),(59.690260418206,59.7955870148005,
59.9009552529612,60.0064809160439,60.1120913042762,60.2179183210521,60.2844535968604,
60.388640016129,60.492671202829,60.596580360987,60.7004240639947,60.8042370905327,
60.9080541758494,61.011979929345,61.1159645264186,61.220131048272,61.281982131297,
61.3861518308915,61.4901756511519,61.5966056762613,61.7004458111016,61.8081707813456,
61.9158957515895),.UNSPECIFIED.);
#2456=B_SPLINE_CURVE_WITH_KNOTS('',3,(#74683,#74684,#74685,#74686,#74687,
#74688,#74689,#74690,#74691,#74692,#74693,#74694,#74695,#74696,#74697,#74698,
#74699,#74700,#74701,#74702,#74703,#74704,#74705,#74706,#74707,#74708,#74709,
#74710,#74711,#74712,#74713,#74714,#74715,#74716,#74717,#74718,#74719,#74720,
#74721,#74722,#74723,#74724,#74725,#74726,#74727,#74728,#74729,#74730,#74731,
#74732,#74733,#74734,#74735,#74736,#74737,#74738,#74739,#74740,#74741,#74742,
#74743,#74744,#74745,#74746,#74747,#74748,#74749,#74750,#74751,#74752,#74753,
#74754,#74755,#74756,#74757,#74758,#74759,#74760,#74761,#74762,#74763,#74764,
#74765,#74766,#74767,#74768,#74769,#74770,#74771,#74772,#74773,#74774,#74775,
#74776,#74777,#74778,#74779,#74780,#74781,#74782,#74783,#74784,#74785,#74786,
#74787,#74788,#74789,#74790,#74791,#74792,#74793,#74794,#74795,#74796,#74797,
#74798,#74799,#74800,#74801,#74802,#74803,#74804,#74805,#74806),
 .UNSPECIFIED.,.F.,.F.,(4,3,3,3,3,3,3,3,3,3,3,3,3,3,3,3,3,3,3,3,3,3,3,3,
3,3,3,3,3,3,3,3,3,3,3,3,3,3,3,3,3,4),(55.6335465345705,55.7373798274981,
55.8411906765822,55.9450138118952,56.0489506768776,56.1529537786039,56.2571314301315,
56.294339459114,56.3985258783826,56.5025570650827,56.6064662232407,56.7103099262484,
56.8141229527865,56.9179400381034,57.021865791599,57.1258503886726,57.230016910526,
57.2918679935506,57.3960544128192,57.5000855995191,57.6039947576771,57.7078384606849,
57.8116514872229,57.9154685725399,58.0193943260355,58.1233789231092,58.2275454449625,
58.2893965279872,58.3935829472558,58.4976141339561,58.6015232921142,58.7053669951219,
58.8091800216597,58.9129971069763,59.0169228604719,59.1209074575456,59.2250739793991,
59.2869250624238,59.4023023747482,59.5173142786563,59.6317214277102,59.6902604178031),
 .UNSPECIFIED.);
#2457=B_SPLINE_CURVE_WITH_KNOTS('',3,(#74812,#74813,#74814,#74815,#74816,
#74817,#74818,#74819,#74820,#74821,#74822,#74823,#74824,#74825,#74826,#74827,
#74828,#74829,#74830,#74831,#74832,#74833,#74834,#74835,#74836,#74837,#74838,
#74839,#74840,#74841,#74842,#74843,#74844,#74845,#74846,#74847,#74848,#74849,
#74850,#74851,#74852,#74853,#74854,#74855,#74856,#74857,#74858,#74859,#74860,
#74861,#74862,#74863,#74864,#74865,#74866,#74867,#74868,#74869,#74870,#74871,
#74872,#74873,#74874,#74875,#74876,#74877,#74878,#74879,#74880,#74881,#74882,
#74883,#74884,#74885,#74886,#74887,#74888,#74889,#74890,#74891,#74892,#74893,
#74894,#74895,#74896,#74897,#74898,#74899,#74900,#74901,#74902,#74903,#74904,
#74905,#74906,#74907,#74908,#74909,#74910,#74911,#74912,#74913,#74914,#74915,
#74916,#74917,#74918,#74919,#74920,#74921,#74922,#74923,#74924,#74925,#74926,
#74927,#74928,#74929,#74930,#74931,#74932,#74933,#74934,#74935),
 .UNSPECIFIED.,.F.,.F.,(4,3,3,3,3,3,3,3,3,3,3,3,3,3,3,3,3,3,3,3,3,3,3,3,
3,3,3,3,3,3,3,3,3,3,3,3,3,3,3,3,3,4),(49.3496692799972,49.4541680382097,
49.5581242127346,49.662894262791,49.7676643128474,49.871850732116,49.9758819188161,
50.0797910769742,50.1836347799818,50.2874478065199,50.3912648918368,50.4951906453325,
50.5991752424062,50.7033417642596,50.765192847284,50.8693792665526,50.9734104532527,
51.0773196114107,51.1811633144184,51.2849763409564,51.3887934262736,51.4927191797692,
51.5967037768428,51.7008702986961,51.7627213817206,51.8669078009892,51.9709389876889,
52.0748481458469,52.1786918488547,52.2825048753927,52.3863219607096,52.4902477142051,
52.5942323112789,52.6983988331322,52.7602499161572,52.8647413337412,52.9690770723351,
53.0785765820079,53.1827008676143,53.2867777522301,53.3908555974491,53.4070751110264),
 .UNSPECIFIED.);
#2458=B_SPLINE_CURVE_WITH_KNOTS('',3,(#74936,#74937,#74938,#74939,#74940,
#74941,#74942,#74943,#74944,#74945,#74946,#74947,#74948,#74949,#74950,#74951,
#74952,#74953,#74954,#74955,#74956,#74957,#74958,#74959,#74960,#74961,#74962,
#74963,#74964,#74965,#74966,#74967,#74968,#74969,#74970,#74971,#74972,#74973,
#74974,#74975,#74976,#74977,#74978,#74979,#74980,#74981,#74982,#74983,#74984,
#74985,#74986,#74987,#74988,#74989,#74990,#74991,#74992,#74993,#74994,#74995,
#74996,#74997,#74998,#74999,#75000,#75001,#75002),.UNSPECIFIED.,.F.,.F.,
(4,3,3,3,3,3,3,3,3,3,3,3,3,3,3,3,3,3,3,3,3,3,4),(53.4070751114695,53.5260746317924,
53.6461595854636,53.7577784505938,53.8619648698624,53.9659960565624,54.0699052147205,
54.1737489177282,54.2775619442662,54.3813790295831,54.4853047830788,54.5892893801525,
54.6934559020058,54.7553069850304,54.8649687703851,54.9689734124943,55.0728760914193,
55.1767116672088,55.280514918126,55.3843665184446,55.4882460133807,55.5922460948382,
55.632601267868),.UNSPECIFIED.);
#2459=B_SPLINE_CURVE_WITH_KNOTS('',3,(#75004,#75005,#75006,#75007,#75008,
#75009,#75010,#75011,#75012,#75013,#75014,#75015,#75016,#75017,#75018,#75019,
#75020,#75021,#75022,#75023,#75024,#75025,#75026,#75027,#75028,#75029,#75030,
#75031,#75032,#75033,#75034,#75035,#75036,#75037,#75038,#75039,#75040,#75041,
#75042,#75043,#75044,#75045,#75046,#75047,#75048,#75049,#75050,#75051,#75052,
#75053,#75054,#75055,#75056,#75057,#75058,#75059,#75060,#75061,#75062,#75063,
#75064,#75065,#75066,#75067,#75068,#75069,#75070,#75071,#75072,#75073),
 .UNSPECIFIED.,.F.,.F.,(4,3,3,3,3,3,3,3,3,3,3,3,3,3,3,3,3,3,3,3,3,3,3,4),
(53.407075111485,53.5098558320716,53.6124863111895,53.7150344153237,53.8175366234483,
53.9200293486255,54.0226180274754,54.1252565130568,54.2280753277761,54.2992823902408,
54.4034688095096,54.5074999962094,54.6114091543675,54.7152528573751,54.8190658839131,
54.9228829692299,55.0268087227256,55.1307933197992,55.2349598416526,55.2968109246774,
55.4009764972003,55.5050059369267,55.6089152722145,55.6335465345705),
 .UNSPECIFIED.);
#2460=B_SPLINE_CURVE_WITH_KNOTS('',3,(#75074,#75075,#75076,#75077,#75078,
#75079,#75080,#75081,#75082,#75083,#75084,#75085,#75086,#75087,#75088,#75089,
#75090,#75091,#75092,#75093,#75094,#75095,#75096,#75097,#75098,#75099,#75100,
#75101,#75102,#75103,#75104,#75105,#75106,#75107,#75108,#75109,#75110,#75111,
#75112,#75113,#75114,#75115,#75116,#75117,#75118,#75119,#75120,#75121,#75122,
#75123,#75124,#75125,#75126,#75127,#75128,#75129,#75130,#75131,#75132,#75133,
#75134,#75135,#75136,#75137,#75138,#75139,#75140,#75141,#75142,#75143,#75144,
#75145,#75146,#75147,#75148,#75149,#75150,#75151,#75152,#75153,#75154,#75155,
#75156,#75157,#75158,#75159,#75160,#75161,#75162,#75163,#75164,#75165,#75166,
#75167,#75168,#75169,#75170,#75171,#75172,#75173,#75174,#75175,#75176,#75177,
#75178,#75179,#75180,#75181,#75182,#75183,#75184,#75185,#75186,#75187,#75188,
#75189,#75190,#75191,#75192,#75193,#75194,#75195,#75196,#75197),
 .UNSPECIFIED.,.F.,.F.,(4,3,3,3,3,3,3,3,3,3,3,3,3,3,3,3,3,3,3,3,3,3,3,3,
3,3,3,3,3,3,3,3,3,3,3,3,3,3,3,3,3,4),(49.3501240392415,49.4542486344756,
49.5611135867279,49.6649925959122,49.7688199626021,49.8726304440509,49.9817648961618,
50.0857131354161,50.1897342007835,50.2939235856819,50.3091682524944,50.413354671763,
50.517385858463,50.621295016621,50.7251387196287,50.8289517461667,50.9327688314835,
51.0366945849791,51.1406791820528,51.2448457039061,51.306696786931,51.4108832061996,
51.5149143928996,51.6188235510576,51.7226672540653,51.8264802806034,51.9302973659202,
52.0342231194158,52.1382077164894,52.2423742383427,52.3042253213676,52.4084117406363,
52.5124429273362,52.6163520854942,52.720195788502,52.82400881504,52.9278259003569,
53.0317516538525,53.1357362509261,53.2399027727795,53.3017538558042,53.4070751110264),
 .UNSPECIFIED.);
#2461=B_SPLINE_CURVE_WITH_KNOTS('',3,(#75203,#75204,#75205,#75206,#75207,
#75208,#75209,#75210,#75211,#75212,#75213,#75214,#75215,#75216,#75217,#75218,
#75219,#75220,#75221,#75222,#75223,#75224,#75225,#75226,#75227,#75228,#75229,
#75230,#75231,#75232,#75233,#75234,#75235,#75236,#75237,#75238,#75239,#75240,
#75241,#75242,#75243,#75244,#75245,#75246,#75247,#75248,#75249,#75250,#75251,
#75252,#75253,#75254,#75255,#75256,#75257,#75258,#75259,#75260,#75261,#75262,
#75263,#75264,#75265,#75266,#75267,#75268,#75269,#75270,#75271,#75272,#75273,
#75274,#75275,#75276,#75277,#75278,#75279,#75280,#75281,#75282,#75283,#75284,
#75285,#75286,#75287,#75288,#75289,#75290,#75291,#75292,#75293,#75294,#75295,
#75296,#75297,#75298,#75299,#75300,#75301,#75302,#75303,#75304,#75305,#75306,
#75307,#75308,#75309,#75310,#75311,#75312,#75313,#75314,#75315,#75316,#75317,
#75318,#75319,#75320,#75321,#75322,#75323),.UNSPECIFIED.,.F.,.F.,(4,3,3,
3,3,3,3,3,3,3,3,3,3,3,3,3,3,3,3,3,3,3,3,3,3,3,3,3,3,3,3,3,3,3,3,3,3,3,3,
3,4),(43.0672711170668,43.1711300481588,43.2749483250992,43.3787606920285,
43.4826753270082,43.5866398512832,43.6907957779855,43.7824931062278,43.8866795254967,
43.990710712197,44.0946198703552,44.1984635733631,44.3022765999014,44.4060936852184,
44.5100194387142,44.6140040357881,44.7181705576417,44.7800216406644,44.884208059933,
44.9882392466327,45.0921484047907,45.1959921077982,45.2998051343363,45.4036222196529,
45.5075479731485,45.6115325702221,45.7156990920753,45.777550175101,45.8817365943698,
45.9857677810699,46.0896769392279,46.1935206422355,46.2973336687735,46.4011507540907,
46.5050765075864,46.6090611046601,46.7132276265135,46.7750787095376,46.8955468165443,
47.0149579004655,47.1238898034052),.UNSPECIFIED.);
#2462=B_SPLINE_CURVE_WITH_KNOTS('',3,(#75324,#75325,#75326,#75327,#75328,
#75329,#75330,#75331,#75332,#75333,#75334,#75335,#75336,#75337,#75338,#75339,
#75340,#75341,#75342,#75343,#75344,#75345,#75346,#75347,#75348,#75349,#75350,
#75351,#75352,#75353,#75354,#75355,#75356,#75357,#75358,#75359,#75360,#75361,
#75362,#75363,#75364,#75365,#75366,#75367,#75368,#75369,#75370,#75371,#75372,
#75373,#75374,#75375,#75376,#75377,#75378,#75379,#75380,#75381,#75382,#75383,
#75384,#75385,#75386,#75387,#75388,#75389,#75390,#75391,#75392,#75393),
 .UNSPECIFIED.,.F.,.F.,(4,3,3,3,3,3,3,3,3,3,3,3,3,3,3,3,3,3,3,3,3,3,3,4),
(47.1238898038468,47.2279417400956,47.3319880830488,47.4360629830602,47.5402700680327,
47.6445565808268,47.7490254998337,47.7726072439742,47.8767936632428,47.9808248499427,
48.0847340081007,48.1885777111083,48.2923907376463,48.3962078229629,48.5001335764585,
48.6041181735321,48.7082846953854,48.7701357784108,48.8743117183293,48.9783401946018,
49.0822482051312,49.1860855662745,49.2899055677676,49.3496692799972),
 .UNSPECIFIED.);
#2463=B_SPLINE_CURVE_WITH_KNOTS('',3,(#75395,#75396,#75397,#75398,#75399,
#75400,#75401,#75402,#75403,#75404,#75405,#75406,#75407,#75408,#75409,#75410,
#75411,#75412,#75413,#75414,#75415,#75416,#75417,#75418,#75419,#75420,#75421,
#75422,#75423,#75424,#75425,#75426,#75427,#75428,#75429,#75430,#75431,#75432,
#75433,#75434,#75435,#75436,#75437,#75438,#75439,#75440,#75441,#75442,#75443,
#75444,#75445,#75446,#75447,#75448,#75449,#75450,#75451,#75452,#75453,#75454,
#75455,#75456,#75457,#75458,#75459,#75460,#75461,#75462,#75463,#75464),
 .UNSPECIFIED.,.F.,.F.,(4,3,3,3,3,3,3,3,3,3,3,3,3,3,3,3,3,3,3,3,3,3,3,4),
(47.1238898038468,47.2757519674259,47.3165826491846,47.4207690684532,47.5248002551532,
47.6287094133112,47.7325531163188,47.8363661428568,47.9401832281736,48.0441089816691,
48.1480935787427,48.252260100596,48.3141111836212,48.4182976028898,48.5223287895898,
48.6262379477478,48.7300816507555,48.8338946772934,48.9377117626103,49.0416375161059,
49.1456221131795,49.2497886350328,49.3116397180578,49.3501240392415),
 .UNSPECIFIED.);
#2464=B_SPLINE_CURVE_WITH_KNOTS('',3,(#75465,#75466,#75467,#75468,#75469,
#75470,#75471,#75472,#75473,#75474,#75475,#75476,#75477,#75478,#75479,#75480,
#75481,#75482,#75483,#75484,#75485,#75486,#75487,#75488,#75489,#75490,#75491,
#75492,#75493,#75494,#75495,#75496,#75497,#75498,#75499,#75500,#75501,#75502,
#75503,#75504,#75505,#75506,#75507,#75508,#75509,#75510,#75511,#75512,#75513,
#75514,#75515,#75516,#75517,#75518,#75519,#75520,#75521,#75522,#75523,#75524,
#75525,#75526,#75527,#75528,#75529,#75530,#75531,#75532,#75533,#75534,#75535,
#75536,#75537,#75538,#75539,#75540,#75541,#75542,#75543,#75544,#75545,#75546,
#75547,#75548,#75549,#75550,#75551,#75552,#75553,#75554,#75555,#75556,#75557,
#75558,#75559,#75560,#75561,#75562,#75563,#75564,#75565,#75566,#75567,#75568,
#75569,#75570,#75571,#75572,#75573,#75574,#75575,#75576,#75577,#75578,#75579,
#75580,#75581,#75582,#75583,#75584,#75585,#75586,#75587,#75588),
 .UNSPECIFIED.,.F.,.F.,(4,3,3,3,3,3,3,3,3,3,3,3,3,3,3,3,3,3,3,3,3,3,3,3,
3,3,3,3,3,3,3,3,3,3,3,3,3,3,3,3,3,4),(43.0661580866905,43.1701497613869,
43.2743204084533,43.3264685114382,43.4306549307085,43.5346861174102,43.63859527557,
43.7424389785794,43.8462520051192,43.9500690904379,44.0539948439353,44.1579794410107,
44.2621459628659,44.3239970458748,44.4281834651431,44.5322146518427,44.6361238100004,
44.7399675130077,44.8437805395454,44.9475976248619,45.0515233783572,45.1555079754305,
45.2596744972836,45.3215255803114,45.4257119995798,45.5297431862795,45.6336523444373,
45.7374960474447,45.8413090739825,45.9451261592991,46.0490519127945,46.1530365098678,
46.2572030317209,46.319054114748,46.4216814718159,46.5241724459795,46.6265638875462,
46.7288925026225,46.8312400381875,46.9335916782503,47.036063908885,47.1238898034172),
 .UNSPECIFIED.);
#2465=B_SPLINE_CURVE_WITH_KNOTS('',3,(#75594,#75595,#75596,#75597,#75598,
#75599,#75600,#75601,#75602,#75603,#75604,#75605,#75606,#75607,#75608,#75609,
#75610,#75611,#75612,#75613,#75614,#75615,#75616,#75617,#75618,#75619,#75620,
#75621,#75622,#75623,#75624,#75625,#75626,#75627,#75628,#75629,#75630,#75631,
#75632,#75633,#75634,#75635,#75636,#75637,#75638,#75639,#75640,#75641,#75642,
#75643,#75644,#75645,#75646,#75647,#75648,#75649,#75650,#75651,#75652,#75653,
#75654,#75655,#75656,#75657,#75658,#75659,#75660,#75661,#75662,#75663,#75664,
#75665,#75666,#75667,#75668,#75669,#75670,#75671,#75672,#75673,#75674,#75675,
#75676,#75677,#75678,#75679,#75680,#75681,#75682,#75683,#75684,#75685,#75686,
#75687,#75688,#75689,#75690,#75691,#75692,#75693,#75694,#75695,#75696,#75697,
#75698,#75699,#75700,#75701,#75702,#75703,#75704,#75705,#75706,#75707,#75708,
#75709,#75710,#75711,#75712,#75713,#75714,#75715,#75716,#75717,#75718,#75719,
#75720),.UNSPECIFIED.,.F.,.F.,(4,3,3,3,3,3,3,3,3,3,3,3,3,3,3,3,3,3,3,3,
3,3,3,3,3,3,3,3,3,3,3,3,3,3,3,3,3,3,3,3,3,3,4),(36.7834458130743,36.7997933651716,
36.9039797844174,37.008010971094,37.1119201292281,37.2157638322115,37.3195768587249,
37.4233939440169,37.5273196974874,37.6313042945357,37.7354708163638,37.7973218996082,
37.9015083188909,38.005539505605,38.1094486637775,38.2132923667998,38.3171053933525,
38.4209224786842,38.5248482321947,38.6288328292833,38.7329993511515,38.7948504340448,
38.8990368533114,39.0030680400094,39.1069771981654,39.2108209011712,39.3146339277072,
39.4184510130221,39.5223767665159,39.6263613635876,39.7305278854392,39.7923789684814,
39.8965653877477,40.0005965744453,40.1045057326009,40.2083494356062,40.3121624621417,
40.4159795474562,40.5199053009493,40.6238898980203,40.7280564198711,40.789907502918,
40.8407044966673),.UNSPECIFIED.);
#2466=B_SPLINE_CURVE_WITH_KNOTS('',3,(#75721,#75722,#75723,#75724,#75725,
#75726,#75727,#75728,#75729,#75730,#75731,#75732,#75733,#75734,#75735,#75736,
#75737,#75738,#75739,#75740,#75741,#75742,#75743,#75744,#75745,#75746,#75747,
#75748,#75749,#75750,#75751,#75752,#75753,#75754,#75755,#75756,#75757,#75758,
#75759,#75760,#75761,#75762,#75763,#75764,#75765,#75766,#75767,#75768,#75769,
#75770,#75771,#75772,#75773,#75774,#75775,#75776,#75777,#75778,#75779,#75780,
#75781,#75782,#75783,#75784,#75785,#75786,#75787,#75788,#75789,#75790),
 .UNSPECIFIED.,.F.,.F.,(4,3,3,3,3,3,3,3,3,3,3,3,3,3,3,3,3,3,3,3,3,3,3,4),
(40.8407044970058,40.9440672893056,41.0494883828118,41.1525861150441,41.2556259852182,
41.3586438439569,41.4658418923063,41.5689883265361,41.6722057013042,41.7755885097156,
41.7874360373546,41.8916224566229,41.9956536433225,42.0995628014801,42.2034065044874,
42.307219531025,42.4110366163413,42.5149623698365,42.6189469669099,42.7231134887628,
42.7849645717912,42.8891423385872,42.9931552860089,43.0672711170668),
 .UNSPECIFIED.);
#2467=B_SPLINE_CURVE_WITH_KNOTS('',3,(#75792,#75793,#75794,#75795,#75796,
#75797,#75798,#75799,#75800,#75801,#75802,#75803,#75804,#75805,#75806,#75807,
#75808,#75809,#75810,#75811,#75812,#75813,#75814,#75815,#75816,#75817,#75818,
#75819,#75820,#75821,#75822,#75823,#75824,#75825,#75826,#75827,#75828,#75829,
#75830,#75831,#75832,#75833,#75834,#75835,#75836,#75837,#75838,#75839,#75840,
#75841,#75842,#75843,#75844,#75845,#75846,#75847,#75848,#75849,#75850,#75851,
#75852,#75853,#75854,#75855,#75856,#75857,#75858),.UNSPECIFIED.,.F.,.F.,
(4,3,3,3,3,3,3,3,3,3,3,3,3,3,3,3,3,3,3,3,3,3,4),(40.8407044970049,40.9498036597887,
41.0592250219573,41.1688181464341,41.2787131705271,41.331411442565,41.4355978618316,
41.5396290485296,41.6435382066856,41.7473819096913,41.8511949362273,41.9550120215421,
42.0589377750358,42.1629223721075,42.2670888939591,42.3289399770016,42.4330996296933,
42.5371164105446,42.6410253236265,42.7473085143925,42.8511267996347,42.9586424431626,
43.0661580866905),.UNSPECIFIED.);
#2468=B_SPLINE_CURVE_WITH_KNOTS('',3,(#75859,#75860,#75861,#75862,#75863,
#75864,#75865,#75866,#75867,#75868,#75869,#75870,#75871,#75872,#75873,#75874,
#75875,#75876,#75877,#75878,#75879,#75880,#75881,#75882,#75883,#75884,#75885,
#75886,#75887,#75888,#75889,#75890,#75891,#75892,#75893,#75894,#75895,#75896,
#75897,#75898,#75899,#75900,#75901,#75902,#75903,#75904,#75905,#75906,#75907,
#75908,#75909,#75910,#75911,#75912,#75913,#75914,#75915,#75916,#75917,#75918,
#75919,#75920,#75921,#75922,#75923,#75924,#75925,#75926,#75927,#75928,#75929,
#75930,#75931,#75932,#75933,#75934,#75935,#75936,#75937,#75938,#75939,#75940,
#75941,#75942,#75943,#75944,#75945,#75946,#75947,#75948,#75949,#75950,#75951,
#75952,#75953,#75954,#75955,#75956,#75957,#75958,#75959,#75960,#75961,#75962,
#75963,#75964,#75965,#75966,#75967,#75968,#75969,#75970,#75971,#75972,#75973,
#75974,#75975,#75976,#75977,#75978,#75979,#75980,#75981,#75982),
 .UNSPECIFIED.,.F.,.F.,(4,3,3,3,3,3,3,3,3,3,3,3,3,3,3,3,3,3,3,3,3,3,3,3,
3,3,3,3,3,3,3,3,3,3,3,3,3,3,3,3,3,4),(36.783721561275,36.8875324408591,
36.991355400596,37.0952919656597,37.1992945822548,37.303471928437,37.3412973048186,
37.445483724201,37.5495149110165,37.6534240692916,37.7572677724174,37.8610807990743,
37.964897884511,38.0688236381266,38.1728082353203,38.2769747572932,38.3388258392552,
38.4430122585159,38.5470434452078,38.6509526033583,38.7547963063587,38.8586093328897,
38.9624264181998,39.0663521716889,39.1703367687562,39.2745032906037,39.3363543736918,
39.4405407929374,39.5445719796139,39.6484811377479,39.7523248407311,39.8561378672445,
39.9599549525365,40.0638807060069,40.1678653030551,40.2720318248831,40.3338829081284,
40.4430298277097,40.551871089477,40.6605292198771,40.7689635848466,40.8407044966672),
 .UNSPECIFIED.);
#2469=B_SPLINE_CURVE_WITH_KNOTS('',3,(#75988,#75989,#75990,#75991,#75992,
#75993,#75994,#75995,#75996,#75997,#75998,#75999,#76000,#76001,#76002,#76003,
#76004,#76005,#76006,#76007,#76008,#76009,#76010,#76011,#76012,#76013,#76014,
#76015,#76016,#76017,#76018,#76019,#76020,#76021,#76022,#76023,#76024,#76025,
#76026,#76027,#76028,#76029,#76030,#76031,#76032,#76033,#76034,#76035,#76036,
#76037,#76038,#76039,#76040,#76041,#76042,#76043,#76044,#76045,#76046,#76047,
#76048,#76049,#76050,#76051,#76052,#76053,#76054,#76055,#76056,#76057,#76058,
#76059,#76060,#76061,#76062,#76063,#76064,#76065,#76066,#76067,#76068,#76069,
#76070,#76071,#76072,#76073,#76074,#76075,#76076,#76077,#76078,#76079,#76080,
#76081,#76082,#76083,#76084,#76085,#76086,#76087,#76088,#76089,#76090,#76091,
#76092,#76093,#76094,#76095,#76096,#76097,#76098,#76099,#76100,#76101,#76102,
#76103,#76104,#76105,#76106,#76107,#76108,#76109,#76110,#76111),
 .UNSPECIFIED.,.F.,.F.,(4,3,3,3,3,3,3,3,3,3,3,3,3,3,3,3,3,3,3,3,3,3,3,3,
3,3,3,3,3,3,3,3,3,3,3,3,3,3,3,3,3,4),(30.4998648068842,30.6038202397747,
30.7092211991633,30.814622158552,30.9188085758033,31.0228397604486,31.1267489165067,
31.2305926173876,31.3344056417751,31.4382227249208,31.5421484762289,31.6461330711024,
31.7502995907594,31.8121506929886,31.9163371131481,32.0203683007503,32.1242774598234,
32.2281211637535,32.3319341912199,32.4357512774697,32.5396770318988,32.6436616299078,
32.747828152689,32.8096792274252,32.9138656467035,33.0178968334163,33.1218059915909,
33.2256496946177,33.3294627211775,33.4332798065188,33.5372055600422,33.6411901571455,
33.7453566790319,33.8072077618618,33.9101447146383,34.0129417465488,34.1156354071306,
34.2182621038491,34.320888212797,34.4235151981865,34.5262219085209,34.5575191894877),
 .UNSPECIFIED.);
#2470=B_SPLINE_CURVE_WITH_KNOTS('',3,(#76112,#76113,#76114,#76115,#76116,
#76117,#76118,#76119,#76120,#76121,#76122,#76123,#76124,#76125,#76126,#76127,
#76128,#76129,#76130,#76131,#76132,#76133,#76134,#76135,#76136,#76137,#76138,
#76139,#76140,#76141,#76142,#76143,#76144,#76145,#76146,#76147,#76148,#76149,
#76150,#76151,#76152,#76153,#76154,#76155,#76156,#76157,#76158,#76159,#76160,
#76161,#76162,#76163,#76164,#76165,#76166,#76167,#76168,#76169,#76170,#76171,
#76172,#76173,#76174,#76175,#76176,#76177,#76178),.UNSPECIFIED.,.F.,.F.,
(4,3,3,3,3,3,3,3,3,3,3,3,3,3,3,3,3,3,3,3,3,3,4),(34.5575191897626,34.6928922558173,
34.8047362962984,34.9089227156804,35.0129539024952,35.1168630607699,35.2207067638953,
35.324519790552,35.4283368759881,35.5322626296032,35.6362472267967,35.7404137487691,
35.802264830735,35.9064523911115,36.0104843860349,36.1143930817557,36.2182358509203,
36.3220474724968,36.4258626813831,36.529781085897,36.6337581406858,36.7379046401052,
36.7834458130743),.UNSPECIFIED.);
#2471=B_SPLINE_CURVE_WITH_KNOTS('',3,(#76180,#76181,#76182,#76183,#76184,
#76185,#76186,#76187,#76188,#76189,#76190,#76191,#76192,#76193,#76194,#76195,
#76196,#76197,#76198,#76199,#76200,#76201,#76202,#76203,#76204,#76205,#76206,
#76207,#76208,#76209,#76210,#76211,#76212,#76213,#76214,#76215,#76216,#76217,
#76218,#76219,#76220,#76221,#76222,#76223,#76224,#76225,#76226,#76227,#76228,
#76229,#76230,#76231,#76232,#76233,#76234,#76235,#76236,#76237,#76238,#76239,
#76240,#76241,#76242,#76243,#76244,#76245,#76246,#76247,#76248,#76249),
 .UNSPECIFIED.,.F.,.F.,(4,3,3,3,3,3,3,3,3,3,3,3,3,3,3,3,3,3,3,3,3,3,3,4),
(34.5575191897576,34.6600276231165,34.7624524447688,34.8648302599786,34.9671976054302,
35.0696598596281,35.1721712597493,35.2748625288798,35.3462402359454,35.4504266552236,
35.554457841936,35.6583670001104,35.7622107031371,35.8660237296966,35.9698408150375,
36.0737665685608,36.1777511656642,36.2819176875504,36.343768770382,36.4479637300599,
36.5519784470317,36.6558896321107,36.7597264522864,36.783721561275),
 .UNSPECIFIED.);
#2472=B_SPLINE_CURVE_WITH_KNOTS('',3,(#76250,#76251,#76252,#76253,#76254,
#76255,#76256,#76257,#76258,#76259,#76260,#76261,#76262,#76263,#76264,#76265,
#76266,#76267,#76268,#76269,#76270,#76271,#76272,#76273,#76274,#76275,#76276,
#76277,#76278,#76279,#76280,#76281,#76282,#76283,#76284,#76285,#76286,#76287,
#76288,#76289,#76290,#76291,#76292,#76293,#76294,#76295,#76296,#76297,#76298,
#76299,#76300,#76301,#76302,#76303,#76304,#76305,#76306,#76307,#76308,#76309,
#76310,#76311,#76312,#76313,#76314,#76315,#76316,#76317,#76318,#76319,#76320,
#76321,#76322,#76323,#76324,#76325,#76326,#76327,#76328,#76329,#76330,#76331,
#76332,#76333,#76334,#76335,#76336,#76337,#76338,#76339,#76340,#76341,#76342,
#76343,#76344,#76345,#76346,#76347,#76348,#76349,#76350,#76351,#76352,#76353,
#76354,#76355,#76356,#76357,#76358,#76359,#76360,#76361,#76362,#76363,#76364,
#76365,#76366,#76367,#76368,#76369,#76370,#76371,#76372,#76373),
 .UNSPECIFIED.,.F.,.F.,(4,3,3,3,3,3,3,3,3,3,3,3,3,3,3,3,3,3,3,3,3,3,3,3,
3,3,3,3,3,3,3,3,3,3,3,3,3,3,3,3,3,4),(30.5008964787964,30.6078001812217,
30.7116793516984,30.8155067886831,30.9193172495801,31.0285194617349,31.1324675695164,
31.2364884422478,31.3406776908237,31.356126098199,31.4603125242633,31.5643437178387,
31.6682528829569,31.7720965929731,31.8759096265576,31.9797267189483,32.0836524795105,
32.1876370836574,32.2918036125174,32.3536546326356,32.4578410526534,32.5618722401369,
32.6657813991261,32.7696251029939,32.8734381304197,32.9772552166507,33.0811809710951,
33.1851655691382,33.2893320919839,33.3511831670722,33.4553695843185,33.5594007689589,
33.6633099250119,33.7671536258876,33.8709666502698,33.9747837334102,34.0787094847129,
34.1826940795811,34.2868605992328,34.3487117015088,34.494592753444,34.5575191894877),
 .UNSPECIFIED.);
#2473=B_SPLINE_CURVE_WITH_KNOTS('',3,(#76379,#76380,#76381,#76382,#76383,
#76384,#76385,#76386,#76387,#76388,#76389,#76390,#76391,#76392,#76393,#76394,
#76395,#76396,#76397,#76398,#76399,#76400,#76401,#76402,#76403,#76404,#76405,
#76406,#76407,#76408,#76409,#76410,#76411,#76412,#76413,#76414,#76415,#76416,
#76417,#76418,#76419,#76420,#76421,#76422,#76423,#76424,#76425,#76426,#76427,
#76428,#76429,#76430,#76431,#76432,#76433,#76434,#76435,#76436,#76437,#76438,
#76439,#76440,#76441,#76442,#76443,#76444,#76445,#76446,#76447,#76448,#76449,
#76450,#76451,#76452,#76453,#76454,#76455,#76456,#76457,#76458,#76459,#76460,
#76461,#76462,#76463,#76464,#76465,#76466,#76467,#76468,#76469,#76470,#76471,
#76472,#76473,#76474,#76475,#76476,#76477,#76478,#76479,#76480,#76481,#76482,
#76483,#76484,#76485,#76486,#76487,#76488,#76489,#76490,#76491,#76492,#76493,
#76494,#76495,#76496,#76497,#76498,#76499),.UNSPECIFIED.,.F.,.F.,(4,3,3,
3,3,3,3,3,3,3,3,3,3,3,3,3,3,3,3,3,3,3,3,3,3,3,3,3,3,3,3,3,3,3,3,3,3,3,3,
3,4),(24.2175036368067,24.3213222069362,24.425134674074,24.5290492836921,
24.6330136088311,24.7371695294641,24.8294509519324,24.9336372113995,25.0376682356061,
25.1415772280614,25.2454207634752,25.3492336207785,25.4530505354683,25.556976117383,
25.6609605420786,25.7651268921614,25.826979486369,25.9311659551075,26.0351971917786,
26.1391064004061,26.2429501541627,26.346763231653,26.4505803680486,26.554506172462,
26.6584908204392,26.7626573926187,26.8245080208056,26.9286944520373,27.0327256510777,
27.1366348220792,27.2404785382343,27.3442915782043,27.448108677219,27.5520344447255,
27.6560190560083,27.7601855922317,27.8220365552422,27.9351108868929,28.0468017146056,
28.1605677982253,28.274333881845),.UNSPECIFIED.);
#2474=B_SPLINE_CURVE_WITH_KNOTS('',3,(#76500,#76501,#76502,#76503,#76504,
#76505,#76506,#76507,#76508,#76509,#76510,#76511,#76512,#76513,#76514,#76515,
#76516,#76517,#76518,#76519,#76520,#76521,#76522,#76523,#76524,#76525,#76526,
#76527,#76528,#76529,#76530,#76531,#76532,#76533,#76534,#76535,#76536,#76537,
#76538,#76539,#76540,#76541,#76542,#76543,#76544,#76545,#76546,#76547,#76548,
#76549,#76550,#76551,#76552,#76553,#76554,#76555,#76556,#76557,#76558,#76559,
#76560,#76561,#76562,#76563,#76564,#76565,#76566),.UNSPECIFIED.,.F.,.F.,
(4,3,3,3,3,3,3,3,3,3,3,3,3,3,3,3,3,3,3,3,3,3,4),(28.2743338823081,28.3811973775882,
28.4907893056108,28.5979678653913,28.7087664775351,28.8195650896788,28.9237515157247,
29.0277827092813,29.1316918743805,29.2355355843776,29.3393486179428,29.4431657103141,
29.5470914708569,29.6510760749844,29.7552426038252,29.8170936241154,29.9212582775505,
30.0252784744292,30.1291892265981,30.2330365854196,30.3368456659329,30.4406864383677,
30.4998648068842),.UNSPECIFIED.);
#2475=B_SPLINE_CURVE_WITH_KNOTS('',3,(#76568,#76569,#76570,#76571,#76572,
#76573,#76574,#76575,#76576,#76577,#76578,#76579,#76580,#76581,#76582,#76583,
#76584,#76585,#76586,#76587,#76588,#76589,#76590,#76591,#76592,#76593,#76594,
#76595,#76596,#76597,#76598,#76599,#76600,#76601,#76602,#76603,#76604,#76605,
#76606,#76607,#76608,#76609,#76610,#76611,#76612,#76613,#76614,#76615,#76616,
#76617,#76618,#76619,#76620,#76621,#76622,#76623,#76624,#76625,#76626,#76627,
#76628,#76629,#76630,#76631,#76632,#76633,#76634,#76635,#76636,#76637),
 .UNSPECIFIED.,.F.,.F.,(4,3,3,3,3,3,3,3,3,3,3,3,3,3,3,3,3,3,3,3,3,3,3,4),
(28.2743338823081,28.3635404948892,28.4677269637498,28.5717582005445,28.6756674092971,
28.7795111631798,28.8833242407966,28.9871413773194,29.0910671818599,29.1950518299642,
29.2992184022696,29.3610690293258,29.4652554605675,29.5692866596186,29.6731958306314,
29.7770395467982,29.8808525867803,29.9846696858073,30.0885954533271,30.1925800646233,
30.2967466008608,30.3585975637624,30.4627747459715,30.5008964787964),
 .UNSPECIFIED.);
#2476=B_SPLINE_CURVE_WITH_KNOTS('',3,(#76638,#76639,#76640,#76641,#76642,
#76643,#76644,#76645,#76646,#76647,#76648,#76649,#76650,#76651,#76652,#76653,
#76654,#76655,#76656,#76657,#76658,#76659,#76660,#76661,#76662,#76663,#76664,
#76665,#76666,#76667,#76668,#76669,#76670,#76671,#76672,#76673,#76674,#76675,
#76676,#76677,#76678,#76679,#76680,#76681,#76682,#76683,#76684,#76685,#76686,
#76687,#76688,#76689,#76690,#76691,#76692,#76693,#76694,#76695,#76696,#76697,
#76698,#76699,#76700,#76701,#76702,#76703,#76704,#76705,#76706,#76707,#76708,
#76709,#76710,#76711,#76712,#76713,#76714,#76715,#76716,#76717,#76718,#76719,
#76720,#76721,#76722,#76723,#76724,#76725,#76726,#76727,#76728,#76729,#76730,
#76731,#76732,#76733,#76734,#76735,#76736,#76737,#76738,#76739,#76740,#76741,
#76742,#76743,#76744,#76745,#76746,#76747,#76748,#76749,#76750,#76751,#76752,
#76753,#76754,#76755,#76756,#76757,#76758,#76759,#76760,#76761),
 .UNSPECIFIED.,.F.,.F.,(4,3,3,3,3,3,3,3,3,3,3,3,3,3,3,3,3,3,3,3,3,3,3,3,
3,3,3,3,3,3,3,3,3,3,3,3,3,3,3,3,3,4),(24.2166108235789,24.3207830822233,
24.3734263571428,24.4776114003836,24.5816411889067,24.6855489227878,24.7893911861822,
24.8932027599223,24.9970183813936,25.1009426642427,25.2049257846131,25.3090908361986,
25.3709548915794,25.4751416526421,25.5791731838078,25.683082688693,25.7869267396297,
25.890740114772,25.9945575488429,26.0984836488904,26.2024685917955,26.3066354545608,
26.368483426016,26.4726699930161,26.5767013313274,26.6806106461392,26.7844545088309,
26.8882676978477,26.9920849482059,27.0960108695371,27.1999956362766,27.3041623288664,
27.3660119604526,27.4689825721463,27.571778027722,27.6744756343169,27.7771117863559,
27.8797227939149,27.982409657317,28.0851324763853,28.1880251693553,28.2743338818544),
 .UNSPECIFIED.);
#2477=B_SPLINE_CURVE_WITH_KNOTS('',3,(#76767,#76768,#76769,#76770,#76771,
#76772,#76773,#76774,#76775,#76776,#76777,#76778,#76779,#76780,#76781,#76782,
#76783,#76784,#76785,#76786,#76787,#76788,#76789,#76790,#76791,#76792,#76793,
#76794,#76795,#76796,#76797,#76798,#76799,#76800,#76801,#76802,#76803,#76804,
#76805,#76806,#76807,#76808,#76809,#76810,#76811,#76812,#76813,#76814,#76815,
#76816,#76817,#76818,#76819,#76820,#76821,#76822,#76823,#76824,#76825,#76826,
#76827,#76828,#76829,#76830,#76831,#76832,#76833,#76834,#76835,#76836),
 .UNSPECIFIED.,.F.,.F.,(4,3,3,3,3,3,3,3,3,3,3,3,3,3,3,3,3,3,3,3,3,3,3,4),
(15.7079632679489,15.8108073354867,15.9136172573649,16.0164289991591,16.1193514864967,
16.2223328513092,16.3255044670683,16.39319808165,16.4974235198284,16.6014922383089,
16.7054365135598,16.8093138195759,16.9131588800528,17.0170063736613,17.1209598212046,
17.2249706213236,17.3291606840235,17.3907266160866,17.4950704275919,17.5992688650338,
17.7033463786647,17.8073550699353,17.9113373205562,17.9338028153519),
 .UNSPECIFIED.);
#2478=B_SPLINE_CURVE_WITH_KNOTS('',3,(#76838,#76839,#76840,#76841,#76842),
 .UNSPECIFIED.,.F.,.F.,(4,1,4),(14.3981410127768,15.3956695472134,15.7079548702164),
 .UNSPECIFIED.);
#2479=B_SPLINE_CURVE_WITH_KNOTS('',3,(#76846,#76847,#76848,#76849,#76850,
#76851,#76852,#76853,#76854,#76855,#76856,#76857,#76858,#76859,#76860,#76861,
#76862,#76863,#76864,#76865,#76866,#76867,#76868,#76869,#76870,#76871,#76872,
#76873,#76874,#76875,#76876,#76877,#76878,#76879,#76880,#76881,#76882,#76883,
#76884,#76885,#76886,#76887,#76888,#76889,#76890,#76891,#76892,#76893,#76894,
#76895,#76896,#76897,#76898,#76899,#76900,#76901,#76902,#76903),
 .UNSPECIFIED.,.F.,.F.,(4,3,3,3,3,3,3,3,3,3,3,3,3,3,3,3,3,3,3,4),(13.876192946452,
13.9800533582401,14.0837577779462,14.1873396637409,14.2908563334949,14.3943430362838,
14.4978349779569,14.6014337917251,14.7050934743387,14.808926820442,14.8541656075664,
14.9608903150641,15.0635179865448,15.1660515661335,15.2685276102982,15.3709825929619,
15.4735044996228,15.5760669133534,15.6787651048717,15.7079632675479),
 .UNSPECIFIED.);
#2480=B_SPLINE_CURVE_WITH_KNOTS('',3,(#76904,#76905,#76906,#76907,#76908,
#76909,#76910,#76911,#76912,#76913,#76914,#76915,#76916,#76917,#76918,#76919,
#76920,#76921,#76922,#76923,#76924,#76925,#76926,#76927,#76928,#76929,#76930,
#76931,#76932,#76933,#76934,#76935,#76936,#76937,#76938,#76939,#76940,#76941,
#76942,#76943,#76944,#76945,#76946,#76947,#76948,#76949,#76950,#76951,#76952,
#76953,#76954,#76955,#76956,#76957,#76958,#76959,#76960,#76961,#76962,#76963,
#76964,#76965,#76966,#76967,#76968,#76969,#76970),.UNSPECIFIED.,.F.,.F.,
(4,3,3,3,3,3,3,3,3,3,3,3,3,3,3,3,3,3,3,3,3,3,4),(15.7079632679489,15.851694142003,
15.9557857876061,16.0597208362763,16.1635322938407,16.2672773831501,16.3709910283821,
16.474708109403,16.5785335927115,16.6824176162874,16.7864841764974,16.8492226764396,
16.9534205085217,17.0574630546861,17.1613834350916,17.2652382690518,17.3690623180458,
17.4728903000167,17.5768266804211,17.6808217681209,17.7849984488684,17.8467512108762,
17.9343860550099),.UNSPECIFIED.);
#2481=B_SPLINE_CURVE_WITH_KNOTS('',3,(#76976,#76977,#76978,#76979,#76980,
#76981,#76982,#76983,#76984,#76985,#76986,#76987,#76988,#76989,#76990,#76991,
#76992,#76993,#76994,#76995,#76996,#76997,#76998,#76999,#77000,#77001,#77002,
#77003,#77004,#77005,#77006,#77007,#77008,#77009,#77010,#77011,#77012,#77013,
#77014,#77015,#77016,#77017,#77018,#77019,#77020,#77021,#77022,#77023,#77024,
#77025,#77026,#77027,#77028,#77029,#77030,#77031,#77032,#77033,#77034,#77035,
#77036,#77037,#77038,#77039,#77040,#77041,#77042,#77043,#77044,#77045,#77046,
#77047,#77048,#77049,#77050,#77051,#77052,#77053,#77054,#77055,#77056,#77057,
#77058,#77059,#77060,#77061,#77062,#77063,#77064,#77065,#77066,#77067,#77068,
#77069,#77070,#77071,#77072,#77073,#77074,#77075,#77076,#77077,#77078,#77079,
#77080,#77081,#77082,#77083,#77084,#77085,#77086,#77087,#77088,#77089,#77090,
#77091,#77092,#77093,#77094,#77095,#77096,#77097,#77098,#77099,#77100,#77101,
#77102,#77103,#77104,#77105,#77106,#77107,#77108,#77109,#77110,#77111,#77112,
#77113,#77114,#77115,#77116,#77117,#77118,#77119,#77120,#77121,#77122,#77123,
#77124,#77125,#77126,#77127,#77128,#77129,#77130,#77131,#77132,#77133,#77134,
#77135),.UNSPECIFIED.,.F.,.F.,(4,2,2,2,2,2,2,2,2,2,2,2,2,2,2,2,2,2,2,2,
2,2,2,2,2,2,2,2,2,2,2,2,2,2,2,2,2,2,2,2,2,2,2,2,2,2,2,2,2,2,2,2,2,2,2,2,
2,2,2,2,2,2,2,2,2,2,2,2,2,2,2,2,2,2,2,2,2,2,2,4),(-0.808582078280263,-0.80375073768972,
-0.763920677015728,-0.755667383612783,-0.751902546185843,-0.748972705871124,
-0.745765490437097,-0.740511666997364,-0.719054979581247,-0.698469123996048,
-0.691966489838367,-0.67237433173504,-0.668941290065012,-0.667023804346531,
-0.665537202421465,-0.663440042769142,-0.659063952645029,-0.64112942335304,
-0.609237968511569,-0.591965807738614,-0.586791483937901,-0.583578373841748,
-0.580606300588323,-0.576666400900211,-0.567786316437348,-0.555350092855608,
-0.532818709676239,-0.507841569834796,-0.503028355554244,-0.50086668124496,
-0.499194036422899,-0.497221122700889,-0.493559006971449,-0.488855239208183,
-0.477797482513651,-0.456889868740997,-0.42796259767417,-0.422295691517184,
-0.418968054825641,-0.416007159183182,-0.412245096918113,-0.404420574707277,
-0.393962693740305,-0.367392504352035,-0.342227416889973,-0.337519843331241,
-0.335359327113237,-0.333720281885442,-0.331917834124533,-0.328671895219693,
-0.310469648551046,-0.274329221166817,-0.257188758276896,-0.252160820829705,
-0.24907621421,-0.246251410997066,-0.242552690871855,-0.234441434443417,
-0.215777455632103,-0.187749031893301,-0.171748096241792,-0.168479233864655,
-0.166625078437752,-0.164969301318631,-0.163326004565586,-0.159703725776366,
-0.154866878239808,-0.143406084942028,-0.108936770040443,-0.0861876884502441,
-0.0802883743038012,-0.0767059478252727,-0.0734364140006466,-0.069152157193184,
-0.0595717908539198,-0.0329949830249145,-0.00749777013076311,-0.00328705758577433,
-0.00149796591859924,-5.90712218287499E-5),.UNSPECIFIED.);
#2482=B_SPLINE_CURVE_WITH_KNOTS('',3,(#77139,#77140,#77141,#77142,#77143,
#77144,#77145,#77146,#77147,#77148,#77149,#77150),.UNSPECIFIED.,.F.,.F.,
(4,2,2,2,2,4),(-1.15749903584995,-1.15636148542137,-1.15405073254735,-1.14499624866471,
-1.11159362809321,-1.10921304536313),.UNSPECIFIED.);
#2483=B_SPLINE_CURVE_WITH_KNOTS('',3,(#77154,#77155,#77156,#77157,#77158,
#77159,#77160,#77161,#77162,#77163,#77164,#77165,#77166,#77167,#77168,#77169,
#77170,#77171,#77172,#77173,#77174,#77175,#77176,#77177,#77178,#77179,#77180,
#77181,#77182,#77183,#77184,#77185,#77186,#77187,#77188,#77189,#77190,#77191,
#77192,#77193,#77194,#77195,#77196,#77197,#77198,#77199,#77200,#77201,#77202,
#77203,#77204,#77205,#77206,#77207,#77208,#77209,#77210,#77211,#77212,#77213,
#77214,#77215,#77216,#77217,#77218,#77219,#77220,#77221,#77222,#77223,#77224,
#77225,#77226,#77227,#77228,#77229,#77230,#77231,#77232,#77233,#77234,#77235,
#77236,#77237,#77238,#77239,#77240,#77241,#77242,#77243,#77244,#77245,#77246,
#77247,#77248,#77249,#77250,#77251,#77252,#77253,#77254,#77255,#77256,#77257,
#77258,#77259,#77260,#77261,#77262,#77263,#77264,#77265,#77266,#77267,#77268,
#77269,#77270,#77271,#77272,#77273,#77274,#77275,#77276,#77277,#77278,#77279,
#77280,#77281,#77282,#77283,#77284,#77285,#77286,#77287,#77288,#77289,#77290,
#77291,#77292,#77293,#77294,#77295,#77296,#77297,#77298,#77299,#77300,#77301,
#77302,#77303,#77304,#77305,#77306,#77307,#77308,#77309,#77310,#77311,#77312,
#77313,#77314,#77315,#77316,#77317,#77318,#77319,#77320,#77321,#77322,#77323,
#77324,#77325,#77326,#77327,#77328,#77329,#77330,#77331,#77332,#77333,#77334,
#77335,#77336,#77337,#77338,#77339,#77340,#77341,#77342,#77343,#77344,#77345,
#77346,#77347,#77348,#77349,#77350,#77351,#77352,#77353,#77354,#77355,#77356,
#77357,#77358,#77359,#77360,#77361,#77362,#77363,#77364,#77365,#77366,#77367,
#77368,#77369,#77370,#77371,#77372,#77373,#77374,#77375,#77376,#77377,#77378,
#77379,#77380,#77381,#77382,#77383,#77384,#77385,#77386,#77387,#77388,#77389,
#77390,#77391,#77392,#77393,#77394,#77395,#77396,#77397,#77398,#77399,#77400,
#77401,#77402,#77403,#77404,#77405,#77406,#77407,#77408,#77409,#77410,#77411,
#77412,#77413,#77414,#77415,#77416,#77417,#77418,#77419,#77420,#77421,#77422,
#77423,#77424,#77425,#77426,#77427,#77428,#77429,#77430,#77431,#77432,#77433,
#77434,#77435,#77436,#77437,#77438,#77439,#77440,#77441,#77442,#77443,#77444,
#77445),.UNSPECIFIED.,.F.,.F.,(4,2,2,2,2,2,2,2,2,2,2,2,2,2,2,2,2,2,2,2,
2,2,2,2,2,2,2,2,2,2,2,2,2,2,2,2,2,2,2,2,2,2,2,2,2,2,2,2,2,2,2,2,2,2,2,2,
2,2,2,2,2,2,2,2,2,2,2,2,2,2,2,2,2,2,2,2,2,2,2,2,2,2,2,2,2,2,2,2,2,2,2,2,
2,2,2,2,2,2,2,2,2,2,2,2,2,2,2,2,2,2,2,2,2,2,2,2,2,2,2,2,2,2,2,2,2,2,2,2,
2,2,2,2,2,2,2,2,2,2,2,2,2,2,2,2,2,4),(-1.10921304536313,-1.08577119322405,
-1.08023789382835,-1.07693925638659,-1.07397418658779,-1.07016513228311,
-1.06395257927994,-1.02008265239652,-1.00173885418572,-0.997298899019347,
-0.995588566735163,-0.995518644712131,-0.995448796458939,-0.995377673235652,
-0.995303608163833,-0.995224348210243,-0.995136529222863,-0.995034488957759,
-0.994906967059261,-0.994779717941947,-0.993170997624818,-0.991039059035374,
-0.986280553047312,-0.96227438564749,-0.941787766874852,-0.927527236686034,
-0.917726530430184,-0.913636099260019,-0.910640938109294,-0.907486036037498,
-0.902582190720856,-0.887581496086737,-0.851324751753463,-0.834868822453056,
-0.830557604876965,-0.828473231876027,-0.82698835841122,-0.825062426160662,
-0.821590084065918,-0.800290720371377,-0.795867224537264,-0.775684410828935,
-0.753556406652984,-0.748263067150557,-0.745047955270015,-0.742121360064723,
-0.738375163877525,-0.732140151813139,-0.694444213623796,-0.666722858872337,
-0.663180423026752,-0.661263327820058,-0.659617512803783,-0.6574789506901,
-0.652903880244482,-0.623419046990851,-0.599108331163135,-0.589793535635475,
-0.582645542039741,-0.579032101247776,-0.576107409243365,-0.572733150550537,
-0.566760214001137,-0.534475438739381,-0.501610642558943,-0.497186242311823,
-0.495081501618787,-0.49343462931103,-0.491444869845802,-0.487594369368031,
-0.482557469483099,-0.470221161640095,-0.433104684538486,-0.419066668075373,
-0.414282975853528,-0.411164265394002,-0.408174001606482,-0.404043224012585,
-0.393904338163363,-0.378936396887228,-0.359032533171688,-0.356815362649411,
-0.333515590386699,-0.330024186704325,-0.328089209449799,-0.326440947869545,
-0.324273025928824,-0.319485762091414,-0.297570820176915,-0.2567206097833,
-0.249607788516314,-0.245959424378439,-0.243038154814013,-0.239702603673773,
-0.233891197218771,-0.198245857868445,-0.168549564860159,-0.163927082024161,
-0.16181214618442,-0.160223079670209,-0.160199713943012,-0.160162681572964,
-0.160127591614206,-0.160094253908694,-0.16006250290469,-0.160032193600147,
-0.160003198416574,-0.159975404506412,-0.159948711611694,-0.159923030353875,
-0.159898280637115,-0.159874390473207,-0.159851294966483,-0.159828935373871,
-0.159807258363925,-0.159786215393173,-0.159765762141485,-0.159745858072496,
-0.159726465948691,-0.159707551462467,-0.159689083040975,-0.15967103147113,
-0.15965336966453,-0.159636072497843,-0.15961911659791,-0.159602480131411,
-0.159586142697773,-0.159570085204795,-0.159554289786106,-0.159538739575203,
-0.159523418664764,-0.159508312135062,-0.159493405771622,-0.159478686223586,
-0.15946414071833,-0.159449757148495,-0.15727084496776,-0.154692765577617,
-0.12620987529064,-0.0896910803513349,-0.0833849232407711,-0.0796082418622991,
-0.0766641226864439,-0.0734356955169596,-0.0681330712760033,-0.0594613373173496),
 .UNSPECIFIED.);
#2484=B_SPLINE_CURVE_WITH_KNOTS('',3,(#77450,#77451,#77452,#77453,#77454,
#77455,#77456,#77457,#77458,#77459,#77460,#77461,#77462,#77463,#77464,#77465,
#77466,#77467,#77468,#77469,#77470,#77471,#77472,#77473,#77474,#77475,#77476,
#77477,#77478,#77479,#77480,#77481,#77482,#77483,#77484,#77485,#77486,#77487,
#77488,#77489,#77490,#77491,#77492,#77493,#77494,#77495,#77496,#77497,#77498,
#77499,#77500,#77501,#77502,#77503,#77504,#77505,#77506,#77507,#77508,#77509,
#77510,#77511,#77512,#77513,#77514,#77515,#77516,#77517,#77518,#77519,#77520,
#77521,#77522,#77523,#77524,#77525,#77526,#77527,#77528,#77529,#77530,#77531,
#77532,#77533,#77534,#77535,#77536,#77537,#77538,#77539,#77540,#77541,#77542,
#77543,#77544,#77545,#77546,#77547,#77548,#77549,#77550,#77551,#77552,#77553,
#77554,#77555,#77556,#77557,#77558,#77559,#77560,#77561,#77562,#77563,#77564,
#77565,#77566,#77567,#77568,#77569,#77570,#77571,#77572,#77573,#77574,#77575,
#77576,#77577,#77578,#77579,#77580,#77581,#77582,#77583,#77584,#77585,#77586,
#77587,#77588,#77589,#77590,#77591,#77592,#77593,#77594,#77595,#77596,#77597,
#77598,#77599,#77600,#77601,#77602,#77603,#77604,#77605,#77606,#77607,#77608,
#77609,#77610,#77611,#77612,#77613,#77614,#77615,#77616,#77617,#77618,#77619,
#77620,#77621,#77622,#77623,#77624,#77625,#77626,#77627,#77628,#77629,#77630,
#77631,#77632,#77633,#77634,#77635,#77636,#77637,#77638,#77639,#77640,#77641,
#77642,#77643,#77644,#77645,#77646,#77647,#77648,#77649,#77650,#77651,#77652,
#77653,#77654,#77655,#77656,#77657),.UNSPECIFIED.,.F.,.F.,(4,2,2,2,2,2,
2,2,2,2,2,2,2,2,2,2,2,2,2,2,2,2,2,2,2,2,2,2,2,2,2,2,2,2,2,2,2,2,2,2,2,2,
2,2,2,2,2,2,2,2,2,2,2,2,2,2,2,2,2,2,2,2,2,2,2,2,2,2,2,2,2,2,2,2,2,2,2,2,
2,2,2,2,2,2,2,2,2,2,2,2,2,2,2,2,2,2,2,2,2,2,2,2,2,4),(-1.85845337396871,
-1.84131054128932,-1.83654050741002,-1.83437450613097,-1.83274032618178,
-1.8308085474797,-1.82733226476466,-1.80641330329208,-1.800721727262,-1.77859509583064,
-1.75897648724238,-1.75382760231245,-1.75107863399526,-1.74815434146029,
-1.74450217234471,-1.7373814774257,-1.70622943200099,-1.68262934433417,
-1.67521982763483,-1.67006229476785,-1.66782815892246,-1.66617172039623,
-1.66427600621078,-1.66096075542767,-1.64528537056015,-1.61447922017851,
-1.59259734538965,-1.58729948150606,-1.58407142410794,-1.58112602325968,
-1.57734545413148,-1.57102772809561,-1.53473165997819,-1.51479785309131,
-1.50804367998779,-1.50323002005008,-1.50105606062821,-1.49942077879233,
-1.49749331889511,-1.49403841837235,-1.47415479593914,-1.46751760455528,
-1.44626826366349,-1.42578977715592,-1.42058038169334,-1.41737090220697,
-1.41441928374303,-1.41059818004274,-1.40209463227193,-1.36272680903702,
-1.34128070722827,-1.33653756879021,-1.33437636584309,-1.33274297467705,
-1.3308091670142,-1.3273206300265,-1.30478747307554,-1.30170640644457,-1.28561597609658,
-1.25963304110213,-1.25413261511685,-1.25086235852088,-1.24792918292639,
-1.2441714462761,-1.23807125582121,-1.19226605905035,-1.17402877644563,
-1.16962605528447,-1.16752865379655,-1.16604280349328,-1.16412269273341,
-1.16070055814407,-1.14311916245153,-1.09804723870709,-1.08934485135883,
-1.08544688816033,-1.08249301169568,-1.07928693534511,-1.07409625673538,
-1.05598924312224,-1.02459983214061,-1.01174143731849,-1.006567743755,-1.00263637235194,
-1.00062975715949,-0.998983161499943,-0.996896536437269,-0.992569322989255,
-0.958661648316373,-0.926714267688992,-0.921025653446815,-0.917711004123216,
-0.915071655499159,-0.911511952038025,-0.904639602485034,-0.87976139783165,
-0.862527766013537,-0.839367510086651,-0.835876542736559,-0.83394148237466,
-0.832298907904304,-0.830144395165269,-0.825392215126631,-0.808582078280263),
 .UNSPECIFIED.);
#2485=B_SPLINE_CURVE_WITH_KNOTS('',3,(#77659,#77660,#77661,#77662,#77663,
#77664,#77665,#77666,#77667,#77668),.UNSPECIFIED.,.F.,.F.,(4,2,2,2,4),(-0.0594613373173496,
-0.0461429177535532,-0.0258669114392458,-0.00683129514723689,-0.000519912267460154),
 .UNSPECIFIED.);
#2486=B_SPLINE_CURVE_WITH_KNOTS('',3,(#77669,#77670,#77671,#77672,#77673,
#77674,#77675,#77676,#77677,#77678,#77679),.UNSPECIFIED.,.F.,.F.,(4,2,1,
1,1,1,1,4),(-91.8109775642065,-91.7726251681672,-90.7750966337306,-89.777568099294,
-88.7800395648574,-87.7825110304208,-86.7849824959842,-85.8810481731868),
 .UNSPECIFIED.);
#2487=B_SPLINE_CURVE_WITH_KNOTS('',3,(#77685,#77686,#77687,#77688,#77689,
#77690,#77691,#77692,#77693,#77694,#77695,#77696,#77697,#77698,#77699,#77700,
#77701,#77702,#77703,#77704,#77705,#77706,#77707,#77708,#77709,#77710,#77711,
#77712,#77713,#77714,#77715,#77716,#77717,#77718,#77719,#77720,#77721,#77722,
#77723,#77724,#77725,#77726,#77727,#77728,#77729,#77730,#77731,#77732,#77733,
#77734,#77735,#77736,#77737,#77738,#77739,#77740,#77741,#77742,#77743,#77744,
#77745,#77746,#77747,#77748,#77749,#77750,#77751,#77752,#77753,#77754,#77755,
#77756,#77757,#77758,#77759,#77760,#77761,#77762,#77763,#77764,#77765,#77766,
#77767,#77768,#77769,#77770,#77771,#77772,#77773,#77774,#77775,#77776,#77777,
#77778,#77779,#77780,#77781,#77782,#77783,#77784,#77785,#77786,#77787,#77788,
#77789,#77790,#77791,#77792,#77793,#77794,#77795,#77796,#77797,#77798,#77799,
#77800,#77801,#77802,#77803,#77804,#77805,#77806,#77807,#77808,#77809,#77810,
#77811,#77812,#77813,#77814,#77815,#77816,#77817,#77818,#77819,#77820,#77821,
#77822,#77823,#77824,#77825,#77826,#77827,#77828,#77829,#77830,#77831,#77832,
#77833,#77834,#77835,#77836,#77837,#77838,#77839,#77840,#77841,#77842,#77843,
#77844,#77845,#77846,#77847,#77848,#77849,#77850,#77851,#77852,#77853,#77854,
#77855,#77856,#77857,#77858,#77859,#77860,#77861,#77862,#77863,#77864,#77865,
#77866,#77867,#77868,#77869,#77870,#77871,#77872),.UNSPECIFIED.,.F.,.F.,
(4,2,2,2,2,2,2,2,2,2,2,2,2,2,2,2,2,2,2,2,2,2,2,2,2,2,2,2,2,2,2,2,2,2,2,
2,2,2,2,2,2,2,2,2,2,2,2,2,2,2,2,2,2,2,2,2,2,2,2,2,2,2,2,2,2,2,2,2,2,2,2,
2,2,2,2,2,2,2,2,2,2,2,2,2,2,2,2,2,2,2,2,2,2,4),(-0.991334733589914,-0.990102265102668,
-0.964597591785105,-0.944430702475018,-0.922441130210619,-0.918953660764064,
-0.917019267435139,-0.915385370687477,-0.913222894564673,-0.908472467431247,
-0.88695149042055,-0.847366140145738,-0.839045619107897,-0.835256909385074,
-0.832310459919263,-0.82908661118544,-0.823808030704901,-0.802238109082765,
-0.781752229472162,-0.775474297656371,-0.755707750683598,-0.752256661904654,
-0.750330456779003,-0.748695459417471,-0.746521044894084,-0.741703984253366,
-0.734942453136958,-0.714971305485189,-0.678691251199009,-0.672370362892898,
-0.668589043069049,-0.665643697933355,-0.662416351976517,-0.657121145870946,
-0.635274293929251,-0.604531306456788,-0.588806529328377,-0.58548779833751,
-0.583591332459823,-0.581935073317462,-0.579702289154817,-0.574552854601264,
-0.567158177300022,-0.543651482000971,-0.512297228346512,-0.505205411759204,
-0.501559138690346,-0.498635250985148,-0.495291976109734,-0.489454413729528,
-0.455740342694028,-0.423984861309953,-0.419542819874911,-0.417407110622622,
-0.415760662980193,-0.413800941799578,-0.410092643436106,-0.381161874569464,
-0.345381283411759,-0.339035085119007,-0.335246690997869,-0.332300445847088,
-0.329076779607281,-0.323798404474412,-0.302227641210784,-0.281744814060202,
-0.275469268701799,-0.255702403588537,-0.252251495373005,-0.250325406847744,
-0.248690516096501,-0.246516257422108,-0.241699609367859,-0.234938715713343,
-0.21497000995162,-0.178708160723568,-0.172377387379905,-0.168593392444139,
-0.165647817545095,-0.1629120783284,-0.158110450006515,-0.142566963737101,
-0.116188035330296,-0.0911116313795588,-0.086383436873767,-0.0842153247984322,
-0.0825623561530884,-0.0806501880045891,-0.0771677145706554,-0.0547810151635225,
-0.0157430710729671,-0.00643938555809663,-0.00281936615891565,-0.000491738252050606),
 .UNSPECIFIED.);
#2488=B_SPLINE_CURVE_WITH_KNOTS('',3,(#77873,#77874,#77875,#77876,#77877,
#77878,#77879,#77880,#77881,#77882,#77883,#77884,#77885,#77886),
 .UNSPECIFIED.,.F.,.F.,(4,2,2,2,2,2,4),(-1.91741621048356,-1.91647148486793,
-1.91479231205858,-1.91153539840836,-1.90506053883497,-1.8630301192281,
-1.85845337396871),.UNSPECIFIED.);
#2489=B_SPLINE_CURVE_WITH_KNOTS('',3,(#77888,#77889,#77890,#77891,#77892),
 .UNSPECIFIED.,.F.,.F.,(4,1,4),(-85.8810481731868,-85.7874539615476,-85.5277944654987),
 .UNSPECIFIED.);
#2490=B_SPLINE_CURVE_WITH_KNOTS('',3,(#77893,#77894,#77895,#77896,#77897,
#77898,#77899,#77900,#77901,#77902,#77903,#77904,#77905,#77906,#77907,#77908,
#77909,#77910,#77911,#77912,#77913,#77914,#77915,#77916,#77917,#77918,#77919,
#77920,#77921,#77922,#77923,#77924,#77925,#77926,#77927,#77928,#77929,#77930,
#77931,#77932,#77933,#77934,#77935,#77936,#77937,#77938,#77939,#77940,#77941,
#77942,#77943,#77944,#77945,#77946,#77947,#77948,#77949,#77950,#77951,#77952,
#77953,#77954,#77955,#77956,#77957,#77958,#77959,#77960,#77961,#77962,#77963,
#77964,#77965,#77966,#77967,#77968,#77969,#77970,#77971,#77972,#77973,#77974,
#77975,#77976,#77977,#77978,#77979,#77980,#77981,#77982,#77983,#77984,#77985,
#77986,#77987,#77988,#77989,#77990,#77991,#77992,#77993,#77994,#77995,#77996,
#77997,#77998,#77999,#78000,#78001,#78002,#78003,#78004,#78005,#78006,#78007,
#78008,#78009,#78010,#78011,#78012,#78013,#78014,#78015,#78016,#78017,#78018,
#78019,#78020,#78021,#78022,#78023,#78024,#78025,#78026,#78027,#78028,#78029,
#78030,#78031,#78032,#78033,#78034,#78035,#78036,#78037,#78038,#78039,#78040,
#78041,#78042,#78043,#78044,#78045,#78046,#78047,#78048,#78049,#78050,#78051,
#78052,#78053,#78054,#78055,#78056,#78057,#78058,#78059,#78060,#78061,#78062,
#78063,#78064,#78065,#78066,#78067,#78068,#78069,#78070,#78071,#78072,#78073,
#78074,#78075,#78076,#78077,#78078,#78079,#78080,#78081,#78082,#78083,#78084,
#78085,#78086,#78087,#78088,#78089,#78090),.UNSPECIFIED.,.F.,.F.,(4,2,2,
2,2,2,2,2,2,2,2,2,2,2,2,2,2,2,2,2,2,2,2,2,2,2,2,2,2,2,2,2,2,2,2,2,2,2,2,
2,2,2,2,2,2,2,2,2,2,2,2,2,2,2,2,2,2,2,2,2,2,2,2,2,2,2,2,2,2,2,2,2,2,2,2,
2,2,2,2,2,2,2,2,2,2,2,2,2,2,2,2,2,2,2,2,2,2,2,4),(-2.10003485435709,-2.07850560390307,
-2.06873850594009,-2.06499512105155,-2.06212405960105,-2.05917970464634,
-2.05595308752978,-2.0506582991449,-2.03115413057728,-2.00232285686385,
-1.98394654317753,-1.97972213189053,-1.9776034371064,-1.97611556214451,
-1.97421137067608,-1.9708566830803,-1.9545420992892,-1.92445096184892,-1.90257565119817,
-1.89727962506651,-1.89405281362857,-1.89110865072312,-1.88732983556868,
-1.88101550585438,-1.84455493658851,-1.82474049876445,-1.81801017899794,
-1.81320971901879,-1.81103873882641,-1.80940457509716,-1.80747733747423,
-1.8040198242005,-1.7839732054177,-1.77747686119903,-1.75580139364505,-1.73570783528188,
-1.73052646350142,-1.72732419823762,-1.72437261414037,-1.72054225281815,
-1.71197739413161,-1.67268402166767,-1.65126173154683,-1.64652181929395,
-1.64436172820778,-1.64272858427348,-1.64079390156835,-1.63730318445725,
-1.6141414406195,-1.59690412174929,-1.5720310402902,-1.56516535075129,-1.56161078295364,
-1.55897608281634,-1.55566847969271,-1.54999567083819,-1.52030823166117,
-1.49905667838791,-1.48772979684491,-1.48073863687029,-1.47822619213792,
-1.47652360855114,-1.47474404827802,-1.47187015349627,-1.46259104948464,
-1.45418552540459,-1.42469859942303,-1.40264392524141,-1.39733718731262,
-1.39410802915073,-1.39116441707891,-1.38739003477805,-1.38109155753135,
-1.3444838638238,-1.32475599329554,-1.31804238698899,-1.31325084264328,
-1.31108143716655,-1.30943262390914,-1.30749800166354,-1.30400746472248,
-1.28087720299464,-1.26368381722062,-1.23874917991307,-1.23187568466448,
-1.22831959923908,-1.225684791166,-1.22237837499058,-1.21671095986433,-1.18591530836976,
-1.16106502622968,-1.1526483558149,-1.14698507190639,-1.14466756337246,
-1.14299980239345,-1.14114779056651,-1.13794310521154,-1.12491860040256,
-1.10913431935646),.UNSPECIFIED.);
#2491=B_SPLINE_CURVE_WITH_KNOTS('',3,(#78095,#78096,#78097,#78098,#78099,
#78100,#78101,#78102,#78103,#78104,#78105,#78106,#78107,#78108,#78109,#78110,
#78111,#78112,#78113,#78114,#78115,#78116,#78117,#78118,#78119,#78120,#78121,
#78122,#78123,#78124,#78125,#78126,#78127,#78128,#78129,#78130,#78131,#78132,
#78133,#78134,#78135,#78136,#78137,#78138,#78139,#78140,#78141,#78142,#78143,
#78144,#78145,#78146,#78147,#78148,#78149,#78150,#78151,#78152,#78153,#78154,
#78155,#78156,#78157,#78158,#78159,#78160,#78161,#78162,#78163,#78164,#78165,
#78166,#78167,#78168,#78169,#78170,#78171,#78172,#78173,#78174,#78175,#78176,
#78177,#78178,#78179,#78180,#78181,#78182,#78183,#78184,#78185,#78186,#78187,
#78188,#78189,#78190,#78191,#78192,#78193,#78194,#78195,#78196,#78197,#78198,
#78199,#78200,#78201,#78202,#78203,#78204,#78205,#78206,#78207,#78208,#78209,
#78210,#78211,#78212,#78213,#78214,#78215,#78216,#78217,#78218,#78219,#78220,
#78221,#78222,#78223,#78224,#78225,#78226,#78227,#78228,#78229,#78230,#78231,
#78232,#78233,#78234,#78235,#78236,#78237,#78238,#78239,#78240,#78241,#78242,
#78243,#78244,#78245,#78246,#78247,#78248,#78249,#78250,#78251,#78252,#78253,
#78254,#78255,#78256,#78257,#78258,#78259,#78260,#78261,#78262,#78263,#78264,
#78265,#78266,#78267,#78268,#78269,#78270,#78271,#78272,#78273,#78274,#78275,
#78276,#78277,#78278,#78279,#78280,#78281,#78282,#78283,#78284,#78285,#78286,
#78287,#78288,#78289,#78290,#78291,#78292,#78293,#78294,#78295,#78296,#78297,
#78298,#78299,#78300,#78301,#78302,#78303,#78304),.UNSPECIFIED.,.F.,.F.,
(4,2,2,2,2,2,2,2,2,2,2,2,2,2,2,2,2,2,2,2,2,2,2,2,2,2,2,2,2,2,2,2,2,2,2,
2,2,2,2,2,2,2,2,2,2,2,2,2,2,2,2,2,2,2,2,2,2,2,2,2,2,2,2,2,2,2,2,2,2,2,2,
2,2,2,2,2,2,2,2,2,2,2,2,2,2,2,2,2,2,2,2,2,2,2,2,2,2,2,2,2,2,2,2,2,4),(-2.041194238912,
-2.03308372227273,-2.01726389886191,-2.0100937942116,-2.00425724602399,
-2.00091395364408,-1.99798971438316,-1.99434256101024,-1.98724757679346,
-1.95633935560485,-1.93251464995055,-1.92506779672676,-1.91989088397756,
-1.9176532671926,-1.91599624905273,-1.91410220792294,-1.91079468905737,
-1.89530638199369,-1.86642842142523,-1.85060179359057,-1.84342975318844,
-1.83759200180659,-1.83424849980843,-1.83132435512702,-1.82767768415656,
-1.82058481152324,-1.78944983567494,-1.76579967476789,-1.75838164414872,
-1.75321960883726,-1.75098456727759,-1.74932790299428,-1.74743247440499,
-1.74411871213512,-1.72847022164124,-1.69766006537984,-1.67575727173645,
-1.67045817199177,-1.66722984744401,-1.66428451698462,-1.66050447606793,
-1.6541886432,-1.61784983238833,-1.58922739944954,-1.58565204897448,-1.58372004111667,
-1.58207005196638,-1.57993117280608,-1.57518446704707,-1.54959169305137,
-1.52725906575456,-1.51487375200263,-1.50602654743202,-1.5021047729433,
-1.4991485047876,-1.49595491192632,-1.49081825693143,-1.47376538737418,
-1.44182880612635,-1.42385444566274,-1.41948071598479,-1.41738826965094,
-1.41590272101662,-1.41397871877751,-1.41053796856741,-1.39118285066854,
-1.38414460233122,-1.36318504073295,-1.34930407770668,-1.33969492554978,
-1.33564720283574,-1.33267117065915,-1.32952571297752,-1.32461490616774,
-1.30940992439892,-1.27658245477355,-1.25739919109829,-1.25289103087495,
-1.25077314971435,-1.24928480724988,-1.24737851483225,-1.24401677610271,
-1.22756277939691,-1.19779757004878,-1.17575557117689,-1.17044806709,-1.16721785387563,
-1.16427288196664,-1.16049618293017,-1.15224468715182,-1.11260314132832,
-1.09106874607068,-1.08631678512989,-1.08415395671605,-1.08251992867439,
-1.08058557322332,-1.07709855607751,-1.05531719734113,-1.05044120166454,
-1.01169043941936,-1.00555651234072,-1.00178780850829,-0.998851799137522,
-0.995584210270059,-0.991334733589914),.UNSPECIFIED.);
#2492=B_SPLINE_CURVE_WITH_KNOTS('',3,(#78305,#78306,#78307,#78308,#78309,
#78310,#78311,#78312,#78313,#78314,#78315,#78316,#78317,#78318,#78319,#78320,
#78321,#78322,#78323,#78324,#78325,#78326,#78327,#78328,#78329,#78330,#78331,
#78332,#78333,#78334,#78335,#78336,#78337,#78338,#78339,#78340,#78341,#78342,
#78343,#78344,#78345,#78346,#78347,#78348,#78349,#78350,#78351,#78352,#78353,
#78354,#78355,#78356,#78357,#78358,#78359,#78360,#78361,#78362,#78363,#78364,
#78365,#78366,#78367,#78368,#78369,#78370,#78371,#78372,#78373,#78374,#78375,
#78376,#78377,#78378,#78379,#78380,#78381,#78382,#78383,#78384,#78385,#78386,
#78387,#78388,#78389,#78390,#78391,#78392,#78393,#78394,#78395,#78396,#78397,
#78398,#78399,#78400,#78401,#78402,#78403,#78404,#78405,#78406,#78407,#78408,
#78409,#78410,#78411,#78412,#78413,#78414,#78415,#78416,#78417,#78418,#78419,
#78420,#78421,#78422,#78423,#78424,#78425,#78426,#78427,#78428,#78429,#78430,
#78431,#78432,#78433,#78434,#78435,#78436,#78437,#78438,#78439,#78440,#78441,
#78442,#78443,#78444,#78445,#78446,#78447,#78448,#78449,#78450,#78451,#78452,
#78453,#78454,#78455,#78456,#78457,#78458,#78459,#78460,#78461,#78462,#78463,
#78464,#78465,#78466,#78467,#78468,#78469,#78470,#78471,#78472,#78473,#78474,
#78475,#78476,#78477,#78478,#78479,#78480,#78481,#78482,#78483,#78484,#78485,
#78486,#78487,#78488,#78489,#78490,#78491,#78492,#78493,#78494,#78495,#78496,
#78497,#78498,#78499,#78500,#78501,#78502,#78503,#78504,#78505,#78506),
 .UNSPECIFIED.,.F.,.F.,(4,2,2,2,2,2,2,2,2,2,2,2,2,2,2,2,2,2,2,2,2,2,2,2,
2,2,2,2,2,2,2,2,2,2,2,2,2,2,2,2,2,2,2,2,2,2,2,2,2,2,2,2,2,2,2,2,2,2,2,2,
2,2,2,2,2,2,2,2,2,2,2,2,2,2,2,2,2,2,2,2,2,2,2,2,2,2,2,2,2,2,2,2,2,2,2,2,
2,2,2,2,4),(-1.10913431935646,-1.09781930985798,-1.07223606504576,-1.0652806695971,
-1.06170837316959,-1.05907199732737,-1.05577710322132,-1.05016342020783,
-1.02080342513179,-0.991354948502371,-0.981637127978031,-0.97871663617906,
-0.976926855580005,-0.975230728648835,-0.972751365795229,-0.966002413402223,
-0.922194469142564,-0.902643457043816,-0.897346259745326,-0.894119361422423,
-0.891175523416381,-0.887333335837165,-0.878937036052964,-0.856163927241126,
-0.830059152552783,-0.815665810777979,-0.812377000601324,-0.81050684523887,
-0.80884495821503,-0.806565742205296,-0.801137086709259,-0.793192609444553,
-0.766123429011453,-0.736730094066658,-0.731120955789178,-0.727795905742393,
-0.725163804162955,-0.721634021674743,-0.7148905967575,-0.690956391977639,
-0.677288939969948,-0.651397443677576,-0.646651577444513,-0.64451356645842,
-0.642864459728906,-0.640933826329793,-0.63736187328623,-0.608745836965906,
-0.572377866117934,-0.56606447896315,-0.562286287478029,-0.559342625252688,
-0.556116376073141,-0.550821283475333,-0.528945304044135,-0.498156258215985,
-0.482514710219044,-0.479202839900898,-0.477308512033124,-0.475652873695394,
-0.473419314974251,-0.468261334213619,-0.460848950628351,-0.43722796370488,
-0.4060355796341,-0.398944610029881,-0.395299626919058,-0.392377212841247,
-0.389036119376414,-0.383203735717486,-0.376039733824192,-0.360236687326912,
-0.331382629821045,-0.315892063539941,-0.312587772879159,-0.31069516145134,
-0.309039144172838,-0.306802556979367,-0.30162686658604,-0.294180097575663,
-0.270350460839101,-0.239430976621142,-0.232337603292078,-0.228692128934005,
-0.225769681483076,-0.222428941716038,-0.216598207433253,-0.182099864476957,
-0.151225305399553,-0.146669298363086,-0.144543254571615,-0.142898273871101,
-0.140936052663352,-0.137463837855134,-0.132881079484305,-0.122199874554399,
-0.0934396652852915,-0.0699637714697171,-0.0644321743130892,-0.0611551620833314,
-0.0595329710308153),.UNSPECIFIED.);
#2493=B_SPLINE_CURVE_WITH_KNOTS('',3,(#78512,#78513,#78514,#78515,#78516,
#78517,#78518,#78519,#78520,#78521,#78522,#78523,#78524,#78525,#78526,#78527,
#78528,#78529,#78530,#78531,#78532,#78533,#78534,#78535,#78536,#78537,#78538,
#78539,#78540,#78541,#78542,#78543,#78544,#78545,#78546,#78547,#78548,#78549,
#78550,#78551,#78552,#78553,#78554,#78555,#78556,#78557,#78558,#78559,#78560,
#78561,#78562,#78563,#78564,#78565,#78566,#78567,#78568,#78569,#78570,#78571,
#78572,#78573,#78574,#78575,#78576,#78577,#78578,#78579,#78580,#78581,#78582,
#78583,#78584,#78585,#78586,#78587,#78588,#78589,#78590,#78591,#78592,#78593,
#78594,#78595,#78596,#78597,#78598,#78599,#78600,#78601,#78602,#78603,#78604,
#78605,#78606,#78607,#78608,#78609,#78610,#78611,#78612,#78613,#78614,#78615,
#78616,#78617,#78618,#78619,#78620,#78621,#78622,#78623,#78624,#78625,#78626,
#78627,#78628,#78629,#78630,#78631,#78632,#78633,#78634,#78635,#78636,#78637,
#78638,#78639,#78640,#78641,#78642,#78643,#78644,#78645,#78646,#78647,#78648,
#78649,#78650,#78651,#78652,#78653,#78654,#78655,#78656,#78657,#78658,#78659,
#78660,#78661,#78662,#78663,#78664,#78665,#78666,#78667,#78668,#78669,#78670,
#78671,#78672,#78673,#78674,#78675,#78676,#78677,#78678,#78679,#78680,#78681,
#78682,#78683,#78684,#78685,#78686,#78687,#78688,#78689,#78690,#78691,#78692,
#78693,#78694,#78695,#78696,#78697,#78698,#78699,#78700,#78701,#78702,#78703,
#78704,#78705,#78706,#78707,#78708,#78709,#78710,#78711,#78712,#78713,#78714,
#78715,#78716,#78717,#78718,#78719,#78720,#78721,#78722,#78723,#78724,#78725,
#78726,#78727,#78728,#78729,#78730,#78731,#78732,#78733,#78734,#78735,#78736,
#78737),.UNSPECIFIED.,.F.,.F.,(4,2,2,2,2,2,2,2,2,2,2,2,2,2,2,2,2,2,2,2,
2,2,2,2,2,2,2,2,2,2,2,2,2,2,2,2,2,2,2,2,2,2,2,2,2,2,2,2,2,2,2,2,2,2,2,2,
2,2,2,2,2,2,2,2,2,2,2,2,2,2,2,2,2,2,2,2,2,2,2,2,2,2,2,2,2,2,2,2,2,2,2,2,
2,2,2,2,2,2,2,2,2,2,2,2,2,2,2,2,2,2,2,2,4),(-0.991195152289668,-0.989058737366125,
-0.985746280099643,-0.983851442811526,-0.982195211269073,-0.979960595162866,
-0.974798999678037,-0.96738026490964,-0.943724650164412,-0.912576733438614,
-0.905484258671559,-0.901838256388501,-0.898914881511217,-0.895572514883543,
-0.889737387391909,-0.882569650841099,-0.866755916923555,-0.837910091686941,
-0.822426299183513,-0.819121626992332,-0.817228552572286,-0.815571930858969,
-0.813334201167262,-0.80815439357529,-0.800700288077559,-0.776829729324303,
-0.745962828097812,-0.738867877613459,-0.73522136907014,-0.732297959487918,
-0.728955956732874,-0.72312252745063,-0.715957457528714,-0.700152820751079,
-0.671304706731191,-0.655809500323241,-0.65250428919936,-0.650611094981761,
-0.648954504142384,-0.646716997950348,-0.641538483424944,-0.634086886242263,
-0.610231590499407,-0.579344866883861,-0.572250113360556,-0.568603649466183,
-0.565680248275633,-0.562338225324299,-0.55650468233309,-0.549339429892438,
-0.533534153341871,-0.50468628527434,-0.489191933969395,-0.485886768380858,
-0.48399358658996,-0.482336996814266,-0.480099478917327,-0.474920881242815,
-0.467469117620409,-0.443612766683756,-0.412727536516204,-0.405632782987422,
-0.401986323141544,-0.399062927157852,-0.395720912291749,-0.389887389030682,
-0.382722163892274,-0.366916964541923,-0.3380691363239,-0.322574754519552,
-0.319269592236183,-0.317376413316051,-0.31571982675763,-0.313482314150901,
-0.308303732737519,-0.300851995868541,-0.276995768039286,-0.246110492151411,
-0.239015752732565,-0.235369299849701,-0.232445909308944,-0.229103900513498,
-0.223270387449267,-0.216105174617946,-0.200300001214167,-0.171802768170646,
-0.156005560667715,-0.152674183893643,-0.150775086188452,-0.149175411933742,
-0.149155775872824,-0.14913626859957,-0.149116883729205,-0.14909761504051,
-0.149078456409151,-0.149059401867339,-0.149040445661379,-0.149021582134666,
-0.149002805768776,-0.148984111130622,-0.146867077204812,-0.144354657772053,
-0.139948468617413,-0.129882808126354,-0.0914865226515943,-0.0755862809040869,
-0.070603894380746,-0.0674439666543175,-0.0644760764373484,-0.0604733657444209,
-0.0511365831183054,-0.0377996321450267,-0.000492023790732501),
 .UNSPECIFIED.);
#2494=B_SPLINE_CURVE_WITH_KNOTS('',3,(#78738,#78739,#78740,#78741,#78742,
#78743,#78744,#78745,#78746,#78747,#78748,#78749,#78750,#78751,#78752,#78753,
#78754,#78755,#78756,#78757),.UNSPECIFIED.,.F.,.F.,(4,2,2,2,2,2,2,2,2,4),
(-2.10002542706347,-2.08879172315445,-2.08637671723263,-2.08465493193565,
-2.08311872769319,-2.08158046349029,-2.07945720600073,-2.07401815885657,
-2.05933454423903,-2.041194238912),.UNSPECIFIED.);
#2495=B_SPLINE_CURVE_WITH_KNOTS('',3,(#78759,#78760,#78761,#78762,#78763,
#78764,#78765,#78766,#78767,#78768,#78769,#78770),.UNSPECIFIED.,.F.,.F.,
(4,2,2,2,2,4),(-0.0595329710308153,-0.0582231334989721,-0.0544767912751946,
-0.0466099706509627,-0.0360357102531513,-0.000491966010066645),
 .UNSPECIFIED.);
#2496=B_SPLINE_CURVE_WITH_KNOTS('',3,(#78771,#78772,#78773,#78774,#78775,
#78776,#78777,#78778,#78779,#78780,#78781,#78782,#78783,#78784,#78785,#78786,
#78787,#78788,#78789,#78790,#78791,#78792,#78793,#78794,#78795,#78796,#78797,
#78798,#78799,#78800,#78801,#78802,#78803,#78804,#78805,#78806,#78807,#78808,
#78809,#78810,#78811,#78812,#78813,#78814,#78815,#78816,#78817,#78818,#78819,
#78820,#78821,#78822,#78823,#78824,#78825,#78826,#78827,#78828,#78829,#78830,
#78831,#78832,#78833,#78834,#78835,#78836,#78837,#78838,#78839,#78840,#78841,
#78842,#78843,#78844,#78845,#78846,#78847,#78848,#78849,#78850,#78851,#78852,
#78853,#78854,#78855,#78856,#78857,#78858,#78859,#78860,#78861,#78862,#78863,
#78864,#78865,#78866,#78867,#78868,#78869,#78870,#78871,#78872,#78873,#78874,
#78875,#78876,#78877,#78878,#78879,#78880,#78881,#78882,#78883,#78884,#78885,
#78886,#78887,#78888,#78889,#78890,#78891,#78892,#78893,#78894,#78895,#78896,
#78897,#78898,#78899,#78900,#78901,#78902,#78903,#78904,#78905,#78906,#78907,
#78908,#78909,#78910,#78911,#78912,#78913,#78914,#78915,#78916,#78917,#78918,
#78919,#78920,#78921,#78922,#78923,#78924,#78925,#78926,#78927,#78928,#78929,
#78930,#78931,#78932,#78933,#78934,#78935,#78936,#78937,#78938,#78939,#78940,
#78941,#78942,#78943,#78944,#78945,#78946,#78947,#78948,#78949,#78950,#78951,
#78952,#78953,#78954,#78955,#78956,#78957,#78958,#78959,#78960,#78961,#78962,
#78963,#78964),.UNSPECIFIED.,.F.,.F.,(4,2,2,2,2,2,2,2,2,2,2,2,2,2,2,2,2,
2,2,2,2,2,2,2,2,2,2,2,2,2,2,2,2,2,2,2,2,2,2,2,2,2,2,2,2,2,2,2,2,2,2,2,2,
2,2,2,2,2,2,2,2,2,2,2,2,2,2,2,2,2,2,2,2,2,2,2,2,2,2,2,2,2,2,2,2,2,2,2,2,
2,2,2,2,2,2,2,4),(-2.10005280646433,-2.0877597629007,-2.08172244365619,
-2.07944716492984,-2.07777813107226,-2.07610982925215,-2.07425779309637,
-2.07105426528615,-2.05805651907365,-2.03137046923152,-2.00296064397461,
-1.9973726251449,-1.99408272127116,-1.99115166457165,-1.98742370918956,
-1.97966090812949,-1.93946926949472,-1.91776072920575,-1.91299190557234,
-1.91082628185997,-1.90917746883294,-1.90723944714018,-1.90373489576291,
-1.8805961089851,-1.86335972444155,-1.83847241728195,-1.83160406865398,
-1.8280484729552,-1.82541315158058,-1.82210495156465,-1.81643158399557,
-1.78665917735656,-1.76520973906637,-1.75405354523577,-1.74933674551142,
-1.74567692997824,-1.74372740094089,-1.74208004726036,-1.73996659763525,
-1.73535943661535,-1.70481855439636,-1.67003000907514,-1.66417877955591,
-1.66083285404909,-1.65790967236107,-1.65426825849505,-1.64719873351372,
-1.61460605219853,-1.59204510201406,-1.58129313707818,-1.57837383047155,
-1.57658405077925,-1.57490704437578,-1.57283523745277,-1.56871597092744,
-1.53780912361497,-1.50329298016392,-1.49745907442349,-1.49411687664774,
-1.49119337212889,-1.48754686431964,-1.48045236331481,-1.44955142963723,
-1.42571825408513,-1.41827037195165,-1.41309317112305,-1.41085584282117,
-1.40919921841139,-1.40730588533527,-1.40400020950129,-1.38850510678613,
-1.35961754925217,-1.34379735703839,-1.33662761736679,-1.33079160236652,
-1.32744900296032,-1.32452561467342,-1.32087986496728,-1.31378881264165,
-1.28251743255758,-1.25896849631792,-1.2515675927052,-1.24641463182871,
-1.24418148289032,-1.24252541351683,-1.24062978354035,-1.237313842706,-1.22162138737103,
-1.19091029750774,-1.16895930632299,-1.16365816462727,-1.16042993391906,
-1.1574855704957,-1.15370801401654,-1.14739922726299,-1.11094501937456,
-1.10916707781729),.UNSPECIFIED.);
#2497=B_SPLINE_CURVE_WITH_KNOTS('',3,(#78969,#78970,#78971,#78972,#78973,
#78974,#78975,#78976,#78977,#78978,#78979,#78980,#78981,#78982,#78983,#78984,
#78985,#78986,#78987,#78988,#78989,#78990,#78991,#78992,#78993,#78994,#78995,
#78996,#78997,#78998,#78999,#79000,#79001,#79002,#79003,#79004,#79005,#79006,
#79007,#79008,#79009,#79010,#79011,#79012,#79013,#79014,#79015,#79016,#79017,
#79018,#79019,#79020,#79021,#79022,#79023,#79024,#79025,#79026,#79027,#79028,
#79029,#79030,#79031,#79032,#79033,#79034,#79035,#79036,#79037,#79038,#79039,
#79040,#79041,#79042,#79043,#79044,#79045,#79046,#79047,#79048,#79049,#79050,
#79051,#79052,#79053,#79054,#79055,#79056,#79057,#79058,#79059,#79060,#79061,
#79062,#79063,#79064,#79065,#79066,#79067,#79068,#79069,#79070,#79071,#79072,
#79073,#79074,#79075,#79076,#79077,#79078,#79079,#79080,#79081,#79082,#79083,
#79084,#79085,#79086,#79087,#79088,#79089,#79090,#79091,#79092,#79093,#79094,
#79095,#79096,#79097,#79098,#79099,#79100,#79101,#79102,#79103,#79104,#79105,
#79106,#79107,#79108,#79109,#79110,#79111,#79112,#79113,#79114,#79115,#79116,
#79117,#79118,#79119,#79120,#79121,#79122,#79123,#79124,#79125,#79126,#79127,
#79128,#79129,#79130,#79131,#79132,#79133,#79134,#79135,#79136,#79137,#79138,
#79139,#79140,#79141,#79142,#79143,#79144,#79145,#79146,#79147,#79148,#79149,
#79150,#79151,#79152,#79153,#79154,#79155,#79156,#79157,#79158,#79159,#79160,
#79161,#79162,#79163,#79164,#79165,#79166),.UNSPECIFIED.,.F.,.F.,(4,2,2,
2,2,2,2,2,2,2,2,2,2,2,2,2,2,2,2,2,2,2,2,2,2,2,2,2,2,2,2,2,2,2,2,2,2,2,2,
2,2,2,2,2,2,2,2,2,2,2,2,2,2,2,2,2,2,2,2,2,2,2,2,2,2,2,2,2,2,2,2,2,2,2,2,
2,2,2,2,2,2,2,2,2,2,2,2,2,2,2,2,2,2,2,2,2,2,2,4),(-2.04073105386379,-2.01788573118281,
-1.99770242346565,-1.98788298098068,-1.98503652231967,-1.98326279792523,
-1.98157601515141,-1.9790587938368,-1.97255913313296,-1.93157182655116,
-1.91665091197269,-1.90653703053737,-1.90241108072283,-1.89942256326465,
-1.89630413499345,-1.8915177851908,-1.87744267553201,-1.8436541590879,-1.82412698116097,
-1.81958263756561,-1.81745845374037,-1.81596981437242,-1.81406890364664,
-1.81072921267484,-1.79480388389642,-1.76422447883087,-1.74242735628701,
-1.73713586443389,-1.73390984754384,-1.73096511971517,-1.72718376780104,
-1.72086100746439,-1.68469636504952,-1.66468520152603,-1.65791711877805,
-1.65309646339385,-1.65092174930524,-1.64928707586521,-1.64736194306839,
-1.64391427796677,-1.62426068280426,-1.61781278124661,-1.59714270782084,
-1.57576531612937,-1.57049941015663,-1.5672788397993,-1.56433249769137,
-1.56053990144258,-1.55250394374847,-1.51275489361259,-1.49118950094329,
-1.48643536924891,-1.48427259321251,-1.48263905806711,-1.48070583220232,
-1.47722210549815,-1.45569353991343,-1.45150361788558,-1.43156538227889,
-1.41673251373306,-1.40666057071851,-1.40254095316983,-1.39955343442379,
-1.39643286013491,-1.39163675686681,-1.3774714617082,-1.34375869992897,
-1.32425849193193,-1.31971692326121,-1.31759319794413,-1.31610455649027,
-1.31420319198498,-1.31086172334449,-1.29489352658803,-1.26457729768814,
-1.24258245085058,-1.23727899537566,-1.23405031296662,-1.23110613549109,
-1.22732962308369,-1.22102433277704,-1.18454356864269,-1.15609611901115,
-1.15250353815158,-1.15056822791244,-1.1489192434793,-1.14678647543737,
-1.14207185555499,-1.11468329984751,-1.08900063900744,-1.07466417491557,
-1.06998879182356,-1.06689337709286,-1.06392439812577,-1.05974156304932,
-1.05002099290182,-1.03548507247329,-1.00469863726224,-0.991195152289668),
 .UNSPECIFIED.);
#2498=B_SPLINE_CURVE_WITH_KNOTS('',3,(#79167,#79168,#79169,#79170,#79171,
#79172,#79173,#79174,#79175,#79176,#79177,#79178,#79179,#79180,#79181,#79182,
#79183,#79184,#79185,#79186,#79187,#79188,#79189,#79190,#79191,#79192,#79193,
#79194,#79195,#79196,#79197,#79198,#79199,#79200,#79201,#79202,#79203,#79204,
#79205,#79206,#79207,#79208,#79209,#79210,#79211,#79212,#79213,#79214,#79215,
#79216,#79217,#79218,#79219,#79220,#79221,#79222,#79223,#79224,#79225,#79226,
#79227,#79228,#79229,#79230,#79231,#79232,#79233,#79234,#79235,#79236,#79237,
#79238,#79239,#79240,#79241,#79242,#79243,#79244,#79245,#79246,#79247,#79248,
#79249,#79250,#79251,#79252,#79253,#79254,#79255,#79256,#79257,#79258,#79259,
#79260,#79261,#79262,#79263,#79264,#79265,#79266,#79267,#79268,#79269,#79270,
#79271,#79272,#79273,#79274,#79275,#79276,#79277,#79278,#79279,#79280,#79281,
#79282,#79283,#79284,#79285,#79286,#79287,#79288,#79289,#79290,#79291,#79292,
#79293,#79294,#79295,#79296,#79297,#79298,#79299,#79300,#79301,#79302,#79303,
#79304,#79305,#79306,#79307,#79308,#79309,#79310,#79311,#79312,#79313,#79314,
#79315,#79316,#79317,#79318,#79319,#79320,#79321,#79322,#79323,#79324,#79325,
#79326,#79327,#79328,#79329,#79330,#79331,#79332,#79333,#79334,#79335,#79336,
#79337,#79338,#79339,#79340,#79341,#79342,#79343,#79344,#79345,#79346,#79347,
#79348,#79349,#79350,#79351,#79352,#79353,#79354,#79355,#79356,#79357,#79358,
#79359,#79360,#79361,#79362,#79363,#79364,#79365,#79366,#79367,#79368,#79369,
#79370,#79371,#79372,#79373,#79374,#79375,#79376,#79377,#79378,#79379,#79380,
#79381,#79382,#79383,#79384,#79385,#79386,#79387,#79388,#79389,#79390,#79391,
#79392),.UNSPECIFIED.,.F.,.F.,(4,2,2,2,2,2,2,2,2,2,2,2,2,2,2,2,2,2,2,2,
2,2,2,2,2,2,2,2,2,2,2,2,2,2,2,2,2,2,2,2,2,2,2,2,2,2,2,2,2,2,2,2,2,2,2,2,
2,2,2,2,2,2,2,2,2,2,2,2,2,2,2,2,2,2,2,2,2,2,2,2,2,2,2,2,2,2,2,2,2,2,2,2,
2,2,2,2,2,2,2,2,2,2,2,2,2,2,2,2,2,2,2,2,4),(-1.10916707781729,-1.09111005051036,
-1.08437531519816,-1.07957230929726,-1.0774006699881,-1.07576622240333,
-1.07383890522614,-1.07038182622291,-1.05037195859777,-1.00503548555728,
-0.99882937402838,-0.995081118323409,-0.99214089918231,-0.988898040559397,
-0.983527791216712,-0.960333984789916,-0.930255836988196,-0.91528849065879,
-0.912008612459382,-0.910121261011901,-0.908463533073702,-0.906216147456696,
-0.900978895097846,-0.893412754136719,-0.868849967399443,-0.838903260267914,
-0.831779106211155,-0.828126783088954,-0.825203175430626,-0.821865805284968,
-0.816053281751308,-0.808920952252066,-0.793227918181996,-0.763827919844489,
-0.748658963323564,-0.745369347094501,-0.743479788226645,-0.741822579646835,
-0.739579198092381,-0.734365530458577,-0.726845447361443,-0.702570185551568,
-0.672223437673162,-0.665119151694647,-0.661470915525603,-0.658547631114411,
-0.655207430293604,-0.649381571504329,-0.615617569649209,-0.583892867035995,
-0.579449934977405,-0.577337011823108,-0.575689965108573,-0.573740701726336,
-0.570081090091581,-0.542248640752413,-0.505148187639104,-0.498879320270475,
-0.495113310376012,-0.492170806413761,-0.488937334145717,-0.483610574010584,
-0.461205328655347,-0.441388928167931,-0.436937911633644,-0.415658863703378,
-0.412178539154411,-0.410246206462,-0.40861280977731,-0.406449437731836,
-0.40169117591681,-0.380082259441481,-0.340217446042829,-0.33295252926446,
-0.329276223730558,-0.326544913199139,-0.323542361876597,-0.319336083541556,
-0.30868502953963,-0.292616303977421,-0.263539992876104,-0.260487630636203,
-0.248334354819878,-0.245189861020655,-0.243351038619057,-0.241678699999058,
-0.239331890452382,-0.233482786241947,-0.224681658745724,-0.190699845878194,
-0.169194737364665,-0.163766776555625,-0.160511769363704,-0.157646324101798,
-0.157475736519576,-0.157320586494377,-0.157176158205232,-0.157039043053849,
-0.156906627047732,-0.156776788899757,-0.156647708924034,-0.15651773901719,
-0.156385307023362,-0.153274062122428,-0.148877173631576,-0.115650479679955,
-0.0839169527816737,-0.0794751547393593,-0.0773626137672975,-0.0757157884155579,
-0.0737666939116656,-0.070107160882403,-0.0593894328077706),
 .UNSPECIFIED.);
#2499=B_SPLINE_CURVE_WITH_KNOTS('',3,(#79398,#79399,#79400,#79401,#79402,
#79403,#79404,#79405,#79406,#79407,#79408,#79409,#79410,#79411,#79412,#79413,
#79414,#79415,#79416,#79417,#79418,#79419,#79420,#79421,#79422,#79423,#79424,
#79425,#79426,#79427,#79428,#79429,#79430,#79431,#79432,#79433,#79434,#79435,
#79436,#79437,#79438,#79439,#79440,#79441,#79442,#79443,#79444,#79445,#79446,
#79447,#79448,#79449,#79450,#79451,#79452,#79453,#79454,#79455,#79456,#79457,
#79458,#79459,#79460,#79461,#79462,#79463,#79464,#79465,#79466,#79467,#79468,
#79469,#79470,#79471,#79472,#79473,#79474,#79475,#79476,#79477,#79478,#79479,
#79480,#79481,#79482,#79483,#79484,#79485,#79486,#79487,#79488,#79489,#79490,
#79491,#79492,#79493,#79494,#79495,#79496,#79497,#79498,#79499,#79500,#79501,
#79502,#79503,#79504,#79505,#79506,#79507,#79508,#79509,#79510,#79511,#79512,
#79513,#79514,#79515,#79516,#79517,#79518,#79519,#79520,#79521,#79522,#79523,
#79524,#79525,#79526,#79527,#79528,#79529,#79530,#79531,#79532,#79533,#79534,
#79535,#79536,#79537,#79538,#79539,#79540,#79541,#79542,#79543,#79544,#79545,
#79546,#79547,#79548,#79549,#79550,#79551,#79552,#79553,#79554,#79555,#79556,
#79557,#79558,#79559,#79560,#79561,#79562,#79563,#79564,#79565,#79566,#79567,
#79568,#79569,#79570,#79571,#79572,#79573,#79574,#79575,#79576,#79577,#79578,
#79579,#79580,#79581,#79582,#79583),.UNSPECIFIED.,.F.,.F.,(4,2,2,2,2,2,
2,2,2,2,2,2,2,2,2,2,2,2,2,2,2,2,2,2,2,2,2,2,2,2,2,2,2,2,2,2,2,2,2,2,2,2,
2,2,2,2,2,2,2,2,2,2,2,2,2,2,2,2,2,2,2,2,2,2,2,2,2,2,2,2,2,2,2,2,2,2,2,2,
2,2,2,2,2,2,2,2,2,2,2,2,2,2,4),(-0.991309629175169,-0.976712442897297,-0.971302120168656,
-0.968049826107873,-0.965110359617235,-0.961313006050606,-0.953174462853071,
-0.925021072452987,-0.891225409952512,-0.886878244931272,-0.884790856603695,
-0.883147072261764,-0.881148294324108,-0.877250383151033,-0.872132242708788,
-0.85948407060637,-0.828328745793215,-0.809705627784808,-0.80446223390786,
-0.801245753691646,-0.798296841362354,-0.794426783850327,-0.785879079445045,
-0.758917436432243,-0.724418734700649,-0.720149274913234,-0.718076841380421,
-0.716433571742665,-0.714421598709655,-0.710458417627441,-0.686991859704004,
-0.645122196010641,-0.639335331082444,-0.635668184529889,-0.632742487414995,
-0.629413253066882,-0.623642246159036,-0.58925948691401,-0.558106058843816,
-0.553570727268718,-0.551447826590666,-0.549802208635513,-0.547832592819959,
-0.54407682407163,-0.517791031746947,-0.479054908839158,-0.472920325757895,
-0.469151582002897,-0.466215756384377,-0.462948592225075,-0.457467894255967,
-0.431984730623042,-0.411714045452939,-0.389809541094334,-0.386322752234575,
-0.384388597228262,-0.38275480858553,-0.380592354762241,-0.375841519551348,
-0.354314463689881,-0.314707927377083,-0.306410089545184,-0.302625539800229,
-0.299679847136787,-0.29645431729276,-0.291167179866853,-0.26945181549805,
-0.239312824709431,-0.222912954694419,-0.219554343178574,-0.217648932795758,
-0.216160744505729,-0.214042343867601,-0.209530327769631,-0.190307154362733,
-0.157403488206974,-0.142277943590563,-0.137375828169927,-0.134232581601323,
-0.131256277672675,-0.131138659838767,-0.13102409447788,-0.127507537188148,
-0.118778756966979,-0.106504121992404,-0.0804932699024008,-0.0565150980680115,
-0.0530185413914019,-0.051082288915653,-0.0494332201491776,-0.0472648689814095,
-0.0424809567350256,-0.000491817198503198),.UNSPECIFIED.);
#2500=B_SPLINE_CURVE_WITH_KNOTS('',3,(#79584,#79585,#79586,#79587,#79588,
#79589,#79590,#79591,#79592,#79593,#79594,#79595,#79596,#79597,#79598,#79599,
#79600,#79601,#79602,#79603),.UNSPECIFIED.,.F.,.F.,(4,2,2,2,2,2,2,2,2,4),
(-2.09977849986764,-2.0844228726502,-2.07591358257984,-2.07195021108648,
-2.06900251719241,-2.06601878699063,-2.06289098508343,-2.05806093965961,
-2.04357697080365,-2.04073105386379),.UNSPECIFIED.);
#2501=B_SPLINE_CURVE_WITH_KNOTS('',3,(#79605,#79606,#79607,#79608,#79609,
#79610,#79611,#79612),.UNSPECIFIED.,.F.,.F.,(4,2,2,4),(-0.0593894328077706,
-0.0422597363646323,-0.00975713810380856,-0.000491699695232061),
 .UNSPECIFIED.);
#2502=B_SPLINE_CURVE_WITH_KNOTS('',3,(#79613,#79614,#79615,#79616,#79617,
#79618,#79619,#79620,#79621,#79622,#79623,#79624,#79625,#79626,#79627,#79628,
#79629,#79630,#79631,#79632,#79633,#79634,#79635,#79636,#79637,#79638,#79639,
#79640,#79641,#79642,#79643,#79644,#79645,#79646,#79647,#79648,#79649,#79650,
#79651,#79652,#79653,#79654,#79655,#79656,#79657,#79658,#79659,#79660,#79661,
#79662,#79663,#79664,#79665,#79666,#79667,#79668,#79669,#79670,#79671,#79672,
#79673,#79674,#79675,#79676,#79677,#79678,#79679,#79680,#79681,#79682,#79683,
#79684,#79685,#79686,#79687,#79688,#79689,#79690,#79691,#79692,#79693,#79694,
#79695,#79696,#79697,#79698,#79699,#79700,#79701,#79702,#79703,#79704,#79705,
#79706,#79707,#79708,#79709,#79710,#79711,#79712,#79713,#79714,#79715,#79716,
#79717,#79718,#79719,#79720,#79721,#79722,#79723,#79724,#79725,#79726,#79727,
#79728,#79729,#79730,#79731,#79732,#79733,#79734,#79735,#79736,#79737,#79738,
#79739,#79740,#79741,#79742,#79743,#79744,#79745,#79746,#79747,#79748,#79749,
#79750,#79751,#79752,#79753,#79754,#79755,#79756,#79757,#79758,#79759,#79760,
#79761,#79762,#79763,#79764,#79765,#79766,#79767,#79768,#79769,#79770,#79771,
#79772,#79773,#79774,#79775,#79776,#79777,#79778,#79779,#79780,#79781,#79782,
#79783,#79784,#79785,#79786,#79787,#79788,#79789,#79790,#79791,#79792,#79793,
#79794,#79795,#79796,#79797,#79798,#79799,#79800,#79801,#79802),
 .UNSPECIFIED.,.F.,.F.,(4,2,2,2,2,2,2,2,2,2,2,2,2,2,2,2,2,2,2,2,2,2,2,2,
2,2,2,2,2,2,2,2,2,2,2,2,2,2,2,2,2,2,2,2,2,2,2,2,2,2,2,2,2,2,2,2,2,2,2,2,
2,2,2,2,2,2,2,2,2,2,2,2,2,2,2,2,2,2,2,2,2,2,2,2,2,2,2,2,2,2,2,2,2,2,4),
(-2.09983941200445,-2.09746751631786,-2.0948338360985,-2.09205900815291,
-2.08895601197975,-2.08424346038491,-2.07072870422845,-2.04417007690264,
-2.01545120294433,-2.01168261622109,-2.00971072883515,-2.00806589739413,
-2.00594748975691,-2.00143407369735,-1.96997115631921,-1.93593070229513,
-1.93010550852794,-1.9267654771214,-1.92384222814522,-1.92019388666864,
-1.91308887786692,-1.88061006830047,-1.85801612226665,-1.84725646898209,
-1.84433685500827,-1.8425472129118,-1.84087060996899,-1.83879958263684,
-1.83468272029919,-1.80376504574054,-1.76926853712739,-1.76343571849032,
-1.7600941269723,-1.75717114317716,-1.75352527229697,-1.74643196998487,
-1.71554427387772,-1.69170943797669,-1.6842619151255,-1.67908513905351,
-1.67684812474515,-1.67519178522279,-1.6732988381194,-1.66999396460366,
-1.65450608953998,-1.62562470986355,-1.60980373877781,-1.60263422492724,
-1.59679858154048,-1.59345643673825,-1.59053358612691,-1.58688869062496,
-1.57979989082555,-1.54843769500868,-1.52496635054924,-1.51757896761954,
-1.51243322356617,-1.5102015535971,-1.50854591443657,-1.50665000725737,
-1.50333193524757,-1.48760685047761,-1.45683903482583,-1.4349838879438,
-1.42968916476265,-1.4264626843352,-1.42351852468058,-1.41973929942555,
-1.41342334332628,-1.37712041031413,-1.35719273061045,-1.35044062428245,
-1.34562854885656,-1.34345551289555,-1.34182117493535,-1.33989537880054,
-1.3364441858045,-1.31664949145988,-1.3103841727319,-1.28987487506093,-1.26830987181352,
-1.26303262378709,-1.25980984873576,-1.25686457570851,-1.25307767435187,
-1.24673465949466,-1.2109515999346,-1.18215998900108,-1.17839141487176,
-1.17641961891532,-1.1747749142392,-1.17265673463904,-1.16814403101848,
-1.13667735610574,-1.10896100326588),.UNSPECIFIED.);
#2503=B_SPLINE_CURVE_WITH_KNOTS('',3,(#79807,#79808,#79809,#79810,#79811,
#79812,#79813,#79814,#79815,#79816,#79817,#79818,#79819,#79820,#79821,#79822,
#79823,#79824,#79825,#79826,#79827,#79828,#79829,#79830,#79831,#79832,#79833,
#79834,#79835,#79836,#79837,#79838,#79839,#79840,#79841,#79842,#79843,#79844,
#79845,#79846,#79847,#79848,#79849,#79850,#79851,#79852,#79853,#79854,#79855,
#79856,#79857,#79858,#79859,#79860,#79861,#79862,#79863,#79864,#79865,#79866,
#79867,#79868,#79869,#79870,#79871,#79872,#79873,#79874,#79875,#79876,#79877,
#79878,#79879,#79880,#79881,#79882,#79883,#79884,#79885,#79886,#79887,#79888,
#79889,#79890,#79891,#79892,#79893,#79894,#79895,#79896,#79897,#79898,#79899,
#79900,#79901,#79902,#79903,#79904,#79905,#79906,#79907,#79908,#79909,#79910,
#79911,#79912,#79913,#79914,#79915,#79916,#79917,#79918,#79919,#79920,#79921,
#79922,#79923,#79924,#79925,#79926,#79927,#79928,#79929,#79930,#79931,#79932,
#79933,#79934,#79935,#79936,#79937,#79938,#79939,#79940,#79941,#79942,#79943,
#79944,#79945,#79946,#79947,#79948,#79949,#79950,#79951,#79952,#79953,#79954,
#79955,#79956,#79957,#79958,#79959,#79960,#79961,#79962,#79963,#79964,#79965,
#79966,#79967,#79968,#79969,#79970,#79971,#79972,#79973,#79974,#79975,#79976,
#79977,#79978,#79979,#79980,#79981,#79982,#79983,#79984,#79985,#79986,#79987,
#79988,#79989,#79990,#79991,#79992,#79993,#79994,#79995,#79996,#79997,#79998,
#79999,#80000,#80001,#80002,#80003,#80004,#80005,#80006,#80007,#80008,#80009,
#80010,#80011,#80012,#80013,#80014,#80015,#80016,#80017,#80018,#80019,#80020,
#80021,#80022,#80023,#80024),.UNSPECIFIED.,.F.,.F.,(4,2,2,2,2,2,2,2,2,2,
2,2,2,2,2,2,2,2,2,2,2,2,2,2,2,2,2,2,2,2,2,2,2,2,2,2,2,2,2,2,2,2,2,2,2,2,
2,2,2,2,2,2,2,2,2,2,2,2,2,2,2,2,2,2,2,2,2,2,2,2,2,2,2,2,2,2,2,2,2,2,2,2,
2,2,2,2,2,2,2,2,2,2,2,2,2,2,2,2,2,2,2,2,2,2,2,2,2,2,4),(-2.04129650139704,
-2.02050217143667,-1.99426655112003,-1.98221452337952,-1.97360583333227,
-1.97010352814216,-1.96998780013201,-1.9698688148636,-1.96974596659654,
-1.96961857114194,-1.96948584782904,-1.96943549110545,-1.96937038609358,
-1.9692853020307,-1.96917249655033,-1.96901997039242,-1.96638351810006,
-1.96307725609551,-1.95741566967795,-1.92990954666347,-1.90130402088819,
-1.89314571267282,-1.88760910985177,-1.88531133445469,-1.88364588390244,
-1.88178296643051,-1.87853087229507,-1.8647544620661,-1.83817666852669,
-1.81284218465127,-1.80591636255214,-1.80234879391527,-1.79971170487989,
-1.79641047388868,-1.79077221717103,-1.76366977906844,-1.73470132532085,
-1.72649480152456,-1.72093434154722,-1.71863272123562,-1.71696672914608,
-1.71510573723172,-1.71186238123998,-1.69827517011355,-1.66630217610909,
-1.64340450040082,-1.63804832203251,-1.63480758504775,-1.63186521873499,
-1.62810862968909,-1.61997095566159,-1.58020192101911,-1.55862677998297,
-1.55387068497824,-1.55170705715486,-1.55007289666676,-1.54813895240977,
-1.54465398097334,-1.52312554234726,-1.51892456839007,-1.49898714598307,
-1.47664707068934,-1.47132193213445,-1.46808777018811,-1.4651435540136,
-1.46137383687282,-1.45509536143535,-1.41813714279326,-1.39862980620633,
-1.3887247358984,-1.38588152843768,-1.38410808345957,-1.38242003202009,
-1.37989861330407,-1.37337562863872,-1.34133360627301,-1.3155059098064,
-1.30678609826977,-1.30288597496673,-1.29993266419096,-1.29672936104297,
-1.29154812806111,-1.27356731064997,-1.24209788214621,-1.22917380128435,
-1.22398405804918,-1.22004387557362,-1.21803646063817,-1.21639293036682,
-1.21431513251944,-1.21001830968317,-1.17572844148365,-1.1488350020391,
-1.14009999130656,-1.13619735900707,-1.13324379665879,-1.13004181467583,
-1.12486630568284,-1.10696568358054,-1.06947000405028,-1.06032634168688,
-1.05431285877752,-1.05193991000559,-1.05026250979406,-1.0484330241394,
-1.04533402683798,-1.03222578157483,-0.998111700818972,-0.991309629175169),
 .UNSPECIFIED.);
#2504=B_SPLINE_CURVE_WITH_KNOTS('',3,(#80025,#80026,#80027,#80028,#80029,
#80030,#80031,#80032,#80033,#80034,#80035,#80036,#80037,#80038,#80039,#80040,
#80041,#80042,#80043,#80044,#80045,#80046,#80047,#80048,#80049,#80050,#80051,
#80052,#80053,#80054,#80055,#80056,#80057,#80058,#80059,#80060,#80061,#80062,
#80063,#80064,#80065,#80066,#80067,#80068,#80069,#80070,#80071,#80072,#80073,
#80074,#80075,#80076,#80077,#80078,#80079,#80080,#80081,#80082,#80083,#80084,
#80085,#80086,#80087,#80088,#80089,#80090,#80091,#80092,#80093,#80094,#80095,
#80096,#80097,#80098,#80099,#80100,#80101,#80102,#80103,#80104,#80105,#80106,
#80107,#80108,#80109,#80110,#80111,#80112,#80113,#80114,#80115,#80116,#80117,
#80118,#80119,#80120,#80121,#80122,#80123,#80124,#80125,#80126,#80127,#80128,
#80129,#80130,#80131,#80132,#80133,#80134,#80135,#80136,#80137,#80138,#80139,
#80140,#80141,#80142,#80143,#80144,#80145,#80146,#80147,#80148,#80149,#80150,
#80151,#80152,#80153,#80154,#80155,#80156,#80157,#80158,#80159,#80160,#80161,
#80162,#80163,#80164,#80165,#80166,#80167,#80168,#80169,#80170,#80171,#80172,
#80173,#80174,#80175,#80176,#80177,#80178,#80179,#80180,#80181,#80182,#80183,
#80184,#80185,#80186,#80187,#80188,#80189,#80190,#80191,#80192,#80193,#80194,
#80195,#80196,#80197,#80198,#80199,#80200,#80201,#80202,#80203,#80204,#80205,
#80206,#80207,#80208,#80209,#80210,#80211,#80212,#80213,#80214,#80215,#80216,
#80217,#80218,#80219,#80220,#80221,#80222,#80223,#80224,#80225,#80226,#80227,
#80228,#80229,#80230),.UNSPECIFIED.,.F.,.F.,(4,2,2,2,2,2,2,2,2,2,2,2,2,
2,2,2,2,2,2,2,2,2,2,2,2,2,2,2,2,2,2,2,2,2,2,2,2,2,2,2,2,2,2,2,2,2,2,2,2,
2,2,2,2,2,2,2,2,2,2,2,2,2,2,2,2,2,2,2,2,2,2,2,2,2,2,2,2,2,2,2,2,2,2,2,2,
2,2,2,2,2,2,2,2,2,2,2,2,2,2,2,2,2,4),(-1.10896100326588,-1.10262103694887,
-1.09680950829537,-1.09347253248744,-1.09054917744227,-1.08689704633842,
-1.0797728310934,-1.04989664098759,-1.01645877921795,-1.01207723862595,
-1.00998387422742,-1.0083405765361,-1.00634875720638,-1.00248227637776,
-0.997417009453012,-0.984968363565762,-0.947040343215284,-0.933776552618257,
-0.929081231408675,-0.925982141253907,-0.922982570162637,-0.918792498268505,
-0.90825096870595,-0.892420489245415,-0.863568688361532,-0.848109848545278,
-0.844806780010933,-0.842914317368835,-0.841258034223744,-0.839020557297983,
-0.833840543231992,-0.826385662620472,-0.802508963608914,-0.771644030973076,
-0.764549335811273,-0.760903345492693,-0.757980563523399,-0.754639527340026,
-0.74880850210391,-0.714411980850648,-0.683416500478926,-0.678867385009774,
-0.676742481818722,-0.675097412500106,-0.673131029622788,-0.669388327723223,
-0.642520965989869,-0.604467894639204,-0.598274003720881,-0.594489006285154,
-0.591552398663583,-0.588296480525749,-0.582863895335284,-0.55841418540684,
-0.543849367171461,-0.542495082316909,-0.517075007846038,-0.512323397368113,
-0.510184367439247,-0.508535166710451,-0.506605256642582,-0.503036697028638,
-0.474375738926622,-0.438051858426659,-0.4317360382244,-0.427957173251727,
-0.425013434844205,-0.421787557268093,-0.416494130552386,-0.394645610858004,
-0.363891692130062,-0.348191822161565,-0.344876158178873,-0.342980980957539,
-0.341325544493112,-0.339093520889043,-0.333944436473672,-0.326549281630532,
-0.303031993480562,-0.271704051062899,-0.26461445842908,-0.260969774914935,
-0.258047403262549,-0.254706143252063,-0.248872902315979,-0.241707537936841,
-0.225899772874974,-0.197047311799649,-0.181568423389682,-0.17826133638004,
-0.176368100924025,-0.174712239129969,-0.17247680124674,-0.167307772205462,
-0.159873923085579,-0.13612272070742,-0.105101243386457,-0.0980088199640418,
-0.0943635576300295,-0.0914411464006612,-0.0881003026529644,-0.0822690040247909,
-0.0593466407402418),.UNSPECIFIED.);
#2505=B_SPLINE_CURVE_WITH_KNOTS('',3,(#80236,#80237,#80238,#80239,#80240,
#80241,#80242,#80243,#80244,#80245,#80246,#80247,#80248,#80249,#80250,#80251,
#80252,#80253,#80254,#80255,#80256,#80257,#80258,#80259,#80260,#80261,#80262,
#80263,#80264,#80265,#80266,#80267,#80268,#80269,#80270,#80271,#80272,#80273,
#80274,#80275,#80276,#80277,#80278,#80279,#80280,#80281,#80282,#80283,#80284,
#80285,#80286,#80287,#80288,#80289,#80290,#80291,#80292,#80293,#80294,#80295,
#80296,#80297,#80298,#80299,#80300,#80301,#80302,#80303,#80304,#80305,#80306,
#80307,#80308,#80309,#80310,#80311,#80312,#80313,#80314,#80315,#80316,#80317,
#80318,#80319,#80320,#80321,#80322,#80323,#80324,#80325,#80326,#80327,#80328,
#80329,#80330,#80331,#80332,#80333,#80334,#80335,#80336,#80337,#80338,#80339,
#80340,#80341,#80342,#80343,#80344,#80345,#80346,#80347,#80348,#80349,#80350,
#80351,#80352,#80353,#80354,#80355,#80356,#80357,#80358,#80359,#80360,#80361,
#80362,#80363,#80364,#80365,#80366,#80367,#80368,#80369,#80370,#80371,#80372,
#80373,#80374,#80375,#80376,#80377,#80378,#80379,#80380,#80381,#80382,#80383,
#80384,#80385,#80386,#80387,#80388,#80389,#80390,#80391,#80392,#80393,#80394,
#80395,#80396,#80397,#80398,#80399,#80400,#80401,#80402,#80403,#80404,#80405,
#80406,#80407,#80408,#80409,#80410,#80411,#80412,#80413,#80414,#80415,#80416,
#80417,#80418,#80419,#80420,#80421,#80422,#80423,#80424,#80425,#80426,#80427,
#80428,#80429,#80430,#80431),.UNSPECIFIED.,.F.,.F.,(4,2,2,2,2,2,2,2,2,2,
2,2,2,2,2,2,2,2,2,2,2,2,2,2,2,2,2,2,2,2,2,2,2,2,2,2,2,2,2,2,2,2,2,2,2,2,
2,2,2,2,2,2,2,2,2,2,2,2,2,2,2,2,2,2,2,2,2,2,2,2,2,2,2,2,2,2,2,2,2,2,2,2,
2,2,2,2,2,2,2,2,2,2,2,2,2,2,2,4),(-0.991375509315892,-0.971325647813708,
-0.956656946350987,-0.953391182320626,-0.951506689619944,-0.949847609452942,
-0.947593126047794,-0.942316274240613,-0.934673159706958,-0.909625473790717,
-0.877722768848919,-0.872089010915296,-0.868757519973074,-0.865860063663532,
-0.862210483579645,-0.854863167175326,-0.845203456380488,-0.819206108415393,
-0.813692841681796,-0.790404323367302,-0.786912860339961,-0.784977658463859,
-0.783344007246142,-0.781183064370636,-0.776440602213076,-0.754998072415802,
-0.715655928564857,-0.7071146577489,-0.703287680514103,-0.700335905265575,
-0.697130631576916,-0.691938003285569,-0.671690929813469,-0.65014110811581,
-0.643366909545774,-0.623672966677335,-0.620223945958354,-0.618298279848431,
-0.616663326782288,-0.614488430502789,-0.609668200140982,-0.602900579483171,
-0.582896724136379,-0.546670099216769,-0.540346852572707,-0.536565001517774,
-0.533619746346397,-0.530393009767133,-0.525099987881885,-0.503285136397791,
-0.47263504888351,-0.465714154600991,-0.455981719639317,-0.453059268566414,
-0.451268762047407,-0.44957232481929,-0.447092995787216,-0.440347040601106,
-0.396536034896136,-0.376986912031471,-0.371688981728305,-0.368461388271975,
-0.365516736840972,-0.361673205304913,-0.353272626051038,-0.33037475660221,
-0.304036260414623,-0.289977806463287,-0.286706271216534,-0.284839558690544,
-0.283176085859649,-0.280888303557429,-0.275409744945854,-0.267366027029317,
-0.239596839505482,-0.211024487297737,-0.205376326231097,-0.202073719706845,
-0.19943792172997,-0.195875244917472,-0.188970070985356,-0.163789678747696,
-0.137521325723465,-0.123362936621702,-0.1200860067375,-0.118218123681791,
-0.116554989982739,-0.114269556516894,-0.108805308367515,-0.0803572397899584,
-0.0564804299161656,-0.0426614192773625,-0.0379022588577338,-0.0347893747368273,
-0.0317972752601317,-0.0288347686752118,-0.0248304547526201,-0.000491209455975046),
 .UNSPECIFIED.);
#2506=B_SPLINE_CURVE_WITH_KNOTS('',3,(#80432,#80433,#80434,#80435,#80436,
#80437,#80438,#80439,#80440,#80441,#80442,#80443,#80444,#80445,#80446,#80447),
 .UNSPECIFIED.,.F.,.F.,(4,2,2,2,2,2,2,4),(-2.10011893460937,-2.05874039818313,
-2.0539606684199,-2.0517927065913,-2.0501432533371,-2.04820577425607,-2.0447051496043,
-2.04129650139704),.UNSPECIFIED.);
#2507=B_SPLINE_CURVE_WITH_KNOTS('',3,(#80449,#80450,#80451,#80452,#80453,
#80454,#80455,#80456,#80457,#80458,#80459,#80460,#80461,#80462,#80463,#80464,
#80465,#80466,#80467,#80468),.UNSPECIFIED.,.F.,.F.,(4,2,2,2,2,2,2,2,2,4),
(-0.0593466407402418,-0.0475921036961166,-0.0244934883160425,-0.0142512537367275,
-0.0112790705691864,-0.00947813397535948,-0.00791635107762846,-0.00623769541915255,
-0.00362381139487444,-0.000491106664933776),.UNSPECIFIED.);
#2508=B_SPLINE_CURVE_WITH_KNOTS('',3,(#80469,#80470,#80471,#80472,#80473,
#80474,#80475,#80476,#80477,#80478,#80479,#80480,#80481,#80482,#80483,#80484,
#80485,#80486,#80487,#80488,#80489,#80490,#80491,#80492,#80493,#80494,#80495,
#80496,#80497,#80498,#80499,#80500,#80501,#80502,#80503,#80504,#80505,#80506,
#80507,#80508,#80509,#80510,#80511,#80512,#80513,#80514,#80515,#80516,#80517,
#80518,#80519,#80520,#80521,#80522,#80523,#80524,#80525,#80526,#80527,#80528,
#80529,#80530,#80531,#80532,#80533,#80534,#80535,#80536,#80537,#80538,#80539,
#80540,#80541,#80542,#80543,#80544,#80545,#80546,#80547,#80548,#80549,#80550,
#80551,#80552,#80553,#80554,#80555,#80556,#80557,#80558,#80559,#80560,#80561,
#80562,#80563,#80564,#80565,#80566,#80567,#80568,#80569,#80570,#80571,#80572,
#80573,#80574,#80575,#80576,#80577,#80578,#80579,#80580,#80581,#80582,#80583,
#80584,#80585,#80586,#80587,#80588,#80589,#80590,#80591,#80592,#80593,#80594,
#80595,#80596,#80597,#80598,#80599,#80600,#80601,#80602,#80603,#80604,#80605,
#80606,#80607,#80608,#80609,#80610,#80611,#80612,#80613,#80614,#80615,#80616,
#80617,#80618,#80619,#80620,#80621,#80622,#80623,#80624,#80625,#80626,#80627,
#80628,#80629,#80630,#80631,#80632,#80633,#80634,#80635,#80636,#80637,#80638,
#80639,#80640,#80641,#80642,#80643,#80644,#80645,#80646,#80647,#80648,#80649,
#80650,#80651,#80652,#80653,#80654,#80655,#80656,#80657,#80658,#80659,#80660,
#80661,#80662,#80663,#80664,#80665,#80666,#80667,#80668,#80669,#80670,#80671,
#80672,#80673,#80674,#80675,#80676,#80677,#80678,#80679,#80680,#80681,#80682),
 .UNSPECIFIED.,.F.,.F.,(4,2,2,2,2,2,2,2,2,2,2,2,2,2,2,2,2,2,2,2,2,2,2,2,
2,2,2,2,2,2,2,2,2,2,2,2,2,2,2,2,2,2,2,2,2,2,2,2,2,2,2,2,2,2,2,2,2,2,2,2,
2,2,2,2,2,2,2,2,2,2,2,2,2,2,2,2,2,2,2,2,2,2,2,2,2,2,2,2,2,2,2,2,2,2,2,2,
2,2,2,2,2,2,2,2,2,2,4),(-2.10025436568081,-2.05988935967928,-2.03995709080465,
-2.03163144250381,-2.02780136713765,-2.02485870160554,-2.02162502330748,
-2.01629785714225,-1.99618429740599,-1.95277314195091,-1.94828775920848,
-1.94574487101294,-1.94359788555784,-1.94357765013498,-1.94355738141956,
-1.9435370734256,-1.94351672001049,-1.94349631496814,-1.94348543071906,
-1.94347427766195,-1.94346284237382,-1.94345111059155,-1.94343906694274,
-1.94342669509122,-1.9434139775649,-1.94340089554668,-1.94179220588074,
-1.93989682336244,-1.93658177415496,-1.92110045184647,-1.89221362083911,
-1.87639772330963,-1.86922939426582,-1.8633943536282,-1.86005208844235,
-1.85712886272789,-1.85348314564426,-1.84639160917657,-1.81521873512535,
-1.79159752295975,-1.78418485327014,-1.77902590403342,-1.77679181042879,
-1.77513570641277,-1.77324080506401,-1.76992777942584,-1.7542808926877,
-1.7234962075332,-1.70156978300996,-1.69627034437933,-1.69304260715778,
-1.69009834331992,-1.68632042906834,-1.68000994317976,-1.64359377630011,
-1.62373627241731,-1.61699735994837,-1.61219219426706,-1.61002024668369,
-1.60838585434544,-1.60645894691865,-1.6030033856196,-1.58304819400471,
-1.57646841529328,-1.55481305118713,-1.53468557648691,-1.52950151165228,
-1.52629847830387,-1.5233467791006,-1.51951710904556,-1.51095751424969,
-1.47165399466463,-1.45022763169339,-1.44548707594442,-1.44332674962259,
-1.44169345290579,-1.43975861923866,-1.43626770061208,-1.41313482149133,
-1.39593943117429,-1.37100224826789,-1.36412802496839,-1.36057155566827,
-1.35793646027117,-1.35462967976717,-1.34896163061532,-1.31818921891525,
-1.29334281292321,-1.28490552376879,-1.27923198092879,-1.27691267747497,
-1.2752444947542,-1.27339298905891,-1.27019120708184,-1.25721570791507,
-1.23007798867549,-1.20208021574403,-1.19650578957859,-1.1932190663698,
-1.19028790734917,-1.18655580114359,-1.18054576845566,-1.13433093390365,
-1.11630245151555,-1.11192301990235,-1.10982980654801,-1.1092440461416),
 .UNSPECIFIED.);
#2509=B_SPLINE_CURVE_WITH_KNOTS('',3,(#80687,#80688,#80689,#80690,#80691,
#80692,#80693,#80694,#80695,#80696,#80697,#80698,#80699,#80700,#80701,#80702,
#80703,#80704,#80705,#80706,#80707,#80708,#80709,#80710,#80711,#80712,#80713,
#80714,#80715,#80716,#80717,#80718,#80719,#80720,#80721,#80722,#80723,#80724,
#80725,#80726,#80727,#80728,#80729,#80730,#80731,#80732,#80733,#80734,#80735,
#80736,#80737,#80738,#80739,#80740,#80741,#80742,#80743,#80744,#80745,#80746,
#80747,#80748,#80749,#80750,#80751,#80752,#80753,#80754,#80755,#80756,#80757,
#80758,#80759,#80760,#80761,#80762,#80763,#80764,#80765,#80766,#80767,#80768,
#80769,#80770,#80771,#80772,#80773,#80774,#80775,#80776,#80777,#80778,#80779,
#80780,#80781,#80782,#80783,#80784,#80785,#80786,#80787,#80788,#80789,#80790,
#80791,#80792,#80793,#80794,#80795,#80796,#80797,#80798,#80799,#80800,#80801,
#80802,#80803,#80804,#80805,#80806,#80807,#80808,#80809,#80810,#80811,#80812,
#80813,#80814,#80815,#80816,#80817,#80818,#80819,#80820,#80821,#80822,#80823,
#80824,#80825,#80826,#80827,#80828,#80829,#80830,#80831,#80832,#80833,#80834,
#80835,#80836,#80837,#80838,#80839,#80840,#80841,#80842,#80843,#80844,#80845,
#80846,#80847,#80848,#80849,#80850,#80851,#80852,#80853,#80854,#80855,#80856,
#80857,#80858,#80859,#80860,#80861,#80862,#80863,#80864,#80865,#80866,#80867,
#80868,#80869,#80870,#80871,#80872,#80873,#80874,#80875,#80876,#80877,#80878,
#80879,#80880,#80881,#80882,#80883,#80884,#80885,#80886,#80887,#80888,#80889,
#80890,#80891,#80892,#80893,#80894,#80895,#80896,#80897,#80898,#80899,#80900,
#80901,#80902,#80903,#80904,#80905,#80906,#80907,#80908,#80909,#80910,#80911,
#80912,#80913,#80914,#80915,#80916,#80917,#80918),.UNSPECIFIED.,.F.,.F.,
(4,2,2,2,2,2,2,2,2,2,2,2,2,2,2,2,2,2,2,2,2,2,2,2,2,2,2,2,2,2,2,2,2,2,2,
2,2,2,2,2,2,2,2,2,2,2,2,2,2,2,2,2,2,2,2,2,2,2,2,2,2,2,2,2,2,2,2,2,2,2,2,
2,2,2,2,2,2,2,2,2,2,2,2,2,2,2,2,2,2,2,2,2,2,2,2,2,2,2,2,2,2,2,2,2,2,2,2,
2,2,2,2,2,2,2,2,4),(-2.04114771859458,-2.03955044215046,-2.0359873324451,
-2.03335094243348,-2.03004722296548,-2.02439622375842,-1.99426110152052,
-1.97146852859624,-1.96137220605286,-1.95695661231143,-1.95444032036714,
-1.95232057439764,-1.95230191979688,-1.95228318355207,-1.95226436027608,
-1.95224544449622,-1.95222643057772,-1.95220731278866,-1.95218808522726,
-1.95216874185421,-1.95214927649478,-1.95212968277069,-1.95052983024196,
-1.94863206629821,-1.94530782384571,-1.92968643462709,-1.89896211512878,
-1.87697689695211,-1.87167301735613,-1.86844372537231,-1.86549876562277,
-1.86172093631104,-1.8554127364574,-1.81894571801047,-1.79912306194497,
-1.79239043970653,-1.78758837442089,-1.78541661388233,-1.78378182562157,
-1.78185375549402,-1.77839446936323,-1.75831195675354,-1.75184651269745,
-1.73053971193123,-1.71697501531594,-1.70752370297998,-1.70350157902085,
-1.70052989019903,-1.69737570651913,-1.6924231617866,-1.67681314288446,
-1.64433457652749,-1.62527779231291,-1.62078354944626,-1.61866836142678,
-1.61718041098861,-1.61527252070741,-1.61190334846076,-1.59528796598961,
-1.56571231358035,-1.54366161884458,-1.53835386255701,-1.5351237303543,
-1.53217898328665,-1.52840278148661,-1.52210036933827,-1.48553581095097,
-1.45727936758489,-1.45360822980282,-1.45165617107427,-1.45000882202314,
-1.44789799477105,-1.44346777915029,-1.41139822010568,-1.37794745453774,
-1.37210589899874,-1.36876173115749,-1.3658378803048,-1.36219272404055,
-1.35510649089822,-1.32342317864337,-1.30019262299668,-1.29284478356411,
-1.28771909121993,-1.28549038067231,-1.28383459371998,-1.28193575719009,
-1.27860657681105,-1.26280177682535,-1.23210213589126,-1.21026988985006,
-1.20497526123325,-1.2017480308493,-1.19880264659717,-1.19502107774251,
-1.18869937743779,-1.15247571026872,-1.13249265593414,-1.12572921501757,
-1.12091072535199,-1.11873606135403,-1.11710102842371,-1.11517499620138,
-1.11172464242704,-1.09199678587012,-1.08522350290935,-1.06404758724812,
-1.05037149736466,-1.0410699957019,-1.03736734894764,-1.03462894007553,
-1.03163070170678,-1.02745323999756,-1.01700352970447,-1.00137333991101,
-0.991375509315892),.UNSPECIFIED.);
#2510=B_SPLINE_CURVE_WITH_KNOTS('',3,(#80919,#80920,#80921,#80922,#80923,
#80924,#80925,#80926,#80927,#80928,#80929,#80930,#80931,#80932,#80933,#80934,
#80935,#80936,#80937,#80938,#80939,#80940,#80941,#80942,#80943,#80944,#80945,
#80946,#80947,#80948,#80949,#80950,#80951,#80952,#80953,#80954,#80955,#80956,
#80957,#80958,#80959,#80960,#80961,#80962,#80963,#80964,#80965,#80966,#80967,
#80968,#80969,#80970,#80971,#80972,#80973,#80974,#80975,#80976,#80977,#80978,
#80979,#80980,#80981,#80982,#80983,#80984,#80985,#80986,#80987,#80988,#80989,
#80990,#80991,#80992,#80993,#80994,#80995,#80996,#80997,#80998,#80999,#81000,
#81001,#81002,#81003,#81004,#81005,#81006,#81007,#81008,#81009,#81010,#81011,
#81012,#81013,#81014,#81015,#81016,#81017,#81018,#81019,#81020,#81021,#81022,
#81023,#81024,#81025,#81026,#81027,#81028,#81029,#81030,#81031,#81032,#81033,
#81034,#81035,#81036,#81037,#81038,#81039,#81040,#81041,#81042,#81043,#81044,
#81045,#81046,#81047,#81048,#81049,#81050,#81051,#81052,#81053,#81054,#81055,
#81056,#81057,#81058,#81059,#81060,#81061,#81062,#81063,#81064,#81065,#81066,
#81067,#81068,#81069,#81070,#81071,#81072,#81073,#81074,#81075,#81076,#81077,
#81078,#81079,#81080,#81081,#81082,#81083,#81084,#81085,#81086,#81087,#81088,
#81089,#81090,#81091,#81092,#81093,#81094,#81095,#81096,#81097,#81098,#81099,
#81100,#81101,#81102,#81103,#81104,#81105,#81106,#81107,#81108,#81109,#81110,
#81111,#81112,#81113,#81114,#81115,#81116,#81117,#81118,#81119,#81120,#81121,
#81122,#81123,#81124,#81125,#81126),.UNSPECIFIED.,.F.,.F.,(4,2,2,2,2,2,
2,2,2,2,2,2,2,2,2,2,2,2,2,2,2,2,2,2,2,2,2,2,2,2,2,2,2,2,2,2,2,2,2,2,2,2,
2,2,2,2,2,2,2,2,2,2,2,2,2,2,2,2,2,2,2,2,2,2,2,2,2,2,2,2,2,2,2,2,2,2,2,2,
2,2,2,2,2,2,2,2,2,2,2,2,2,2,2,2,2,2,2,2,2,2,2,2,2,4),(-1.1092440461416,
-1.10834451449087,-1.10642202474537,-1.10298671449132,-1.08381054346351,
-1.0504100854777,-1.03426701466328,-1.02925665226071,-1.02609066645499,
-1.02312515882606,-1.01913811477839,-1.00989751419581,-0.996750879904674,
-0.974876872255874,-0.969805854640356,-0.94825810638846,-0.944774396692011,
-0.942841166484129,-0.941207661746437,-0.939044993609643,-0.934291511417377,
-0.91273423613294,-0.873036179927103,-0.864818334381091,-0.861048371066553,
-0.85810519030908,-0.854873433241854,-0.849555241083263,-0.827303569840712,
-0.807292604730401,-0.803040718692191,-0.781585822563856,-0.778103264704438,
-0.776170366235679,-0.774536938111132,-0.772374106185186,-0.767619252470507,
-0.746046390857894,-0.706297337120878,-0.698935735727955,-0.695235960067629,
-0.69249887939359,-0.689501336746625,-0.68532344758395,-0.674865143808652,
-0.659214923536852,-0.629365499275763,-0.614547677125586,-0.611275237441311,
-0.609389620513822,-0.607731563596552,-0.605481238897973,-0.600226293513572,
-0.592625416003843,-0.567842517002867,-0.53822360296346,-0.531072297611526,
-0.527414488088338,-0.524490544361041,-0.521157175903367,-0.515363088287735,
-0.508259610180924,-0.492664244006215,-0.462258486331871,-0.447867117307472,
-0.444578118847412,-0.44270778988695,-0.441045700710015,-0.438766142346748,
-0.43333637407794,-0.425390008211735,-0.398310902818856,-0.368922795369496,
-0.363246544866067,-0.359938244165254,-0.357303690848199,-0.353750254844742,
-0.346889962726889,-0.32205971132695,-0.304814407871312,-0.281650150469743,
-0.278160044115444,-0.276225529854654,-0.274592437922467,-0.272432264596464,
-0.267691676801547,-0.246261209468699,-0.206960920297067,-0.198384182370283,
-0.194551864359339,-0.191600104691203,-0.188398969347303,-0.183222381242241,
-0.163191711660756,-0.141495438283894,-0.135264345803247,-0.114955763361533,
-0.111492672353607,-0.109564250233118,-0.107930389284136,-0.105761481838837,
-0.10097214377063,-0.0942617145351005,-0.0595087977532423),
 .UNSPECIFIED.);
#2511=B_SPLINE_CURVE_WITH_KNOTS('',3,(#81132,#81133,#81134,#81135,#81136,
#81137,#81138,#81139,#81140,#81141,#81142,#81143,#81144,#81145,#81146,#81147,
#81148,#81149,#81150,#81151,#81152,#81153,#81154,#81155,#81156,#81157,#81158,
#81159,#81160,#81161,#81162,#81163,#81164,#81165,#81166,#81167,#81168,#81169,
#81170,#81171,#81172,#81173,#81174,#81175,#81176,#81177,#81178,#81179,#81180,
#81181,#81182,#81183,#81184,#81185,#81186,#81187,#81188,#81189,#81190,#81191,
#81192,#81193,#81194,#81195,#81196,#81197,#81198,#81199,#81200,#81201,#81202,
#81203,#81204,#81205,#81206,#81207,#81208,#81209,#81210,#81211,#81212,#81213,
#81214,#81215,#81216,#81217,#81218,#81219,#81220,#81221,#81222,#81223,#81224,
#81225,#81226,#81227,#81228,#81229,#81230,#81231,#81232,#81233,#81234,#81235,
#81236,#81237,#81238,#81239,#81240,#81241,#81242,#81243,#81244,#81245,#81246,
#81247,#81248,#81249,#81250,#81251,#81252,#81253,#81254,#81255,#81256,#81257,
#81258,#81259,#81260,#81261,#81262,#81263,#81264,#81265,#81266,#81267,#81268,
#81269,#81270,#81271,#81272,#81273,#81274,#81275,#81276,#81277,#81278,#81279,
#81280,#81281,#81282,#81283,#81284,#81285,#81286,#81287,#81288,#81289,#81290,
#81291,#81292,#81293,#81294,#81295,#81296,#81297,#81298,#81299,#81300,#81301,
#81302,#81303,#81304,#81305,#81306,#81307,#81308,#81309,#81310,#81311,#81312,
#81313,#81314,#81315,#81316,#81317,#81318,#81319,#81320,#81321,#81322,#81323),
 .UNSPECIFIED.,.F.,.F.,(4,2,2,2,2,2,2,2,2,2,2,2,2,2,2,2,2,2,2,2,2,2,2,2,
2,2,2,2,2,2,2,2,2,2,2,2,2,2,2,2,2,2,2,2,2,2,2,2,2,2,2,2,2,2,2,2,2,2,2,2,
2,2,2,2,2,2,2,2,2,2,2,2,2,2,2,2,2,2,2,2,2,2,2,2,2,2,2,2,2,2,2,2,2,2,2,4),
(-0.991163431562309,-0.983026812983697,-0.946840791955441,-0.940514654088063,
-0.93673181834429,-0.933786222648764,-0.930559545204441,-0.925267622091985,
-0.903476681762918,-0.872928619819918,-0.856985166116892,-0.853644373617409,
-0.851742910550934,-0.85025391199805,-0.848129268342275,-0.843584242970056,
-0.824055907907021,-0.790277275137965,-0.776148805171909,-0.771355815786866,
-0.768235477427027,-0.765246890764966,-0.761123697641,-0.751031564934833,
-0.736159654005757,-0.716318134095772,-0.711906387224396,-0.690591623746885,
-0.687110147030128,-0.685177203908985,-0.683543289207713,-0.681379171066148,
-0.676618966274426,-0.654996501094427,-0.615087927979628,-0.607064429282978,
-0.603288365301109,-0.600351899616149,-0.597089196853831,-0.591628502524685,
-0.566595277446982,-0.54540975777923,-0.523933315526696,-0.520450202276971,
-0.518516961887957,-0.516883201098184,-0.514719814405494,-0.50996323232123,
-0.488375900745767,-0.448577027546068,-0.440457420126384,-0.436704653655309,
-0.433763451149865,-0.43052211536294,-0.425160492711937,-0.402135965730442,
-0.370001367280284,-0.356732274298548,-0.353512600958904,-0.351657080526661,
-0.349989999528961,-0.347678593320234,-0.34205518155407,-0.333719168119961,
-0.307647687571344,-0.277915753685912,-0.272241716735928,-0.26893345999275,
-0.266298254058415,-0.262743025146357,-0.255875943489336,-0.230996521707243,
-0.213788097923434,-0.190640849959093,-0.187157610616563,-0.185224388704467,
-0.18359070214555,-0.181427490070131,-0.176671583085754,-0.155090014022952,
-0.115308219377761,-0.107174966849337,-0.103419858380921,-0.100478446324007,
-0.0972385481211124,-0.0918832347812257,-0.0689721053730947,-0.0424639122988463,
-0.0276457692725278,-0.0218131539447601,-0.0194033311085543,-0.0177365565132501,
-0.0162021764441248,-0.0143991166696238,-0.0117759066718596,-0.000490982254256552),
 .UNSPECIFIED.);
#2512=B_SPLINE_CURVE_WITH_KNOTS('',3,(#81324,#81325,#81326,#81327,#81328,
#81329,#81330,#81331),.UNSPECIFIED.,.F.,.F.,(4,2,2,4),(-2.10019346878139,
-2.07162495664198,-2.04645503985977,-2.04114771859458),.UNSPECIFIED.);
#2513=B_SPLINE_CURVE_WITH_KNOTS('',3,(#81333,#81334,#81335,#81336,#81337,
#81338,#81339,#81340,#81341,#81342,#81343,#81344,#81345,#81346,#81347,#81348,
#81349,#81350,#81351,#81352),.UNSPECIFIED.,.F.,.F.,(4,2,2,2,2,2,2,2,2,4),
(-0.0595087977532423,-0.0586975082944341,-0.0373425380828879,-0.0313459888537824,
-0.0276182134449585,-0.0246879961510923,-0.0219472198498188,-0.0187144246772699,
-0.0116643696517348,-0.00049107690068497),.UNSPECIFIED.);
#2514=B_SPLINE_CURVE_WITH_KNOTS('',3,(#81353,#81354,#81355,#81356,#81357,
#81358,#81359,#81360,#81361,#81362,#81363,#81364,#81365,#81366,#81367,#81368,
#81369,#81370,#81371,#81372,#81373,#81374,#81375,#81376,#81377,#81378,#81379,
#81380,#81381,#81382,#81383,#81384,#81385,#81386,#81387,#81388,#81389,#81390,
#81391,#81392,#81393,#81394,#81395,#81396,#81397,#81398,#81399,#81400,#81401,
#81402,#81403,#81404,#81405,#81406,#81407,#81408,#81409,#81410,#81411,#81412,
#81413,#81414,#81415,#81416,#81417,#81418,#81419,#81420,#81421,#81422,#81423,
#81424,#81425,#81426,#81427,#81428,#81429,#81430,#81431,#81432,#81433,#81434,
#81435,#81436,#81437,#81438,#81439,#81440,#81441,#81442,#81443,#81444,#81445,
#81446,#81447,#81448,#81449,#81450,#81451,#81452,#81453,#81454,#81455,#81456,
#81457,#81458,#81459,#81460,#81461,#81462,#81463,#81464,#81465,#81466,#81467,
#81468,#81469,#81470,#81471,#81472,#81473,#81474,#81475,#81476,#81477,#81478,
#81479,#81480,#81481,#81482,#81483,#81484,#81485,#81486,#81487,#81488,#81489,
#81490,#81491,#81492,#81493,#81494,#81495,#81496,#81497,#81498,#81499,#81500,
#81501,#81502,#81503,#81504,#81505,#81506,#81507,#81508,#81509,#81510,#81511,
#81512,#81513,#81514,#81515,#81516,#81517,#81518,#81519,#81520,#81521,#81522,
#81523,#81524,#81525,#81526,#81527,#81528,#81529,#81530,#81531,#81532,#81533,
#81534,#81535,#81536,#81537,#81538,#81539,#81540,#81541,#81542,#81543,#81544,
#81545,#81546,#81547,#81548,#81549,#81550,#81551,#81552,#81553,#81554),
 .UNSPECIFIED.,.F.,.F.,(4,2,2,2,2,2,2,2,2,2,2,2,2,2,2,2,2,2,2,2,2,2,2,2,
2,2,2,2,2,2,2,2,2,2,2,2,2,2,2,2,2,2,2,2,2,2,2,2,2,2,2,2,2,2,2,2,2,2,2,2,
2,2,2,2,2,2,2,2,2,2,2,2,2,2,2,2,2,2,2,2,2,2,2,2,2,2,2,2,2,2,2,2,2,2,2,2,
2,2,2,2,4),(-2.09985433564141,-2.07657965371477,-2.05654300630488,-2.04976929128882,
-2.04494540288815,-2.04276994739049,-2.04113503780234,-2.03921006349314,
-2.03576372793023,-2.01618178886459,-2.00962512910649,-1.98885844223598,
-1.97471647142805,-1.96805222276279,-1.962621965938,-1.95944583360317,-1.95652135298477,
-1.95286333271904,-1.94571307748359,-1.91491073286433,-1.89107005387601,
-1.88362087024361,-1.87844297263702,-1.87620549818488,-1.87454882780183,
-1.87265551391689,-1.86935002416176,-1.85385991267236,-1.82497297918086,
-1.80914819767212,-1.80197706462812,-1.7961401381916,-1.79279730349086,
-1.78987387556106,-1.78622829424746,-1.7791382704522,-1.74775279268874,
-1.72428975604382,-1.71690306601617,-1.71175741547485,-1.70952549386682,
-1.70786954981482,-1.7059731570057,-1.7026539429633,-1.68692030590257,-1.6562687506758,
-1.63430523221504,-1.62900326569337,-1.62577481493943,-1.62283043273642,
-1.61905310408836,-1.61274526921994,-1.57627188535292,-1.55644871384975,
-1.5497162003448,-1.54491435786216,-1.54274290088386,-1.54110844267879,
-1.5391809355745,-1.53572311271344,-1.51568507597026,-1.50917683223058,
-1.4875003775627,-1.46739930889587,-1.46221676020551,-1.45901388037046,
-1.45606180447947,-1.45223091089343,-1.44366533127775,-1.40436428711742,
-1.38293799933997,-1.37819723722115,-1.37603676692299,-1.37440333954468,
-1.37246832481659,-1.36897701892388,-1.34581571155995,-1.32858167438782,
-1.30369536362377,-1.29682734142661,-1.29327192886806,-1.29063674894047,
-1.28732873391396,-1.28165570246101,-1.25188183601931,-1.23042656095483,
-1.21927738019487,-1.21456261563906,-1.21090406784536,-1.20895486746383,
-1.20730757669922,-1.20519393951989,-1.20058537384566,-1.1700610192424,
-1.13526077399985,-1.12941051648516,-1.1260649105148,-1.12314187142691,
-1.11950045654299,-1.11243035665219,-1.1090417761794),.UNSPECIFIED.);
#2515=B_SPLINE_CURVE_WITH_KNOTS('',3,(#81559,#81560,#81561,#81562,#81563,
#81564,#81565,#81566,#81567,#81568,#81569,#81570,#81571,#81572,#81573,#81574,
#81575,#81576,#81577,#81578,#81579,#81580,#81581,#81582,#81583,#81584,#81585,
#81586,#81587,#81588,#81589,#81590,#81591,#81592,#81593,#81594,#81595,#81596,
#81597,#81598,#81599,#81600,#81601,#81602,#81603,#81604,#81605,#81606,#81607,
#81608,#81609,#81610,#81611,#81612,#81613,#81614,#81615,#81616,#81617,#81618,
#81619,#81620,#81621,#81622,#81623,#81624,#81625,#81626,#81627,#81628,#81629,
#81630,#81631,#81632,#81633,#81634,#81635,#81636,#81637,#81638,#81639,#81640,
#81641,#81642,#81643,#81644,#81645,#81646,#81647,#81648,#81649,#81650,#81651,
#81652,#81653,#81654,#81655,#81656,#81657,#81658,#81659,#81660,#81661,#81662,
#81663,#81664,#81665,#81666,#81667,#81668,#81669,#81670,#81671,#81672,#81673,
#81674,#81675,#81676,#81677,#81678,#81679,#81680,#81681,#81682,#81683,#81684,
#81685,#81686,#81687,#81688,#81689,#81690,#81691,#81692,#81693,#81694,#81695,
#81696,#81697,#81698,#81699,#81700,#81701,#81702,#81703,#81704,#81705,#81706,
#81707,#81708,#81709,#81710,#81711,#81712,#81713,#81714,#81715,#81716,#81717,
#81718,#81719,#81720,#81721,#81722,#81723,#81724,#81725,#81726,#81727,#81728,
#81729,#81730,#81731,#81732,#81733,#81734,#81735,#81736,#81737,#81738,#81739,
#81740,#81741,#81742,#81743,#81744,#81745,#81746,#81747,#81748,#81749,#81750,
#81751,#81752,#81753,#81754,#81755,#81756,#81757,#81758,#81759,#81760,#81761,
#81762,#81763,#81764,#81765,#81766,#81767,#81768,#81769,#81770,#81771,#81772),
 .UNSPECIFIED.,.F.,.F.,(4,2,2,2,2,2,2,2,2,2,2,2,2,2,2,2,2,2,2,2,2,2,2,2,
2,2,2,2,2,2,2,2,2,2,2,2,2,2,2,2,2,2,2,2,2,2,2,2,2,2,2,2,2,2,2,2,2,2,2,2,
2,2,2,2,2,2,2,2,2,2,2,2,2,2,2,2,2,2,2,2,2,2,2,2,2,2,2,2,2,2,2,2,2,2,2,2,
2,2,2,2,2,2,2,2,2,2,4),(-2.04098557160315,-2.03563970820405,-2.02721151915856,
-2.02154202375354,-2.01922288867902,-2.01755427494498,-2.01570162385464,
-2.01249641222889,-1.99947887565978,-1.96066340863327,-1.94321709398517,
-1.93823899648528,-1.93549755095925,-1.93273585369067,-1.92908317184212,
-1.92196074102959,-1.89115500174544,-1.86728847958394,-1.85983496990153,
-1.85465470693968,-1.85241659378497,-1.85075959027282,-1.84886600631082,
-1.84556022263514,-1.83007058311279,-1.8011943549787,-1.78536820180773,
-1.77819644395789,-1.7723589444424,-1.76901561486162,-1.76609163729158,
-1.76244519612132,-1.75535283932053,-1.72420677790114,-1.70056776856453,
-1.69315177983521,-1.68799087287038,-1.68575610094944,-1.68409954824832,
-1.68220414545671,-1.67889021088619,-1.66323617717807,-1.63246337766471,
-1.6105362474992,-1.60523592518145,-1.60200745612423,-1.59906238096588,
-1.59528320413929,-1.58897003262656,-1.55259277947306,-1.53271181706041,
-1.52596801241401,-1.52116000269857,-1.51898721050742,-1.51735235775532,
-1.51542506572358,-1.51196911578833,-1.49202070237809,-1.48543673595591,
-1.4641707523055,-1.44370011333476,-1.4384918382117,-1.43528307077011,-1.43233214484196,
-1.4285120140822,-1.42001109821947,-1.38064535966,-1.35919967996132,-1.35445672368895,
-1.3522956293284,-1.35066187982258,-1.34872661164412,-1.34523508561935,
-1.32208877616988,-1.30487302360003,-1.27996654209721,-1.27309554531736,
-1.26953915959961,-1.26690346818418,-1.26359506681647,-1.25792196573599,
-1.22812200957773,-1.20660055156191,-1.19551575715169,-1.19081873993744,
-1.18717075868413,-1.18522355643755,-1.18357567627554,-1.18145837843927,
-1.17683093982489,-1.13794433370012,-1.11097138129367,-1.10543147475197,
-1.10215168223015,-1.09921846137134,-1.09547236034357,-1.0894157072123,
-1.04993119268329,-1.0434781664719,-1.02384306614861,-1.02039533237019,
-1.01846985639277,-1.01683470969483,-1.01465909148722,-1.00983545419509,
-1.00306164058815,-0.991163431562309),.UNSPECIFIED.);
#2516=B_SPLINE_CURVE_WITH_KNOTS('',3,(#81773,#81774,#81775,#81776,#81777,
#81778,#81779,#81780,#81781,#81782,#81783,#81784,#81785,#81786,#81787,#81788,
#81789,#81790,#81791,#81792,#81793,#81794,#81795,#81796,#81797,#81798,#81799,
#81800,#81801,#81802,#81803,#81804,#81805,#81806,#81807,#81808,#81809,#81810,
#81811,#81812,#81813,#81814,#81815,#81816,#81817,#81818,#81819,#81820,#81821,
#81822,#81823,#81824,#81825,#81826,#81827,#81828,#81829,#81830,#81831,#81832,
#81833,#81834,#81835,#81836,#81837,#81838,#81839,#81840,#81841,#81842,#81843,
#81844,#81845,#81846,#81847,#81848,#81849,#81850,#81851,#81852,#81853,#81854,
#81855,#81856,#81857,#81858,#81859,#81860,#81861,#81862,#81863,#81864,#81865,
#81866,#81867,#81868,#81869,#81870,#81871,#81872,#81873,#81874,#81875,#81876,
#81877,#81878,#81879,#81880,#81881,#81882,#81883,#81884,#81885,#81886,#81887,
#81888,#81889,#81890,#81891,#81892,#81893,#81894,#81895,#81896,#81897,#81898,
#81899,#81900,#81901,#81902,#81903,#81904,#81905,#81906,#81907,#81908,#81909,
#81910,#81911,#81912,#81913,#81914,#81915,#81916,#81917,#81918,#81919,#81920,
#81921,#81922,#81923,#81924,#81925,#81926,#81927,#81928,#81929,#81930,#81931,
#81932,#81933,#81934,#81935,#81936,#81937,#81938,#81939,#81940,#81941,#81942,
#81943,#81944,#81945,#81946,#81947,#81948,#81949,#81950,#81951,#81952,#81953,
#81954,#81955,#81956,#81957,#81958,#81959,#81960,#81961,#81962,#81963,#81964,
#81965,#81966),.UNSPECIFIED.,.F.,.F.,(4,2,2,2,2,2,2,2,2,2,2,2,2,2,2,2,2,
2,2,2,2,2,2,2,2,2,2,2,2,2,2,2,2,2,2,2,2,2,2,2,2,2,2,2,2,2,2,2,2,2,2,2,2,
2,2,2,2,2,2,2,2,2,2,2,2,2,2,2,2,2,2,2,2,2,2,2,2,2,2,2,2,2,2,2,2,2,2,2,2,
2,2,2,2,2,2,2,4),(-1.1090417761794,-1.07988086625166,-1.05729058618643,
-1.05005201336957,-1.04498318261964,-1.04278824747931,-1.0411321173552,
-1.03923678396174,-1.03583245287252,-1.01633592113168,-0.984416466042156,
-0.967260749509081,-0.962115494665457,-0.958920706854573,-0.955966129746268,
-0.952050792004092,-0.943236889210629,-0.93091574040323,-0.908814707192146,
-0.882920137911538,-0.87817381196359,-0.876035426052958,-0.874385956020462,
-0.872454807990772,-0.86888168237218,-0.864307828480602,-0.820609106792188,
-0.800892714355112,-0.795586543110736,-0.792357561489918,-0.789414002000317,
-0.785575320221527,-0.777199829895772,-0.755202250859291,-0.715897573098805,
-0.711363607055685,-0.709241468934196,-0.707596515637242,-0.705627837219407,
-0.701874296690441,-0.674622394323279,-0.637038786295313,-0.630806184936431,
-0.627050603703619,-0.624109669725413,-0.620871185835822,-0.615520349037995,
-0.592678764357737,-0.560884677171424,-0.547125872121436,-0.543876284284986,
-0.542014563100982,-0.54035005960954,-0.538053428045315,-0.532519087268654,
-0.524362897063695,-0.495770183643399,-0.468199425752467,-0.462555140124699,
-0.459253781368635,-0.456618446620025,-0.453055717410229,-0.446148106701857,
-0.420944683457092,-0.394630088295682,-0.380532404007987,-0.37725912367687,
-0.375392263624808,-0.373729299752075,-0.371443149625252,-0.365972894134721,
-0.357945459765812,-0.330292062635853,-0.301627450836764,-0.295947942145964,
-0.292639065264374,-0.290004763357313,-0.286452589986169,-0.279598008689047,
-0.254810676685214,-0.216118799307858,-0.211914807871398,-0.209822563100135,
-0.208140569202345,-0.206360285111265,-0.203482890147348,-0.193199397885009,
-0.172371538738913,-0.137331708581453,-0.130962802562926,-0.127168680490406,
-0.12422246343744,-0.121003367345744,-0.116909623789973,-0.102586557738656,
-0.0768746775274151,-0.0592762986750658),.UNSPECIFIED.);
#2517=B_SPLINE_CURVE_WITH_KNOTS('',3,(#81972,#81973,#81974,#81975,#81976,
#81977,#81978,#81979,#81980,#81981,#81982,#81983,#81984,#81985,#81986,#81987,
#81988,#81989,#81990,#81991,#81992,#81993,#81994,#81995,#81996,#81997,#81998,
#81999,#82000,#82001,#82002,#82003,#82004,#82005,#82006,#82007,#82008,#82009,
#82010,#82011,#82012,#82013,#82014,#82015,#82016,#82017,#82018,#82019,#82020,
#82021,#82022,#82023,#82024,#82025,#82026,#82027,#82028,#82029,#82030,#82031,
#82032,#82033,#82034,#82035,#82036,#82037,#82038,#82039,#82040,#82041,#82042,
#82043,#82044,#82045,#82046,#82047,#82048,#82049,#82050,#82051,#82052,#82053,
#82054,#82055,#82056,#82057,#82058,#82059,#82060,#82061,#82062,#82063,#82064,
#82065,#82066,#82067,#82068,#82069,#82070,#82071,#82072,#82073,#82074,#82075,
#82076,#82077,#82078,#82079,#82080,#82081,#82082,#82083,#82084,#82085,#82086,
#82087,#82088,#82089,#82090,#82091,#82092,#82093,#82094,#82095,#82096,#82097,
#82098,#82099,#82100,#82101,#82102,#82103,#82104,#82105,#82106,#82107,#82108,
#82109,#82110,#82111,#82112,#82113,#82114,#82115,#82116,#82117,#82118,#82119,
#82120,#82121,#82122,#82123,#82124,#82125,#82126,#82127,#82128,#82129,#82130,
#82131,#82132,#82133,#82134,#82135,#82136,#82137,#82138,#82139,#82140,#82141,
#82142,#82143,#82144,#82145,#82146,#82147,#82148,#82149,#82150,#82151,#82152,
#82153,#82154,#82155,#82156,#82157,#82158,#82159,#82160,#82161,#82162,#82163,
#82164,#82165,#82166,#82167,#82168,#82169,#82170,#82171),.UNSPECIFIED.,
 .F.,.F.,(4,2,2,2,2,2,2,2,2,2,2,2,2,2,2,2,2,2,2,2,2,2,2,2,2,2,2,2,2,2,2,
2,2,2,2,2,2,2,2,2,2,2,2,2,2,2,2,2,2,2,2,2,2,2,2,2,2,2,2,2,2,2,2,2,2,2,2,
2,2,2,2,2,2,2,2,2,2,2,2,2,2,2,2,2,2,2,2,2,2,2,2,2,2,2,2,2,2,2,2,4),(-0.991202703725535,
-0.970522559222933,-0.939735394018657,-0.924083759353349,-0.920770364998682,
-0.918875187784806,-0.917218799597893,-0.914984160051106,-0.909823307970298,
-0.902406305126986,-0.878763531249245,-0.847591869623134,-0.840498787106726,
-0.836852415666169,-0.833928717311233,-0.830585950957878,-0.824750046886789,
-0.817581313403194,-0.801765141945526,-0.772916244083387,-0.757431590730897,
-0.754126590834429,-0.752233314380364,-0.750576505579371,-0.748338509404223,
-0.743158026232733,-0.735702899500169,-0.711828522715385,-0.680959679338312,
-0.673863922461446,-0.670217003808648,-0.667293267545249,-0.663950893619949,
-0.658116822490968,-0.650950967495996,-0.635144617249224,-0.606293266531227,
-0.590796266244502,-0.587490682993342,-0.585597276674732,-0.583940500982808,
-0.581702746118521,-0.576523660374982,-0.569071244836912,-0.545213369345774,
-0.514323086198759,-0.507227541336903,-0.503580670401441,-0.50065694272665,
-0.497314546370527,-0.491480351148642,-0.484314297334193,-0.468507251701242,
-0.439656163517481,-0.424160086739221,-0.420854552255572,-0.418961159077121,
-0.417304384280238,-0.415066616403597,-0.409887439804569,-0.402434842836434,
-0.378575820652435,-0.347687150498304,-0.340591604570006,-0.336944737486079,
-0.334021015030818,-0.330678626959087,-0.324844452304657,-0.317678427094565,
-0.301871463072638,-0.273020412866674,-0.257524300170147,-0.254218768756,
-0.252325378410742,-0.250668606854038,-0.248430844383581,-0.24325168472544,
-0.235799115831433,-0.211940224808054,-0.181091284162821,-0.173971235279214,
-0.170319326718561,-0.16739521036242,-0.164646530503026,-0.159497949413282,
-0.139876617129393,-0.117778325588309,-0.112151591383416,-0.0911956334541362,
-0.087719441072008,-0.0857877513251872,-0.0841537801009711,-0.0819881326914908,
-0.077218999577992,-0.0555041694092805,-0.0133613952491335,-0.00693651896192096,
-0.00347621653055332,-0.0017044654462795,-0.000491452588193953),
 .UNSPECIFIED.);
#2518=B_SPLINE_CURVE_WITH_KNOTS('',3,(#82172,#82173,#82174,#82175,#82176,
#82177,#82178,#82179,#82180,#82181),.UNSPECIFIED.,.F.,.F.,(4,2,2,2,4),(-2.09994892392206,
-2.09740773666934,-2.09305353736742,-2.08013651306197,-2.04098557160315),
 .UNSPECIFIED.);
#2519=B_SPLINE_CURVE_WITH_KNOTS('',3,(#82183,#82184,#82185,#82186,#82187,
#82188,#82189,#82190,#82191,#82192,#82193,#82194,#82195,#82196,#82197,#82198,
#82199,#82200),.UNSPECIFIED.,.F.,.F.,(4,2,2,2,2,2,2,2,4),(-0.0592762986750658,
-0.0495542205447057,-0.0448430910167832,-0.0427112328124616,-0.0410626509152269,
-0.0391275338177746,-0.0370497816162303,-0.0337442454856563,-0.000491569883824227),
 .UNSPECIFIED.);
#2520=B_SPLINE_CURVE_WITH_KNOTS('',3,(#82201,#82202,#82203,#82204,#82205,
#82206,#82207,#82208,#82209,#82210,#82211,#82212,#82213,#82214,#82215,#82216,
#82217,#82218,#82219,#82220,#82221,#82222,#82223,#82224,#82225,#82226,#82227,
#82228,#82229,#82230,#82231,#82232,#82233,#82234,#82235,#82236,#82237,#82238,
#82239,#82240,#82241,#82242,#82243,#82244,#82245,#82246,#82247,#82248,#82249,
#82250,#82251,#82252,#82253,#82254,#82255,#82256,#82257,#82258,#82259,#82260,
#82261,#82262,#82263,#82264,#82265,#82266,#82267,#82268,#82269,#82270,#82271,
#82272,#82273,#82274,#82275,#82276,#82277,#82278,#82279,#82280,#82281,#82282,
#82283,#82284,#82285,#82286,#82287,#82288,#82289,#82290,#82291,#82292,#82293,
#82294,#82295,#82296,#82297,#82298,#82299,#82300,#82301,#82302,#82303,#82304,
#82305,#82306,#82307,#82308,#82309,#82310,#82311,#82312,#82313,#82314,#82315,
#82316,#82317,#82318,#82319,#82320,#82321,#82322,#82323,#82324,#82325,#82326,
#82327,#82328,#82329,#82330,#82331,#82332,#82333,#82334,#82335,#82336,#82337,
#82338,#82339,#82340,#82341,#82342,#82343,#82344,#82345,#82346,#82347,#82348,
#82349,#82350,#82351,#82352,#82353,#82354,#82355,#82356,#82357,#82358,#82359,
#82360,#82361,#82362,#82363,#82364,#82365,#82366,#82367,#82368,#82369,#82370,
#82371,#82372,#82373,#82374,#82375,#82376,#82377,#82378,#82379,#82380,#82381,
#82382,#82383,#82384,#82385,#82386,#82387,#82388,#82389,#82390),
 .UNSPECIFIED.,.F.,.F.,(4,2,2,2,2,2,2,2,2,2,2,2,2,2,2,2,2,2,2,2,2,2,2,2,
2,2,2,2,2,2,2,2,2,2,2,2,2,2,2,2,2,2,2,2,2,2,2,2,2,2,2,2,2,2,2,2,2,2,2,2,
2,2,2,2,2,2,2,2,2,2,2,2,2,2,2,2,2,2,2,2,2,2,2,2,2,2,2,2,2,2,2,2,2,2,4),
(-3.79235008026687,-3.76879104347154,-3.75883026516241,-3.75512635641919,
-3.75226780474209,-3.74932856094105,-3.74607818361715,-3.74067505922862,
-3.71937735048599,-3.68731998843125,-3.67635882076812,-3.67058549835473,
-3.66820568956278,-3.66652741236532,-3.66470137813792,-3.66161693879173,
-3.65015300503789,-3.6219716319717,-3.5933140491505,-3.5877185302108,-3.58442701644351,
-3.58149622845065,-3.57777094090938,-3.57178518594219,-3.53165638983071,
-3.50653993698235,-3.50276659469806,-3.50079349474002,-3.4991484104026,
-3.49703064963911,-3.49252201064742,-3.46095531282508,-3.42698696341232,
-3.42116638000915,-3.4178269176096,-3.41490296122218,-3.41125215266787,
-3.40413722284319,-3.37511937734592,-3.34983534343432,-3.34215632841335,
-3.33686081537245,-3.33460336692293,-3.3329440564725,-3.33106162722549,
-3.32780427023879,-3.31330283380641,-3.28300653913868,-3.26738435055625,
-3.26027265974359,-3.25447355349318,-3.2511387167445,-3.24821432322312,
-3.24455705540249,-3.23741036201886,-3.20777528667571,-3.18301921430959,
-3.17542276176001,-3.17016937059013,-3.16791907195565,-3.16626075763165,
-3.16437457171243,-3.16110049826273,-3.14626360082182,-3.11546827062215,
-3.09275149299329,-3.0874063116763,-3.08416857478599,-3.08122661918422,
-3.07746740143087,-3.07122358693279,-3.03379680981587,-3.00627035238142,
-3.00261077882638,-3.00066136853779,-2.999014108332,-2.99690077018904,-2.99245653363706,
-2.9607122720554,-2.92693317192425,-2.9211019549393,-2.91776039548315,-2.91483692612768,
-2.91118977566164,-2.90409181244655,-2.87352577323981,-2.8494382911359,
-2.84194902811961,-2.83675059471398,-2.83450968654787,-2.83285265165939,
-2.83096142877433,-2.8276649057338,-2.81236115396795,-2.80116782631181),
 .UNSPECIFIED.);
#2521=B_SPLINE_CURVE_WITH_KNOTS('',3,(#82395,#82396,#82397,#82398,#82399,
#82400,#82401,#82402,#82403,#82404,#82405,#82406,#82407,#82408,#82409,#82410,
#82411,#82412,#82413,#82414,#82415,#82416,#82417,#82418,#82419,#82420,#82421,
#82422,#82423,#82424,#82425,#82426,#82427,#82428,#82429,#82430,#82431,#82432,
#82433,#82434,#82435,#82436,#82437,#82438,#82439,#82440,#82441,#82442,#82443,
#82444,#82445,#82446,#82447,#82448,#82449,#82450,#82451,#82452,#82453,#82454,
#82455,#82456,#82457,#82458,#82459,#82460,#82461,#82462,#82463,#82464,#82465,
#82466,#82467,#82468,#82469,#82470,#82471,#82472,#82473,#82474,#82475,#82476,
#82477,#82478,#82479,#82480,#82481,#82482,#82483,#82484,#82485,#82486,#82487,
#82488,#82489,#82490,#82491,#82492,#82493,#82494,#82495,#82496,#82497,#82498,
#82499,#82500,#82501,#82502,#82503,#82504,#82505,#82506,#82507,#82508,#82509,
#82510,#82511,#82512,#82513,#82514,#82515,#82516,#82517,#82518,#82519,#82520,
#82521,#82522,#82523,#82524,#82525,#82526,#82527,#82528,#82529,#82530,#82531,
#82532,#82533,#82534,#82535,#82536,#82537,#82538,#82539,#82540,#82541,#82542,
#82543,#82544,#82545,#82546,#82547,#82548,#82549,#82550,#82551,#82552,#82553,
#82554,#82555,#82556,#82557,#82558,#82559,#82560,#82561,#82562,#82563,#82564,
#82565,#82566,#82567,#82568,#82569,#82570,#82571,#82572,#82573,#82574,#82575,
#82576,#82577,#82578,#82579,#82580,#82581,#82582,#82583,#82584,#82585,#82586,
#82587,#82588,#82589,#82590,#82591,#82592,#82593,#82594,#82595,#82596,#82597,
#82598,#82599,#82600,#82601,#82602,#82603,#82604,#82605,#82606),
 .UNSPECIFIED.,.F.,.F.,(4,2,2,2,2,2,2,2,2,2,2,2,2,2,2,2,2,2,2,2,2,2,2,2,
2,2,2,2,2,2,2,2,2,2,2,2,2,2,2,2,2,2,2,2,2,2,2,2,2,2,2,2,2,2,2,2,2,2,2,2,
2,2,2,2,2,2,2,2,2,2,2,2,2,2,2,2,2,2,2,2,2,2,2,2,2,2,2,2,2,2,2,2,2,2,2,2,
2,2,2,2,2,2,2,2,2,4),(-2.04089325283701,-2.03488002345817,-2.01905373839352,
-2.01188227520751,-2.00604512953212,-2.00270214928738,-1.99977856191135,
-1.99613271797884,-1.98904187672968,-1.95783920246601,-1.93424999138621,
-1.92684271232618,-1.92168647215752,-1.91945267404391,-1.91779642241602,
-1.91590088077647,-1.91258565837322,-1.89694549843513,-1.86614272293891,
-1.84424133897509,-1.83894308347855,-1.83571533796038,-1.83277057751776,
-1.82899132605999,-1.82267694399171,-1.78634047600345,-1.76643820778235,
-1.75969068256678,-1.75488084600167,-1.75270790168013,-1.75107322378854,
-1.74914648520908,-1.74569231611137,-1.7257996322519,-1.7191700797636,-1.69792530801829,
-1.6774333267711,-1.67222413498434,-1.66901545280829,-1.66606503292354,
-1.66224616064027,-1.6537506877938,-1.61438555152277,-1.5929412425914,-1.58819877356428,
-1.58603794271696,-1.58440440997375,-1.58246941923715,-1.57897844440839,
-1.55585755676623,-1.53867538939302,-1.51372775712608,-1.50685199516778,
-1.50329495167688,-1.50065950146912,-1.49735235032511,-1.49168379841302,
-1.4632566528171,-1.4354259318336,-1.42737453362951,-1.42189153944527,-1.41960292161523,
-1.41793919682846,-1.41607264897645,-1.41280229794322,-1.39877347449417,
-1.37238893832772,-1.34946330208362,-1.34105963914633,-1.33721537056422,
-1.33427044600554,-1.33104284422303,-1.32574555533296,-1.30620631217469,
-1.26241419098538,-1.25566910647138,-1.25318988995585,-1.25149344190071,
-1.24970285388847,-1.24678010302129,-1.23704579310809,-1.2291690541304,
-1.1997053828338,-1.17765134794191,-1.17234377622827,-1.1691138822367,-1.16616943338814,
-1.16239372615637,-1.15609239353053,-1.1195233629592,-1.09977209401011,
-1.09305356353447,-1.08825914668566,-1.08608888168716,-1.08445437311293,
-1.08252561696834,-1.0790627881582,-1.05881616229235,-1.05029467310212,
-1.01396627191361,-1.00764867937674,-1.0038684326236,-1.00092340819177,
-0.997695890953684,-0.992399191014008,-0.991202703725535),.UNSPECIFIED.);
#2522=B_SPLINE_CURVE_WITH_KNOTS('',3,(#82607,#82608,#82609,#82610,#82611,
#82612,#82613,#82614,#82615,#82616,#82617,#82618,#82619,#82620,#82621,#82622,
#82623,#82624,#82625,#82626,#82627,#82628,#82629,#82630,#82631,#82632,#82633,
#82634,#82635,#82636,#82637,#82638,#82639,#82640,#82641,#82642,#82643,#82644,
#82645,#82646,#82647,#82648,#82649,#82650,#82651,#82652,#82653,#82654,#82655,
#82656,#82657,#82658,#82659,#82660,#82661,#82662,#82663,#82664,#82665,#82666,
#82667,#82668,#82669,#82670,#82671,#82672,#82673,#82674,#82675,#82676,#82677,
#82678,#82679,#82680,#82681,#82682,#82683,#82684,#82685,#82686,#82687,#82688,
#82689,#82690,#82691,#82692,#82693,#82694,#82695,#82696,#82697,#82698,#82699,
#82700,#82701,#82702,#82703,#82704,#82705,#82706,#82707,#82708,#82709,#82710,
#82711,#82712,#82713,#82714,#82715,#82716,#82717,#82718,#82719,#82720,#82721,
#82722,#82723,#82724,#82725,#82726,#82727,#82728,#82729,#82730,#82731,#82732,
#82733,#82734,#82735,#82736,#82737,#82738,#82739,#82740,#82741,#82742,#82743,
#82744,#82745,#82746,#82747,#82748,#82749,#82750,#82751,#82752,#82753,#82754,
#82755,#82756,#82757,#82758,#82759,#82760,#82761,#82762,#82763,#82764,#82765,
#82766,#82767,#82768,#82769,#82770,#82771,#82772,#82773,#82774,#82775,#82776,
#82777,#82778,#82779,#82780,#82781,#82782,#82783,#82784,#82785,#82786,#82787,
#82788,#82789,#82790,#82791,#82792,#82793,#82794,#82795,#82796,#82797,#82798,
#82799,#82800,#82801,#82802,#82803,#82804,#82805,#82806,#82807,#82808,#82809,
#82810,#82811,#82812,#82813,#82814,#82815,#82816),.UNSPECIFIED.,.F.,.F.,
(4,2,2,2,2,2,2,2,2,2,2,2,2,2,2,2,2,2,2,2,2,2,2,2,2,2,2,2,2,2,2,2,2,2,2,
2,2,2,2,2,2,2,2,2,2,2,2,2,2,2,2,2,2,2,2,2,2,2,2,2,2,2,2,2,2,2,2,2,2,2,2,
2,2,2,2,2,2,2,2,2,2,2,2,2,2,2,2,2,2,2,2,2,2,2,2,2,2,2,2,2,2,2,2,2,4),(-2.80116782631181,
-2.78345590479573,-2.76752029609109,-2.76031694495084,-2.75445961730744,
-2.75111257458051,-2.74818978514135,-2.74455064852746,-2.73749127432704,
-2.70985972968383,-2.68710773507315,-2.6770199676966,-2.67057130291734,
-2.66813428564755,-2.66644599107477,-2.66464174578481,-2.66165588854913,
-2.65128716642556,-2.64412803770998,-2.61526530905202,-2.60027008346914,
-2.59012040289523,-2.58598888338326,-2.58299935706053,-2.57988257312088,
-2.57510423029716,-2.56110563901031,-2.52723649010585,-2.50767777851583,
-2.50312984630463,-2.50100496403787,-2.49951622113102,-2.49761576272922,
-2.49427820286278,-2.47841408752629,-2.44776855049549,-2.42595142674195,
-2.42065845973856,-2.41743208075945,-2.41448738785635,-2.4107066097561,
-2.40438608446808,-2.36814603262279,-2.34817067278152,-2.34140901587174,
-2.33659168369742,-2.3344175340602,-2.33278290413906,-2.3308574243206,-2.32740826826218,
-2.30770686444933,-2.30131499788068,-2.2807009110262,-2.25924717837823,
-2.25397629975452,-2.25075463981858,-2.24780858690943,-2.24401817826321,
-2.23766357188359,-2.20211151093786,-2.17275056624929,-2.16918864667136,
-2.16725981503818,-2.16560993671905,-2.16346797894878,-2.15870199111724,
-2.13274418915726,-2.11067813679549,-2.09836429633697,-2.08955500120654,
-2.08564036330166,-2.08268582671481,-2.07949061657841,-2.07434362233748,
-2.05716749156462,-2.02529865620164,-2.0073898210671,-2.00302406836584,
-2.00093348852086,-1.99944847027742,-1.9975240620685,-1.99408023644856,
-1.97459008553509,-1.96762703131112,-1.94612239807934,-1.93260090140743,
-1.92317158612055,-1.91915349793937,-1.91618292336195,-1.91340858598037,
-1.90879699485854,-1.8961697534092,-1.87477223497412,-1.84064401704851,
-1.83633318782534,-1.83425312099807,-1.83261013002256,-1.83060631706391,
-1.82668138959702,-1.82151666665777,-1.80868719972153,-1.77730233395422,
-1.75908736583416,-1.75389141464338,-1.75137704512006),.UNSPECIFIED.);
#2523=B_SPLINE_CURVE_WITH_KNOTS('',3,(#82822,#82823,#82824,#82825,#82826,
#82827,#82828,#82829,#82830,#82831,#82832,#82833,#82834,#82835,#82836,#82837,
#82838,#82839,#82840,#82841,#82842,#82843,#82844,#82845,#82846,#82847,#82848,
#82849,#82850,#82851,#82852,#82853,#82854,#82855,#82856,#82857,#82858,#82859,
#82860,#82861,#82862,#82863,#82864,#82865,#82866,#82867,#82868,#82869,#82870,
#82871,#82872,#82873,#82874,#82875,#82876,#82877,#82878,#82879,#82880,#82881,
#82882,#82883,#82884,#82885,#82886,#82887,#82888,#82889,#82890,#82891,#82892,
#82893,#82894,#82895,#82896,#82897,#82898,#82899,#82900,#82901,#82902,#82903,
#82904,#82905,#82906,#82907,#82908,#82909,#82910,#82911,#82912,#82913,#82914,
#82915,#82916,#82917,#82918,#82919,#82920,#82921,#82922,#82923,#82924,#82925,
#82926,#82927,#82928,#82929,#82930,#82931,#82932,#82933,#82934,#82935,#82936,
#82937,#82938,#82939,#82940,#82941,#82942,#82943,#82944,#82945,#82946,#82947,
#82948,#82949,#82950,#82951,#82952,#82953,#82954,#82955,#82956,#82957,#82958,
#82959,#82960,#82961,#82962,#82963,#82964,#82965),.UNSPECIFIED.,.F.,.F.,
(4,2,2,2,2,2,2,2,2,2,2,2,2,2,2,2,2,2,2,2,2,2,2,2,2,2,2,2,2,2,2,2,2,2,2,
2,2,2,2,2,2,2,2,2,2,2,2,2,2,2,2,2,2,2,2,2,2,2,2,2,2,2,2,2,2,2,2,2,2,2,2,
4),(-0.701455818686197,-0.698653963592177,-0.691733645617641,-0.67233866922822,
-0.668909941523022,-0.666993636225862,-0.665507204284839,-0.663409406310534,
-0.659028751159122,-0.641051618920354,-0.609116173669334,-0.591917434080134,
-0.586750285374402,-0.58353911656745,-0.580567178226023,-0.576625002024718,
-0.567728957486467,-0.555261715585714,-0.532610357436752,-0.507747248261715,
-0.50296958310099,-0.500814510256348,-0.499142720004325,-0.497165956102399,
-0.493484291703485,-0.466294859234326,-0.430016946196202,-0.423807661692584,
-0.419999365597747,-0.417034130629177,-0.413734538725469,-0.408197743417828,
-0.382292138534256,-0.361569207108754,-0.340175889225034,-0.337002642524091,
-0.334978232915764,-0.333362195540539,-0.331436557804319,-0.327574485585619,
-0.322455936128793,-0.309597496131773,-0.269851509362339,-0.256289974976441,
-0.251669583775284,-0.248672768437047,-0.245813765045003,-0.241891739593872,
-0.232442279509338,-0.218698164151186,-0.197987678407573,-0.193654360067149,
-0.171938229712865,-0.168523693226541,-0.166637316892073,-0.164990049769026,
-0.162823727698003,-0.158373869897881,-0.152163018407613,-0.135220922452886,
-0.103808910639883,-0.0854968837232444,-0.0799212842823975,-0.0764082854379601,
-0.0731161486297614,-0.0686710206803845,-0.058080089679953,-0.0324939177520532,
-0.00750210209393403,-0.00328873696137956,-0.00149728998100912,-2.30206508348421E-6),
 .UNSPECIFIED.);
#2524=B_SPLINE_CURVE_WITH_KNOTS('',3,(#82968,#82969,#82970,#82971,#82972,
#82973,#82974,#82975,#82976,#82977,#82978,#82979,#82980,#82981,#82982,#82983,
#82984,#82985,#82986,#82987,#82988,#82989,#82990,#82991,#82992,#82993,#82994,
#82995,#82996,#82997,#82998,#82999,#83000,#83001,#83002,#83003,#83004,#83005,
#83006,#83007,#83008,#83009,#83010,#83011,#83012,#83013,#83014,#83015,#83016,
#83017,#83018,#83019,#83020,#83021,#83022,#83023,#83024,#83025,#83026,#83027,
#83028,#83029,#83030,#83031,#83032,#83033,#83034,#83035,#83036,#83037,#83038,
#83039,#83040,#83041,#83042,#83043,#83044,#83045,#83046,#83047,#83048,#83049,
#83050,#83051,#83052,#83053,#83054,#83055,#83056,#83057,#83058,#83059,#83060,
#83061,#83062,#83063,#83064,#83065,#83066,#83067,#83068,#83069,#83070,#83071,
#83072,#83073,#83074,#83075,#83076,#83077,#83078,#83079,#83080,#83081,#83082,
#83083,#83084,#83085,#83086,#83087,#83088,#83089,#83090,#83091,#83092,#83093,
#83094,#83095,#83096,#83097,#83098,#83099,#83100,#83101,#83102,#83103,#83104,
#83105,#83106,#83107,#83108,#83109,#83110,#83111,#83112,#83113,#83114,#83115,
#83116,#83117,#83118,#83119,#83120,#83121,#83122,#83123,#83124,#83125,#83126,
#83127,#83128,#83129,#83130,#83131,#83132,#83133,#83134,#83135,#83136,#83137,
#83138,#83139,#83140,#83141,#83142,#83143,#83144,#83145,#83146,#83147,#83148,
#83149,#83150,#83151,#83152,#83153,#83154,#83155,#83156,#83157,#83158,#83159,
#83160,#83161,#83162,#83163,#83164,#83165,#83166,#83167,#83168,#83169,#83170,
#83171,#83172,#83173),.UNSPECIFIED.,.F.,.F.,(4,2,2,2,2,2,2,2,2,2,2,2,2,
2,2,2,2,2,2,2,2,2,2,2,2,2,2,2,2,2,2,2,2,2,2,2,2,2,2,2,2,2,2,2,2,2,2,2,2,
2,2,2,2,2,2,2,2,2,2,2,2,2,2,2,2,2,2,2,2,2,2,2,2,2,2,2,2,2,2,2,2,2,2,2,2,
2,2,2,2,2,2,2,2,2,2,2,2,2,2,2,2,2,4),(-1.97983394230133,-1.97900451886366,
-1.97063146157784,-1.93648801128863,-1.91065213232886,-1.90511696257423,
-1.90181716899311,-1.89885101333463,-1.89504047381688,-1.88882522384161,
-1.84496296546329,-1.82661363535744,-1.82217236919534,-1.8204614449492,
-1.82040777467674,-1.82035415061966,-1.82029977953099,-1.82024373210191,
-1.82018484641563,-1.82012156651851,-1.82005164731877,-1.8199715544604,
-1.81987505596187,-1.81974909698431,-1.81965240054471,-1.81804302975405,
-1.81591017172596,-1.81114898786551,-1.78667034155205,-1.76371333245863,
-1.75116537602916,-1.7422277354903,-1.73827787479246,-1.735304195007,-1.73209500887285,
-1.72693958121286,-1.70956507108421,-1.67774153037674,-1.65983436156657,
-1.65546120451375,-1.65336455111082,-1.65187793303597,-1.64995992905371,
-1.646524764736,-1.62685214439612,-1.62043001027448,-1.59988466043694,-1.57835621247424,
-1.57309756788494,-1.56988924018687,-1.56695957608449,-1.56319662250912,
-1.55495434497435,-1.51513377921272,-1.49350021054638,-1.48874870441909,
-1.48659429026472,-1.48495168817658,-1.48301649259009,-1.47952499891444,
-1.4563828866039,-1.43917887815406,-1.4142276305881,-1.40734606897575,-1.40378450037163,
-1.40114496183966,-1.39783160731943,-1.39214911656198,-1.36018433952475,
-1.33533804670777,-1.32402299358437,-1.32105191789151,-1.31924768161973,
-1.31757339097878,-1.31551911809628,-1.31147543164471,-1.27930347712204,
-1.25674501813584,-1.24345805845707,-1.23890052791752,-1.23582783994372,
-1.23283920424316,-1.22855643497251,-1.21814946913638,-1.18091548599778,
-1.15827711380007,-1.15478865391077,-1.15287488798208,-1.15122243670024,
-1.14905700523686,-1.14434043776846,-1.11913052204263,-1.09622838271795,
-1.08397500647484,-1.07519819064596,-1.07129000843219,-1.0683373432556,
-1.06514129752539,-1.05998664636342,-1.04241427631523,-1.01073053722208,
-0.991436009503103,-0.991428410285835),.UNSPECIFIED.);
#2525=B_SPLINE_CURVE_WITH_KNOTS('',3,(#83179,#83180,#83181,#83182,#83183,
#83184,#83185,#83186),.UNSPECIFIED.,.F.,.F.,(4,1,1,1,1,4),(99.6151588638684,
99.6457915387123,100.643339397058,101.640887255404,102.638435113751,103.635982972097),
 .UNSPECIFIED.);
#2526=B_SPLINE_CURVE_WITH_KNOTS('',3,(#83190,#83191,#83192,#83193,#83194,
#83195,#83196,#83197,#83198,#83199,#83200,#83201,#83202,#83203,#83204,#83205),
 .UNSPECIFIED.,.F.,.F.,(4,3,3,3,3,4),(103.672557568922,103.780375531908,
103.888461548137,103.996693219235,104.105202005396,104.157845013106),
 .UNSPECIFIED.);
#2527=B_SPLINE_CURVE_WITH_KNOTS('',3,(#83206,#83207,#83208,#83209,#83210,
#83211,#83212,#83213,#83214,#83215,#83216,#83217,#83218,#83219,#83220,#83221,
#83222,#83223,#83224,#83225,#83226,#83227,#83228,#83229,#83230,#83231,#83232,
#83233,#83234,#83235,#83236,#83237,#83238,#83239,#83240,#83241,#83242,#83243,
#83244,#83245,#83246,#83247,#83248,#83249,#83250,#83251,#83252,#83253,#83254,
#83255,#83256,#83257,#83258,#83259,#83260,#83261,#83262,#83263,#83264,#83265,
#83266,#83267,#83268,#83269,#83270,#83271,#83272,#83273,#83274,#83275,#83276,
#83277,#83278,#83279,#83280,#83281,#83282,#83283,#83284,#83285,#83286,#83287,
#83288,#83289,#83290,#83291,#83292,#83293,#83294,#83295,#83296,#83297,#83298,
#83299,#83300,#83301,#83302,#83303,#83304,#83305,#83306,#83307,#83308,#83309,
#83310,#83311,#83312,#83313,#83314,#83315,#83316,#83317,#83318,#83319,#83320,
#83321,#83322,#83323,#83324,#83325,#83326,#83327,#83328,#83329),
 .UNSPECIFIED.,.F.,.F.,(4,3,3,3,3,3,3,3,3,3,3,3,3,3,3,3,3,3,3,3,3,3,3,3,
3,3,3,3,3,3,3,3,3,3,3,3,3,3,3,3,3,4),(99.615625602745,99.7194574215928,
99.823296387637,99.9272456323374,100.031256457386,100.135445667234,100.18725683054,
100.291460612789,100.395509455028,100.499436614079,100.603298520284,100.707129923664,
100.810965531,100.91490990262,101.018913196422,101.12309834819,101.184804688886,
101.288871403733,101.392782575209,101.496571828225,101.600295754678,101.703989304635,
101.807687384949,101.911495669506,102.01536347923,102.119415573608,102.182352547233,
102.286727524034,102.390946759316,102.495042311179,102.599071279357,102.703068173021,
102.807067456587,102.911171629233,103.015332769855,103.119670998472,103.179900405579,
103.28927700551,103.398344095977,103.507224113031,103.615874575054,103.672557568463),
 .UNSPECIFIED.);
#2528=B_SPLINE_CURVE_WITH_KNOTS('',3,(#83335,#83336,#83337,#83338,#83339,
#83340,#83341,#83342,#83343,#83344,#83345,#83346,#83347,#83348,#83349,#83350,
#83351,#83352,#83353,#83354,#83355,#83356,#83357,#83358,#83359,#83360,#83361,
#83362,#83363,#83364,#83365,#83366,#83367,#83368,#83369,#83370,#83371,#83372,
#83373,#83374,#83375,#83376,#83377,#83378,#83379,#83380,#83381,#83382,#83383,
#83384,#83385,#83386,#83387,#83388,#83389,#83390,#83391,#83392,#83393,#83394,
#83395,#83396,#83397,#83398,#83399,#83400,#83401,#83402,#83403,#83404,#83405,
#83406,#83407,#83408,#83409,#83410,#83411,#83412,#83413,#83414,#83415,#83416,
#83417,#83418,#83419,#83420,#83421,#83422,#83423,#83424,#83425,#83426,#83427,
#83428,#83429,#83430,#83431,#83432,#83433,#83434,#83435,#83436,#83437,#83438,
#83439,#83440,#83441,#83442,#83443,#83444,#83445,#83446,#83447,#83448,#83449,
#83450,#83451,#83452,#83453,#83454,#83455,#83456,#83457,#83458,#83459,#83460,
#83461),.UNSPECIFIED.,.F.,.F.,(4,3,3,3,3,3,3,3,3,3,3,3,3,3,3,3,3,3,3,3,
3,3,3,3,3,3,3,3,3,3,3,3,3,3,3,3,3,3,3,3,3,3,4),(93.3317490773308,93.4356943203675,
93.5397120063864,93.6438984303392,93.6605043886358,93.7646927373985,93.8687258349393,
93.9726368683761,94.0764824233719,94.1802972760791,94.284116159193,94.3880436609508,
94.492029977504,94.5961981698983,94.6580522469819,94.7622418063083,94.8662761651276,
94.9701885281509,95.0740354540436,95.1778517165687,95.2816720460736,95.3856010393288,
95.4895888750435,95.5937586132198,95.6556001053279,95.7597703830589,95.8637853923205,
95.967678398161,96.071505972573,96.1753029176117,96.2791039919371,96.3830139571369,
96.4869828641112,96.5911340358051,96.653147963674,96.7562487060057,96.8592080768891,
96.9620624522899,97.0688899045384,97.1716683414833,97.2744473203426,97.3772955171232,
97.3893722612836),.UNSPECIFIED.);
#2529=B_SPLINE_CURVE_WITH_KNOTS('',3,(#83462,#83463,#83464,#83465,#83466,
#83467),.UNSPECIFIED.,.F.,.F.,(4,1,1,4),(97.3893748526128,97.6506958220201,
98.6482436803662,99.6151588638684),.UNSPECIFIED.);
#2530=B_SPLINE_CURVE_WITH_KNOTS('',3,(#83469,#83470,#83471,#83472,#83473,
#83474,#83475,#83476,#83477,#83478,#83479,#83480,#83481,#83482,#83483,#83484,
#83485,#83486,#83487,#83488,#83489,#83490,#83491,#83492,#83493,#83494,#83495,
#83496,#83497,#83498,#83499,#83500,#83501,#83502,#83503,#83504,#83505,#83506,
#83507,#83508,#83509,#83510,#83511,#83512,#83513,#83514,#83515,#83516,#83517,
#83518,#83519,#83520,#83521,#83522,#83523,#83524,#83525,#83526,#83527,#83528,
#83529,#83530,#83531,#83532,#83533,#83534,#83535),.UNSPECIFIED.,.F.,.F.,
(4,3,3,3,3,3,3,3,3,3,3,3,3,3,3,3,3,3,3,3,3,3,4),(97.3893722616737,97.4918529892095,
97.5942444088535,97.6965831845408,97.7989059037925,97.9013194298888,98.0037771698216,
98.1064188388956,98.1921611138482,98.2963314227872,98.4003464633012,98.5042395003148,
98.6080671058345,98.7118640818712,98.8156651870409,98.9195751826418,99.0235441198136,
99.1276953210577,99.1897089721943,99.296188129832,99.4002221364742,99.5079238696096,
99.615625602745),.UNSPECIFIED.);
#2531=B_SPLINE_CURVE_WITH_KNOTS('',3,(#83536,#83537,#83538,#83539,#83540,
#83541,#83542,#83543,#83544,#83545,#83546,#83547,#83548,#83549,#83550,#83551,
#83552,#83553,#83554,#83555,#83556,#83557,#83558,#83559,#83560,#83561,#83562,
#83563,#83564,#83565,#83566,#83567,#83568,#83569,#83570,#83571,#83572,#83573,
#83574,#83575,#83576,#83577,#83578,#83579,#83580,#83581,#83582,#83583,#83584,
#83585,#83586,#83587,#83588,#83589,#83590,#83591,#83592,#83593,#83594,#83595,
#83596,#83597,#83598,#83599,#83600,#83601,#83602,#83603,#83604,#83605,#83606,
#83607,#83608,#83609,#83610,#83611,#83612,#83613,#83614,#83615,#83616,#83617,
#83618,#83619,#83620,#83621,#83622,#83623,#83624,#83625,#83626,#83627,#83628,
#83629,#83630,#83631,#83632,#83633,#83634,#83635,#83636,#83637,#83638,#83639,
#83640,#83641,#83642,#83643,#83644,#83645,#83646,#83647,#83648,#83649,#83650,
#83651,#83652,#83653,#83654,#83655,#83656,#83657,#83658,#83659),
 .UNSPECIFIED.,.F.,.F.,(4,3,3,3,3,3,3,3,3,3,3,3,3,3,3,3,3,3,3,3,3,3,3,3,
3,3,3,3,3,3,3,3,3,3,3,3,3,3,3,3,3,4),(93.3327290376809,93.4413841180287,
93.5452716275018,93.6491032997823,93.7529138981754,93.8567381522104,93.9606769597197,
94.0646832349844,94.1688628732916,94.2019696804638,94.3061564126513,94.4101879112232,
94.5140973791007,94.6179413899405,94.7217547219675,94.8255721099723,94.9294981655111,
95.0334830612258,95.1376498879826,95.1995175388099,95.3037016482382,95.4077305168747,
95.5116373568137,95.6154787423622,95.7192894555727,95.8231042350685,95.9270277156885,
96.0310100515411,96.135174369962,96.197065397156,96.3012537430123,96.4052868376805,
96.5091978683075,96.6130434205334,96.7168582705147,96.8206771509499,96.9246046501185,
97.0285909641294,97.1327591540816,97.1946132555021,97.3456022854055,97.3893722612836),
 .UNSPECIFIED.);
#2532=B_SPLINE_CURVE_WITH_KNOTS('',3,(#83665,#83666,#83667,#83668,#83669,
#83670,#83671,#83672,#83673,#83674,#83675,#83676,#83677,#83678,#83679,#83680,
#83681,#83682,#83683,#83684,#83685,#83686,#83687,#83688,#83689,#83690,#83691,
#83692,#83693,#83694,#83695,#83696,#83697,#83698,#83699,#83700,#83701,#83702,
#83703,#83704,#83705,#83706,#83707,#83708,#83709,#83710,#83711,#83712,#83713,
#83714,#83715,#83716,#83717,#83718,#83719,#83720,#83721,#83722,#83723,#83724,
#83725,#83726,#83727,#83728,#83729,#83730,#83731,#83732,#83733,#83734,#83735,
#83736,#83737,#83738,#83739,#83740,#83741,#83742,#83743,#83744,#83745,#83746,
#83747,#83748,#83749,#83750,#83751,#83752,#83753,#83754,#83755,#83756,#83757,
#83758,#83759,#83760,#83761,#83762,#83763,#83764,#83765,#83766,#83767,#83768,
#83769,#83770,#83771,#83772,#83773,#83774,#83775,#83776,#83777,#83778,#83779,
#83780,#83781,#83782,#83783,#83784,#83785),.UNSPECIFIED.,.F.,.F.,(4,3,3,
3,3,3,3,3,3,3,3,3,3,3,3,3,3,3,3,3,3,3,3,3,3,3,3,3,3,3,3,3,3,3,3,3,3,3,3,
3,4),(87.0493974330828,87.1532189759333,87.2570297769115,87.3615766423234,
87.4655324356433,87.5703748371013,87.6752172385592,87.7794034197749,87.8834343624418,
87.9873432698304,88.0911867176639,88.1949994850163,88.2988163075253,88.4027418002447,
88.5067261338019,88.6108924055833,88.6727650969053,88.7769513493665,88.8809823641162,
88.9848913444718,89.0887348657768,89.1925477069926,89.2963646036455,89.4002901704179,
89.5042745780882,89.6084409232665,89.6703129552514,89.7744988577207,89.8785295217727,
89.9824381520657,90.0862813238876,90.1900938167078,90.2939103665602,90.3978355913381,
90.5018196592078,90.60598567173,90.6678608135975,90.7807059010898,90.8932651225515,
91.0053652788941,91.106186953809),.UNSPECIFIED.);
#2533=B_SPLINE_CURVE_WITH_KNOTS('',3,(#83786,#83787,#83788,#83789,#83790,
#83791,#83792,#83793,#83794,#83795,#83796,#83797,#83798,#83799,#83800,#83801,
#83802,#83803,#83804,#83805,#83806,#83807,#83808,#83809,#83810,#83811,#83812,
#83813,#83814,#83815,#83816,#83817,#83818,#83819,#83820,#83821,#83822,#83823,
#83824,#83825,#83826,#83827,#83828,#83829,#83830,#83831,#83832,#83833,#83834,
#83835,#83836,#83837,#83838,#83839,#83840,#83841,#83842,#83843,#83844,#83845,
#83846,#83847,#83848,#83849,#83850,#83851,#83852,#83853,#83854,#83855),
 .UNSPECIFIED.,.F.,.F.,(4,3,3,3,3,3,3,3,3,3,3,3,3,3,3,3,3,3,3,3,3,3,3,4),
(91.106186954104,91.212569719702,91.3190337392315,91.4256926630366,91.5324645384253,
91.6394564162905,91.6654086719436,91.7695954062995,91.873626907053,91.977536377121,
92.0813803901557,92.1851937243787,92.2890111145775,92.3929371722919,92.4969220701752,
92.6010888990659,92.6629565302897,92.7671202580396,92.8711391143289,92.9750481164967,
93.0788912429734,93.1826959325472,93.2865260637055,93.3317490773308),
 .UNSPECIFIED.);
#2534=B_SPLINE_CURVE_WITH_KNOTS('',3,(#83857,#83858,#83859,#83860,#83861,
#83862,#83863,#83864,#83865,#83866,#83867,#83868,#83869,#83870,#83871,#83872,
#83873,#83874,#83875,#83876,#83877,#83878,#83879,#83880,#83881,#83882,#83883,
#83884,#83885,#83886,#83887,#83888,#83889,#83890,#83891,#83892,#83893,#83894,
#83895,#83896,#83897,#83898,#83899,#83900,#83901,#83902,#83903,#83904,#83905,
#83906,#83907,#83908,#83909,#83910,#83911,#83912,#83913,#83914,#83915,#83916,
#83917,#83918,#83919,#83920,#83921,#83922,#83923,#83924,#83925,#83926),
 .UNSPECIFIED.,.F.,.F.,(4,3,3,3,3,3,3,3,3,3,3,3,3,3,3,3,3,3,3,3,3,3,3,4),
(91.106186954104,91.2093261054256,91.3135123575092,91.4175433718793,91.5214523518541,
91.6252958727778,91.7291087136125,91.8329256098846,91.9368511762801,92.040835583575,
92.145001928384,92.2068739637717,92.3110598670734,92.4150905319584,92.5189991630805,
92.6228423357289,92.7266548293718,92.8304713800421,92.9343966056245,93.0383806742926,
93.1425466875947,93.2044218221178,93.3086062150329,93.3327290376809),
 .UNSPECIFIED.);
#2535=B_SPLINE_CURVE_WITH_KNOTS('',3,(#83927,#83928,#83929,#83930,#83931,
#83932,#83933,#83934,#83935,#83936,#83937,#83938,#83939,#83940,#83941,#83942,
#83943,#83944,#83945,#83946,#83947,#83948,#83949,#83950,#83951,#83952,#83953,
#83954,#83955,#83956,#83957,#83958,#83959,#83960,#83961,#83962,#83963,#83964,
#83965,#83966,#83967,#83968,#83969,#83970,#83971,#83972,#83973,#83974,#83975,
#83976,#83977,#83978,#83979,#83980,#83981,#83982,#83983,#83984,#83985,#83986,
#83987,#83988,#83989,#83990,#83991,#83992,#83993,#83994,#83995,#83996,#83997,
#83998,#83999,#84000,#84001,#84002,#84003,#84004,#84005,#84006,#84007,#84008,
#84009,#84010,#84011,#84012,#84013,#84014,#84015,#84016,#84017,#84018,#84019,
#84020,#84021,#84022,#84023,#84024,#84025,#84026,#84027,#84028,#84029,#84030,
#84031,#84032,#84033,#84034,#84035,#84036,#84037,#84038,#84039,#84040,#84041,
#84042,#84043,#84044,#84045,#84046,#84047,#84048,#84049,#84050),
 .UNSPECIFIED.,.F.,.F.,(4,3,3,3,3,3,3,3,3,3,3,3,3,3,3,3,3,3,3,3,3,3,3,3,
3,3,3,3,3,3,3,3,3,3,3,3,3,3,3,3,3,4),(87.0484536449252,87.1526180428666,
87.2191346720412,87.3233208365449,87.427351762735,87.5312606540702,87.6351040861194,
87.7389168379772,87.8427336453024,87.9466591234119,88.0506434426604,88.1548097007605,
88.2166825303873,88.3208687069942,88.4248996453911,88.5288085490268,88.6326519934275,
88.7364647576692,88.8402815773922,88.9442070678346,89.048191399398,89.1523576696502,
89.2142303887334,89.318416520009,89.4224474130143,89.5263562713859,89.6301996706254,
89.7340123898743,89.8378291648382,89.9417546111836,90.0457388989569,90.1499051263774,
90.2117782470795,90.3146405386459,90.4173275776686,90.519916863471,90.6224449017458,
90.7249481124086,90.8275243327546,90.9301371295155,91.0329110104793,91.1061869536468),
 .UNSPECIFIED.);
#2536=B_SPLINE_CURVE_WITH_KNOTS('',3,(#84056,#84057,#84058,#84059,#84060,
#84061,#84062,#84063,#84064,#84065,#84066,#84067,#84068,#84069,#84070,#84071,
#84072,#84073,#84074,#84075,#84076,#84077,#84078,#84079,#84080,#84081,#84082,
#84083,#84084,#84085,#84086,#84087,#84088,#84089,#84090,#84091,#84092,#84093,
#84094,#84095,#84096,#84097,#84098,#84099,#84100,#84101,#84102,#84103,#84104,
#84105,#84106,#84107,#84108,#84109,#84110,#84111,#84112,#84113,#84114,#84115,
#84116,#84117,#84118,#84119,#84120,#84121,#84122,#84123,#84124,#84125,#84126,
#84127,#84128,#84129,#84130,#84131,#84132,#84133,#84134,#84135,#84136,#84137,
#84138,#84139,#84140,#84141,#84142,#84143,#84144,#84145,#84146,#84147,#84148,
#84149,#84150,#84151,#84152,#84153,#84154,#84155,#84156,#84157,#84158,#84159,
#84160,#84161,#84162,#84163,#84164,#84165,#84166,#84167,#84168,#84169,#84170,
#84171,#84172,#84173,#84174,#84175,#84176),.UNSPECIFIED.,.F.,.F.,(4,3,3,
3,3,3,3,3,3,3,3,3,3,3,3,3,3,3,3,3,3,3,3,3,3,3,3,3,3,3,3,3,3,3,3,3,3,3,3,
3,4),(80.7662049517566,80.8702771424413,80.9742116846458,81.0780706111053,
81.1818887201993,81.2857007566465,81.3896149590624,81.4935789052622,81.5977344251198,
81.6899300884827,81.7941162519364,81.8981471771091,82.0020560674793,82.1058994985962,
82.2097122495556,82.3135290560174,82.4174545333221,82.5214388517977,82.6256051091832,
82.6874779468288,82.7916641121974,82.8956950392976,82.9996039316046,83.103447364663,
83.2072601175657,83.3110769259696,83.4150024052014,83.5189867255985,83.6231529848757,
83.6850258051749,83.7892119647545,83.8932428860618,83.997151772598,84.1009951999023,
84.2048079470758,84.3086247497839,84.4125502234095,84.5165345382425,84.6207007920821,
84.682573663521,84.8230016469244),.UNSPECIFIED.);
#2537=B_SPLINE_CURVE_WITH_KNOTS('',3,(#84177,#84178,#84179,#84180,#84181,
#84182,#84183,#84184,#84185,#84186,#84187,#84188,#84189,#84190,#84191,#84192,
#84193,#84194,#84195,#84196,#84197,#84198,#84199,#84200,#84201,#84202,#84203,
#84204,#84205,#84206,#84207,#84208,#84209,#84210,#84211,#84212,#84213,#84214,
#84215,#84216,#84217,#84218,#84219,#84220,#84221,#84222,#84223,#84224,#84225,
#84226,#84227,#84228,#84229,#84230,#84231,#84232,#84233,#84234,#84235,#84236,
#84237,#84238,#84239,#84240,#84241,#84242,#84243,#84244,#84245,#84246),
 .UNSPECIFIED.,.F.,.F.,(4,3,3,3,3,3,3,3,3,3,3,3,3,3,3,3,3,3,3,3,3,3,3,4),
(84.8230016473326,84.9301416316494,85.0325714156837,85.1349307967564,85.2372563939059,
85.3395847740871,85.4420166327826,85.5445096289189,85.647171050854,85.6801215218671,
85.7843076985368,85.8883386369968,85.9922475406958,86.0960909851597,86.1999037494645,
86.3037205692504,86.4076460597552,86.5116303913806,86.6157966616937,86.6776693802132,
86.7818282136128,86.8858513274357,86.9897581895972,87.0493974330828),
 .UNSPECIFIED.);
#2538=B_SPLINE_CURVE_WITH_KNOTS('',3,(#84248,#84249,#84250,#84251,#84252,
#84253,#84254,#84255,#84256,#84257,#84258,#84259,#84260,#84261,#84262,#84263,
#84264,#84265,#84266,#84267,#84268,#84269,#84270,#84271,#84272,#84273,#84274,
#84275,#84276,#84277,#84278,#84279,#84280,#84281,#84282,#84283,#84284,#84285,
#84286,#84287,#84288,#84289,#84290,#84291,#84292,#84293,#84294,#84295,#84296,
#84297,#84298,#84299,#84300,#84301,#84302,#84303,#84304,#84305,#84306,#84307,
#84308,#84309,#84310,#84311,#84312,#84313,#84314),.UNSPECIFIED.,.F.,.F.,
(4,3,3,3,3,3,3,3,3,3,3,3,3,3,3,3,3,3,3,3,3,3,4),(84.8230016473381,84.9376554433318,
85.0527190367478,85.1683359261974,85.2240389553491,85.3282251207077,85.4322560477978,
85.5361649400947,85.6400083731431,85.7438211260357,85.8476379344296,85.9515634136515,
86.0555477340388,86.1597139933064,86.2215868136952,86.3257394075668,86.4297517315697,
86.5336587783484,86.6374954176377,86.7413356684595,86.8451704367942,86.949111266428,
87.0484536449252),.UNSPECIFIED.);
#2539=B_SPLINE_CURVE_WITH_KNOTS('',3,(#84315,#84316,#84317,#84318,#84319,
#84320,#84321,#84322,#84323,#84324,#84325,#84326,#84327,#84328,#84329,#84330,
#84331,#84332,#84333,#84334,#84335,#84336,#84337,#84338,#84339,#84340,#84341,
#84342,#84343,#84344,#84345,#84346,#84347,#84348,#84349,#84350,#84351,#84352,
#84353,#84354,#84355,#84356,#84357,#84358,#84359,#84360,#84361,#84362,#84363,
#84364,#84365,#84366,#84367,#84368,#84369,#84370,#84371,#84372,#84373,#84374,
#84375,#84376,#84377,#84378,#84379,#84380,#84381,#84382,#84383,#84384,#84385,
#84386,#84387,#84388,#84389,#84390,#84391,#84392,#84393,#84394,#84395,#84396,
#84397,#84398,#84399,#84400,#84401,#84402,#84403,#84404,#84405,#84406,#84407,
#84408,#84409,#84410,#84411,#84412,#84413,#84414,#84415,#84416,#84417,#84418,
#84419,#84420,#84421,#84422,#84423,#84424,#84425,#84426,#84427,#84428,#84429,
#84430,#84431,#84432,#84433,#84434,#84435,#84436,#84437,#84438),
 .UNSPECIFIED.,.F.,.F.,(4,3,3,3,3,3,3,3,3,3,3,3,3,3,3,3,3,3,3,3,3,3,3,3,
3,3,3,3,3,3,3,3,3,3,3,3,3,3,3,3,3,4),(80.7657498360629,80.8695687878009,
80.9734984237827,81.0774898067219,81.1816601811464,81.2338475219647,81.3380336854277,
81.442064610614,81.5459735010043,81.6498169321452,81.7536296831326,81.8574464896258,
81.9613719669677,82.0653562854834,82.1695225429137,82.2313953803108,82.3355815440577,
82.4396124695294,82.5435213602058,82.6473647916331,82.7511775429067,82.8549943496858,
82.9589198273108,83.0629041461088,83.1670704038163,83.2289432386569,83.3331294016878,
83.4371603264439,83.541069216408,83.6449126471255,83.7487253976928,83.8525422037707,
83.9564676807057,84.060451998819,84.1646182558581,84.226491097003,84.3322636670966,
84.4378652907378,84.5433026053193,84.6486432054607,84.7539210457271,84.8230016469244),
 .UNSPECIFIED.);
#2540=B_SPLINE_CURVE_WITH_KNOTS('',3,(#84444,#84445,#84446,#84447,#84448,
#84449,#84450,#84451,#84452,#84453,#84454,#84455,#84456,#84457,#84458,#84459,
#84460,#84461,#84462,#84463,#84464,#84465,#84466,#84467,#84468,#84469,#84470,
#84471,#84472,#84473,#84474,#84475,#84476,#84477,#84478,#84479,#84480,#84481,
#84482,#84483,#84484,#84485,#84486,#84487,#84488,#84489,#84490,#84491,#84492,
#84493,#84494,#84495,#84496,#84497,#84498,#84499,#84500,#84501,#84502,#84503,
#84504,#84505,#84506,#84507,#84508,#84509,#84510,#84511,#84512,#84513,#84514,
#84515,#84516,#84517,#84518,#84519,#84520,#84521,#84522,#84523,#84524,#84525,
#84526,#84527,#84528,#84529,#84530,#84531,#84532,#84533,#84534,#84535,#84536,
#84537,#84538,#84539,#84540,#84541,#84542,#84543,#84544,#84545,#84546,#84547,
#84548,#84549,#84550,#84551,#84552,#84553,#84554,#84555,#84556,#84557,#84558,
#84559,#84560,#84561,#84562,#84563,#84564,#84565,#84566,#84567,#84568,#84569,
#84570),.UNSPECIFIED.,.F.,.F.,(4,3,3,3,3,3,3,3,3,3,3,3,3,3,3,3,3,3,3,3,
3,3,3,3,3,3,3,3,3,3,3,3,3,3,3,3,3,3,3,3,3,3,4),(74.4820670614279,74.586086530966,
74.6902747630355,74.7070950800601,74.8112812435426,74.9153121687491,75.0192210591604,
75.1230644903229,75.2268772413324,75.3306940478484,75.4346195252135,75.538603843753,
75.6427701012071,75.7046429384062,75.8088291018885,75.9128600270946,76.0167689175055,
76.1206123486675,76.2244250996763,76.3282419061915,76.4321673835557,76.5361517020942,
76.6403179595472,76.7021907967523,76.8063769602756,76.9104078855229,77.014316775975,
77.1181602071782,77.2219729582282,77.3257897647846,77.4297152421893,77.5336995607682,
77.637865818261,77.6997386550984,77.8047483656351,77.9072108121554,78.0095758369095,
78.11188016269,78.2188642068654,78.3212057259318,78.423587071241,78.5260937325055,
78.5398163393917),.UNSPECIFIED.);
#2541=B_SPLINE_CURVE_WITH_KNOTS('',3,(#84571,#84572,#84573,#84574,#84575,
#84576,#84577,#84578,#84579,#84580,#84581,#84582,#84583,#84584,#84585,#84586,
#84587,#84588,#84589,#84590,#84591,#84592,#84593,#84594,#84595,#84596,#84597,
#84598,#84599,#84600,#84601,#84602,#84603,#84604,#84605,#84606,#84607,#84608,
#84609,#84610,#84611,#84612,#84613,#84614,#84615,#84616,#84617,#84618,#84619,
#84620,#84621,#84622,#84623,#84624,#84625,#84626,#84627,#84628,#84629,#84630,
#84631,#84632,#84633,#84634,#84635,#84636,#84637),.UNSPECIFIED.,.F.,.F.,
(4,3,3,3,3,3,3,3,3,3,3,3,3,3,3,3,3,3,3,3,3,3,4),(78.5398163397448,78.6972865134445,
78.8014726769072,78.9055036020933,79.0094124924833,79.113255923624,79.217068674611,
79.3208854811044,79.4248109584459,79.5287952769616,79.6329615343917,79.6948343717905,
79.7990205355389,79.9030514610121,80.0069603516901,80.1108037831191,80.2146165343943,
80.3184333411751,80.4223588188016,80.5263431376011,80.6305093953101,80.6923822301366,
80.7662049517566),.UNSPECIFIED.);
#2542=B_SPLINE_CURVE_WITH_KNOTS('',3,(#84639,#84640,#84641,#84642,#84643,
#84644,#84645,#84646,#84647,#84648,#84649,#84650,#84651,#84652,#84653,#84654,
#84655,#84656,#84657,#84658,#84659,#84660,#84661,#84662,#84663,#84664,#84665,
#84666,#84667,#84668,#84669,#84670,#84671,#84672,#84673,#84674,#84675,#84676,
#84677,#84678,#84679,#84680,#84681,#84682,#84683,#84684,#84685,#84686,#84687,
#84688,#84689,#84690,#84691,#84692,#84693,#84694,#84695,#84696,#84697,#84698,
#84699,#84700,#84701,#84702,#84703,#84704,#84705),.UNSPECIFIED.,.F.,.F.,
(4,3,3,3,3,3,3,3,3,3,3,3,3,3,3,3,3,3,3,3,3,3,4),(78.5398163397448,78.6430480181452,
78.7462408135878,78.849430289094,78.9527248465251,79.0560730499682,79.1596112159241,
79.2387518052725,79.3429379687956,79.4469688940427,79.5508777844945,79.6547212156975,
79.7585339667471,79.8623507733033,79.9662762507078,80.0702605692864,80.174426826779,
80.2362996636186,80.3404816764164,80.446798716328,80.5507036981358,80.6582267670993,
80.7657498360629),.UNSPECIFIED.);
#2543=B_SPLINE_CURVE_WITH_KNOTS('',3,(#84706,#84707,#84708,#84709,#84710,
#84711,#84712,#84713,#84714,#84715,#84716,#84717,#84718,#84719,#84720,#84721,
#84722,#84723,#84724,#84725,#84726,#84727,#84728,#84729,#84730,#84731,#84732,
#84733,#84734,#84735,#84736,#84737,#84738,#84739,#84740,#84741,#84742,#84743,
#84744,#84745,#84746,#84747,#84748,#84749,#84750,#84751,#84752,#84753,#84754,
#84755,#84756,#84757,#84758,#84759,#84760,#84761,#84762,#84763,#84764,#84765,
#84766,#84767,#84768,#84769,#84770,#84771,#84772,#84773,#84774,#84775,#84776,
#84777,#84778,#84779,#84780,#84781,#84782,#84783,#84784,#84785,#84786,#84787,
#84788,#84789,#84790,#84791,#84792,#84793,#84794,#84795,#84796,#84797,#84798,
#84799,#84800,#84801,#84802,#84803,#84804,#84805,#84806,#84807,#84808,#84809,
#84810,#84811,#84812,#84813,#84814,#84815,#84816,#84817,#84818,#84819,#84820,
#84821,#84822,#84823,#84824,#84825,#84826,#84827,#84828,#84829),
 .UNSPECIFIED.,.F.,.F.,(4,3,3,3,3,3,3,3,3,3,3,3,3,3,3,3,3,3,3,3,3,3,3,3,
3,3,3,3,3,3,3,3,3,3,3,3,3,3,3,3,3,4),(74.4832484951464,74.5871391658907,
74.690972419831,74.7947830229148,74.8986057057301,75.0025419983178,75.1065443425921,
75.2107214275004,75.2485603718882,75.3527465353754,75.4567774605867,75.5606863510026,
75.6645297821697,75.7683425331835,75.8721593397041,75.9760848170733,76.080069135617,
76.1842353930752,76.2461082302343,76.350294393727,76.454325318944,76.5582342093655,
76.6620776405382,76.7658903915577,76.8697071980837,76.9736326754586,77.0776169940078,
77.1817832514714,77.2436560885804,77.3478422520627,77.451873177269,77.5557820676804,
77.6596254988429,77.7634382498522,77.8672550563685,77.9711805337336,78.0751648522732,
78.1793311097274,78.2412039469264,78.3682032552001,78.4934616304961,78.5398163394136),
 .UNSPECIFIED.);
#2544=B_SPLINE_CURVE_WITH_KNOTS('',3,(#84835,#84836,#84837,#84838,#84839,
#84840,#84841,#84842,#84843,#84844,#84845,#84846,#84847,#84848,#84849,#84850,
#84851,#84852,#84853,#84854,#84855,#84856,#84857,#84858,#84859,#84860,#84861,
#84862,#84863,#84864,#84865,#84866,#84867,#84868,#84869,#84870,#84871,#84872,
#84873,#84874,#84875,#84876,#84877,#84878,#84879,#84880,#84881,#84882,#84883,
#84884,#84885,#84886,#84887,#84888,#84889,#84890,#84891,#84892,#84893,#84894,
#84895,#84896,#84897,#84898,#84899,#84900,#84901,#84902,#84903,#84904,#84905,
#84906,#84907,#84908,#84909,#84910,#84911,#84912,#84913,#84914,#84915,#84916,
#84917,#84918,#84919,#84920,#84921,#84922,#84923,#84924,#84925,#84926,#84927,
#84928,#84929,#84930,#84931,#84932,#84933,#84934,#84935,#84936,#84937,#84938,
#84939,#84940,#84941,#84942,#84943,#84944,#84945,#84946,#84947,#84948,#84949,
#84950,#84951,#84952,#84953,#84954,#84955),.UNSPECIFIED.,.F.,.F.,(4,3,3,
3,3,3,3,3,3,3,3,3,3,3,3,3,3,3,3,3,3,3,3,3,3,3,3,3,3,3,3,3,3,3,3,3,3,3,3,
3,4),(68.1995463442873,68.303357160343,68.4079698527532,68.5119255604329,
68.6168667452082,68.7218079299836,68.8259940934717,68.9300250186839,69.0339339091008,
69.1377773402689,69.2415900912838,69.3454068978052,69.4493323751756,69.5533166937201,
69.6574829511793,69.7193557883297,69.8235419518176,69.9275728770298,70.0314817674466,
70.1353251986145,70.2391379496291,70.3429547561503,70.4468802335205,70.5508645520649,
70.655030809524,70.7169036466758,70.8210898101647,70.9251207353772,71.0290296257948,
71.1328730569634,71.2366858079789,71.3405026145003,71.4444280918713,71.5484124104167,
71.6525786678765,71.7144515050219,71.8220784528936,71.9307165978115,72.0379272940082,
72.1472791632867,72.2566310325652),.UNSPECIFIED.);
#2545=B_SPLINE_CURVE_WITH_KNOTS('',3,(#84956,#84957,#84958,#84959,#84960,
#84961,#84962,#84963,#84964,#84965,#84966,#84967,#84968,#84969,#84970,#84971,
#84972,#84973,#84974,#84975,#84976,#84977,#84978,#84979,#84980,#84981,#84982,
#84983,#84984,#84985,#84986,#84987,#84988,#84989,#84990,#84991,#84992,#84993,
#84994,#84995,#84996,#84997,#84998,#84999,#85000,#85001,#85002,#85003,#85004,
#85005,#85006,#85007,#85008,#85009,#85010,#85011,#85012,#85013,#85014,#85015,
#85016,#85017,#85018,#85019,#85020,#85021,#85022),.UNSPECIFIED.,.F.,.F.,
(4,3,3,3,3,3,3,3,3,3,3,3,3,3,3,3,3,3,3,3,3,3,4),(72.2566310330054,72.3704731155961,
72.4818133112498,72.5969063373089,72.711999363368,72.8161855268551,72.9202164520663,
73.0241253424822,73.1279687736492,73.231781524663,73.3355983311835,73.4395238085528,
73.5435081270964,73.6476743845545,73.709547221714,73.8137037279895,73.9177183838733,
74.021626189057,74.1254620178884,74.2292882438035,74.3331083624519,74.437001647525,
74.4820670614279),.UNSPECIFIED.);
#2546=B_SPLINE_CURVE_WITH_KNOTS('',3,(#85024,#85025,#85026,#85027,#85028,
#85029,#85030,#85031,#85032,#85033,#85034,#85035,#85036,#85037,#85038,#85039,
#85040,#85041,#85042,#85043,#85044,#85045,#85046,#85047,#85048,#85049,#85050,
#85051,#85052,#85053,#85054,#85055,#85056,#85057,#85058,#85059,#85060,#85061,
#85062,#85063,#85064,#85065,#85066,#85067,#85068,#85069,#85070,#85071,#85072,
#85073,#85074,#85075,#85076,#85077,#85078,#85079,#85080,#85081,#85082,#85083,
#85084,#85085,#85086,#85087,#85088,#85089,#85090,#85091,#85092,#85093),
 .UNSPECIFIED.,.F.,.F.,(4,3,3,3,3,3,3,3,3,3,3,3,3,3,3,3,3,3,3,3,3,3,3,4),
(72.2566310325652,72.3608036974115,72.4648211348936,72.5687165871306,72.6725466326848,
72.7763460710619,72.8801496583902,72.9840619405009,73.0880331866151,73.1921861589882,
73.253464655196,73.3576508186848,73.4616817438974,73.565590634315,73.6694340654837,
73.7732468164993,73.8770636230215,73.9809891003924,74.0849734189378,74.1891396763976,
74.2510125135421,74.3552035653643,74.4592285306948,74.4832484951464),
 .UNSPECIFIED.);
#2547=B_SPLINE_CURVE_WITH_KNOTS('',3,(#85094,#85095,#85096,#85097,#85098,
#85099,#85100,#85101,#85102,#85103,#85104,#85105,#85106,#85107,#85108,#85109,
#85110,#85111,#85112,#85113,#85114,#85115,#85116,#85117,#85118,#85119,#85120,
#85121,#85122,#85123,#85124,#85125,#85126,#85127,#85128,#85129,#85130,#85131,
#85132,#85133,#85134,#85135,#85136,#85137,#85138,#85139,#85140,#85141,#85142,
#85143,#85144,#85145,#85146,#85147,#85148,#85149,#85150,#85151,#85152,#85153,
#85154,#85155,#85156,#85157,#85158,#85159,#85160,#85161,#85162,#85163,#85164,
#85165,#85166,#85167,#85168,#85169,#85170,#85171,#85172,#85173,#85174,#85175,
#85176,#85177,#85178,#85179,#85180,#85181,#85182,#85183,#85184,#85185,#85186,
#85187,#85188,#85189,#85190,#85191,#85192,#85193,#85194,#85195,#85196,#85197,
#85198,#85199,#85200,#85201,#85202,#85203,#85204,#85205,#85206,#85207,#85208,
#85209,#85210,#85211,#85212,#85213,#85214,#85215,#85216,#85217,#85218,#85219,
#85220),.UNSPECIFIED.,.F.,.F.,(4,3,3,3,3,3,3,3,3,3,3,3,3,3,3,3,3,3,3,3,
3,3,3,3,3,3,3,3,3,3,3,3,3,3,3,3,3,3,3,3,3,3,4),(68.1991404978387,68.2657253634656,
68.3699115269538,68.473942452166,68.5778513425829,68.6816947737511,68.785507524766,
68.8893243312875,68.9932498086579,69.0972341272027,69.2014003846619,69.2632732218117,
69.3674593852998,69.4714903105119,69.5753992009289,69.6792426320969,69.7830553831118,
69.8868721896332,69.9907976670036,70.0947819855483,70.1989482430075,70.2608210801578,
70.365007243646,70.4690381688583,70.5729470592753,70.6767904904435,70.7806032414585,
70.8844200479801,70.9883455253506,71.0923298438955,71.1964961013548,71.2583689385038,
71.3625551019919,71.466586027204,71.5704949176209,71.674338348789,71.7781510998038,
71.8819679063252,71.9858933836955,72.0898777022403,72.1940439596994,72.2559167968499,
72.2566310325397),.UNSPECIFIED.);
#2548=B_SPLINE_CURVE_WITH_KNOTS('',3,(#85226,#85227,#85228,#85229,#85230,
#85231,#85232,#85233,#85234,#85235,#85236,#85237,#85238,#85239,#85240,#85241,
#85242,#85243,#85244,#85245,#85246,#85247,#85248,#85249,#85250,#85251,#85252,
#85253,#85254,#85255,#85256,#85257,#85258,#85259,#85260,#85261,#85262,#85263,
#85264,#85265,#85266,#85267,#85268,#85269,#85270,#85271,#85272,#85273,#85274,
#85275,#85276,#85277,#85278,#85279,#85280,#85281,#85282,#85283,#85284,#85285,
#85286,#85287,#85288,#85289,#85290,#85291,#85292,#85293,#85294,#85295,#85296,
#85297,#85298,#85299,#85300,#85301,#85302,#85303,#85304,#85305,#85306,#85307,
#85308,#85309,#85310,#85311,#85312,#85313,#85314,#85315,#85316,#85317,#85318,
#85319,#85320,#85321,#85322,#85323,#85324,#85325,#85326,#85327,#85328,#85329,
#85330,#85331,#85332,#85333,#85334,#85335,#85336,#85337,#85338,#85339,#85340,
#85341,#85342,#85343,#85344,#85345,#85346),.UNSPECIFIED.,.F.,.F.,(4,3,3,
3,3,3,3,3,3,3,3,3,3,3,3,3,3,3,3,3,3,3,3,3,3,3,3,3,3,3,3,3,3,3,3,3,3,3,3,
3,4),(61.9168706104259,62.0208051506025,62.1246640759619,62.2284821848811,
62.3322942220771,62.4362084258424,62.5401723742201,62.6443278953337,62.7365207799071,
62.8407069433953,62.9447378686075,63.0486467590245,63.1524901901926,63.2563029412075,
63.3601197477291,63.4640452250995,63.5680295436442,63.6721958011035,63.7340686382532,
63.8382548017414,63.9422857269535,64.0461946173705,64.1500380485386,64.2538507995536,
64.357667606075,64.4615930834454,64.5655774019902,64.6697436594494,64.7316164965993,
64.8358026600875,64.9398335852996,65.0437424757166,65.1475859068847,65.2513986578996,
65.3552154644213,65.4591409417916,65.5631252603364,65.6672915177956,65.7291643549453,
65.8652061647553,65.973445725137),.UNSPECIFIED.);
#2549=B_SPLINE_CURVE_WITH_KNOTS('',3,(#85347,#85348,#85349,#85350,#85351,
#85352,#85353,#85354,#85355,#85356,#85357,#85358,#85359,#85360,#85361,#85362,
#85363,#85364,#85365,#85366,#85367,#85368,#85369,#85370,#85371,#85372,#85373,
#85374,#85375,#85376,#85377,#85378,#85379,#85380,#85381,#85382,#85383,#85384,
#85385,#85386,#85387,#85388,#85389,#85390,#85391,#85392,#85393,#85394,#85395,
#85396,#85397,#85398,#85399,#85400,#85401,#85402,#85403,#85404,#85405,#85406,
#85407,#85408,#85409,#85410,#85411,#85412,#85413,#85414,#85415,#85416),
 .UNSPECIFIED.,.F.,.F.,(4,3,3,3,3,3,3,3,3,3,3,3,3,3,3,3,3,3,3,3,3,3,3,4),
(65.9734457253856,66.07613177282,66.1787500761625,66.2813369783484,66.3839287747715,
66.4866268116115,66.5893873525257,66.6923186639464,66.7267122132914,66.8308983767795,
66.9349293019917,67.0388381924086,67.1426816235766,67.2464943745915,67.3503111811129,
67.4542366584833,67.558220977028,67.6623872344871,67.7242600716375,67.8284495541671,
67.9324611612316,68.036369644885,68.1402112750346,68.1995463442873),
 .UNSPECIFIED.);
#2550=B_SPLINE_CURVE_WITH_KNOTS('',3,(#85418,#85419,#85420,#85421,#85422,
#85423,#85424,#85425,#85426,#85427,#85428,#85429,#85430,#85431,#85432,#85433,
#85434,#85435,#85436,#85437,#85438,#85439,#85440,#85441,#85442,#85443,#85444,
#85445,#85446,#85447,#85448,#85449,#85450,#85451,#85452,#85453,#85454,#85455,
#85456,#85457,#85458,#85459,#85460,#85461,#85462,#85463,#85464,#85465,#85466,
#85467,#85468,#85469,#85470,#85471,#85472,#85473,#85474,#85475,#85476,#85477,
#85478,#85479,#85480,#85481,#85482,#85483,#85484),.UNSPECIFIED.,.F.,.F.,
(4,3,3,3,3,3,3,3,3,3,3,3,3,3,3,3,3,3,3,3,3,3,4),(65.9734457257113,66.0987387056004,
66.225833092448,66.2706296467734,66.3748158102615,66.4788467354737,66.5827556258906,
66.6865990570587,66.7904118080736,66.8942286145952,66.9981540919656,67.1021384105103,
67.2063046679696,67.2681775051195,67.3723684093497,67.4763780578101,67.580285456456,
67.684125467286,67.7879328708108,67.8918030347045,67.995700077725,68.099756768058,
68.1991404978387),.UNSPECIFIED.);
#2551=B_SPLINE_CURVE_WITH_KNOTS('',3,(#85485,#85486,#85487,#85488,#85489,
#85490,#85491,#85492,#85493,#85494,#85495,#85496,#85497,#85498,#85499,#85500,
#85501,#85502,#85503,#85504,#85505,#85506,#85507,#85508,#85509,#85510,#85511,
#85512,#85513,#85514,#85515,#85516,#85517,#85518,#85519,#85520,#85521,#85522,
#85523,#85524,#85525,#85526,#85527,#85528,#85529,#85530,#85531,#85532,#85533,
#85534,#85535,#85536,#85537,#85538,#85539,#85540,#85541,#85542,#85543,#85544,
#85545,#85546,#85547,#85548,#85549,#85550,#85551,#85552,#85553,#85554,#85555,
#85556,#85557,#85558,#85559,#85560,#85561,#85562,#85563,#85564,#85565,#85566,
#85567,#85568,#85569,#85570,#85571,#85572,#85573,#85574,#85575,#85576,#85577,
#85578,#85579,#85580,#85581,#85582,#85583,#85584,#85585,#85586,#85587,#85588,
#85589,#85590,#85591,#85592,#85593,#85594,#85595,#85596,#85597,#85598,#85599,
#85600,#85601,#85602,#85603,#85604,#85605,#85606,#85607,#85608),
 .UNSPECIFIED.,.F.,.F.,(4,3,3,3,3,3,3,3,3,3,3,3,3,3,3,3,3,3,3,3,3,3,3,3,
3,3,3,3,3,3,3,3,3,3,3,3,3,3,3,3,3,4),(61.9159031139283,62.0198326362226,
62.1238238284354,62.2279940894635,62.2804382133891,62.3846243768772,62.4886553020894,
62.5925641925064,62.6964076236745,62.8002203746894,62.9040371812111,63.0079626585815,
63.1119469771264,63.2161132345856,63.2779860717351,63.3821722352233,63.4862031604358,
63.5901120508527,63.6939554820209,63.7977682330357,63.9015850395574,64.0055105169278,
64.1094948354724,64.2136610929316,64.2755339300812,64.3797200935694,64.4837510187815,
64.5876599091985,64.6915033403665,64.7953160913815,64.8991328979027,65.0030583752731,
65.1070426938177,65.2112089512769,65.2730817884273,65.376601737324,65.4799760620944,
65.583240636246,65.6864470474333,65.789616042058,65.8928309399417,65.9734457253856),
 .UNSPECIFIED.);
#2552=B_SPLINE_CURVE_WITH_KNOTS('',3,(#85614,#85615,#85616,#85617,#85618,
#85619,#85620,#85621,#85622,#85623,#85624,#85625,#85626,#85627,#85628,#85629,
#85630,#85631,#85632,#85633,#85634,#85635,#85636,#85637,#85638,#85639,#85640,
#85641,#85642,#85643,#85644,#85645,#85646,#85647,#85648,#85649,#85650,#85651,
#85652,#85653,#85654,#85655,#85656,#85657,#85658,#85659,#85660,#85661,#85662,
#85663,#85664,#85665,#85666,#85667,#85668,#85669,#85670,#85671,#85672,#85673,
#85674,#85675,#85676,#85677,#85678,#85679,#85680,#85681,#85682,#85683,#85684,
#85685,#85686,#85687,#85688,#85689,#85690,#85691,#85692,#85693,#85694,#85695,
#85696,#85697,#85698,#85699,#85700,#85701,#85702,#85703,#85704,#85705,#85706,
#85707,#85708,#85709,#85710,#85711,#85712,#85713,#85714,#85715,#85716,#85717,
#85718,#85719,#85720,#85721,#85722,#85723,#85724,#85725,#85726,#85727,#85728,
#85729,#85730,#85731,#85732,#85733,#85734,#85735,#85736,#85737),
 .UNSPECIFIED.,.F.,.F.,(4,3,3,3,3,3,3,3,3,3,3,3,3,3,3,3,3,3,3,3,3,3,3,3,
3,3,3,3,3,3,3,3,3,3,3,3,3,3,3,3,3,4),(55.6326045181743,55.7367927089603,
55.7536857714845,55.8578719349726,55.9619028601848,56.0658117506018,56.1696551817699,
56.2734679327848,56.3772847393064,56.4812102166767,56.5851945352215,56.6893607926807,
56.7512336298306,56.8554197933188,56.959450718531,57.0633596089479,57.1672030401161,
57.271015791131,57.3748325976526,57.478758075023,57.5827423935677,57.6869086510269,
57.7487814881766,57.8529676516647,57.9569985768769,58.0609074672939,58.1647508984619,
58.2685636494768,58.3723804559983,58.4763059333687,58.5802902519134,58.6844565093726,
58.7463293465227,58.8496743122095,58.9547475754165,59.0578171667581,59.1608249277454,
59.2638067574364,59.3704201725438,59.4735201525633,59.5818902852146,59.6902604178659),
 .UNSPECIFIED.);
#2553=B_SPLINE_CURVE_WITH_KNOTS('',3,(#85738,#85739,#85740,#85741,#85742,
#85743,#85744,#85745,#85746,#85747,#85748,#85749,#85750,#85751,#85752,#85753,
#85754,#85755,#85756,#85757,#85758,#85759,#85760,#85761,#85762,#85763,#85764,
#85765,#85766,#85767,#85768,#85769,#85770,#85771,#85772,#85773,#85774,#85775,
#85776,#85777,#85778,#85779,#85780,#85781,#85782,#85783,#85784,#85785,#85786,
#85787,#85788,#85789,#85790,#85791,#85792,#85793,#85794,#85795,#85796,#85797,
#85798,#85799,#85800,#85801,#85802,#85803,#85804,#85805,#85806,#85807),
 .UNSPECIFIED.,.F.,.F.,(4,3,3,3,3,3,3,3,3,3,3,3,3,3,3,3,3,3,3,3,3,3,3,4),
(59.690260418206,59.7438772048688,59.8480633683569,59.9520942935691,60.0560031839861,
60.1598466151541,60.2636593661691,60.3674761726906,60.471401650061,60.5753859686057,
60.679552226065,60.7414250632149,60.8456112267031,60.9496421519151,61.0535510423321,
61.1573944735002,61.2612072245151,61.3650240310367,61.468949508407,61.5729338269518,
61.677100084411,61.738972921561,61.8431345897348,61.9168706104259),
 .UNSPECIFIED.);
#2554=B_SPLINE_CURVE_WITH_KNOTS('',3,(#85809,#85810,#85811,#85812,#85813,
#85814,#85815,#85816,#85817,#85818,#85819,#85820,#85821,#85822,#85823,#85824,
#85825,#85826,#85827,#85828,#85829,#85830,#85831,#85832,#85833,#85834,#85835,
#85836,#85837,#85838,#85839,#85840,#85841,#85842,#85843,#85844,#85845,#85846,
#85847,#85848,#85849,#85850,#85851,#85852,#85853,#85854,#85855,#85856,#85857,
#85858,#85859,#85860,#85861,#85862,#85863,#85864,#85865,#85866,#85867,#85868,
#85869,#85870,#85871,#85872,#85873,#85874,#85875),.UNSPECIFIED.,.F.,.F.,
(4,3,3,3,3,3,3,3,3,3,3,3,3,3,3,3,3,3,3,3,3,3,4),(59.690260418206,59.7955628120766,
59.9009059652378,60.0064057077464,60.1119895277645,60.2177899509134,60.2853424966969,
60.3895286601851,60.4935595853974,60.5974684758143,60.7013119069825,60.8051246579974,
60.9089414645189,61.0128669418892,61.116851260434,61.2210175178932,61.282890355043,
61.3870598972607,61.4910835282165,61.5972884246445,61.701128313575,61.8085157137517,
61.9159031139283),.UNSPECIFIED.);
#2555=B_SPLINE_CURVE_WITH_KNOTS('',3,(#85876,#85877,#85878,#85879,#85880,
#85881,#85882,#85883,#85884,#85885,#85886,#85887,#85888,#85889,#85890,#85891,
#85892,#85893,#85894,#85895,#85896,#85897,#85898,#85899,#85900,#85901,#85902,
#85903,#85904,#85905,#85906,#85907,#85908,#85909,#85910,#85911,#85912,#85913,
#85914,#85915,#85916,#85917,#85918,#85919,#85920,#85921,#85922,#85923,#85924,
#85925,#85926,#85927,#85928,#85929,#85930,#85931,#85932,#85933,#85934,#85935,
#85936,#85937,#85938,#85939,#85940,#85941,#85942,#85943,#85944,#85945,#85946,
#85947,#85948,#85949,#85950,#85951,#85952,#85953,#85954,#85955,#85956,#85957,
#85958,#85959,#85960,#85961,#85962,#85963,#85964,#85965,#85966,#85967,#85968,
#85969,#85970,#85971,#85972,#85973,#85974,#85975,#85976,#85977,#85978,#85979,
#85980,#85981,#85982,#85983,#85984,#85985,#85986,#85987,#85988,#85989,#85990,
#85991,#85992,#85993,#85994,#85995,#85996,#85997,#85998,#85999),
 .UNSPECIFIED.,.F.,.F.,(4,3,3,3,3,3,3,3,3,3,3,3,3,3,3,3,3,3,3,3,3,3,3,3,
3,3,3,3,3,3,3,3,3,3,3,3,3,3,3,3,3,4),(55.6335534449754,55.7373867669536,
55.8411973790614,55.9450200119163,56.0489562189317,56.1529584246219,56.2571354224554,
56.2951510633125,56.3993372268006,56.5033681520127,56.6072770424296,56.7111204735977,
56.8149332246126,56.9187500311341,57.0226755085045,57.1266598270492,57.2308260845083,
57.2926989216586,57.3968850851468,57.5009160103587,57.6048249007757,57.7086683319439,
57.812481082959,57.9162978894803,58.0202233668508,58.1242076853956,58.2283739428548,
58.2902467800047,58.3944329434929,58.4984638687049,58.6023727591219,58.70621619029,
58.8100289413049,58.9138457478266,59.0177712251969,59.1217555437416,59.2259218012008,
59.2877946383508,59.4032420886154,59.5183215991948,59.6327919924172,59.6902604177957),
 .UNSPECIFIED.);
#2556=B_SPLINE_CURVE_WITH_KNOTS('',3,(#86005,#86006,#86007,#86008,#86009,
#86010,#86011,#86012,#86013,#86014,#86015,#86016,#86017,#86018,#86019,#86020,
#86021,#86022,#86023,#86024,#86025,#86026,#86027,#86028,#86029,#86030,#86031,
#86032,#86033,#86034,#86035,#86036,#86037,#86038,#86039,#86040,#86041,#86042,
#86043,#86044,#86045,#86046,#86047,#86048,#86049,#86050,#86051,#86052,#86053,
#86054,#86055,#86056,#86057,#86058,#86059,#86060,#86061,#86062,#86063,#86064,
#86065,#86066,#86067,#86068,#86069,#86070,#86071,#86072,#86073,#86074,#86075,
#86076,#86077,#86078,#86079,#86080,#86081,#86082,#86083,#86084,#86085,#86086,
#86087,#86088,#86089,#86090,#86091,#86092,#86093,#86094,#86095,#86096,#86097,
#86098,#86099,#86100,#86101,#86102,#86103,#86104,#86105,#86106,#86107,#86108,
#86109,#86110,#86111,#86112,#86113,#86114,#86115,#86116,#86117,#86118,#86119,
#86120,#86121,#86122,#86123,#86124,#86125,#86126,#86127,#86128),
 .UNSPECIFIED.,.F.,.F.,(4,3,3,3,3,3,3,3,3,3,3,3,3,3,3,3,3,3,3,3,3,3,3,3,
3,3,3,3,3,3,3,3,3,3,3,3,3,3,3,3,3,4),(49.3496765008647,49.4543570310005,
49.5583126187223,49.6633556200652,49.768398621408,49.8725847848962,49.9766157101085,
50.0805246005255,50.1843680316935,50.2881807827084,50.3919975892301,50.4959230666004,
50.5999073851451,50.7040736426044,50.765946479754,50.8701326432422,50.9741635684545,
51.0780724588715,51.1819158900396,51.2857286410545,51.3895454475762,51.4934709249466,
51.5974552434913,51.7016215009506,51.7634943381001,51.8676805015883,51.9717114268002,
52.0756203172172,52.1794637483851,52.2832764994002,52.3870933059214,52.4910187832919,
52.5950031018364,52.6991693592957,52.7610421964462,52.8655509126695,52.9699037514312,
53.07919659133,53.1833373805659,53.2874304651171,53.3915238347378,53.4070751110264),
 .UNSPECIFIED.);
#2557=B_SPLINE_CURVE_WITH_KNOTS('',3,(#86129,#86130,#86131,#86132,#86133,
#86134,#86135,#86136,#86137,#86138,#86139,#86140,#86141,#86142,#86143,#86144,
#86145,#86146,#86147,#86148,#86149,#86150,#86151,#86152,#86153,#86154,#86155,
#86156,#86157,#86158,#86159,#86160,#86161,#86162,#86163,#86164,#86165,#86166,
#86167,#86168,#86169,#86170,#86171,#86172,#86173,#86174,#86175,#86176,#86177,
#86178,#86179,#86180,#86181,#86182,#86183,#86184,#86185,#86186,#86187,#86188,
#86189,#86190,#86191,#86192,#86193,#86194,#86195),.UNSPECIFIED.,.F.,.F.,
(4,3,3,3,3,3,3,3,3,3,3,3,3,3,3,3,3,3,3,3,3,3,4),(53.4070751114777,53.5259953052185,
53.6459937542286,53.7585900547923,53.8627762182805,53.9668071434928,54.0707160339098,
54.1745594650779,54.2783722160929,54.3821890226143,54.4861144999848,54.5900988185296,
54.6942650759888,54.7561379131384,54.8656962387679,54.9697007565417,55.0736032474321,
55.1774385720688,55.28124150922,55.38509253526,55.4889714123817,55.5929703714219,
55.6326045181743),.UNSPECIFIED.);
#2558=B_SPLINE_CURVE_WITH_KNOTS('',3,(#86197,#86198,#86199,#86200,#86201,
#86202,#86203,#86204,#86205,#86206,#86207,#86208,#86209,#86210,#86211,#86212,
#86213,#86214,#86215,#86216,#86217,#86218,#86219,#86220,#86221,#86222,#86223,
#86224,#86225,#86226,#86227,#86228,#86229,#86230,#86231,#86232,#86233,#86234,
#86235,#86236,#86237,#86238,#86239,#86240,#86241,#86242,#86243,#86244,#86245,
#86246,#86247,#86248,#86249,#86250,#86251,#86252,#86253,#86254,#86255,#86256,
#86257,#86258,#86259,#86260,#86261,#86262,#86263,#86264,#86265,#86266),
 .UNSPECIFIED.,.F.,.F.,(4,3,3,3,3,3,3,3,3,3,3,3,3,3,3,3,3,3,3,3,3,3,3,4),
(53.4070751114785,53.5098614913148,53.6124973139475,53.7150505550742,53.8175576893134,
53.9200551251567,54.0226483900827,54.1252912590462,54.2281147116669,54.3000553466204,
54.4042415101085,54.5082724353207,54.6121813257377,54.7160247569058,54.8198375079206,
54.9236543144423,55.0275797918127,55.1315641103575,55.2357303678167,55.2976032049664,
55.401768679066,55.5057980059528,55.609707173043,55.6335534449754),
 .UNSPECIFIED.);
#2559=B_SPLINE_CURVE_WITH_KNOTS('',3,(#86267,#86268,#86269,#86270,#86271,
#86272,#86273,#86274,#86275,#86276,#86277,#86278,#86279,#86280,#86281,#86282,
#86283,#86284,#86285,#86286,#86287,#86288,#86289,#86290,#86291,#86292,#86293,
#86294,#86295,#86296,#86297,#86298,#86299,#86300,#86301,#86302,#86303,#86304,
#86305,#86306,#86307,#86308,#86309,#86310,#86311,#86312,#86313,#86314,#86315,
#86316,#86317,#86318,#86319,#86320,#86321,#86322,#86323,#86324,#86325,#86326,
#86327,#86328,#86329,#86330,#86331,#86332,#86333,#86334,#86335,#86336,#86337,
#86338,#86339,#86340,#86341,#86342,#86343,#86344,#86345,#86346,#86347,#86348,
#86349,#86350,#86351,#86352,#86353,#86354,#86355,#86356,#86357,#86358,#86359,
#86360,#86361,#86362,#86363,#86364,#86365,#86366,#86367,#86368,#86369,#86370,
#86371,#86372,#86373,#86374,#86375,#86376,#86377,#86378,#86379,#86380,#86381,
#86382,#86383,#86384,#86385,#86386,#86387,#86388,#86389,#86390),
 .UNSPECIFIED.,.F.,.F.,(4,3,3,3,3,3,3,3,3,3,3,3,3,3,3,3,3,3,3,3,3,3,3,3,
3,3,3,3,3,3,3,3,3,3,3,3,3,3,3,3,3,4),(49.3501259974606,49.4542513728051,
49.561202940359,49.6650820702675,49.7689093574742,49.8727195599115,49.9820056482427,
50.085953371695,50.1899737885933,50.2941626580275,50.309863913236,50.4140500767242,
50.5180810019363,50.6219898923532,50.7258333235213,50.8296460745363,50.9334628810578,
51.0373883584282,51.1413726769729,51.2455389344321,51.3074117715821,51.4115979350703,
51.5156288602825,51.6195377506995,51.7233811818676,51.8271939328825,51.9310107394041,
52.0349362167745,52.1389205353193,52.2430867927785,52.3049596299282,52.4091457934164,
52.5131767186286,52.6170856090455,52.7209290402137,52.8247417912286,52.9285585977501,
53.0324840751205,53.1364683936651,53.2406346511244,53.3025074882743,53.4070751110264),
 .UNSPECIFIED.);
#2560=B_SPLINE_CURVE_WITH_KNOTS('',3,(#86396,#86397,#86398,#86399,#86400,
#86401,#86402,#86403,#86404,#86405,#86406,#86407,#86408,#86409,#86410,#86411,
#86412,#86413,#86414,#86415,#86416,#86417,#86418,#86419,#86420,#86421,#86422,
#86423,#86424,#86425,#86426,#86427,#86428,#86429,#86430,#86431,#86432,#86433,
#86434,#86435,#86436,#86437,#86438,#86439,#86440,#86441,#86442,#86443,#86444,
#86445,#86446,#86447,#86448,#86449,#86450,#86451,#86452,#86453,#86454,#86455,
#86456,#86457,#86458,#86459,#86460,#86461,#86462,#86463,#86464,#86465,#86466,
#86467,#86468,#86469,#86470,#86471,#86472,#86473,#86474,#86475,#86476,#86477,
#86478,#86479,#86480,#86481,#86482,#86483,#86484,#86485,#86486,#86487,#86488,
#86489,#86490,#86491,#86492,#86493,#86494,#86495,#86496,#86497,#86498,#86499,
#86500,#86501,#86502,#86503,#86504,#86505,#86506,#86507,#86508,#86509,#86510,
#86511,#86512,#86513,#86514,#86515,#86516),.UNSPECIFIED.,.F.,.F.,(4,3,3,
3,3,3,3,3,3,3,3,3,3,3,3,3,3,3,3,3,3,3,3,3,3,3,3,3,3,3,3,3,3,3,3,3,3,3,3,
3,4),(43.0672771687041,43.171136160571,43.2749542962854,43.3787663206053,
43.482680485421,43.5866443592237,43.690799844705,43.7831114713314,43.8872976348201,
43.9913285600328,44.0952374504504,44.1990808816191,44.3028936326345,44.4067104391567,
44.5106359165277,44.614620235073,44.7187864925329,44.7806593296775,44.8848454931656,
44.9888764183777,45.0927853087945,45.1966287399624,45.3004414909772,45.4042582974987,
45.5081837748689,45.6121680934133,45.7163343508724,45.7782071880236,45.8823933515117,
45.9864242767239,46.0903331671409,46.1941765983088,46.2979893493237,46.401806155845,
46.5057316332152,46.6097159517598,46.713882209219,46.7757550463697,46.8962986192151,
47.0157785770634,47.123889803398),.UNSPECIFIED.);
#2561=B_SPLINE_CURVE_WITH_KNOTS('',3,(#86517,#86518,#86519,#86520,#86521,
#86522,#86523,#86524,#86525,#86526,#86527,#86528,#86529,#86530,#86531,#86532,
#86533,#86534,#86535,#86536,#86537,#86538,#86539,#86540,#86541,#86542,#86543,
#86544,#86545,#86546,#86547,#86548,#86549,#86550,#86551,#86552,#86553,#86554,
#86555,#86556,#86557,#86558,#86559,#86560,#86561,#86562,#86563,#86564,#86565,
#86566,#86567,#86568,#86569,#86570,#86571,#86572,#86573,#86574,#86575,#86576,
#86577,#86578,#86579,#86580,#86581,#86582,#86583,#86584,#86585,#86586),
 .UNSPECIFIED.,.F.,.F.,(4,3,3,3,3,3,3,3,3,3,3,3,3,3,3,3,3,3,3,3,3,3,3,4),
(47.1238898038468,47.2279281355325,47.3319603652862,47.4360206698574,47.5402127556636,
47.644483889522,47.7489375131547,47.7733029047158,47.877489068204,47.9815199934162,
48.0854288838331,48.1892723150013,48.2930850660162,48.3969018725376,48.500827349908,
48.6048116684528,48.7089779259121,48.7708507630619,48.8750265334989,48.9790548139493,
49.0829625287115,49.186799581749,49.2906190127585,49.3496765008647),
 .UNSPECIFIED.);
#2562=B_SPLINE_CURVE_WITH_KNOTS('',3,(#86588,#86589,#86590,#86591,#86592,
#86593,#86594,#86595,#86596,#86597,#86598,#86599,#86600,#86601,#86602,#86603,
#86604,#86605,#86606,#86607,#86608,#86609,#86610,#86611,#86612,#86613,#86614,
#86615,#86616,#86617,#86618,#86619,#86620,#86621,#86622,#86623,#86624,#86625,
#86626,#86627,#86628,#86629,#86630,#86631,#86632,#86633,#86634,#86635,#86636,
#86637,#86638,#86639,#86640,#86641,#86642,#86643,#86644,#86645,#86646,#86647,
#86648,#86649,#86650,#86651,#86652,#86653,#86654,#86655,#86656,#86657),
 .UNSPECIFIED.,.F.,.F.,(4,3,3,3,3,3,3,3,3,3,3,3,3,3,3,3,3,3,3,3,3,3,3,4),
(47.1238898038468,47.2754958859011,47.3172203381978,47.4214065016858,47.5254374268979,
47.6293463173146,47.7331897484826,47.8370024994973,47.9408193060187,48.0447447833889,
48.1487291019335,48.2528953593925,48.3147681965438,48.4189543600319,48.522985285244,
48.6268941756609,48.730737606829,48.8345503578439,48.9383671643653,49.0422926417356,
49.1462769602803,49.2504432177395,49.3123160548899,49.3501259974606),
 .UNSPECIFIED.);
#2563=B_SPLINE_CURVE_WITH_KNOTS('',3,(#86658,#86659,#86660,#86661,#86662,
#86663,#86664,#86665,#86666,#86667,#86668,#86669,#86670,#86671,#86672,#86673,
#86674,#86675,#86676,#86677,#86678,#86679,#86680,#86681,#86682,#86683,#86684,
#86685,#86686,#86687,#86688,#86689,#86690,#86691,#86692,#86693,#86694,#86695,
#86696,#86697,#86698,#86699,#86700,#86701,#86702,#86703,#86704,#86705,#86706,
#86707,#86708,#86709,#86710,#86711,#86712,#86713,#86714,#86715,#86716,#86717,
#86718,#86719,#86720,#86721,#86722,#86723,#86724,#86725,#86726,#86727,#86728,
#86729,#86730,#86731,#86732,#86733,#86734,#86735,#86736,#86737,#86738,#86739,
#86740,#86741,#86742,#86743,#86744,#86745,#86746,#86747,#86748,#86749,#86750,
#86751,#86752,#86753,#86754,#86755,#86756,#86757,#86758,#86759,#86760,#86761,
#86762,#86763,#86764,#86765,#86766,#86767,#86768,#86769,#86770,#86771,#86772,
#86773,#86774,#86775,#86776,#86777,#86778,#86779,#86780,#86781),
 .UNSPECIFIED.,.F.,.F.,(4,3,3,3,3,3,3,3,3,3,3,3,3,3,3,3,3,3,3,3,3,3,3,3,
3,3,3,3,3,3,3,3,3,3,3,3,3,3,3,3,3,4),(43.0661637600767,43.1701547594049,
43.2743249058554,43.3270289048134,43.431215068306,43.5352459935225,43.639154883944,
43.7429983151167,43.8468110661362,43.9506278726624,44.0545533500374,44.1585376685868,
44.2627039260507,44.3245767631595,44.4287629266466,44.5327938518577,44.6367027422735,
44.7405461734405,44.8443589244543,44.9481757309747,45.052101208344,45.1560855268876,
45.2602517843458,45.3221246215056,45.4263107849933,45.530341710205,45.6342506006214,
45.738094031789,45.8419067828034,45.9457235893243,46.0496490666941,46.1536333852383,
46.2577996426969,46.3196724798517,46.4223012412914,46.5247935864418,46.6271863644391,
46.729516280193,46.8318649061931,46.9342176129156,47.0366904241979,47.1238898034407),
 .UNSPECIFIED.);
#2564=B_SPLINE_CURVE_WITH_KNOTS('',3,(#86787,#86788,#86789,#86790,#86791,
#86792,#86793,#86794,#86795,#86796,#86797,#86798,#86799,#86800,#86801,#86802,
#86803,#86804,#86805,#86806,#86807,#86808,#86809,#86810,#86811,#86812,#86813,
#86814,#86815,#86816,#86817,#86818,#86819,#86820,#86821,#86822,#86823,#86824,
#86825,#86826,#86827,#86828,#86829,#86830,#86831,#86832,#86833,#86834,#86835,
#86836,#86837,#86838,#86839,#86840,#86841,#86842,#86843,#86844,#86845,#86846,
#86847,#86848,#86849,#86850,#86851,#86852,#86853,#86854,#86855,#86856,#86857,
#86858,#86859,#86860,#86861,#86862,#86863,#86864,#86865,#86866,#86867,#86868,
#86869,#86870,#86871,#86872,#86873,#86874,#86875,#86876,#86877,#86878,#86879,
#86880,#86881,#86882,#86883,#86884,#86885,#86886,#86887,#86888,#86889,#86890,
#86891,#86892,#86893,#86894,#86895,#86896,#86897,#86898,#86899,#86900,#86901,
#86902,#86903,#86904,#86905,#86906,#86907,#86908,#86909,#86910,#86911,#86912,
#86913),.UNSPECIFIED.,.F.,.F.,(4,3,3,3,3,3,3,3,3,3,3,3,3,3,3,3,3,3,3,3,
3,3,3,3,3,3,3,3,3,3,3,3,3,3,3,3,3,3,3,3,3,3,4),(36.7834483157109,36.8002764629088,
36.9044626263498,37.0084935515138,37.1124024418814,37.2162458729993,37.3200586239635,
37.4238754304336,37.527800907752,37.6317852262444,37.7359514836513,37.7978243212549,
37.9020104847763,38.0060414100222,38.1099503004735,38.2137937316762,38.3176064827261,
38.4214232892828,38.5253487666884,38.6293330852686,38.733499342763,38.795372179601,
38.899558343083,39.003589268289,39.1074981586998,39.2113415898617,39.3151543408705,
39.4189711473858,39.5228966247501,39.6268809432888,39.7310472007422,39.7929200379471,
39.8971062014302,40.0011371266371,40.1050460170487,40.2088894482114,40.3127021992209,
40.4165190057369,40.5204444831017,40.6244288016407,40.7285950590942,40.7904678962932,
40.8407044966673),.UNSPECIFIED.);
#2565=B_SPLINE_CURVE_WITH_KNOTS('',3,(#86914,#86915,#86916,#86917,#86918,
#86919,#86920,#86921,#86922,#86923,#86924,#86925,#86926,#86927,#86928,#86929,
#86930,#86931,#86932,#86933,#86934,#86935,#86936,#86937,#86938,#86939,#86940,
#86941,#86942,#86943,#86944,#86945,#86946,#86947,#86948,#86949,#86950,#86951,
#86952,#86953,#86954,#86955,#86956,#86957,#86958,#86959,#86960,#86961,#86962,
#86963,#86964,#86965,#86966,#86967,#86968,#86969,#86970,#86971,#86972,#86973,
#86974,#86975,#86976,#86977,#86978,#86979,#86980,#86981,#86982,#86983),
 .UNSPECIFIED.,.F.,.F.,(4,3,3,3,3,3,3,3,3,3,3,3,3,3,3,3,3,3,3,3,3,3,3,4),
(40.8407044969994,40.9440746115611,41.0495672544459,41.1526720053879,41.2557188072319,
41.3587435025164,41.4660615655471,41.5692147500897,41.6724388016654,41.7758284060395,
41.7880157546393,41.8922019181263,41.9962328433371,42.100141733753,42.20398516492,
42.3077979159338,42.4116147224541,42.5155401998234,42.6195245183671,42.7236907758253,
42.7855636129853,42.8897412721982,42.9937540506562,43.0672771687041),
 .UNSPECIFIED.);
#2566=B_SPLINE_CURVE_WITH_KNOTS('',3,(#86985,#86986,#86987,#86988,#86989,
#86990,#86991,#86992,#86993,#86994,#86995,#86996,#86997,#86998,#86999,#87000,
#87001,#87002,#87003,#87004,#87005,#87006,#87007,#87008,#87009,#87010,#87011,
#87012,#87013,#87014,#87015,#87016,#87017,#87018,#87019,#87020,#87021,#87022,
#87023,#87024,#87025,#87026,#87027,#87028,#87029,#87030,#87031,#87032,#87033,
#87034,#87035,#87036,#87037,#87038,#87039,#87040,#87041,#87042,#87043,#87044,
#87045,#87046,#87047,#87048,#87049,#87050,#87051),.UNSPECIFIED.,.F.,.F.,
(4,3,3,3,3,3,3,3,3,3,3,3,3,3,3,3,3,3,3,3,3,3,4),(40.8407044969871,40.9497796083699,
41.0591756422983,41.1687426604485,41.2786112447893,41.3319331881212,41.4361193516032,
41.5401502768092,41.64405916722,41.7479025983819,41.8517153493907,41.9555321559061,
42.0594576332705,42.1634419518092,42.2676082092626,42.3294810464673,42.4336404890036,
42.5376570384834,42.6415656994843,42.7477152146324,42.8515331414174,42.9588484507471,
43.0661637600767),.UNSPECIFIED.);
#2567=B_SPLINE_CURVE_WITH_KNOTS('',3,(#87052,#87053,#87054,#87055,#87056,
#87057,#87058,#87059,#87060,#87061,#87062,#87063,#87064,#87065,#87066,#87067,
#87068,#87069,#87070,#87071,#87072,#87073,#87074,#87075,#87076,#87077,#87078,
#87079,#87080,#87081,#87082,#87083,#87084,#87085,#87086,#87087,#87088,#87089,
#87090,#87091,#87092,#87093,#87094,#87095,#87096,#87097,#87098,#87099,#87100,
#87101,#87102,#87103,#87104,#87105,#87106,#87107,#87108,#87109,#87110,#87111,
#87112,#87113,#87114,#87115,#87116,#87117,#87118,#87119,#87120,#87121,#87122,
#87123,#87124,#87125,#87126,#87127,#87128,#87129,#87130,#87131,#87132,#87133,
#87134,#87135,#87136,#87137,#87138,#87139,#87140,#87141,#87142,#87143,#87144,
#87145,#87146,#87147,#87148,#87149,#87150,#87151,#87152,#87153,#87154,#87155,
#87156,#87157,#87158,#87159,#87160,#87161,#87162,#87163,#87164,#87165,#87166,
#87167,#87168,#87169,#87170,#87171,#87172,#87173,#87174,#87175),
 .UNSPECIFIED.,.F.,.F.,(4,3,3,3,3,3,3,3,3,3,3,3,3,3,3,3,3,3,3,3,3,3,3,3,
3,3,3,3,3,3,3,3,3,3,3,3,3,3,3,3,3,4),(36.7837280398568,36.8875386644498,
36.9913612263603,37.095297312041,37.1992993214154,37.3034761958223,37.3417417547369,
37.4459279184719,37.5499588439342,37.6538677346054,37.75771116603,37.8615239173034,
37.9653407240849,38.069266201716,38.1732505205219,38.2774167782407,38.339289613083,
38.4434757765423,38.5475067017258,38.6514155921144,38.7552590232545,38.8590717742416,
38.9628885807358,39.0668140580795,39.170798376598,39.2749646340317,39.3368374714291,
39.4410236348703,39.5450545600342,39.6489634504021,39.7528068815202,39.8566196324845,
39.9604364389551,40.0643619162737,40.1683462347665,40.2725124921736,40.3343853297752,
40.4435562695039,40.5524208008743,40.6611016633605,40.769557770341,40.8407044966673),
 .UNSPECIFIED.);
#2568=B_SPLINE_CURVE_WITH_KNOTS('',3,(#87181,#87182,#87183,#87184,#87185,
#87186,#87187,#87188),.UNSPECIFIED.,.F.,.F.,(4,1,1,1,1,4),(30.4995505102364,
30.8149893128323,31.8125371711784,32.8100850295245,33.8076328878706,34.5575191894876),
 .UNSPECIFIED.);
#2569=B_SPLINE_CURVE_WITH_KNOTS('',3,(#87189,#87190,#87191,#87192,#87193,
#87194,#87195,#87196,#87197,#87198,#87199,#87200,#87201,#87202,#87203,#87204,
#87205,#87206,#87207,#87208,#87209,#87210,#87211,#87212,#87213,#87214,#87215,
#87216,#87217,#87218,#87219,#87220,#87221,#87222,#87223,#87224,#87225,#87226,
#87227,#87228,#87229,#87230,#87231,#87232,#87233,#87234,#87235,#87236,#87237,
#87238,#87239,#87240,#87241,#87242,#87243,#87244,#87245,#87246,#87247,#87248,
#87249,#87250,#87251,#87252,#87253,#87254,#87255),.UNSPECIFIED.,.F.,.F.,
(4,3,3,3,3,3,3,3,3,3,3,3,3,3,3,3,3,3,3,3,3,3,4),(34.557519274484,34.6927957333214,
34.8051807462166,34.909366909953,35.0133978354169,35.1173067260896,35.2211501575158,
35.3249629087908,35.4287797155739,35.5327051932064,35.6366895120138,35.7408557697342,
35.8027286045627,35.9069159429535,36.0109477003919,36.1148561156626,36.2186985864117,
36.3225098920313,36.426324767821,36.5302426834859,36.6342192413344,36.73836490079,
36.7834483157109),.UNSPECIFIED.);
#2570=B_SPLINE_CURVE_WITH_KNOTS('',3,(#87257,#87258,#87259,#87260,#87261,
#87262,#87263,#87264,#87265,#87266,#87267,#87268,#87269,#87270,#87271,#87272,
#87273,#87274,#87275,#87276,#87277,#87278,#87279,#87280,#87281,#87282,#87283,
#87284,#87285,#87286,#87287,#87288,#87289,#87290,#87291,#87292,#87293,#87294,
#87295,#87296,#87297,#87298,#87299,#87300,#87301,#87302,#87303,#87304,#87305,
#87306,#87307,#87308,#87309,#87310,#87311,#87312,#87313,#87314,#87315,#87316,
#87317,#87318,#87319,#87320,#87321,#87322,#87323,#87324,#87325,#87326),
 .UNSPECIFIED.,.F.,.F.,(4,3,3,3,3,3,3,3,3,3,3,3,3,3,3,3,3,3,3,3,3,3,3,4),
(34.5575191897439,34.6600261058214,34.7624492437677,34.8648252112055,34.9671905469454,
35.0696506767749,35.1721598105506,35.2748489352923,35.3466460380447,35.4508322014595,
35.554863126602,35.6587720169556,35.7626154480643,35.8664281990237,35.970245005494,
36.0741704828196,36.1781548013232,36.2823210587477,36.3441938963908,36.4483886654221,
36.5524031605798,36.6563141143402,36.7601506285695,36.7837280398568),
 .UNSPECIFIED.);
#2571=B_SPLINE_CURVE_WITH_KNOTS('',3,(#87327,#87328,#87329,#87330,#87331,
#87332,#87333,#87334,#87335,#87336,#87337,#87338,#87339,#87340,#87341,#87342,
#87343,#87344,#87345,#87346,#87347,#87348,#87349,#87350,#87351,#87352,#87353,
#87354,#87355,#87356,#87357,#87358,#87359,#87360,#87361,#87362,#87363,#87364,
#87365,#87366,#87367,#87368,#87369,#87370,#87371,#87372,#87373,#87374,#87375,
#87376,#87377,#87378,#87379,#87380,#87381,#87382,#87383,#87384,#87385,#87386,
#87387,#87388,#87389,#87390,#87391,#87392,#87393,#87394,#87395,#87396,#87397,
#87398,#87399,#87400,#87401,#87402,#87403,#87404,#87405,#87406,#87407,#87408,
#87409,#87410,#87411,#87412,#87413,#87414,#87415,#87416,#87417,#87418,#87419,
#87420,#87421,#87422,#87423,#87424,#87425,#87426,#87427,#87428,#87429,#87430,
#87431,#87432,#87433,#87434,#87435,#87436,#87437,#87438,#87439,#87440,#87441,
#87442,#87443,#87444,#87445,#87446,#87447,#87448,#87449,#87450),
 .UNSPECIFIED.,.F.,.F.,(4,3,3,3,3,3,3,3,3,3,3,3,3,3,3,3,3,3,3,3,3,3,3,3,
3,3,3,3,3,3,3,3,3,3,3,3,3,3,3,3,3,4),(30.5009012256866,30.6078453980583,
30.7117244622742,30.8155517007811,30.9193618715342,31.0286350548158,31.1325827673511,
31.2366031848782,31.3407920442357,31.3564546046604,31.4606407808707,31.5646717189603,
31.6685806224221,31.7724240667314,31.8762368309641,31.9800536507603,32.0839791414007,
32.1879634732329,32.2921297438626,32.3540024630065,32.4581886271226,32.5622195530122,
32.6661284441775,32.7699718761373,32.8737846279862,32.9776014353829,33.081526913686,
33.1855112331973,33.2896774916665,33.3515503213525,33.455736481262,33.5597674028288,
33.6636762895192,33.7675197169125,33.8713324641099,33.975149266777,34.0790747402627,
34.1830590548998,34.2872253084573,34.3490981796986,34.4951131661248,34.5575191894876),
 .UNSPECIFIED.);
#2572=B_SPLINE_CURVE_WITH_KNOTS('',3,(#87456,#87457,#87458,#87459,#87460,
#87461,#87462,#87463,#87464,#87465,#87466,#87467,#87468,#87469,#87470,#87471,
#87472,#87473,#87474,#87475,#87476,#87477,#87478,#87479,#87480,#87481,#87482,
#87483,#87484,#87485,#87486,#87487,#87488,#87489,#87490,#87491,#87492,#87493,
#87494,#87495,#87496,#87497,#87498,#87499,#87500,#87501,#87502,#87503,#87504,
#87505,#87506,#87507,#87508,#87509,#87510,#87511,#87512,#87513,#87514,#87515,
#87516,#87517,#87518,#87519,#87520,#87521,#87522,#87523,#87524,#87525,#87526,
#87527,#87528,#87529,#87530,#87531,#87532,#87533,#87534,#87535,#87536,#87537,
#87538,#87539,#87540,#87541,#87542,#87543,#87544,#87545,#87546,#87547,#87548,
#87549,#87550,#87551,#87552,#87553,#87554,#87555,#87556,#87557,#87558,#87559,
#87560,#87561,#87562,#87563,#87564,#87565,#87566,#87567,#87568,#87569,#87570,
#87571,#87572,#87573,#87574,#87575,#87576),.UNSPECIFIED.,.F.,.F.,(4,3,3,
3,3,3,3,3,3,3,3,3,3,3,3,3,3,3,3,3,3,3,3,3,3,3,3,3,3,3,3,3,3,3,3,3,3,3,3,
3,4),(24.2175094594017,24.3213278434285,24.4251400466915,24.5290543466609,
24.633018292731,24.737173924033,24.8297021627558,24.9338880829223,25.0379187606929,
25.1418273987454,25.2456705746464,25.3494830678712,25.4532996144562,25.5572248303944,
25.6612088862683,25.7653748819406,25.8272500211019,25.9314362718495,26.0354672852708,
26.1393762648751,26.2432197857851,26.3470326269618,26.4508495239306,26.5547750915589,
26.6587595003909,26.7629258472006,26.824797879448,26.9289840570988,27.0330149970021,
27.1369239028275,27.2407673498393,27.3445801171099,27.4483969402773,27.5523224347774,
27.6563067707512,27.7604730459268,27.822345737794,27.9353427130054,28.0470527868882,
28.160693212764,28.2743336386397),.UNSPECIFIED.);
#2573=B_SPLINE_CURVE_WITH_KNOTS('',3,(#87577,#87578,#87579,#87580,#87581,
#87582),.UNSPECIFIED.,.F.,.F.,(4,1,1,4),(28.2743338823081,28.8198935961401,
29.8174414544862,30.4995505102364),.UNSPECIFIED.);
#2574=B_SPLINE_CURVE_WITH_KNOTS('',3,(#87584,#87585,#87586,#87587,#87588,
#87589,#87590,#87591,#87592,#87593,#87594,#87595,#87596,#87597,#87598,#87599,
#87600,#87601,#87602,#87603,#87604,#87605,#87606,#87607,#87608,#87609,#87610,
#87611,#87612,#87613,#87614,#87615,#87616,#87617,#87618,#87619,#87620,#87621,
#87622,#87623,#87624,#87625,#87626,#87627,#87628,#87629,#87630,#87631,#87632,
#87633,#87634,#87635,#87636,#87637,#87638,#87639,#87640,#87641,#87642,#87643,
#87644,#87645,#87646,#87647,#87648,#87649,#87650,#87651,#87652,#87653),
 .UNSPECIFIED.,.F.,.F.,(4,3,3,3,3,3,3,3,3,3,3,3,3,3,3,3,3,3,3,3,3,3,3,4),
(28.2743338823081,28.3638110296221,28.4679972800027,28.5720282930528,28.675937272281,
28.7797807928121,28.8835936336079,28.9874105301943,29.0913360974404,29.1953205058895,
29.29948685232,29.3613588879682,29.4655450656047,29.5695760054923,29.6734849113002,
29.7773283582932,29.881141125544,29.9849579486899,30.0888834431674,30.1928677791174,
30.2970340542683,30.3589067463143,30.4630838119772,30.5009012256866),
 .UNSPECIFIED.);
#2575=B_SPLINE_CURVE_WITH_KNOTS('',3,(#87654,#87655,#87656,#87657,#87658,
#87659,#87660,#87661,#87662,#87663,#87664,#87665,#87666,#87667,#87668,#87669,
#87670,#87671,#87672,#87673,#87674,#87675,#87676,#87677,#87678,#87679,#87680,
#87681,#87682,#87683,#87684,#87685,#87686,#87687,#87688,#87689,#87690,#87691,
#87692,#87693,#87694,#87695,#87696,#87697,#87698,#87699,#87700,#87701,#87702,
#87703,#87704,#87705,#87706,#87707,#87708,#87709,#87710,#87711,#87712,#87713,
#87714,#87715,#87716,#87717,#87718,#87719,#87720,#87721,#87722,#87723,#87724,
#87725,#87726,#87727,#87728,#87729,#87730,#87731,#87732,#87733,#87734,#87735,
#87736,#87737,#87738,#87739,#87740,#87741,#87742,#87743,#87744,#87745,#87746,
#87747,#87748,#87749,#87750,#87751,#87752,#87753,#87754,#87755,#87756,#87757,
#87758,#87759,#87760,#87761,#87762,#87763,#87764,#87765,#87766,#87767,#87768,
#87769,#87770,#87771,#87772,#87773,#87774,#87775,#87776,#87777),
 .UNSPECIFIED.,.F.,.F.,(4,3,3,3,3,3,3,3,3,3,3,3,3,3,3,3,3,3,3,3,3,3,3,3,
3,3,3,3,3,3,3,3,3,3,3,3,3,3,3,3,3,4),(24.2166158528785,24.3207881219797,
24.3736195962378,24.4778038331522,24.5818328006132,24.685739696451,24.7895811113854,
24.8933918275129,24.9972065834734,25.101130000418,25.2051122498594,25.3092764469012,
25.3711674545839,25.4753541846193,25.5793856815231,25.6832951484569,25.7871391588007,
25.8909524907785,25.9947698791806,26.0986959357944,26.2026808329677,26.3068476617735,
26.3687153129299,26.4729016564542,26.5769327668191,26.680841849117,26.7846854762195,
26.8884984269359,26.9923154366431,27.0962411211505,27.2002256493751,27.3043921182881,
27.366263171276,27.4692311191777,27.572023901783,27.6747188328349,27.7773523095505,
27.8799606447598,27.9826447839181,28.085364888699,28.1882547111826,28.27433388186),
 .UNSPECIFIED.);
#2576=B_SPLINE_CURVE_WITH_KNOTS('',3,(#87783,#87784,#87785,#87786,#87787,
#87788,#87789,#87790,#87791,#87792,#87793,#87794,#87795,#87796,#87797,#87798,
#87799,#87800,#87801,#87802,#87803,#87804,#87805,#87806,#87807,#87808,#87809,
#87810,#87811,#87812,#87813,#87814,#87815,#87816,#87817,#87818,#87819,#87820,
#87821,#87822,#87823,#87824,#87825,#87826,#87827,#87828,#87829,#87830,#87831,
#87832,#87833,#87834,#87835,#87836,#87837,#87838,#87839,#87840,#87841,#87842,
#87843,#87844,#87845,#87846,#87847,#87848,#87849,#87850,#87851,#87852),
 .UNSPECIFIED.,.F.,.F.,(4,3,3,3,3,3,3,3,3,3,3,3,3,3,3,3,3,3,3,3,3,3,3,4),
(15.7079632679489,15.8106738927763,15.9133494515527,16.0160260414383,16.1188128612619,
16.2216580789275,16.3246939332088,16.3932367294691,16.4975142314111,16.6016358337152,
16.7056339423556,16.8095656348978,16.9134655491479,17.0173682784092,17.1213771604187,
17.2254435848118,17.3296889783796,17.3907845878152,17.4951357241063,17.6048037953017,
17.7088847254726,17.8128986127177,17.9168871416275,17.9338080088879),
 .UNSPECIFIED.);
#2577=B_SPLINE_CURVE_WITH_KNOTS('',3,(#87854,#87855,#87856,#87857,#87858),
 .UNSPECIFIED.,.F.,.F.,(4,1,4),(14.3981410127769,15.395688871123,15.7079548164659),
 .UNSPECIFIED.);
#2578=B_SPLINE_CURVE_WITH_KNOTS('',3,(#87862,#87863,#87864,#87865,#87866,
#87867,#87868,#87869,#87870,#87871,#87872,#87873,#87874,#87875,#87876,#87877,
#87878,#87879,#87880,#87881,#87882,#87883,#87884,#87885,#87886,#87887,#87888,
#87889,#87890,#87891,#87892,#87893,#87894,#87895,#87896,#87897,#87898,#87899,
#87900,#87901,#87902,#87903,#87904,#87905,#87906,#87907,#87908,#87909,#87910,
#87911,#87912,#87913,#87914,#87915,#87916,#87917,#87918,#87919),
 .UNSPECIFIED.,.F.,.F.,(4,3,3,3,3,3,3,3,3,3,3,3,3,3,3,3,3,3,3,4),(13.8761929172068,
13.9801050066969,14.0838618081371,14.1874968767277,14.2910672014661,14.3946079563068,
14.4981542724688,14.6018076115749,14.7055219776147,14.8094097434174,14.8542235792949,
14.9609410403274,15.0635681569975,15.1661013730925,15.2685772460228,15.3710322508939,
15.4735544551065,15.5761173355011,15.6788162057539,15.7079632675546),
 .UNSPECIFIED.);
#2579=B_SPLINE_CURVE_WITH_KNOTS('',3,(#87920,#87921,#87922,#87923,#87924,
#87925,#87926,#87927,#87928,#87929,#87930,#87931,#87932,#87933,#87934,#87935,
#87936,#87937,#87938,#87939,#87940,#87941,#87942,#87943,#87944,#87945,#87946,
#87947,#87948,#87949,#87950,#87951,#87952,#87953,#87954,#87955,#87956,#87957,
#87958,#87959,#87960,#87961,#87962,#87963,#87964,#87965,#87966,#87967,#87968,
#87969,#87970,#87971,#87972,#87973,#87974,#87975,#87976,#87977,#87978,#87979,
#87980,#87981,#87982,#87983,#87984,#87985,#87986),.UNSPECIFIED.,.F.,.F.,
(4,3,3,3,3,3,3,3,3,3,3,3,3,3,3,3,3,3,3,3,3,3,4),(15.7079632679489,15.851771437641,
15.9558439816741,16.0597596364386,16.1635513569498,16.2672765065998,16.3709700377575,
16.4746668582794,16.5784719990463,16.6823355986529,16.7863818407608,16.8493192959871,
16.9535243585492,17.0575742080196,17.1615019650239,17.2653642163339,17.3691957122932,
17.4730311597456,17.5769749880005,17.6809775212887,17.785161578003,17.8468671543332,
17.9343899947098),.UNSPECIFIED.);
#2580=B_SPLINE_CURVE_WITH_KNOTS('',3,(#87992,#87993,#87994,#87995,#87996,
#87997,#87998,#87999),.UNSPECIFIED.,.F.,.F.,(4,1,1,1,1,4),(99.6151588600969,
99.6457915387123,100.643339397058,101.640887255404,102.638435113751,103.635982972097),
 .UNSPECIFIED.);
#2581=B_SPLINE_CURVE_WITH_KNOTS('',3,(#88003,#88004,#88005,#88006,#88007,
#88008,#88009,#88010,#88011,#88012,#88013,#88014,#88015,#88016,#88017,#88018),
 .UNSPECIFIED.,.F.,.F.,(4,3,3,3,3,4),(103.672557568922,103.78037580106,
103.888462090901,103.99669403761,104.105203098963,104.157845063177),
 .UNSPECIFIED.);
#2582=B_SPLINE_CURVE_WITH_KNOTS('',3,(#88019,#88020,#88021,#88022,#88023,
#88024,#88025,#88026,#88027,#88028,#88029,#88030,#88031,#88032,#88033,#88034,
#88035,#88036,#88037,#88038,#88039,#88040,#88041,#88042,#88043,#88044,#88045,
#88046,#88047,#88048,#88049,#88050,#88051,#88052,#88053,#88054,#88055,#88056,
#88057,#88058,#88059,#88060,#88061,#88062,#88063,#88064,#88065,#88066,#88067,
#88068,#88069,#88070,#88071,#88072,#88073,#88074,#88075,#88076,#88077,#88078,
#88079,#88080,#88081,#88082,#88083,#88084,#88085,#88086,#88087,#88088,#88089,
#88090,#88091,#88092,#88093,#88094,#88095,#88096,#88097,#88098,#88099,#88100,
#88101,#88102,#88103,#88104,#88105,#88106,#88107,#88108,#88109,#88110,#88111,
#88112,#88113,#88114,#88115,#88116,#88117,#88118,#88119,#88120,#88121,#88122,
#88123,#88124,#88125,#88126,#88127,#88128,#88129,#88130,#88131,#88132,#88133,
#88134,#88135,#88136,#88137,#88138,#88139,#88140,#88141,#88142),
 .UNSPECIFIED.,.F.,.F.,(4,3,3,3,3,3,3,3,3,3,3,3,3,3,3,3,3,3,3,3,3,3,3,3,
3,3,3,3,3,3,3,3,3,3,3,3,3,3,3,3,3,4),(99.6156256169323,99.7194574413302,
99.8232964128399,99.9272456628453,100.031256493114,100.135445708004,100.18725683054,
100.291460632875,100.395509495336,100.499436674714,100.603298601299,100.707130025082,
100.810965652815,100.914910044679,101.018913358671,101.123098530321,101.184804688886,
101.288871352726,101.392782473111,101.49657167515,101.600295550718,101.703989049953,
101.807687079777,101.911495314534,102.015363074771,102.119415120688,102.182352547233,
102.286727546173,102.39094680336,102.495042376685,102.59907136604,102.703068280569,
102.807067584658,102.911171777178,103.015332937334,103.11967118475,103.179900405579,
103.289277016351,103.398344121045,103.507224154213,103.615874635127,103.672557568463),
 .UNSPECIFIED.);
#2583=B_SPLINE_CURVE_WITH_KNOTS('',3,(#88148,#88149,#88150,#88151,#88152,
#88153,#88154,#88155,#88156,#88157,#88158,#88159,#88160,#88161,#88162,#88163,
#88164,#88165,#88166,#88167,#88168,#88169,#88170,#88171,#88172,#88173,#88174,
#88175,#88176,#88177,#88178,#88179,#88180,#88181,#88182,#88183,#88184,#88185,
#88186,#88187,#88188,#88189,#88190,#88191,#88192,#88193,#88194,#88195,#88196,
#88197,#88198,#88199,#88200,#88201,#88202,#88203,#88204,#88205,#88206,#88207,
#88208,#88209,#88210,#88211,#88212,#88213,#88214,#88215,#88216,#88217,#88218,
#88219,#88220,#88221,#88222,#88223,#88224,#88225,#88226,#88227,#88228,#88229,
#88230,#88231,#88232,#88233,#88234,#88235,#88236,#88237,#88238,#88239,#88240,
#88241,#88242,#88243,#88244,#88245,#88246,#88247,#88248,#88249,#88250,#88251,
#88252,#88253,#88254,#88255,#88256,#88257,#88258,#88259,#88260,#88261,#88262,
#88263,#88264,#88265,#88266,#88267,#88268,#88269,#88270,#88271,#88272,#88273,
#88274),.UNSPECIFIED.,.F.,.F.,(4,3,3,3,3,3,3,3,3,3,3,3,3,3,3,3,3,3,3,3,
3,3,3,3,3,3,3,3,3,3,3,3,3,3,3,3,3,3,3,3,3,3,4),(93.3317490905774,93.435694332417,
93.5397120172538,93.6438984400441,93.6605043886358,93.7646927380818,93.8687258362982,
93.9726368703958,94.0764824260428,94.180297279391,94.284116163135,94.3880436655015,
94.4920299826526,94.596198175621,94.6580522469818,94.7622418091092,94.8662761707485,
94.9701885366066,95.0740354653412,95.1778517307116,95.2816720630607,95.3856010591389,
95.489588897669,95.5937586386179,95.6556001053279,95.7597703757183,95.8637853776279,
95.9676783761358,96.0715059432305,96.1753028809778,96.2791039480478,96.3830139060965,
96.4869828059679,96.5911339707109,96.653147963674,96.7562487155586,96.8592080959374,
96.9620624807666,97.0688899258958,97.1716683720447,97.2744473600228,97.3772955657622,
97.3893722612836),.UNSPECIFIED.);
#2584=B_SPLINE_CURVE_WITH_KNOTS('',3,(#88275,#88276,#88277,#88278,#88279,
#88280),.UNSPECIFIED.,.F.,.F.,(4,1,1,4),(97.3893748528935,97.6506958220201,
98.6482436803662,99.6151588600969),.UNSPECIFIED.);
#2585=B_SPLINE_CURVE_WITH_KNOTS('',3,(#88282,#88283,#88284,#88285,#88286,
#88287,#88288,#88289,#88290,#88291,#88292,#88293,#88294,#88295,#88296,#88297,
#88298,#88299,#88300,#88301,#88302,#88303,#88304,#88305,#88306,#88307,#88308,
#88309,#88310,#88311,#88312,#88313,#88314,#88315,#88316,#88317,#88318,#88319,
#88320,#88321,#88322,#88323,#88324,#88325,#88326,#88327,#88328,#88329,#88330,
#88331,#88332,#88333,#88334,#88335,#88336,#88337,#88338,#88339,#88340,#88341,
#88342,#88343,#88344,#88345,#88346,#88347,#88348),.UNSPECIFIED.,.F.,.F.,
(4,3,3,3,3,3,3,3,3,3,3,3,3,3,3,3,3,3,3,3,3,3,4),(97.3893722616736,97.4918529942681,
97.5942444189893,97.6965831997679,97.7989059241202,97.9013194553043,98.0037772003265,
98.1064188744439,98.1921611138482,98.296331412984,98.4003464436805,98.5042394709017,
98.6080670666496,98.711864032949,98.8156651284298,98.9195751144808,99.0235440421667,
99.1276952341283,99.1897089721943,99.2961881333788,99.4002221458023,99.5079238813673,
99.6156256169323),.UNSPECIFIED.);
#2586=B_SPLINE_CURVE_WITH_KNOTS('',3,(#88349,#88350,#88351,#88352,#88353,
#88354,#88355,#88356,#88357,#88358,#88359,#88360,#88361,#88362,#88363,#88364,
#88365,#88366,#88367,#88368,#88369,#88370,#88371,#88372,#88373,#88374,#88375,
#88376,#88377,#88378,#88379,#88380,#88381,#88382,#88383,#88384,#88385,#88386,
#88387,#88388,#88389,#88390,#88391,#88392,#88393,#88394,#88395,#88396,#88397,
#88398,#88399,#88400,#88401,#88402,#88403,#88404,#88405,#88406,#88407,#88408,
#88409,#88410,#88411,#88412,#88413,#88414,#88415,#88416,#88417,#88418,#88419,
#88420,#88421,#88422,#88423,#88424,#88425,#88426,#88427,#88428,#88429,#88430,
#88431,#88432,#88433,#88434,#88435,#88436,#88437,#88438,#88439,#88440,#88441,
#88442,#88443,#88444,#88445,#88446,#88447,#88448,#88449,#88450,#88451,#88452,
#88453,#88454,#88455,#88456,#88457,#88458,#88459,#88460,#88461,#88462,#88463,
#88464,#88465,#88466,#88467,#88468,#88469,#88470,#88471,#88472),
 .UNSPECIFIED.,.F.,.F.,(4,3,3,3,3,3,3,3,3,3,3,3,3,3,3,3,3,3,3,3,3,3,3,3,
3,3,3,3,3,3,3,3,3,3,3,3,3,3,3,3,3,4),(93.3327290514497,93.4413841300764,
93.5452716396415,93.6491033120159,93.7529139105045,93.8567381646366,93.9606769722411,
94.0646832476024,94.1688628859985,94.2019696804638,94.3061564133321,94.410187912589,
94.5140973811542,94.6179413926832,94.7217547253996,94.8255721140933,94.9294981703152,
95.0334830667106,95.1376498941375,95.1995175388099,95.3037016465712,95.4077305135391,
95.5116373518152,95.615478735705,95.7192894472635,95.8231042251162,95.9270277041183,
96.0310100383646,96.1351743552147,96.197065397156,96.3012537439254,96.4052868394961,
96.509197871006,96.6130434241022,96.71685827494,96.8206771562169,96.9246046561991,
97.0285909710088,97.1327591617284,97.1946132555021,97.345602266741,97.3893722612836),
 .UNSPECIFIED.);
#2587=B_SPLINE_CURVE_WITH_KNOTS('',3,(#88478,#88479,#88480,#88481,#88482,
#88483,#88484,#88485,#88486,#88487,#88488,#88489,#88490,#88491,#88492,#88493,
#88494,#88495,#88496,#88497,#88498,#88499,#88500,#88501,#88502,#88503,#88504,
#88505,#88506,#88507,#88508,#88509,#88510,#88511,#88512,#88513,#88514,#88515,
#88516,#88517,#88518,#88519,#88520,#88521,#88522,#88523,#88524,#88525,#88526,
#88527,#88528,#88529,#88530,#88531,#88532,#88533,#88534,#88535,#88536,#88537,
#88538,#88539,#88540,#88541,#88542,#88543,#88544,#88545,#88546,#88547,#88548,
#88549,#88550,#88551,#88552,#88553,#88554,#88555,#88556,#88557,#88558,#88559,
#88560,#88561,#88562,#88563,#88564,#88565,#88566,#88567,#88568,#88569,#88570,
#88571,#88572,#88573,#88574,#88575,#88576,#88577,#88578,#88579,#88580,#88581,
#88582,#88583,#88584,#88585,#88586,#88587,#88588,#88589,#88590,#88591,#88592,
#88593,#88594,#88595,#88596,#88597,#88598),.UNSPECIFIED.,.F.,.F.,(4,3,3,
3,3,3,3,3,3,3,3,3,3,3,3,3,3,3,3,3,3,3,3,3,3,3,3,3,3,3,3,3,3,3,3,3,3,3,3,
3,4),(87.0493974468485,87.1532189896668,87.2570297906175,87.3615766526029,
87.4655324459015,87.5703748422304,87.6752172385592,87.7794034197809,87.8834343624533,
87.9873432698471,88.0911867176855,88.1949994850426,88.2988163075558,88.4027418002793,
88.5067261338403,88.6108924056251,88.6727650969053,88.7769513494554,88.8809823642944,
88.9848913447398,89.0887348661345,89.1925477074401,89.2963646041826,89.4002901710438,
89.5042745788026,89.6084409240676,89.6703129552514,89.7744988575247,89.8785295213807,
89.9824381514785,90.0862813231058,90.1900938157322,90.2939103653924,90.3978355899808,
90.5018196576624,90.6059856700009,90.6678608135975,90.7807059016893,90.8932651237372,
91.005365280633,91.106186953809),.UNSPECIFIED.);
#2588=B_SPLINE_CURVE_WITH_KNOTS('',3,(#88599,#88600,#88601,#88602,#88603,
#88604,#88605,#88606,#88607,#88608,#88609,#88610,#88611,#88612,#88613,#88614,
#88615,#88616,#88617,#88618,#88619,#88620,#88621,#88622,#88623,#88624,#88625,
#88626,#88627,#88628,#88629,#88630,#88631,#88632,#88633,#88634,#88635,#88636,
#88637,#88638,#88639,#88640,#88641,#88642,#88643,#88644,#88645,#88646,#88647,
#88648,#88649,#88650,#88651,#88652,#88653,#88654,#88655,#88656,#88657,#88658,
#88659,#88660,#88661,#88662,#88663,#88664,#88665,#88666,#88667,#88668),
 .UNSPECIFIED.,.F.,.F.,(4,3,3,3,3,3,3,3,3,3,3,3,3,3,3,3,3,3,3,3,3,3,3,4),
(91.106186954104,91.2125697194757,91.3190337387694,91.4256926623267,91.5324645374607,
91.6394564150643,91.6654086719436,91.76959540681,91.8736269080771,91.9775363786608,
92.0813803922122,92.1851937269521,92.2890111176673,92.3929371758939,92.4969220742875,
92.6010889036804,92.6629565302897,92.7671202567895,92.8711391118278,92.9750481127459,
93.078891237982,93.1826959263191,93.2865260562585,93.3317490905774),
 .UNSPECIFIED.);
#2589=B_SPLINE_CURVE_WITH_KNOTS('',3,(#88670,#88671,#88672,#88673,#88674,
#88675,#88676,#88677,#88678,#88679,#88680,#88681,#88682,#88683,#88684,#88685,
#88686,#88687,#88688,#88689,#88690,#88691,#88692,#88693,#88694,#88695,#88696,
#88697,#88698,#88699,#88700,#88701,#88702,#88703,#88704,#88705,#88706,#88707,
#88708,#88709,#88710,#88711,#88712,#88713,#88714,#88715,#88716,#88717,#88718,
#88719,#88720,#88721,#88722,#88723,#88724,#88725,#88726,#88727,#88728,#88729,
#88730,#88731,#88732,#88733,#88734,#88735,#88736,#88737,#88738,#88739),
 .UNSPECIFIED.,.F.,.F.,(4,3,3,3,3,3,3,3,3,3,3,3,3,3,3,3,3,3,3,3,3,3,3,4),
(91.106186954104,91.2093261054256,91.3135123576276,91.4175433721169,91.5214523522112,
91.6252958732545,91.7291087142088,91.8329256106003,91.9368511771141,92.0408355845268,
92.1450019294517,92.2068739637717,92.3110598668121,92.4150905314355,92.5189991622972,
92.6228423346862,92.7266548280707,92.8304713784842,92.9343966038141,93.0383806722314,
93.1425466852886,93.2044218221177,93.3086062151315,93.3327290514497),
 .UNSPECIFIED.);
#2590=B_SPLINE_CURVE_WITH_KNOTS('',3,(#88740,#88741,#88742,#88743,#88744,
#88745,#88746,#88747,#88748,#88749,#88750,#88751,#88752,#88753,#88754,#88755,
#88756,#88757,#88758,#88759,#88760,#88761,#88762,#88763,#88764,#88765,#88766,
#88767,#88768,#88769,#88770,#88771,#88772,#88773,#88774,#88775,#88776,#88777,
#88778,#88779,#88780,#88781,#88782,#88783,#88784,#88785,#88786,#88787,#88788,
#88789,#88790,#88791,#88792,#88793,#88794,#88795,#88796,#88797,#88798,#88799,
#88800,#88801,#88802,#88803,#88804,#88805,#88806,#88807,#88808,#88809,#88810,
#88811,#88812,#88813,#88814,#88815,#88816,#88817,#88818,#88819,#88820,#88821,
#88822,#88823,#88824,#88825,#88826,#88827,#88828,#88829,#88830,#88831,#88832,
#88833,#88834,#88835,#88836,#88837,#88838,#88839,#88840,#88841,#88842,#88843,
#88844,#88845,#88846,#88847,#88848,#88849,#88850,#88851,#88852,#88853,#88854,
#88855,#88856,#88857,#88858,#88859,#88860,#88861,#88862,#88863),
 .UNSPECIFIED.,.F.,.F.,(4,3,3,3,3,3,3,3,3,3,3,3,3,3,3,3,3,3,3,3,3,3,3,3,
3,3,3,3,3,3,3,3,3,3,3,3,3,3,3,3,3,4),(87.0484536587393,87.1526180566811,
87.2191346720412,87.3233208365446,87.4273517627344,87.5312606540692,87.6351040861179,
87.7389168379752,87.8427336452998,87.9466591234087,88.0506434426566,88.154809700756,
88.2166825303873,88.3208687070139,88.4248996454306,88.5288085490861,88.6326519935066,
88.7364647577682,88.840281577511,88.9442070679729,89.0481913995558,89.1523576698271,
89.2142303887334,89.3184165199705,89.4224474129372,89.5263562712705,89.6301996704719,
89.7340123896828,89.8378291646089,89.9417546109172,90.0457388986538,90.1499051260383,
90.2117782470795,90.3146405386673,90.4173275777108,90.5199168635336,90.6224449018284,
90.7249481125111,90.8275243328762,90.9301371296558,91.0329110106376,91.1061869536468),
 .UNSPECIFIED.);
#2591=B_SPLINE_CURVE_WITH_KNOTS('',3,(#88869,#88870,#88871,#88872,#88873,
#88874,#88875,#88876,#88877,#88878,#88879,#88880,#88881,#88882,#88883,#88884,
#88885,#88886,#88887,#88888,#88889,#88890,#88891,#88892,#88893,#88894,#88895,
#88896,#88897,#88898,#88899,#88900,#88901,#88902,#88903,#88904,#88905,#88906,
#88907,#88908,#88909,#88910,#88911,#88912,#88913,#88914,#88915,#88916,#88917,
#88918,#88919,#88920,#88921,#88922,#88923,#88924,#88925,#88926,#88927,#88928,
#88929,#88930,#88931,#88932,#88933,#88934,#88935,#88936,#88937,#88938,#88939,
#88940,#88941,#88942,#88943,#88944,#88945,#88946,#88947,#88948,#88949,#88950,
#88951,#88952,#88953,#88954,#88955,#88956,#88957,#88958,#88959,#88960,#88961,
#88962,#88963,#88964,#88965,#88966,#88967,#88968,#88969,#88970,#88971,#88972,
#88973,#88974,#88975,#88976,#88977,#88978,#88979,#88980,#88981,#88982,#88983,
#88984,#88985,#88986,#88987,#88988,#88989),.UNSPECIFIED.,.F.,.F.,(4,3,3,
3,3,3,3,3,3,3,3,3,3,3,3,3,3,3,3,3,3,3,3,3,3,3,3,3,3,3,3,3,3,3,3,3,3,3,3,
3,4),(80.7662049656111,80.8702771562758,80.9742116984674,81.0780706249186,
81.181888734009,81.2857007704572,81.3896149728771,81.4935789190852,81.5977344389464,
81.6899300884827,81.7941162519362,81.8981471771086,82.0020560674785,82.1058994985952,
82.2097122495543,82.3135290560159,82.4174545333203,82.5214388517957,82.6256051091809,
82.6874779468288,82.7916641121998,82.8956950393023,82.9996039316116,83.1034473646724,
83.2072601175775,83.3110769259838,83.4150024052179,83.5189867256173,83.6231529848968,
83.6850258051749,83.7892119647504,83.8932428860536,83.9971517725858,84.100995199886,
84.2048079470555,84.3086247497596,84.4125502233813,84.5165345382103,84.6207007920462,
84.682573663521,84.8230016469244),.UNSPECIFIED.);
#2592=B_SPLINE_CURVE_WITH_KNOTS('',3,(#88990,#88991,#88992,#88993,#88994,
#88995,#88996,#88997,#88998,#88999,#89000,#89001,#89002,#89003,#89004,#89005,
#89006,#89007,#89008,#89009,#89010,#89011,#89012,#89013,#89014,#89015,#89016,
#89017,#89018,#89019,#89020,#89021,#89022,#89023,#89024,#89025,#89026,#89027,
#89028,#89029,#89030,#89031,#89032,#89033,#89034,#89035,#89036,#89037,#89038,
#89039,#89040,#89041,#89042,#89043,#89044,#89045,#89046,#89047,#89048,#89049,
#89050,#89051,#89052,#89053,#89054,#89055,#89056,#89057,#89058,#89059),
 .UNSPECIFIED.,.F.,.F.,(4,3,3,3,3,3,3,3,3,3,3,3,3,3,3,3,3,3,3,3,3,3,3,4),
(84.8230016473325,84.9301416316494,85.0325714156815,85.1349307967517,85.2372563938986,
85.3395847740774,85.4420166327704,85.5445096289043,85.6471710508368,85.6801215218671,
85.7843076985516,85.8883386370265,85.9922475407404,86.0960909852193,86.1999037495391,
86.3037205693399,86.4076460598594,86.5116303914995,86.6157966618271,86.6776693802132,
86.7818282135815,86.8858513273734,86.9897581895063,87.0493974468485),
 .UNSPECIFIED.);
#2593=B_SPLINE_CURVE_WITH_KNOTS('',3,(#89061,#89062,#89063,#89064,#89065,
#89066,#89067,#89068,#89069,#89070,#89071,#89072,#89073,#89074,#89075,#89076,
#89077,#89078,#89079,#89080,#89081,#89082,#89083,#89084,#89085,#89086,#89087,
#89088,#89089,#89090,#89091,#89092,#89093,#89094,#89095,#89096,#89097,#89098,
#89099,#89100,#89101,#89102,#89103,#89104,#89105,#89106,#89107,#89108,#89109,
#89110,#89111,#89112,#89113,#89114,#89115,#89116,#89117,#89118,#89119,#89120,
#89121,#89122,#89123,#89124,#89125,#89126,#89127),.UNSPECIFIED.,.F.,.F.,
(4,3,3,3,3,3,3,3,3,3,3,3,3,3,3,3,3,3,3,3,3,3,4),(84.8230016473381,84.9376554433282,
85.0527190367408,85.1683359261865,85.224038955349,85.3282251207107,85.4322560478039,
85.536164940104,85.6400083731555,85.7438211260512,85.8476379344483,85.9515634136733,
86.0555477340635,86.1597139933341,86.2215868136951,86.3257394075604,86.4297517315574,
86.5336587783306,86.6374954176148,86.7413356684352,86.8451704367688,86.9491112664109,
87.0484536587393),.UNSPECIFIED.);
#2594=B_SPLINE_CURVE_WITH_KNOTS('',3,(#89128,#89129,#89130,#89131,#89132,
#89133,#89134,#89135,#89136,#89137,#89138,#89139,#89140,#89141,#89142,#89143,
#89144,#89145,#89146,#89147,#89148,#89149,#89150,#89151,#89152,#89153,#89154,
#89155,#89156,#89157,#89158,#89159,#89160,#89161,#89162,#89163,#89164,#89165,
#89166,#89167,#89168,#89169,#89170,#89171,#89172,#89173,#89174,#89175,#89176,
#89177,#89178,#89179,#89180,#89181,#89182,#89183,#89184,#89185,#89186,#89187,
#89188,#89189,#89190,#89191,#89192,#89193,#89194,#89195,#89196,#89197,#89198,
#89199,#89200,#89201,#89202,#89203,#89204,#89205,#89206,#89207,#89208,#89209,
#89210,#89211,#89212,#89213,#89214,#89215,#89216,#89217,#89218,#89219,#89220,
#89221,#89222,#89223,#89224,#89225,#89226,#89227,#89228,#89229,#89230,#89231,
#89232,#89233,#89234,#89235,#89236,#89237,#89238,#89239,#89240,#89241,#89242,
#89243,#89244,#89245,#89246,#89247,#89248,#89249,#89250,#89251),
 .UNSPECIFIED.,.F.,.F.,(4,3,3,3,3,3,3,3,3,3,3,3,3,3,3,3,3,3,3,3,3,3,3,3,
3,3,3,3,3,3,3,3,3,3,3,3,3,3,3,3,3,4),(80.7657498498246,80.8695688015658,
80.9734984375536,81.0774898205032,81.1816601949338,81.2338475219647,81.3380336854276,
81.4420646106138,81.545973501004,81.6498169321448,81.7536296831319,81.8574464896251,
81.9613719669668,82.0653562854825,82.1695225429127,82.2313953803108,82.3355815440582,
82.4396124695303,82.5435213602072,82.6473647916352,82.7511775429095,82.8549943496892,
82.9589198273146,83.0629041461133,83.1670704038213,83.2289432386569,83.3331294016869,
83.4371603264421,83.5410692164054,83.6449126471221,83.7487253976887,83.8525422037659,
83.9564676807001,84.0604519988128,84.1646182558513,84.226491097003,84.3322636670979,
84.4378652907398,84.5433026053224,84.6486432054657,84.7539210457329,84.8230016469244),
 .UNSPECIFIED.);
#2595=B_SPLINE_CURVE_WITH_KNOTS('',3,(#89257,#89258,#89259,#89260,#89261,
#89262,#89263,#89264,#89265,#89266,#89267,#89268,#89269,#89270,#89271,#89272,
#89273,#89274,#89275,#89276,#89277,#89278,#89279,#89280,#89281,#89282,#89283,
#89284,#89285,#89286,#89287,#89288,#89289,#89290,#89291,#89292,#89293,#89294,
#89295,#89296,#89297,#89298,#89299,#89300,#89301,#89302,#89303,#89304,#89305,
#89306,#89307,#89308,#89309,#89310,#89311,#89312,#89313,#89314,#89315,#89316,
#89317,#89318,#89319,#89320,#89321,#89322,#89323,#89324,#89325,#89326,#89327,
#89328,#89329,#89330,#89331,#89332,#89333,#89334,#89335,#89336,#89337,#89338,
#89339,#89340,#89341,#89342,#89343,#89344,#89345,#89346,#89347,#89348,#89349,
#89350,#89351,#89352,#89353,#89354,#89355,#89356,#89357,#89358,#89359,#89360,
#89361,#89362,#89363,#89364,#89365,#89366,#89367,#89368,#89369,#89370,#89371,
#89372,#89373,#89374,#89375,#89376,#89377,#89378,#89379,#89380,#89381,#89382,
#89383),.UNSPECIFIED.,.F.,.F.,(4,3,3,3,3,3,3,3,3,3,3,3,3,3,3,3,3,3,3,3,
3,3,3,3,3,3,3,3,3,3,3,3,3,3,3,3,3,3,3,3,3,3,4),(74.4820670752277,74.5860865447775,
74.6902747768549,74.7070950800601,74.8112812435426,74.9153121687491,75.0192210591604,
75.123064490323,75.2268772413324,75.3306940478485,75.4346195252135,75.538603843753,
75.6427701012072,75.7046429384062,75.8088291018885,75.9128600270946,76.0167689175055,
76.1206123486675,76.2244250996762,76.3282419061915,76.4321673835557,76.5361517020941,
76.6403179595472,76.7021907967523,76.8063769602756,76.9104078855229,77.0143167759751,
77.1181602071783,77.2219729582282,77.3257897647846,77.4297152421894,77.5336995607683,
77.6378658182611,77.6997386550984,77.8047483656351,77.9072108121553,78.0095758369094,
78.1118801626899,78.2188642068654,78.3212057259318,78.4235870712412,78.5260937325057,
78.5398163393917),.UNSPECIFIED.);
#2596=B_SPLINE_CURVE_WITH_KNOTS('',3,(#89384,#89385,#89386,#89387,#89388,
#89389,#89390,#89391,#89392,#89393,#89394,#89395,#89396,#89397,#89398,#89399,
#89400,#89401,#89402,#89403,#89404,#89405,#89406,#89407,#89408,#89409,#89410,
#89411,#89412,#89413,#89414,#89415,#89416,#89417,#89418,#89419,#89420,#89421,
#89422,#89423,#89424,#89425,#89426,#89427,#89428,#89429,#89430,#89431,#89432,
#89433,#89434,#89435,#89436,#89437,#89438,#89439,#89440,#89441,#89442,#89443,
#89444,#89445,#89446,#89447,#89448,#89449,#89450),.UNSPECIFIED.,.F.,.F.,
(4,3,3,3,3,3,3,3,3,3,3,3,3,3,3,3,3,3,3,3,3,3,4),(78.5398163397448,78.6972865134445,
78.8014726769072,78.9055036020932,79.0094124924832,79.1132559236238,79.2170686746107,
79.3208854811037,79.4248109584452,79.5287952769607,79.6329615343907,79.6948343717906,
79.7990205355393,79.9030514610129,80.0069603516911,80.1108037831204,80.214616534396,
80.3184333411772,80.4223588188041,80.5263431376039,80.6305093953132,80.6923822301366,
80.7662049656111),.UNSPECIFIED.);
#2597=B_SPLINE_CURVE_WITH_KNOTS('',3,(#89452,#89453,#89454,#89455,#89456,
#89457,#89458,#89459,#89460,#89461,#89462,#89463,#89464,#89465,#89466,#89467,
#89468,#89469,#89470,#89471,#89472,#89473,#89474,#89475,#89476,#89477,#89478,
#89479,#89480,#89481,#89482,#89483,#89484,#89485,#89486,#89487,#89488,#89489,
#89490,#89491,#89492,#89493,#89494,#89495,#89496,#89497,#89498,#89499,#89500,
#89501,#89502,#89503,#89504,#89505,#89506,#89507,#89508,#89509,#89510,#89511,
#89512,#89513,#89514,#89515,#89516,#89517,#89518),.UNSPECIFIED.,.F.,.F.,
(4,3,3,3,3,3,3,3,3,3,3,3,3,3,3,3,3,3,3,3,3,3,4),(78.5398163397448,78.6430480181452,
78.7462408135878,78.8494302890941,78.9527248465251,79.0560730499683,79.1596112159242,
79.2387518052725,79.3429379687955,79.4469688940425,79.5508777844944,79.6547212156974,
79.7585339667471,79.8623507733033,79.9662762507079,80.0702605692866,80.1744268267791,
80.2362996636186,80.3404816764144,80.4467987197669,80.5507037015718,80.6582267756982,
80.7657498498246),.UNSPECIFIED.);
#2598=B_SPLINE_CURVE_WITH_KNOTS('',3,(#89519,#89520,#89521,#89522,#89523,
#89524,#89525,#89526,#89527,#89528,#89529,#89530,#89531,#89532,#89533,#89534,
#89535,#89536,#89537,#89538,#89539,#89540,#89541,#89542,#89543,#89544,#89545,
#89546,#89547,#89548,#89549,#89550,#89551,#89552,#89553,#89554,#89555,#89556,
#89557,#89558,#89559,#89560,#89561,#89562,#89563,#89564,#89565,#89566,#89567,
#89568,#89569,#89570,#89571,#89572,#89573,#89574,#89575,#89576,#89577,#89578,
#89579,#89580,#89581,#89582,#89583,#89584,#89585,#89586,#89587,#89588,#89589,
#89590,#89591,#89592,#89593,#89594,#89595,#89596,#89597,#89598,#89599,#89600,
#89601,#89602,#89603,#89604,#89605,#89606,#89607,#89608,#89609,#89610,#89611,
#89612,#89613,#89614,#89615,#89616,#89617,#89618,#89619,#89620,#89621,#89622,
#89623,#89624,#89625,#89626,#89627,#89628,#89629,#89630,#89631,#89632,#89633,
#89634,#89635,#89636,#89637,#89638,#89639,#89640,#89641,#89642),
 .UNSPECIFIED.,.F.,.F.,(4,3,3,3,3,3,3,3,3,3,3,3,3,3,3,3,3,3,3,3,3,3,3,3,
3,3,3,3,3,3,3,3,3,3,3,3,3,3,3,3,3,4),(74.4832485089442,74.5871391796787,
74.6909724336135,74.7947830366967,74.8986057195159,75.0025420121103,75.1065443563955,
75.2107214413106,75.2485603718882,75.3527465353754,75.4567774605866,75.5606863510025,
75.6645297821696,75.7683425331833,75.8721593397041,75.9760848170734,76.0800691356172,
76.1842353930753,76.2461082302343,76.350294393727,76.4543253189437,76.5582342093654,
76.662077640538,76.7658903915576,76.8697071980835,76.9736326754583,77.0776169940075,
77.1817832514711,77.2436560885804,77.3478422520629,77.4518731772695,77.5557820676809,
77.6596254988434,77.7634382498528,77.867255056369,77.9711805337341,78.0751648522737,
78.1793311097278,78.2412039469264,78.3682032551961,78.4934616304905,78.5398163394136),
 .UNSPECIFIED.);
#2599=B_SPLINE_CURVE_WITH_KNOTS('',3,(#89648,#89649,#89650,#89651,#89652,
#89653,#89654,#89655,#89656,#89657,#89658,#89659,#89660,#89661,#89662,#89663,
#89664,#89665,#89666,#89667,#89668,#89669,#89670,#89671,#89672,#89673,#89674,
#89675,#89676,#89677,#89678,#89679,#89680,#89681,#89682,#89683,#89684,#89685,
#89686,#89687,#89688,#89689,#89690,#89691,#89692,#89693,#89694,#89695,#89696,
#89697,#89698,#89699,#89700,#89701,#89702,#89703,#89704,#89705,#89706,#89707,
#89708,#89709,#89710,#89711,#89712,#89713,#89714,#89715,#89716,#89717,#89718,
#89719,#89720,#89721,#89722,#89723,#89724,#89725,#89726,#89727,#89728,#89729,
#89730,#89731,#89732,#89733,#89734,#89735,#89736,#89737,#89738,#89739,#89740,
#89741,#89742,#89743,#89744,#89745,#89746,#89747,#89748,#89749,#89750,#89751,
#89752,#89753,#89754,#89755,#89756,#89757,#89758,#89759,#89760,#89761,#89762,
#89763,#89764,#89765,#89766,#89767,#89768),.UNSPECIFIED.,.F.,.F.,(4,3,3,
3,3,3,3,3,3,3,3,3,3,3,3,3,3,3,3,3,3,3,3,3,3,3,3,3,3,3,3,3,3,3,3,3,3,3,3,
3,4),(68.1995463580489,68.3033571741053,68.4079698630748,68.5119255707606,
68.6168667503721,68.7218079299836,68.8259940934717,68.930025018684,69.0339339091009,
69.1377773402689,69.2415900912839,69.3454068978052,69.4493323751755,69.5533166937202,
69.6574829511794,69.7193557883297,69.8235419518177,69.9275728770295,70.0314817674464,
70.1353251986144,70.239137949629,70.34295475615,70.4468802335202,70.550864552065,
70.6550308095241,70.7169036466758,70.8210898101646,70.9251207353769,71.0290296257945,
71.1328730569633,71.2366858079789,71.3405026145007,71.4444280918716,71.5484124104166,
71.6525786678764,71.7144515050219,71.8220784528937,71.9307165978116,72.0379272940085,
72.1472791632869,72.2566310325652),.UNSPECIFIED.);
#2600=B_SPLINE_CURVE_WITH_KNOTS('',3,(#89769,#89770,#89771,#89772,#89773,
#89774,#89775,#89776,#89777,#89778,#89779,#89780,#89781,#89782,#89783,#89784,
#89785,#89786,#89787,#89788,#89789,#89790,#89791,#89792,#89793,#89794,#89795,
#89796,#89797,#89798,#89799,#89800,#89801,#89802,#89803,#89804,#89805,#89806,
#89807,#89808,#89809,#89810,#89811,#89812,#89813,#89814,#89815,#89816,#89817,
#89818,#89819,#89820,#89821,#89822,#89823,#89824,#89825,#89826,#89827,#89828,
#89829,#89830,#89831,#89832,#89833,#89834,#89835),.UNSPECIFIED.,.F.,.F.,
(4,3,3,3,3,3,3,3,3,3,3,3,3,3,3,3,3,3,3,3,3,3,4),(72.2566310330055,72.3704731155961,
72.4818133112497,72.5969063373088,72.7119993633679,72.816185526855,72.9202164520661,
73.024125342482,73.127968773649,73.2317815246628,73.3355983311831,73.4395238085524,
73.543508127096,73.6476743845542,73.709547221714,73.8137037279885,73.9177183838715,
74.021626189055,74.1254620178865,74.2292882438049,74.3331083624566,74.4370016475404,
74.4820670752277),.UNSPECIFIED.);
#2601=B_SPLINE_CURVE_WITH_KNOTS('',3,(#89837,#89838,#89839,#89840,#89841,
#89842,#89843,#89844,#89845,#89846,#89847,#89848,#89849,#89850,#89851,#89852,
#89853,#89854,#89855,#89856,#89857,#89858,#89859,#89860,#89861,#89862,#89863,
#89864,#89865,#89866,#89867,#89868,#89869,#89870,#89871,#89872,#89873,#89874,
#89875,#89876,#89877,#89878,#89879,#89880,#89881,#89882,#89883,#89884,#89885,
#89886,#89887,#89888,#89889,#89890,#89891,#89892,#89893,#89894,#89895,#89896,
#89897,#89898,#89899,#89900,#89901,#89902,#89903,#89904,#89905,#89906),
 .UNSPECIFIED.,.F.,.F.,(4,3,3,3,3,3,3,3,3,3,3,3,3,3,3,3,3,3,3,3,3,3,3,4),
(72.2566310325652,72.3608036974116,72.4648211348936,72.5687165871306,72.6725466326848,
72.776346071062,72.8801496583905,72.9840619405011,73.0880331866153,73.1921861589884,
73.253464655196,73.3576508186849,73.4616817438977,73.5655906343152,73.6694340654839,
73.7732468164996,73.8770636230217,73.9809891003927,74.0849734189379,74.1891396763978,
74.2510125135421,74.3552035653614,74.459228530687,74.4832485089442),
 .UNSPECIFIED.);
#2602=B_SPLINE_CURVE_WITH_KNOTS('',3,(#89907,#89908,#89909,#89910,#89911,
#89912,#89913,#89914,#89915,#89916,#89917,#89918,#89919,#89920,#89921,#89922,
#89923,#89924,#89925,#89926,#89927,#89928,#89929,#89930,#89931,#89932,#89933,
#89934,#89935,#89936,#89937,#89938,#89939,#89940,#89941,#89942,#89943,#89944,
#89945,#89946,#89947,#89948,#89949,#89950,#89951,#89952,#89953,#89954,#89955,
#89956,#89957,#89958,#89959,#89960,#89961,#89962,#89963,#89964,#89965,#89966,
#89967,#89968,#89969,#89970,#89971,#89972,#89973,#89974,#89975,#89976,#89977,
#89978,#89979,#89980,#89981,#89982,#89983,#89984,#89985,#89986,#89987,#89988,
#89989,#89990,#89991,#89992,#89993,#89994,#89995,#89996,#89997,#89998,#89999,
#90000,#90001,#90002,#90003,#90004,#90005,#90006,#90007,#90008,#90009,#90010,
#90011,#90012,#90013,#90014,#90015,#90016,#90017,#90018,#90019,#90020,#90021,
#90022,#90023,#90024,#90025,#90026,#90027,#90028,#90029,#90030,#90031,#90032,
#90033),.UNSPECIFIED.,.F.,.F.,(4,3,3,3,3,3,3,3,3,3,3,3,3,3,3,3,3,3,3,3,
3,3,3,3,3,3,3,3,3,3,3,3,3,3,3,3,3,3,3,3,3,3,4),(68.1991405116964,68.2657253634656,
68.3699115269538,68.4739424521659,68.5778513425829,68.681694773751,68.785507524766,
68.8893243312875,68.9932498086579,69.0972341272026,69.2014003846619,69.2632732218117,
69.3674593852998,69.471490310512,69.5753992009289,69.679242632097,69.7830553831119,
69.8868721896334,69.9907976670037,70.0947819855484,70.1989482430077,70.2608210801577,
70.365007243646,70.4690381688582,70.5729470592752,70.6767904904434,70.7806032414584,
70.8844200479799,70.9883455253504,71.0923298438952,71.1964961013545,71.2583689385038,
71.3625551019919,71.4665860272041,71.570494917621,71.674338348789,71.7781510998039,
71.8819679063254,71.9858933836958,72.0898777022405,72.1940439596997,72.2559167968499,
72.2566310325397),.UNSPECIFIED.);
#2603=B_SPLINE_CURVE_WITH_KNOTS('',3,(#90039,#90040,#90041,#90042,#90043,
#90044,#90045,#90046,#90047,#90048,#90049,#90050,#90051,#90052,#90053,#90054,
#90055,#90056,#90057,#90058,#90059,#90060,#90061,#90062,#90063,#90064,#90065,
#90066,#90067,#90068,#90069,#90070,#90071,#90072,#90073,#90074,#90075,#90076,
#90077,#90078,#90079,#90080,#90081,#90082,#90083,#90084,#90085,#90086,#90087,
#90088,#90089,#90090,#90091,#90092,#90093,#90094,#90095,#90096,#90097,#90098,
#90099,#90100,#90101,#90102,#90103,#90104,#90105,#90106,#90107,#90108,#90109,
#90110,#90111,#90112,#90113,#90114,#90115,#90116,#90117,#90118,#90119,#90120,
#90121,#90122,#90123,#90124,#90125,#90126,#90127,#90128,#90129,#90130,#90131,
#90132,#90133,#90134,#90135,#90136,#90137,#90138,#90139,#90140,#90141,#90142,
#90143,#90144,#90145,#90146,#90147,#90148,#90149,#90150,#90151,#90152,#90153,
#90154,#90155,#90156,#90157,#90158,#90159),.UNSPECIFIED.,.F.,.F.,(4,3,3,
3,3,3,3,3,3,3,3,3,3,3,3,3,3,3,3,3,3,3,3,3,3,3,3,3,3,3,3,3,3,3,3,3,3,3,3,
3,4),(61.9168706242402,62.0208051644045,62.1246640897561,62.2284821986722,
62.3322942358697,62.4362084396395,62.540172388026,62.6443279091437,62.7365207799071,
62.8407069433953,62.9447378686074,63.0486467590244,63.1524901901925,63.2563029412074,
63.3601197477289,63.4640452250993,63.5680295436441,63.6721958011033,63.7340686382532,
63.8382548017414,63.9422857269536,64.0461946173705,64.1500380485386,64.2538507995535,
64.357667606075,64.4615930834454,64.5655774019901,64.6697436594494,64.7316164965992,
64.8358026600874,64.9398335852995,65.0437424757165,65.1475859068846,65.2513986578996,
65.3552154644212,65.4591409417916,65.5631252603363,65.6672915177955,65.7291643549453,
65.8652061647477,65.9734457251369),.UNSPECIFIED.);
#2604=B_SPLINE_CURVE_WITH_KNOTS('',3,(#90160,#90161,#90162,#90163,#90164,
#90165,#90166,#90167,#90168,#90169,#90170,#90171,#90172,#90173,#90174,#90175,
#90176,#90177,#90178,#90179,#90180,#90181,#90182,#90183,#90184,#90185,#90186,
#90187,#90188,#90189,#90190,#90191,#90192,#90193,#90194,#90195,#90196,#90197,
#90198,#90199,#90200,#90201,#90202,#90203,#90204,#90205,#90206,#90207,#90208,
#90209,#90210,#90211,#90212,#90213,#90214,#90215,#90216,#90217,#90218,#90219,
#90220,#90221,#90222,#90223,#90224,#90225,#90226,#90227,#90228,#90229),
 .UNSPECIFIED.,.F.,.F.,(4,3,3,3,3,3,3,3,3,3,3,3,3,3,3,3,3,3,3,3,3,3,3,4),
(65.9734457253856,66.0761317728201,66.1787500761627,66.2813369783486,66.3839287747718,
66.4866268116119,66.5893873525262,66.692318663947,66.7267122132914,66.8308983767796,
66.9349293019916,67.0388381924084,67.1426816235765,67.2464943745914,67.3503111811128,
67.4542366584832,67.5582209770279,67.6623872344871,67.7242600716375,67.8284495541652,
67.9324611612288,68.0363696448814,68.1402112750339,68.1995463580489),
 .UNSPECIFIED.);
#2605=B_SPLINE_CURVE_WITH_KNOTS('',3,(#90231,#90232,#90233,#90234,#90235,
#90236,#90237,#90238,#90239,#90240,#90241,#90242,#90243,#90244,#90245,#90246,
#90247,#90248,#90249,#90250,#90251,#90252,#90253,#90254,#90255,#90256,#90257,
#90258,#90259,#90260,#90261,#90262,#90263,#90264,#90265,#90266,#90267,#90268,
#90269,#90270,#90271,#90272,#90273,#90274,#90275,#90276,#90277,#90278,#90279,
#90280,#90281,#90282,#90283,#90284,#90285,#90286,#90287,#90288,#90289,#90290,
#90291,#90292,#90293,#90294,#90295,#90296,#90297),.UNSPECIFIED.,.F.,.F.,
(4,3,3,3,3,3,3,3,3,3,3,3,3,3,3,3,3,3,3,3,3,3,4),(65.9734457257113,66.0987387055991,
66.2258330924451,66.2706296467734,66.3748158102616,66.4788467354737,66.5827556258907,
66.6865990570588,66.7904118080738,66.8942286145953,66.9981540919657,67.1021384105105,
67.2063046679698,67.2681775051195,67.3723684093487,67.4763780578089,67.580285456455,
67.6841254672856,67.7879328708114,67.8918030347104,67.9957000777364,68.0997567680858,
68.1991405116964),.UNSPECIFIED.);
#2606=B_SPLINE_CURVE_WITH_KNOTS('',3,(#90298,#90299,#90300,#90301,#90302,
#90303,#90304,#90305,#90306,#90307,#90308,#90309,#90310,#90311,#90312,#90313,
#90314,#90315,#90316,#90317,#90318,#90319,#90320,#90321,#90322,#90323,#90324,
#90325,#90326,#90327,#90328,#90329,#90330,#90331,#90332,#90333,#90334,#90335,
#90336,#90337,#90338,#90339,#90340,#90341,#90342,#90343,#90344,#90345,#90346,
#90347,#90348,#90349,#90350,#90351,#90352,#90353,#90354,#90355,#90356,#90357,
#90358,#90359,#90360,#90361,#90362,#90363,#90364,#90365,#90366,#90367,#90368,
#90369,#90370,#90371,#90372,#90373,#90374,#90375,#90376,#90377,#90378,#90379,
#90380,#90381,#90382,#90383,#90384,#90385,#90386,#90387,#90388,#90389,#90390,
#90391,#90392,#90393,#90394,#90395,#90396,#90397,#90398,#90399,#90400,#90401,
#90402,#90403,#90404,#90405,#90406,#90407,#90408,#90409,#90410,#90411,#90412,
#90413,#90414,#90415,#90416,#90417,#90418,#90419,#90420,#90421),
 .UNSPECIFIED.,.F.,.F.,(4,3,3,3,3,3,3,3,3,3,3,3,3,3,3,3,3,3,3,3,3,3,3,3,
3,3,3,3,3,3,3,3,3,3,3,3,3,3,3,3,3,4),(61.9159031276989,62.0198326499991,
62.1238238422221,62.2279941032561,62.2804382133891,62.3846243768772,62.4886553020894,
62.5925641925064,62.6964076236745,62.8002203746894,62.9040371812107,63.0079626585811,
63.1119469771257,63.216113234585,63.2779860717351,63.3821722352232,63.4862031604353,
63.5901120508523,63.6939554820204,63.7977682330354,63.901585039557,64.0055105169275,
64.1094948354721,64.2136610929313,64.2755339300812,64.3797200935694,64.4837510187816,
64.5876599091986,64.6915033403668,64.7953160913818,64.8991328979035,65.0030583752739,
65.1070426938189,65.2112089512782,65.2730817884273,65.3766017373238,65.4799760620943,
65.5832406362457,65.6864470474328,65.7896160420576,65.8928309399411,65.9734457253856),
 .UNSPECIFIED.);
#2607=B_SPLINE_CURVE_WITH_KNOTS('',3,(#90427,#90428,#90429,#90430,#90431,
#90432,#90433,#90434,#90435,#90436,#90437,#90438,#90439,#90440,#90441,#90442,
#90443,#90444,#90445,#90446,#90447,#90448,#90449,#90450,#90451,#90452,#90453,
#90454,#90455,#90456,#90457,#90458,#90459,#90460,#90461,#90462,#90463,#90464,
#90465,#90466,#90467,#90468,#90469,#90470,#90471,#90472,#90473,#90474,#90475,
#90476,#90477,#90478,#90479,#90480,#90481,#90482,#90483,#90484,#90485,#90486,
#90487,#90488,#90489,#90490,#90491,#90492,#90493,#90494,#90495,#90496,#90497,
#90498,#90499,#90500,#90501,#90502,#90503,#90504,#90505,#90506,#90507,#90508,
#90509,#90510,#90511,#90512,#90513,#90514,#90515,#90516,#90517,#90518,#90519,
#90520,#90521,#90522,#90523,#90524,#90525,#90526,#90527,#90528,#90529,#90530,
#90531,#90532,#90533,#90534,#90535,#90536,#90537,#90538,#90539,#90540,#90541,
#90542,#90543,#90544,#90545,#90546,#90547,#90548,#90549,#90550),
 .UNSPECIFIED.,.F.,.F.,(4,3,3,3,3,3,3,3,3,3,3,3,3,3,3,3,3,3,3,3,3,3,3,3,
3,3,3,3,3,3,3,3,3,3,3,3,3,3,3,3,3,4),(55.6326045320091,55.736792722803,
55.7536857714845,55.8578719349727,55.9619028601848,56.0658117506018,56.1696551817699,
56.2734679327848,56.3772847393064,56.4812102166767,56.5851945352215,56.6893607926807,
56.7512336298306,56.8554197933188,56.959450718531,57.063359608948,57.1672030401161,
57.2710157911311,57.3748325976526,57.478758075023,57.5827423935677,57.686908651027,
57.7487814881766,57.8529676516648,57.9569985768769,58.0609074672938,58.1647508984619,
58.2685636494768,58.3723804559983,58.4763059333687,58.5802902519134,58.6844565093726,
58.7463293465227,58.8496743122095,58.9547475754165,59.0578171667581,59.1608249277454,
59.2638067574364,59.3704201725438,59.4735201525633,59.5818902852146,59.6902604178659),
 .UNSPECIFIED.);
#2608=B_SPLINE_CURVE_WITH_KNOTS('',3,(#90551,#90552,#90553,#90554,#90555,
#90556,#90557,#90558,#90559,#90560,#90561,#90562,#90563,#90564,#90565,#90566,
#90567,#90568,#90569,#90570,#90571,#90572,#90573,#90574,#90575,#90576,#90577,
#90578,#90579,#90580,#90581,#90582,#90583,#90584,#90585,#90586,#90587,#90588,
#90589,#90590,#90591,#90592,#90593,#90594,#90595,#90596,#90597,#90598,#90599,
#90600,#90601,#90602,#90603,#90604,#90605,#90606,#90607,#90608,#90609,#90610,
#90611,#90612,#90613,#90614,#90615,#90616,#90617,#90618,#90619,#90620),
 .UNSPECIFIED.,.F.,.F.,(4,3,3,3,3,3,3,3,3,3,3,3,3,3,3,3,3,3,3,3,3,3,3,4),
(59.690260418206,59.7438772048688,59.8480633683569,59.9520942935691,60.056003183986,
60.1598466151541,60.263659366169,60.3674761726906,60.4714016500609,60.5753859686056,
60.6795522260648,60.7414250632149,60.845611226703,60.9496421519152,61.0535510423322,
61.1573944735003,61.2612072245152,61.3650240310368,61.4689495084072,61.5729338269519,
61.6771000844111,61.738972921561,61.8431345897298,61.9168706242402),
 .UNSPECIFIED.);
#2609=B_SPLINE_CURVE_WITH_KNOTS('',3,(#90622,#90623,#90624,#90625,#90626,
#90627,#90628,#90629,#90630,#90631,#90632,#90633,#90634,#90635,#90636,#90637,
#90638,#90639,#90640,#90641,#90642,#90643,#90644,#90645,#90646,#90647,#90648,
#90649,#90650,#90651,#90652,#90653,#90654,#90655,#90656,#90657,#90658,#90659,
#90660,#90661,#90662,#90663,#90664,#90665,#90666,#90667,#90668,#90669,#90670,
#90671,#90672,#90673,#90674,#90675,#90676,#90677,#90678,#90679,#90680,#90681,
#90682,#90683,#90684,#90685,#90686,#90687,#90688),.UNSPECIFIED.,.F.,.F.,
(4,3,3,3,3,3,3,3,3,3,3,3,3,3,3,3,3,3,3,3,3,3,4),(59.690260418206,59.7955628120765,
59.9009059652381,60.0064057077468,60.1119895277649,60.2177899509138,60.2853424966969,
60.3895286601852,60.4935595853974,60.5974684758143,60.7013119069825,60.8051246579975,
60.9089414645191,61.0128669418895,61.1168512604342,61.2210175178934,61.282890355043,
61.3870598972592,61.4910835282141,61.5972884280853,61.7011283170153,61.8085157223571,
61.9159031276989),.UNSPECIFIED.);
#2610=B_SPLINE_CURVE_WITH_KNOTS('',3,(#90689,#90690,#90691,#90692,#90693,
#90694,#90695,#90696,#90697,#90698,#90699,#90700,#90701,#90702,#90703,#90704,
#90705,#90706,#90707,#90708,#90709,#90710,#90711,#90712,#90713,#90714,#90715,
#90716,#90717,#90718,#90719,#90720,#90721,#90722,#90723,#90724,#90725,#90726,
#90727,#90728,#90729,#90730,#90731,#90732,#90733,#90734,#90735,#90736,#90737,
#90738,#90739,#90740,#90741,#90742,#90743,#90744,#90745,#90746,#90747,#90748,
#90749,#90750,#90751,#90752,#90753,#90754,#90755,#90756,#90757,#90758,#90759,
#90760,#90761,#90762,#90763,#90764,#90765,#90766,#90767,#90768,#90769,#90770,
#90771,#90772,#90773,#90774,#90775,#90776,#90777,#90778,#90779,#90780,#90781,
#90782,#90783,#90784,#90785,#90786,#90787,#90788,#90789,#90790,#90791,#90792,
#90793,#90794,#90795,#90796,#90797,#90798,#90799,#90800,#90801,#90802,#90803,
#90804,#90805,#90806,#90807,#90808,#90809,#90810,#90811,#90812),
 .UNSPECIFIED.,.F.,.F.,(4,3,3,3,3,3,3,3,3,3,3,3,3,3,3,3,3,3,3,3,3,3,3,3,
3,3,3,3,3,3,3,3,3,3,3,3,3,3,3,3,3,4),(55.6335534587503,55.7373867807232,
55.8411973928298,55.9450200256885,56.0489562327104,56.1529584384112,56.2571354362515,
56.2951510633125,56.3993372268008,56.5033681520131,56.6072770424301,56.7111204735982,
56.8149332246131,56.9187500311349,57.0226755085053,57.12665982705,57.2308260845093,
57.2926989216586,57.3968850851468,57.5009160103588,57.6048249007758,57.7086683319439,
57.8124810829588,57.9162978894801,58.0202233668504,58.124207685395,58.2283739428542,
58.2902467800047,58.3944329434929,58.498463868705,58.6023727591219,58.7062161902901,
58.8100289413054,58.9138457478275,59.0177712251979,59.1217555437426,59.2259218012019,
59.2877946383508,59.4032420886161,59.5183215991953,59.6327919924175,59.6902604177957),
 .UNSPECIFIED.);
#2611=B_SPLINE_CURVE_WITH_KNOTS('',3,(#90818,#90819,#90820,#90821,#90822,
#90823,#90824,#90825,#90826,#90827,#90828,#90829,#90830,#90831,#90832,#90833,
#90834,#90835,#90836,#90837,#90838,#90839,#90840,#90841,#90842,#90843,#90844,
#90845,#90846,#90847,#90848,#90849,#90850,#90851,#90852,#90853,#90854,#90855,
#90856,#90857,#90858,#90859,#90860,#90861,#90862,#90863,#90864,#90865,#90866,
#90867,#90868,#90869,#90870,#90871,#90872,#90873,#90874,#90875,#90876,#90877,
#90878,#90879,#90880,#90881,#90882,#90883,#90884,#90885,#90886,#90887,#90888,
#90889,#90890,#90891,#90892,#90893,#90894,#90895,#90896,#90897,#90898,#90899,
#90900,#90901,#90902,#90903,#90904,#90905,#90906,#90907,#90908,#90909,#90910,
#90911,#90912,#90913,#90914,#90915,#90916,#90917,#90918,#90919,#90920,#90921,
#90922,#90923,#90924,#90925,#90926,#90927,#90928,#90929,#90930,#90931,#90932,
#90933,#90934,#90935,#90936,#90937,#90938,#90939,#90940,#90941),
 .UNSPECIFIED.,.F.,.F.,(4,3,3,3,3,3,3,3,3,3,3,3,3,3,3,3,3,3,3,3,3,3,3,3,
3,3,3,3,3,3,3,3,3,3,3,3,3,3,3,3,3,4),(49.3496765146293,49.4543570413239,
49.558312629052,49.6633556252299,49.7683986214079,49.872584784896,49.9766157101083,
50.0805246005252,50.1843680316934,50.2881807827085,50.3919975892302,50.4959230666005,
50.5999073851452,50.7040736426044,50.765946479754,50.8701326432422,50.9741635684541,
51.0780724588711,51.1819158900391,51.2857286410542,51.3895454475755,51.493470924946,
51.5974552434908,51.70162150095,51.7634943381001,51.8676805015882,51.9717114268003,
52.0756203172173,52.1794637483854,52.2832764994004,52.387093305922,52.4910187832924,
52.5950031018373,52.6991693592965,52.7610421964462,52.8655509126696,52.9699037514317,
53.0791965913304,53.1833373805663,53.2874304651177,53.3915238347385,53.4070751110264),
 .UNSPECIFIED.);
#2612=B_SPLINE_CURVE_WITH_KNOTS('',3,(#90942,#90943,#90944,#90945,#90946,
#90947,#90948,#90949,#90950,#90951,#90952,#90953,#90954,#90955,#90956,#90957,
#90958,#90959,#90960,#90961,#90962,#90963,#90964,#90965,#90966,#90967,#90968,
#90969,#90970,#90971,#90972,#90973,#90974,#90975,#90976,#90977,#90978,#90979,
#90980,#90981,#90982,#90983,#90984,#90985,#90986,#90987,#90988,#90989,#90990,
#90991,#90992,#90993,#90994,#90995,#90996,#90997,#90998,#90999,#91000,#91001,
#91002,#91003,#91004,#91005,#91006,#91007,#91008),.UNSPECIFIED.,.F.,.F.,
(4,3,3,3,3,3,3,3,3,3,3,3,3,3,3,3,3,3,3,3,3,3,4),(53.4070751114778,53.5259953052186,
53.6459937542289,53.7585900547923,53.8627762182805,53.9668071434927,54.0707160339097,
54.1745594650778,54.2783722160927,54.3821890226141,54.4861144999845,54.5900988185292,
54.6942650759884,54.7561379131384,54.8656962404972,54.9697007582687,55.0736032491578,
55.1774385737942,55.281241510946,55.385092536991,55.4889714141182,55.5929703731723,
55.6326045320091),.UNSPECIFIED.);
#2613=B_SPLINE_CURVE_WITH_KNOTS('',3,(#91010,#91011,#91012,#91013,#91014,
#91015,#91016,#91017,#91018,#91019,#91020,#91021,#91022,#91023,#91024,#91025,
#91026,#91027,#91028,#91029,#91030,#91031,#91032,#91033,#91034,#91035,#91036,
#91037,#91038,#91039,#91040,#91041,#91042,#91043,#91044,#91045,#91046,#91047,
#91048,#91049,#91050,#91051,#91052,#91053,#91054,#91055,#91056,#91057,#91058,
#91059,#91060,#91061,#91062,#91063,#91064,#91065,#91066,#91067,#91068,#91069,
#91070,#91071,#91072,#91073,#91074,#91075,#91076,#91077,#91078,#91079),
 .UNSPECIFIED.,.F.,.F.,(4,3,3,3,3,3,3,3,3,3,3,3,3,3,3,3,3,3,3,3,3,3,3,4),
(53.4070751114786,53.5098614913149,53.6124973139476,53.7150505550743,53.8175576893134,
53.9200551251567,54.0226483900827,54.1252912590462,54.2281147116669,54.3000553466204,
54.4042415101086,54.5082724353209,54.6121813257378,54.7160247569059,54.8198375079208,
54.9236543144422,55.0275797918125,55.1315641103571,55.2357303678164,55.2976032049664,
55.4017686790633,55.5057980059472,55.6097071730358,55.6335534587503),
 .UNSPECIFIED.);
#2614=B_SPLINE_CURVE_WITH_KNOTS('',3,(#91080,#91081,#91082,#91083,#91084,
#91085,#91086,#91087,#91088,#91089,#91090,#91091,#91092,#91093,#91094,#91095,
#91096,#91097,#91098,#91099,#91100,#91101,#91102,#91103,#91104,#91105,#91106,
#91107,#91108,#91109,#91110,#91111,#91112,#91113,#91114,#91115,#91116,#91117,
#91118,#91119,#91120,#91121,#91122,#91123,#91124,#91125,#91126,#91127,#91128,
#91129,#91130,#91131,#91132,#91133,#91134,#91135,#91136,#91137,#91138,#91139,
#91140,#91141,#91142,#91143,#91144,#91145,#91146,#91147,#91148,#91149,#91150,
#91151,#91152,#91153,#91154,#91155,#91156,#91157,#91158,#91159,#91160,#91161,
#91162,#91163,#91164,#91165,#91166,#91167,#91168,#91169,#91170,#91171,#91172,
#91173,#91174,#91175,#91176,#91177,#91178,#91179,#91180,#91181,#91182,#91183,
#91184,#91185,#91186,#91187,#91188,#91189,#91190,#91191,#91192,#91193,#91194,
#91195,#91196,#91197,#91198,#91199,#91200,#91201,#91202,#91203),
 .UNSPECIFIED.,.F.,.F.,(4,3,3,3,3,3,3,3,3,3,3,3,3,3,3,3,3,3,3,3,3,3,3,3,
3,3,3,3,3,3,3,3,3,3,3,3,3,3,3,3,3,4),(49.3501260113316,49.4542513866548,
49.5612029524774,49.6650820823779,49.7689093695806,49.872719572018,49.9820056573225,
50.0859533807799,50.1899737976859,50.2941626671254,50.309863913236,50.4140500767241,
50.5180810019363,50.6219898923532,50.7258333235213,50.8296460745361,50.9334628810576,
51.0373883584279,51.1413726769726,51.2455389344318,51.3074117715821,51.4115979350703,
51.5156288602825,51.6195377506995,51.7233811818676,51.8271939328825,51.9310107394041,
52.0349362167745,52.1389205353193,52.2430867927785,52.3049596299282,52.4091457934164,
52.5131767186285,52.6170856090454,52.7209290402135,52.8247417912284,52.92855859775,
53.0324840751203,53.136468393665,53.2406346511242,53.3025074882743,53.4070751110265),
 .UNSPECIFIED.);
#2615=B_SPLINE_CURVE_WITH_KNOTS('',3,(#91209,#91210,#91211,#91212,#91213,
#91214,#91215,#91216,#91217,#91218,#91219,#91220,#91221,#91222,#91223,#91224,
#91225,#91226,#91227,#91228,#91229,#91230,#91231,#91232,#91233,#91234,#91235,
#91236,#91237,#91238,#91239,#91240,#91241,#91242,#91243,#91244,#91245,#91246,
#91247,#91248,#91249,#91250,#91251,#91252,#91253,#91254,#91255,#91256,#91257,
#91258,#91259,#91260,#91261,#91262,#91263,#91264,#91265,#91266,#91267,#91268,
#91269,#91270,#91271,#91272,#91273,#91274,#91275,#91276,#91277,#91278,#91279,
#91280,#91281,#91282,#91283,#91284,#91285,#91286,#91287,#91288,#91289,#91290,
#91291,#91292,#91293,#91294,#91295,#91296,#91297,#91298,#91299,#91300,#91301,
#91302,#91303,#91304,#91305,#91306,#91307,#91308,#91309,#91310,#91311,#91312,
#91313,#91314,#91315,#91316,#91317,#91318,#91319,#91320,#91321,#91322,#91323,
#91324,#91325,#91326,#91327,#91328,#91329),.UNSPECIFIED.,.F.,.F.,(4,3,3,
3,3,3,3,3,3,3,3,3,3,3,3,3,3,3,3,3,3,3,3,3,3,3,3,3,3,3,3,3,3,3,3,3,3,3,3,
3,4),(43.0672771824896,43.1711361743488,43.2749543100599,43.3787663343812,
43.4826804992014,43.5866443730128,43.6907998584982,43.7831114713314,43.8872976348202,
43.991328560033,44.0952374504505,44.1990808816192,44.3028936326347,44.4067104391569,
44.5106359165279,44.6146202350732,44.718786492533,44.7806593296775,44.8848454931655,
44.9888764183773,45.0927853087942,45.1966287399621,45.3004414909768,45.4042582974981,
45.5081837748683,45.6121680934129,45.7163343508719,45.7782071880236,45.8823933515116,
45.9864242767236,46.0903331671405,46.1941765983085,46.2979893493234,46.4018061558448,
46.5057316332153,46.60971595176,46.7138822092192,46.7757550463697,46.8962986192144,
47.0157785770619,47.123889803398),.UNSPECIFIED.);
#2616=B_SPLINE_CURVE_WITH_KNOTS('',3,(#91330,#91331,#91332,#91333,#91334,
#91335,#91336,#91337,#91338,#91339,#91340,#91341,#91342,#91343,#91344,#91345,
#91346,#91347,#91348,#91349,#91350,#91351,#91352,#91353,#91354,#91355,#91356,
#91357,#91358,#91359,#91360,#91361,#91362,#91363,#91364,#91365,#91366,#91367,
#91368,#91369,#91370,#91371,#91372,#91373,#91374,#91375,#91376,#91377,#91378,
#91379,#91380,#91381,#91382,#91383,#91384,#91385,#91386,#91387,#91388,#91389,
#91390,#91391,#91392,#91393,#91394,#91395,#91396,#91397,#91398,#91399),
 .UNSPECIFIED.,.F.,.F.,(4,3,3,3,3,3,3,3,3,3,3,3,3,3,3,3,3,3,3,3,3,3,3,4),
(47.1238898038468,47.2279281355327,47.3319603652865,47.4360206698572,47.5402127556636,
47.6444838895222,47.7489375131551,47.7733029047158,47.8774890682039,47.981519993416,
48.0854288838329,48.189272315001,48.2930850660159,48.3969018725375,48.5008273499079,
48.6048116684526,48.7089779259118,48.7708507630619,48.8750265334971,48.9790548139466,
49.0829625287093,49.1867995817475,49.2906190127626,49.3496765146293),
 .UNSPECIFIED.);
#2617=B_SPLINE_CURVE_WITH_KNOTS('',3,(#91401,#91402,#91403,#91404,#91405,
#91406,#91407,#91408,#91409,#91410,#91411,#91412,#91413,#91414,#91415,#91416,
#91417,#91418,#91419,#91420,#91421,#91422,#91423,#91424,#91425,#91426,#91427,
#91428,#91429,#91430,#91431,#91432,#91433,#91434,#91435,#91436,#91437,#91438,
#91439,#91440,#91441,#91442,#91443,#91444,#91445,#91446,#91447,#91448,#91449,
#91450,#91451,#91452,#91453,#91454,#91455,#91456,#91457,#91458,#91459,#91460,
#91461,#91462,#91463,#91464,#91465,#91466,#91467,#91468,#91469,#91470),
 .UNSPECIFIED.,.F.,.F.,(4,3,3,3,3,3,3,3,3,3,3,3,3,3,3,3,3,3,3,3,3,3,3,4),
(47.1238898038469,47.2754958859209,47.3172203381977,47.4214065016857,47.5254374268976,
47.6293463173144,47.7331897484823,47.837002499497,47.9408193060184,48.0447447833886,
48.1487291019331,48.2528953593921,48.3147681965438,48.4189543600319,48.522985285244,
48.626894175661,48.730737606829,48.8345503578439,48.9383671643654,49.0422926417358,
49.1462769602805,49.2504432177397,49.3123160548899,49.3501260113316),
 .UNSPECIFIED.);
#2618=B_SPLINE_CURVE_WITH_KNOTS('',3,(#91471,#91472,#91473,#91474,#91475,
#91476,#91477,#91478,#91479,#91480,#91481,#91482,#91483,#91484,#91485,#91486,
#91487,#91488,#91489,#91490,#91491,#91492,#91493,#91494,#91495,#91496,#91497,
#91498,#91499,#91500,#91501,#91502,#91503,#91504,#91505,#91506,#91507,#91508,
#91509,#91510,#91511,#91512,#91513,#91514,#91515,#91516,#91517,#91518,#91519,
#91520,#91521,#91522,#91523,#91524,#91525,#91526,#91527,#91528,#91529,#91530,
#91531,#91532,#91533,#91534,#91535,#91536,#91537,#91538,#91539,#91540,#91541,
#91542,#91543,#91544,#91545,#91546,#91547,#91548,#91549,#91550,#91551,#91552,
#91553,#91554,#91555,#91556,#91557,#91558,#91559,#91560,#91561,#91562,#91563,
#91564,#91565,#91566,#91567,#91568,#91569,#91570,#91571,#91572,#91573,#91574,
#91575,#91576,#91577,#91578,#91579,#91580,#91581,#91582,#91583,#91584,#91585,
#91586,#91587,#91588,#91589,#91590,#91591,#91592,#91593,#91594),
 .UNSPECIFIED.,.F.,.F.,(4,3,3,3,3,3,3,3,3,3,3,3,3,3,3,3,3,3,3,3,3,3,3,3,
3,3,3,3,3,3,3,3,3,3,3,3,3,3,3,3,3,4),(43.0661637738671,43.1701547732055,
43.2743249196621,43.3270289048134,43.431215068306,43.5352459935225,43.639154883944,
43.7429983151167,43.8468110661362,43.9506278726623,44.0545533500374,44.1585376685868,
44.2627039260507,44.3245767631595,44.4287629266466,44.5327938518577,44.6367027422736,
44.7405461734406,44.8443589244544,44.9481757309749,45.0521012083441,45.1560855268878,
45.260251784346,45.3221246215056,45.4263107849932,45.5303417102049,45.6342506006213,
45.7380940317888,45.8419067828031,45.9457235893239,46.0496490666937,46.1536333852379,
46.2577996426965,46.3196724798517,46.4223012412915,46.524793586442,46.6271863644393,
46.7295162801934,46.8318649061936,46.9342176129162,47.0366904241986,47.1238898034408),
 .UNSPECIFIED.);
#2619=B_SPLINE_CURVE_WITH_KNOTS('',3,(#91600,#91601,#91602,#91603,#91604,
#91605,#91606,#91607,#91608,#91609,#91610,#91611,#91612,#91613,#91614,#91615,
#91616,#91617,#91618,#91619,#91620,#91621,#91622,#91623,#91624,#91625,#91626,
#91627,#91628,#91629,#91630,#91631,#91632,#91633,#91634,#91635,#91636,#91637,
#91638,#91639,#91640,#91641,#91642,#91643,#91644,#91645,#91646,#91647,#91648,
#91649,#91650,#91651,#91652,#91653,#91654,#91655,#91656,#91657,#91658,#91659,
#91660,#91661,#91662,#91663,#91664,#91665,#91666,#91667,#91668,#91669,#91670,
#91671,#91672,#91673,#91674,#91675,#91676,#91677,#91678,#91679,#91680,#91681,
#91682,#91683,#91684,#91685,#91686,#91687,#91688,#91689,#91690,#91691,#91692,
#91693,#91694,#91695,#91696,#91697,#91698,#91699,#91700,#91701,#91702,#91703,
#91704,#91705,#91706,#91707,#91708,#91709,#91710,#91711,#91712,#91713,#91714,
#91715,#91716,#91717,#91718,#91719,#91720,#91721,#91722,#91723,#91724,#91725,
#91726),.UNSPECIFIED.,.F.,.F.,(4,3,3,3,3,3,3,3,3,3,3,3,3,3,3,3,3,3,3,3,
3,3,3,3,3,3,3,3,3,3,3,3,3,3,3,3,3,3,3,3,3,3,4),(36.7834483295922,36.8002764629088,
36.9044626263497,37.0084935515136,37.1124024418811,37.216245872999,37.3200586239631,
37.4238754304332,37.5278009077515,37.6317852262439,37.7359514836507,37.7978243212549,
37.9020104847764,38.0060414100223,38.1099503004736,38.2137937316764,38.3176064827263,
38.4214232892831,38.5253487666888,38.629333085269,38.7334993427635,38.795372179601,
38.899558343083,39.0035892682889,39.1074981586996,39.2113415898615,39.3151543408703,
39.4189711473856,39.5228966247499,39.6268809432886,39.7310472007419,39.7929200379471,
39.8971062014302,40.0011371266371,40.1050460170488,40.2088894482115,40.3127021992209,
40.4165190057368,40.5204444831015,40.6244288016405,40.7285950590941,40.7904678962932,
40.8407044966673),.UNSPECIFIED.);
#2620=B_SPLINE_CURVE_WITH_KNOTS('',3,(#91727,#91728,#91729,#91730,#91731,
#91732,#91733,#91734,#91735,#91736,#91737,#91738,#91739,#91740,#91741,#91742,
#91743,#91744,#91745,#91746,#91747,#91748,#91749,#91750,#91751,#91752,#91753,
#91754,#91755,#91756,#91757,#91758,#91759,#91760,#91761,#91762,#91763,#91764,
#91765,#91766,#91767,#91768,#91769,#91770,#91771,#91772,#91773,#91774,#91775,
#91776,#91777,#91778,#91779,#91780,#91781,#91782,#91783,#91784,#91785,#91786,
#91787,#91788,#91789,#91790,#91791,#91792,#91793,#91794,#91795,#91796),
 .UNSPECIFIED.,.F.,.F.,(4,3,3,3,3,3,3,3,3,3,3,3,3,3,3,3,3,3,3,3,3,3,3,4),
(40.8407044969994,40.9440746115612,41.0495672544459,41.152672005388,41.2557188072321,
41.3587435025167,41.4660615655473,41.56921475009,41.6724388016659,41.7758284060399,
41.7880157546392,41.8922019181263,41.9962328433373,42.1001417337531,42.2039851649202,
42.3077979159341,42.4116147224543,42.5155401998236,42.6195245183673,42.7236907758254,
42.7855636129853,42.8897412721946,42.9937540506505,43.0672771824896),
 .UNSPECIFIED.);
#2621=B_SPLINE_CURVE_WITH_KNOTS('',3,(#91798,#91799,#91800,#91801,#91802,
#91803,#91804,#91805,#91806,#91807,#91808,#91809,#91810,#91811,#91812,#91813,
#91814,#91815,#91816,#91817,#91818,#91819,#91820,#91821,#91822,#91823,#91824,
#91825,#91826,#91827,#91828,#91829,#91830,#91831,#91832,#91833,#91834,#91835,
#91836,#91837,#91838,#91839,#91840,#91841,#91842,#91843,#91844,#91845,#91846,
#91847,#91848,#91849,#91850,#91851,#91852,#91853,#91854,#91855,#91856,#91857,
#91858,#91859,#91860,#91861,#91862,#91863,#91864),.UNSPECIFIED.,.F.,.F.,
(4,3,3,3,3,3,3,3,3,3,3,3,3,3,3,3,3,3,3,3,3,3,4),(40.8407044969871,40.9497796083695,
41.0591756422976,41.1687426604475,41.278611244788,41.3319331881212,41.4361193516033,
41.5401502768092,41.64405916722,41.747902598382,41.8517153493908,41.9555321559062,
42.0594576332706,42.1634419518094,42.2676082092628,42.3294810464673,42.4336404890024,
42.5376570384814,42.6415656994819,42.7477152180782,42.8515331448653,42.9588484593662,
43.0661637738671),.UNSPECIFIED.);
#2622=B_SPLINE_CURVE_WITH_KNOTS('',3,(#91865,#91866,#91867,#91868,#91869,
#91870,#91871,#91872,#91873,#91874,#91875,#91876,#91877,#91878,#91879,#91880,
#91881,#91882,#91883,#91884,#91885,#91886,#91887,#91888,#91889,#91890,#91891,
#91892,#91893,#91894,#91895,#91896,#91897,#91898,#91899,#91900,#91901,#91902,
#91903,#91904,#91905,#91906,#91907,#91908,#91909,#91910,#91911,#91912,#91913,
#91914,#91915,#91916,#91917,#91918,#91919,#91920,#91921,#91922,#91923,#91924,
#91925,#91926,#91927,#91928,#91929,#91930,#91931,#91932,#91933,#91934,#91935,
#91936,#91937,#91938,#91939,#91940,#91941,#91942,#91943,#91944,#91945,#91946,
#91947,#91948,#91949,#91950,#91951,#91952,#91953,#91954,#91955,#91956,#91957,
#91958,#91959,#91960,#91961,#91962,#91963,#91964,#91965,#91966,#91967,#91968,
#91969,#91970,#91971,#91972,#91973,#91974,#91975,#91976,#91977,#91978,#91979,
#91980,#91981,#91982,#91983,#91984,#91985,#91986,#91987,#91988),
 .UNSPECIFIED.,.F.,.F.,(4,3,3,3,3,3,3,3,3,3,3,3,3,3,3,3,3,3,3,3,3,3,3,3,
3,3,3,3,3,3,3,3,3,3,3,3,3,3,3,3,3,4),(36.7837280536202,36.8875386782118,
36.9913612401259,37.0952973258126,37.199299335197,37.30347620961,37.3417417547369,
37.4459279184724,37.5499588439353,37.6538677346069,37.7577111660321,37.861523917306,
37.9653407240879,38.0692662017194,38.173250520526,38.2774167782453,38.339289613083,
38.443475776542,38.547506701725,38.6514155921136,38.7552590232534,38.8590717742405,
38.9628885807346,39.0668140580781,39.1707983765966,39.2749646340303,39.3368374714291,
39.4410236348703,39.5450545600343,39.6489634504021,39.7528068815202,39.8566196324846,
39.9604364389555,40.0643619162741,40.1683462347668,40.272512492174,40.3343853297751,
40.4435562695043,40.5524208008746,40.6611016633604,40.769557770341,40.8407044966673),
 .UNSPECIFIED.);
#2623=B_SPLINE_CURVE_WITH_KNOTS('',3,(#91994,#91995,#91996,#91997,#91998,
#91999,#92000,#92001),.UNSPECIFIED.,.F.,.F.,(4,1,1,1,1,4),(30.4995505242199,
30.8149893128323,31.8125371711784,32.8100850295245,33.8076328878706,34.5575191894876),
 .UNSPECIFIED.);
#2624=B_SPLINE_CURVE_WITH_KNOTS('',3,(#92002,#92003,#92004,#92005,#92006,
#92007,#92008,#92009,#92010,#92011,#92012,#92013,#92014,#92015,#92016,#92017,
#92018,#92019,#92020,#92021,#92022,#92023,#92024,#92025,#92026,#92027,#92028,
#92029,#92030,#92031,#92032,#92033,#92034,#92035,#92036,#92037,#92038,#92039,
#92040,#92041,#92042,#92043,#92044,#92045,#92046,#92047,#92048,#92049,#92050,
#92051,#92052,#92053,#92054,#92055,#92056,#92057,#92058,#92059,#92060,#92061,
#92062,#92063,#92064,#92065,#92066,#92067,#92068),.UNSPECIFIED.,.F.,.F.,
(4,3,3,3,3,3,3,3,3,3,3,3,3,3,3,3,3,3,3,3,3,3,4),(34.5575192744995,34.6927957333311,
34.8051807462166,34.9093669099533,35.0133978354175,35.1173067260906,35.2211501575171,
35.3249629087925,35.4287797155758,35.5327051932087,35.6366895120167,35.7408557697374,
35.8027286045627,35.9069159429525,36.0109477003902,36.1148561156612,36.218698586411,
36.3225098920317,36.4263247678229,36.5302426834939,36.6342192413487,36.7383649008209,
36.7834483295922),.UNSPECIFIED.);
#2625=B_SPLINE_CURVE_WITH_KNOTS('',3,(#92070,#92071,#92072,#92073,#92074,
#92075,#92076,#92077,#92078,#92079,#92080,#92081,#92082,#92083,#92084,#92085,
#92086,#92087,#92088,#92089,#92090,#92091,#92092,#92093,#92094,#92095,#92096,
#92097,#92098,#92099,#92100,#92101,#92102,#92103,#92104,#92105,#92106,#92107,
#92108,#92109,#92110,#92111,#92112,#92113,#92114,#92115,#92116,#92117,#92118,
#92119,#92120,#92121,#92122,#92123,#92124,#92125,#92126,#92127,#92128,#92129,
#92130,#92131,#92132,#92133,#92134,#92135,#92136,#92137,#92138,#92139),
 .UNSPECIFIED.,.F.,.F.,(4,3,3,3,3,3,3,3,3,3,3,3,3,3,3,3,3,3,3,3,3,3,3,4),
(34.5575191897439,34.6600261058238,34.7624492437726,34.8648252112128,34.9671905469551,
35.0696506767871,35.1721598105652,35.2748489353093,35.3466460380447,35.4508322014592,
35.5548631266016,35.6587720169549,35.7626154480633,35.8664281990224,35.9702450054921,
36.0741704828175,36.1781548013209,36.2823210587452,36.3441938963908,36.4483886654195,
36.5524031605752,36.6563141143339,36.7601506285633,36.7837280536202),
 .UNSPECIFIED.);
#2626=B_SPLINE_CURVE_WITH_KNOTS('',3,(#92140,#92141,#92142,#92143,#92144,
#92145,#92146,#92147,#92148,#92149,#92150,#92151,#92152,#92153,#92154,#92155,
#92156,#92157,#92158,#92159,#92160,#92161,#92162,#92163,#92164,#92165,#92166,
#92167,#92168,#92169,#92170,#92171,#92172,#92173,#92174,#92175,#92176,#92177,
#92178,#92179,#92180,#92181,#92182,#92183,#92184,#92185,#92186,#92187,#92188,
#92189,#92190,#92191,#92192,#92193,#92194,#92195,#92196,#92197,#92198,#92199,
#92200,#92201,#92202,#92203,#92204,#92205,#92206,#92207,#92208,#92209,#92210,
#92211,#92212,#92213,#92214,#92215,#92216,#92217,#92218,#92219,#92220,#92221,
#92222,#92223,#92224,#92225,#92226,#92227,#92228,#92229,#92230,#92231,#92232,
#92233,#92234,#92235,#92236,#92237,#92238,#92239,#92240,#92241,#92242,#92243,
#92244,#92245,#92246,#92247,#92248,#92249,#92250,#92251,#92252,#92253,#92254,
#92255,#92256,#92257,#92258,#92259,#92260,#92261,#92262,#92263),
 .UNSPECIFIED.,.F.,.F.,(4,3,3,3,3,3,3,3,3,3,3,3,3,3,3,3,3,3,3,3,3,3,3,3,
3,3,3,3,3,3,3,3,3,3,3,3,3,3,3,3,3,4),(30.5009012395315,30.6078454101726,
30.7117244743431,30.8155517128082,30.9193618835234,31.0286350638077,31.1325827763094,
31.2366031938056,31.3407920531297,31.3564546046604,31.4606407808898,31.5646717189986,
31.6685806224799,31.7724240668089,31.8762368310614,31.9800536508775,32.0839791415378,
32.18796347339,32.2921297440395,32.3540024630065,32.4581886271218,32.5622195530108,
32.6661284441755,32.7699718761347,32.873784627983,32.9776014353793,33.0815269136819,
33.1855112331928,33.2896774916617,33.3515503213525,33.4557364812571,33.5597674028189,
33.6636762895042,33.7675197168922,33.8713324640845,33.9751492667464,34.0790747402267,
34.1830590548584,34.2872253084106,34.3490981796986,34.4951131661409,34.5575191894877),
 .UNSPECIFIED.);
#2627=B_SPLINE_CURVE_WITH_KNOTS('',3,(#92269,#92270,#92271,#92272,#92273,
#92274,#92275,#92276,#92277,#92278,#92279,#92280,#92281,#92282,#92283,#92284,
#92285,#92286,#92287,#92288,#92289,#92290,#92291,#92292,#92293,#92294,#92295,
#92296,#92297,#92298,#92299,#92300,#92301,#92302,#92303,#92304,#92305,#92306,
#92307,#92308,#92309,#92310,#92311,#92312,#92313,#92314,#92315,#92316,#92317,
#92318,#92319,#92320,#92321,#92322,#92323,#92324,#92325,#92326,#92327,#92328,
#92329,#92330,#92331,#92332,#92333,#92334,#92335,#92336,#92337,#92338,#92339,
#92340,#92341,#92342,#92343,#92344,#92345,#92346,#92347,#92348,#92349,#92350,
#92351,#92352,#92353,#92354,#92355,#92356,#92357,#92358,#92359,#92360,#92361,
#92362,#92363,#92364,#92365,#92366,#92367,#92368,#92369,#92370,#92371,#92372,
#92373,#92374,#92375,#92376,#92377,#92378,#92379,#92380,#92381,#92382,#92383,
#92384,#92385,#92386,#92387,#92388,#92389),.UNSPECIFIED.,.F.,.F.,(4,3,3,
3,3,3,3,3,3,3,3,3,3,3,3,3,3,3,3,3,3,3,3,3,3,3,3,3,3,3,3,3,3,3,3,3,3,3,3,
3,4),(24.2175094731414,24.3213278572364,24.4251400605738,24.5290543606235,
24.6330183067792,24.7371739381643,24.8297021627558,24.93388808274,25.037918760325,
25.1418273981882,25.2456705738977,25.3494830669292,25.4532996133197,25.5572248290617,
25.6612088847385,25.7653748802143,25.8272500211019,25.931436271936,26.0354672854447,
26.1393762651375,26.2432197861367,26.347032627403,26.450849524462,26.5547750921803,
26.6587595011022,26.7629258480012,26.8247978794479,26.928984057102,27.0330149970091,
27.1369239028387,27.2407673498547,27.34458011713,27.4483969403018,27.5523224348072,
27.6563067707863,27.7604730459679,27.822345737794,27.9353427130044,28.0470527868677,
28.1606932127517,28.2743336386358),.UNSPECIFIED.);
#2628=B_SPLINE_CURVE_WITH_KNOTS('',3,(#92390,#92391,#92392,#92393,#92394,
#92395),.UNSPECIFIED.,.F.,.F.,(4,1,1,4),(28.2743338823081,28.8198935961401,
29.8174414544862,30.4995505242199),.UNSPECIFIED.);
#2629=B_SPLINE_CURVE_WITH_KNOTS('',3,(#92397,#92398,#92399,#92400,#92401,
#92402,#92403,#92404,#92405,#92406,#92407,#92408,#92409,#92410,#92411,#92412,
#92413,#92414,#92415,#92416,#92417,#92418,#92419,#92420,#92421,#92422,#92423,
#92424,#92425,#92426,#92427,#92428,#92429,#92430,#92431,#92432,#92433,#92434,
#92435,#92436,#92437,#92438,#92439,#92440,#92441,#92442,#92443,#92444,#92445,
#92446,#92447,#92448,#92449,#92450,#92451,#92452,#92453,#92454,#92455,#92456,
#92457,#92458,#92459,#92460,#92461,#92462,#92463,#92464,#92465,#92466),
 .UNSPECIFIED.,.F.,.F.,(4,3,3,3,3,3,3,3,3,3,3,3,3,3,3,3,3,3,3,3,3,3,3,4),
(28.2743338823081,28.3638110296221,28.4679972801179,28.5720282932844,28.6759372726305,
28.7797807932806,28.8835936341959,28.9874105309025,29.0913360982685,29.1953205068379,
29.2994868533873,29.3613588879682,29.4655450656092,29.5695760055018,29.6734849113152,
29.7773283583141,29.8811411255711,29.9849579487237,30.0888834432082,30.1928677791657,
30.2970340543243,30.3589067463143,30.4630838119347,30.5009012395315),
 .UNSPECIFIED.);
#2630=B_SPLINE_CURVE_WITH_KNOTS('',3,(#92467,#92468,#92469,#92470,#92471,
#92472,#92473,#92474,#92475,#92476,#92477,#92478,#92479,#92480,#92481,#92482,
#92483,#92484,#92485,#92486,#92487,#92488,#92489,#92490,#92491,#92492,#92493,
#92494,#92495,#92496,#92497,#92498,#92499,#92500,#92501,#92502,#92503,#92504,
#92505,#92506,#92507,#92508,#92509,#92510,#92511,#92512,#92513,#92514,#92515,
#92516,#92517,#92518,#92519,#92520,#92521,#92522,#92523,#92524,#92525,#92526,
#92527,#92528,#92529,#92530,#92531,#92532,#92533,#92534,#92535,#92536,#92537,
#92538,#92539,#92540,#92541,#92542,#92543,#92544,#92545,#92546,#92547,#92548,
#92549,#92550,#92551,#92552,#92553,#92554,#92555,#92556,#92557,#92558,#92559,
#92560,#92561,#92562,#92563,#92564,#92565,#92566,#92567,#92568,#92569,#92570,
#92571,#92572,#92573,#92574,#92575,#92576,#92577,#92578,#92579,#92580,#92581,
#92582,#92583,#92584,#92585,#92586,#92587,#92588,#92589,#92590),
 .UNSPECIFIED.,.F.,.F.,(4,3,3,3,3,3,3,3,3,3,3,3,3,3,3,3,3,3,3,3,3,3,3,3,
3,3,3,3,3,3,3,3,3,3,3,3,3,3,3,3,3,4),(24.2166158670722,24.3207881370909,
24.3736195962378,24.4778038315917,24.5818327974666,24.6857396916881,24.7895811049884,
24.8933918194664,24.9972065737642,25.1011299890377,25.2051122368004,25.3092764321701,
25.3711674545838,25.4753541852857,25.5793856828633,25.6832951504786,25.7871391615083,
25.8909524941752,25.9947698832689,26.098695940573,26.2026808384369,26.3068476679265,
26.3687153129299,26.4729016565365,26.576932766987,26.6808418493753,26.7846854765711,
26.8884984273835,26.9923154371893,27.0962411217986,27.2002256501272,27.3043921191463,
27.366263171276,27.4692311189486,27.5720239013197,27.6747188321344,27.77735230861,
27.8799606435766,27.9826447824898,28.0853648870236,28.1882547092596,28.27433388186),
 .UNSPECIFIED.);
#2631=B_SPLINE_CURVE_WITH_KNOTS('',3,(#92596,#92597,#92598,#92599,#92600,
#92601,#92602,#92603,#92604,#92605,#92606,#92607,#92608,#92609,#92610,#92611,
#92612,#92613,#92614,#92615,#92616,#92617,#92618,#92619,#92620,#92621,#92622,
#92623,#92624,#92625,#92626,#92627,#92628,#92629,#92630,#92631,#92632,#92633,
#92634,#92635,#92636,#92637,#92638,#92639,#92640,#92641,#92642,#92643,#92644,
#92645,#92646,#92647,#92648,#92649,#92650,#92651,#92652,#92653,#92654,#92655,
#92656,#92657,#92658,#92659,#92660,#92661,#92662,#92663,#92664,#92665),
 .UNSPECIFIED.,.F.,.F.,(4,3,3,3,3,3,3,3,3,3,3,3,3,3,3,3,3,3,3,3,3,3,3,4),
(15.7079632679489,15.8106735934767,15.91334885119,16.0160251385365,16.1188116550667,
16.2216565686017,16.3246921199071,16.3932367294691,16.4975143581255,16.6016360889328,
16.7056343280856,16.8095661523013,16.9134661991799,17.0173690618201,17.1213780774191,
17.2254446357146,17.329690162223,17.3907845878152,17.495135742761,17.6048038128368,
17.7088847629099,17.8128986704477,17.916887220124,17.9338080230641),
 .UNSPECIFIED.);
#2632=B_SPLINE_CURVE_WITH_KNOTS('',3,(#92667,#92668,#92669,#92670,#92671),
 .UNSPECIFIED.,.F.,.F.,(4,1,4),(14.3981410127769,15.395688871123,15.7079548163673),
 .UNSPECIFIED.);
#2633=B_SPLINE_CURVE_WITH_KNOTS('',3,(#92675,#92676,#92677,#92678,#92679,
#92680,#92681,#92682,#92683,#92684,#92685,#92686,#92687,#92688,#92689,#92690,
#92691,#92692,#92693,#92694,#92695,#92696,#92697,#92698,#92699,#92700,#92701,
#92702,#92703,#92704,#92705,#92706,#92707,#92708,#92709,#92710,#92711,#92712,
#92713,#92714,#92715,#92716,#92717,#92718,#92719,#92720,#92721,#92722,#92723,
#92724,#92725,#92726,#92727,#92728,#92729,#92730,#92731,#92732),
 .UNSPECIFIED.,.F.,.F.,(4,3,3,3,3,3,3,3,3,3,3,3,3,3,3,3,3,3,3,4),(13.8761929171444,
13.9801050982006,14.0838619923275,14.1874971548373,14.2910675742173,14.394608424291,
14.4981548361472,14.6018082710274,14.7055227330307,14.809410594129,14.8542235792949,
14.9609410403274,15.0635681563456,15.1661013721572,15.2685772451739,15.3710322505032,
15.473554455726,15.5761173374535,15.6788162095048,15.7079632675546),
 .UNSPECIFIED.);
#2634=B_SPLINE_CURVE_WITH_KNOTS('',3,(#92733,#92734,#92735,#92736,#92737,
#92738,#92739,#92740,#92741,#92742,#92743,#92744,#92745,#92746,#92747,#92748,
#92749,#92750,#92751,#92752,#92753,#92754,#92755,#92756,#92757,#92758,#92759,
#92760,#92761,#92762,#92763,#92764,#92765,#92766,#92767,#92768,#92769,#92770,
#92771,#92772,#92773,#92774,#92775,#92776,#92777,#92778,#92779,#92780,#92781,
#92782,#92783,#92784,#92785,#92786,#92787,#92788,#92789,#92790,#92791,#92792,
#92793,#92794,#92795,#92796,#92797,#92798,#92799),.UNSPECIFIED.,.F.,.F.,
(4,3,3,3,3,3,3,3,3,3,3,3,3,3,3,3,3,3,3,3,3,3,4),(15.7079632679489,15.851771437641,
15.9558439456397,16.0597595638296,16.1635512471327,16.2672763592019,16.3709698524584,
16.4746666348114,16.5784717372559,16.6823352983937,16.7863815022145,16.8493192959871,
16.9535243733574,17.0575742377897,17.1615020099112,17.2653642764257,17.3691957876541,
17.4730312504175,17.5769750939415,17.6809776424981,17.7851617143139,17.8468671543332,
17.9343900068785),.UNSPECIFIED.);
#2635=B_SPLINE_CURVE_WITH_KNOTS('',3,(#92805,#92806,#92807,#92808,#92809,
#92810,#92811,#92812),.UNSPECIFIED.,.F.,.F.,(4,1,1,1,1,4),(99.6151611513019,
99.6457915387123,100.643339397058,101.640887255404,102.638435113751,103.635982972097),
 .UNSPECIFIED.);
#2636=B_SPLINE_CURVE_WITH_KNOTS('',3,(#92816,#92817,#92818,#92819,#92820,
#92821,#92822,#92823,#92824,#92825,#92826,#92827,#92828,#92829,#92830,#92831),
 .UNSPECIFIED.,.F.,.F.,(4,3,3,3,3,4),(103.672557568829,103.780299930425,
103.88830919533,103.996463610122,104.104895341938,104.157833394917),
 .UNSPECIFIED.);
#2637=B_SPLINE_CURVE_WITH_KNOTS('',3,(#92832,#92833,#92834,#92835,#92836,
#92837,#92838,#92839,#92840,#92841,#92842,#92843,#92844,#92845,#92846,#92847,
#92848,#92849,#92850,#92851,#92852,#92853,#92854,#92855,#92856,#92857,#92858,
#92859,#92860,#92861,#92862,#92863,#92864,#92865,#92866,#92867,#92868,#92869,
#92870,#92871,#92872,#92873,#92874,#92875,#92876,#92877,#92878,#92879,#92880,
#92881,#92882,#92883,#92884,#92885,#92886,#92887,#92888,#92889,#92890,#92891,
#92892,#92893,#92894,#92895,#92896,#92897,#92898,#92899,#92900,#92901,#92902,
#92903,#92904,#92905,#92906,#92907,#92908,#92909,#92910,#92911,#92912,#92913,
#92914,#92915,#92916,#92917,#92918,#92919,#92920,#92921,#92922,#92923,#92924,
#92925,#92926,#92927,#92928,#92929,#92930,#92931,#92932,#92933,#92934,#92935,
#92936,#92937,#92938,#92939,#92940,#92941,#92942,#92943,#92944,#92945,#92946,
#92947,#92948,#92949,#92950,#92951,#92952,#92953,#92954,#92955),
 .UNSPECIFIED.,.F.,.F.,(4,3,3,3,3,3,3,3,3,3,3,3,3,3,3,3,3,3,3,3,3,3,3,3,
3,3,3,3,3,3,3,3,3,3,3,3,3,3,3,3,3,4),(99.6156213899676,99.719451702261,
99.8232891842525,99.9272369878061,100.03124639439,100.135434233686,100.18725683054,
100.291455310788,100.395498815188,100.499420609254,100.603277136689,100.707103155531,
100.810933380572,100.914872410489,101.018870377466,101.123050283818,101.184804688886,
101.288885178202,101.392810145172,101.496613161362,101.600350824598,101.704058066099,
101.807769773832,101.911591496786,102.015472659481,102.119537827642,102.182352547233,
102.286721401994,102.390934579093,102.495024194029,102.599047303358,102.703038423928,
102.807032027915,102.911130699731,103.015286432589,103.119619455548,103.179900405579,
103.289272719893,103.398334669506,103.507209075267,103.615853248157,103.672557568463),
 .UNSPECIFIED.);
#2638=B_SPLINE_CURVE_WITH_KNOTS('',3,(#92961,#92962,#92963,#92964,#92965,
#92966,#92967,#92968,#92969,#92970,#92971,#92972,#92973,#92974,#92975,#92976,
#92977,#92978,#92979,#92980,#92981,#92982,#92983,#92984,#92985,#92986,#92987,
#92988,#92989,#92990,#92991,#92992,#92993,#92994,#92995,#92996,#92997,#92998,
#92999,#93000,#93001,#93002,#93003,#93004,#93005,#93006,#93007,#93008,#93009,
#93010,#93011,#93012,#93013,#93014,#93015,#93016,#93017,#93018,#93019,#93020,
#93021,#93022,#93023,#93024,#93025,#93026,#93027,#93028,#93029,#93030,#93031,
#93032,#93033,#93034,#93035,#93036,#93037,#93038,#93039,#93040,#93041,#93042,
#93043,#93044,#93045,#93046,#93047,#93048,#93049,#93050,#93051,#93052,#93053,
#93054,#93055,#93056,#93057,#93058,#93059,#93060,#93061,#93062,#93063,#93064,
#93065,#93066,#93067,#93068,#93069,#93070,#93071,#93072,#93073,#93074,#93075,
#93076,#93077,#93078,#93079,#93080,#93081,#93082,#93083,#93084,#93085,#93086,
#93087),.UNSPECIFIED.,.F.,.F.,(4,3,3,3,3,3,3,3,3,3,3,3,3,3,3,3,3,3,3,3,
3,3,3,3,3,3,3,3,3,3,3,3,3,3,3,3,3,3,3,3,3,3,4),(93.3317451830118,93.4356908335088,
93.539708921792,93.6438957414934,93.6605043886357,93.7646924917536,93.868725346352,
93.9726361419404,94.076481462347,94.1802960840316,94.28411474,94.3880420220064,
94.4920281226445,94.5961961074607,94.6580522469818,94.7622408524121,94.8662742508428,
94.9701856485116,95.0740316065126,95.1778469000452,95.2816662608905,95.3855942926708,
95.489581169514,95.5937499633514,95.6556001053279,95.7597729568001,95.8637905433978,
95.9676861197645,96.071516259166,96.1753157600107,96.279119377306,96.3830318486896,
96.4870032449124,96.5911568522755,96.653147963674,96.7562452951427,96.8592012753662,
96.9620522837591,97.0688822781402,97.1716574277158,97.2744331495273,97.3772781459456,
97.3893722612836),.UNSPECIFIED.);
#2639=B_SPLINE_CURVE_WITH_KNOTS('',3,(#93088,#93089,#93090,#93091,#93092,
#93093),.UNSPECIFIED.,.F.,.F.,(4,1,1,4),(97.3893747333975,97.6506958220201,
98.6482436803662,99.6151611513019),.UNSPECIFIED.);
#2640=B_SPLINE_CURVE_WITH_KNOTS('',3,(#93095,#93096,#93097,#93098,#93099,
#93100,#93101,#93102,#93103,#93104,#93105,#93106,#93107,#93108,#93109,#93110,
#93111,#93112,#93113,#93114,#93115,#93116,#93117,#93118,#93119,#93120,#93121,
#93122,#93123,#93124,#93125,#93126,#93127,#93128,#93129,#93130,#93131,#93132,
#93133,#93134,#93135,#93136,#93137,#93138,#93139,#93140,#93141,#93142,#93143,
#93144,#93145,#93146,#93147,#93148,#93149,#93150,#93151,#93152,#93153,#93154,
#93155,#93156,#93157,#93158,#93159,#93160,#93161),.UNSPECIFIED.,.F.,.F.,
(4,3,3,3,3,3,3,3,3,3,3,3,3,3,3,3,3,3,3,3,3,3,4),(97.3893722616848,97.4918516969082,
97.5942418193773,97.6965792942248,97.7989007101473,97.901312936064,98.0037693753309,
98.1064097553564,98.1921611138482,98.2963339822745,98.4003515858491,98.5042471791462,
98.6080773354404,98.7118768531167,98.8156804871574,98.9195929750428,99.0235643876549,
99.1277180110528,99.1897089721943,99.2961870766376,99.4002195153588,99.5079204526632,
99.6156213899676),.UNSPECIFIED.);
#2641=B_SPLINE_CURVE_WITH_KNOTS('',3,(#93162,#93163,#93164,#93165,#93166,
#93167,#93168,#93169,#93170,#93171,#93172,#93173,#93174,#93175,#93176,#93177,
#93178,#93179,#93180,#93181,#93182,#93183,#93184,#93185,#93186,#93187,#93188,
#93189,#93190,#93191,#93192,#93193,#93194,#93195,#93196,#93197,#93198,#93199,
#93200,#93201,#93202,#93203,#93204,#93205,#93206,#93207,#93208,#93209,#93210,
#93211,#93212,#93213,#93214,#93215,#93216,#93217,#93218,#93219,#93220,#93221,
#93222,#93223,#93224,#93225,#93226,#93227,#93228,#93229,#93230,#93231,#93232,
#93233,#93234,#93235,#93236,#93237,#93238,#93239,#93240,#93241,#93242,#93243,
#93244,#93245,#93246,#93247,#93248,#93249,#93250,#93251,#93252,#93253,#93254,
#93255,#93256,#93257,#93258,#93259,#93260,#93261,#93262,#93263,#93264,#93265,
#93266,#93267,#93268,#93269,#93270,#93271,#93272,#93273,#93274,#93275,#93276,
#93277,#93278,#93279,#93280,#93281,#93282,#93283,#93284,#93285),
 .UNSPECIFIED.,.F.,.F.,(4,3,3,3,3,3,3,3,3,3,3,3,3,3,3,3,3,3,3,3,3,3,3,3,
3,3,3,3,3,3,3,3,3,3,3,3,3,3,3,3,3,4),(93.3327249610222,93.4413805509524,
93.5452680358632,93.6490996829472,93.7529102555451,93.8567344832209,93.9606732647267,
94.0646795135131,94.1688591274354,94.2019696804638,94.3061562454964,94.4101875758906,
94.5140968748872,94.6179407165043,94.7217538792165,94.8255710980645,94.9294969858512,
95.033481714353,95.1376483765647,95.1995175388099,95.303702070536,95.4077313618506,
95.511638623033,95.6154804287179,95.7192915603578,95.8231067559746,95.9270306463741,
96.0310133890498,96.1351781052391,96.197065397156,96.3012534986124,96.4052863515668,
96.5091971455439,96.6130424643603,96.716857084478,96.8206757389046,96.9246030194181,
97.0285891185885,97.1327571019925,97.1946132555021,97.345607244739,97.3893722612836),
 .UNSPECIFIED.);
#2642=B_SPLINE_CURVE_WITH_KNOTS('',3,(#93291,#93292,#93293,#93294,#93295,
#93296,#93297,#93298,#93299,#93300,#93301,#93302,#93303,#93304,#93305,#93306,
#93307,#93308,#93309,#93310,#93311,#93312,#93313,#93314,#93315,#93316,#93317,
#93318,#93319,#93320,#93321,#93322,#93323,#93324,#93325,#93326,#93327,#93328,
#93329,#93330,#93331,#93332,#93333,#93334,#93335,#93336,#93337,#93338,#93339,
#93340,#93341,#93342,#93343,#93344,#93345,#93346,#93347,#93348,#93349,#93350,
#93351,#93352,#93353,#93354,#93355,#93356,#93357,#93358,#93359,#93360,#93361,
#93362,#93363,#93364,#93365,#93366,#93367,#93368,#93369,#93370,#93371,#93372,
#93373,#93374,#93375,#93376,#93377,#93378,#93379,#93380,#93381,#93382,#93383,
#93384,#93385,#93386,#93387,#93388,#93389,#93390,#93391,#93392,#93393,#93394,
#93395,#93396,#93397,#93398,#93399,#93400,#93401,#93402,#93403,#93404,#93405,
#93406,#93407,#93408,#93409,#93410,#93411),.UNSPECIFIED.,.F.,.F.,(4,3,3,
3,3,3,3,3,3,3,3,3,3,3,3,3,3,3,3,3,3,3,3,3,3,3,3,3,3,3,3,3,3,3,3,3,3,3,3,
3,4),(87.0493933608437,87.1532149139967,87.2570257238478,87.3615736025257,
87.4655294029247,87.5703733207419,87.6752172385592,87.7794034175018,87.8834343579763,
87.9873432633011,88.091186709151,88.194999474602,88.2988162952939,88.4027417863365,
88.5067261182931,88.6108923886106,88.6727650969053,88.7769513208729,88.8809823069786,
88.9848912586063,89.0887347511468,89.1925475636041,89.2963644315469,89.4002899698799,
89.5042743492206,89.6084406665499,89.6703129552514,89.7744989225328,89.8785296514156,
89.9824383462603,90.0862815824279,90.1900941392956,90.293910752806,90.3978360402153,
90.5018201702324,90.6059862434675,90.6678608135975,90.7807057008014,90.8932647263971,
91.0053646978595,91.1061869538111),.UNSPECIFIED.);
#2643=B_SPLINE_CURVE_WITH_KNOTS('',3,(#93412,#93413,#93414,#93415,#93416,
#93417,#93418,#93419,#93420,#93421,#93422,#93423,#93424,#93425,#93426,#93427,
#93428,#93429,#93430,#93431,#93432,#93433,#93434,#93435,#93436,#93437,#93438,
#93439,#93440,#93441,#93442,#93443,#93444,#93445,#93446,#93447,#93448,#93449,
#93450,#93451,#93452,#93453,#93454,#93455,#93456,#93457,#93458,#93459,#93460,
#93461,#93462,#93463,#93464,#93465,#93466,#93467,#93468,#93469,#93470,#93471,
#93472,#93473,#93474,#93475,#93476,#93477,#93478,#93479,#93480,#93481),
 .UNSPECIFIED.,.F.,.F.,(4,3,3,3,3,3,3,3,3,3,3,3,3,3,3,3,3,3,3,3,3,3,3,4),
(91.106186954104,91.2125697915894,91.3190338862199,91.4256928890665,91.5324648457377,
91.6394568072871,91.6654086719436,91.7695952380118,91.8736265694479,91.977535869491,
92.0813797121567,92.1851928759182,92.2890100958143,92.3929359846407,92.4969207141789,
92.6010873774105,92.6629565302897,92.7671206832539,92.8711399649714,92.9750493921735,
93.0788929406494,93.1826980509479,93.2865285969047,93.3317451830118),
 .UNSPECIFIED.);
#2644=B_SPLINE_CURVE_WITH_KNOTS('',3,(#93483,#93484,#93485,#93486,#93487,
#93488,#93489,#93490,#93491,#93492,#93493,#93494,#93495,#93496,#93497,#93498,
#93499,#93500,#93501,#93502,#93503,#93504,#93505,#93506,#93507,#93508,#93509,
#93510,#93511,#93512,#93513,#93514,#93515,#93516,#93517,#93518,#93519,#93520,
#93521,#93522,#93523,#93524,#93525,#93526,#93527,#93528,#93529,#93530,#93531,
#93532,#93533,#93534,#93535,#93536,#93537,#93538,#93539,#93540,#93541,#93542,
#93543,#93544,#93545,#93546,#93547,#93548,#93549,#93550,#93551,#93552),
 .UNSPECIFIED.,.F.,.F.,(4,3,3,3,3,3,3,3,3,3,3,3,3,3,3,3,3,3,3,3,3,3,3,4),
(91.106186954104,91.2093261054256,91.3135123292234,91.4175433151588,91.5214522666154,
91.6252957589846,91.7291085712708,91.8329254390422,91.9368509772058,92.0408353563778,
92.1450016735413,92.2068739637717,92.3110599314537,92.4150906607374,92.5189993559811,
92.6228425925464,92.7266551498102,92.830471763714,92.9343970515104,93.0383811819116,
93.1425472555219,93.2044218221178,93.3086061887592,93.3327249610222),
 .UNSPECIFIED.);
#2645=B_SPLINE_CURVE_WITH_KNOTS('',3,(#93553,#93554,#93555,#93556,#93557,
#93558,#93559,#93560,#93561,#93562,#93563,#93564,#93565,#93566,#93567,#93568,
#93569,#93570,#93571,#93572,#93573,#93574,#93575,#93576,#93577,#93578,#93579,
#93580,#93581,#93582,#93583,#93584,#93585,#93586,#93587,#93588,#93589,#93590,
#93591,#93592,#93593,#93594,#93595,#93596,#93597,#93598,#93599,#93600,#93601,
#93602,#93603,#93604,#93605,#93606,#93607,#93608,#93609,#93610,#93611,#93612,
#93613,#93614,#93615,#93616,#93617,#93618,#93619,#93620,#93621,#93622,#93623,
#93624,#93625,#93626,#93627,#93628,#93629,#93630,#93631,#93632,#93633,#93634,
#93635,#93636,#93637,#93638,#93639,#93640,#93641,#93642,#93643,#93644,#93645,
#93646,#93647,#93648,#93649,#93650,#93651,#93652,#93653,#93654,#93655,#93656,
#93657,#93658,#93659,#93660,#93661,#93662,#93663,#93664,#93665,#93666,#93667,
#93668,#93669,#93670,#93671,#93672,#93673,#93674,#93675,#93676),
 .UNSPECIFIED.,.F.,.F.,(4,3,3,3,3,3,3,3,3,3,3,3,3,3,3,3,3,3,3,3,3,3,3,3,
3,3,3,3,3,3,3,3,3,3,3,3,3,3,3,3,3,4),(87.0484495580493,87.1526139555506,
87.2191346720412,87.323320836556,87.4273517627698,87.5312606541471,87.6351040862496,
87.7389168381718,87.8427336455723,87.946659123773,88.0506434431219,88.1548097013355,
88.2166825303873,88.3208687024162,88.4248996362149,88.5288085352445,88.6326519750365,
88.736464734674,88.8402815498039,88.9442070357016,89.0481913627408,89.1523576285501,
89.2142303887334,89.3184165292485,89.4224474314894,89.5263562990473,89.6301997074378,
89.7340124357895,89.8378292197948,89.9417546750267,90.0457389716127,90.1499052076343,
90.2117782470795,90.3146405331901,90.4173275668862,90.5199168474419,90.6224448805545,
90.7249480861439,90.8275243015791,90.9301370935116,91.0329109698248,91.1061869536426),
 .UNSPECIFIED.);
#2646=B_SPLINE_CURVE_WITH_KNOTS('',3,(#93682,#93683,#93684,#93685,#93686,
#93687,#93688,#93689,#93690,#93691,#93692,#93693,#93694,#93695,#93696,#93697,
#93698,#93699,#93700,#93701,#93702,#93703,#93704,#93705,#93706,#93707,#93708,
#93709,#93710,#93711,#93712,#93713,#93714,#93715,#93716,#93717,#93718,#93719,
#93720,#93721,#93722,#93723,#93724,#93725,#93726,#93727,#93728,#93729,#93730,
#93731,#93732,#93733,#93734,#93735,#93736,#93737,#93738,#93739,#93740,#93741,
#93742,#93743,#93744,#93745,#93746,#93747,#93748,#93749,#93750,#93751,#93752,
#93753,#93754,#93755,#93756,#93757,#93758,#93759,#93760,#93761,#93762,#93763,
#93764,#93765,#93766,#93767,#93768,#93769,#93770,#93771,#93772,#93773,#93774,
#93775,#93776,#93777,#93778,#93779,#93780,#93781,#93782,#93783,#93784,#93785,
#93786,#93787,#93788,#93789,#93790,#93791,#93792,#93793,#93794,#93795,#93796,
#93797,#93798,#93799,#93800,#93801,#93802),.UNSPECIFIED.,.F.,.F.,(4,3,3,
3,3,3,3,3,3,3,3,3,3,3,3,3,3,3,3,3,3,3,3,3,3,3,3,3,3,3,3,3,3,3,3,3,3,3,3,
3,4),(80.7662008530864,80.8702730497271,80.9742075957574,81.0780665246705,
81.1818846348487,81.2856966710118,81.389610872242,81.4935748160271,81.5977303348073,
81.6899300884827,81.7941162519913,81.8981471772207,82.0020560676502,82.1058994988279,
82.2097122498495,82.3135290563748,82.4174545337446,82.5214388522863,82.6256051097386,
82.6874779468288,82.7916641114806,82.8956950378613,82.9996039294484,83.103447361787,
83.2072601139711,83.3110769216587,83.4150024001824,83.518986719875,83.6231529784611,
83.6850258051749,83.7892119660234,83.893242888598,83.9971517763933,84.1009952049509,
84.2048079533701,84.3086247573145,84.4125502321539,84.5165345481899,84.6207008032023,
84.682573663521,84.8230016469244),.UNSPECIFIED.);
#2647=B_SPLINE_CURVE_WITH_KNOTS('',3,(#93803,#93804,#93805,#93806,#93807,
#93808,#93809,#93810,#93811,#93812,#93813,#93814,#93815,#93816,#93817,#93818,
#93819,#93820,#93821,#93822,#93823,#93824,#93825,#93826,#93827,#93828,#93829,
#93830,#93831,#93832,#93833,#93834,#93835,#93836,#93837,#93838,#93839,#93840,
#93841,#93842,#93843,#93844,#93845,#93846,#93847,#93848,#93849,#93850,#93851,
#93852,#93853,#93854,#93855,#93856,#93857,#93858,#93859,#93860,#93861,#93862,
#93863,#93864,#93865,#93866,#93867,#93868,#93869,#93870,#93871,#93872),
 .UNSPECIFIED.,.F.,.F.,(4,3,3,3,3,3,3,3,3,3,3,3,3,3,3,3,3,3,3,3,3,3,3,4),
(84.8230016473375,84.9301416316537,85.0325714163376,85.1349307980759,85.2372563959065,
85.3395847767837,85.4420166361939,85.5445096330566,85.6471710557298,85.6801215218671,
85.7843076939228,85.8883386277482,85.9922475268047,86.0960909666236,86.199903726288,
86.3037205414444,86.4076460273685,86.5116303544343,86.6157966202695,86.6776693802131,
86.7818282235991,86.8858513473607,86.9897582187876,87.0493933608437),
 .UNSPECIFIED.);
#2648=B_SPLINE_CURVE_WITH_KNOTS('',3,(#93874,#93875,#93876,#93877,#93878,
#93879,#93880,#93881,#93882,#93883,#93884,#93885,#93886,#93887,#93888,#93889,
#93890,#93891,#93892,#93893,#93894,#93895,#93896,#93897,#93898,#93899,#93900,
#93901,#93902,#93903,#93904,#93905,#93906,#93907,#93908,#93909,#93910,#93911,
#93912,#93913,#93914,#93915,#93916,#93917,#93918,#93919,#93920,#93921,#93922,
#93923,#93924,#93925,#93926,#93927,#93928,#93929,#93930,#93931,#93932,#93933,
#93934,#93935,#93936,#93937,#93938,#93939,#93940),.UNSPECIFIED.,.F.,.F.,
(4,3,3,3,3,3,3,3,3,3,3,3,3,3,3,3,3,3,3,3,3,3,4),(84.8230016473347,84.9376554440836,
85.0527190382934,85.1683359285703,85.2240389553491,85.3282251199969,85.4322560463736,
85.5361649379567,85.6400083702913,85.7438211224714,85.847637930155,85.9515634086748,
86.0555477283636,86.1597139869458,86.2215868136951,86.3257394090933,86.4297517345021,
86.5336587825648,86.6374954230147,86.7413356739134,86.8451704422707,86.9491112691339,
87.0484495580493),.UNSPECIFIED.);
#2649=B_SPLINE_CURVE_WITH_KNOTS('',3,(#93941,#93942,#93943,#93944,#93945,
#93946,#93947,#93948,#93949,#93950,#93951,#93952,#93953,#93954,#93955,#93956,
#93957,#93958,#93959,#93960,#93961,#93962,#93963,#93964,#93965,#93966,#93967,
#93968,#93969,#93970,#93971,#93972,#93973,#93974,#93975,#93976,#93977,#93978,
#93979,#93980,#93981,#93982,#93983,#93984,#93985,#93986,#93987,#93988,#93989,
#93990,#93991,#93992,#93993,#93994,#93995,#93996,#93997,#93998,#93999,#94000,
#94001,#94002,#94003,#94004,#94005,#94006,#94007,#94008,#94009,#94010,#94011,
#94012,#94013,#94014,#94015,#94016,#94017,#94018,#94019,#94020,#94021,#94022,
#94023,#94024,#94025,#94026,#94027,#94028,#94029,#94030,#94031,#94032,#94033,
#94034,#94035,#94036,#94037,#94038,#94039,#94040,#94041,#94042,#94043,#94044,
#94045,#94046,#94047,#94048,#94049,#94050,#94051,#94052,#94053,#94054,#94055,
#94056,#94057,#94058,#94059,#94060,#94061,#94062,#94063,#94064),
 .UNSPECIFIED.,.F.,.F.,(4,3,3,3,3,3,3,3,3,3,3,3,3,3,3,3,3,3,3,3,3,3,3,3,
3,3,3,3,3,3,3,3,3,3,3,3,3,3,3,3,3,4),(80.7657457648301,80.8695647156208,
80.9734943498133,81.0774857297398,81.1816561023789,81.2338475219647,81.3380336854432,
81.4420646106447,81.5459735010509,81.6498169322079,81.7536296832115,81.8574464897212,
81.9613719670797,82.0653562856124,82.1695225430592,82.2313953803108,82.3355815439513,
82.4396124693163,82.5435213598861,82.6473647912069,82.7511775423742,82.8549943490479,
82.9589198265682,83.0629041452623,83.1670704028679,83.2289432386569,83.3331294018511,
83.4371603267697,83.5410692168954,83.6449126477737,83.7487253985006,83.8525422047368,
83.956467681827,84.0604520000942,84.1646182572832,84.226491097003,84.3322636668447,
84.4378652902381,84.5433026045803,84.6486432044876,84.7539210445285,84.8230016469244),
 .UNSPECIFIED.);
#2650=B_SPLINE_CURVE_WITH_KNOTS('',3,(#94070,#94071,#94072,#94073,#94074,
#94075,#94076,#94077,#94078,#94079,#94080,#94081,#94082,#94083,#94084,#94085,
#94086,#94087,#94088,#94089,#94090,#94091,#94092,#94093,#94094,#94095,#94096,
#94097,#94098,#94099,#94100,#94101,#94102,#94103,#94104,#94105,#94106,#94107,
#94108,#94109,#94110,#94111,#94112,#94113,#94114,#94115,#94116,#94117,#94118,
#94119,#94120,#94121,#94122,#94123,#94124,#94125,#94126,#94127,#94128,#94129,
#94130,#94131,#94132,#94133,#94134,#94135,#94136,#94137,#94138,#94139,#94140,
#94141,#94142,#94143,#94144,#94145,#94146,#94147,#94148,#94149,#94150,#94151,
#94152,#94153,#94154,#94155,#94156,#94157,#94158,#94159,#94160,#94161,#94162,
#94163,#94164,#94165,#94166,#94167,#94168,#94169,#94170,#94171,#94172,#94173,
#94174,#94175,#94176,#94177,#94178,#94179,#94180,#94181,#94182,#94183,#94184,
#94185,#94186,#94187,#94188,#94189,#94190,#94191,#94192,#94193,#94194,#94195,
#94196),.UNSPECIFIED.,.F.,.F.,(4,3,3,3,3,3,3,3,3,3,3,3,3,3,3,3,3,3,3,3,
3,3,3,3,3,3,3,3,3,3,3,3,3,3,3,3,3,3,3,3,3,3,4),(74.4820629789471,74.5860824450287,
74.6902706747757,74.7070950800601,74.811281243545,74.9153121687539,75.0192210591676,
75.1230644903326,75.2268772413443,75.3306940478627,75.43461952523,75.5386038437718,
75.6427701012281,75.7046429384062,75.8088291018917,75.9128600271012,76.0167689175154,
76.1206123486807,76.2244250996928,76.3282419062114,76.4321673835789,76.5361517021208,
76.6403179595772,76.7021907967523,76.80637696026,76.9104078854918,77.0143167759283,
77.1181602071159,77.2219729581504,77.3257897646913,77.4297152420809,77.5336995606446,
77.6378658181225,77.6997386550984,77.8047483656344,77.9072108121793,78.0095758369578,
78.1118801627626,78.2188642069186,78.3212057260089,78.4235870713419,78.5260937326297,
78.5398163393865),.UNSPECIFIED.);
#2651=B_SPLINE_CURVE_WITH_KNOTS('',3,(#94197,#94198,#94199,#94200,#94201,
#94202,#94203,#94204,#94205,#94206,#94207,#94208,#94209,#94210,#94211,#94212,
#94213,#94214,#94215,#94216,#94217,#94218,#94219,#94220,#94221,#94222,#94223,
#94224,#94225,#94226,#94227,#94228,#94229,#94230,#94231,#94232,#94233,#94234,
#94235,#94236,#94237,#94238,#94239,#94240,#94241,#94242,#94243,#94244,#94245,
#94246,#94247,#94248,#94249,#94250,#94251,#94252,#94253,#94254,#94255,#94256,
#94257,#94258,#94259,#94260,#94261,#94262,#94263),.UNSPECIFIED.,.F.,.F.,
(4,3,3,3,3,3,3,3,3,3,3,3,3,3,3,3,3,3,3,3,3,3,4),(78.5398163397448,78.6972865134445,
78.8014726769225,78.905503602124,79.0094124925299,79.1132559236866,79.2170686746898,
79.3208854811994,79.4248109585574,79.5287952770896,79.6329615345361,79.6948343717905,
79.7990205354316,79.9030514607972,80.0069603513676,80.1108037826891,80.2146165338571,
80.3184333405311,80.4223588180522,80.5263431367468,80.630509394353,80.6923822301366,
80.7662008530864),.UNSPECIFIED.);
#2652=B_SPLINE_CURVE_WITH_KNOTS('',3,(#94265,#94266,#94267,#94268,#94269,
#94270,#94271,#94272,#94273,#94274,#94275,#94276,#94277,#94278,#94279,#94280,
#94281,#94282,#94283,#94284,#94285,#94286,#94287,#94288,#94289,#94290,#94291,
#94292,#94293,#94294,#94295,#94296,#94297,#94298,#94299,#94300,#94301,#94302,
#94303,#94304,#94305,#94306,#94307,#94308,#94309,#94310,#94311,#94312,#94313,
#94314,#94315,#94316,#94317,#94318,#94319,#94320,#94321,#94322,#94323,#94324,
#94325,#94326,#94327,#94328,#94329,#94330,#94331),.UNSPECIFIED.,.F.,.F.,
(4,3,3,3,3,3,3,3,3,3,3,3,3,3,3,3,3,3,3,3,3,3,4),(78.5398163397448,78.6430480181522,
78.7462408136019,78.8494302891154,78.9527248465537,79.056073050004,79.159611215967,
79.2387518052725,79.3429379687801,79.4469688940118,79.5508777844482,79.6547212156358,
79.7585339666699,79.8623507732107,79.9662762506001,80.0702605691636,80.1744268266413,
80.2362996636186,80.3404816769733,80.4467976989375,80.550702681629,80.6582242232296,
80.7657457648301),.UNSPECIFIED.);
#2653=B_SPLINE_CURVE_WITH_KNOTS('',3,(#94332,#94333,#94334,#94335,#94336,
#94337,#94338,#94339,#94340,#94341,#94342,#94343,#94344,#94345,#94346,#94347,
#94348,#94349,#94350,#94351,#94352,#94353,#94354,#94355,#94356,#94357,#94358,
#94359,#94360,#94361,#94362,#94363,#94364,#94365,#94366,#94367,#94368,#94369,
#94370,#94371,#94372,#94373,#94374,#94375,#94376,#94377,#94378,#94379,#94380,
#94381,#94382,#94383,#94384,#94385,#94386,#94387,#94388,#94389,#94390,#94391,
#94392,#94393,#94394,#94395,#94396,#94397,#94398,#94399,#94400,#94401,#94402,
#94403,#94404,#94405,#94406,#94407,#94408,#94409,#94410,#94411,#94412,#94413,
#94414,#94415,#94416,#94417,#94418,#94419,#94420,#94421,#94422,#94423,#94424,
#94425,#94426,#94427,#94428,#94429,#94430,#94431,#94432,#94433,#94434,#94435,
#94436,#94437,#94438,#94439,#94440,#94441,#94442,#94443,#94444,#94445,#94446,
#94447,#94448,#94449,#94450,#94451,#94452,#94453,#94454,#94455),
 .UNSPECIFIED.,.F.,.F.,(4,3,3,3,3,3,3,3,3,3,3,3,3,3,3,3,3,3,3,3,3,3,3,3,
3,3,3,3,3,3,3,3,3,3,3,3,3,3,3,3,3,4),(74.4832444132594,74.5871350869426,
74.6909683424548,74.7947789457462,74.8986016274051,75.0025379180133,75.1065402590823,
75.210717341976,75.2485603718882,75.3527465353761,75.4567774605879,75.5606863510045,
75.6645297821723,75.7683425331867,75.8721593397079,75.9760848170779,76.0800691356223,
76.1842353930812,76.2461082302343,76.3502943937249,76.4543253189398,76.5582342093591,
76.6620776405297,76.7658903915471,76.8697071980708,76.9736326754436,77.0776169939906,
77.1817832514521,77.2436560885804,77.3478422520653,77.4518731772742,77.5557820676879,
77.6596254988527,77.7634382498646,77.8672550563835,77.9711805337506,78.0751648522923,
78.1793311097485,78.2412039469264,78.3682032551823,78.4934616304658,78.5398163394195),
 .UNSPECIFIED.);
#2654=B_SPLINE_CURVE_WITH_KNOTS('',3,(#94461,#94462,#94463,#94464,#94465,
#94466,#94467,#94468,#94469,#94470,#94471,#94472,#94473,#94474,#94475,#94476,
#94477,#94478,#94479,#94480,#94481,#94482,#94483,#94484,#94485,#94486,#94487,
#94488,#94489,#94490,#94491,#94492,#94493,#94494,#94495,#94496,#94497,#94498,
#94499,#94500,#94501,#94502,#94503,#94504,#94505,#94506,#94507,#94508,#94509,
#94510,#94511,#94512,#94513,#94514,#94515,#94516,#94517,#94518,#94519,#94520,
#94521,#94522,#94523,#94524,#94525,#94526,#94527,#94528,#94529,#94530,#94531,
#94532,#94533,#94534,#94535,#94536,#94537,#94538,#94539,#94540,#94541,#94542,
#94543,#94544,#94545,#94546,#94547,#94548,#94549,#94550,#94551,#94552,#94553,
#94554,#94555,#94556,#94557,#94558,#94559,#94560,#94561,#94562,#94563,#94564,
#94565,#94566,#94567,#94568,#94569,#94570,#94571,#94572,#94573,#94574,#94575,
#94576,#94577,#94578,#94579,#94580,#94581),.UNSPECIFIED.,.F.,.F.,(4,3,3,
3,3,3,3,3,3,3,3,3,3,3,3,3,3,3,3,3,3,3,3,3,3,3,3,3,3,3,3,3,3,3,3,3,3,3,3,
3,4),(68.199542273107,68.3033530889066,68.4079667991759,68.5119225050548,
68.6168652175192,68.7218079299836,68.8259940934717,68.9300250186838,69.0339339091007,
69.1377773402688,69.2415900912837,69.3454068978053,69.4493323751756,69.5533166937204,
69.6574829511797,69.7193557883297,69.8235419518178,69.9275728770296,70.0314817674465,
70.1353251986146,70.2391379496294,70.342954756151,70.4468802335214,70.5508645520662,
70.6550308095254,70.7169036466757,70.8210898101641,70.9251207353764,71.0290296257936,
71.1328730569619,71.2366858079772,71.340502614499,71.4444280918697,71.5484124104147,
71.6525786678742,71.7144515050218,71.8220784528947,71.9307165978123,72.0379272940099,
72.1472791632875,72.2566310325652),.UNSPECIFIED.);
#2655=B_SPLINE_CURVE_WITH_KNOTS('',3,(#94582,#94583,#94584,#94585,#94586,
#94587,#94588,#94589,#94590,#94591,#94592,#94593,#94594,#94595,#94596,#94597,
#94598,#94599,#94600,#94601,#94602,#94603,#94604,#94605,#94606,#94607,#94608,
#94609,#94610,#94611,#94612,#94613,#94614,#94615,#94616,#94617,#94618,#94619,
#94620,#94621,#94622,#94623,#94624,#94625,#94626,#94627,#94628,#94629,#94630,
#94631,#94632,#94633,#94634,#94635,#94636,#94637,#94638,#94639,#94640,#94641,
#94642,#94643,#94644,#94645,#94646,#94647,#94648),.UNSPECIFIED.,.F.,.F.,
(4,3,3,3,3,3,3,3,3,3,3,3,3,3,3,3,3,3,3,3,3,3,4),(72.2566310330023,72.3704731155937,
72.481813311248,72.5969063373079,72.7119993633679,72.8161855268555,72.920216452067,
73.0241253424834,73.127968773651,73.2317815246655,73.3355983311864,73.4395238085563,
73.5435081271006,73.6476743845593,73.709547221714,73.8137037283056,73.9177183843865,
74.0216261896493,74.125462018442,74.2292882433997,74.3331083610436,74.4370016429364,
74.4820629789471),.UNSPECIFIED.);
#2656=B_SPLINE_CURVE_WITH_KNOTS('',3,(#94650,#94651,#94652,#94653,#94654,
#94655,#94656,#94657,#94658,#94659,#94660,#94661,#94662,#94663,#94664,#94665,
#94666,#94667,#94668,#94669,#94670,#94671,#94672,#94673,#94674,#94675,#94676,
#94677,#94678,#94679,#94680,#94681,#94682,#94683,#94684,#94685,#94686,#94687,
#94688,#94689,#94690,#94691,#94692,#94693,#94694,#94695,#94696,#94697,#94698,
#94699,#94700,#94701,#94702,#94703,#94704,#94705,#94706,#94707,#94708,#94709,
#94710,#94711,#94712,#94713,#94714,#94715,#94716,#94717,#94718,#94719),
 .UNSPECIFIED.,.F.,.F.,(4,3,3,3,3,3,3,3,3,3,3,3,3,3,3,3,3,3,3,3,3,3,3,4),
(72.2566310325652,72.3608036974116,72.4648211348936,72.5687165871306,72.6725466326848,
72.7763460710619,72.8801496583902,72.9840619405008,73.088033186615,73.1921861589881,
73.253464655196,73.3576508186845,73.4616817438972,73.5655906343145,73.669434065483,
73.7732468164982,73.8770636230202,73.980989100391,74.0849734189361,74.1891396763956,
74.2510125135421,74.3552035665589,74.4592285332535,74.4832444132594),
 .UNSPECIFIED.);
#2657=B_SPLINE_CURVE_WITH_KNOTS('',3,(#94720,#94721,#94722,#94723,#94724,
#94725,#94726,#94727,#94728,#94729,#94730,#94731,#94732,#94733,#94734,#94735,
#94736,#94737,#94738,#94739,#94740,#94741,#94742,#94743,#94744,#94745,#94746,
#94747,#94748,#94749,#94750,#94751,#94752,#94753,#94754,#94755,#94756,#94757,
#94758,#94759,#94760,#94761,#94762,#94763,#94764,#94765,#94766,#94767,#94768,
#94769,#94770,#94771,#94772,#94773,#94774,#94775,#94776,#94777,#94778,#94779,
#94780,#94781,#94782,#94783,#94784,#94785,#94786,#94787,#94788,#94789,#94790,
#94791,#94792,#94793,#94794,#94795,#94796,#94797,#94798,#94799,#94800,#94801,
#94802,#94803,#94804,#94805,#94806,#94807,#94808,#94809,#94810,#94811,#94812,
#94813,#94814,#94815,#94816,#94817,#94818,#94819,#94820,#94821,#94822,#94823,
#94824,#94825,#94826,#94827,#94828,#94829,#94830,#94831,#94832,#94833,#94834,
#94835,#94836,#94837,#94838,#94839,#94840,#94841,#94842,#94843,#94844,#94845,
#94846),.UNSPECIFIED.,.F.,.F.,(4,3,3,3,3,3,3,3,3,3,3,3,3,3,3,3,3,3,3,3,
3,3,3,3,3,3,3,3,3,3,3,3,3,3,3,3,3,3,3,3,3,3,4),(68.1991363982496,68.2657253634656,
68.3699115269536,68.4739424521657,68.5778513425825,68.6816947737505,68.7855075247653,
68.8893243312867,68.993249808657,69.0972341272016,69.2014003846607,69.2632732218117,
69.3674593852999,69.4714903105121,69.5753992009292,69.6792426320973,69.7830553831123,
69.8868721896339,69.9907976670044,70.0947819855492,70.1989482430085,70.2608210801578,
70.365007243646,70.4690381688582,70.5729470592753,70.6767904904434,70.7806032414585,
70.88442004798,70.9883455253505,71.0923298438953,71.1964961013546,71.2583689385038,
71.3625551019918,71.4665860272038,71.5704949176206,71.6743383487885,71.7781510998033,
71.8819679063248,71.985893383695,72.0898777022396,72.1940439596986,72.2559167968499,
72.2566310325399),.UNSPECIFIED.);
#2658=B_SPLINE_CURVE_WITH_KNOTS('',3,(#94852,#94853,#94854,#94855,#94856,
#94857,#94858,#94859,#94860,#94861,#94862,#94863,#94864,#94865,#94866,#94867,
#94868,#94869,#94870,#94871,#94872,#94873,#94874,#94875,#94876,#94877,#94878,
#94879,#94880,#94881,#94882,#94883,#94884,#94885,#94886,#94887,#94888,#94889,
#94890,#94891,#94892,#94893,#94894,#94895,#94896,#94897,#94898,#94899,#94900,
#94901,#94902,#94903,#94904,#94905,#94906,#94907,#94908,#94909,#94910,#94911,
#94912,#94913,#94914,#94915,#94916,#94917,#94918,#94919,#94920,#94921,#94922,
#94923,#94924,#94925,#94926,#94927,#94928,#94929,#94930,#94931,#94932,#94933,
#94934,#94935,#94936,#94937,#94938,#94939,#94940,#94941,#94942,#94943,#94944,
#94945,#94946,#94947,#94948,#94949,#94950,#94951,#94952,#94953,#94954,#94955,
#94956,#94957,#94958,#94959,#94960,#94961,#94962,#94963,#94964,#94965,#94966,
#94967,#94968,#94969,#94970,#94971,#94972),.UNSPECIFIED.,.F.,.F.,(4,3,3,
3,3,3,3,3,3,3,3,3,3,3,3,3,3,3,3,3,3,3,3,3,3,3,3,3,3,3,3,3,3,3,3,3,3,3,3,
3,4),(61.9168665236723,62.0208010675058,62.1246599951528,62.2284781049933,
62.3322901417457,62.4362043441703,62.5401682899817,62.6443238098686,62.7365207799071,
62.8407069433952,62.9447378686072,63.048646759024,63.152490190192,63.2563029412068,
63.3601197477283,63.4640452250985,63.5680295436432,63.6721958011023,63.7340686382531,
63.8382548017413,63.9422857269535,64.0461946173705,64.1500380485387,64.2538507995537,
64.3576676060754,64.4615930834458,64.5655774019906,64.6697436594499,64.7316164965992,
64.8358026600872,64.9398335852992,65.043742475716,65.147585906884,65.2513986578987,
65.3552154644202,65.4591409417905,65.5631252603351,65.6672915177941,65.7291643549453,
65.8652061647349,65.9734457249408),.UNSPECIFIED.);
#2659=B_SPLINE_CURVE_WITH_KNOTS('',3,(#94973,#94974,#94975,#94976,#94977,
#94978,#94979,#94980,#94981,#94982,#94983,#94984,#94985,#94986,#94987,#94988,
#94989,#94990,#94991,#94992,#94993,#94994,#94995,#94996,#94997,#94998,#94999,
#95000,#95001,#95002,#95003,#95004,#95005,#95006,#95007,#95008,#95009,#95010,
#95011,#95012,#95013,#95014,#95015,#95016,#95017,#95018,#95019,#95020,#95021,
#95022,#95023,#95024,#95025,#95026,#95027,#95028,#95029,#95030,#95031,#95032,
#95033,#95034,#95035,#95036,#95037,#95038,#95039,#95040,#95041,#95042),
 .UNSPECIFIED.,.F.,.F.,(4,3,3,3,3,3,3,3,3,3,3,3,3,3,3,3,3,3,3,3,3,3,3,4),
(65.9734457253856,66.0761317728206,66.1787500761636,66.2813369783501,66.3839287747738,
66.4866268116144,66.5893873525292,66.6923186639505,66.7267122132914,66.8308983767795,
66.9349293019916,67.0388381924084,67.1426816235763,67.2464943745912,67.3503111811127,
67.454236658483,67.5582209770277,67.6623872344868,67.7242600716375,67.828449554753,
67.9324611620818,68.0363696459519,68.1402112752601,68.199542273107),
 .UNSPECIFIED.);
#2660=B_SPLINE_CURVE_WITH_KNOTS('',3,(#95044,#95045,#95046,#95047,#95048,
#95049,#95050,#95051,#95052,#95053,#95054,#95055,#95056,#95057,#95058,#95059,
#95060,#95061,#95062,#95063,#95064,#95065,#95066,#95067,#95068,#95069,#95070,
#95071,#95072,#95073,#95074,#95075,#95076,#95077,#95078,#95079,#95080,#95081,
#95082,#95083,#95084,#95085,#95086,#95087,#95088,#95089,#95090,#95091,#95092,
#95093,#95094,#95095,#95096,#95097,#95098,#95099,#95100,#95101,#95102,#95103,
#95104,#95105,#95106,#95107,#95108,#95109,#95110),.UNSPECIFIED.,.F.,.F.,
(4,3,3,3,3,3,3,3,3,3,3,3,3,3,3,3,3,3,3,3,3,3,4),(65.9734457257054,66.0987387056024,
66.2258330924599,66.2706296467734,66.3748158102617,66.4788467354739,66.582755625891,
66.6865990570591,66.7904118080742,66.8942286145957,66.9981540919662,67.102138410511,
67.2063046679703,67.2681775051195,67.3723684096492,67.4763780581656,67.580285456749,
67.6841254673981,67.7879328706238,67.8918030329342,67.9957000743238,68.0997567598233,
68.1991363982496),.UNSPECIFIED.);
#2661=B_SPLINE_CURVE_WITH_KNOTS('',3,(#95111,#95112,#95113,#95114,#95115,
#95116,#95117,#95118,#95119,#95120,#95121,#95122,#95123,#95124,#95125,#95126,
#95127,#95128,#95129,#95130,#95131,#95132,#95133,#95134,#95135,#95136,#95137,
#95138,#95139,#95140,#95141,#95142,#95143,#95144,#95145,#95146,#95147,#95148,
#95149,#95150,#95151,#95152,#95153,#95154,#95155,#95156,#95157,#95158,#95159,
#95160,#95161,#95162,#95163,#95164,#95165,#95166,#95167,#95168,#95169,#95170,
#95171,#95172,#95173,#95174,#95175,#95176,#95177,#95178,#95179,#95180,#95181,
#95182,#95183,#95184,#95185,#95186,#95187,#95188,#95189,#95190,#95191,#95192,
#95193,#95194,#95195,#95196,#95197,#95198,#95199,#95200,#95201,#95202,#95203,
#95204,#95205,#95206,#95207,#95208,#95209,#95210,#95211,#95212,#95213,#95214,
#95215,#95216,#95217,#95218,#95219,#95220,#95221,#95222,#95223,#95224,#95225,
#95226,#95227,#95228,#95229,#95230,#95231,#95232,#95233,#95234),
 .UNSPECIFIED.,.F.,.F.,(4,3,3,3,3,3,3,3,3,3,3,3,3,3,3,3,3,3,3,3,3,3,3,3,
3,3,3,3,3,3,3,3,3,3,3,3,3,3,3,3,3,4),(61.9158990401002,62.0198285605887,
62.1238197497715,62.2279900089989,62.2804382133891,62.3846243768772,62.4886553020892,
62.5925641925062,62.6964076236741,62.800220374689,62.9040371812104,63.0079626585807,
63.1119469771253,63.2161132345845,63.2779860717351,63.3821722352234,63.4862031604355,
63.5901120508525,63.6939554820206,63.7977682330355,63.9015850395571,64.0055105169275,
64.1094948354722,64.2136610929316,64.2755339300812,64.3797200935693,64.4837510187814,
64.5876599091983,64.6915033403663,64.795316091381,64.8991328979023,65.0030583752726,
65.107042693817,65.2112089512763,65.2730817884273,65.3766017373238,65.4799760620941,
65.5832406362455,65.6864470474328,65.7896160420574,65.892830939941,65.9734457253856),
 .UNSPECIFIED.);
#2662=B_SPLINE_CURVE_WITH_KNOTS('',3,(#95240,#95241,#95242,#95243,#95244,
#95245,#95246,#95247,#95248,#95249,#95250,#95251,#95252,#95253,#95254,#95255,
#95256,#95257,#95258,#95259,#95260,#95261,#95262,#95263,#95264,#95265,#95266,
#95267,#95268,#95269,#95270,#95271,#95272,#95273,#95274,#95275,#95276,#95277,
#95278,#95279,#95280,#95281,#95282,#95283,#95284,#95285,#95286,#95287,#95288,
#95289,#95290,#95291,#95292,#95293,#95294,#95295,#95296,#95297,#95298,#95299,
#95300,#95301,#95302,#95303,#95304,#95305,#95306,#95307,#95308,#95309,#95310,
#95311,#95312,#95313,#95314,#95315,#95316,#95317,#95318,#95319,#95320,#95321,
#95322,#95323,#95324,#95325,#95326,#95327,#95328,#95329,#95330,#95331,#95332,
#95333,#95334,#95335,#95336,#95337,#95338,#95339,#95340,#95341,#95342,#95343,
#95344,#95345,#95346,#95347,#95348,#95349,#95350,#95351,#95352,#95353,#95354,
#95355,#95356,#95357,#95358,#95359,#95360,#95361,#95362,#95363),
 .UNSPECIFIED.,.F.,.F.,(4,3,3,3,3,3,3,3,3,3,3,3,3,3,3,3,3,3,3,3,3,3,3,3,
3,3,3,3,3,3,3,3,3,3,3,3,3,3,3,3,3,4),(55.6326004253535,55.7367886138164,
55.7536857714845,55.8578719349726,55.9619028601848,56.0658117506017,56.1696551817698,
56.2734679327847,56.3772847393062,56.4812102166765,56.5851945352213,56.6893607926805,
56.7512336298305,56.8554197933186,56.9594507185307,57.0633596089476,57.1672030401157,
57.2710157911306,57.3748325976521,57.4787580750224,57.5827423935671,57.6869086510263,
57.7487814881766,57.8529676516648,57.9569985768771,58.0609074672941,58.1647508984623,
58.2685636494773,58.3723804559989,58.4763059333693,58.5802902519141,58.6844565093734,
58.7463293465227,58.8496743122095,58.9547475754163,59.057817166758,59.1608249277454,
59.2638067574365,59.3704201725432,59.4735201525628,59.5818902852131,59.6902604178635),
 .UNSPECIFIED.);
#2663=B_SPLINE_CURVE_WITH_KNOTS('',3,(#95364,#95365,#95366,#95367,#95368,
#95369,#95370,#95371,#95372,#95373,#95374,#95375,#95376,#95377,#95378,#95379,
#95380,#95381,#95382,#95383,#95384,#95385,#95386,#95387,#95388,#95389,#95390,
#95391,#95392,#95393,#95394,#95395,#95396,#95397,#95398,#95399,#95400,#95401,
#95402,#95403,#95404,#95405,#95406,#95407,#95408,#95409,#95410,#95411,#95412,
#95413,#95414,#95415,#95416,#95417,#95418,#95419,#95420,#95421,#95422,#95423,
#95424,#95425,#95426,#95427,#95428,#95429,#95430,#95431,#95432,#95433),
 .UNSPECIFIED.,.F.,.F.,(4,3,3,3,3,3,3,3,3,3,3,3,3,3,3,3,3,3,3,3,3,3,3,4),
(59.690260418206,59.7438772048688,59.8480633683568,59.9520942935688,60.0560031839856,
60.1598466151536,60.2636593661684,60.3674761726897,60.4714016500599,60.5753859686045,
60.6795522260636,60.7414250632149,60.8456112267031,60.9496421519152,61.0535510423322,
61.1573944735003,61.2612072245152,61.3650240310366,61.468949508407,61.5729338269518,
61.677100084411,61.738972921561,61.8431345912304,61.9168665236723),
 .UNSPECIFIED.);
#2664=B_SPLINE_CURVE_WITH_KNOTS('',3,(#95435,#95436,#95437,#95438,#95439,
#95440,#95441,#95442,#95443,#95444,#95445,#95446,#95447,#95448,#95449,#95450,
#95451,#95452,#95453,#95454,#95455,#95456,#95457,#95458,#95459,#95460,#95461,
#95462,#95463,#95464,#95465,#95466,#95467,#95468,#95469,#95470,#95471,#95472,
#95473,#95474,#95475,#95476,#95477,#95478,#95479,#95480,#95481,#95482,#95483,
#95484,#95485,#95486,#95487,#95488,#95489,#95490,#95491,#95492,#95493,#95494,
#95495,#95496,#95497,#95498,#95499,#95500,#95501),.UNSPECIFIED.,.F.,.F.,
(4,3,3,3,3,3,3,3,3,3,3,3,3,3,3,3,3,3,3,3,3,3,4),(59.690260418206,59.7955628120771,
59.9009059652391,60.0064057077483,60.1119895277669,60.2177899509164,60.2853424966969,
60.3895286601851,60.4935595853973,60.5974684758143,60.7013119069824,60.8051246579973,
60.9089414645188,61.0128669418892,61.116851260434,61.2210175178933,61.282890355043,
61.3870598977045,61.4910835289854,61.5972874067641,61.7011272958194,61.8085131679598,
61.9158990401002),.UNSPECIFIED.);
#2665=B_SPLINE_CURVE_WITH_KNOTS('',3,(#95502,#95503,#95504,#95505,#95506,
#95507,#95508,#95509,#95510,#95511,#95512,#95513,#95514,#95515,#95516,#95517,
#95518,#95519,#95520,#95521,#95522,#95523,#95524,#95525,#95526,#95527,#95528,
#95529,#95530,#95531,#95532,#95533,#95534,#95535,#95536,#95537,#95538,#95539,
#95540,#95541,#95542,#95543,#95544,#95545,#95546,#95547,#95548,#95549,#95550,
#95551,#95552,#95553,#95554,#95555,#95556,#95557,#95558,#95559,#95560,#95561,
#95562,#95563,#95564,#95565,#95566,#95567,#95568,#95569,#95570,#95571,#95572,
#95573,#95574,#95575,#95576,#95577,#95578,#95579,#95580,#95581,#95582,#95583,
#95584,#95585,#95586,#95587,#95588,#95589,#95590,#95591,#95592,#95593,#95594,
#95595,#95596,#95597,#95598,#95599,#95600,#95601,#95602,#95603,#95604,#95605,
#95606,#95607,#95608,#95609,#95610,#95611,#95612,#95613,#95614,#95615,#95616,
#95617,#95618,#95619,#95620,#95621,#95622,#95623,#95624,#95625),
 .UNSPECIFIED.,.F.,.F.,(4,3,3,3,3,3,3,3,3,3,3,3,3,3,3,3,3,3,3,3,3,3,3,3,
3,3,3,3,3,3,3,3,3,3,3,3,3,3,3,3,3,4),(55.6335493698586,55.7373826934096,
55.8411933057268,55.9450159374289,56.0489521424687,56.1529543449585,56.2571313407819,
56.2951510633125,56.3993372268007,56.503368152013,56.6072770424299,56.7111204735982,
56.8149332246131,56.9187500311345,57.0226755085049,57.1266598270495,57.2308260845087,
57.2926989216586,57.3968850851467,57.5009160103588,57.6048249007758,57.7086683319438,
57.8124810829587,57.9162978894804,58.0202233668507,58.1242076853955,58.2283739428547,
58.2902467800047,58.3944329434928,58.498463868705,58.602372759122,58.70621619029,
58.810028941305,58.9138457478263,59.0177712251967,59.1217555437414,59.2259218012006,
59.2877946383508,59.403242088617,59.5183215991976,59.6327919924206,59.690260417799),
 .UNSPECIFIED.);
#2666=B_SPLINE_CURVE_WITH_KNOTS('',3,(#95631,#95632,#95633,#95634,#95635,
#95636,#95637,#95638,#95639,#95640,#95641,#95642,#95643,#95644,#95645,#95646,
#95647,#95648,#95649,#95650,#95651,#95652,#95653,#95654,#95655,#95656,#95657,
#95658,#95659,#95660,#95661,#95662,#95663,#95664,#95665,#95666,#95667,#95668,
#95669,#95670,#95671,#95672,#95673,#95674,#95675,#95676,#95677,#95678,#95679,
#95680,#95681,#95682,#95683,#95684,#95685,#95686,#95687,#95688,#95689,#95690,
#95691,#95692,#95693,#95694,#95695,#95696,#95697,#95698,#95699,#95700,#95701,
#95702,#95703,#95704,#95705,#95706,#95707,#95708,#95709,#95710,#95711,#95712,
#95713,#95714,#95715,#95716,#95717,#95718,#95719,#95720,#95721,#95722,#95723,
#95724,#95725,#95726,#95727,#95728,#95729,#95730,#95731,#95732,#95733,#95734,
#95735,#95736,#95737,#95738,#95739,#95740,#95741,#95742,#95743,#95744,#95745,
#95746,#95747,#95748,#95749,#95750,#95751,#95752,#95753,#95754),
 .UNSPECIFIED.,.F.,.F.,(4,3,3,3,3,3,3,3,3,3,3,3,3,3,3,3,3,3,3,3,3,3,3,3,
3,3,3,3,3,3,3,3,3,3,3,3,3,3,3,3,3,4),(49.349672428797,49.4543539769497,
49.5583095628721,49.66335409214,49.7683986214079,49.872584784896,49.976615710108,
50.0805246005249,50.184368031693,50.2881807827079,50.3919975892296,50.4959230665999,
50.5999073851446,50.7040736426038,50.765946479754,50.8701326432423,50.9741635684547,
51.0780724588717,51.1819158900398,51.2857286410548,51.3895454475765,51.4934709249469,
51.5974552434917,51.701621500951,51.7634943381001,51.8676805015885,51.9717114268005,
52.0756203172177,52.1794637483859,52.283276499401,52.3870933059224,52.491018783293,
52.595003101838,52.6991693592974,52.7610421964462,52.8655509126688,52.9699037514302,
53.0791965913293,53.1833373805645,53.2874304651154,53.3915238347356,53.4070751110264),
 .UNSPECIFIED.);
#2667=B_SPLINE_CURVE_WITH_KNOTS('',3,(#95755,#95756,#95757,#95758,#95759,
#95760,#95761,#95762,#95763,#95764,#95765,#95766,#95767,#95768,#95769,#95770,
#95771,#95772,#95773,#95774,#95775,#95776,#95777,#95778,#95779,#95780,#95781,
#95782,#95783,#95784,#95785,#95786,#95787,#95788,#95789,#95790,#95791,#95792,
#95793,#95794,#95795,#95796,#95797,#95798,#95799,#95800,#95801,#95802,#95803,
#95804,#95805,#95806,#95807,#95808,#95809,#95810,#95811,#95812,#95813,#95814,
#95815,#95816,#95817,#95818,#95819,#95820,#95821),.UNSPECIFIED.,.F.,.F.,
(4,3,3,3,3,3,3,3,3,3,3,3,3,3,3,3,3,3,3,3,3,3,4),(53.407075111473,53.5259953052154,
53.6459937542275,53.7585900547923,53.8627762182805,53.9668071434925,54.0707160339095,
54.1745594650776,54.2783722160926,54.3821890226141,54.4861144999845,54.5900988185293,
54.6942650759886,54.7561379131384,54.8656957271653,54.9697002456262,55.0736027369136,
55.177438061658,55.2812409986278,55.3850920232226,55.4889708986981,55.5929698536114,
55.6326004253535),.UNSPECIFIED.);
#2668=B_SPLINE_CURVE_WITH_KNOTS('',3,(#95823,#95824,#95825,#95826,#95827,
#95828,#95829,#95830,#95831,#95832,#95833,#95834,#95835,#95836,#95837,#95838,
#95839,#95840,#95841,#95842,#95843,#95844,#95845,#95846,#95847,#95848,#95849,
#95850,#95851,#95852,#95853,#95854,#95855,#95856,#95857,#95858,#95859,#95860,
#95861,#95862,#95863,#95864,#95865,#95866,#95867,#95868,#95869,#95870,#95871,
#95872,#95873,#95874,#95875,#95876,#95877,#95878,#95879,#95880,#95881,#95882,
#95883,#95884,#95885,#95886,#95887,#95888,#95889,#95890,#95891,#95892),
 .UNSPECIFIED.,.F.,.F.,(4,3,3,3,3,3,3,3,3,3,3,3,3,3,3,3,3,3,3,3,3,3,3,4),
(53.4070751114826,53.5098614913189,53.6124973139516,53.7150505550782,53.8175576893174,
53.9200551251608,54.0226483900868,54.1252912590503,54.2281147116709,54.3000553466204,
54.4042415101085,54.5082724353208,54.6121813257378,54.7160247569059,54.8198375079209,
54.9236543144423,55.0275797918127,55.1315641103574,55.2357303678167,55.2976032049664,
55.4017686798836,55.5057980075389,55.6097071751473,55.6335493698586),
 .UNSPECIFIED.);
#2669=B_SPLINE_CURVE_WITH_KNOTS('',3,(#95893,#95894,#95895,#95896,#95897,
#95898,#95899,#95900,#95901,#95902,#95903,#95904,#95905,#95906,#95907,#95908,
#95909,#95910,#95911,#95912,#95913,#95914,#95915,#95916,#95917,#95918,#95919,
#95920,#95921,#95922,#95923,#95924,#95925,#95926,#95927,#95928,#95929,#95930,
#95931,#95932,#95933,#95934,#95935,#95936,#95937,#95938,#95939,#95940,#95941,
#95942,#95943,#95944,#95945,#95946,#95947,#95948,#95949,#95950,#95951,#95952,
#95953,#95954,#95955,#95956,#95957,#95958,#95959,#95960,#95961,#95962,#95963,
#95964,#95965,#95966,#95967,#95968,#95969,#95970,#95971,#95972,#95973,#95974,
#95975,#95976,#95977,#95978,#95979,#95980,#95981,#95982,#95983,#95984,#95985,
#95986,#95987,#95988,#95989,#95990,#95991,#95992,#95993,#95994,#95995,#95996,
#95997,#95998,#95999,#96000,#96001,#96002,#96003,#96004,#96005,#96006,#96007,
#96008,#96009,#96010,#96011,#96012,#96013,#96014,#96015,#96016),
 .UNSPECIFIED.,.F.,.F.,(4,3,3,3,3,3,3,3,3,3,3,3,3,3,3,3,3,3,3,3,3,3,3,3,
3,3,3,3,3,3,3,3,3,3,3,3,3,3,3,3,3,4),(49.3501218939192,49.4542472755859,
49.5611993552922,49.6650784875894,49.7689057759847,49.8727159784123,49.9820029621182,
50.0859506840952,50.1899710987106,50.2941599666065,50.309863913236,50.4140500767242,
50.5180810019365,50.6219898923535,50.7258333235217,50.8296460745367,50.9334628810583,
51.0373883584288,51.1413726769736,51.2455389344329,51.3074117715821,51.4115979350702,
51.5156288602824,51.6195377506993,51.7233811818674,51.8271939328822,51.9310107394038,
52.0349362167741,52.1389205353188,52.2430867927781,52.3049596299282,52.4091457934165,
52.5131767186288,52.6170856090459,52.7209290402142,52.8247417912293,52.928558597751,
53.0324840751215,53.1364683936664,53.2406346511258,53.3025074882743,53.4070751110264),
 .UNSPECIFIED.);
#2670=B_SPLINE_CURVE_WITH_KNOTS('',3,(#96022,#96023,#96024,#96025,#96026,
#96027,#96028,#96029,#96030,#96031,#96032,#96033,#96034,#96035,#96036,#96037,
#96038,#96039,#96040,#96041,#96042,#96043,#96044,#96045,#96046,#96047,#96048,
#96049,#96050,#96051,#96052,#96053,#96054,#96055,#96056,#96057,#96058,#96059,
#96060,#96061,#96062,#96063,#96064,#96065,#96066,#96067,#96068,#96069,#96070,
#96071,#96072,#96073,#96074,#96075,#96076,#96077,#96078,#96079,#96080,#96081,
#96082,#96083,#96084,#96085,#96086,#96087,#96088,#96089,#96090,#96091,#96092,
#96093,#96094,#96095,#96096,#96097,#96098,#96099,#96100,#96101,#96102,#96103,
#96104,#96105,#96106,#96107,#96108,#96109,#96110,#96111,#96112,#96113,#96114,
#96115,#96116,#96117,#96118,#96119,#96120,#96121,#96122,#96123,#96124,#96125,
#96126,#96127,#96128,#96129,#96130,#96131,#96132,#96133,#96134,#96135,#96136,
#96137,#96138,#96139,#96140,#96141,#96142),.UNSPECIFIED.,.F.,.F.,(4,3,3,
3,3,3,3,3,3,3,3,3,3,3,3,3,3,3,3,3,3,3,3,3,3,3,3,3,3,3,3,3,3,3,3,3,3,3,3,
3,4),(43.0672730904575,43.1711320846111,43.2749502212473,43.3787622451258,
43.482676408604,43.586640279845,43.6907957641029,43.7831114713314,43.8872976348199,
43.9913285600324,44.0952374504496,44.199080881618,44.3028936326331,44.4067104391551,
44.5106359165258,44.6146202350706,44.7187864925301,44.7806593296775,44.8848454931656,
44.9888764183775,45.0927853087944,45.1966287399624,45.3004414909772,45.4042582974986,
45.5081837748688,45.6121680934134,45.7163343508724,45.7782071880236,45.882393351512,
45.986424276724,46.090333167141,46.1941765983091,46.2979893493239,46.4018061558458,
46.5057316332163,46.6097159517613,46.7138822092206,46.7757550463697,46.8962986192127,
47.0157785770585,47.1238898034029),.UNSPECIFIED.);
#2671=B_SPLINE_CURVE_WITH_KNOTS('',3,(#96143,#96144,#96145,#96146,#96147,
#96148,#96149,#96150,#96151,#96152,#96153,#96154,#96155,#96156,#96157,#96158,
#96159,#96160,#96161,#96162,#96163,#96164,#96165,#96166,#96167,#96168,#96169,
#96170,#96171,#96172,#96173,#96174,#96175,#96176,#96177,#96178,#96179,#96180,
#96181,#96182,#96183,#96184,#96185,#96186,#96187,#96188,#96189,#96190,#96191,
#96192,#96193,#96194,#96195,#96196,#96197,#96198,#96199,#96200,#96201,#96202,
#96203,#96204,#96205,#96206,#96207,#96208,#96209,#96210,#96211,#96212),
 .UNSPECIFIED.,.F.,.F.,(4,3,3,3,3,3,3,3,3,3,3,3,3,3,3,3,3,3,3,3,3,3,3,4),
(47.1238898038468,47.227928135532,47.3319603652853,47.4360206698557,47.5402127556614,
47.6444838895193,47.7489375131514,47.7733029047158,47.8774890682039,47.981519993416,
48.0854288838329,48.189272315001,48.2930850660161,48.3969018725377,48.5008273499081,
48.6048116684528,48.7089779259121,48.7708507630618,48.8750265339913,48.9790548148158,
49.0829625294199,49.1867995822523,49.2906190115793,49.349672428797),
 .UNSPECIFIED.);
#2672=B_SPLINE_CURVE_WITH_KNOTS('',3,(#96214,#96215,#96216,#96217,#96218,
#96219,#96220,#96221,#96222,#96223,#96224,#96225,#96226,#96227,#96228,#96229,
#96230,#96231,#96232,#96233,#96234,#96235,#96236,#96237,#96238,#96239,#96240,
#96241,#96242,#96243,#96244,#96245,#96246,#96247,#96248,#96249,#96250,#96251,
#96252,#96253,#96254,#96255,#96256,#96257,#96258,#96259,#96260,#96261,#96262,
#96263,#96264,#96265,#96266,#96267,#96268,#96269,#96270,#96271,#96272,#96273,
#96274,#96275,#96276,#96277,#96278,#96279,#96280,#96281,#96282,#96283),
 .UNSPECIFIED.,.F.,.F.,(4,3,3,3,3,3,3,3,3,3,3,3,3,3,3,3,3,3,3,3,3,3,3,4),
(47.1238898038468,47.2754958859059,47.3172203381978,47.4214065016861,47.5254374268983,
47.6293463173154,47.7331897484836,47.8370024994987,47.9408193060204,48.0447447833909,
48.1487291019357,48.2528953593951,48.3147681965438,48.4189543600319,48.5229852852439,
48.6268941756608,48.7307376068289,48.8345503578437,48.9383671643652,49.0422926417355,
49.1462769602802,49.2504432177394,49.3123160548899,49.3501218939192),
 .UNSPECIFIED.);
#2673=B_SPLINE_CURVE_WITH_KNOTS('',3,(#96284,#96285,#96286,#96287,#96288,
#96289,#96290,#96291,#96292,#96293,#96294,#96295,#96296,#96297,#96298,#96299,
#96300,#96301,#96302,#96303,#96304,#96305,#96306,#96307,#96308,#96309,#96310,
#96311,#96312,#96313,#96314,#96315,#96316,#96317,#96318,#96319,#96320,#96321,
#96322,#96323,#96324,#96325,#96326,#96327,#96328,#96329,#96330,#96331,#96332,
#96333,#96334,#96335,#96336,#96337,#96338,#96339,#96340,#96341,#96342,#96343,
#96344,#96345,#96346,#96347,#96348,#96349,#96350,#96351,#96352,#96353,#96354,
#96355,#96356,#96357,#96358,#96359,#96360,#96361,#96362,#96363,#96364,#96365,
#96366,#96367,#96368,#96369,#96370,#96371,#96372,#96373,#96374,#96375,#96376,
#96377,#96378,#96379,#96380,#96381,#96382,#96383,#96384,#96385,#96386,#96387,
#96388,#96389,#96390,#96391,#96392,#96393,#96394,#96395,#96396,#96397,#96398,
#96399,#96400,#96401,#96402,#96403,#96404,#96405,#96406,#96407),
 .UNSPECIFIED.,.F.,.F.,(4,3,3,3,3,3,3,3,3,3,3,3,3,3,3,3,3,3,3,3,3,3,3,3,
3,3,3,3,3,3,3,3,3,3,3,3,3,3,3,3,3,4),(43.0661596803882,43.1701506766889,
43.274320821343,43.3270289048134,43.4312150683039,43.5352459935185,43.6391548839378,
43.7429983151084,43.8468110661257,43.9506278726497,44.0545533500226,44.1585376685698,
44.2627039260315,44.3245767631595,44.4287629266471,44.5327938518588,44.6367027422752,
44.7405461734428,44.8443589244572,44.9481757309782,45.0521012083481,45.1560855268923,
45.2602517843511,45.3221246215056,45.4263107849935,45.5303417102054,45.6342506006221,
45.7380940317899,45.8419067828045,45.9457235893257,46.0496490666958,46.1536333852403,
46.2577996426992,46.3196724798517,46.4223012412912,46.5247935864413,46.6271863644384,
46.729516280192,46.8318649061918,46.934217612914,47.0366904241961,47.1238898034296),
 .UNSPECIFIED.);
#2674=B_SPLINE_CURVE_WITH_KNOTS('',3,(#96413,#96414,#96415,#96416,#96417,
#96418,#96419,#96420,#96421,#96422,#96423,#96424,#96425,#96426,#96427,#96428,
#96429,#96430,#96431,#96432,#96433,#96434,#96435,#96436,#96437,#96438,#96439,
#96440,#96441,#96442,#96443,#96444,#96445,#96446,#96447,#96448,#96449,#96450,
#96451,#96452,#96453,#96454,#96455,#96456,#96457,#96458,#96459,#96460,#96461,
#96462,#96463,#96464,#96465,#96466,#96467,#96468,#96469,#96470,#96471,#96472,
#96473,#96474,#96475,#96476,#96477,#96478,#96479,#96480,#96481,#96482,#96483,
#96484,#96485,#96486,#96487,#96488,#96489,#96490,#96491,#96492,#96493,#96494,
#96495,#96496,#96497,#96498,#96499,#96500,#96501,#96502,#96503,#96504,#96505,
#96506,#96507,#96508,#96509,#96510,#96511,#96512,#96513,#96514,#96515,#96516,
#96517,#96518,#96519,#96520,#96521,#96522,#96523,#96524,#96525,#96526,#96527,
#96528,#96529,#96530,#96531,#96532,#96533,#96534,#96535,#96536,#96537,#96538,
#96539),.UNSPECIFIED.,.F.,.F.,(4,3,3,3,3,3,3,3,3,3,3,3,3,3,3,3,3,3,3,3,
3,3,3,3,3,3,3,3,3,3,3,3,3,3,3,3,3,3,3,3,3,3,4),(36.7834442091166,36.8002764629088,
36.904462626368,37.0084935515507,37.1124024419373,37.2162458730747,37.3200586240585,
37.4238754305486,37.5278009078871,37.6317852263998,37.735951483827,37.7978243212549,
37.9020104847617,38.0060414099927,38.1099503004289,38.2137937316164,38.3176064826509,
38.4214232891921,38.5253487665822,38.6293330851467,38.7334993426256,38.795372179601,
38.8995583430862,39.0035892682954,39.1074981587095,39.2113415898746,39.3151543408867,
39.4189711474052,39.5228966247727,39.6268809433146,39.7310472007711,39.7929200379471,
39.8971062014326,40.0011371266419,40.105046017056,40.2088894482213,40.3127021992333,
40.4165190057517,40.520444483119,40.6244288016607,40.7285950591169,40.7904678962932,
40.8407044966672),.UNSPECIFIED.);
#2675=B_SPLINE_CURVE_WITH_KNOTS('',3,(#96540,#96541,#96542,#96543,#96544,
#96545,#96546,#96547,#96548,#96549,#96550,#96551,#96552,#96553,#96554,#96555,
#96556,#96557,#96558,#96559,#96560,#96561,#96562,#96563,#96564,#96565,#96566,
#96567,#96568,#96569,#96570,#96571,#96572,#96573,#96574,#96575,#96576,#96577,
#96578,#96579,#96580,#96581,#96582,#96583,#96584,#96585,#96586,#96587,#96588,
#96589,#96590,#96591,#96592,#96593,#96594,#96595,#96596,#96597,#96598,#96599,
#96600,#96601,#96602,#96603,#96604,#96605,#96606,#96607,#96608,#96609),
 .UNSPECIFIED.,.F.,.F.,(4,3,3,3,3,3,3,3,3,3,3,3,3,3,3,3,3,3,3,3,3,3,3,4),
(40.8407044970017,40.9440746115611,41.0495672544458,41.1526720053855,41.2557188072273,
41.3587435025094,41.4660615655418,41.569214750082,41.6724388016555,41.7758284060269,
41.7880157546392,41.8922019181268,41.9962328433386,42.1001417337551,42.2039851649227,
42.3077979159372,42.4116147224583,42.5155401998282,42.6195245183725,42.7236907758313,
42.7855636129853,42.8897412732124,42.9937540523167,43.0672730904575),
 .UNSPECIFIED.);
#2676=B_SPLINE_CURVE_WITH_KNOTS('',3,(#96611,#96612,#96613,#96614,#96615,
#96616,#96617,#96618,#96619,#96620,#96621,#96622,#96623,#96624,#96625,#96626,
#96627,#96628,#96629,#96630,#96631,#96632,#96633,#96634,#96635,#96636,#96637,
#96638,#96639,#96640,#96641,#96642,#96643,#96644,#96645,#96646,#96647,#96648,
#96649,#96650,#96651,#96652,#96653,#96654,#96655,#96656,#96657,#96658,#96659,
#96660,#96661,#96662,#96663,#96664,#96665,#96666,#96667,#96668,#96669,#96670,
#96671,#96672,#96673,#96674,#96675,#96676,#96677),.UNSPECIFIED.,.F.,.F.,
(4,3,3,3,3,3,3,3,3,3,3,3,3,3,3,3,3,3,3,3,3,3,4),(40.8407044969848,40.9497796083564,
41.0591756422735,41.1687426604124,41.2786112447421,41.3319331881212,41.4361193516064,
41.5401502768156,41.6440591672297,41.7479025983948,41.8517153494069,41.9555321559254,
42.059457633293,42.1634419518348,42.2676082092913,42.3294810464673,42.4336404893563,
42.53765703907,42.6415657001868,42.7477141952371,42.851532121409,42.9588459008986,
43.0661596803882),.UNSPECIFIED.);
#2677=B_SPLINE_CURVE_WITH_KNOTS('',3,(#96678,#96679,#96680,#96681,#96682,
#96683,#96684,#96685,#96686,#96687,#96688,#96689,#96690,#96691,#96692,#96693,
#96694,#96695,#96696,#96697,#96698,#96699,#96700,#96701,#96702,#96703,#96704,
#96705,#96706,#96707,#96708,#96709,#96710,#96711,#96712,#96713,#96714,#96715,
#96716,#96717,#96718,#96719,#96720,#96721,#96722,#96723,#96724,#96725,#96726,
#96727,#96728,#96729,#96730,#96731,#96732,#96733,#96734,#96735,#96736,#96737,
#96738,#96739,#96740,#96741,#96742,#96743,#96744,#96745,#96746,#96747,#96748,
#96749,#96750,#96751,#96752,#96753,#96754,#96755,#96756,#96757,#96758,#96759,
#96760,#96761,#96762,#96763,#96764,#96765,#96766,#96767,#96768,#96769,#96770,
#96771,#96772,#96773,#96774,#96775,#96776,#96777,#96778,#96779,#96780,#96781,
#96782,#96783,#96784,#96785,#96786,#96787,#96788,#96789,#96790,#96791,#96792,
#96793,#96794,#96795,#96796,#96797,#96798,#96799,#96800,#96801),
 .UNSPECIFIED.,.F.,.F.,(4,3,3,3,3,3,3,3,3,3,3,3,3,3,3,3,3,3,3,3,3,3,3,3,
3,3,3,3,3,3,3,3,3,3,3,3,3,3,3,3,3,4),(36.783723968172,36.8875345931376,
36.9913571540606,37.0952932379323,37.1992952442744,37.3034721168394,37.3417417547369,
37.4459279183704,37.5499588437298,37.6538677342965,37.7577111656157,37.8615239167828,
37.965340723457,38.0692662009808,38.1732505196793,38.2774167772914,38.339289613083,
38.4434757765587,38.5475067017588,38.6514155921638,38.7552590233201,38.8590717743237,
38.9628885808336,39.0668140581933,39.1707983767274,39.2749646341767,39.3368374714291,
39.4410236348884,39.5450545600711,39.6489634504579,39.7528068815956,39.8566196325795,
39.9604364390695,40.0643619164082,40.168346234921,40.2725124923483,40.3343853297751,
40.443556269481,40.5524208008283,40.6611016632913,40.7695577702486,40.8407044966672),
 .UNSPECIFIED.);
#2678=B_SPLINE_CURVE_WITH_KNOTS('',3,(#96807,#96808,#96809,#96810,#96811,
#96812,#96813,#96814,#96815,#96816,#96817,#96818,#96819,#96820,#96821,#96822,
#96823,#96824,#96825,#96826,#96827,#96828,#96829,#96830,#96831,#96832,#96833,
#96834,#96835,#96836,#96837,#96838,#96839,#96840,#96841,#96842,#96843,#96844,
#96845,#96846,#96847,#96848,#96849,#96850,#96851,#96852,#96853,#96854,#96855,
#96856,#96857,#96858,#96859,#96860,#96861,#96862,#96863,#96864,#96865,#96866,
#96867,#96868,#96869,#96870,#96871,#96872,#96873,#96874,#96875,#96876,#96877,
#96878,#96879,#96880,#96881,#96882,#96883,#96884,#96885,#96886,#96887,#96888,
#96889,#96890,#96891,#96892,#96893,#96894,#96895,#96896,#96897,#96898,#96899,
#96900,#96901,#96902,#96903,#96904,#96905,#96906,#96907,#96908,#96909,#96910,
#96911,#96912,#96913,#96914,#96915,#96916,#96917,#96918,#96919,#96920,#96921,
#96922,#96923,#96924,#96925,#96926,#96927,#96928,#96929,#96930),
 .UNSPECIFIED.,.F.,.F.,(4,3,3,3,3,3,3,3,3,3,3,3,3,3,3,3,3,3,3,3,3,3,3,3,
3,3,3,3,3,3,3,3,3,3,3,3,3,3,3,3,3,4),(30.4998665259952,30.6038214794107,
30.7094053961215,30.8149893128323,30.9191754738907,31.0232063966284,31.1271152845158,
31.230958713122,31.3347714615463,31.4385882654523,31.5425137401869,31.6464980560807,
31.7506643108935,31.8125371711784,31.9167233357869,32.0207542621341,32.1246631537022,
32.2285065860308,32.3323193382138,32.4361361459094,32.5400616244546,32.6440459441764,
32.7482122028035,32.8100850295245,32.9142711930052,33.0183021182129,33.1222110086302,
33.2260544398017,33.3298671908226,33.4336839973534,33.5376094747372,33.6415937932978,
33.7457600507769,33.8076328878706,33.9105733956083,34.0133739392442,34.1160710646397,
34.2187011756055,34.3213305265982,34.4239607110243,34.5266703118432,34.5575191894876),
 .UNSPECIFIED.);
#2679=B_SPLINE_CURVE_WITH_KNOTS('',3,(#96931,#96932,#96933,#96934,#96935,
#96936,#96937,#96938,#96939,#96940,#96941,#96942,#96943,#96944,#96945,#96946,
#96947,#96948,#96949,#96950,#96951,#96952,#96953,#96954,#96955,#96956,#96957,
#96958,#96959,#96960,#96961,#96962,#96963,#96964,#96965,#96966,#96967,#96968,
#96969,#96970,#96971,#96972,#96973,#96974,#96975,#96976,#96977,#96978,#96979,
#96980,#96981,#96982,#96983,#96984,#96985,#96986,#96987,#96988,#96989,#96990,
#96991,#96992,#96993,#96994,#96995,#96996,#96997),.UNSPECIFIED.,.F.,.F.,
(4,3,3,3,3,3,3,3,3,3,3,3,3,3,3,3,3,3,3,3,3,3,4),(34.5575191897883,34.6927956482481,
34.8051807462166,34.909366909851,35.0133978352114,35.1173067257789,35.2211501570989,
35.3249629082669,35.4287797149424,35.532705192467,35.6366895111664,35.7408557687793,
35.8027286045627,35.9069159432588,36.0109477009189,36.1148561160979,36.2186985866368,
36.3225098919278,36.4263247672704,36.5302426811368,36.6342192371381,36.738364891705,
36.7834442091166),.UNSPECIFIED.);
#2680=B_SPLINE_CURVE_WITH_KNOTS('',3,(#96999,#97000,#97001,#97002,#97003,
#97004,#97005,#97006,#97007,#97008,#97009,#97010,#97011,#97012,#97013,#97014,
#97015,#97016,#97017,#97018,#97019,#97020,#97021,#97022,#97023,#97024,#97025,
#97026,#97027,#97028,#97029,#97030,#97031,#97032,#97033,#97034,#97035,#97036,
#97037,#97038,#97039,#97040,#97041,#97042,#97043,#97044,#97045,#97046,#97047,
#97048,#97049,#97050,#97051,#97052,#97053,#97054,#97055,#97056,#97057,#97058,
#97059,#97060,#97061,#97062,#97063,#97064,#97065,#97066,#97067,#97068),
 .UNSPECIFIED.,.F.,.F.,(4,3,3,3,3,3,3,3,3,3,3,3,3,3,3,3,3,3,3,3,3,3,3,4),
(34.557519189755,34.6600261052929,34.7624492426979,34.8648252095929,34.9671905447891,
35.0696506740761,35.1721598073091,35.2748489315128,35.3466460380447,35.4508322015257,
35.5548631267337,35.6587720171512,35.7626154483228,35.8664281993442,35.9702450058752,
36.0741704832593,36.1781548018204,36.2823210592997,36.3441938963908,36.4483886661888,
36.5524031618926,36.6563141161534,36.7601506302161,36.783723968172),
 .UNSPECIFIED.);
#2681=B_SPLINE_CURVE_WITH_KNOTS('',3,(#97069,#97070,#97071,#97072,#97073,
#97074,#97075,#97076,#97077,#97078,#97079,#97080,#97081,#97082,#97083,#97084,
#97085,#97086,#97087,#97088,#97089,#97090,#97091,#97092,#97093,#97094,#97095,
#97096,#97097,#97098,#97099,#97100,#97101,#97102,#97103,#97104,#97105,#97106,
#97107,#97108,#97109,#97110,#97111,#97112,#97113,#97114,#97115,#97116,#97117,
#97118,#97119,#97120,#97121,#97122,#97123,#97124,#97125,#97126,#97127,#97128,
#97129,#97130,#97131,#97132,#97133,#97134,#97135,#97136,#97137,#97138,#97139,
#97140,#97141,#97142,#97143,#97144,#97145,#97146,#97147,#97148,#97149,#97150,
#97151,#97152,#97153,#97154,#97155,#97156,#97157,#97158,#97159,#97160,#97161,
#97162,#97163,#97164,#97165,#97166,#97167,#97168,#97169,#97170,#97171,#97172,
#97173,#97174,#97175,#97176,#97177,#97178,#97179,#97180,#97181,#97182,#97183,
#97184,#97185,#97186,#97187,#97188,#97189,#97190,#97191,#97192),
 .UNSPECIFIED.,.F.,.F.,(4,3,3,3,3,3,3,3,3,3,3,3,3,3,3,3,3,3,3,3,3,3,3,3,
3,3,3,3,3,3,3,3,3,3,3,3,3,3,3,3,3,4),(30.5008971308904,30.6078418151117,
30.7117208906534,30.8155481393843,30.9193583192481,31.0286323906012,31.1325801108998,
31.2366005354176,31.3407894024993,31.3564546046604,31.4606407764529,31.5646717100683,
31.6685806089942,31.7724240487317,31.8762368083637,31.980053623537,32.0839791095526,
32.1879634367518,32.2921297027861,32.3540024630065,32.4581886272382,32.5622195532326,
32.6661284444858,32.7699718765231,32.8737846284388,32.9776014358916,33.0815269142338,
33.1855112337746,33.2896774922579,33.3515503213525,33.4557364824179,33.5597674051624,
33.663676293057,33.7675197216704,33.871332470102,33.9751492740155,34.0790747487577,
34.183059064659,34.2872253194792,34.3490981796986,34.4951131604683,34.5575191894876),
 .UNSPECIFIED.);
#2682=B_SPLINE_CURVE_WITH_KNOTS('',3,(#97198,#97199,#97200,#97201,#97202,
#97203,#97204,#97205,#97206,#97207,#97208,#97209,#97210,#97211,#97212,#97213,
#97214,#97215,#97216,#97217,#97218,#97219,#97220,#97221,#97222,#97223,#97224,
#97225,#97226,#97227,#97228,#97229,#97230,#97231,#97232,#97233,#97234,#97235,
#97236,#97237,#97238,#97239,#97240,#97241,#97242,#97243,#97244,#97245,#97246,
#97247,#97248,#97249,#97250,#97251,#97252,#97253,#97254,#97255,#97256,#97257,
#97258,#97259,#97260,#97261,#97262,#97263,#97264,#97265,#97266,#97267,#97268,
#97269,#97270,#97271,#97272,#97273,#97274,#97275,#97276,#97277,#97278,#97279,
#97280,#97281,#97282,#97283,#97284,#97285,#97286,#97287,#97288,#97289,#97290,
#97291,#97292,#97293,#97294,#97295,#97296,#97297,#97298,#97299,#97300,#97301,
#97302,#97303,#97304,#97305,#97306,#97307,#97308,#97309,#97310,#97311,#97312,
#97313,#97314,#97315,#97316,#97317,#97318),.UNSPECIFIED.,.F.,.F.,(4,3,3,
3,3,3,3,3,3,3,3,3,3,3,3,3,3,3,3,3,3,3,3,3,3,3,3,3,3,3,3,3,3,3,3,3,3,3,3,
3,4),(24.2175053970322,24.321323756092,24.4251359323839,24.5290502036337,
24.6330141192664,24.7371697208814,24.8297021627558,24.9338881432323,25.0379188823439,
25.1418275829741,25.2456708221829,25.3494833793523,25.4532999904265,25.5572252712448,
25.6612093923175,25.7653754529891,25.8272500211019,25.931436244153,26.035467229549,
26.1393761807748,26.2432196731041,26.3470324855408,26.4508493536522,26.5547748924429,
26.6587592724048,26.7629255906066,26.8247978794479,26.9289840556633,27.0330149940236,
27.1369238981528,27.2407673433741,27.3445801087626,27.4483969299582,27.5523224223632,
27.6563067561686,27.760473029083,27.822345737794,27.9353427738055,28.0470528540681,
28.1606933679541,28.27433388184),.UNSPECIFIED.);
#2683=B_SPLINE_CURVE_WITH_KNOTS('',3,(#97319,#97320,#97321,#97322,#97323,
#97324,#97325,#97326,#97327,#97328,#97329,#97330,#97331,#97332,#97333,#97334,
#97335,#97336,#97337,#97338,#97339,#97340,#97341,#97342,#97343,#97344,#97345,
#97346,#97347,#97348,#97349,#97350,#97351,#97352,#97353,#97354,#97355,#97356,
#97357,#97358,#97359,#97360,#97361,#97362,#97363,#97364,#97365,#97366,#97367,
#97368,#97369,#97370,#97371,#97372,#97373,#97374,#97375,#97376,#97377,#97378,
#97379,#97380,#97381,#97382,#97383,#97384,#97385),.UNSPECIFIED.,.F.,.F.,
(4,3,3,3,3,3,3,3,3,3,3,3,3,3,3,3,3,3,3,3,3,3,4),(28.2743338823081,28.381185874661,
28.4908628050308,28.5980291137702,28.7089613549551,28.8198935961401,28.9240797679585,
29.0281107016001,29.1320196005526,29.2358630403168,29.3396757999759,29.4434926151765,
29.5474181012193,29.6514024284455,29.7555686945067,29.8174414544862,29.9216058860559,
30.025625845333,30.1295363446483,30.2333833809726,30.3371921312322,30.4410324079646,
30.4998665259952),.UNSPECIFIED.);
#2684=B_SPLINE_CURVE_WITH_KNOTS('',3,(#97387,#97388,#97389,#97390,#97391,
#97392,#97393,#97394,#97395,#97396,#97397,#97398,#97399,#97400,#97401,#97402,
#97403,#97404,#97405,#97406,#97407,#97408,#97409,#97410,#97411,#97412,#97413,
#97414,#97415,#97416,#97417,#97418,#97419,#97420,#97421,#97422,#97423,#97424,
#97425,#97426,#97427,#97428,#97429,#97430,#97431,#97432,#97433,#97434,#97435,
#97436,#97437,#97438,#97439,#97440,#97441,#97442,#97443,#97444,#97445,#97446,
#97447,#97448,#97449,#97450,#97451,#97452,#97453,#97454,#97455,#97456),
 .UNSPECIFIED.,.F.,.F.,(4,3,3,3,3,3,3,3,3,3,3,3,3,3,3,3,3,3,3,3,3,3,3,4),
(28.2743338823081,28.3638110296221,28.4679972525077,28.5720282377358,28.6759371887921,
28.7797806809506,28.8835934932153,28.9874103611545,29.0913358997729,29.1953202795622,
29.2994865975932,29.3613588879682,29.4655450641724,29.569576002521,29.6734849066373,
29.7773283518453,29.8811411172201,29.9849579384014,30.0888834307912,30.1928677645809,
30.297034037479,30.3589067463143,30.4630838225526,30.5008971308904),
 .UNSPECIFIED.);
#2685=B_SPLINE_CURVE_WITH_KNOTS('',3,(#97457,#97458,#97459,#97460,#97461,
#97462,#97463,#97464,#97465,#97466,#97467,#97468,#97469,#97470,#97471,#97472,
#97473,#97474,#97475,#97476,#97477,#97478,#97479,#97480,#97481,#97482,#97483,
#97484,#97485,#97486,#97487,#97488,#97489,#97490,#97491,#97492,#97493,#97494,
#97495,#97496,#97497,#97498,#97499,#97500,#97501,#97502,#97503,#97504,#97505,
#97506,#97507,#97508,#97509,#97510,#97511,#97512,#97513,#97514,#97515,#97516,
#97517,#97518,#97519,#97520,#97521,#97522,#97523,#97524,#97525,#97526,#97527,
#97528,#97529,#97530,#97531,#97532,#97533,#97534,#97535,#97536,#97537,#97538,
#97539,#97540,#97541,#97542,#97543,#97544,#97545,#97546,#97547,#97548,#97549,
#97550,#97551,#97552,#97553,#97554,#97555,#97556,#97557,#97558,#97559,#97560,
#97561,#97562,#97563,#97564,#97565,#97566,#97567,#97568,#97569,#97570,#97571,
#97572,#97573,#97574,#97575,#97576,#97577,#97578,#97579,#97580),
 .UNSPECIFIED.,.F.,.F.,(4,3,3,3,3,3,3,3,3,3,3,3,3,3,3,3,3,3,3,3,3,3,3,3,
3,3,3,3,3,3,3,3,3,3,3,3,3,3,3,3,3,4),(24.2166116715314,24.3207836948893,
24.3736195962378,24.4778042283434,24.5818335974701,24.6857409026657,24.789582731488,
24.8933938654244,24.9972090425095,25.101132882772,25.2051155574088,25.3092801780267,
25.3711674545838,25.4753540209415,25.5793853523628,25.6832946519404,25.7871384938629,
25.8909516566054,25.9947688752086,26.0986947623334,26.2026794899368,26.3068461508868,
26.3687153129299,26.4729016340226,26.5769327210748,26.6808417788562,26.7846853807111,
26.8884983054843,26.9923152885876,27.096240945657,27.2002254459312,27.304391886379,
27.366263171276,27.4692311758098,27.5720240162915,27.674719005969,27.7773525419992,
27.8799609371538,27.9826451368982,28.0853653027244,28.1882551863936,28.2743338818562),
 .UNSPECIFIED.);
#2686=B_SPLINE_CURVE_WITH_KNOTS('',3,(#97586,#97587,#97588,#97589,#97590,
#97591,#97592,#97593,#97594,#97595,#97596,#97597,#97598,#97599,#97600,#97601,
#97602,#97603,#97604,#97605,#97606,#97607,#97608,#97609,#97610,#97611,#97612,
#97613,#97614,#97615,#97616,#97617,#97618,#97619,#97620,#97621,#97622,#97623,
#97624,#97625,#97626,#97627,#97628,#97629,#97630,#97631,#97632,#97633,#97634,
#97635,#97636,#97637,#97638,#97639,#97640,#97641,#97642,#97643,#97644,#97645,
#97646,#97647,#97648,#97649,#97650,#97651,#97652,#97653,#97654,#97655),
 .UNSPECIFIED.,.F.,.F.,(4,3,3,3,3,3,3,3,3,3,3,3,3,3,3,3,3,3,3,3,3,3,3,4),
(15.7079632679489,15.810762470857,15.9135271820867,16.0162934123199,16.1191701702764,
16.2221056149525,16.325231416605,16.3932367294691,16.4974784029602,16.6015636324797,
16.7055247443385,16.8094190773204,16.9132813279835,17.0171461480443,17.1211170127319,
17.2251453032834,17.3293527949952,17.3907845878152,17.495130558486,17.6047989097489,
17.7088743312222,17.8128826024111,17.9168653850884,17.9338039635375),
 .UNSPECIFIED.);
#2687=B_SPLINE_CURVE_WITH_KNOTS('',3,(#97657,#97658,#97659,#97660,#97661),
 .UNSPECIFIED.,.F.,.F.,(4,1,4),(14.3981410127769,15.395688871123,15.7079548497411),
 .UNSPECIFIED.);
#2688=B_SPLINE_CURVE_WITH_KNOTS('',3,(#97665,#97666,#97667,#97668,#97669,
#97670,#97671,#97672,#97673,#97674,#97675,#97676,#97677,#97678,#97679,#97680,
#97681,#97682,#97683,#97684,#97685,#97686,#97687,#97688,#97689,#97690,#97691,
#97692,#97693,#97694,#97695,#97696,#97697,#97698,#97699,#97700,#97701,#97702,
#97703,#97704,#97705,#97706,#97707,#97708,#97709,#97710,#97711,#97712,#97713,
#97714,#97715,#97716,#97717,#97718,#97719,#97720,#97721,#97722),
 .UNSPECIFIED.,.F.,.F.,(4,3,3,3,3,3,3,3,3,3,3,3,3,3,3,3,3,3,3,4),(13.8761929392347,
13.9800702154537,14.0837917405706,14.1873910108393,14.2909252293335,14.3944296203396,
14.4979393650901,14.6015560560448,14.7052336748237,14.809084909705,14.8542235792949,
14.9609410403269,15.0635682984915,15.1661015202186,15.2685772625233,15.3710319999417,
15.473553733857,15.5761160252208,15.6788141359347,15.7079632675506),
 .UNSPECIFIED.);
#2689=B_SPLINE_CURVE_WITH_KNOTS('',3,(#97723,#97724,#97725,#97726,#97727,
#97728,#97729,#97730,#97731,#97732,#97733,#97734,#97735,#97736,#97737,#97738,
#97739,#97740,#97741,#97742,#97743,#97744,#97745,#97746,#97747,#97748,#97749,
#97750,#97751,#97752,#97753,#97754,#97755,#97756,#97757,#97758,#97759,#97760,
#97761,#97762,#97763,#97764,#97765,#97766,#97767,#97768,#97769,#97770,#97771,
#97772,#97773,#97774,#97775,#97776,#97777,#97778,#97779,#97780,#97781,#97782,
#97783,#97784,#97785,#97786,#97787,#97788,#97789),.UNSPECIFIED.,.F.,.F.,
(4,3,3,3,3,3,3,3,3,3,3,3,3,3,3,3,3,3,3,3,3,3,4),(15.7079632679489,15.851771437641,
15.9558570373361,16.0597859454429,16.1635911514287,16.2673299233138,16.3710371942513,
16.4747478530179,16.5785668897293,16.682444439463,16.7865045674077,16.8493192959871,
16.9535191120831,17.0575636601841,17.1614860602557,17.2653429233163,17.3691690078,
17.4729990286134,17.5769374445946,17.6809345655956,17.7851132688137,17.8468671543332,
17.9343865323097),.UNSPECIFIED.);
#2690=B_SPLINE_CURVE_WITH_KNOTS('',3,(#97795,#97796,#97797,#97798,#97799,
#97800,#97801,#97802),.UNSPECIFIED.,.F.,.F.,(4,1,1,1,1,4),(99.6151611575392,
99.6457915387122,100.643339397058,101.640887255404,102.638435113751,103.635982972097),
 .UNSPECIFIED.);
#2691=B_SPLINE_CURVE_WITH_KNOTS('',3,(#97806,#97807,#97808,#97809,#97810,
#97811,#97812,#97813,#97814,#97815,#97816,#97817,#97818,#97819,#97820,#97821),
 .UNSPECIFIED.,.F.,.F.,(4,3,3,3,3,4),(103.672557568828,103.780299746495,
103.888308824944,103.996463052203,104.104894597203,104.157833373966),
 .UNSPECIFIED.);
#2692=B_SPLINE_CURVE_WITH_KNOTS('',3,(#97822,#97823,#97824,#97825,#97826,
#97827,#97828,#97829,#97830,#97831,#97832,#97833,#97834,#97835,#97836,#97837,
#97838,#97839,#97840,#97841,#97842,#97843,#97844,#97845,#97846,#97847,#97848,
#97849,#97850,#97851,#97852,#97853,#97854,#97855,#97856,#97857,#97858,#97859,
#97860,#97861,#97862,#97863,#97864,#97865,#97866,#97867,#97868,#97869,#97870,
#97871,#97872,#97873,#97874,#97875,#97876,#97877,#97878,#97879,#97880,#97881,
#97882,#97883,#97884,#97885,#97886,#97887,#97888,#97889,#97890,#97891,#97892,
#97893,#97894,#97895,#97896,#97897,#97898,#97899,#97900,#97901,#97902,#97903,
#97904,#97905,#97906,#97907,#97908,#97909,#97910,#97911,#97912,#97913,#97914,
#97915,#97916,#97917,#97918,#97919,#97920,#97921,#97922,#97923,#97924,#97925,
#97926,#97927,#97928,#97929,#97930,#97931,#97932,#97933,#97934,#97935,#97936,
#97937,#97938,#97939,#97940,#97941,#97942,#97943,#97944,#97945),
 .UNSPECIFIED.,.F.,.F.,(4,3,3,3,3,3,3,3,3,3,3,3,3,3,3,3,3,3,3,3,3,3,3,3,
3,3,3,3,3,3,3,3,3,3,3,3,3,3,3,3,3,4),(99.615621384741,99.7194516934841,
99.823289171979,99.9272369721367,100.031246375379,100.135434211443,100.18725683054,
100.291455298671,100.395498790872,100.499420572679,100.603277087823,100.707103094362,
100.810933307106,100.91487232482,101.018870279629,101.123050173999,101.184804688886,
101.28888521047,101.392810209752,101.496613258174,101.600350953578,101.704058227136,
101.807769966774,101.911591721183,102.015472915131,102.119538113885,102.182352547233,
102.286721387124,102.390934549507,102.495024150017,102.599047245106,102.703038351641,
102.807031941819,102.911130600256,103.015286319959,103.119619330251,103.179900405579,
103.289272706435,103.398334640765,103.507209030259,103.615853185506,103.672557568463),
 .UNSPECIFIED.);
#2693=B_SPLINE_CURVE_WITH_KNOTS('',3,(#97951,#97952,#97953,#97954,#97955,
#97956,#97957,#97958,#97959,#97960,#97961,#97962,#97963,#97964,#97965,#97966,
#97967,#97968,#97969,#97970,#97971,#97972,#97973,#97974,#97975,#97976,#97977,
#97978,#97979,#97980,#97981,#97982,#97983,#97984,#97985,#97986,#97987,#97988,
#97989,#97990,#97991,#97992,#97993,#97994,#97995,#97996,#97997,#97998,#97999,
#98000,#98001,#98002,#98003,#98004,#98005,#98006,#98007,#98008,#98009,#98010,
#98011,#98012,#98013,#98014,#98015,#98016,#98017,#98018,#98019,#98020,#98021,
#98022,#98023,#98024,#98025,#98026,#98027,#98028,#98029,#98030,#98031,#98032,
#98033,#98034,#98035,#98036,#98037,#98038,#98039,#98040,#98041,#98042,#98043,
#98044,#98045,#98046,#98047,#98048,#98049,#98050,#98051,#98052,#98053,#98054,
#98055,#98056,#98057,#98058,#98059,#98060,#98061,#98062,#98063,#98064,#98065,
#98066,#98067,#98068,#98069,#98070,#98071,#98072,#98073,#98074,#98075,#98076,
#98077),.UNSPECIFIED.,.F.,.F.,(4,3,3,3,3,3,3,3,3,3,3,3,3,3,3,3,3,3,3,3,
3,3,3,3,3,3,3,3,3,3,3,3,3,3,3,3,3,3,3,3,3,3,4),(93.3317451784711,93.4356908296324,
93.5397089185721,93.6438957389185,93.6605043886357,93.7646924913296,93.8687253455085,
93.9726361406856,94.0764814606864,94.1802960819711,94.2841147375458,94.388042019171,
94.4920281194343,94.5961961038901,94.6580522469818,94.7622408508587,94.8662742477253,
94.970185643822,95.0740316002466,95.1778468922007,95.2816662514685,95.3855942816827,
95.4895811569642,95.5937499492636,95.6556001053279,95.759772961128,95.8637905520596,
95.9676861327482,96.0715162764619,96.1753157816034,96.2791194031735,96.3830318787696,
96.4870032791763,96.5911568906327,96.653147963674,96.7562452892943,96.8592012637035,
96.9620522663221,97.0688822650625,97.1716574089993,97.2744331252244,97.3772781161521,
97.3893722612836),.UNSPECIFIED.);
#2694=B_SPLINE_CURVE_WITH_KNOTS('',3,(#98078,#98079,#98080,#98081,#98082,
#98083),.UNSPECIFIED.,.F.,.F.,(4,1,1,4),(97.3893747331526,97.6506958220201,
98.6482436803662,99.6151611575392),.UNSPECIFIED.);
#2695=B_SPLINE_CURVE_WITH_KNOTS('',3,(#98085,#98086,#98087,#98088,#98089,
#98090,#98091,#98092,#98093,#98094,#98095,#98096,#98097,#98098,#98099,#98100,
#98101,#98102,#98103,#98104,#98105,#98106,#98107,#98108,#98109,#98110,#98111,
#98112,#98113,#98114,#98115,#98116,#98117,#98118,#98119,#98120,#98121,#98122,
#98123,#98124,#98125,#98126,#98127,#98128,#98129,#98130,#98131,#98132,#98133,
#98134,#98135,#98136,#98137,#98138,#98139,#98140,#98141,#98142,#98143,#98144,
#98145,#98146,#98147,#98148,#98149,#98150,#98151),.UNSPECIFIED.,.F.,.F.,
(4,3,3,3,3,3,3,3,3,3,3,3,3,3,3,3,3,3,3,3,3,3,4),(97.3893722616848,97.4918516940551,
97.5942418136602,97.6965792856351,97.7989006986796,97.9013129217246,98.0037693581187,
98.1064097352967,98.1921611138482,98.2963339880605,98.400351597429,98.504247196504,
98.6080773585636,98.7118768819842,98.8156805217399,98.9195930152571,99.0235644334626,
99.1277180623331,99.1897089721943,99.296187075331,99.4002195103592,99.5079204475501,
99.615621384741),.UNSPECIFIED.);
#2696=B_SPLINE_CURVE_WITH_KNOTS('',3,(#98152,#98153,#98154,#98155,#98156,
#98157,#98158,#98159,#98160,#98161,#98162,#98163,#98164,#98165,#98166,#98167,
#98168,#98169,#98170,#98171,#98172,#98173,#98174,#98175,#98176,#98177,#98178,
#98179,#98180,#98181,#98182,#98183,#98184,#98185,#98186,#98187,#98188,#98189,
#98190,#98191,#98192,#98193,#98194,#98195,#98196,#98197,#98198,#98199,#98200,
#98201,#98202,#98203,#98204,#98205,#98206,#98207,#98208,#98209,#98210,#98211,
#98212,#98213,#98214,#98215,#98216,#98217,#98218,#98219,#98220,#98221,#98222,
#98223,#98224,#98225,#98226,#98227,#98228,#98229,#98230,#98231,#98232,#98233,
#98234,#98235,#98236,#98237,#98238,#98239,#98240,#98241,#98242,#98243,#98244,
#98245,#98246,#98247,#98248,#98249,#98250,#98251,#98252,#98253,#98254,#98255,
#98256,#98257,#98258,#98259,#98260,#98261,#98262,#98263,#98264,#98265,#98266,
#98267,#98268,#98269,#98270,#98271,#98272,#98273,#98274,#98275),
 .UNSPECIFIED.,.F.,.F.,(4,3,3,3,3,3,3,3,3,3,3,3,3,3,3,3,3,3,3,3,3,3,3,3,
3,3,3,3,3,3,3,3,3,3,3,3,3,3,3,3,3,4),(93.3327249561973,93.4413805467306,
93.5452680315814,93.6490996786052,93.7529102511427,93.8567344787581,93.960673260205,
94.0646795089325,94.1688591227995,94.2019696804638,94.3061562451431,94.4101875751818,
94.5140968738215,94.6179407150807,94.721753877435,94.8255710959254,94.9294969833574,
95.0334817115056,95.1376483733693,95.1995175388099,95.3037020714602,95.4077313636999,
95.5116386258043,95.6154804324086,95.7192915649643,95.8231067614917,95.9270306527879,
96.0310133963537,96.1351781134134,96.197065397156,96.3012534980456,96.405286350439,
96.5091971438664,96.6130424621404,96.7168570817235,96.8206757356245,96.9246030156287,
97.0285891142985,97.1327570972207,97.1946132555021,97.3456072562199,97.3893722612836),
 .UNSPECIFIED.);
#2697=B_SPLINE_CURVE_WITH_KNOTS('',3,(#98281,#98282,#98283,#98284,#98285,
#98286,#98287,#98288,#98289,#98290,#98291,#98292,#98293,#98294,#98295,#98296,
#98297,#98298,#98299,#98300,#98301,#98302,#98303,#98304,#98305,#98306,#98307,
#98308,#98309,#98310,#98311,#98312,#98313,#98314,#98315,#98316,#98317,#98318,
#98319,#98320,#98321,#98322,#98323,#98324,#98325,#98326,#98327,#98328,#98329,
#98330,#98331,#98332,#98333,#98334,#98335,#98336,#98337,#98338,#98339,#98340,
#98341,#98342,#98343,#98344,#98345,#98346,#98347,#98348,#98349,#98350,#98351,
#98352,#98353,#98354,#98355,#98356,#98357,#98358,#98359,#98360,#98361,#98362,
#98363,#98364,#98365,#98366,#98367,#98368,#98369,#98370,#98371,#98372,#98373,
#98374,#98375,#98376,#98377,#98378,#98379,#98380,#98381,#98382,#98383,#98384,
#98385,#98386,#98387,#98388,#98389,#98390,#98391,#98392,#98393,#98394,#98395,
#98396,#98397,#98398,#98399,#98400,#98401),.UNSPECIFIED.,.F.,.F.,(4,3,3,
3,3,3,3,3,3,3,3,3,3,3,3,3,3,3,3,3,3,3,3,3,3,3,3,3,3,3,3,3,3,3,3,3,3,3,3,
3,4),(87.0493933560106,87.1532149091787,87.2570257190436,87.3615735989225,
87.4655293993329,87.570373318946,87.6752172385592,87.7794034174978,87.8834343579682,
87.9873432632894,88.0911867091357,88.1949994745833,88.2988162952719,88.4027417863115,
88.5067261182652,88.6108923885799,88.6727650969053,88.7769513208292,88.8809823068916,
88.9848912584753,89.088734750972,89.1925475633854,89.2963644312838,89.4002899695733,
89.5042743488706,89.6084406661575,89.6703129552514,89.7744989226349,89.8785296516199,
89.9824383465664,90.0862815828356,90.1900941398043,90.2939107534151,90.3978360409233,
90.5018201710385,90.6059862443694,90.6678608135975,90.7807057004803,90.8932647257622,
91.0053646969276,91.1061869538112),.UNSPECIFIED.);
#2698=B_SPLINE_CURVE_WITH_KNOTS('',3,(#98402,#98403,#98404,#98405,#98406,
#98407,#98408,#98409,#98410,#98411,#98412,#98413,#98414,#98415,#98416,#98417,
#98418,#98419,#98420,#98421,#98422,#98423,#98424,#98425,#98426,#98427,#98428,
#98429,#98430,#98431,#98432,#98433,#98434,#98435,#98436,#98437,#98438,#98439,
#98440,#98441,#98442,#98443,#98444,#98445,#98446,#98447,#98448,#98449,#98450,
#98451,#98452,#98453,#98454,#98455,#98456,#98457,#98458,#98459,#98460,#98461,
#98462,#98463,#98464,#98465,#98466,#98467,#98468,#98469,#98470,#98471),
 .UNSPECIFIED.,.F.,.F.,(4,3,3,3,3,3,3,3,3,3,3,3,3,3,3,3,3,3,3,3,3,3,3,4),
(91.106186954104,91.2125697916978,91.319033886442,91.4256928894083,91.5324648462027,
91.6394568078794,91.6654086719436,91.7695952377474,91.8736265689175,91.9775358686934,
92.0813797110913,92.1851928745849,92.2890100942136,92.3929359827745,92.496920712048,
92.6010873750192,92.6629565302896,92.7671206839459,92.8711399663559,92.9750493942499,
93.078892943413,93.1826980543968,93.2865286010299,93.3317451784711),
 .UNSPECIFIED.);
#2699=B_SPLINE_CURVE_WITH_KNOTS('',3,(#98473,#98474,#98475,#98476,#98477,
#98478,#98479,#98480,#98481,#98482,#98483,#98484,#98485,#98486,#98487,#98488,
#98489,#98490,#98491,#98492,#98493,#98494,#98495,#98496,#98497,#98498,#98499,
#98500,#98501,#98502,#98503,#98504,#98505,#98506,#98507,#98508,#98509,#98510,
#98511,#98512,#98513,#98514,#98515,#98516,#98517,#98518,#98519,#98520,#98521,
#98522,#98523,#98524,#98525,#98526,#98527,#98528,#98529,#98530,#98531,#98532,
#98533,#98534,#98535,#98536,#98537,#98538,#98539,#98540,#98541,#98542),
 .UNSPECIFIED.,.F.,.F.,(4,3,3,3,3,3,3,3,3,3,3,3,3,3,3,3,3,3,3,3,3,3,3,4),
(91.106186954104,91.2093261054256,91.3135123291656,91.4175433150428,91.5214522664409,
91.6252957587517,91.7291085709795,91.8329254386925,91.9368509767983,92.0408353559126,
92.1450016730195,92.2068739637717,92.3110599315904,92.4150906610108,92.5189993563906,
92.6228425930916,92.7266551504905,92.8304717645285,92.934397052457,93.0383811829892,
93.1425472567276,93.2044218221178,93.3086061886958,93.3327249561973),
 .UNSPECIFIED.);
#2700=B_SPLINE_CURVE_WITH_KNOTS('',3,(#98543,#98544,#98545,#98546,#98547,
#98548,#98549,#98550,#98551,#98552,#98553,#98554,#98555,#98556,#98557,#98558,
#98559,#98560,#98561,#98562,#98563,#98564,#98565,#98566,#98567,#98568,#98569,
#98570,#98571,#98572,#98573,#98574,#98575,#98576,#98577,#98578,#98579,#98580,
#98581,#98582,#98583,#98584,#98585,#98586,#98587,#98588,#98589,#98590,#98591,
#98592,#98593,#98594,#98595,#98596,#98597,#98598,#98599,#98600,#98601,#98602,
#98603,#98604,#98605,#98606,#98607,#98608,#98609,#98610,#98611,#98612,#98613,
#98614,#98615,#98616,#98617,#98618,#98619,#98620,#98621,#98622,#98623,#98624,
#98625,#98626,#98627,#98628,#98629,#98630,#98631,#98632,#98633,#98634,#98635,
#98636,#98637,#98638,#98639,#98640,#98641,#98642,#98643,#98644,#98645,#98646,
#98647,#98648,#98649,#98650,#98651,#98652,#98653,#98654,#98655,#98656,#98657,
#98658,#98659,#98660,#98661,#98662,#98663,#98664,#98665,#98666),
 .UNSPECIFIED.,.F.,.F.,(4,3,3,3,3,3,3,3,3,3,3,3,3,3,3,3,3,3,3,3,3,3,3,3,
3,3,3,3,3,3,3,3,3,3,3,3,3,3,3,3,3,4),(87.0484495531988,87.1526139507006,
87.2191346720412,87.3233208365559,87.4273517627696,87.5312606541469,87.6351040862493,
87.7389168381715,87.8427336455721,87.9466591237729,88.0506434431218,88.1548097013355,
88.2166825303873,88.3208687024072,88.4248996361967,88.5288085352171,88.632651975,
88.7364647346284,88.8402815497491,88.9442070356378,89.048191362668,89.1523576284685,
89.2142303887334,89.3184165292674,89.4224474315273,89.5263562991041,89.6301997075135,
89.7340124358838,89.8378292199076,89.9417546751579,90.0457389717619,90.1499052078012,
90.2117782470795,90.3146405331782,90.4173275668627,90.519916847407,90.6224448805082,
90.7249480860865,90.8275243015109,90.9301370934329,91.0329109697359,91.1061869536426),
 .UNSPECIFIED.);
#2701=B_SPLINE_CURVE_WITH_KNOTS('',3,(#98672,#98673,#98674,#98675,#98676,
#98677,#98678,#98679,#98680,#98681,#98682,#98683,#98684,#98685,#98686,#98687,
#98688,#98689,#98690,#98691,#98692,#98693,#98694,#98695,#98696,#98697,#98698,
#98699,#98700,#98701,#98702,#98703,#98704,#98705,#98706,#98707,#98708,#98709,
#98710,#98711,#98712,#98713,#98714,#98715,#98716,#98717,#98718,#98719,#98720,
#98721,#98722,#98723,#98724,#98725,#98726,#98727,#98728,#98729,#98730,#98731,
#98732,#98733,#98734,#98735,#98736,#98737,#98738,#98739,#98740,#98741,#98742,
#98743,#98744,#98745,#98746,#98747,#98748,#98749,#98750,#98751,#98752,#98753,
#98754,#98755,#98756,#98757,#98758,#98759,#98760,#98761,#98762,#98763,#98764,
#98765,#98766,#98767,#98768,#98769,#98770,#98771,#98772,#98773,#98774,#98775,
#98776,#98777,#98778,#98779,#98780,#98781,#98782,#98783,#98784,#98785,#98786,
#98787,#98788,#98789,#98790,#98791,#98792),.UNSPECIFIED.,.F.,.F.,(4,3,3,
3,3,3,3,3,3,3,3,3,3,3,3,3,3,3,3,3,3,3,3,3,3,3,3,3,3,3,3,3,3,3,3,3,3,3,3,
3,4),(80.7662008482215,80.8702730448693,80.974207590904,81.0780665198201,
81.1818846299995,81.2856966661622,81.389610867391,81.4935748111732,81.5977303299521,
81.6899300884827,81.7941162519914,81.8981471772209,82.0020560676505,82.1058994988283,
82.2097122498501,82.3135290563755,82.4174545337454,82.5214388522872,82.6256051097397,
82.6874779468288,82.7916641114795,82.8956950378591,82.9996039294452,83.1034473617827,
83.2072601139657,83.3110769216523,83.4150024001749,83.5189867198666,83.6231529784516,
83.6850258051749,83.7892119660255,83.8932428886023,83.9971517763997,84.1009952049595,
84.2048079533809,84.3086247573275,84.412550232169,84.5165345482068,84.6207008032212,
84.682573663521,84.8230016469244),.UNSPECIFIED.);
#2702=B_SPLINE_CURVE_WITH_KNOTS('',3,(#98793,#98794,#98795,#98796,#98797,
#98798,#98799,#98800,#98801,#98802,#98803,#98804,#98805,#98806,#98807,#98808,
#98809,#98810,#98811,#98812,#98813,#98814,#98815,#98816,#98817,#98818,#98819,
#98820,#98821,#98822,#98823,#98824,#98825,#98826,#98827,#98828,#98829,#98830,
#98831,#98832,#98833,#98834,#98835,#98836,#98837,#98838,#98839,#98840,#98841,
#98842,#98843,#98844,#98845,#98846,#98847,#98848,#98849,#98850,#98851,#98852,
#98853,#98854,#98855,#98856,#98857,#98858,#98859,#98860,#98861,#98862),
 .UNSPECIFIED.,.F.,.F.,(4,3,3,3,3,3,3,3,3,3,3,3,3,3,3,3,3,3,3,3,3,3,3,4),
(84.8230016473375,84.9301416316537,85.0325714163389,85.1349307980786,85.2372563959105,
85.3395847767895,85.4420166362011,85.5445096330654,85.64717105574,85.6801215218671,
85.7843076939159,85.8883386277345,85.9922475267839,86.096090966596,86.1999037262534,
86.3037205414031,86.4076460273204,86.5116303543791,86.6157966202077,86.6776693802131,
86.7818282236142,86.8858513473907,86.9897582188318,87.0493933560106),
 .UNSPECIFIED.);
#2703=B_SPLINE_CURVE_WITH_KNOTS('',3,(#98864,#98865,#98866,#98867,#98868,
#98869,#98870,#98871,#98872,#98873,#98874,#98875,#98876,#98877,#98878,#98879,
#98880,#98881,#98882,#98883,#98884,#98885,#98886,#98887,#98888,#98889,#98890,
#98891,#98892,#98893,#98894,#98895,#98896,#98897,#98898,#98899,#98900,#98901,
#98902,#98903,#98904,#98905,#98906,#98907,#98908,#98909,#98910,#98911,#98912,
#98913,#98914,#98915,#98916,#98917,#98918,#98919,#98920,#98921,#98922,#98923,
#98924,#98925,#98926,#98927,#98928,#98929,#98930),.UNSPECIFIED.,.F.,.F.,
(4,3,3,3,3,3,3,3,3,3,3,3,3,3,3,3,3,3,3,3,3,3,4),(84.8230016473347,84.9376554440844,
85.0527190382953,85.1683359285729,85.2240389553491,85.3282251199953,85.4322560463704,
85.5361649379519,85.640008370285,85.7438211224634,85.8476379301455,85.9515634086638,
86.0555477283509,86.1597139869317,86.2215868136951,86.3257394090962,86.4297517345076,
86.5336587825729,86.6374954230253,86.741335673925,86.8451704422834,86.9491112691442,
87.0484495531988),.UNSPECIFIED.);
#2704=B_SPLINE_CURVE_WITH_KNOTS('',3,(#98931,#98932,#98933,#98934,#98935,
#98936,#98937,#98938,#98939,#98940,#98941,#98942,#98943,#98944,#98945,#98946,
#98947,#98948,#98949,#98950,#98951,#98952,#98953,#98954,#98955,#98956,#98957,
#98958,#98959,#98960,#98961,#98962,#98963,#98964,#98965,#98966,#98967,#98968,
#98969,#98970,#98971,#98972,#98973,#98974,#98975,#98976,#98977,#98978,#98979,
#98980,#98981,#98982,#98983,#98984,#98985,#98986,#98987,#98988,#98989,#98990,
#98991,#98992,#98993,#98994,#98995,#98996,#98997,#98998,#98999,#99000,#99001,
#99002,#99003,#99004,#99005,#99006,#99007,#99008,#99009,#99010,#99011,#99012,
#99013,#99014,#99015,#99016,#99017,#99018,#99019,#99020,#99021,#99022,#99023,
#99024,#99025,#99026,#99027,#99028,#99029,#99030,#99031,#99032,#99033,#99034,
#99035,#99036,#99037,#99038,#99039,#99040,#99041,#99042,#99043,#99044,#99045,
#99046,#99047,#99048,#99049,#99050,#99051,#99052,#99053,#99054),
 .UNSPECIFIED.,.F.,.F.,(4,3,3,3,3,3,3,3,3,3,3,3,3,3,3,3,3,3,3,3,3,3,3,3,
3,3,3,3,3,3,3,3,3,3,3,3,3,3,3,3,3,4),(80.7657457599978,80.8695647107879,
80.9734943449784,81.0774857249014,81.1816560975386,81.2338475219647,81.3380336854428,
81.4420646106446,81.5459735010506,81.6498169322074,81.7536296832108,81.8574464897206,
81.9613719670788,82.065356285611,82.1695225430577,82.2313953803108,82.335581543951,
82.439612469316,82.5435213598856,82.6473647912064,82.7511775423736,82.8549943490468,
82.9589198265672,83.0629041452611,83.1670704028666,83.2289432386569,83.3331294018515,
83.4371603267706,83.5410692168966,83.6449126477754,83.748725398503,83.8525422047394,
83.95646768183,84.0604520000977,84.1646182572869,84.226491097003,84.3322636668441,
84.437865290237,84.5433026045784,84.6486432044847,84.7539210445246,84.8230016469244),
 .UNSPECIFIED.);
#2705=B_SPLINE_CURVE_WITH_KNOTS('',3,(#99060,#99061,#99062,#99063,#99064,
#99065,#99066,#99067,#99068,#99069,#99070,#99071,#99072,#99073,#99074,#99075,
#99076,#99077,#99078,#99079,#99080,#99081,#99082,#99083,#99084,#99085,#99086,
#99087,#99088,#99089,#99090,#99091,#99092,#99093,#99094,#99095,#99096,#99097,
#99098,#99099,#99100,#99101,#99102,#99103,#99104,#99105,#99106,#99107,#99108,
#99109,#99110,#99111,#99112,#99113,#99114,#99115,#99116,#99117,#99118,#99119,
#99120,#99121,#99122,#99123,#99124,#99125,#99126,#99127,#99128,#99129,#99130,
#99131,#99132,#99133,#99134,#99135,#99136,#99137,#99138,#99139,#99140,#99141,
#99142,#99143,#99144,#99145,#99146,#99147,#99148,#99149,#99150,#99151,#99152,
#99153,#99154,#99155,#99156,#99157,#99158,#99159,#99160,#99161,#99162,#99163,
#99164,#99165,#99166,#99167,#99168,#99169,#99170,#99171,#99172,#99173,#99174,
#99175,#99176,#99177,#99178,#99179,#99180,#99181,#99182,#99183,#99184,#99185,
#99186),.UNSPECIFIED.,.F.,.F.,(4,3,3,3,3,3,3,3,3,3,3,3,3,3,3,3,3,3,3,3,
3,3,3,3,3,3,3,3,3,3,3,3,3,3,3,3,3,3,3,3,3,3,4),(74.4820629741015,74.5860824401791,
74.6902706699235,74.7070950800601,74.8112812435448,74.9153121687535,75.0192210591671,
75.1230644903318,75.2268772413434,75.3306940478616,75.4346195252287,75.5386038437702,
75.6427701012263,75.7046429384062,75.8088291018918,75.9128600271013,76.0167689175156,
76.120612348681,76.2244250996931,76.3282419062119,76.4321673835794,76.5361517021214,
76.6403179595778,76.7021907967523,76.8063769602599,76.9104078854914,77.0143167759279,
77.1181602071154,77.2219729581496,77.3257897646905,77.4297152420799,77.5336995606436,
77.6378658181213,77.6997386550983,77.8047483656343,77.9072108121797,78.0095758369587,
78.111880162764,78.2188642069196,78.3212057260103,78.4235870713438,78.526093732632,
78.5398163393865),.UNSPECIFIED.);
#2706=B_SPLINE_CURVE_WITH_KNOTS('',3,(#99187,#99188,#99189,#99190,#99191,
#99192,#99193,#99194,#99195,#99196,#99197,#99198,#99199,#99200,#99201,#99202,
#99203,#99204,#99205,#99206,#99207,#99208,#99209,#99210,#99211,#99212,#99213,
#99214,#99215,#99216,#99217,#99218,#99219,#99220,#99221,#99222,#99223,#99224,
#99225,#99226,#99227,#99228,#99229,#99230,#99231,#99232,#99233,#99234,#99235,
#99236,#99237,#99238,#99239,#99240,#99241,#99242,#99243,#99244,#99245,#99246,
#99247,#99248,#99249,#99250,#99251,#99252,#99253),.UNSPECIFIED.,.F.,.F.,
(4,3,3,3,3,3,3,3,3,3,3,3,3,3,3,3,3,3,3,3,3,3,4),(78.5398163397448,78.6972865134445,
78.8014726769226,78.9055036021242,79.0094124925302,79.1132559236869,79.2170686746902,
79.3208854811998,79.4248109585579,79.5287952770901,79.6329615345367,79.6948343717905,
79.7990205354315,79.9030514607969,80.0069603513672,80.1108037826886,80.2146165338564,
80.3184333405304,80.4223588180514,80.5263431367459,80.630509394352,80.6923822301366,
80.7662008482215),.UNSPECIFIED.);
#2707=B_SPLINE_CURVE_WITH_KNOTS('',3,(#99255,#99256,#99257,#99258,#99259,
#99260,#99261,#99262,#99263,#99264,#99265,#99266,#99267,#99268,#99269,#99270,
#99271,#99272,#99273,#99274,#99275,#99276,#99277,#99278,#99279,#99280,#99281,
#99282,#99283,#99284,#99285,#99286,#99287,#99288,#99289,#99290,#99291,#99292,
#99293,#99294,#99295,#99296,#99297,#99298,#99299,#99300,#99301,#99302,#99303,
#99304,#99305,#99306,#99307,#99308,#99309,#99310,#99311,#99312,#99313,#99314,
#99315,#99316,#99317,#99318,#99319,#99320,#99321),.UNSPECIFIED.,.F.,.F.,
(4,3,3,3,3,3,3,3,3,3,3,3,3,3,3,3,3,3,3,3,3,3,4),(78.5398163397448,78.6430480181532,
78.7462408136039,78.8494302891181,78.9527248465574,79.0560730500088,79.159611215973,
79.2387518052725,79.3429379687799,79.4469688940115,79.5508777844477,79.6547212156351,
79.7585339666693,79.8623507732101,79.9662762505993,80.0702605691627,80.1744268266403,
80.2362996636186,80.3404816769743,80.4467976977302,80.5507026804229,80.6582242202103,
80.7657457599978),.UNSPECIFIED.);
#2708=B_SPLINE_CURVE_WITH_KNOTS('',3,(#99322,#99323,#99324,#99325,#99326,
#99327,#99328,#99329,#99330,#99331,#99332,#99333,#99334,#99335,#99336,#99337,
#99338,#99339,#99340,#99341,#99342,#99343,#99344,#99345,#99346,#99347,#99348,
#99349,#99350,#99351,#99352,#99353,#99354,#99355,#99356,#99357,#99358,#99359,
#99360,#99361,#99362,#99363,#99364,#99365,#99366,#99367,#99368,#99369,#99370,
#99371,#99372,#99373,#99374,#99375,#99376,#99377,#99378,#99379,#99380,#99381,
#99382,#99383,#99384,#99385,#99386,#99387,#99388,#99389,#99390,#99391,#99392,
#99393,#99394,#99395,#99396,#99397,#99398,#99399,#99400,#99401,#99402,#99403,
#99404,#99405,#99406,#99407,#99408,#99409,#99410,#99411,#99412,#99413,#99414,
#99415,#99416,#99417,#99418,#99419,#99420,#99421,#99422,#99423,#99424,#99425,
#99426,#99427,#99428,#99429,#99430,#99431,#99432,#99433,#99434,#99435,#99436,
#99437,#99438,#99439,#99440,#99441,#99442,#99443,#99444,#99445),
 .UNSPECIFIED.,.F.,.F.,(4,3,3,3,3,3,3,3,3,3,3,3,3,3,3,3,3,3,3,3,3,3,3,3,
3,3,3,3,3,3,3,3,3,3,3,3,3,3,3,3,3,4),(74.4832444084144,74.5871350821012,
74.6909683376155,74.7947789409073,74.8986016225652,75.0025379131712,75.1065402542367,
75.2107173371283,75.2485603718882,75.3527465353759,75.4567774605873,75.5606863510037,
75.6645297821712,75.7683425331857,75.8721593397066,75.9760848170764,76.0800691356207,
76.1842353930795,76.2461082302343,76.3502943937249,76.4543253189395,76.5582342093588,
76.6620776405292,76.7658903915466,76.8697071980705,76.9736326754433,77.0776169939903,
77.1817832514518,77.2436560885804,77.3478422520654,77.4518731772744,77.5557820676882,
77.6596254988533,77.7634382498651,77.8672550563838,77.9711805337513,78.0751648522932,
78.1793311097497,78.2412039469264,78.3682032551631,78.4934616304309,78.5398163394195),
 .UNSPECIFIED.);
#2709=B_SPLINE_CURVE_WITH_KNOTS('',3,(#99451,#99452,#99453,#99454,#99455,
#99456,#99457,#99458,#99459,#99460,#99461,#99462,#99463,#99464,#99465,#99466,
#99467,#99468,#99469,#99470,#99471,#99472,#99473,#99474,#99475,#99476,#99477,
#99478,#99479,#99480,#99481,#99482,#99483,#99484,#99485,#99486,#99487,#99488,
#99489,#99490,#99491,#99492,#99493,#99494,#99495,#99496,#99497,#99498,#99499,
#99500,#99501,#99502,#99503,#99504,#99505,#99506,#99507,#99508,#99509,#99510,
#99511,#99512,#99513,#99514,#99515,#99516,#99517,#99518,#99519,#99520,#99521,
#99522,#99523,#99524,#99525,#99526,#99527,#99528,#99529,#99530,#99531,#99532,
#99533,#99534,#99535,#99536,#99537,#99538,#99539,#99540,#99541,#99542,#99543,
#99544,#99545,#99546,#99547,#99548,#99549,#99550,#99551,#99552,#99553,#99554,
#99555,#99556,#99557,#99558,#99559,#99560,#99561,#99562,#99563,#99564,#99565,
#99566,#99567,#99568,#99569,#99570,#99571),.UNSPECIFIED.,.F.,.F.,(4,3,3,
3,3,3,3,3,3,3,3,3,3,3,3,3,3,3,3,3,3,3,3,3,3,3,3,3,3,3,3,3,3,3,3,3,3,3,3,
3,4),(68.1995422682746,68.3033530840735,68.407966795551,68.5119225014276,
68.6168652157056,68.7218079299836,68.8259940934719,68.9300250186842,69.0339339091014,
69.1377773402697,69.2415900912848,69.3454068978068,69.4493323751773,69.5533166937223,
69.6574829511817,69.7193557883297,69.8235419518177,69.9275728770298,70.0314817674467,
70.1353251986146,70.2391379496294,70.3429547561507,70.4468802335209,70.5508645520653,
70.6550308095243,70.7169036466757,70.821089810164,70.9251207353765,71.0290296257937,
71.132873056962,71.2366858079771,71.3405026144985,71.4444280918692,71.5484124104144,
71.6525786678739,71.7144515050218,71.8220784528942,71.930716597812,72.0379272940092,
72.1472791632872,72.2566310325652),.UNSPECIFIED.);
#2710=B_SPLINE_CURVE_WITH_KNOTS('',3,(#99572,#99573,#99574,#99575,#99576,
#99577,#99578,#99579,#99580,#99581,#99582,#99583,#99584,#99585,#99586,#99587,
#99588,#99589,#99590,#99591,#99592,#99593,#99594,#99595,#99596,#99597,#99598,
#99599,#99600,#99601,#99602,#99603,#99604,#99605,#99606,#99607,#99608,#99609,
#99610,#99611,#99612,#99613,#99614,#99615,#99616,#99617,#99618,#99619,#99620,
#99621,#99622,#99623,#99624,#99625,#99626,#99627,#99628,#99629,#99630,#99631,
#99632,#99633,#99634,#99635,#99636,#99637,#99638),.UNSPECIFIED.,.F.,.F.,
(4,3,3,3,3,3,3,3,3,3,3,3,3,3,3,3,3,3,3,3,3,3,4),(72.2566310330023,72.3704731155937,
72.4818133112494,72.5969063373086,72.7119993633679,72.8161855268553,72.9202164520667,
73.0241253424829,73.1279687736503,73.2317815246645,73.3355983311853,73.439523808555,
73.5435081270989,73.6476743845574,73.709547221714,73.8137037283061,73.9177183843876,
74.0216261896506,74.1254620184434,74.2292882434002,74.3331083610432,74.4370016429324,
74.4820629741015),.UNSPECIFIED.);
#2711=B_SPLINE_CURVE_WITH_KNOTS('',3,(#99640,#99641,#99642,#99643,#99644,
#99645,#99646,#99647,#99648,#99649,#99650,#99651,#99652,#99653,#99654,#99655,
#99656,#99657,#99658,#99659,#99660,#99661,#99662,#99663,#99664,#99665,#99666,
#99667,#99668,#99669,#99670,#99671,#99672,#99673,#99674,#99675,#99676,#99677,
#99678,#99679,#99680,#99681,#99682,#99683,#99684,#99685,#99686,#99687,#99688,
#99689,#99690,#99691,#99692,#99693,#99694,#99695,#99696,#99697,#99698,#99699,
#99700,#99701,#99702,#99703,#99704,#99705,#99706,#99707,#99708,#99709),
 .UNSPECIFIED.,.F.,.F.,(4,3,3,3,3,3,3,3,3,3,3,3,3,3,3,3,3,3,3,3,3,3,3,4),
(72.256631032763,72.3608036976092,72.4648211350913,72.5687165873283,72.6725466328826,
72.7763460712598,72.8801496585883,72.9840619406992,73.0880331868138,73.1921861591871,
73.253464655196,73.3576508186844,73.4616817438966,73.5655906343139,73.6694340654822,
73.7732468164974,73.8770636230193,73.9809891003899,74.084973418935,74.1891396763946,
74.2510125135421,74.3552035665601,74.4592285332565,74.4832444084144),
 .UNSPECIFIED.);
#2712=B_SPLINE_CURVE_WITH_KNOTS('',3,(#99710,#99711,#99712,#99713,#99714,
#99715,#99716,#99717,#99718,#99719,#99720,#99721,#99722,#99723,#99724,#99725,
#99726,#99727,#99728,#99729,#99730,#99731,#99732,#99733,#99734,#99735,#99736,
#99737,#99738,#99739,#99740,#99741,#99742,#99743,#99744,#99745,#99746,#99747,
#99748,#99749,#99750,#99751,#99752,#99753,#99754,#99755,#99756,#99757,#99758,
#99759,#99760,#99761,#99762,#99763,#99764,#99765,#99766,#99767,#99768,#99769,
#99770,#99771,#99772,#99773,#99774,#99775,#99776,#99777,#99778,#99779,#99780,
#99781,#99782,#99783,#99784,#99785,#99786,#99787,#99788,#99789,#99790,#99791,
#99792,#99793,#99794,#99795,#99796,#99797,#99798,#99799,#99800,#99801,#99802,
#99803,#99804,#99805,#99806,#99807,#99808,#99809,#99810,#99811,#99812,#99813,
#99814,#99815,#99816,#99817,#99818,#99819,#99820,#99821,#99822,#99823,#99824,
#99825,#99826,#99827,#99828,#99829,#99830,#99831,#99832,#99833,#99834,#99835,
#99836),.UNSPECIFIED.,.F.,.F.,(4,3,3,3,3,3,3,3,3,3,3,3,3,3,3,3,3,3,3,3,
3,3,3,3,3,3,3,3,3,3,3,3,3,3,3,3,3,3,3,3,3,3,4),(68.1991363933835,68.2657253634656,
68.3699115269538,68.4739424521661,68.5778513425831,68.6816947737513,68.7855075247663,
68.8893243312879,68.9932498086583,69.0972341272032,69.2014003846625,69.2632732218117,
69.3674593852998,69.4714903105119,69.5753992009287,69.6792426320967,69.7830553831116,
69.886872189633,69.9907976670033,70.094781985548,70.1989482430071,70.2608210801578,
70.3650072436461,70.4690381688584,70.5729470592755,70.6767904904437,70.7806032414588,
70.8844200479804,70.988345525351,71.0923298438958,71.1964961013552,71.2583689385038,
71.3625551019916,71.4665860272034,71.57049491762,71.6743383487877,71.7781510998022,
71.8819679063233,71.9858933836933,72.0898777022377,72.1940439596966,72.2559167968499,
72.2566310325399),.UNSPECIFIED.);
#2713=B_SPLINE_CURVE_WITH_KNOTS('',3,(#99842,#99843,#99844,#99845,#99846,
#99847,#99848,#99849,#99850,#99851,#99852,#99853,#99854,#99855,#99856,#99857,
#99858,#99859,#99860,#99861,#99862,#99863,#99864,#99865,#99866,#99867,#99868,
#99869,#99870,#99871,#99872,#99873,#99874,#99875,#99876,#99877,#99878,#99879,
#99880,#99881,#99882,#99883,#99884,#99885,#99886,#99887,#99888,#99889,#99890,
#99891,#99892,#99893,#99894,#99895,#99896,#99897,#99898,#99899,#99900,#99901,
#99902,#99903,#99904,#99905,#99906,#99907,#99908,#99909,#99910,#99911,#99912,
#99913,#99914,#99915,#99916,#99917,#99918,#99919,#99920,#99921,#99922,#99923,
#99924,#99925,#99926,#99927,#99928,#99929,#99930,#99931,#99932,#99933,#99934,
#99935,#99936,#99937,#99938,#99939,#99940,#99941,#99942,#99943,#99944,#99945,
#99946,#99947,#99948,#99949,#99950,#99951,#99952,#99953,#99954,#99955,#99956,
#99957,#99958,#99959,#99960,#99961,#99962),.UNSPECIFIED.,.F.,.F.,(4,3,3,
3,3,3,3,3,3,3,3,3,3,3,3,3,3,3,3,3,3,3,3,3,3,3,3,3,3,3,3,3,3,3,3,3,3,3,3,
3,4),(61.9168665188216,62.0208010626594,62.1246599903092,62.2284781001507,
62.3322901369026,62.4362043393257,62.540168285134,62.6443238050195,62.7365207799071,
62.8407069433951,62.944737868607,63.0486467590238,63.1524901901917,63.2563029412064,
63.3601197477278,63.464045225098,63.5680295436425,63.6721958011016,63.7340686382531,
63.8382548017414,63.9422857269537,64.0461946173708,64.1500380485391,64.2538507995541,
64.3576676060758,64.4615930834463,64.5655774019912,64.6697436594505,64.7316164965992,
64.8358026600872,64.9398335852992,65.043742475716,65.147585906884,65.2513986578988,
65.3552154644202,65.4591409417905,65.5631252603351,65.6672915177942,65.7291643549453,
65.8652061647753,65.9734457249409),.UNSPECIFIED.);
#2714=B_SPLINE_CURVE_WITH_KNOTS('',3,(#99963,#99964,#99965,#99966,#99967,
#99968,#99969,#99970,#99971,#99972,#99973,#99974,#99975,#99976,#99977,#99978,
#99979,#99980,#99981,#99982,#99983,#99984,#99985,#99986,#99987,#99988,#99989,
#99990,#99991,#99992,#99993,#99994,#99995,#99996,#99997,#99998,#99999,#100000,
#100001,#100002,#100003,#100004,#100005,#100006,#100007,#100008,#100009,
#100010,#100011,#100012,#100013,#100014,#100015,#100016,#100017,#100018,
#100019,#100020,#100021,#100022,#100023,#100024,#100025,#100026,#100027,
#100028,#100029,#100030,#100031,#100032),.UNSPECIFIED.,.F.,.F.,(4,3,3,3,
3,3,3,3,3,3,3,3,3,3,3,3,3,3,3,3,3,3,3,4),(65.9734457253856,66.07613177282,
66.1787500761624,66.2813369783481,66.3839287747712,66.4866268116111,66.5893873525251,
66.6923186639457,66.7267122132914,66.8308983767795,66.9349293019917,67.0388381924087,
67.1426816235768,67.2464943745917,67.3503111811132,67.4542366584835,67.5582209770282,
67.6623872344874,67.7242600716375,67.8284495547535,67.9324611620825,68.0363696459528,
68.14021127526,68.1995422682746),.UNSPECIFIED.);
#2715=B_SPLINE_CURVE_WITH_KNOTS('',3,(#100034,#100035,#100036,#100037,#100038,
#100039,#100040,#100041,#100042,#100043,#100044,#100045,#100046,#100047,
#100048,#100049,#100050,#100051,#100052,#100053,#100054,#100055,#100056,
#100057,#100058,#100059,#100060,#100061,#100062,#100063,#100064,#100065,
#100066,#100067,#100068,#100069,#100070,#100071,#100072,#100073,#100074,
#100075,#100076,#100077,#100078,#100079,#100080,#100081,#100082,#100083,
#100084,#100085,#100086,#100087,#100088,#100089,#100090,#100091,#100092,
#100093,#100094,#100095,#100096,#100097,#100098,#100099,#100100),
 .UNSPECIFIED.,.F.,.F.,(4,3,3,3,3,3,3,3,3,3,3,3,3,3,3,3,3,3,3,3,3,3,4),
(65.9734457257054,66.0987387055914,66.2258330924359,66.2706296467734,66.3748158102617,
66.4788467354739,66.582755625891,66.6865990570592,66.7904118080743,66.8942286145959,
66.9981540919664,67.1021384105113,67.2063046679707,67.2681775051195,67.3723684096495,
67.4763780581658,67.580285456749,67.6841254673978,67.7879328706231,67.8918030329315,
67.995700074319,68.0997567598127,68.1991363933835),.UNSPECIFIED.);
#2716=B_SPLINE_CURVE_WITH_KNOTS('',3,(#100101,#100102,#100103,#100104,#100105,
#100106,#100107,#100108,#100109,#100110,#100111,#100112,#100113,#100114,
#100115,#100116,#100117,#100118,#100119,#100120,#100121,#100122,#100123,
#100124,#100125,#100126,#100127,#100128,#100129,#100130,#100131,#100132,
#100133,#100134,#100135,#100136,#100137,#100138,#100139,#100140,#100141,
#100142,#100143,#100144,#100145,#100146,#100147,#100148,#100149,#100150,
#100151,#100152,#100153,#100154,#100155,#100156,#100157,#100158,#100159,
#100160,#100161,#100162,#100163,#100164,#100165,#100166,#100167,#100168,
#100169,#100170,#100171,#100172,#100173,#100174,#100175,#100176,#100177,
#100178,#100179,#100180,#100181,#100182,#100183,#100184,#100185,#100186,
#100187,#100188,#100189,#100190,#100191,#100192,#100193,#100194,#100195,
#100196,#100197,#100198,#100199,#100200,#100201,#100202,#100203,#100204,
#100205,#100206,#100207,#100208,#100209,#100210,#100211,#100212,#100213,
#100214,#100215,#100216,#100217,#100218,#100219,#100220,#100221,#100222,
#100223,#100224),.UNSPECIFIED.,.F.,.F.,(4,3,3,3,3,3,3,3,3,3,3,3,3,3,3,3,
3,3,3,3,3,3,3,3,3,3,3,3,3,3,3,3,3,3,3,3,3,3,3,3,3,4),(61.9158990352648,
62.0198285557511,62.1238197449305,62.2279900041556,62.2804382133891,62.3846243768772,
62.4886553020892,62.5925641925061,62.6964076236741,62.8002203746889,62.9040371812104,
63.0079626585807,63.1119469771254,63.2161132345845,63.2779860717351,63.3821722352233,
63.4862031604357,63.5901120508526,63.6939554820208,63.7977682330357,63.9015850395572,
64.0055105169275,64.1094948354721,64.2136610929314,64.2755339300812,64.3797200935694,
64.4837510187817,64.5876599091986,64.6915033403668,64.7953160913816,64.899132897903,
65.0030583752734,65.1070426938181,65.2112089512772,65.2730817884273,65.3766017373241,
65.4799760620947,65.583240636247,65.6864470474344,65.7896160420592,65.8928309399432,
65.9734457253856),.UNSPECIFIED.);
#2717=B_SPLINE_CURVE_WITH_KNOTS('',3,(#100230,#100231,#100232,#100233,#100234,
#100235,#100236,#100237,#100238,#100239,#100240,#100241,#100242,#100243,
#100244,#100245,#100246,#100247,#100248,#100249,#100250,#100251,#100252,
#100253,#100254,#100255,#100256,#100257,#100258,#100259,#100260,#100261,
#100262,#100263,#100264,#100265,#100266,#100267,#100268,#100269,#100270,
#100271,#100272,#100273,#100274,#100275,#100276,#100277,#100278,#100279,
#100280,#100281,#100282,#100283,#100284,#100285,#100286,#100287,#100288,
#100289,#100290,#100291,#100292,#100293,#100294,#100295,#100296,#100297,
#100298,#100299,#100300,#100301,#100302,#100303,#100304,#100305,#100306,
#100307,#100308,#100309,#100310,#100311,#100312,#100313,#100314,#100315,
#100316,#100317,#100318,#100319,#100320,#100321,#100322,#100323,#100324,
#100325,#100326,#100327,#100328,#100329,#100330,#100331,#100332,#100333,
#100334,#100335,#100336,#100337,#100338,#100339,#100340,#100341,#100342,
#100343,#100344,#100345,#100346,#100347,#100348,#100349,#100350,#100351,
#100352,#100353),.UNSPECIFIED.,.F.,.F.,(4,3,3,3,3,3,3,3,3,3,3,3,3,3,3,3,
3,3,3,3,3,3,3,3,3,3,3,3,3,3,3,3,3,3,3,3,3,3,3,3,3,4),(55.6326004204955,
55.7367886089557,55.7536857714844,55.8578719349727,55.961902860185,56.065811750602,
56.1696551817703,56.2734679327853,56.3772847393069,56.4812102166774,56.5851945352223,
56.6893607926816,56.7512336298305,56.8554197933186,56.9594507185306,57.0633596089474,
57.1672030401154,57.2710157911302,57.3748325976516,57.4787580750219,57.5827423935665,
57.6869086510257,57.7487814881766,57.8529676516648,57.956998576877,58.060907467294,
58.1647508984621,58.2685636494771,58.3723804559986,58.4763059333691,58.5802902519139,
58.6844565093732,58.7463293465227,58.8496743122095,58.9547475754162,59.0578171667579,
59.1608249277453,59.2638067574362,59.370420172543,59.4735201525627,59.5818902852131,
59.6902604178635),.UNSPECIFIED.);
#2718=B_SPLINE_CURVE_WITH_KNOTS('',3,(#100354,#100355,#100356,#100357,#100358,
#100359,#100360,#100361,#100362,#100363,#100364,#100365,#100366,#100367,
#100368,#100369,#100370,#100371,#100372,#100373,#100374,#100375,#100376,
#100377,#100378,#100379,#100380,#100381,#100382,#100383,#100384,#100385,
#100386,#100387,#100388,#100389,#100390,#100391,#100392,#100393,#100394,
#100395,#100396,#100397,#100398,#100399,#100400,#100401,#100402,#100403,
#100404,#100405,#100406,#100407,#100408,#100409,#100410,#100411,#100412,
#100413,#100414,#100415,#100416,#100417,#100418,#100419,#100420,#100421,
#100422,#100423),.UNSPECIFIED.,.F.,.F.,(4,3,3,3,3,3,3,3,3,3,3,3,3,3,3,3,
3,3,3,3,3,3,3,4),(59.690260418206,59.7438772048688,59.8480633683569,59.952094293569,
60.0560031839859,60.1598466151539,60.2636593661687,60.36747617269,60.4714016500603,
60.5753859686049,60.6795522260641,60.7414250632149,60.8456112267031,60.9496421519152,
61.0535510423322,61.1573944735003,61.2612072245153,61.3650240310368,61.4689495084072,
61.5729338269519,61.6771000844112,61.738972921561,61.8431345912322,61.9168665188216),
 .UNSPECIFIED.);
#2719=B_SPLINE_CURVE_WITH_KNOTS('',3,(#100425,#100426,#100427,#100428,#100429,
#100430,#100431,#100432,#100433,#100434,#100435,#100436,#100437,#100438,
#100439,#100440,#100441,#100442,#100443,#100444,#100445,#100446,#100447,
#100448,#100449,#100450,#100451,#100452,#100453,#100454,#100455,#100456,
#100457,#100458,#100459,#100460,#100461,#100462,#100463,#100464,#100465,
#100466,#100467,#100468,#100469,#100470,#100471,#100472,#100473,#100474,
#100475,#100476,#100477,#100478,#100479,#100480,#100481,#100482,#100483,
#100484,#100485,#100486,#100487,#100488,#100489,#100490,#100491),
 .UNSPECIFIED.,.F.,.F.,(4,3,3,3,3,3,3,3,3,3,3,3,3,3,3,3,3,3,3,3,3,3,4),
(59.690260418206,59.7955628120765,59.9009059652381,60.0064057077467,60.1119895277649,
60.2177899509138,60.2853424966969,60.3895286601851,60.4935595853973,60.5974684758143,
60.7013119069824,60.8051246579975,60.9089414645192,61.0128669418897,61.1168512604345,
61.2210175178938,61.282890355043,61.3870598977049,61.4910835289864,61.597287405556,
61.7011272946116,61.8085131649381,61.9158990352648),.UNSPECIFIED.);
#2720=B_SPLINE_CURVE_WITH_KNOTS('',3,(#100492,#100493,#100494,#100495,#100496,
#100497,#100498,#100499,#100500,#100501,#100502,#100503,#100504,#100505,
#100506,#100507,#100508,#100509,#100510,#100511,#100512,#100513,#100514,
#100515,#100516,#100517,#100518,#100519,#100520,#100521,#100522,#100523,
#100524,#100525,#100526,#100527,#100528,#100529,#100530,#100531,#100532,
#100533,#100534,#100535,#100536,#100537,#100538,#100539,#100540,#100541,
#100542,#100543,#100544,#100545,#100546,#100547,#100548,#100549,#100550,
#100551,#100552,#100553,#100554,#100555,#100556,#100557,#100558,#100559,
#100560,#100561,#100562,#100563,#100564,#100565,#100566,#100567,#100568,
#100569,#100570,#100571,#100572,#100573,#100574,#100575,#100576,#100577,
#100578,#100579,#100580,#100581,#100582,#100583,#100584,#100585,#100586,
#100587,#100588,#100589,#100590,#100591,#100592,#100593,#100594,#100595,
#100596,#100597,#100598,#100599,#100600,#100601,#100602,#100603,#100604,
#100605,#100606,#100607,#100608,#100609,#100610,#100611,#100612,#100613,
#100614,#100615),.UNSPECIFIED.,.F.,.F.,(4,3,3,3,3,3,3,3,3,3,3,3,3,3,3,3,
3,3,3,3,3,3,3,3,3,3,3,3,3,3,3,3,3,3,3,3,3,3,3,3,3,4),(55.6335493650217,
55.7373826885747,55.8411933008923,55.945015932593,56.0489521376303,56.1529543401164,
56.2571313359375,56.2951510633125,56.3993372268005,56.5033681520124,56.6072770424293,
56.7111204735973,56.8149332246122,56.9187500311337,57.022675508504,57.1266598270485,
57.2308260845077,57.2926989216586,57.3968850851468,57.500916010359,57.604824900776,
57.7086683319441,57.812481082959,57.9162978894807,58.0202233668511,58.124207685396,
58.2283739428553,58.2902467800047,58.3944329434927,58.4984638687049,58.6023727591218,
58.7062161902899,58.8100289413047,58.9138457478264,59.0177712251967,59.1217555437412,
59.2259218012003,59.2877946383508,59.4032420886146,59.5183215991923,59.6327919924132,
59.690260417799),.UNSPECIFIED.);
#2721=B_SPLINE_CURVE_WITH_KNOTS('',3,(#100621,#100622,#100623,#100624,#100625,
#100626,#100627,#100628,#100629,#100630,#100631,#100632,#100633,#100634,
#100635,#100636,#100637,#100638,#100639,#100640,#100641,#100642,#100643,
#100644,#100645,#100646,#100647,#100648,#100649,#100650,#100651,#100652,
#100653,#100654,#100655,#100656,#100657,#100658,#100659,#100660,#100661,
#100662,#100663,#100664,#100665,#100666,#100667,#100668,#100669,#100670,
#100671,#100672,#100673,#100674,#100675,#100676,#100677,#100678,#100679,
#100680,#100681,#100682,#100683,#100684,#100685,#100686,#100687,#100688,
#100689,#100690,#100691,#100692,#100693,#100694,#100695,#100696,#100697,
#100698,#100699,#100700,#100701,#100702,#100703,#100704,#100705,#100706,
#100707,#100708,#100709,#100710,#100711,#100712,#100713,#100714,#100715,
#100716,#100717,#100718,#100719,#100720,#100721,#100722,#100723,#100724,
#100725,#100726,#100727,#100728,#100729,#100730,#100731,#100732,#100733,
#100734,#100735,#100736,#100737,#100738,#100739,#100740,#100741,#100742,
#100743,#100744),.UNSPECIFIED.,.F.,.F.,(4,3,3,3,3,3,3,3,3,3,3,3,3,3,3,3,
3,3,3,3,3,3,3,3,3,3,3,3,3,3,3,3,3,3,3,3,3,3,3,3,3,4),(49.3496724239637,
49.4543539733247,49.5583095592452,49.6633540903265,49.7683986214079,49.8725847848961,
49.9766157101083,50.0805246005253,50.1843680316935,50.2881807827085,50.3919975892302,
50.4959230666006,50.5999073851454,50.7040736426047,50.765946479754,50.8701326432421,
50.9741635684544,51.0780724588712,51.1819158900393,51.2857286410541,51.3895454475756,
51.493470924946,51.5974552434907,51.7016215009499,51.7634943381001,51.8676805015883,
51.9717114268001,52.0756203172171,52.1794637483852,52.2832764994001,52.387093305922,
52.4910187832923,52.5950031018368,52.699169359296,52.7610421964462,52.86555091267,
52.9699037514327,53.0791965913311,53.1833373805671,53.2874304651186,53.3915238347397,
53.4070751110264),.UNSPECIFIED.);
#2722=B_SPLINE_CURVE_WITH_KNOTS('',3,(#100745,#100746,#100747,#100748,#100749,
#100750,#100751,#100752,#100753,#100754,#100755,#100756,#100757,#100758,
#100759,#100760,#100761,#100762,#100763,#100764,#100765,#100766,#100767,
#100768,#100769,#100770,#100771,#100772,#100773,#100774,#100775,#100776,
#100777,#100778,#100779,#100780,#100781,#100782,#100783,#100784,#100785,
#100786,#100787,#100788,#100789,#100790,#100791,#100792,#100793,#100794,
#100795,#100796,#100797,#100798,#100799,#100800,#100801,#100802,#100803,
#100804,#100805,#100806,#100807,#100808,#100809,#100810,#100811),
 .UNSPECIFIED.,.F.,.F.,(4,3,3,3,3,3,3,3,3,3,3,3,3,3,3,3,3,3,3,3,3,3,4),
(53.407075111473,53.5259953052066,53.6459937542086,53.7585900547923,53.8627762182803,
53.9668071434923,54.070716033909,54.174559465077,54.2783722160917,54.3821890226131,
54.4861144999833,54.5900988185279,54.6942650759869,54.7561379131384,54.865695726558,
54.9697002450198,55.0736027363077,55.1774380610522,55.2812409980219,55.3850920226149,
55.4889708980885,55.5929698529969,55.6326004204955),.UNSPECIFIED.);
#2723=B_SPLINE_CURVE_WITH_KNOTS('',3,(#100813,#100814,#100815,#100816,#100817,
#100818,#100819,#100820,#100821,#100822,#100823,#100824,#100825,#100826,
#100827,#100828,#100829,#100830,#100831,#100832,#100833,#100834,#100835,
#100836,#100837,#100838,#100839,#100840,#100841,#100842,#100843,#100844,
#100845,#100846,#100847,#100848,#100849,#100850,#100851,#100852,#100853,
#100854,#100855,#100856,#100857,#100858,#100859,#100860,#100861,#100862,
#100863,#100864,#100865,#100866,#100867,#100868,#100869,#100870,#100871,
#100872,#100873,#100874,#100875,#100876,#100877,#100878,#100879,#100880,
#100881,#100882),.UNSPECIFIED.,.F.,.F.,(4,3,3,3,3,3,3,3,3,3,3,3,3,3,3,3,
3,3,3,3,3,3,3,4),(53.4070751114826,53.509861491319,53.6124973139519,53.7150505550788,
53.8175576893182,53.9200551251618,54.0226483900881,54.1252912590518,54.2281147116727,
54.3000553466204,54.4042415101085,54.5082724353208,54.6121813257378,54.7160247569059,
54.8198375079208,54.9236543144423,55.0275797918127,55.1315641103575,55.2357303678167,
55.2976032049664,55.4017686798842,55.5057980075404,55.609707175149,55.6335493650217),
 .UNSPECIFIED.);
#2724=B_SPLINE_CURVE_WITH_KNOTS('',3,(#100883,#100884,#100885,#100886,#100887,
#100888,#100889,#100890,#100891,#100892,#100893,#100894,#100895,#100896,
#100897,#100898,#100899,#100900,#100901,#100902,#100903,#100904,#100905,
#100906,#100907,#100908,#100909,#100910,#100911,#100912,#100913,#100914,
#100915,#100916,#100917,#100918,#100919,#100920,#100921,#100922,#100923,
#100924,#100925,#100926,#100927,#100928,#100929,#100930,#100931,#100932,
#100933,#100934,#100935,#100936,#100937,#100938,#100939,#100940,#100941,
#100942,#100943,#100944,#100945,#100946,#100947,#100948,#100949,#100950,
#100951,#100952,#100953,#100954,#100955,#100956,#100957,#100958,#100959,
#100960,#100961,#100962,#100963,#100964,#100965,#100966,#100967,#100968,
#100969,#100970,#100971,#100972,#100973,#100974,#100975,#100976,#100977,
#100978,#100979,#100980,#100981,#100982,#100983,#100984,#100985,#100986,
#100987,#100988,#100989,#100990,#100991,#100992,#100993,#100994,#100995,
#100996,#100997,#100998,#100999,#101000,#101001,#101002,#101003,#101004,
#101005,#101006),.UNSPECIFIED.,.F.,.F.,(4,3,3,3,3,3,3,3,3,3,3,3,3,3,3,3,
3,3,3,3,3,3,3,3,3,3,3,3,3,3,3,3,3,3,3,3,3,3,3,3,3,4),(49.3501218890484,
49.4542472707228,49.5611993510369,49.6650784833371,49.7689057717339,49.8727159741616,
49.9820029589302,50.0859506809055,50.1899710955183,50.2941599634125,50.309863913236,
50.4140500767242,50.5180810019363,50.6219898923533,50.7258333235213,50.8296460745363,
50.9334628810577,51.0373883584281,51.1413726769728,51.2455389344321,51.3074117715821,
51.4115979350702,51.5156288602823,51.6195377506992,51.7233811818673,51.8271939328822,
51.9310107394036,52.0349362167739,52.1389205353186,52.2430867927778,52.3049596299282,
52.4091457934165,52.5131767186289,52.6170856090461,52.7209290402144,52.8247417912295,
52.9285585977512,53.0324840751217,53.1364683936667,53.2406346511261,53.3025074882743,
53.4070751110264),.UNSPECIFIED.);
#2725=B_SPLINE_CURVE_WITH_KNOTS('',3,(#101012,#101013,#101014,#101015,#101016,
#101017,#101018,#101019,#101020,#101021,#101022,#101023,#101024,#101025,
#101026,#101027,#101028,#101029,#101030,#101031,#101032,#101033,#101034,
#101035,#101036,#101037,#101038,#101039,#101040,#101041,#101042,#101043,
#101044,#101045,#101046,#101047,#101048,#101049,#101050,#101051,#101052,
#101053,#101054,#101055,#101056,#101057,#101058,#101059,#101060,#101061,
#101062,#101063,#101064,#101065,#101066,#101067,#101068,#101069,#101070,
#101071,#101072,#101073,#101074,#101075,#101076,#101077,#101078,#101079,
#101080,#101081,#101082,#101083,#101084,#101085,#101086,#101087,#101088,
#101089,#101090,#101091,#101092,#101093,#101094,#101095,#101096,#101097,
#101098,#101099,#101100,#101101,#101102,#101103,#101104,#101105,#101106,
#101107,#101108,#101109,#101110,#101111,#101112,#101113,#101114,#101115,
#101116,#101117,#101118,#101119,#101120,#101121,#101122,#101123,#101124,
#101125,#101126,#101127,#101128,#101129,#101130,#101131,#101132),
 .UNSPECIFIED.,.F.,.F.,(4,3,3,3,3,3,3,3,3,3,3,3,3,3,3,3,3,3,3,3,3,3,3,3,
3,3,3,3,3,3,3,3,3,3,3,3,3,3,3,3,4),(43.0672730856169,43.1711320797731,43.2749502164102,
43.3787622402884,43.4826764037649,43.5866402750026,43.6907957592589,43.7831114713314,
43.8872976348198,43.991328560032,44.0952374504493,44.1990808816178,44.3028936326331,
44.406710439155,44.5106359165257,44.6146202350708,44.7187864925303,44.7806593296775,
44.8848454931656,44.9888764183774,45.0927853087944,45.1966287399625,45.3004414909774,
45.4042582974991,45.5081837748694,45.6121680934142,45.7163343508734,45.7782071880236,
45.8823933515121,45.9864242767244,46.0903331671415,46.1941765983097,46.2979893493246,
46.401806155846,46.5057316332165,46.6097159517615,46.7138822092208,46.7757550463697,
46.8962986192121,47.0157785770578,47.123889803403),.UNSPECIFIED.);
#2726=B_SPLINE_CURVE_WITH_KNOTS('',3,(#101133,#101134,#101135,#101136,#101137,
#101138,#101139,#101140,#101141,#101142,#101143,#101144,#101145,#101146,
#101147,#101148,#101149,#101150,#101151,#101152,#101153,#101154,#101155,
#101156,#101157,#101158,#101159,#101160,#101161,#101162,#101163,#101164,
#101165,#101166,#101167,#101168,#101169,#101170,#101171,#101172,#101173,
#101174,#101175,#101176,#101177,#101178,#101179,#101180,#101181,#101182,
#101183,#101184,#101185,#101186,#101187,#101188,#101189,#101190,#101191,
#101192,#101193,#101194,#101195,#101196,#101197,#101198,#101199,#101200,
#101201,#101202),.UNSPECIFIED.,.F.,.F.,(4,3,3,3,3,3,3,3,3,3,3,3,3,3,3,3,
3,3,3,3,3,3,3,4),(47.1238898038469,47.227928135533,47.3319603652871,47.4360206698583,
47.540212755665,47.6444838895238,47.7489375131569,47.7733029047158,47.8774890682039,
47.981519993416,48.0854288838329,48.1892723150009,48.2930850660158,48.3969018725371,
48.5008273499074,48.604811668452,48.7089779259112,48.7708507630618,48.8750265339919,
48.9790548148166,49.0829625294207,49.1867995822529,49.290619011578,49.3496724239637),
 .UNSPECIFIED.);
#2727=B_SPLINE_CURVE_WITH_KNOTS('',3,(#101204,#101205,#101206,#101207,#101208,
#101209,#101210,#101211,#101212,#101213,#101214,#101215,#101216,#101217,
#101218,#101219,#101220,#101221,#101222,#101223,#101224,#101225,#101226,
#101227,#101228,#101229,#101230,#101231,#101232,#101233,#101234,#101235,
#101236,#101237,#101238,#101239,#101240,#101241,#101242,#101243,#101244,
#101245,#101246,#101247,#101248,#101249,#101250,#101251,#101252,#101253,
#101254,#101255,#101256,#101257,#101258,#101259,#101260,#101261,#101262,
#101263,#101264,#101265,#101266,#101267,#101268,#101269,#101270,#101271,
#101272,#101273),.UNSPECIFIED.,.F.,.F.,(4,3,3,3,3,3,3,3,3,3,3,3,3,3,3,3,
3,3,3,3,3,3,3,4),(47.1238898038468,47.2754958858741,47.3172203381978,47.4214065016859,
47.5254374268981,47.629346317315,47.7331897484832,47.8370024994981,47.9408193060197,
48.0447447833901,48.1487291019349,48.2528953593942,48.3147681965438,48.4189543600319,
48.5229852852439,48.6268941756608,48.7307376068288,48.8345503578437,48.9383671643651,
49.0422926417354,49.14627696028,49.2504432177392,49.3123160548899,49.3501218890484),
 .UNSPECIFIED.);
#2728=B_SPLINE_CURVE_WITH_KNOTS('',3,(#101274,#101275,#101276,#101277,#101278,
#101279,#101280,#101281,#101282,#101283,#101284,#101285,#101286,#101287,
#101288,#101289,#101290,#101291,#101292,#101293,#101294,#101295,#101296,
#101297,#101298,#101299,#101300,#101301,#101302,#101303,#101304,#101305,
#101306,#101307,#101308,#101309,#101310,#101311,#101312,#101313,#101314,
#101315,#101316,#101317,#101318,#101319,#101320,#101321,#101322,#101323,
#101324,#101325,#101326,#101327,#101328,#101329,#101330,#101331,#101332,
#101333,#101334,#101335,#101336,#101337,#101338,#101339,#101340,#101341,
#101342,#101343,#101344,#101345,#101346,#101347,#101348,#101349,#101350,
#101351,#101352,#101353,#101354,#101355,#101356,#101357,#101358,#101359,
#101360,#101361,#101362,#101363,#101364,#101365,#101366,#101367,#101368,
#101369,#101370,#101371,#101372,#101373,#101374,#101375,#101376,#101377,
#101378,#101379,#101380,#101381,#101382,#101383,#101384,#101385,#101386,
#101387,#101388,#101389,#101390,#101391,#101392,#101393,#101394,#101395,
#101396,#101397),.UNSPECIFIED.,.F.,.F.,(4,3,3,3,3,3,3,3,3,3,3,3,3,3,3,3,
3,3,3,3,3,3,3,3,3,3,3,3,3,3,3,3,3,3,3,3,3,3,3,3,3,4),(43.0661596755458,
43.1701506718428,43.2743208164948,43.3270289048134,43.4312150683038,43.5352459935183,
43.6391548839376,43.7429983151081,43.8468110661254,43.9506278726493,44.0545533500222,
44.1585376685693,44.262703926031,44.3245767631595,44.4287629266472,44.5327938518589,
44.6367027422754,44.740546173443,44.8443589244575,44.9481757309785,45.0521012083484,
45.1560855268927,45.2602517843515,45.3221246215056,45.4263107849935,45.5303417102053,
45.6342506006219,45.7380940317896,45.8419067828042,45.9457235893253,46.0496490666953,
46.1536333852397,46.2577996426985,46.3196724798517,46.4223012412911,46.5247935864412,
46.6271863644381,46.7295162801918,46.8318649061915,46.9342176129136,47.0366904241956,
47.1238898034296),.UNSPECIFIED.);
#2729=B_SPLINE_CURVE_WITH_KNOTS('',3,(#101403,#101404,#101405,#101406,#101407,
#101408,#101409,#101410,#101411,#101412,#101413,#101414,#101415,#101416,
#101417,#101418,#101419,#101420,#101421,#101422,#101423,#101424,#101425,
#101426,#101427,#101428,#101429,#101430,#101431,#101432,#101433,#101434,
#101435,#101436,#101437,#101438,#101439,#101440,#101441,#101442,#101443,
#101444,#101445,#101446,#101447,#101448,#101449,#101450,#101451,#101452,
#101453,#101454,#101455,#101456,#101457,#101458,#101459,#101460,#101461,
#101462,#101463,#101464,#101465,#101466,#101467,#101468,#101469,#101470,
#101471,#101472,#101473,#101474,#101475,#101476,#101477,#101478,#101479,
#101480,#101481,#101482,#101483,#101484,#101485,#101486,#101487,#101488,
#101489,#101490,#101491,#101492,#101493,#101494,#101495,#101496,#101497,
#101498,#101499,#101500,#101501,#101502,#101503,#101504,#101505,#101506,
#101507,#101508,#101509,#101510,#101511,#101512,#101513,#101514,#101515,
#101516,#101517,#101518,#101519,#101520,#101521,#101522,#101523,#101524,
#101525,#101526,#101527,#101528,#101529),.UNSPECIFIED.,.F.,.F.,(4,3,3,3,
3,3,3,3,3,3,3,3,3,3,3,3,3,3,3,3,3,3,3,3,3,3,3,3,3,3,3,3,3,3,3,3,3,3,3,3,
3,3,4),(36.7834442042422,36.8002764629088,36.904462626368,37.0084935515507,
37.1124024419373,37.2162458730747,37.3200586240585,37.4238754305485,37.5278009078871,
37.6317852263998,37.735951483827,37.7978243212549,37.9020104847617,38.0060414099928,
38.1099503004289,38.2137937316164,38.317606482651,38.4214232891922,38.5253487665823,
38.6293330851469,38.7334993426258,38.795372179601,38.8995583430862,39.0035892682954,
39.1074981587095,39.2113415898747,39.3151543408867,39.4189711474052,39.5228966247728,
39.6268809433147,39.7310472007711,39.7929200379471,39.8971062014322,40.0011371266412,
40.1050460170549,40.2088894482198,40.3127021992315,40.4165190057495,40.5204444831166,
40.624428801658,40.7285950591138,40.7904678962932,40.8407044966673),
 .UNSPECIFIED.);
#2730=B_SPLINE_CURVE_WITH_KNOTS('',3,(#101530,#101531,#101532,#101533,#101534,
#101535,#101536,#101537,#101538,#101539,#101540,#101541,#101542,#101543,
#101544,#101545,#101546,#101547,#101548,#101549,#101550,#101551,#101552,
#101553,#101554,#101555,#101556,#101557,#101558,#101559,#101560,#101561,
#101562,#101563,#101564,#101565,#101566,#101567,#101568,#101569,#101570,
#101571,#101572,#101573,#101574,#101575,#101576,#101577,#101578,#101579,
#101580,#101581,#101582,#101583,#101584,#101585,#101586,#101587,#101588,
#101589,#101590,#101591,#101592,#101593,#101594,#101595,#101596,#101597,
#101598,#101599),.UNSPECIFIED.,.F.,.F.,(4,3,3,3,3,3,3,3,3,3,3,3,3,3,3,3,
3,3,3,3,3,3,3,4),(40.8407044970018,40.9440746115614,41.0495672544461,41.1526720053859,
41.2557188072278,41.3587435025102,41.4660615655424,41.5692147500828,41.6724388016563,
41.7758284060282,41.7880157546392,41.8922019181269,41.9962328433386,42.1001417337551,
42.2039851649228,42.3077979159374,42.4116147224584,42.5155401998284,42.6195245183727,
42.7236907758316,42.7855636129853,42.8897412732137,42.9937540523187,43.0672730856169),
 .UNSPECIFIED.);
#2731=B_SPLINE_CURVE_WITH_KNOTS('',3,(#101601,#101602,#101603,#101604,#101605,
#101606,#101607,#101608,#101609,#101610,#101611,#101612,#101613,#101614,
#101615,#101616,#101617,#101618,#101619,#101620,#101621,#101622,#101623,
#101624,#101625,#101626,#101627,#101628,#101629,#101630,#101631,#101632,
#101633,#101634,#101635,#101636,#101637,#101638,#101639,#101640,#101641,
#101642,#101643,#101644,#101645,#101646,#101647,#101648,#101649,#101650,
#101651,#101652,#101653,#101654,#101655,#101656,#101657,#101658,#101659,
#101660,#101661,#101662,#101663,#101664,#101665,#101666,#101667),
 .UNSPECIFIED.,.F.,.F.,(4,3,3,3,3,3,3,3,3,3,3,3,3,3,3,3,3,3,3,3,3,3,4),
(40.8407044969849,40.9497796083558,41.0591756422725,41.1687426604111,41.2786112447405,
41.3319331881212,41.4361193516065,41.5401502768156,41.6440591672296,41.7479025983948,
41.8517153494068,41.9555321559254,42.059457633293,42.1634419518349,42.2676082092914,
42.3294810464673,42.4336404893567,42.5376570390707,42.6415657001877,42.7477141940272,
42.8515321201983,42.9588458978721,43.0661596755458),.UNSPECIFIED.);
#2732=B_SPLINE_CURVE_WITH_KNOTS('',3,(#101668,#101669,#101670,#101671,#101672,
#101673,#101674,#101675,#101676,#101677,#101678,#101679,#101680,#101681,
#101682,#101683,#101684,#101685,#101686,#101687,#101688,#101689,#101690,
#101691,#101692,#101693,#101694,#101695,#101696,#101697,#101698,#101699,
#101700,#101701,#101702,#101703,#101704,#101705,#101706,#101707,#101708,
#101709,#101710,#101711,#101712,#101713,#101714,#101715,#101716,#101717,
#101718,#101719,#101720,#101721,#101722,#101723,#101724,#101725,#101726,
#101727,#101728,#101729,#101730,#101731,#101732,#101733,#101734,#101735,
#101736,#101737,#101738,#101739,#101740,#101741,#101742,#101743,#101744,
#101745,#101746,#101747,#101748,#101749,#101750,#101751,#101752,#101753,
#101754,#101755,#101756,#101757,#101758,#101759,#101760,#101761,#101762,
#101763,#101764,#101765,#101766,#101767,#101768,#101769,#101770,#101771,
#101772,#101773,#101774,#101775,#101776,#101777,#101778,#101779,#101780,
#101781,#101782,#101783,#101784,#101785,#101786,#101787,#101788,#101789,
#101790,#101791),.UNSPECIFIED.,.F.,.F.,(4,3,3,3,3,3,3,3,3,3,3,3,3,3,3,3,
3,3,3,3,3,3,3,3,3,3,3,3,3,3,3,3,3,3,3,3,3,3,3,3,3,4),(36.7837239633391,
36.8875345883055,36.9913571492279,37.0952932330975,37.1992952394363,37.3034721119993,
37.3417417547369,37.4459279183704,37.5499588437299,37.6538677342964,37.7577111656155,
37.8615239167826,37.9653407234571,38.0692662009808,38.1732505196793,38.2774167772912,
38.339289613083,38.4434757765587,38.5475067017587,38.6514155921638,38.7552590233201,
38.8590717743235,38.9628885808337,39.0668140581934,39.1707983767275,39.2749646341767,
39.3368374714291,39.4410236348886,39.5450545600716,39.6489634504586,39.7528068815964,
39.8566196325803,39.960436439071,40.0643619164099,40.1683462349231,40.2725124923507,
40.3343853297751,40.4435562694802,40.5524208008269,40.6611016632894,40.7695577702461,
40.8407044966673),.UNSPECIFIED.);
#2733=B_SPLINE_CURVE_WITH_KNOTS('',3,(#101797,#101798,#101799,#101800,#101801,
#101802,#101803,#101804,#101805,#101806,#101807,#101808,#101809,#101810,
#101811,#101812,#101813,#101814,#101815,#101816,#101817,#101818,#101819,
#101820,#101821,#101822,#101823,#101824,#101825,#101826,#101827,#101828,
#101829,#101830,#101831,#101832,#101833,#101834,#101835,#101836,#101837,
#101838,#101839,#101840,#101841,#101842,#101843,#101844,#101845,#101846,
#101847,#101848,#101849,#101850,#101851,#101852,#101853,#101854,#101855,
#101856,#101857,#101858,#101859,#101860,#101861,#101862,#101863,#101864,
#101865,#101866,#101867,#101868,#101869,#101870,#101871,#101872,#101873,
#101874,#101875,#101876,#101877,#101878,#101879,#101880,#101881,#101882,
#101883,#101884,#101885,#101886,#101887,#101888,#101889,#101890,#101891,
#101892,#101893,#101894,#101895,#101896,#101897,#101898,#101899,#101900,
#101901,#101902,#101903,#101904,#101905,#101906,#101907,#101908,#101909,
#101910,#101911,#101912,#101913,#101914,#101915,#101916,#101917,#101918,
#101919,#101920),.UNSPECIFIED.,.F.,.F.,(4,3,3,3,3,3,3,3,3,3,3,3,3,3,3,3,
3,3,3,3,3,3,3,3,3,3,3,3,3,3,3,3,3,3,3,3,3,3,3,3,3,4),(30.4998665211569,
30.6038214745698,30.7094053937011,30.8149893128323,30.9191754738923,31.0232063966314,
31.1271152845205,31.2309587131284,31.3347714615544,31.4385882654618,31.5425137401983,
31.6464980560938,31.7506643109082,31.8125371711784,31.916723335786,32.0207542621321,
32.1246631536991,32.2285065860268,32.3323193382088,32.4361361459029,32.5400616244471,
32.6440459441679,32.7482122027941,32.8100850295245,32.9142711930052,33.0183021182129,
33.1222110086303,33.2260544398016,33.3298671908228,33.4336839973533,33.5376094747372,
33.641593793298,33.7457600507772,33.8076328878705,33.9105733956088,34.0133739392451,
34.1160710646413,34.2187011756074,34.3213305266006,34.4239607110272,34.5266703118465,
34.5575191894877),.UNSPECIFIED.);
#2734=B_SPLINE_CURVE_WITH_KNOTS('',3,(#101921,#101922,#101923,#101924,#101925,
#101926,#101927,#101928,#101929,#101930,#101931,#101932,#101933,#101934,
#101935,#101936,#101937,#101938,#101939,#101940,#101941,#101942,#101943,
#101944,#101945,#101946,#101947,#101948,#101949,#101950,#101951,#101952,
#101953,#101954,#101955,#101956,#101957,#101958,#101959,#101960,#101961,
#101962,#101963,#101964,#101965,#101966,#101967,#101968,#101969,#101970,
#101971,#101972,#101973,#101974,#101975,#101976,#101977,#101978,#101979,
#101980,#101981,#101982,#101983,#101984,#101985,#101986,#101987),
 .UNSPECIFIED.,.F.,.F.,(4,3,3,3,3,3,3,3,3,3,3,3,3,3,3,3,3,3,3,3,3,3,4),
(34.5575191897883,34.6927956482503,34.8051807462166,34.9093669098508,35.0133978352109,
35.1173067257782,35.221150157098,35.3249629082657,35.4287797149408,35.5327051924652,
35.6366895111642,35.7408557687768,35.8027286045627,35.9069159432592,36.0109477009195,
36.1148561160984,36.2186985866371,36.3225098919277,36.4263247672698,36.5302426811341,
36.6342192371332,36.7383648916943,36.7834442042422),.UNSPECIFIED.);
#2735=B_SPLINE_CURVE_WITH_KNOTS('',3,(#101989,#101990,#101991,#101992,#101993,
#101994,#101995,#101996,#101997,#101998,#101999,#102000,#102001,#102002,
#102003,#102004,#102005,#102006,#102007,#102008,#102009,#102010,#102011,
#102012,#102013,#102014,#102015,#102016,#102017,#102018,#102019,#102020,
#102021,#102022,#102023,#102024,#102025,#102026,#102027,#102028,#102029,
#102030,#102031,#102032,#102033,#102034,#102035,#102036,#102037,#102038,
#102039,#102040,#102041,#102042,#102043,#102044,#102045,#102046,#102047,
#102048,#102049,#102050,#102051,#102052,#102053,#102054,#102055,#102056,
#102057,#102058),.UNSPECIFIED.,.F.,.F.,(4,3,3,3,3,3,3,3,3,3,3,3,3,3,3,3,
3,3,3,3,3,3,3,4),(34.557519189755,34.6600261052919,34.7624492426958,34.8648252095896,
34.9671905447845,35.0696506740705,35.1721598073025,35.274848931505,35.3466460380447,
35.4508322015257,35.5548631267338,35.6587720171514,35.7626154483231,35.8664281993446,
35.9702450058755,36.0741704832597,36.1781548018206,36.2823210593,36.3441938963908,
36.44838866619,36.5524031618947,36.6563141161565,36.7601506302188,36.7837239633391),
 .UNSPECIFIED.);
#2736=B_SPLINE_CURVE_WITH_KNOTS('',3,(#102059,#102060,#102061,#102062,#102063,
#102064,#102065,#102066,#102067,#102068,#102069,#102070,#102071,#102072,
#102073,#102074,#102075,#102076,#102077,#102078,#102079,#102080,#102081,
#102082,#102083,#102084,#102085,#102086,#102087,#102088,#102089,#102090,
#102091,#102092,#102093,#102094,#102095,#102096,#102097,#102098,#102099,
#102100,#102101,#102102,#102103,#102104,#102105,#102106,#102107,#102108,
#102109,#102110,#102111,#102112,#102113,#102114,#102115,#102116,#102117,
#102118,#102119,#102120,#102121,#102122,#102123,#102124,#102125,#102126,
#102127,#102128,#102129,#102130,#102131,#102132,#102133,#102134,#102135,
#102136,#102137,#102138,#102139,#102140,#102141,#102142,#102143,#102144,
#102145,#102146,#102147,#102148,#102149,#102150,#102151,#102152,#102153,
#102154,#102155,#102156,#102157,#102158,#102159,#102160,#102161,#102162,
#102163,#102164,#102165,#102166,#102167,#102168,#102169,#102170,#102171,
#102172,#102173,#102174,#102175,#102176,#102177,#102178,#102179,#102180,
#102181,#102182),.UNSPECIFIED.,.F.,.F.,(4,3,3,3,3,3,3,3,3,3,3,3,3,3,3,3,
3,3,3,3,3,3,3,3,3,3,3,3,3,3,3,3,3,3,3,3,3,3,3,3,3,4),(30.5008971260263,
30.6078418108556,30.7117208864184,30.8155481351692,30.9193583150517,31.0286323874539,
31.1325801077697,31.2366005323038,31.3407893994026,31.3564546046604,31.4606407764442,
31.5646717100508,31.6685806089678,31.7724240486963,31.8762368083192,31.9800536234836,
32.0839791094901,32.1879634366803,32.2921297027055,32.3540024630065,32.4581886272383,
32.5622195532328,32.6661284444861,32.7699718765233,32.8737846284391,32.977601435892,
33.0815269142341,33.1855112337748,33.2896774922579,33.3515503213525,33.45573648242,
33.5597674051667,33.6636762930636,33.7675197216792,33.8713324701132,33.9751492740289,
34.0790747487735,34.1830590646772,34.2872253194997,34.3490981796986,34.4951131604689,
34.5575191894876),.UNSPECIFIED.);
#2737=B_SPLINE_CURVE_WITH_KNOTS('',3,(#102188,#102189,#102190,#102191,#102192,
#102193,#102194,#102195,#102196,#102197,#102198,#102199,#102200,#102201,
#102202,#102203,#102204,#102205,#102206,#102207,#102208,#102209,#102210,
#102211,#102212,#102213,#102214,#102215,#102216,#102217,#102218,#102219,
#102220,#102221,#102222,#102223,#102224,#102225,#102226,#102227,#102228,
#102229,#102230,#102231,#102232,#102233,#102234,#102235,#102236,#102237,
#102238,#102239,#102240,#102241,#102242,#102243,#102244,#102245,#102246,
#102247,#102248,#102249,#102250,#102251,#102252,#102253,#102254,#102255,
#102256,#102257,#102258,#102259,#102260,#102261,#102262,#102263,#102264,
#102265,#102266,#102267,#102268,#102269,#102270,#102271,#102272,#102273,
#102274,#102275,#102276,#102277,#102278,#102279,#102280,#102281,#102282,
#102283,#102284,#102285,#102286,#102287,#102288,#102289,#102290,#102291,
#102292,#102293,#102294,#102295,#102296,#102297,#102298,#102299,#102300,
#102301,#102302,#102303,#102304,#102305,#102306,#102307,#102308),
 .UNSPECIFIED.,.F.,.F.,(4,3,3,3,3,3,3,3,3,3,3,3,3,3,3,3,3,3,3,3,3,3,3,3,
3,3,3,3,3,3,3,3,3,3,3,3,3,3,3,3,4),(24.2175053922168,24.3213237512326,24.4251359274773,
24.529050198678,24.6330141142592,24.7371697158236,24.8297021627558,24.9338881433276,
25.0379188825363,25.1418275832654,25.2456708225743,25.3494833798447,25.4532999910205,
25.5572252719414,25.6612093931172,25.7653754538915,25.8272500211019,25.9314362441109,
26.0354672294637,26.1393761806463,26.2432196729321,26.3470324853247,26.4508493533922,
26.5547748921389,26.6587592720567,26.762925590215,26.8247978794479,26.9289840556603,
27.0330149940174,27.1369238981433,27.2407673433612,27.3445801087465,27.4483969299387,
27.5523224223397,27.6563067561414,27.7604730290516,27.822345737794,27.9353427738055,
28.0470528540771,28.1606933679585,28.27433388184),.UNSPECIFIED.);
#2738=B_SPLINE_CURVE_WITH_KNOTS('',3,(#102309,#102310,#102311,#102312,#102313,
#102314,#102315,#102316,#102317,#102318,#102319,#102320,#102321,#102322,
#102323,#102324,#102325,#102326,#102327,#102328,#102329,#102330,#102331,
#102332,#102333,#102334,#102335,#102336,#102337,#102338,#102339,#102340,
#102341,#102342,#102343,#102344,#102345,#102346,#102347,#102348,#102349,
#102350,#102351,#102352,#102353,#102354,#102355,#102356,#102357,#102358,
#102359,#102360,#102361,#102362,#102363,#102364,#102365,#102366,#102367,
#102368,#102369,#102370,#102371,#102372,#102373,#102374,#102375),
 .UNSPECIFIED.,.F.,.F.,(4,3,3,3,3,3,3,3,3,3,3,3,3,3,3,3,3,3,3,3,3,3,4),
(28.2743338823081,28.3811858746811,28.4908628050458,28.598029113806,28.7089613549731,
28.8198935961401,28.9240797679517,29.0281107015868,29.1320196005323,29.2358630402896,
29.3396757999416,29.4434926151352,29.5474181011709,29.6514024283902,29.7555686944444,
29.8174414544862,29.9216058860566,30.0256258453343,30.1295363446499,30.2333833809737,
30.3371921312327,30.4410324079623,30.4998665211569),.UNSPECIFIED.);
#2739=B_SPLINE_CURVE_WITH_KNOTS('',3,(#102377,#102378,#102379,#102380,#102381,
#102382,#102383,#102384,#102385,#102386,#102387,#102388,#102389,#102390,
#102391,#102392,#102393,#102394,#102395,#102396,#102397,#102398,#102399,
#102400,#102401,#102402,#102403,#102404,#102405,#102406,#102407,#102408,
#102409,#102410,#102411,#102412,#102413,#102414,#102415,#102416,#102417,
#102418,#102419,#102420,#102421,#102422,#102423,#102424,#102425,#102426,
#102427,#102428,#102429,#102430,#102431,#102432,#102433,#102434,#102435,
#102436,#102437,#102438,#102439,#102440,#102441,#102442,#102443,#102444,
#102445,#102446),.UNSPECIFIED.,.F.,.F.,(4,3,3,3,3,3,3,3,3,3,3,3,3,3,3,3,
3,3,3,3,3,3,3,4),(28.2743338823081,28.3638110296221,28.4679972524518,28.5720282376233,
28.6759371886222,28.779780680723,28.8835934929296,28.9874103608106,29.0913358993708,
29.1953202791018,29.2994865970749,29.3613588879682,29.4655450641685,29.569576002513,
29.6734849066249,29.7773283518282,29.8811411171982,29.9849579383745,30.0888834307589,
30.1928677645433,30.2970340374357,30.3589067463143,30.4630838225724,30.5008971260263),
 .UNSPECIFIED.);
#2740=B_SPLINE_CURVE_WITH_KNOTS('',3,(#102447,#102448,#102449,#102450,#102451,
#102452,#102453,#102454,#102455,#102456,#102457,#102458,#102459,#102460,
#102461,#102462,#102463,#102464,#102465,#102466,#102467,#102468,#102469,
#102470,#102471,#102472,#102473,#102474,#102475,#102476,#102477,#102478,
#102479,#102480,#102481,#102482,#102483,#102484,#102485,#102486,#102487,
#102488,#102489,#102490,#102491,#102492,#102493,#102494,#102495,#102496,
#102497,#102498,#102499,#102500,#102501,#102502,#102503,#102504,#102505,
#102506,#102507,#102508,#102509,#102510,#102511,#102512,#102513,#102514,
#102515,#102516,#102517,#102518,#102519,#102520,#102521,#102522,#102523,
#102524,#102525,#102526,#102527,#102528,#102529,#102530,#102531,#102532,
#102533,#102534,#102535,#102536,#102537,#102538,#102539,#102540,#102541,
#102542,#102543,#102544,#102545,#102546,#102547,#102548,#102549,#102550,
#102551,#102552,#102553,#102554,#102555,#102556,#102557,#102558,#102559,
#102560,#102561,#102562,#102563,#102564,#102565,#102566,#102567,#102568,
#102569,#102570),.UNSPECIFIED.,.F.,.F.,(4,3,3,3,3,3,3,3,3,3,3,3,3,3,3,3,
3,3,3,3,3,3,3,3,3,3,3,3,3,3,3,3,3,3,3,3,3,3,3,3,3,4),(24.2166116664802,
24.3207836892698,24.3736195962378,24.4778042292082,24.5818335992139,24.6857409053055,
24.7895827350337,24.8933938698845,24.9972090478915,25.1011328890806,25.2051155646482,
25.3092801861933,25.3711674545838,25.4753540205954,25.5793853516668,25.6832946508906,
25.787138492457,25.8909516548417,25.994768873086,26.0986947598526,26.2026794870977,
26.3068461476929,26.3687153129299,26.4729016339696,26.5769327209669,26.6808417786907,
26.7846853804865,26.8884983051989,26.9923152882402,27.0962409452456,27.2002254454547,
27.3043918858362,27.366263171276,27.4692311759306,27.5720240165358,27.6747190063384,
27.7773525424952,27.8799609377777,27.9826451376514,28.0853653036078,28.1882551874075,
28.2743338818562),.UNSPECIFIED.);
#2741=B_SPLINE_CURVE_WITH_KNOTS('',3,(#102576,#102577,#102578,#102579,#102580,
#102581,#102582,#102583,#102584,#102585,#102586,#102587,#102588,#102589,
#102590,#102591,#102592,#102593,#102594,#102595,#102596,#102597,#102598,
#102599,#102600,#102601,#102602,#102603,#102604,#102605,#102606,#102607,
#102608,#102609,#102610,#102611,#102612,#102613,#102614,#102615,#102616,
#102617,#102618,#102619,#102620,#102621,#102622,#102623,#102624,#102625,
#102626,#102627,#102628,#102629,#102630,#102631,#102632,#102633,#102634,
#102635,#102636,#102637,#102638,#102639,#102640,#102641,#102642,#102643,
#102644,#102645),.UNSPECIFIED.,.F.,.F.,(4,3,3,3,3,3,3,3,3,3,3,3,3,3,3,3,
3,3,3,3,3,3,3,4),(15.7079632679489,15.8107626988751,15.9135276397438,16.0162941010105,
16.1191710909696,16.2221067685037,16.3252328024632,16.3932367294691,16.4974783152938,
16.601563455709,16.7055244767834,16.8094187179986,16.9132808760585,17.0171456028236,
17.1211163738189,17.2251445703169,17.3293519684345,17.3907845878152,17.4951305459153,
17.6047988992279,17.7088743073029,17.8128825648351,17.9168653335439,17.9338039591658),
 .UNSPECIFIED.);
#2742=B_SPLINE_CURVE_WITH_KNOTS('',3,(#102647,#102648,#102649,#102650,#102651),
 .UNSPECIFIED.,.F.,.F.,(4,1,4),(14.3981410127769,15.395688871123,15.7079548498383),
 .UNSPECIFIED.);
#2743=B_SPLINE_CURVE_WITH_KNOTS('',3,(#102655,#102656,#102657,#102658,#102659,
#102660,#102661,#102662,#102663,#102664,#102665,#102666,#102667,#102668,
#102669,#102670,#102671,#102672,#102673,#102674,#102675,#102676,#102677,
#102678,#102679,#102680,#102681,#102682,#102683,#102684,#102685,#102686,
#102687,#102688,#102689,#102690,#102691,#102692,#102693,#102694,#102695,
#102696,#102697,#102698,#102699,#102700,#102701,#102702,#102703,#102704,
#102705,#102706,#102707,#102708,#102709,#102710,#102711,#102712),
 .UNSPECIFIED.,.F.,.F.,(4,3,3,3,3,3,3,3,3,3,3,3,3,3,3,3,3,3,3,4),(13.8761929392676,
13.9800701520378,14.0837916127864,14.1873908176266,14.2909249700636,14.3944292944766,
14.4979389721904,14.6015555958747,14.7052331471479,14.8090843148421,14.8542235792949,
14.9609410403269,15.0635682984263,15.1661015198455,15.2685772615991,15.3710319982226,
15.473553730983,15.5761160209808,15.6788141300276,15.7079632675506),
 .UNSPECIFIED.);
#2744=B_SPLINE_CURVE_WITH_KNOTS('',3,(#102713,#102714,#102715,#102716,#102717,
#102718,#102719,#102720,#102721,#102722,#102723,#102724,#102725,#102726,
#102727,#102728,#102729,#102730,#102731,#102732,#102733,#102734,#102735,
#102736,#102737,#102738,#102739,#102740,#102741,#102742,#102743,#102744,
#102745,#102746,#102747,#102748,#102749,#102750,#102751,#102752,#102753,
#102754,#102755,#102756,#102757,#102758,#102759,#102760,#102761,#102762,
#102763,#102764,#102765,#102766,#102767,#102768,#102769,#102770,#102771,
#102772,#102773,#102774,#102775,#102776,#102777,#102778,#102779),
 .UNSPECIFIED.,.F.,.F.,(4,3,3,3,3,3,3,3,3,3,3,3,3,3,3,3,3,3,3,3,3,3,4),
(15.7079632679489,15.851771437641,15.9558570600629,16.0597859912443,16.1635912207135,
16.2673300163232,16.3710373111926,16.4747479940652,16.578567054987,16.6824446290273,
16.7865047811698,16.8493192959871,16.9535191031687,17.0575636422614,17.1614860332293,
17.2653428871325,17.3691689624188,17.4729989740083,17.5769373807894,17.6809344925897,
17.7851131867065,17.8468671543332,17.9343865285971),.UNSPECIFIED.);
#2745=B_SPLINE_CURVE_WITH_KNOTS('',3,(#102785,#102786,#102787,#102788,#102789,
#102790,#102791,#102792,#102793,#102794,#102795,#102796,#102797,#102798,
#102799,#102800,#102801,#102802,#102803,#102804,#102805,#102806,#102807,
#102808,#102809,#102810,#102811,#102812,#102813,#102814,#102815,#102816,
#102817,#102818,#102819,#102820,#102821,#102822,#102823,#102824,#102825,
#102826,#102827,#102828,#102829,#102830,#102831,#102832,#102833,#102834,
#102835,#102836,#102837,#102838,#102839,#102840,#102841,#102842,#102843,
#102844,#102845,#102846,#102847,#102848),.UNSPECIFIED.,.F.,.F.,(4,3,3,3,
3,3,3,3,3,3,3,3,3,3,3,3,3,3,3,3,3,4),(89.6265204900684,89.7423240812235,
89.7793072511478,89.8880546694006,89.9991547244123,90.1076029303331,90.2159879164032,
90.324351856268,90.4374776695745,90.5460056337737,90.6546213577008,90.7634384533039,
90.7768551094939,90.8896161868303,91.0021364331478,91.1145147206211,91.2267846088042,
91.3389795079967,91.4511679814058,91.5633431986276,91.675606607642,91.7744029678399),
 .UNSPECIFIED.);
#2746=B_SPLINE_CURVE_WITH_KNOTS('',3,(#102851,#102852,#102853,#102854,#102855,
#102856,#102857,#102858,#102859,#102860,#102861,#102862,#102863,#102864,
#102865,#102866,#102867,#102868,#102869,#102870,#102871,#102872,#102873,
#102874,#102875,#102876,#102877,#102878,#102879,#102880,#102881,#102882,
#102883,#102884,#102885,#102886,#102887,#102888,#102889,#102890,#102891,
#102892,#102893,#102894,#102895,#102896,#102897,#102898,#102899,#102900,
#102901,#102902,#102903,#102904,#102905,#102906,#102907,#102908,#102909,
#102910,#102911,#102912,#102913,#102914,#102915,#102916,#102917,#102918,
#102919,#102920,#102921,#102922,#102923,#102924,#102925,#102926,#102927,
#102928,#102929,#102930,#102931,#102932,#102933,#102934,#102935,#102936,
#102937,#102938,#102939,#102940,#102941,#102942,#102943,#102944,#102945,
#102946,#102947,#102948,#102949,#102950,#102951,#102952,#102953,#102954,
#102955,#102956,#102957,#102958,#102959,#102960,#102961,#102962,#102963,
#102964,#102965,#102966,#102967,#102968,#102969,#102970),.UNSPECIFIED.,
 .F.,.F.,(4,2,2,2,2,2,2,2,2,2,2,2,2,2,2,2,2,2,2,2,2,2,2,2,2,2,2,2,2,2,2,
2,2,2,2,2,2,2,2,2,2,2,2,2,2,2,2,2,2,2,2,2,2,2,2,2,2,2,2,4),(-1.75478141683255,
-1.75474714622055,-1.75154566303739,-1.71244934856324,-1.69483238573248,
-1.68695596995421,-1.68054846350455,-1.67685394387567,-1.67359857524207,
-1.66949553212815,-1.66293957404403,-1.62998536351094,-1.60154438751122,
-1.59714207279607,-1.59489598236586,-1.59305759514252,-1.59070389455029,
-1.58582216073164,-1.56157050494364,-1.53947860741533,-1.5267269204622,
-1.51753715024743,-1.51332270787878,-1.51007730786042,-1.50649576904019,
-1.50053816651313,-1.47409251915458,-1.44517675981777,-1.4368177153129,
-1.43108068460839,-1.42861752332292,-1.42679807750872,-1.42471145136723,
-1.42100639265604,-1.39657501271319,-1.36801382302935,-1.352634645584,-1.34759671952704,
-1.34423546772831,-1.34098617056533,-1.33635431768738,-1.32511563116455,
-1.28876527539643,-1.27368221212848,-1.26508274154723,-1.26223065867346,
-1.26035249587754,-1.25841798138827,-1.25534160276798,-1.24569846165095,
-1.21643969142406,-1.19706671198549,-1.18479961744929,-1.18011648208558,
-1.1768052418789,-1.17380872819427,-1.16903000431917,-1.15701838544427,
-1.11837736041743,-1.10915475680411),.UNSPECIFIED.);
#2747=B_SPLINE_CURVE_WITH_KNOTS('',3,(#102976,#102977,#102978,#102979,#102980,
#102981,#102982,#102983,#102984,#102985,#102986,#102987,#102988,#102989,
#102990,#102991,#102992,#102993,#102994,#102995,#102996,#102997,#102998,
#102999,#103000,#103001,#103002,#103003,#103004,#103005,#103006,#103007,
#103008,#103009,#103010,#103011,#103012,#103013,#103014,#103015,#103016,
#103017,#103018,#103019,#103020,#103021,#103022,#103023,#103024,#103025,
#103026,#103027,#103028,#103029,#103030,#103031,#103032,#103033,#103034,
#103035,#103036,#103037,#103038,#103039,#103040,#103041,#103042,#103043,
#103044,#103045,#103046,#103047,#103048,#103049,#103050,#103051,#103052,
#103053,#103054,#103055,#103056,#103057,#103058,#103059,#103060,#103061,
#103062,#103063,#103064,#103065,#103066,#103067,#103068,#103069,#103070,
#103071,#103072,#103073,#103074,#103075,#103076,#103077,#103078,#103079,
#103080,#103081,#103082,#103083,#103084,#103085,#103086,#103087,#103088,
#103089,#103090,#103091,#103092,#103093,#103094,#103095,#103096,#103097,
#103098,#103099,#103100,#103101,#103102,#103103,#103104,#103105,#103106,
#103107,#103108,#103109,#103110,#103111,#103112,#103113,#103114,#103115,
#103116,#103117,#103118,#103119,#103120,#103121,#103122,#103123,#103124,
#103125,#103126,#103127,#103128,#103129,#103130,#103131,#103132,#103133,
#103134,#103135,#103136,#103137,#103138,#103139,#103140,#103141,#103142,
#103143,#103144,#103145,#103146,#103147,#103148,#103149,#103150,#103151,
#103152,#103153,#103154,#103155,#103156,#103157,#103158,#103159,#103160,
#103161,#103162,#103163,#103164,#103165,#103166,#103167,#103168,#103169,
#103170,#103171),.UNSPECIFIED.,.F.,.F.,(4,2,2,2,2,2,2,2,2,2,2,2,2,2,2,2,
2,2,2,2,2,2,2,2,2,2,2,2,2,2,2,2,2,2,2,2,2,2,2,2,2,2,2,2,2,2,2,2,2,2,2,2,
2,2,2,2,2,2,2,2,2,2,2,2,2,2,2,2,2,2,2,2,2,2,2,2,2,2,2,2,2,2,2,2,2,2,2,2,
2,2,2,2,2,2,2,2,2,4),(-0.991222240709418,-0.988027886510137,-0.950886399888337,
-0.924345861055636,-0.91939272677848,-0.917071588897676,-0.915265403854227,
-0.913074670459631,-0.908788938176693,-0.903122234160721,-0.888766291940011,
-0.854914221798932,-0.841198188334745,-0.836187351597118,-0.833155052601022,
-0.829888975005128,-0.825426509686339,-0.81463091207118,-0.798615464231531,
-0.781977473278559,-0.777830949901933,-0.755715088919002,-0.752024837541532,
-0.749936119343352,-0.74811598639392,-0.745645412251508,-0.739842832637144,
-0.731343456422572,-0.701271273382964,-0.676328173391544,-0.670426337811458,
-0.666867761715694,-0.663636852275534,-0.659432704790222,-0.650233601775503,
-0.637457774523331,-0.61531379424856,-0.611209132472771,-0.589073143637183,
-0.585379077426616,-0.583287273735827,-0.581461429124973,-0.57897943684902,
-0.573136104128642,-0.564558346736028,-0.533822637681052,-0.509893132988251,
-0.50402697404592,-0.500472737586186,-0.497234545897751,-0.493004471675793,
-0.483676907308556,-0.43930484978909,-0.42235425926687,-0.418771555600446,
-0.416705924315107,-0.41488881339156,-0.412392684417977,-0.406370448494366,
-0.397410028659741,-0.363340767616483,-0.342468561364955,-0.336809871273662,
-0.333317967621712,-0.33009612876436,-0.325828838066538,-0.31616398715047,
-0.302460908956749,-0.281564485489673,-0.277755910692359,-0.255644113267809,
-0.251963257435088,-0.24988178959726,-0.248060682024771,-0.245587143236691,
-0.239789998047193,-0.231309788374238,-0.201479588045942,-0.176111312588489,
-0.170162170914639,-0.166582013185077,-0.163335511683964,-0.159116231810544,
-0.149901036997746,-0.137102693271951,-0.115168965334172,-0.111682021691364,
-0.0889718063890053,-0.0852573968865036,-0.0831502676931111,-0.0812886601938547,
-0.0787377028270211,-0.0726542678425233,-0.0363620134325881,-0.0113176275066724,
-0.00552567108098689,-0.00256674334763014,-0.000511608811820447),
 .UNSPECIFIED.);
#2748=B_SPLINE_CURVE_WITH_KNOTS('',3,(#103172,#103173,#103174,#103175,#103176,
#103177,#103178,#103179,#103180,#103181),.UNSPECIFIED.,.F.,.F.,(4,3,3,4),
(89.2744165561713,89.3894329271381,89.5079767086033,89.6265204900684),
 .UNSPECIFIED.);
#2749=B_SPLINE_CURVE_WITH_KNOTS('',3,(#103182,#103183,#103184,#103185,#103186,
#103187,#103188,#103189,#103190,#103191,#103192,#103193,#103194,#103195,
#103196,#103197,#103198,#103199,#103200,#103201,#103202,#103203,#103204,
#103205,#103206,#103207,#103208,#103209,#103210,#103211,#103212,#103213,
#103214,#103215,#103216,#103217,#103218,#103219,#103220,#103221,#103222,
#103223,#103224,#103225,#103226,#103227,#103228,#103229,#103230,#103231,
#103232,#103233,#103234,#103235,#103236,#103237,#103238,#103239,#103240,
#103241,#103242,#103243,#103244,#103245,#103246,#103247,#103248,#103249,
#103250,#103251,#103252,#103253,#103254,#103255,#103256,#103257,#103258,
#103259,#103260,#103261,#103262,#103263,#103264,#103265,#103266,#103267,
#103268,#103269,#103270,#103271,#103272,#103273,#103274,#103275,#103276,
#103277,#103278,#103279,#103280,#103281,#103282,#103283,#103284,#103285,
#103286,#103287,#103288,#103289,#103290,#103291,#103292,#103293,#103294,
#103295,#103296,#103297,#103298,#103299,#103300,#103301,#103302,#103303,
#103304,#103305,#103306,#103307,#103308,#103309,#103310,#103311,#103312,
#103313,#103314,#103315,#103316,#103317,#103318,#103319,#103320,#103321,
#103322,#103323,#103324,#103325,#103326,#103327,#103328,#103329,#103330,
#103331,#103332,#103333,#103334,#103335,#103336,#103337,#103338,#103339,
#103340,#103341,#103342,#103343,#103344,#103345,#103346,#103347,#103348,
#103349,#103350,#103351,#103352,#103353,#103354,#103355,#103356,#103357,
#103358,#103359,#103360,#103361,#103362,#103363,#103364,#103365,#103366,
#103367,#103368,#103369,#103370,#103371,#103372,#103373,#103374,#103375,
#103376,#103377,#103378,#103379,#103380,#103381,#103382,#103383,#103384,
#103385,#103386,#103387,#103388,#103389,#103390,#103391,#103392,#103393,
#103394,#103395,#103396,#103397,#103398,#103399),.UNSPECIFIED.,.F.,.F.,
(4,2,2,2,2,2,2,2,2,2,2,2,2,2,2,2,2,2,2,2,2,2,2,2,2,2,2,2,2,2,2,2,2,2,2,
2,2,2,2,2,2,2,2,2,2,2,2,2,2,2,2,2,2,2,2,2,2,2,2,2,2,2,2,2,2,2,2,2,2,2,2,
2,2,2,2,2,2,2,2,2,2,2,2,2,2,2,2,2,2,2,2,2,2,2,2,2,2,2,2,2,2,2,2,2,2,2,2,
2,4),(-1.10915475680411,-1.10590829758048,-1.09831161527419,-1.0955682913694,
-1.09369941402947,-1.09172085515654,-1.08844853815534,-1.07683204011244,
-1.04904897643187,-1.02093801199038,-1.01503665165844,-1.01147865015438,
-1.00824844491306,-1.00411566609876,-0.995066094606954,-0.952417953911051,
-0.939448552235861,-0.931650082640437,-0.928885238508515,-0.927016294348523,
-0.925051909309595,-0.921834195894843,-0.910795265200498,-0.878917578122148,
-0.854166835149102,-0.848276575307823,-0.844723781974713,-0.841497499285981,
-0.837298670188879,-0.828109782162662,-0.81535121284868,-0.79317009368756,
-0.789184196923743,-0.766857343376418,-0.763166659664749,-0.761078350117616,
-0.759258782181685,-0.756789566808509,-0.750993529741101,-0.742506521548799,
-0.712520275057755,-0.687505554106076,-0.681603733744546,-0.678046098167778,
-0.674816651296248,-0.670615317425667,-0.661426604830529,-0.648670055245723,
-0.626513207218797,-0.622406915862476,-0.600236593914423,-0.596544406651792,
-0.594454130792412,-0.592633539121673,-0.590162332514379,-0.584354649314002,
-0.575844183719526,-0.545670575765058,-0.520882316207129,-0.514988473781557,
-0.511433178795329,-0.50820432315119,-0.504001605406358,-0.494801135016941,
-0.482022284355135,-0.459859124408289,-0.455687901260009,-0.43359084300555,
-0.42989958696087,-0.427810164081731,-0.425990265862755,-0.423520359822213,
-0.417718389337441,-0.409218909876642,-0.379129533244734,-0.354240080201269,
-0.348343609205929,-0.34478809507672,-0.341559918258493,-0.337359357241499,
-0.328169097342547,-0.315409057612669,-0.293241579517659,-0.289168801363912,
-0.266951351589867,-0.263259953184448,-0.261170607434454,-0.259350666912133,
-0.256880707718876,-0.251079153859075,-0.242580682598317,-0.2124999395904,
-0.187582914355486,-0.181696072390992,-0.178142339924079,-0.174913216716446,
-0.170707721102072,-0.161490724083596,-0.148679746909174,-0.126536571672967,
-0.122249600366427,-0.100319329977102,-0.0966288118337607,-0.094539486612291,
-0.0927194160660713,-0.0902488910351242,-0.0844437354937957,-0.0759379299276961,
-0.0594803408397951),.UNSPECIFIED.);
#2750=B_SPLINE_CURVE_WITH_KNOTS('',3,(#103404,#103405,#103406,#103407,#103408,
#103409,#103410,#103411,#103412,#103413,#103414,#103415,#103416,#103417,
#103418,#103419,#103420,#103421,#103422,#103423,#103424,#103425,#103426,
#103427,#103428,#103429,#103430,#103431,#103432,#103433,#103434,#103435,
#103436,#103437,#103438,#103439,#103440,#103441,#103442,#103443,#103444,
#103445,#103446,#103447,#103448,#103449,#103450,#103451,#103452,#103453,
#103454,#103455,#103456,#103457,#103458,#103459,#103460,#103461,#103462,
#103463,#103464,#103465,#103466,#103467,#103468,#103469,#103470,#103471,
#103472,#103473,#103474,#103475,#103476,#103477,#103478,#103479,#103480,
#103481,#103482,#103483,#103484,#103485,#103486,#103487,#103488,#103489,
#103490,#103491,#103492,#103493,#103494,#103495,#103496,#103497,#103498,
#103499,#103500,#103501,#103502,#103503,#103504,#103505,#103506,#103507,
#103508,#103509,#103510,#103511,#103512,#103513,#103514,#103515,#103516,
#103517,#103518,#103519,#103520,#103521,#103522,#103523,#103524,#103525,
#103526,#103527,#103528,#103529,#103530,#103531,#103532,#103533,#103534,
#103535,#103536,#103537,#103538,#103539,#103540,#103541,#103542,#103543,
#103544,#103545,#103546,#103547,#103548,#103549,#103550,#103551,#103552,
#103553,#103554,#103555,#103556,#103557,#103558,#103559,#103560,#103561,
#103562,#103563,#103564,#103565,#103566,#103567,#103568,#103569,#103570,
#103571,#103572,#103573,#103574,#103575,#103576,#103577,#103578,#103579,
#103580,#103581,#103582,#103583,#103584,#103585,#103586,#103587,#103588,
#103589,#103590,#103591,#103592,#103593,#103594,#103595,#103596,#103597,
#103598,#103599,#103600,#103601,#103602,#103603,#103604,#103605,#103606,
#103607,#103608,#103609,#103610,#103611,#103612,#103613,#103614,#103615,
#103616,#103617,#103618,#103619),.UNSPECIFIED.,.F.,.F.,(4,2,2,2,2,2,2,2,
2,2,2,2,2,2,2,2,2,2,2,2,2,2,2,2,2,2,2,2,2,2,2,2,2,2,2,2,2,2,2,2,2,2,2,2,
2,2,2,2,2,2,2,2,2,2,2,2,2,2,2,2,2,2,2,2,2,2,2,2,2,2,2,2,2,2,2,2,2,2,2,2,
2,2,2,2,2,2,2,2,2,2,2,2,2,2,2,2,2,2,2,2,2,2,2,2,2,2,2,4),(-2.040887232292,
-2.03666953291386,-2.0185720126827,-2.01059751838255,-2.00414950872928,
-2.00047651251808,-1.99726744017411,-1.99326106182471,-1.98694722344255,
-1.94834691626407,-1.92309843911034,-1.91886514099533,-1.91668379939785,
-1.91487611940143,-1.91254070485979,-1.90768712736404,-1.88333166076441,
-1.86116015524922,-1.84836589844149,-1.83915786005575,-1.83495306334523,
-1.83172313944319,-1.82816717314162,-1.82227332125794,-1.79749633400461,
-1.76734066126651,-1.75883371237663,-1.75302706307418,-1.75055576875164,
-1.7487350547587,-1.74664493382882,-1.74295259629403,-1.7209534966772,-1.71668992074694,
-1.69451921602787,-1.68172257591819,-1.67251327119726,-1.66830824174573,
-1.66507827484309,-1.66152239593185,-1.65562900606932,-1.63086664042829,
-1.60069923242269,-1.59219081053239,-1.58638341468938,-1.58391196909029,
-1.58209118032001,-1.58000095951105,-1.57630853701169,-1.55430482274811,
-1.55004567236767,-1.52787603274915,-1.51508209200769,-1.50587422114435,
-1.50166935980776,-1.49843931856505,-1.49488314919549,-1.4889887699192,
-1.46419883956259,-1.43405487367914,-1.42554940409071,-1.41974347875045,
-1.41727228543911,-1.41545162873656,-1.41336166106002,-1.40966942642515,
-1.38763559713052,-1.38339728456899,-1.36122341224976,-1.34843346352139,
-1.33922783408728,-1.33502371350972,-1.33179415647721,-1.32823845050265,
-1.32234471172692,-1.2975590206639,-1.2674111639463,-1.25890541597281,-1.25309947941384,
-1.25062844768177,-1.24880788817346,-1.24671787694427,-1.24302578039765,
-1.22108241257199,-1.21677978374381,-1.19461377713962,-1.18180182076469,
-1.17258438924115,-1.16837790792402,-1.16514771916264,-1.1615924861753,
-1.15570227338321,-1.13103844638362,-1.10078946033223,-1.09227077558248,
-1.08645820359103,-1.0839857597272,-1.0821645353642,-1.08007383292645,-1.07638136684009,
-1.05448561699236,-1.05031828120701,-1.01168417378539,-1.00537323267675,
-1.0013672146156,-0.998157426840153,-0.994482483610981,-0.991222240709418),
 .UNSPECIFIED.);
#2751=B_SPLINE_CURVE_WITH_KNOTS('',3,(#103621,#103622,#103623,#103624,#103625,
#103626,#103627,#103628,#103629,#103630,#103631,#103632,#103633,#103634,
#103635,#103636),.UNSPECIFIED.,.F.,.F.,(4,2,2,2,2,2,2,4),(-0.0594803408397951,
-0.0341317359818735,-0.0193897131176647,-0.0142713275473659,-0.0108796444644127,
-0.00784109551082508,-0.0042585004903553,-0.000493910869673254),
 .UNSPECIFIED.);
#2752=B_SPLINE_CURVE_WITH_KNOTS('',3,(#103637,#103638,#103639,#103640,#103641,
#103642,#103643,#103644,#103645,#103646,#103647,#103648,#103649,#103650,
#103651,#103652,#103653,#103654,#103655,#103656,#103657,#103658,#103659,
#103660,#103661,#103662,#103663,#103664,#103665,#103666,#103667,#103668,
#103669,#103670,#103671,#103672,#103673,#103674,#103675,#103676,#103677,
#103678,#103679,#103680,#103681,#103682,#103683,#103684,#103685,#103686,
#103687,#103688,#103689,#103690,#103691,#103692,#103693,#103694,#103695,
#103696,#103697,#103698,#103699,#103700,#103701,#103702,#103703,#103704,
#103705,#103706,#103707,#103708,#103709,#103710,#103711,#103712,#103713,
#103714,#103715,#103716,#103717,#103718,#103719,#103720,#103721,#103722,
#103723,#103724,#103725,#103726,#103727,#103728,#103729,#103730,#103731,
#103732,#103733,#103734,#103735,#103736,#103737,#103738,#103739,#103740,
#103741,#103742,#103743,#103744,#103745,#103746,#103747,#103748,#103749,
#103750,#103751,#103752,#103753,#103754,#103755,#103756,#103757,#103758,
#103759,#103760,#103761,#103762,#103763,#103764,#103765,#103766,#103767,
#103768,#103769,#103770,#103771,#103772,#103773,#103774,#103775,#103776,
#103777,#103778,#103779,#103780,#103781,#103782,#103783,#103784,#103785,
#103786,#103787,#103788,#103789,#103790,#103791,#103792,#103793,#103794,
#103795,#103796,#103797,#103798,#103799,#103800,#103801,#103802,#103803,
#103804,#103805,#103806,#103807,#103808,#103809,#103810,#103811,#103812,
#103813,#103814,#103815,#103816,#103817,#103818,#103819,#103820,#103821,
#103822,#103823,#103824,#103825,#103826,#103827,#103828,#103829,#103830,
#103831,#103832),.UNSPECIFIED.,.F.,.F.,(4,2,2,2,2,2,2,2,2,2,2,2,2,2,2,2,
2,2,2,2,2,2,2,2,2,2,2,2,2,2,2,2,2,2,2,2,2,2,2,2,2,2,2,2,2,2,2,2,2,2,2,2,
2,2,2,2,2,2,2,2,2,2,2,2,2,2,2,2,2,2,2,2,2,2,2,2,2,2,2,2,2,2,2,2,2,2,2,2,
2,2,2,2,2,2,2,2,2,4),(-2.09955737348478,-2.09249363804168,-2.05186478690352,
-2.03400314306285,-2.02947537347083,-2.0272357297974,-2.02543105400486,
-2.02316384751153,-2.01849400394995,-1.9873709083723,-1.9541141692392,-1.94952711601161,
-1.9453345446043,-1.94210703370573,-1.93854676517244,-1.93262924894321,
-1.90781234846578,-1.87772525631266,-1.86922745320003,-1.86342568254911,
-1.86095566271704,-1.85913558857435,-1.85704591490962,-1.853353868358,-1.83124248110219,
-1.82705931735847,-1.80487911738487,-1.79210538553673,-1.78290858945313,
-1.77870651816563,-1.77547777925015,-1.77192223645062,-1.76602706289011,
-1.74117144173959,-1.71108225543972,-1.70258421325185,-1.69678231830782,
-1.69431226066999,-1.69249217443838,-1.69040251932229,-1.68671050682692,
-1.66460000893884,-1.66041651063186,-1.6382365892748,-1.62546275382996,
-1.61626593658586,-1.61206389636168,-1.60883519830179,-1.60527971819416,
-1.59938469322923,-1.57453249944831,-1.54444016056601,-1.53594174913135,
-1.53013968954824,-1.52766962982034,-1.52584956587825,-1.52375996058633,
-1.52006811355725,-1.49799401422789,-1.49378267950112,-1.47160508382937,
-1.45882522618436,-1.44962527419592,-1.44542270858241,-1.44219396510963,
-1.43863879273166,-1.43274512905879,-1.40793663212211,-1.37780676136823,
-1.36930365386673,-1.36349927471159,-1.36102883831851,-1.35920873596894,
-1.35711936331163,-1.35342852653399,-1.33159286973978,-1.32723609446333,
-1.30470510220014,-1.29207102500343,-1.2829475836689,-1.2787583958394,-1.27553135379609,
-1.27196945817642,-1.26604409931025,-1.23992280513,-1.21091816593292,-1.19851546132101,
-1.19528414826038,-1.19331603493944,-1.19147054838449,-1.18917264054935,
-1.18337493725435,-1.15093572219253,-1.12524601824734,-1.11623303387197,
-1.11206331586998,-1.10883870340174,-1.10882130641878),.UNSPECIFIED.);
#2753=B_SPLINE_CURVE_WITH_KNOTS('',3,(#103838,#103839,#103840,#103841,#103842,
#103843,#103844,#103845,#103846,#103847,#103848,#103849,#103850,#103851,
#103852,#103853,#103854,#103855,#103856,#103857,#103858,#103859,#103860,
#103861,#103862,#103863,#103864,#103865,#103866,#103867,#103868,#103869,
#103870,#103871,#103872,#103873,#103874,#103875,#103876,#103877,#103878,
#103879,#103880,#103881,#103882,#103883,#103884,#103885,#103886,#103887,
#103888,#103889,#103890,#103891,#103892,#103893,#103894,#103895,#103896,
#103897,#103898,#103899,#103900,#103901,#103902,#103903,#103904,#103905,
#103906,#103907,#103908,#103909,#103910,#103911,#103912,#103913,#103914,
#103915,#103916,#103917,#103918,#103919,#103920,#103921,#103922,#103923,
#103924,#103925,#103926,#103927,#103928,#103929,#103930,#103931,#103932,
#103933,#103934,#103935,#103936,#103937,#103938,#103939,#103940,#103941,
#103942,#103943,#103944,#103945,#103946,#103947,#103948,#103949,#103950,
#103951,#103952,#103953,#103954,#103955,#103956,#103957,#103958,#103959,
#103960,#103961,#103962,#103963,#103964,#103965,#103966,#103967,#103968,
#103969,#103970,#103971,#103972,#103973,#103974,#103975,#103976,#103977,
#103978,#103979,#103980,#103981,#103982,#103983,#103984,#103985,#103986,
#103987,#103988,#103989,#103990,#103991,#103992,#103993,#103994,#103995,
#103996,#103997,#103998,#103999,#104000,#104001,#104002,#104003,#104004,
#104005,#104006,#104007,#104008,#104009,#104010,#104011,#104012,#104013,
#104014,#104015,#104016,#104017,#104018,#104019,#104020,#104021,#104022,
#104023,#104024,#104025,#104026,#104027,#104028,#104029,#104030,#104031,
#104032,#104033,#104034,#104035,#104036,#104037,#104038,#104039,#104040,
#104041),.UNSPECIFIED.,.F.,.F.,(4,2,2,2,2,2,2,2,2,2,2,2,2,2,2,2,2,2,2,2,
2,2,2,2,2,2,2,2,2,2,2,2,2,2,2,2,2,2,2,2,2,2,2,2,2,2,2,2,2,2,2,2,2,2,2,2,
2,2,2,2,2,2,2,2,2,2,2,2,2,2,2,2,2,2,2,2,2,2,2,2,2,2,2,2,2,2,2,2,2,2,2,2,
2,2,2,2,2,2,2,2,2,4),(-0.991134658234024,-0.989393770439243,-0.985702139618141,
-0.983612358447809,-0.981791924665051,-0.979320930487852,-0.973514818048519,
-0.96500746119274,-0.934855935054433,-0.9100501113684,-0.90415544427592,
-0.900599670820795,-0.89737036637796,-0.89316700846563,-0.883964624168734,
-0.871182009641986,-0.849028683931204,-0.844834803383067,-0.82277855198614,
-0.819087319716109,-0.816997653907286,-0.815177242189328,-0.812706172704248,
-0.806899418659536,-0.798390701952386,-0.768227605827526,-0.743436286898861,
-0.737542171952347,-0.73398656428089,-0.73075730455012,-0.726553852890641,
-0.717350616097084,-0.704566271854376,-0.682414222128694,-0.678212664596025,
-0.656167297778629,-0.652476182179802,-0.650386569088503,-0.648566193710558,
-0.64609516089619,-0.640288437683084,-0.631779716589814,-0.601615813029859,
-0.576826631096773,-0.570932687960036,-0.567377164647168,-0.564147969337476,
-0.55994458402742,-0.550741417839805,-0.53795710810973,-0.515805619963614,
-0.511603297382461,-0.489559558032337,-0.485868523031835,-0.483778953869424,
-0.481958614062506,-0.479487626576206,-0.473680999501288,-0.465172407768735,
-0.435008749362983,-0.410220601814559,-0.40432679571375,-0.400771347344671,
-0.397542215077954,-0.393338904482458,-0.384135869830907,-0.371351715421386,
-0.34920072853768,-0.344998000516914,-0.322955350331874,-0.319264393601979,
-0.317174867834826,-0.315354568567354,-0.312883637679022,-0.307077143138314,
-0.298568747939646,-0.268405860680431,-0.243617990564167,-0.237724305658577,
-0.234168935720165,-0.230939878292876,-0.226736670573006,-0.217533886255367,
-0.204750103840634,-0.182599525294963,-0.158267438071558,-0.153413460110191,
-0.151078328699636,-0.149271108133408,-0.147179669269353,-0.143468184043144,
-0.138511203216898,-0.126878925379223,-0.105635912780473,-0.0772181914200325,
-0.0712212824659521,-0.0676440420580335,-0.0644202985524751,-0.0602596924002813,
-0.0512989624219987,-0.00636760239601622,-0.000492473137004156),
 .UNSPECIFIED.);
#2754=B_SPLINE_CURVE_WITH_KNOTS('',3,(#104042,#104043,#104044,#104045,#104046,
#104047,#104048,#104049,#104050,#104051,#104052,#104053,#104054,#104055,
#104056,#104057,#104058,#104059,#104060,#104061),.UNSPECIFIED.,.F.,.F.,
(4,2,2,2,2,2,2,2,2,4),(-2.09970265449674,-2.09186541748599,-2.08704536647685,
-2.08492637274696,-2.08321642563898,-2.08140245998211,-2.07903034634331,
-2.07385587384966,-2.057152820964,-2.040887232292),.UNSPECIFIED.);
#2755=B_SPLINE_CURVE_WITH_KNOTS('',3,(#104062,#104063,#104064,#104065,#104066,
#104067,#104068,#104069,#104070,#104071,#104072,#104073,#104074,#104075,
#104076,#104077,#104078,#104079,#104080,#104081,#104082,#104083,#104084,
#104085,#104086,#104087,#104088,#104089,#104090,#104091,#104092,#104093,
#104094,#104095,#104096,#104097,#104098,#104099,#104100,#104101,#104102,
#104103,#104104,#104105,#104106,#104107,#104108,#104109,#104110,#104111,
#104112,#104113,#104114,#104115,#104116,#104117,#104118,#104119,#104120,
#104121,#104122,#104123,#104124,#104125,#104126,#104127,#104128,#104129,
#104130,#104131,#104132,#104133,#104134,#104135,#104136,#104137,#104138,
#104139,#104140,#104141,#104142,#104143,#104144,#104145,#104146,#104147,
#104148,#104149,#104150,#104151,#104152,#104153,#104154,#104155,#104156,
#104157,#104158,#104159,#104160,#104161,#104162,#104163,#104164,#104165,
#104166,#104167,#104168,#104169,#104170,#104171,#104172,#104173,#104174,
#104175,#104176,#104177,#104178,#104179,#104180,#104181,#104182,#104183,
#104184,#104185,#104186,#104187,#104188,#104189,#104190,#104191,#104192,
#104193,#104194,#104195,#104196,#104197,#104198,#104199,#104200,#104201,
#104202,#104203,#104204,#104205,#104206,#104207,#104208,#104209,#104210,
#104211,#104212,#104213,#104214,#104215,#104216,#104217,#104218,#104219,
#104220,#104221,#104222,#104223,#104224,#104225,#104226,#104227,#104228,
#104229,#104230,#104231,#104232,#104233,#104234,#104235,#104236,#104237,
#104238,#104239,#104240,#104241,#104242,#104243,#104244,#104245,#104246,
#104247,#104248,#104249,#104250,#104251,#104252,#104253,#104254,#104255,
#104256,#104257,#104258,#104259,#104260,#104261,#104262,#104263,#104264,
#104265,#104266,#104267,#104268,#104269),.UNSPECIFIED.,.F.,.F.,(4,2,2,2,
2,2,2,2,2,2,2,2,2,2,2,2,2,2,2,2,2,2,2,2,2,2,2,2,2,2,2,2,2,2,2,2,2,2,2,2,
2,2,2,2,2,2,2,2,2,2,2,2,2,2,2,2,2,2,2,2,2,2,2,2,2,2,2,2,2,2,2,2,2,2,2,2,
2,2,2,2,2,2,2,2,2,2,2,2,2,2,2,2,2,2,2,2,2,2,2,2,2,2,2,4),(-1.10882130641878,
-1.10526679940843,-1.09929416858599,-1.07124182863778,-1.04978224507737,
-1.03261309916525,-1.02901859513812,-1.0269508692399,-1.02512549235125,
-1.02261513154994,-1.01656742080071,-1.0075668423812,-0.97311244338185,
-0.952936247658493,-0.947296301784389,-0.943795119647905,-0.940550174283224,
-0.936229606484671,-0.926332766823546,-0.912188999288603,-0.891751518712453,
-0.890602302139632,-0.866184405812538,-0.862471273019752,-0.860376962533257,
-0.858558048943376,-0.856096500177943,-0.850344966230737,-0.841946911634021,
-0.812645844209904,-0.786842140877459,-0.780922528658991,-0.777361961893787,
-0.774134797989161,-0.769943554181892,-0.760807455057905,-0.748150693251636,
-0.725521450964616,-0.721449714601169,-0.6995129487726,-0.695822543273843,
-0.69373333814469,-0.691913357886711,-0.689442999862523,-0.683638606677296,
-0.675134267439443,-0.645005466786183,-0.620165728542786,-0.614270716983036,
-0.610715424066274,-0.607487021297597,-0.603285541068394,-0.594090516808393,
-0.581321345463812,-0.559159715171629,-0.555024203999076,-0.532886515600972,
-0.52919542362308,-0.527106091103647,-0.52528618644532,-0.522816180975426,
-0.517013717335917,-0.508513200005048,-0.478413903667141,-0.453541477754723,
-0.447645590053882,-0.444090158226479,-0.440861875705518,-0.436660905531994,
-0.427468502450932,-0.414704238642015,-0.392541428554948,-0.388430977889081,
-0.366262337160064,-0.362571204701923,-0.360481888980159,-0.358662027335582,
-0.356192118217168,-0.350390048069933,-0.341890258147388,-0.311795956979986,
-0.286919007150828,-0.281023090080332,-0.277467699139969,-0.274239490806532,
-0.270038670350879,-0.260846821164539,-0.248083517011967,-0.225920921886999,
-0.201545888528755,-0.196697066266929,-0.194363217222348,-0.192556416795263,
-0.19037583703054,-0.186143204541015,-0.160916035860181,-0.122261374434154,
-0.11595196999513,-0.111947958382465,-0.108740517883322,-0.105069133520523,
-0.0986233217537091,-0.0777398511691188,-0.059270596115177),
 .UNSPECIFIED.);
#2756=B_SPLINE_CURVE_WITH_KNOTS('',3,(#104274,#104275,#104276,#104277,#104278,
#104279,#104280,#104281,#104282,#104283,#104284,#104285,#104286,#104287,
#104288,#104289,#104290,#104291,#104292,#104293,#104294,#104295,#104296,
#104297,#104298,#104299,#104300,#104301,#104302,#104303,#104304,#104305,
#104306,#104307,#104308,#104309,#104310,#104311,#104312,#104313,#104314,
#104315,#104316,#104317,#104318,#104319,#104320,#104321,#104322,#104323,
#104324,#104325,#104326,#104327,#104328,#104329,#104330,#104331,#104332,
#104333,#104334,#104335,#104336,#104337,#104338,#104339,#104340,#104341,
#104342,#104343,#104344,#104345,#104346,#104347,#104348,#104349,#104350,
#104351,#104352,#104353,#104354,#104355,#104356,#104357,#104358,#104359,
#104360,#104361,#104362,#104363,#104364,#104365,#104366,#104367,#104368,
#104369,#104370,#104371,#104372,#104373,#104374,#104375,#104376,#104377,
#104378,#104379,#104380,#104381,#104382,#104383,#104384,#104385,#104386,
#104387,#104388,#104389,#104390,#104391,#104392,#104393,#104394,#104395,
#104396,#104397,#104398,#104399,#104400,#104401,#104402,#104403,#104404,
#104405,#104406,#104407,#104408,#104409,#104410,#104411,#104412,#104413,
#104414,#104415,#104416,#104417,#104418,#104419,#104420,#104421,#104422,
#104423,#104424,#104425,#104426,#104427,#104428,#104429,#104430,#104431,
#104432,#104433,#104434,#104435,#104436,#104437,#104438,#104439,#104440,
#104441,#104442,#104443,#104444,#104445,#104446,#104447,#104448,#104449,
#104450,#104451,#104452,#104453,#104454,#104455,#104456,#104457,#104458,
#104459,#104460,#104461,#104462,#104463,#104464,#104465,#104466,#104467,
#104468,#104469,#104470,#104471,#104472,#104473),.UNSPECIFIED.,.F.,.F.,
(4,2,2,2,2,2,2,2,2,2,2,2,2,2,2,2,2,2,2,2,2,2,2,2,2,2,2,2,2,2,2,2,2,2,2,
2,2,2,2,2,2,2,2,2,2,2,2,2,2,2,2,2,2,2,2,2,2,2,2,2,2,2,2,2,2,2,2,2,2,2,2,
2,2,2,2,2,2,2,2,2,2,2,2,2,2,2,2,2,2,2,2,2,2,2,2,2,2,2,2,4),(-2.04071874618918,
-2.01961546049806,-1.99508613993201,-1.98732410099392,-1.98456387022839,
-1.98269551899839,-1.98072776909657,-1.9774994004954,-1.96635980234788,
-1.93822854429145,-1.91932946004213,-1.90726512582464,-1.9026149791725,
-1.89931415047375,-1.89592079794045,-1.89079831020504,-1.87611539979841,
-1.84315966082654,-1.82906442346955,-1.82082638711687,-1.81800560900694,
-1.81612529129228,-1.81441340890215,-1.81149639993504,-1.80316570486508,
-1.76971950645519,-1.75201166396843,-1.74045465128701,-1.73587666863379,
-1.73258894838706,-1.72917596183277,-1.72395779314342,-1.70837145446095,
-1.66922697733333,-1.65979372110739,-1.65353803863191,-1.65099419516361,
-1.64916361240751,-1.64711177126416,-1.6434964357234,-1.62670620419294,
-1.59208048384329,-1.57521728519362,-1.57000985238046,-1.56659913551912,
-1.56334728386305,-1.55878770901516,-1.5481986355223,-1.51142267142515,
-1.49626443202158,-1.48763084957389,-1.48476232305994,-1.48287230012894,
-1.48093546872148,-1.47784842443634,-1.46810946931968,-1.43894936540656,
-1.41963182371838,-1.40739501512038,-1.40272119391912,-1.39941615380399,
-1.39642515253182,-1.39241496618285,-1.38245951795514,-1.34503893597047,
-1.32970696593158,-1.32380454627599,-1.31938266977623,-1.31716371042709,
-1.31535829981061,-1.31306805182323,-1.30827846743112,-1.2782909051088,
-1.26674571982802,-1.2509211652044,-1.24021410642035,-1.23576340877781,
-1.23249747474174,-1.22945930711066,-1.22442441322099,-1.21052708360301,
-1.17090754868407,-1.16048900064823,-1.15377736382872,-1.15116374621136,
-1.14932207539876,-1.14730143844741,-1.14383046949961,-1.1296720110462,
-1.09931376619849,-1.07624189647906,-1.07056686680982,-1.06705771578794,
-1.0638145043765,-1.05958375829601,-1.04995277931304,-1.03633858779808,
-1.01533355633792,-1.01153671361318,-0.991134658234024),.UNSPECIFIED.);
#2757=B_SPLINE_CURVE_WITH_KNOTS('',3,(#104475,#104476,#104477,#104478,#104479,
#104480,#104481,#104482,#104483,#104484,#104485,#104486,#104487,#104488,
#104489,#104490,#104491,#104492,#104493,#104494),.UNSPECIFIED.,.F.,.F.,
(4,2,2,2,2,2,2,2,2,4),(-0.059270596115177,-0.0463606215788353,-0.0324747524269931,
-0.0290287076097999,-0.0270139937505328,-0.0251710223838709,-0.0233127838313809,
-0.0207405458901744,-0.0142423388580124,-0.000491547373460261),
 .UNSPECIFIED.);
#2758=B_SPLINE_CURVE_WITH_KNOTS('',3,(#104495,#104496,#104497,#104498,#104499,
#104500,#104501,#104502,#104503,#104504,#104505,#104506,#104507,#104508,
#104509,#104510,#104511,#104512,#104513,#104514,#104515,#104516,#104517,
#104518,#104519,#104520,#104521,#104522,#104523,#104524,#104525,#104526,
#104527,#104528,#104529,#104530,#104531,#104532,#104533,#104534,#104535,
#104536,#104537,#104538,#104539,#104540,#104541,#104542,#104543,#104544,
#104545,#104546,#104547,#104548,#104549,#104550,#104551,#104552,#104553,
#104554,#104555,#104556,#104557,#104558,#104559,#104560,#104561,#104562,
#104563,#104564,#104565,#104566,#104567,#104568,#104569,#104570,#104571,
#104572,#104573,#104574,#104575,#104576,#104577,#104578,#104579,#104580,
#104581,#104582,#104583,#104584,#104585,#104586,#104587,#104588,#104589,
#104590,#104591,#104592,#104593,#104594,#104595,#104596,#104597,#104598,
#104599,#104600,#104601,#104602,#104603,#104604,#104605,#104606,#104607,
#104608,#104609,#104610,#104611,#104612,#104613,#104614,#104615,#104616,
#104617,#104618,#104619,#104620,#104621,#104622,#104623,#104624,#104625,
#104626,#104627,#104628,#104629,#104630,#104631,#104632,#104633,#104634,
#104635,#104636,#104637,#104638,#104639,#104640,#104641,#104642,#104643,
#104644,#104645,#104646,#104647,#104648,#104649,#104650,#104651,#104652,
#104653,#104654,#104655,#104656,#104657,#104658,#104659,#104660,#104661,
#104662,#104663,#104664,#104665,#104666,#104667,#104668,#104669,#104670,
#104671,#104672,#104673,#104674,#104675,#104676,#104677,#104678,#104679,
#104680,#104681,#104682,#104683,#104684,#104685,#104686,#104687,#104688,
#104689,#104690,#104691,#104692,#104693,#104694,#104695,#104696,#104697,
#104698,#104699,#104700,#104701,#104702,#104703,#104704,#104705,#104706,
#104707,#104708,#104709,#104710,#104711,#104712,#104713,#104714,#104715,
#104716,#104717,#104718,#104719,#104720,#104721,#104722,#104723,#104724,
#104725,#104726,#104727,#104728,#104729,#104730,#104731,#104732,#104733,
#104734,#104735,#104736,#104737,#104738,#104739,#104740,#104741,#104742,
#104743,#104744,#104745,#104746,#104747,#104748,#104749,#104750,#104751,
#104752,#104753,#104754),.UNSPECIFIED.,.F.,.F.,(4,2,2,2,2,2,2,2,2,2,2,2,
2,2,2,2,2,2,2,2,2,2,2,2,2,2,2,2,2,2,2,2,2,2,2,2,2,2,2,2,2,2,2,2,2,2,2,2,
2,2,2,2,2,2,2,2,2,2,2,2,2,2,2,2,2,2,2,2,2,2,2,2,2,2,2,2,2,2,2,2,2,2,2,2,
2,2,2,2,2,2,2,2,2,2,2,2,2,2,2,2,2,2,2,2,2,2,2,2,2,2,2,2,2,2,2,2,2,2,2,2,
2,2,2,2,2,2,2,2,2,4),(-2.09991236431288,-2.05890814058238,-2.04942205507822,
-2.04517041685067,-2.04193540108864,-2.03840424310071,-2.03262268862309,
-2.01022431038967,-1.97796231366217,-1.96917168160048,-1.96331605603006,
-1.96094125373947,-1.96092453242584,-1.96090748382121,-1.96089009076418,
-1.96087233502679,-1.96085419725018,-1.96083565682671,-1.96081669174899,
-1.9607972786029,-1.96077739238786,-1.96075700641465,-1.96073609197738,
-1.96071461834799,-1.96069255255636,-1.96066985907439,-1.96064649965018,
-1.96062243302663,-1.96059761458855,-1.96057199603318,-1.96054552493718,
-1.96051814433738,-1.96048979225843,-1.960460401058,-1.96042989675817,-1.96039819832757,
-1.96036521684046,-1.9603308543533,-1.96029500277823,-1.96025754263415,
-1.96021834137281,-1.96017725155573,-1.95837029312953,-1.95603585834615,
-1.95118461416921,-1.92679835442126,-1.90461953487397,-1.89184728047984,
-1.88265144690322,-1.87844974116405,-1.87522125468098,-1.87166596212373,
-1.86577113961512,-1.84091474816518,-1.81082947983554,-1.80233226152457,
-1.79653089347695,-1.79406104145929,-1.79224109639157,-1.79015158736273,
-1.78645982225327,-1.76434674591972,-1.76016667379764,-1.73798804520478,
-1.72521579651358,-1.71601998411648,-1.71181830091257,-1.70858983682433,
-1.70503457400087,-1.6991398128623,-1.67428422602823,-1.64419863240782,
-1.63570140706375,-1.62990004699466,-1.62743020720255,-1.62561027461307,
-1.62352078394823,-1.61982905998773,-1.59772008498846,-1.59353698491781,
-1.57135873861843,-1.55858594727366,-1.54938986898487,-1.5451881582712,
-1.54195971016492,-1.53840450200631,-1.53250991970523,-1.50765906946368,
-1.47756972979603,-1.46907206543475,-1.46327049884719,-1.46080063550284,
-1.45898071086584,-1.4568912587972,-1.45319966646328,-1.43111947532519,
-1.4269144080036,-1.40473803983379,-1.3919605448457,-1.38276202263598,-1.37855990482942,
-1.37533142411474,-1.37177645978604,-1.36588294731705,-1.34106641469367,
-1.31094757684405,-1.30244622415752,-1.2966428378658,-1.29417268199262,
-1.29235273130574,-1.29026346994139,-1.2865726894119,-1.26469242852159,
-1.26050792417017,-1.23789272794201,-1.22523750836744,-1.21610314271166,
-1.21191224626731,-1.20868520387774,-1.20512462787616,-1.19920462500042,
-1.17333065400964,-1.14412056857565,-1.13573616760502,-1.12999101849191,
-1.12753061443486,-1.12571188575448,-1.1236170637095,-1.11990136925088,
-1.10912241679603),.UNSPECIFIED.);
#2759=B_SPLINE_CURVE_WITH_KNOTS('',3,(#104760,#104761,#104762,#104763,#104764,
#104765,#104766,#104767,#104768,#104769,#104770,#104771,#104772,#104773,
#104774,#104775,#104776,#104777,#104778,#104779,#104780,#104781,#104782,
#104783,#104784,#104785,#104786,#104787,#104788,#104789,#104790,#104791,
#104792,#104793,#104794,#104795,#104796,#104797,#104798,#104799,#104800,
#104801,#104802,#104803,#104804,#104805,#104806,#104807,#104808,#104809,
#104810,#104811,#104812,#104813,#104814,#104815,#104816,#104817,#104818,
#104819,#104820,#104821,#104822,#104823,#104824,#104825,#104826,#104827,
#104828,#104829,#104830,#104831,#104832,#104833,#104834,#104835,#104836,
#104837,#104838,#104839,#104840,#104841,#104842,#104843,#104844,#104845,
#104846,#104847,#104848,#104849,#104850,#104851,#104852,#104853,#104854,
#104855,#104856,#104857,#104858,#104859,#104860,#104861,#104862,#104863,
#104864,#104865,#104866,#104867,#104868,#104869,#104870,#104871,#104872,
#104873,#104874,#104875,#104876,#104877,#104878,#104879,#104880,#104881,
#104882,#104883,#104884,#104885,#104886,#104887,#104888,#104889,#104890,
#104891,#104892,#104893,#104894,#104895,#104896,#104897,#104898,#104899,
#104900,#104901,#104902,#104903,#104904,#104905,#104906,#104907,#104908,
#104909,#104910,#104911,#104912,#104913,#104914,#104915,#104916,#104917,
#104918,#104919,#104920,#104921,#104922,#104923,#104924,#104925,#104926,
#104927,#104928,#104929,#104930,#104931,#104932,#104933,#104934,#104935,
#104936,#104937,#104938,#104939,#104940,#104941,#104942,#104943,#104944,
#104945,#104946,#104947,#104948,#104949,#104950,#104951,#104952,#104953,
#104954,#104955,#104956,#104957,#104958,#104959,#104960,#104961,#104962,
#104963,#104964,#104965,#104966,#104967,#104968,#104969,#104970,#104971,
#104972,#104973,#104974,#104975,#104976,#104977,#104978,#104979,#104980,
#104981),.UNSPECIFIED.,.F.,.F.,(4,2,2,2,2,2,2,2,2,2,2,2,2,2,2,2,2,2,2,2,
2,2,2,2,2,2,2,2,2,2,2,2,2,2,2,2,2,2,2,2,2,2,2,2,2,2,2,2,2,2,2,2,2,2,2,2,
2,2,2,2,2,2,2,2,2,2,2,2,2,2,2,2,2,2,2,2,2,2,2,2,2,2,2,2,2,2,2,2,2,2,2,2,
2,2,2,2,2,2,2,2,2,2,2,2,2,2,2,2,2,2,4),(-0.991205554037858,-0.979929488239522,
-0.973239680348427,-0.969124100324602,-0.96590456768069,-0.962300386779387,
-0.956179932514309,-0.921052257246141,-0.891628407896895,-0.886845712937254,
-0.884556476683887,-0.882750718757385,-0.88052993113071,-0.876100275497577,
-0.870183962523765,-0.854795534377931,-0.817182797173947,-0.807377773103285,
-0.803391583271509,-0.8001073485437,-0.796741462203431,-0.791755968593157,
-0.777027038131106,-0.750739733210124,-0.725140728152079,-0.7202978832177,
-0.71796453677848,-0.716156915981696,-0.713973798356414,-0.70973188745755,
-0.704142062956238,-0.690100988823647,-0.657347521488646,-0.642394121064468,
-0.637243019677451,-0.633843521538133,-0.630546274055562,-0.625917293356997,
-0.614005991356797,-0.595475186460841,-0.568243261838846,-0.555883599898062,
-0.552541068481579,-0.550548245130541,-0.548693674369856,-0.546007268064864,
-0.538792364667649,-0.527228811182223,-0.506007000557386,-0.477461266304887,
-0.471451539889824,-0.467870895582047,-0.464646712316049,-0.460489238715048,
-0.451550443978713,-0.425068681636558,-0.391103554260244,-0.386665001386152,
-0.384442506470657,-0.38263688140735,-0.380349724468751,-0.375577694724279,
-0.355540891292406,-0.31978169523648,-0.308117911232646,-0.303394216420157,
-0.30011249911231,-0.296743747198049,-0.291743575231823,-0.276883187416715,
-0.250164442692066,-0.225260701749933,-0.220294179723399,-0.217970593637933,
-0.216163578025005,-0.213972707013279,-0.209692181873003,-0.185106378317987,
-0.145694351108715,-0.139480476804126,-0.135503536322483,-0.132296684993092,
-0.131787137618101,-0.131527804925709,-0.13132014286362,-0.131149430904764,
-0.131006168900059,-0.13088392131668,-0.130778157724808,-0.130685587416395,
-0.130603757150829,-0.130530797308936,-0.130465255932637,-0.130405986857194,
-0.130352072267633,-0.130302767846003,-0.130257463110954,-0.130215652326327,
-0.130057786506376,-0.129899898005545,-0.124976252442725,-0.10988205423827,
-0.0822694396196656,-0.0804589308759995,-0.0566193668578111,-0.0529166787477501,
-0.0508243112860018,-0.0490042430694455,-0.0465372457426665,-0.0407558851820747,
-0.000492258923205386),.UNSPECIFIED.);
#2760=B_SPLINE_CURVE_WITH_KNOTS('',3,(#104982,#104983,#104984,#104985,#104986,
#104987,#104988,#104989,#104990,#104991,#104992,#104993,#104994,#104995,
#104996,#104997,#104998,#104999),.UNSPECIFIED.,.F.,.F.,(4,2,2,2,2,2,2,2,
4),(-2.09977792447378,-2.07701759521765,-2.07253004579203,-2.06924681052091,
-2.06594529428715,-2.06295025244637,-2.05815818445511,-2.04603073547732,
-2.04071874618918),.UNSPECIFIED.);
#2761=B_SPLINE_CURVE_WITH_KNOTS('',3,(#105000,#105001,#105002,#105003,#105004,
#105005,#105006,#105007,#105008,#105009,#105010,#105011,#105012,#105013,
#105014,#105015,#105016,#105017,#105018,#105019,#105020,#105021,#105022,
#105023,#105024,#105025,#105026,#105027,#105028,#105029,#105030,#105031,
#105032,#105033,#105034,#105035,#105036,#105037,#105038,#105039,#105040,
#105041,#105042,#105043,#105044,#105045,#105046,#105047,#105048,#105049,
#105050,#105051,#105052,#105053,#105054,#105055,#105056,#105057,#105058,
#105059,#105060,#105061,#105062,#105063,#105064,#105065,#105066,#105067,
#105068,#105069,#105070,#105071,#105072,#105073,#105074,#105075,#105076,
#105077,#105078,#105079,#105080,#105081,#105082,#105083,#105084,#105085,
#105086,#105087,#105088,#105089,#105090,#105091,#105092,#105093,#105094,
#105095,#105096,#105097,#105098,#105099,#105100,#105101,#105102,#105103,
#105104,#105105,#105106,#105107,#105108,#105109,#105110,#105111,#105112,
#105113,#105114,#105115,#105116,#105117,#105118,#105119,#105120,#105121,
#105122,#105123,#105124,#105125,#105126,#105127,#105128,#105129,#105130,
#105131,#105132,#105133,#105134,#105135,#105136,#105137,#105138,#105139,
#105140,#105141,#105142,#105143,#105144,#105145,#105146,#105147,#105148,
#105149,#105150,#105151,#105152,#105153,#105154,#105155,#105156,#105157,
#105158,#105159,#105160,#105161,#105162,#105163,#105164,#105165,#105166,
#105167,#105168,#105169,#105170,#105171,#105172,#105173,#105174,#105175,
#105176,#105177,#105178,#105179,#105180,#105181,#105182,#105183,#105184,
#105185,#105186,#105187,#105188,#105189,#105190,#105191,#105192,#105193,
#105194,#105195,#105196,#105197),.UNSPECIFIED.,.F.,.F.,(4,2,2,2,2,2,2,2,
2,2,2,2,2,2,2,2,2,2,2,2,2,2,2,2,2,2,2,2,2,2,2,2,2,2,2,2,2,2,2,2,2,2,2,2,
2,2,2,2,2,2,2,2,2,2,2,2,2,2,2,2,2,2,2,2,2,2,2,2,2,2,2,2,2,2,2,2,2,2,2,2,
2,2,2,2,2,2,2,2,2,2,2,2,2,2,2,2,2,2,4),(-1.10912241679603,-1.09537616038099,
-1.07747396274481,-1.06117113868342,-1.05024299434426,-1.04620603905425,
-1.04320923530063,-1.03991167869396,-1.03527510639529,-1.02330113889305,
-1.00461877832252,-0.977009612586079,-0.965169028350568,-0.961879849746099,
-0.959899223268496,-0.958039491207421,-0.955321984160442,-0.947876355979257,
-0.935765227971143,-0.900051965429733,-0.885129537697124,-0.879983103809995,
-0.876585638973385,-0.873289611476752,-0.868661120861592,-0.856744178551556,
-0.838197160155459,-0.810923613877317,-0.798628264142535,-0.795291796493434,
-0.793300872978823,-0.791446689910993,-0.788758967192956,-0.781529311498818,
-0.769929524591374,-0.748753934919004,-0.720223032384794,-0.714216426599012,
-0.710637494906361,-0.707414793028382,-0.703259179597336,-0.694324410716642,
-0.667815224220001,-0.633886307497032,-0.629445156774992,-0.627222756755551,
-0.625418003697579,-0.623133036513319,-0.618369249228712,-0.598400130521092,
-0.562835222525317,-0.550973114514668,-0.54622232076107,-0.542936663406515,
-0.539576175286326,-0.534611778118246,-0.520054724256004,-0.494312875574829,
-0.467968686324046,-0.463123628792559,-0.46079051256424,-0.458983741420501,
-0.456802543264675,-0.452566915501582,-0.42679727919605,-0.388813513831111,
-0.38243847116907,-0.378415241075314,-0.375206226601998,-0.371547978758963,
-0.365164920259045,-0.357293913441052,-0.339569945749232,-0.30613493905344,
-0.297849302311913,-0.294938933959659,-0.293228785125839,-0.291348251526259,
-0.288523707660054,-0.280249850114902,-0.26605718374843,-0.232768512616576,
-0.218444422325762,-0.213361428469145,-0.210315254278324,-0.207056460603241,
-0.202643586668177,-0.192171767052842,-0.176846014280266,-0.146551191965447,
-0.132329082941721,-0.128859438601076,-0.126839594476986,-0.124998726569516,
-0.12238641645134,-0.11606002628771,-0.0944046175112616,-0.0678885621054014,
-0.0595555566481069),.UNSPECIFIED.);
#2762=B_SPLINE_CURVE_WITH_KNOTS('',3,(#105202,#105203,#105204,#105205,#105206,
#105207,#105208,#105209,#105210,#105211,#105212,#105213,#105214,#105215,
#105216,#105217,#105218,#105219,#105220,#105221,#105222,#105223,#105224,
#105225,#105226,#105227,#105228,#105229,#105230,#105231,#105232,#105233,
#105234,#105235,#105236,#105237,#105238,#105239,#105240,#105241,#105242,
#105243,#105244,#105245,#105246,#105247,#105248,#105249,#105250,#105251,
#105252,#105253,#105254,#105255,#105256,#105257,#105258,#105259,#105260,
#105261,#105262,#105263,#105264,#105265,#105266,#105267,#105268,#105269,
#105270,#105271,#105272,#105273,#105274,#105275,#105276,#105277,#105278,
#105279,#105280,#105281,#105282,#105283,#105284,#105285,#105286,#105287,
#105288,#105289,#105290,#105291,#105292,#105293,#105294,#105295,#105296,
#105297,#105298,#105299,#105300,#105301,#105302,#105303,#105304,#105305,
#105306,#105307,#105308,#105309,#105310,#105311,#105312,#105313,#105314,
#105315,#105316,#105317,#105318,#105319,#105320,#105321,#105322,#105323,
#105324,#105325,#105326,#105327,#105328,#105329,#105330,#105331,#105332,
#105333,#105334,#105335,#105336,#105337,#105338,#105339,#105340,#105341,
#105342,#105343,#105344,#105345,#105346,#105347,#105348,#105349,#105350,
#105351,#105352,#105353,#105354,#105355,#105356,#105357,#105358,#105359,
#105360,#105361,#105362,#105363,#105364,#105365,#105366,#105367,#105368,
#105369,#105370,#105371,#105372,#105373,#105374,#105375,#105376,#105377,
#105378,#105379,#105380,#105381,#105382,#105383,#105384,#105385,#105386,
#105387,#105388,#105389,#105390,#105391,#105392,#105393,#105394,#105395,
#105396,#105397,#105398,#105399,#105400,#105401,#105402,#105403,#105404,
#105405,#105406,#105407,#105408,#105409,#105410,#105411,#105412,#105413,
#105414,#105415,#105416,#105417,#105418,#105419,#105420,#105421,#105422,
#105423,#105424,#105425,#105426,#105427,#105428,#105429,#105430,#105431,
#105432,#105433,#105434,#105435,#105436,#105437),.UNSPECIFIED.,.F.,.F.,
(4,2,2,2,2,2,2,2,2,2,2,2,2,2,2,2,2,2,2,2,2,2,2,2,2,2,2,2,2,2,2,2,2,2,2,
2,2,2,2,2,2,2,2,2,2,2,2,2,2,2,2,2,2,2,2,2,2,2,2,2,2,2,2,2,2,2,2,2,2,2,2,
2,2,2,2,2,2,2,2,2,2,2,2,2,2,2,2,2,2,2,2,2,2,2,2,2,2,2,2,2,2,2,2,2,2,2,2,
2,2,2,2,2,2,2,2,2,2,4),(-2.04099839520778,-2.01939573360936,-2.01831944035928,
-1.9906444489668,-1.9755310051931,-1.97060527853868,-1.97044735083837,-1.97028944353156,
-1.97024760888034,-1.97020227361801,-1.97015293101081,-1.97009896938324,
-1.97003964291678,-1.96997403196382,-1.96990098801235,-1.96981905616593,
-1.96972636299089,-1.96962045018923,-1.96949802030445,-1.96935453368078,
-1.96918354181598,-1.96897552594511,-1.96871573814881,-1.96806955035828,
-1.96485695328726,-1.9608084691524,-1.9524682042581,-1.91308143183545,-1.89722023380667,
-1.88833466357603,-1.88543653049693,-1.88354015844704,-1.8816103879941,
-1.87855663265051,-1.86911353166549,-1.83634965688227,-1.81908433252053,
-1.80772124937577,-1.80317125991983,-1.79988820011862,-1.7968724903244,
-1.7919632564458,-1.7790259856766,-1.74450215625132,-1.72996454631121,-1.72425243998551,
-1.7199395222239,-1.71774215112674,-1.71593556301261,-1.71361988816888,
-1.70869584268628,-1.68530494250538,-1.66523433708602,-1.65068347229347,
-1.64058578819142,-1.63623137082558,-1.63298039200552,-1.62949100537016,
-1.62391058415889,-1.60471680059066,-1.56121982196668,-1.55440303719899,
-1.55177363457131,-1.54992907673756,-1.54791442729921,-1.54447190894558,
-1.53066901158982,-1.50442861802324,-1.48627728381298,-1.47452804242991,
-1.46992189534187,-1.46662870195648,-1.46362423583537,-1.45955919989408,
-1.44926613205415,-1.40847253598747,-1.39572105892504,-1.38801067860277,
-1.38525694464806,-1.38338963129241,-1.38141936946125,-1.37818045677944,
-1.36692740607782,-1.33516254934427,-1.31862416523762,-1.3075871883527,
-1.30308554780868,-1.29981062285941,-1.29678386394173,-1.2918139878612,
-1.27843362866053,-1.24431536573725,-1.22989107396882,-1.22420650605244,
-1.21990938860676,-1.21771508652841,-1.21590816366619,-1.21358840858768,
-1.20864304259139,-1.18220319675944,-1.16749602490232,-1.15157547130906,
-1.14082292105715,-1.13636460945623,-1.13309689095308,-1.13005973846244,
-1.12503283608603,-1.11120709438071,-1.07749135416292,-1.06318025572464,
-1.05485981693471,-1.05202857007244,-1.0501459009344,-1.04819854897539,
-1.04506450603386,-1.03384432349115,-1.01015486702639,-0.991205554037858),
 .UNSPECIFIED.);
#2763=B_SPLINE_CURVE_WITH_KNOTS('',3,(#105439,#105440,#105441,#105442,#105443,
#105444,#105445,#105446,#105447,#105448,#105449,#105450,#105451,#105452,
#105453,#105454),.UNSPECIFIED.,.F.,.F.,(4,2,2,2,2,2,2,4),(-0.0595555566481069,
-0.052158634671153,-0.0469231542530946,-0.0435074117017776,-0.0402233239291963,
-0.0369694877437875,-0.0325599867995973,-0.000491890560030468),
 .UNSPECIFIED.);
#2764=B_SPLINE_CURVE_WITH_KNOTS('',3,(#105455,#105456,#105457,#105458,#105459,
#105460,#105461,#105462,#105463,#105464,#105465,#105466,#105467,#105468,
#105469,#105470,#105471,#105472,#105473,#105474,#105475,#105476,#105477,
#105478,#105479,#105480,#105481,#105482,#105483,#105484,#105485,#105486,
#105487,#105488,#105489,#105490,#105491,#105492,#105493,#105494,#105495,
#105496,#105497,#105498,#105499,#105500,#105501,#105502,#105503,#105504,
#105505,#105506,#105507,#105508,#105509,#105510,#105511,#105512,#105513,
#105514,#105515,#105516,#105517,#105518,#105519,#105520,#105521,#105522,
#105523,#105524,#105525,#105526,#105527,#105528,#105529,#105530,#105531,
#105532,#105533,#105534,#105535,#105536,#105537,#105538,#105539,#105540,
#105541,#105542,#105543,#105544,#105545,#105546,#105547,#105548,#105549,
#105550,#105551,#105552,#105553,#105554,#105555,#105556,#105557,#105558,
#105559,#105560,#105561,#105562,#105563,#105564,#105565,#105566,#105567,
#105568,#105569,#105570,#105571,#105572,#105573,#105574,#105575,#105576,
#105577,#105578,#105579,#105580,#105581,#105582,#105583,#105584,#105585,
#105586,#105587,#105588,#105589,#105590,#105591,#105592,#105593,#105594,
#105595,#105596,#105597,#105598,#105599,#105600,#105601,#105602,#105603,
#105604,#105605,#105606,#105607,#105608,#105609,#105610,#105611,#105612,
#105613,#105614,#105615,#105616,#105617),.UNSPECIFIED.,.F.,.F.,(4,3,3,3,
3,3,3,3,3,3,3,3,3,3,3,3,3,3,3,3,3,3,3,3,3,3,3,3,3,3,3,3,3,3,3,3,3,3,3,3,
3,3,3,3,3,3,3,3,3,3,3,3,3,3,4),(-54.1118657207119,-53.968500634934,-53.8675843506887,
-53.7577897347117,-53.6468205794156,-53.5373284361958,-53.4279032844601,
-53.3185044306203,-53.2063874460508,-53.0968489113658,-52.9834427018542,
-52.8700364923426,-52.7602418763654,-52.6492727210693,-52.5397805778494,
-52.4303554261136,-52.3209565722737,-52.2088395877044,-52.0993010530191,
-51.9858948435078,-51.8724886339965,-51.7626940180194,-51.6517248627233,
-51.5422327195034,-51.4328075677676,-51.3234087139278,-51.2112917293584,
-51.1017531946732,-50.9883469851618,-50.8749407756504,-50.7651461596733,
-50.6541770043772,-50.5446848611574,-50.4352597094216,-50.3258608555818,
-50.2137438710124,-50.1042053363273,-49.9907991268158,-49.8773929173043,
-49.7675983013272,-49.6566291460311,-49.5471370028112,-49.4377118510754,
-49.3283129972355,-49.2161960126662,-49.1066574779811,-48.9932512684696,
-48.8798450589582,-48.7700749181095,-48.6604636787918,-48.5509703718656,
-48.4415394130409,-48.3321442536605,-48.2227090186297,-48.1819144221909),
 .UNSPECIFIED.);
#2765=B_SPLINE_CURVE_WITH_KNOTS('',3,(#105623,#105624,#105625,#105626,#105627,
#105628,#105629,#105630,#105631,#105632,#105633,#105634,#105635,#105636,
#105637,#105638,#105639,#105640,#105641,#105642,#105643,#105644,#105645,
#105646,#105647,#105648,#105649,#105650,#105651,#105652,#105653,#105654,
#105655,#105656,#105657,#105658,#105659,#105660,#105661,#105662,#105663,
#105664,#105665,#105666,#105667,#105668,#105669,#105670,#105671,#105672,
#105673,#105674,#105675,#105676,#105677,#105678,#105679,#105680,#105681,
#105682,#105683,#105684,#105685,#105686,#105687,#105688,#105689,#105690,
#105691,#105692,#105693,#105694,#105695,#105696,#105697,#105698,#105699,
#105700,#105701,#105702,#105703,#105704,#105705,#105706,#105707,#105708,
#105709,#105710,#105711,#105712,#105713,#105714,#105715,#105716,#105717,
#105718,#105719,#105720,#105721,#105722,#105723,#105724,#105725,#105726,
#105727,#105728,#105729,#105730,#105731,#105732,#105733,#105734,#105735,
#105736,#105737,#105738,#105739,#105740,#105741,#105742,#105743,#105744,
#105745,#105746,#105747,#105748,#105749,#105750,#105751,#105752,#105753,
#105754,#105755,#105756,#105757,#105758,#105759,#105760,#105761,#105762,
#105763,#105764,#105765,#105766,#105767,#105768,#105769,#105770,#105771,
#105772,#105773,#105774,#105775,#105776,#105777,#105778,#105779,#105780,
#105781,#105782,#105783,#105784,#105785,#105786,#105787,#105788,#105789,
#105790,#105791,#105792,#105793,#105794,#105795,#105796,#105797,#105798,
#105799,#105800,#105801,#105802,#105803,#105804,#105805,#105806,#105807,
#105808,#105809,#105810,#105811,#105812,#105813,#105814,#105815,#105816,
#105817,#105818,#105819,#105820,#105821,#105822,#105823,#105824,#105825,
#105826,#105827,#105828),.UNSPECIFIED.,.F.,.F.,(4,2,2,2,2,2,2,2,2,2,2,2,
2,2,2,2,2,2,2,2,2,2,2,2,2,2,2,2,2,2,2,2,2,2,2,2,2,2,2,2,2,2,2,2,2,2,2,2,
2,2,2,2,2,2,2,2,2,2,2,2,2,2,2,2,2,2,2,2,2,2,2,2,2,2,2,2,2,2,2,2,2,2,2,2,
2,2,2,2,2,2,2,2,2,2,2,2,2,2,2,2,2,2,4),(-0.991228980721755,-0.983399078957842,
-0.979460113584548,-0.957084565640262,-0.953391691373635,-0.951301495530232,
-0.949480907430011,-0.947009980657939,-0.941205245558575,-0.932701008487992,
-0.902578244436011,-0.877732967343426,-0.871836546988952,-0.868280152433777,
-0.865050560141928,-0.860847224092474,-0.851646576915701,-0.83886779977462,
-0.816710006188954,-0.812537405379585,-0.790450018785875,-0.786758279881265,
-0.784668364252601,-0.782847761123251,-0.780376467081482,-0.774569341318892,
-0.766060220822828,-0.735897959636949,-0.711099264715003,-0.705204368136027,
-0.701648345184216,-0.698418743869457,-0.694214898646253,-0.685011017654734,
-0.672225961689675,-0.650071244330366,-0.645871809402301,-0.623820593470023,
-0.620129065532894,-0.618039223390797,-0.616218651426804,-0.613747355708804,
-0.607940032226353,-0.599430446836377,-0.569263718166024,-0.544471384435351,
-0.538576790007748,-0.535020879171879,-0.531791335278851,-0.527587501045188,
-0.518383372429963,-0.505597743317259,-0.483443832258745,-0.479241265067081,
-0.457194845703296,-0.453503410940628,-0.451413615940351,-0.449593081035736,
-0.447121830257443,-0.441314588734614,-0.432805102066618,-0.40263837927036,
-0.377847274631405,-0.371952824777447,-0.368396992584879,-0.365167514691985,
-0.360963758579918,-0.35175976781384,-0.338974302188154,-0.316820894417893,
-0.312618024795321,-0.290572590485879,-0.286881234515208,-0.284791483440623,
-0.282970986315148,-0.280499786167051,-0.274692660752007,-0.26618334162358,
-0.236017170985046,-0.211219097846803,-0.205328748067624,-0.201773835172136,
-0.198544207948106,-0.194338843513685,-0.185125300529055,-0.172321473124871,
-0.149944659398351,-0.145934749141311,-0.123953037556204,-0.120261997744582,
-0.118172343197543,-0.116351871197342,-0.113880626212398,-0.108073047562501,
-0.0818761565133594,-0.0549676500763384,-0.0424561977089353,-0.0376077067301623,
-0.0346029870465107,-0.0313111572356573,-0.0280446275150207,-0.0236019623783744,
-0.000491634459526482),.UNSPECIFIED.);
#2766=B_SPLINE_CURVE_WITH_KNOTS('',3,(#105829,#105830,#105831,#105832,#105833,
#105834,#105835,#105836,#105837,#105838,#105839,#105840,#105841,#105842,
#105843,#105844),.UNSPECIFIED.,.F.,.F.,(4,2,2,2,2,2,2,4),(-2.09980207912905,
-2.05974703936122,-2.05399628535234,-2.05153435059402,-2.04971481350122,
-2.04761936391674,-2.04390312850233,-2.04099839520778),.UNSPECIFIED.);
#2767=B_SPLINE_CURVE_WITH_KNOTS('',3,(#105846,#105847,#105848,#105849,#105850,
#105851,#105852,#105853,#105854,#105855,#105856,#105857,#105858),
 .UNSPECIFIED.,.F.,.F.,(4,3,3,3,4),(-48.1819144221909,-48.0723535220419,
-47.9625891320687,-47.8822972006122,-47.8286804139494),.UNSPECIFIED.);
#2768=B_SPLINE_CURVE_WITH_KNOTS('',3,(#105859,#105860,#105861,#105862,#105863,
#105864,#105865,#105866,#105867),.UNSPECIFIED.,.F.,.F.,(4,1,1,1,1,1,4),
(-47.8286738934412,-46.8847493422661,-45.88720148392,-44.8896536255739,
-43.8921057672278,-42.8945579088817,-41.8982186577127),.UNSPECIFIED.);
#2769=B_SPLINE_CURVE_WITH_KNOTS('',3,(#105872,#105873,#105874,#105875,#105876,
#105877,#105878,#105879,#105880,#105881,#105882,#105883,#105884,#105885,
#105886,#105887,#105888,#105889,#105890,#105891,#105892,#105893,#105894,
#105895,#105896,#105897,#105898,#105899,#105900,#105901,#105902,#105903,
#105904,#105905,#105906,#105907,#105908,#105909,#105910,#105911,#105912,
#105913,#105914,#105915,#105916,#105917,#105918,#105919,#105920,#105921,
#105922,#105923,#105924,#105925,#105926,#105927,#105928,#105929,#105930,
#105931,#105932,#105933,#105934,#105935,#105936,#105937,#105938,#105939,
#105940,#105941,#105942,#105943,#105944,#105945,#105946,#105947,#105948,
#105949,#105950,#105951,#105952,#105953,#105954,#105955,#105956,#105957,
#105958,#105959,#105960,#105961,#105962,#105963,#105964,#105965,#105966,
#105967,#105968,#105969,#105970,#105971,#105972,#105973,#105974,#105975,
#105976,#105977,#105978,#105979,#105980,#105981,#105982,#105983,#105984,
#105985,#105986,#105987,#105988,#105989,#105990,#105991,#105992,#105993,
#105994,#105995,#105996,#105997,#105998,#105999,#106000,#106001,#106002,
#106003,#106004,#106005,#106006,#106007,#106008,#106009,#106010,#106011,
#106012,#106013,#106014,#106015,#106016,#106017,#106018,#106019,#106020,
#106021,#106022,#106023,#106024,#106025,#106026,#106027,#106028,#106029,
#106030,#106031,#106032,#106033,#106034,#106035,#106036,#106037,#106038,
#106039,#106040,#106041,#106042,#106043,#106044,#106045,#106046,#106047,
#106048,#106049,#106050,#106051,#106052,#106053,#106054,#106055,#106056,
#106057,#106058,#106059,#106060,#106061,#106062,#106063,#106064,#106065,
#106066,#106067,#106068,#106069,#106070,#106071,#106072,#106073,#106074,
#106075,#106076,#106077),.UNSPECIFIED.,.F.,.F.,(4,2,2,2,2,2,2,2,2,2,2,2,
2,2,2,2,2,2,2,2,2,2,2,2,2,2,2,2,2,2,2,2,2,2,2,2,2,2,2,2,2,2,2,2,2,2,2,2,
2,2,2,2,2,2,2,2,2,2,2,2,2,2,2,2,2,2,2,2,2,2,2,2,2,2,2,2,2,2,2,2,2,2,2,2,
2,2,2,2,2,2,2,2,2,2,2,2,2,2,2,2,2,2,4),(-2.04104007014271,-2.0387525359055,
-2.03514317100133,-2.03192444057663,-2.0278173682406,-2.02115754469679,
-1.98880506671721,-1.96672848881058,-1.95943883257924,-1.95580738612716,
-1.95292532574864,-1.95103268219419,-1.94919305726299,-1.94692052220931,
-1.94119266427461,-1.90869784896389,-1.8829003498935,-1.87389715730153,
-1.86972808226165,-1.86650235363778,-1.86292755179802,-1.85694596726494,
-1.82754916128068,-1.80533947904071,-1.79492278112375,-1.78821162585083,
-1.78559779403393,-1.7837558389576,-1.78173474119667,-1.77826268249817,
-1.76402689582707,-1.73369326423287,-1.71836584183501,-1.70789277115906,
-1.70347813427133,-1.70021760141858,-1.69716948850042,-1.69208239359735,
-1.67773598291939,-1.64145865182086,-1.62927324680306,-1.62179529747193,
-1.61907264261978,-1.617211282177,-1.6154769339966,-1.61244502578709,-1.60319029021224,
-1.57031221478931,-1.5529701490403,-1.54157292972686,-1.53701777282535,
-1.53373367625438,-1.53071885529284,-1.52581525223006,-1.51291955083575,
-1.47835452282733,-1.46380512849904,-1.45809003230311,-1.4537753371727,
-1.4515775381009,-1.44977087104003,-1.44745544311587,-1.44253312301147,
-1.41924099168559,-1.39126246543584,-1.37603081688486,-1.37098945439346,
-1.36761232917214,-1.36433695078348,-1.35964795279919,-1.34818367976645,
-1.30873945363392,-1.29614993194195,-1.28850546335625,-1.28576047473732,
-1.28389486636067,-1.28192185865187,-1.27867028479885,-1.26727401006814,
-1.23932112787998,-1.22049431678454,-1.20845948096966,-1.20381300759226,
-1.20051248893365,-1.19711749130626,-1.19198866924457,-1.17725004030893,
-1.13717557409296,-1.12766615899306,-1.12137410103298,-1.11882424158117,
-1.11699247244179,-1.11494287637059,-1.11133911737094,-1.09484515789665,
-1.05022618693345,-1.04074433881468,-1.0365382240233,-1.03329840976035,
-1.02977758489838,-1.02404866411753,-0.999989180191607,-0.991228980721755),
 .UNSPECIFIED.);
#2770=B_SPLINE_CURVE_WITH_KNOTS('',3,(#106079,#106080,#106081,#106082,#106083),
 .UNSPECIFIED.,.F.,.F.,(4,1,4),(-41.8982186577127,-41.8970100505357,-41.5455025263571),
 .UNSPECIFIED.);
#2771=B_SPLINE_CURVE_WITH_KNOTS('',3,(#106084,#106085,#106086,#106087,#106088,
#106089,#106090,#106091,#106092,#106093,#106094,#106095,#106096,#106097,
#106098,#106099,#106100,#106101,#106102,#106103,#106104,#106105,#106106,
#106107,#106108,#106109,#106110,#106111,#106112,#106113,#106114,#106115,
#106116,#106117,#106118,#106119,#106120,#106121,#106122,#106123,#106124,
#106125,#106126,#106127,#106128,#106129,#106130,#106131,#106132,#106133,
#106134,#106135,#106136,#106137,#106138,#106139,#106140,#106141,#106142,
#106143,#106144,#106145,#106146,#106147,#106148,#106149,#106150,#106151,
#106152,#106153,#106154,#106155,#106156,#106157,#106158,#106159,#106160,
#106161,#106162,#106163,#106164,#106165,#106166,#106167,#106168,#106169,
#106170,#106171,#106172,#106173,#106174,#106175,#106176,#106177,#106178,
#106179,#106180,#106181,#106182,#106183,#106184,#106185,#106186,#106187,
#106188,#106189,#106190,#106191,#106192,#106193,#106194,#106195,#106196,
#106197,#106198,#106199,#106200,#106201,#106202,#106203,#106204,#106205,
#106206,#106207,#106208,#106209,#106210,#106211,#106212,#106213,#106214,
#106215,#106216,#106217,#106218,#106219,#106220,#106221,#106222,#106223,
#106224,#106225,#106226,#106227,#106228,#106229,#106230,#106231,#106232,
#106233,#106234,#106235,#106236,#106237,#106238,#106239,#106240,#106241,
#106242,#106243,#106244,#106245,#106246,#106247,#106248,#106249,#106250,
#106251,#106252,#106253,#106254,#106255,#106256,#106257,#106258,#106259,
#106260,#106261,#106262,#106263,#106264,#106265,#106266,#106267,#106268,
#106269,#106270,#106271),.UNSPECIFIED.,.F.,.F.,(4,2,2,2,2,2,2,2,2,2,2,2,
2,2,2,2,2,2,2,2,2,2,2,2,2,2,2,2,2,2,2,2,2,2,2,2,2,2,2,2,2,2,2,2,2,2,2,2,
2,2,2,2,2,2,2,2,2,2,2,2,2,2,2,2,2,2,2,2,2,2,2,2,2,2,2,2,2,2,2,2,2,2,2,2,
2,2,2,2,2,2,2,2,2,4),(-2.0999861052273,-2.08479811344361,-2.08072130504199,
-2.07758229687025,-2.07447976083113,-2.07095046814617,-2.06517836607562,
-2.04122384415751,-2.01745915487528,-1.99960623806886,-1.99507973234757,
-1.99284046335875,-1.99103595124351,-1.98876877237535,-1.98409842203353,
-1.95299505284556,-1.91972780320091,-1.91339999589749,-1.90975309020251,
-1.90654219000092,-1.90250081158415,-1.89606440827894,-1.85879803922154,
-1.8324595733498,-1.82822129934136,-1.82603943778134,-1.8242325383008,-1.82189977284635,
-1.8170571352358,-1.79135334870695,-1.76511595349078,-1.75040359007509,
-1.74542112761741,-1.74205683803193,-1.73877385721018,-1.73478886659469,
-1.72488166282933,-1.68737042139817,-1.67201284469986,-1.66610457837662,
-1.6616795163636,-1.65946020386398,-1.65765522167537,-1.65536650363912,
-1.65058348758094,-1.6205343449857,-1.58619676800124,-1.57997261724512,
-1.57634752311013,-1.57313334449525,-1.56905744179811,-1.56250213901544,
-1.51862602993176,-1.50465899356999,-1.49647018029549,-1.49365587960851,
-1.49177716149441,-1.48982624360926,-1.48667353911659,-1.47632350257792,
-1.44407866758827,-1.42717771362486,-1.41953697949825,-1.41329945485087,
-1.40967146361122,-1.40645762206397,-1.40238608746289,-1.39584612765182,
-1.35189016674987,-1.33795594904815,-1.32977963593475,-1.32696683364986,
-1.32508837421632,-1.32313694257043,-1.31998207182596,-1.3096118970306,
-1.2773769983291,-1.2604835037349,-1.2492867578625,-1.24476216742133,-1.24148425132606,
-1.23846421036066,-1.23352724709438,-1.22038282572925,-1.18604888771317,
-1.17156359541554,-1.16317837008891,-1.16033989869803,-1.15845627809937,
-1.15651204009753,-1.15338998818168,-1.14332915741797,-1.11092203612512,
-1.1089889728157),.UNSPECIFIED.);
#2772=B_SPLINE_CURVE_WITH_KNOTS('',3,(#106277,#106278,#106279,#106280,#106281,
#106282,#106283,#106284,#106285,#106286,#106287,#106288,#106289,#106290,
#106291,#106292,#106293,#106294,#106295,#106296,#106297,#106298,#106299,
#106300,#106301,#106302,#106303,#106304,#106305,#106306,#106307,#106308,
#106309,#106310,#106311,#106312,#106313,#106314,#106315,#106316,#106317,
#106318,#106319,#106320,#106321,#106322,#106323,#106324,#106325,#106326,
#106327,#106328,#106329,#106330,#106331,#106332,#106333,#106334,#106335,
#106336,#106337,#106338,#106339,#106340,#106341,#106342,#106343,#106344,
#106345,#106346,#106347,#106348,#106349,#106350,#106351,#106352,#106353,
#106354,#106355,#106356,#106357,#106358,#106359,#106360,#106361,#106362,
#106363,#106364,#106365,#106366,#106367,#106368,#106369,#106370,#106371,
#106372,#106373,#106374,#106375,#106376,#106377,#106378,#106379,#106380,
#106381,#106382,#106383,#106384,#106385,#106386,#106387,#106388,#106389,
#106390,#106391,#106392,#106393,#106394,#106395,#106396,#106397,#106398,
#106399,#106400,#106401,#106402,#106403,#106404,#106405,#106406,#106407,
#106408,#106409,#106410,#106411,#106412,#106413,#106414,#106415,#106416,
#106417,#106418,#106419,#106420,#106421,#106422,#106423,#106424,#106425,
#106426,#106427,#106428,#106429,#106430,#106431,#106432,#106433,#106434,
#106435,#106436,#106437,#106438,#106439,#106440,#106441,#106442,#106443,
#106444,#106445,#106446,#106447,#106448,#106449,#106450,#106451,#106452,
#106453,#106454,#106455,#106456,#106457,#106458,#106459,#106460,#106461,
#106462,#106463,#106464,#106465,#106466,#106467,#106468,#106469,#106470,
#106471,#106472,#106473,#106474,#106475,#106476,#106477,#106478,#106479,
#106480),.UNSPECIFIED.,.F.,.F.,(4,2,2,2,2,2,2,2,2,2,2,2,2,2,2,2,2,2,2,2,
2,2,2,2,2,2,2,2,2,2,2,2,2,2,2,2,2,2,2,2,2,2,2,2,2,2,2,2,2,2,2,2,2,2,2,2,
2,2,2,2,2,2,2,2,2,2,2,2,2,2,2,2,2,2,2,2,2,2,2,2,2,2,2,2,2,2,2,2,2,2,2,2,
2,2,2,2,2,2,2,2,2,4),(-0.991072635368184,-0.969596543045493,-0.944678719631752,
-0.938779709992405,-0.935222573374277,-0.931992825682933,-0.927790031406633,
-0.918593737599609,-0.905823675865204,-0.883660390886621,-0.879534039801498,
-0.857384842615779,-0.853692572712348,-0.851602432914164,-0.849781689150038,
-0.847310277367632,-0.841503197222112,-0.832994434878307,-0.802838130039271,
-0.778027646791767,-0.772131961052143,-0.768575578377908,-0.765345723986346,
-0.761141655047993,-0.751937734662634,-0.739153003863647,-0.716995871741904,
-0.712801538341332,-0.690741174039202,-0.687049310762138,-0.684959288211624,
-0.683138565829683,-0.680667074960377,-0.674859332681809,-0.666349169592394,
-0.636180971994663,-0.61138537080215,-0.605490247999528,-0.601934032840117,
-0.598704221680831,-0.594500052655769,-0.58529524686925,-0.572508724189121,
-0.550352894801331,-0.546150634773762,-0.524101489984738,-0.520409744085937,
-0.518319774092841,-0.51649908756241,-0.514027632059696,-0.508219914290156,
-0.499709734140254,-0.46954062331062,-0.444747305679363,-0.438852359866513,
-0.435296230240233,-0.432066483322266,-0.427862378619087,-0.418657631417134,
-0.405871120740144,-0.383715857180284,-0.379512716851832,-0.357465336771777,
-0.353773672614241,-0.351683747207611,-0.349863098311555,-0.347391692278746,
-0.341584083637129,-0.333074056956888,-0.302905386541787,-0.278112799595176,
-0.272217983039022,-0.268661928804817,-0.265432248724814,-0.261228228676944,
-0.252023656825121,-0.239237381295077,-0.217082591459106,-0.19274122279055,
-0.187889351840766,-0.185554371677818,-0.183746838367228,-0.181565469863344,
-0.177331470787363,-0.15204128050393,-0.113463271695869,-0.107144754786843,
-0.103137247646399,-0.0999283891798736,-0.0962568557303748,-0.0898146312481536,
-0.0818500030684211,-0.0637876457998723,-0.0434746717486012,-0.0267336435729644,
-0.0214005665803968,-0.0190362204664168,-0.0172232234894831,-0.0155121948018241,
-0.0133884108843324,-0.00853636427515829,-0.000491426210657643),
 .UNSPECIFIED.);
#2773=B_SPLINE_CURVE_WITH_KNOTS('',3,(#106481,#106482,#106483,#106484,#106485,
#106486,#106487,#106488,#106489,#106490),.UNSPECIFIED.,.F.,.F.,(4,2,2,2,
4),(-2.10008367110316,-2.06877505387508,-2.05239041309396,-2.04489701650639,
-2.04104007014271),.UNSPECIFIED.);
#2774=B_SPLINE_CURVE_WITH_KNOTS('',3,(#106491,#106492,#106493,#106494,#106495,
#106496,#106497,#106498,#106499,#106500,#106501,#106502,#106503,#106504,
#106505,#106506,#106507,#106508,#106509,#106510,#106511,#106512,#106513,
#106514,#106515,#106516,#106517,#106518,#106519,#106520,#106521,#106522,
#106523,#106524,#106525,#106526,#106527,#106528,#106529,#106530,#106531,
#106532,#106533,#106534,#106535,#106536,#106537,#106538,#106539,#106540,
#106541,#106542,#106543,#106544,#106545,#106546,#106547,#106548,#106549,
#106550,#106551,#106552,#106553,#106554,#106555,#106556,#106557,#106558,
#106559,#106560,#106561,#106562,#106563,#106564,#106565,#106566,#106567,
#106568,#106569,#106570,#106571,#106572,#106573,#106574,#106575,#106576,
#106577,#106578,#106579,#106580,#106581,#106582,#106583,#106584,#106585,
#106586,#106587,#106588,#106589,#106590,#106591,#106592,#106593,#106594,
#106595,#106596,#106597,#106598,#106599,#106600,#106601,#106602,#106603,
#106604,#106605,#106606,#106607,#106608,#106609,#106610,#106611,#106612,
#106613,#106614,#106615,#106616,#106617,#106618,#106619,#106620,#106621,
#106622,#106623,#106624,#106625,#106626,#106627,#106628,#106629,#106630,
#106631,#106632,#106633,#106634,#106635,#106636,#106637,#106638,#106639,
#106640,#106641,#106642,#106643,#106644,#106645,#106646,#106647,#106648,
#106649,#106650,#106651,#106652,#106653,#106654,#106655,#106656,#106657,
#106658,#106659,#106660,#106661,#106662,#106663,#106664,#106665,#106666,
#106667,#106668,#106669,#106670,#106671,#106672,#106673,#106674,#106675,
#106676,#106677,#106678,#106679,#106680,#106681,#106682,#106683,#106684,
#106685,#106686,#106687,#106688,#106689,#106690,#106691,#106692,#106693,
#106694,#106695,#106696,#106697,#106698,#106699,#106700,#106701,#106702,
#106703,#106704,#106705,#106706),.UNSPECIFIED.,.F.,.F.,(4,2,2,2,2,2,2,2,
2,2,2,2,2,2,2,2,2,2,2,2,2,2,2,2,2,2,2,2,2,2,2,2,2,2,2,2,2,2,2,2,2,2,2,2,
2,2,2,2,2,2,2,2,2,2,2,2,2,2,2,2,2,2,2,2,2,2,2,2,2,2,2,2,2,2,2,2,2,2,2,2,
2,2,2,2,2,2,2,2,2,2,2,2,2,2,2,2,2,2,2,2,2,2,2,2,2,2,2,4),(-1.1089889728157,
-1.09390413199034,-1.08265173652397,-1.07811894729916,-1.07483967776895,
-1.07141429716938,-1.06613416749878,-1.04996520560814,-1.02124021050552,
-0.998263004278718,-0.994568306427569,-0.992478075489208,-0.990658204302517,
-0.988189336114603,-0.982394345455833,-0.973909108028063,-0.943933102140492,
-0.918914312155114,-0.913013794878952,-0.909457211950628,-0.906228921420988,
-0.902029428305775,-0.892846582087099,-0.880100909907931,-0.857930445448674,
-0.853947569498232,-0.831621684569698,-0.827929712876744,-0.825840117333333,
-0.824020151489138,-0.821550287698292,-0.815749145962188,-0.807251458413545,
-0.777176491751801,-0.752272965702892,-0.74637588459982,-0.742820078557052,
-0.739591674739637,-0.735390860198296,-0.726200131530252,-0.713439315930764,
-0.6912739573022,-0.687187080682848,-0.66498773275848,-0.661296298047347,
-0.659206848475852,-0.657386896882586,-0.654916901325263,-0.649114784964344,
-0.640615069012252,-0.610523300550814,-0.585640320492522,-0.579743953767783,
-0.576188346635443,-0.572959976771102,-0.568758996004514,-0.559567008353891,
-0.546803690778839,-0.52463971049363,-0.520536775452562,-0.498357893186431,
-0.494666607719804,-0.492577217418344,-0.490757299434606,-0.488287325375634,
-0.482485153348242,-0.473985259954077,-0.443891326351587,-0.419012054787095,
-0.41311590403831,-0.40956038996555,-0.406332081080179,-0.402131145921418,
-0.392939114469771,-0.380175615144535,-0.358012239679808,-0.35390686628024,
-0.331731579184435,-0.328040380915067,-0.325951036008301,-0.324131154733593,
-0.321661226706775,-0.31585914612673,-0.307359371626219,-0.277265617386782,
-0.252387358302804,-0.246491343327156,-0.242935905281727,-0.239707661728668,
-0.235506806278244,-0.226314926651039,-0.213551619119762,-0.191388721522952,
-0.167084329966978,-0.162128643290664,-0.159807694581368,-0.158001596142522,
-0.155810531906684,-0.151526082090662,-0.145862056975638,-0.131518121766425,
-0.0976949918441955,-0.0839718529526503,-0.0789592205958121,-0.0759258305504556,
-0.0726585305873539,-0.0681942348434812,-0.0594454739927945),
 .UNSPECIFIED.);
#2775=B_SPLINE_CURVE_WITH_KNOTS('',3,(#106711,#106712,#106713,#106714,#106715,
#106716,#106717,#106718,#106719,#106720,#106721,#106722,#106723,#106724,
#106725,#106726,#106727,#106728,#106729,#106730,#106731,#106732,#106733,
#106734,#106735,#106736,#106737,#106738,#106739,#106740,#106741,#106742,
#106743,#106744,#106745,#106746,#106747,#106748,#106749,#106750,#106751,
#106752,#106753,#106754,#106755,#106756,#106757,#106758,#106759,#106760,
#106761,#106762,#106763,#106764,#106765,#106766,#106767,#106768,#106769,
#106770,#106771,#106772,#106773,#106774,#106775,#106776,#106777,#106778,
#106779,#106780,#106781,#106782,#106783,#106784,#106785,#106786,#106787,
#106788,#106789,#106790,#106791,#106792,#106793,#106794,#106795,#106796,
#106797,#106798,#106799,#106800,#106801,#106802,#106803,#106804,#106805,
#106806,#106807,#106808,#106809,#106810,#106811,#106812,#106813,#106814,
#106815,#106816,#106817,#106818,#106819,#106820,#106821,#106822,#106823,
#106824,#106825,#106826,#106827,#106828,#106829,#106830,#106831,#106832,
#106833,#106834,#106835,#106836,#106837,#106838,#106839,#106840,#106841,
#106842,#106843,#106844,#106845,#106846,#106847,#106848,#106849,#106850,
#106851,#106852,#106853,#106854,#106855,#106856,#106857,#106858,#106859,
#106860,#106861,#106862,#106863,#106864,#106865,#106866,#106867,#106868,
#106869,#106870,#106871,#106872,#106873,#106874,#106875,#106876,#106877,
#106878,#106879,#106880,#106881,#106882,#106883,#106884,#106885,#106886,
#106887,#106888,#106889,#106890,#106891,#106892,#106893,#106894,#106895,
#106896,#106897,#106898,#106899,#106900,#106901,#106902,#106903,#106904,
#106905,#106906,#106907,#106908),.UNSPECIFIED.,.F.,.F.,(4,2,2,2,2,2,2,2,
2,2,2,2,2,2,2,2,2,2,2,2,2,2,2,2,2,2,2,2,2,2,2,2,2,2,2,2,2,2,2,2,2,2,2,2,
2,2,2,2,2,2,2,2,2,2,2,2,2,2,2,2,2,2,2,2,2,2,2,2,2,2,2,2,2,2,2,2,2,2,2,2,
2,2,2,2,2,2,2,2,2,2,2,2,2,2,2,2,2,2,4),(-2.04093771886338,-2.02934880549598,
-2.02208728420423,-2.01939460153838,-2.01753903188509,-2.01554880266114,
-2.01221744650086,-1.99999639770519,-1.97264867053721,-1.95406888501436,
-1.94596437990255,-1.93943534866577,-1.93574559522477,-1.93253853150594,
-1.92855634836747,-1.92232435336443,-1.87687277414369,-1.858814724624,-1.85426367841449,
-1.852019179815,-1.85021411053806,-1.8479507327422,-1.84330238579878,-1.8117269651815,
-1.77921103001925,-1.77270841521009,-1.76902409775747,-1.76581637920758,
-1.76182637916616,-1.75379651199526,-1.70985147132532,-1.692063355684,-1.6875437850885,
-1.68530540896126,-1.68350022696993,-1.68123038059221,-1.67654859845027,
-1.64560421939891,-1.61181826504183,-1.60569498564409,-1.60209046598481,
-1.59887144737075,-1.59475764912396,-1.58807322779605,-1.54327776624413,
-1.52537337940295,-1.52084010980807,-1.51859901171743,-1.51679381025957,
-1.51452666899179,-1.50985916867113,-1.47869032466852,-1.44518440640319,
-1.43901777186325,-1.43540400857167,-1.43218654237743,-1.42808820227649,
-1.42145778039966,-1.3879596731307,-1.36671281712231,-1.35957386728726,
-1.35447057091157,-1.35212188061865,-1.3504853011976,-1.348389114066,-1.34466952444868,
-1.32003753521421,-1.30210209767399,-1.28588654130804,-1.27499766230629,
-1.27051871073989,-1.26724780750002,-1.26380366587999,-1.25843743789684,
-1.24145938424182,-1.20379992283226,-1.18998986735269,-1.18665622691549,
-1.18466533684014,-1.18283105292315,-1.1801557120098,-1.17350603734251,
-1.14182623222866,-1.11243487352282,-1.10595171469238,-1.10227130429957,
-1.09906293989677,-1.09506685072939,-1.08878828639482,-1.04984422968113,
-1.04683086993838,-1.0240357954697,-1.0203409895536,-1.01825025635086,-1.01642959739132,
-1.01395910600654,-1.0081577327812,-0.999660533259873,-0.991072635368184),
 .UNSPECIFIED.);
#2776=B_SPLINE_CURVE_WITH_KNOTS('',3,(#106910,#106911,#106912,#106913,#106914,
#106915,#106916,#106917,#106918,#106919),.UNSPECIFIED.,.F.,.F.,(4,2,2,2,
4),(-0.0594454739927945,-0.0573927227399692,-0.0413658239800665,-0.0230003290355216,
-0.000492308750634391),.UNSPECIFIED.);
#2777=B_SPLINE_CURVE_WITH_KNOTS('',3,(#106920,#106921,#106922,#106923,#106924,
#106925,#106926,#106927,#106928,#106929,#106930,#106931,#106932,#106933,
#106934,#106935,#106936,#106937,#106938,#106939,#106940,#106941,#106942,
#106943,#106944,#106945,#106946,#106947,#106948,#106949,#106950,#106951,
#106952,#106953,#106954,#106955,#106956,#106957,#106958,#106959,#106960,
#106961,#106962,#106963,#106964,#106965,#106966,#106967,#106968,#106969,
#106970,#106971,#106972,#106973,#106974,#106975,#106976,#106977,#106978,
#106979,#106980,#106981,#106982,#106983,#106984,#106985,#106986,#106987,
#106988,#106989,#106990,#106991,#106992,#106993,#106994,#106995,#106996,
#106997,#106998,#106999,#107000,#107001,#107002,#107003,#107004,#107005,
#107006,#107007,#107008,#107009,#107010,#107011,#107012,#107013,#107014,
#107015,#107016,#107017,#107018,#107019,#107020,#107021,#107022,#107023,
#107024,#107025,#107026,#107027,#107028,#107029,#107030,#107031,#107032,
#107033,#107034,#107035,#107036,#107037,#107038,#107039,#107040,#107041,
#107042,#107043,#107044,#107045,#107046,#107047,#107048,#107049,#107050,
#107051,#107052,#107053,#107054,#107055,#107056,#107057,#107058,#107059,
#107060,#107061,#107062,#107063,#107064,#107065,#107066,#107067,#107068,
#107069,#107070,#107071,#107072,#107073,#107074,#107075,#107076,#107077,
#107078,#107079,#107080,#107081,#107082,#107083,#107084,#107085,#107086,
#107087,#107088,#107089,#107090,#107091,#107092,#107093,#107094,#107095,
#107096,#107097,#107098,#107099,#107100,#107101,#107102,#107103,#107104,
#107105,#107106,#107107,#107108,#107109,#107110,#107111,#107112,#107113,
#107114,#107115),.UNSPECIFIED.,.F.,.F.,(4,2,2,2,2,2,2,2,2,2,2,2,2,2,2,2,
2,2,2,2,2,2,2,2,2,2,2,2,2,2,2,2,2,2,2,2,2,2,2,2,2,2,2,2,2,2,2,2,2,2,2,2,
2,2,2,2,2,2,2,2,2,2,2,2,2,2,2,2,2,2,2,2,2,2,2,2,2,2,2,2,2,2,2,2,2,2,2,2,
2,2,2,2,2,2,2,2,2,4),(-2.0999332011157,-2.09739257213916,-2.09498989078277,
-2.09312545477489,-2.09142054753589,-2.08945798611463,-2.08625190489876,
-2.07532885103696,-2.05324117035067,-2.01909304476526,-2.01291996774835,
-2.00930561995666,-2.00608958104554,-2.00199576136644,-1.9953785284513,
-1.96145632974956,-1.9322235428279,-1.92791495351409,-1.92571887553611,
-1.92391285774309,-1.92159736719967,-1.91667193680883,-1.89231320551945,
-1.87013520243629,-1.8573569327959,-1.84815782576031,-1.84395542035515,
-1.84072671060947,-1.83717148603319,-1.8312775229547,-1.8064582405382,-1.77633810170779,
-1.76783624896193,-1.76203250133046,-1.75956217786685,-1.7577420982829,
-1.7556526826346,-1.75196161597438,-1.73007499878915,-1.7258976861844,-1.70327904647239,
-1.6906224535315,-1.68148718866209,-1.67729594969833,-1.67406867142039,
-1.6705078630853,-1.6645875407792,-1.63871671453179,-1.60950030599841,-1.60111475018943,
-1.59536891312331,-1.59290828673919,-1.59108942246822,-1.58899447782239,
-1.58527863890755,-1.56075626580516,-1.54281501020186,-1.52653120562676,
-1.51561153054425,-1.51112874037027,-1.5078580121975,-1.50482851831038,
-1.49983880987619,-1.48629841320236,-1.45232893461133,-1.43794613501771,
-1.43227234129906,-1.42798177683983,-1.42578931697462,-1.42398307511072,
-1.4216632082487,-1.41671428804292,-1.39165550396451,-1.36500095017407,
-1.35016065053659,-1.34516366344477,-1.34179638079056,-1.3385156210613,
-1.3345396637354,-1.32676441568341,-1.28361005229642,-1.27058873479754,
-1.26277026407991,-1.26000299063039,-1.25813353583669,-1.25641064298414,
-1.2534354337856,-1.24464497765278,-1.21148405375483,-1.19395537315626,
-1.18247674363694,-1.17791061589915,-1.17462545041544,-1.17161433286871,
-1.1667274068165,-1.15394354632791,-1.11927429955175,-1.10920668715445),
 .UNSPECIFIED.);
#2778=B_SPLINE_CURVE_WITH_KNOTS('',3,(#107121,#107122,#107123,#107124,#107125,
#107126,#107127,#107128,#107129,#107130,#107131,#107132,#107133,#107134,
#107135,#107136,#107137,#107138,#107139,#107140,#107141,#107142,#107143,
#107144,#107145,#107146,#107147,#107148,#107149,#107150,#107151,#107152,
#107153,#107154,#107155,#107156,#107157,#107158,#107159,#107160,#107161,
#107162,#107163,#107164,#107165,#107166,#107167,#107168,#107169,#107170,
#107171,#107172,#107173,#107174,#107175,#107176,#107177,#107178,#107179,
#107180,#107181,#107182,#107183,#107184,#107185,#107186,#107187,#107188,
#107189,#107190,#107191,#107192,#107193,#107194,#107195,#107196,#107197,
#107198,#107199,#107200,#107201,#107202,#107203,#107204,#107205,#107206,
#107207,#107208,#107209,#107210,#107211,#107212,#107213,#107214,#107215,
#107216,#107217,#107218,#107219,#107220,#107221,#107222,#107223,#107224,
#107225,#107226,#107227,#107228,#107229,#107230,#107231,#107232,#107233,
#107234,#107235,#107236,#107237,#107238,#107239,#107240,#107241,#107242,
#107243,#107244,#107245,#107246,#107247,#107248,#107249,#107250,#107251,
#107252,#107253,#107254,#107255,#107256,#107257,#107258,#107259,#107260,
#107261,#107262,#107263,#107264,#107265,#107266,#107267,#107268,#107269,
#107270,#107271,#107272,#107273,#107274,#107275,#107276,#107277,#107278,
#107279,#107280,#107281,#107282,#107283,#107284,#107285,#107286,#107287,
#107288,#107289,#107290,#107291,#107292,#107293,#107294,#107295,#107296,
#107297,#107298,#107299,#107300,#107301,#107302,#107303,#107304),
 .UNSPECIFIED.,.F.,.F.,(4,2,2,2,2,2,2,2,2,2,2,2,2,2,2,2,2,2,2,2,2,2,2,2,
2,2,2,2,2,2,2,2,2,2,2,2,2,2,2,2,2,2,2,2,2,2,2,2,2,2,2,2,2,2,2,2,2,2,2,2,
2,2,2,2,2,2,2,2,2,2,2,2,2,2,2,2,2,2,2,2,2,2,2,2,2,2,2,2,2,2,2,4),(-0.991330164355917,
-0.990766673158264,-0.959591636185856,-0.925979033127857,-0.921500948499669,
-0.919270680392501,-0.917465297118865,-0.915186703690311,-0.910459471075429,
-0.890836516252776,-0.856260979658556,-0.843351122288363,-0.83844554343868,
-0.835430412585874,-0.832146711864749,-0.827593431388309,-0.816208070289606,
-0.798894632841549,-0.766094469815978,-0.756774845606066,-0.753735485512362,
-0.751999734313239,-0.750139600382626,-0.747423060730761,-0.739989739037843,
-0.727909772889895,-0.692422293359357,-0.677270997051221,-0.672099599596438,
-0.66869598311718,-0.665401620099456,-0.66078822864453,-0.648986548240062,
-0.630713966697872,-0.604142184920789,-0.590846857313886,-0.587436936983213,
-0.585429456181567,-0.58358195392054,-0.580934936181083,-0.573996687579575,
-0.534763104895739,-0.511901266438737,-0.506090472113298,-0.50255235059563,
-0.499317956599565,-0.495077316434386,-0.485660193901215,-0.441152234568637,
-0.424501457388614,-0.420892603736543,-0.418841993136153,-0.417010739822306,
-0.414463475561524,-0.408187368209675,-0.39871031712467,-0.359075980765575,
-0.343908557072825,-0.33873560008038,-0.335331731704337,-0.332037698399195,
-0.327425728979654,-0.315633435910989,-0.297382590401466,-0.270867039032409,
-0.25749308392221,-0.254078082402757,-0.252069533138092,-0.250222590701594,
-0.247578545543798,-0.240660485235741,-0.196897818160312,-0.178027596320046,
-0.172473276582961,-0.168989755030561,-0.165737165851204,-0.161369754541182,
-0.151189044584545,-0.136469210954872,-0.106935850396378,-0.0910898619089166,
-0.0875346131291738,-0.0854957609543481,-0.0836610100241452,-0.0810895833329044,
-0.0746565105184794,-0.064844202217108,-0.0421401538965219,-0.0122237431867097,
-0.00636347452454314,-0.00292195652754838,-0.000491893798650521),
 .UNSPECIFIED.);
#2779=B_SPLINE_CURVE_WITH_KNOTS('',3,(#107305,#107306,#107307,#107308,#107309,
#107310,#107311,#107312,#107313,#107314,#107315,#107316),.UNSPECIFIED.,
 .F.,.F.,(4,2,2,2,2,4),(-2.09986416909328,-2.09704942948014,-2.09234257063096,
-2.07828695470315,-2.04102086288901,-2.04093771886338),.UNSPECIFIED.);
#2780=B_SPLINE_CURVE_WITH_KNOTS('',3,(#107317,#107318,#107319,#107320,#107321,
#107322,#107323,#107324,#107325,#107326,#107327,#107328,#107329,#107330,
#107331,#107332,#107333,#107334,#107335,#107336,#107337,#107338,#107339,
#107340,#107341,#107342,#107343,#107344,#107345,#107346,#107347,#107348,
#107349,#107350,#107351,#107352,#107353,#107354,#107355,#107356,#107357,
#107358,#107359,#107360,#107361,#107362,#107363,#107364,#107365,#107366,
#107367,#107368,#107369,#107370,#107371,#107372,#107373,#107374,#107375,
#107376,#107377,#107378,#107379,#107380,#107381,#107382,#107383,#107384,
#107385,#107386,#107387,#107388,#107389,#107390,#107391,#107392,#107393,
#107394,#107395,#107396,#107397,#107398,#107399,#107400,#107401,#107402,
#107403,#107404,#107405,#107406,#107407,#107408,#107409,#107410,#107411,
#107412,#107413,#107414,#107415,#107416,#107417,#107418,#107419,#107420,
#107421,#107422,#107423,#107424,#107425,#107426,#107427,#107428,#107429,
#107430,#107431,#107432,#107433,#107434,#107435,#107436,#107437,#107438,
#107439,#107440,#107441,#107442,#107443,#107444,#107445,#107446,#107447,
#107448,#107449,#107450,#107451,#107452,#107453,#107454,#107455,#107456,
#107457,#107458,#107459,#107460,#107461,#107462,#107463,#107464,#107465,
#107466,#107467,#107468,#107469,#107470,#107471,#107472,#107473,#107474,
#107475,#107476,#107477,#107478,#107479,#107480,#107481,#107482,#107483,
#107484,#107485,#107486,#107487,#107488,#107489,#107490,#107491,#107492,
#107493,#107494,#107495,#107496,#107497,#107498,#107499,#107500,#107501,
#107502,#107503,#107504,#107505,#107506,#107507,#107508,#107509,#107510,
#107511,#107512,#107513,#107514,#107515,#107516),.UNSPECIFIED.,.F.,.F.,
(4,2,2,2,2,2,2,2,2,2,2,2,2,2,2,2,2,2,2,2,2,2,2,2,2,2,2,2,2,2,2,2,2,2,2,
2,2,2,2,2,2,2,2,2,2,2,2,2,2,2,2,2,2,2,2,2,2,2,2,2,2,2,2,2,2,2,2,2,2,2,2,
2,2,2,2,2,2,2,2,2,2,2,2,2,2,2,2,2,2,2,2,2,2,2,2,2,2,2,2,4),(-1.10920668715445,
-1.0996208901351,-1.09489094482217,-1.09261228347598,-1.09080749542534,
-1.08857885286122,-1.08410677844814,-1.05041616918713,-1.02139402565753,
-1.01465732244867,-1.01052920981668,-1.00730947983556,-1.00371501157452,
-0.997635836565699,-0.963375204078934,-0.93293484609209,-0.928205233836145,
-0.925926673263352,-0.92412193484134,-0.921893316214902,-0.91742117838395,
-0.911429462598563,-0.895715643008634,-0.856865639577424,-0.848010232232837,
-0.843868615178909,-0.840647407737652,-0.837060572532154,-0.831017203768369,
-0.823681911626312,-0.807834520690982,-0.79509607326041,-0.766424290357316,
-0.761603593758634,-0.7593078388466,-0.757502742922307,-0.755289986964268,
-0.750897506396175,-0.721124777032205,-0.687884599740569,-0.681246898014919,
-0.677147393987621,-0.673931008264072,-0.670320567965648,-0.664164974236288,
-0.630349770704053,-0.599552372370897,-0.594862189026562,-0.592591300529295,
-0.590786864391447,-0.588551451550751,-0.584044123259823,-0.548497466815328,
-0.521257443239317,-0.514596958620304,-0.51049097885111,-0.507274007092641,
-0.503667582783319,-0.497530589476048,-0.463714253489563,-0.432881191133514,
-0.428194387216505,-0.425924194315586,-0.424119829481707,-0.421883907545715,
-0.417373747266782,-0.411314614179666,-0.395307361004748,-0.355298314354327,
-0.347564513551573,-0.343582449680913,-0.340376568042505,-0.336689399422382,
-0.330168327408791,-0.322076682893815,-0.303541812768545,-0.276297384622105,
-0.263964430063889,-0.260625139999804,-0.258633686713554,-0.256779967352318,
-0.254094280815001,-0.246878396123331,-0.235310453118137,-0.214100216860016,
-0.185482989472097,-0.179517064827112,-0.175946926720627,-0.172722520394608,
-0.168551098522937,-0.159526083262268,-0.114639209580094,-0.0978078882512786,
-0.0941910559951095,-0.0921392492594382,-0.0903094205536025,-0.0877676294695378,
-0.0815223303886219,-0.0721091902688607,-0.0594666017457383),
 .UNSPECIFIED.);
#2781=B_SPLINE_CURVE_WITH_KNOTS('',3,(#107521,#107522,#107523,#107524,#107525,
#107526,#107527,#107528,#107529,#107530,#107531,#107532,#107533,#107534,
#107535,#107536,#107537,#107538,#107539,#107540,#107541,#107542,#107543,
#107544,#107545,#107546,#107547,#107548,#107549,#107550,#107551,#107552,
#107553,#107554,#107555,#107556,#107557,#107558,#107559,#107560,#107561,
#107562,#107563,#107564,#107565,#107566,#107567,#107568,#107569,#107570,
#107571,#107572,#107573,#107574,#107575,#107576,#107577,#107578,#107579,
#107580,#107581,#107582,#107583,#107584,#107585,#107586,#107587,#107588,
#107589,#107590,#107591,#107592,#107593,#107594,#107595,#107596,#107597,
#107598,#107599,#107600,#107601,#107602,#107603,#107604,#107605,#107606,
#107607,#107608,#107609,#107610,#107611,#107612,#107613,#107614,#107615,
#107616,#107617,#107618,#107619,#107620,#107621,#107622,#107623,#107624,
#107625,#107626,#107627,#107628,#107629,#107630,#107631,#107632,#107633,
#107634,#107635,#107636,#107637,#107638,#107639,#107640,#107641,#107642,
#107643,#107644,#107645,#107646,#107647,#107648,#107649,#107650,#107651,
#107652,#107653,#107654,#107655,#107656,#107657,#107658,#107659,#107660,
#107661,#107662,#107663,#107664,#107665,#107666,#107667,#107668,#107669,
#107670,#107671,#107672,#107673,#107674,#107675,#107676,#107677,#107678,
#107679,#107680,#107681,#107682,#107683,#107684,#107685,#107686,#107687,
#107688,#107689,#107690,#107691,#107692,#107693,#107694,#107695,#107696,
#107697,#107698,#107699,#107700,#107701,#107702,#107703,#107704,#107705,
#107706,#107707,#107708,#107709,#107710,#107711,#107712,#107713,#107714,
#107715,#107716,#107717,#107718),.UNSPECIFIED.,.F.,.F.,(4,2,2,2,2,2,2,2,
2,2,2,2,2,2,2,2,2,2,2,2,2,2,2,2,2,2,2,2,2,2,2,2,2,2,2,2,2,2,2,2,2,2,2,2,
2,2,2,2,2,2,2,2,2,2,2,2,2,2,2,2,2,2,2,2,2,2,2,2,2,2,2,2,2,2,2,2,2,2,2,2,
2,2,2,2,2,2,2,2,2,2,2,2,2,2,2,2,2,2,4),(-2.0412420799731,-2.04034028984006,
-2.02158199735914,-2.00957594468979,-2.00493359672236,-2.00163391631721,
-1.99863650512635,-1.99460071303198,-1.98448875220065,-1.94722404217195,
-1.93193304781641,-1.9260399202716,-1.92162316274255,-1.91940498657613,
-1.91759923076491,-1.91530729835558,-1.91051003425248,-1.88146752229286,
-1.84673917232611,-1.84018223804752,-1.83648641450168,-1.83327953241321,
-1.82930464138898,-1.82309820286662,-1.77751834262795,-1.7595199556566,
-1.75497558586645,-1.75273224635372,-1.75092697206141,-1.74866191211158,
-1.74400559751323,-1.71259623433521,-1.67981225399705,-1.67336865881302,
-1.66969644353272,-1.66648706129433,-1.66247899304551,-1.65435520769229,
-1.61470143687081,-1.59878745547793,-1.59274894142858,-1.58824956964224,
-1.58601505429387,-1.5842096706824,-1.58193540040753,-1.5772311046547,-1.54652905447861,
-1.51275274146498,-1.50650813211005,-1.50287778022188,-1.49966286065376,
-1.49559129860902,-1.487127133432,-1.44786181710417,-1.43204628652902,-1.42317663268646,
-1.42028021952343,-1.41838413325667,-1.41645378952942,-1.41339772770353,
-1.40393557935066,-1.37118077950192,-1.35392191498966,-1.34256148238213,
-1.33801171939212,-1.33472855794252,-1.33171257327552,-1.32680247897091,
-1.31386029331505,-1.27933837199892,-1.26480101608667,-1.25639572777873,
-1.25355421855214,-1.25166952241778,-1.24996145219351,-1.24706530673577,
-1.23889475695405,-1.20533945783425,-1.18756518601257,-1.1796791906009,
-1.17328659578504,-1.16962515881791,-1.1664146460508,-1.16239122297399,
-1.15601930283333,-1.11801032093176,-1.09228266080915,-1.08804663163659,
-1.0858647006441,-1.08405699639688,-1.0817221501291,-1.07687173054787,-1.05042524709968,
-1.01446375046852,-1.0079305684096,-1.00386026813836,-1.000645543293,-0.997014566849272,
-0.991330164355917),.UNSPECIFIED.);
#2782=B_SPLINE_CURVE_WITH_KNOTS('',3,(#107720,#107721,#107722,#107723,#107724,
#107725,#107726,#107727,#107728,#107729,#107730,#107731,#107732,#107733,
#107734,#107735),.UNSPECIFIED.,.F.,.F.,(4,2,2,2,2,2,2,4),(-0.0594666017457383,
-0.032621887068177,-0.0172456592650443,-0.012157102551331,-0.008731466438282,
-0.0056783971083446,-0.00301214739693347,-0.000491717955116048),
 .UNSPECIFIED.);
#2783=B_SPLINE_CURVE_WITH_KNOTS('',3,(#107736,#107737,#107738,#107739,#107740,
#107741,#107742,#107743,#107744,#107745,#107746,#107747,#107748,#107749,
#107750,#107751,#107752,#107753,#107754,#107755,#107756,#107757,#107758,
#107759,#107760,#107761,#107762,#107763,#107764,#107765,#107766,#107767,
#107768,#107769,#107770,#107771,#107772,#107773,#107774,#107775,#107776,
#107777,#107778,#107779,#107780,#107781,#107782,#107783,#107784,#107785,
#107786,#107787,#107788,#107789,#107790,#107791,#107792,#107793,#107794,
#107795,#107796,#107797,#107798,#107799,#107800,#107801,#107802,#107803,
#107804,#107805,#107806,#107807,#107808,#107809,#107810,#107811,#107812,
#107813,#107814,#107815,#107816,#107817,#107818,#107819,#107820,#107821,
#107822,#107823,#107824,#107825,#107826,#107827,#107828,#107829,#107830,
#107831,#107832,#107833,#107834,#107835,#107836,#107837,#107838,#107839,
#107840,#107841,#107842,#107843,#107844,#107845,#107846,#107847,#107848,
#107849,#107850,#107851,#107852,#107853,#107854,#107855,#107856,#107857,
#107858,#107859,#107860,#107861,#107862,#107863,#107864,#107865,#107866,
#107867,#107868,#107869,#107870,#107871,#107872,#107873,#107874,#107875,
#107876,#107877,#107878,#107879,#107880,#107881,#107882,#107883,#107884,
#107885,#107886,#107887,#107888,#107889,#107890,#107891,#107892,#107893,
#107894,#107895,#107896,#107897,#107898,#107899,#107900,#107901,#107902,
#107903,#107904,#107905,#107906,#107907,#107908,#107909,#107910,#107911,
#107912,#107913,#107914,#107915,#107916,#107917,#107918,#107919,#107920,
#107921,#107922,#107923,#107924,#107925,#107926,#107927,#107928,#107929,
#107930,#107931,#107932,#107933),.UNSPECIFIED.,.F.,.F.,(4,2,2,2,2,2,2,2,
2,2,2,2,2,2,2,2,2,2,2,2,2,2,2,2,2,2,2,2,2,2,2,2,2,2,2,2,2,2,2,2,2,2,2,2,
2,2,2,2,2,2,2,2,2,2,2,2,2,2,2,2,2,2,2,2,2,2,2,2,2,2,2,2,2,2,2,2,2,2,2,2,
2,2,2,2,2,2,2,2,2,2,2,2,2,2,2,2,2,2,4),(-2.09987818931514,-2.09265685916745,
-2.04920876173439,-2.03648785482216,-2.02879046050777,-2.02603905676681,
-2.02417269259838,-2.02244616551281,-2.019452239282,-2.01050935080262,-1.9774428436789,
-1.95997517026093,-1.95217475319003,-1.94758124349242,-1.94338415960361,
-1.94015612592297,-1.9365982335642,-1.93069171455341,-1.90585709216354,
-1.87576930286984,-1.86727153065022,-1.86146980714479,-1.85899981872863,
-1.85717977494456,-1.85509014713664,-1.85139817990397,-1.82928256869064,
-1.82510347560292,-1.80292379079051,-1.79015128634646,-1.78095521137088,
-1.77675333815717,-1.77352469905287,-1.76996921381308,-1.76407401157867,
-1.73921302722891,-1.7091295051988,-1.70063230028604,-1.69483086794757,
-1.69236093685382,-1.69054092080869,-1.68845132825768,-1.68475936950186,
-1.66262952579751,-1.65846163420306,-1.63628113390123,-1.62351070725589,
-1.61431575741793,-1.61011414106341,-1.60688560092258,-1.60333012823298,
-1.59743472210822,-1.57256366448291,-1.54248915881248,-1.53399315068875,
-1.5281923400351,-1.52572254473798,-1.52390257009703,-1.52181294613885,
-1.5181208168879,-1.49594210025623,-1.49181276074532,-1.4696297562061,-1.45686643453461,
-1.44767518629898,-1.44347420405053,-1.44024573278455,-1.43668991729546,
-1.43079294299026,-1.40586805919897,-1.37584136231047,-1.36735140769438,
-1.36155358860689,-1.35908426598509,-1.35726429563889,-1.35517421925982,
-1.35148042744211,-1.32885913541171,-1.31192821630655,-1.29380910736794,
-1.2820746357516,-1.27747158899413,-1.27417983369694,-1.27117617106732,
-1.26711146923517,-1.2568150911615,-1.21602760324243,-1.20327728745127,
-1.19556800697994,-1.19281505441106,-1.19094842809758,-1.18897931324107,
-1.18574278720833,-1.17450551448091,-1.14643858817064,-1.12756418754894,
-1.11938163011068,-1.11280441351441,-1.10915669663231),.UNSPECIFIED.);
#2784=B_SPLINE_CURVE_WITH_KNOTS('',3,(#107939,#107940,#107941,#107942,#107943,
#107944,#107945,#107946,#107947,#107948,#107949,#107950,#107951,#107952,
#107953,#107954,#107955,#107956,#107957,#107958),.UNSPECIFIED.,.F.,.F.,
(4,2,2,2,2,2,2,2,2,4),(-0.0592977063510342,-0.0406565713569759,-0.0296459142995207,
-0.0264393932675981,-0.0244829701643915,-0.0227840180597207,-0.0209206230480024,
-0.0183407941751122,-0.012273668438799,-0.000511201039480913),
 .UNSPECIFIED.);
#2785=B_SPLINE_CURVE_WITH_KNOTS('',3,(#107960,#107961,#107962,#107963,#107964,
#107965,#107966,#107967,#107968,#107969,#107970,#107971,#107972,#107973,
#107974,#107975,#107976,#107977,#107978,#107979,#107980,#107981,#107982,
#107983,#107984,#107985,#107986,#107987,#107988,#107989,#107990,#107991,
#107992,#107993,#107994,#107995,#107996,#107997,#107998,#107999,#108000,
#108001,#108002,#108003,#108004,#108005,#108006,#108007,#108008,#108009,
#108010,#108011,#108012,#108013,#108014,#108015,#108016,#108017,#108018,
#108019,#108020,#108021,#108022,#108023,#108024,#108025,#108026,#108027,
#108028,#108029,#108030,#108031,#108032,#108033,#108034,#108035,#108036,
#108037,#108038,#108039,#108040,#108041,#108042,#108043,#108044,#108045,
#108046,#108047,#108048,#108049,#108050,#108051,#108052,#108053,#108054,
#108055,#108056,#108057,#108058,#108059,#108060,#108061,#108062,#108063,
#108064,#108065,#108066,#108067,#108068),.UNSPECIFIED.,.F.,.F.,(4,3,3,3,
3,3,3,3,3,3,3,3,3,3,3,3,3,3,3,3,3,3,3,3,3,3,3,3,3,3,3,3,3,3,3,3,4),(-3.84638326322104,
-3.73817304644031,-3.63008307635761,-3.52207051640325,-3.41409265085555,
-3.30603153247512,-3.19793262975346,-3.08963570929982,-2.99264357503826,
-2.88276576904152,-2.77180701249785,-2.6622259577447,-2.55271003115832,
-2.44321871026559,-2.33118796187223,-2.22155393901983,-2.108324827856,-1.99509571669217,
-1.88634917197483,-1.77524900777124,-1.66680167782881,-1.55841756692922,
-1.45005450048505,-1.33692783995031,-1.22840073648774,-1.11978586886727,
-1.01096961743765,-0.997547858346085,-0.884786118899249,-0.772265208178043,
-0.659886256614288,-0.547615706777961,-0.43542015049968,-0.323231033746395,
-0.211055181000669,-0.0987911575872374,0.),.UNSPECIFIED.);
#2786=B_SPLINE_CURVE_WITH_KNOTS('',3,(#108071,#108072,#108073,#108074,#108075,
#108076,#108077,#108078,#108079,#108080,#108081,#108082,#108083,#108084,
#108085,#108086,#108087,#108088,#108089,#108090,#108091,#108092,#108093,
#108094,#108095,#108096,#108097,#108098,#108099,#108100,#108101,#108102,
#108103,#108104,#108105,#108106,#108107,#108108,#108109,#108110,#108111,
#108112,#108113,#108114,#108115,#108116,#108117,#108118,#108119,#108120,
#108121,#108122,#108123,#108124,#108125,#108126,#108127,#108128,#108129,
#108130,#108131,#108132,#108133,#108134,#108135,#108136,#108137,#108138,
#108139,#108140,#108141,#108142,#108143,#108144,#108145,#108146,#108147,
#108148,#108149,#108150,#108151,#108152,#108153,#108154,#108155,#108156,
#108157,#108158,#108159,#108160,#108161,#108162,#108163,#108164,#108165,
#108166,#108167,#108168,#108169,#108170,#108171,#108172,#108173,#108174,
#108175,#108176,#108177,#108178,#108179,#108180,#108181,#108182,#108183,
#108184,#108185,#108186,#108187,#108188,#108189,#108190,#108191,#108192,
#108193,#108194,#108195,#108196,#108197,#108198,#108199,#108200,#108201,
#108202,#108203,#108204,#108205,#108206,#108207,#108208,#108209,#108210,
#108211,#108212,#108213,#108214,#108215,#108216,#108217,#108218,#108219,
#108220,#108221,#108222,#108223,#108224,#108225,#108226,#108227,#108228,
#108229,#108230,#108231,#108232,#108233,#108234,#108235,#108236,#108237,
#108238,#108239,#108240,#108241,#108242,#108243,#108244,#108245,#108246,
#108247,#108248,#108249,#108250),.UNSPECIFIED.,.F.,.F.,(4,2,2,2,2,2,2,2,
2,2,2,2,2,2,2,2,2,2,2,2,2,2,2,2,2,2,2,2,2,2,2,2,2,2,2,2,2,2,2,2,2,2,2,2,
2,2,2,2,2,2,2,2,2,2,2,2,2,2,2,2,2,2,2,2,2,2,2,2,2,2,2,2,2,2,2,2,2,2,2,2,
2,2,2,2,2,2,2,2,2,4),(-1.9798082478801,-1.97972857885761,-1.97636370684344,
-1.93875794853755,-1.92034230820633,-1.90842989899881,-1.90376413773363,
-1.900427415003,-1.89697415830706,-1.89171126908936,-1.8759895379423,-1.84031468570726,
-1.82499010409875,-1.82151830834034,-1.81946738308023,-1.81761159279483,
-1.8153496532383,-1.81090414679126,-1.78707124954771,-1.76439509235973,
-1.75172599216021,-1.74257924009979,-1.7383717667015,-1.73512660116134,
-1.73154013228812,-1.72556177893816,-1.69808723799443,-1.67004433406912,
-1.65781653480299,-1.65459244300484,-1.6526222427315,-1.65078120674275,
-1.64804459181953,-1.64097352945887,-1.60966033578755,-1.58067315828821,
-1.57409363647062,-1.57040718173468,-1.56722144981701,-1.56329026534161,
-1.55718906344407,-1.51650588498505,-1.49271417254024,-1.48844567288275,
-1.48626659336839,-1.48446520562592,-1.48214832529626,-1.47721925534661,
-1.45363371065508,-1.43337047940566,-1.41901690938295,-1.40901067535155,
-1.40466598470465,-1.40141121869766,-1.3979070732372,-1.39227857560915,
-1.3724240621606,-1.33789274299452,-1.32453323833562,-1.32122410181192,
-1.31923432254535,-1.31739280198788,-1.31512089888867,-1.30949427575413,
-1.27689820567008,-1.25112716224158,-1.24212609660851,-1.23795630698055,
-1.23472924745761,-1.23115214436295,-1.22516464537184,-1.19608432621958,
-1.16951459537087,-1.15761641614849,-1.15442448805689,-1.15246445640105,
-1.15061397541791,-1.1478474270415,-1.14061619101804,-1.10944393232432,
-1.08438063722298,-1.0753951491831,-1.07123121727475,-1.06800835004163,
-1.06443566654792,-1.05845531946044,-1.02913335488853,-1.00714774457551,
-0.991411872917561,-0.991403523612787),.UNSPECIFIED.);
#2787=B_SPLINE_CURVE_WITH_KNOTS('',3,(#108256,#108257,#108258,#108259,#108260,
#108261,#108262,#108263,#108264,#108265,#108266,#108267,#108268,#108269,
#108270,#108271,#108272,#108273,#108274,#108275,#108276,#108277,#108278,
#108279,#108280,#108281,#108282,#108283,#108284,#108285,#108286,#108287,
#108288,#108289,#108290,#108291,#108292,#108293,#108294,#108295,#108296,
#108297,#108298,#108299,#108300,#108301,#108302,#108303,#108304,#108305,
#108306,#108307,#108308,#108309,#108310,#108311,#108312,#108313,#108314,
#108315,#108316,#108317,#108318,#108319),.UNSPECIFIED.,.F.,.F.,(4,3,3,3,
3,3,3,3,3,3,3,3,3,3,3,3,3,3,3,3,3,4),(89.6265204120243,89.7423236955964,
89.7793072511478,89.8880549678023,89.9991549855138,90.1076034906654,90.2159887756881,
90.3243530139057,90.4374785378027,90.5460067960164,90.6546228124427,90.7634401963979,
90.7768551094939,90.8896159606061,91.0021359799181,91.1145140404942,91.2267837026141,
91.3389783773049,91.4511666309088,91.5633416309981,91.6756048300988,91.77440296784),
 .UNSPECIFIED.);
#2788=B_SPLINE_CURVE_WITH_KNOTS('',3,(#108322,#108323,#108324,#108325,#108326,
#108327,#108328,#108329,#108330,#108331,#108332,#108333,#108334,#108335,
#108336,#108337,#108338,#108339,#108340,#108341,#108342,#108343,#108344,
#108345,#108346,#108347,#108348,#108349,#108350,#108351,#108352,#108353,
#108354,#108355,#108356,#108357,#108358,#108359,#108360,#108361,#108362,
#108363,#108364,#108365,#108366,#108367,#108368,#108369,#108370,#108371,
#108372,#108373,#108374,#108375,#108376,#108377,#108378,#108379,#108380,
#108381,#108382,#108383,#108384,#108385,#108386,#108387,#108388,#108389,
#108390,#108391,#108392,#108393,#108394,#108395,#108396,#108397,#108398,
#108399,#108400,#108401,#108402,#108403,#108404,#108405,#108406,#108407,
#108408,#108409,#108410,#108411,#108412,#108413,#108414,#108415,#108416,
#108417,#108418,#108419,#108420,#108421,#108422,#108423,#108424,#108425,
#108426,#108427,#108428,#108429,#108430,#108431,#108432,#108433,#108434,
#108435,#108436,#108437,#108438,#108439),.UNSPECIFIED.,.F.,.F.,(4,2,2,2,
2,2,2,2,2,2,2,2,2,2,2,2,2,2,2,2,2,2,2,2,2,2,2,2,2,2,2,2,2,2,2,2,2,2,2,2,
2,2,2,2,2,2,2,2,2,2,2,2,2,2,2,2,2,2,4),(-1.75481728510969,-1.75477181337264,
-1.75153187178093,-1.71275849427788,-1.69497582072548,-1.683337395363,-1.67871180999002,
-1.67538295114897,-1.67191960250538,-1.66660456046912,-1.65037913960663,
-1.60504731770615,-1.59826860042396,-1.59560949386773,-1.59373031824308,
-1.59167630480205,-1.58810673052832,-1.57241518926486,-1.54292081107085,
-1.52819502118948,-1.51800868340683,-1.51362687471493,-1.51035825589616,
-1.50685212820087,-1.50124890871277,-1.48201218035526,-1.4384075977429,
-1.43151370044267,-1.42886927969711,-1.42702102419335,-1.4250209951348,
-1.42161605848922,-1.40824164098538,-1.38168743495141,-1.36341339699232,
-1.35162601713303,-1.34703193709419,-1.34375687734004,-1.34037859829957,
-1.33525779623736,-1.32041932433269,-1.28441371753311,-1.27223733355736,
-1.26477052417365,-1.26206143967995,-1.26021071906368,-1.2584793794237,
-1.25546173708441,-1.2463249096779,-1.21667700630301,-1.19715006646039,
-1.18482019530896,-1.1801284704705,-1.17681564299213,-1.17382065619317,
-1.16905081057468,-1.15709755632943,-1.11839002684626,-1.10915476758989),
 .UNSPECIFIED.);
#2789=B_SPLINE_CURVE_WITH_KNOTS('',3,(#108445,#108446,#108447,#108448,#108449,
#108450,#108451,#108452,#108453,#108454,#108455,#108456,#108457,#108458,
#108459,#108460,#108461,#108462,#108463,#108464,#108465,#108466,#108467,
#108468,#108469,#108470,#108471,#108472,#108473,#108474,#108475,#108476,
#108477,#108478,#108479,#108480,#108481,#108482,#108483,#108484,#108485,
#108486,#108487,#108488,#108489,#108490,#108491,#108492,#108493,#108494,
#108495,#108496,#108497,#108498,#108499,#108500,#108501,#108502,#108503,
#108504,#108505,#108506,#108507,#108508,#108509,#108510,#108511,#108512,
#108513,#108514,#108515,#108516,#108517,#108518,#108519,#108520,#108521,
#108522,#108523,#108524,#108525,#108526,#108527,#108528,#108529,#108530,
#108531,#108532,#108533,#108534,#108535,#108536,#108537,#108538,#108539,
#108540,#108541,#108542,#108543,#108544,#108545,#108546,#108547,#108548,
#108549,#108550,#108551,#108552,#108553,#108554,#108555,#108556,#108557,
#108558,#108559,#108560,#108561,#108562,#108563,#108564,#108565,#108566,
#108567,#108568,#108569,#108570,#108571,#108572,#108573,#108574,#108575,
#108576,#108577,#108578,#108579,#108580,#108581,#108582,#108583,#108584,
#108585,#108586,#108587,#108588,#108589,#108590,#108591,#108592,#108593,
#108594,#108595,#108596,#108597,#108598,#108599,#108600,#108601,#108602,
#108603,#108604,#108605,#108606,#108607,#108608,#108609,#108610,#108611,
#108612,#108613,#108614,#108615,#108616,#108617,#108618,#108619,#108620,
#108621,#108622,#108623,#108624,#108625,#108626,#108627,#108628),
 .UNSPECIFIED.,.F.,.F.,(4,2,2,2,2,2,2,2,2,2,2,2,2,2,2,2,2,2,2,2,2,2,2,2,
2,2,2,2,2,2,2,2,2,2,2,2,2,2,2,2,2,2,2,2,2,2,2,2,2,2,2,2,2,2,2,2,2,2,2,2,
2,2,2,2,2,2,2,2,2,2,2,2,2,2,2,2,2,2,2,2,2,2,2,2,2,2,2,2,2,2,2,4),(-0.991365966097619,
-0.988171403346623,-0.951027708418659,-0.924485213621447,-0.919532060449943,
-0.917210835975265,-0.91540454613298,-0.913213639481231,-0.908927440911297,
-0.877285678772001,-0.84577788527823,-0.839101439246275,-0.834991520611357,
-0.83177503323073,-0.828172910207905,-0.822052804129883,-0.788117655616523,
-0.757375988151864,-0.752680411982564,-0.750408822704871,-0.748604220264088,
-0.746369106028614,-0.741866430389762,-0.735821578711076,-0.71988238002869,
-0.680158740793254,-0.672049915076576,-0.668043654999549,-0.66483322181507,
-0.661157052101005,-0.654698917509413,-0.621093460965964,-0.590739757177692,
-0.585998485575938,-0.58371576167084,-0.581906308604257,-0.579668955140634,
-0.575176607633632,-0.569153334899086,-0.553314308664931,-0.513867326472703,
-0.505674317180689,-0.501648920062505,-0.498432738193541,-0.494760148481005,
-0.488334920949002,-0.480402422841681,-0.462476277896191,-0.428742094787966,
-0.42089209671108,-0.418039325772129,-0.416339634829174,-0.414459619557906,
-0.411599685015836,-0.402936981831098,-0.387679147675741,-0.350697237862635,
-0.340099791172841,-0.335556591542221,-0.332322551037855,-0.328936500753204,
-0.323780105104325,-0.307248622439695,-0.274080309521543,-0.255531550411014,
-0.251924635015031,-0.24985975941104,-0.248034397591261,-0.245530546972807,
-0.239549921144152,-0.230697456376526,-0.206475386124692,-0.1787310156925,
-0.172040192323377,-0.167912677850742,-0.164676766789898,-0.161046485613818,
-0.154860499093797,-0.14730965957079,-0.130746118999874,-0.0988550790677954,
-0.0879914983010599,-0.0847701619770891,-0.0827915461032264,-0.0808695332414206,
-0.0779944094387794,-0.0696293301742921,-0.0552214154328846,-0.0133076718806713,
-0.00643057283658562,-0.00291508547563278,-0.0005116043560236),
 .UNSPECIFIED.);
#2790=B_SPLINE_CURVE_WITH_KNOTS('',3,(#108629,#108630,#108631,#108632,#108633,
#108634,#108635,#108636,#108637,#108638),.UNSPECIFIED.,.F.,.F.,(4,3,3,4),
(89.2744165561707,89.38943262493,89.5079765184772,89.6265204120243),
 .UNSPECIFIED.);
#2791=B_SPLINE_CURVE_WITH_KNOTS('',3,(#108639,#108640,#108641,#108642,#108643,
#108644,#108645,#108646,#108647,#108648,#108649,#108650,#108651,#108652,
#108653,#108654,#108655,#108656,#108657,#108658,#108659,#108660,#108661,
#108662,#108663,#108664,#108665,#108666,#108667,#108668,#108669,#108670,
#108671,#108672,#108673,#108674,#108675,#108676,#108677,#108678,#108679,
#108680,#108681,#108682,#108683,#108684,#108685,#108686,#108687,#108688,
#108689,#108690,#108691,#108692,#108693,#108694,#108695,#108696,#108697,
#108698,#108699,#108700,#108701,#108702,#108703,#108704,#108705,#108706,
#108707,#108708,#108709,#108710,#108711,#108712,#108713,#108714,#108715,
#108716,#108717,#108718,#108719,#108720,#108721,#108722,#108723,#108724,
#108725,#108726,#108727,#108728,#108729,#108730,#108731,#108732,#108733,
#108734,#108735,#108736,#108737,#108738,#108739,#108740,#108741,#108742,
#108743,#108744,#108745,#108746,#108747,#108748,#108749,#108750,#108751,
#108752,#108753,#108754,#108755,#108756,#108757,#108758,#108759,#108760,
#108761,#108762,#108763,#108764,#108765,#108766,#108767,#108768,#108769,
#108770,#108771,#108772,#108773,#108774,#108775,#108776,#108777,#108778,
#108779,#108780,#108781,#108782,#108783,#108784,#108785,#108786,#108787,
#108788,#108789,#108790,#108791,#108792,#108793,#108794,#108795,#108796,
#108797,#108798,#108799,#108800,#108801,#108802,#108803,#108804,#108805,
#108806,#108807,#108808,#108809,#108810,#108811,#108812,#108813,#108814,
#108815,#108816,#108817,#108818,#108819,#108820,#108821,#108822,#108823,
#108824,#108825,#108826,#108827,#108828,#108829,#108830,#108831,#108832,
#108833,#108834,#108835,#108836,#108837,#108838,#108839,#108840,#108841,
#108842,#108843,#108844,#108845,#108846,#108847,#108848,#108849,#108850,
#108851,#108852,#108853,#108854,#108855,#108856),.UNSPECIFIED.,.F.,.F.,
(4,2,2,2,2,2,2,2,2,2,2,2,2,2,2,2,2,2,2,2,2,2,2,2,2,2,2,2,2,2,2,2,2,2,2,
2,2,2,2,2,2,2,2,2,2,2,2,2,2,2,2,2,2,2,2,2,2,2,2,2,2,2,2,2,2,2,2,2,2,2,2,
2,2,2,2,2,2,2,2,2,2,2,2,2,2,2,2,2,2,2,2,2,2,2,2,2,2,2,2,2,2,2,2,2,2,2,2,
2,4),(-1.10915476758989,-1.10591269887554,-1.09831262663028,-1.09556885125491,
-1.09369988839749,-1.09172147898789,-1.08844984566113,-1.07684122676752,
-1.04905253340296,-1.02093818842599,-1.01503671458796,-1.011478688229,-1.00824848794993,
-1.00411575334142,-0.995066440372814,-0.95241799962058,-0.939448567678061,
-0.931650085503435,-0.928885238733866,-0.927016293223566,-0.925051907038574,
-0.921834192030397,-0.910795257199551,-0.878917573244537,-0.854166838220865,
-0.848276576579817,-0.844723781452716,-0.841497496625485,-0.837298663939667,
-0.828109764114612,-0.815351174088964,-0.793170065098792,-0.78918399667406,
-0.76685734926639,-0.763166664998647,-0.761078354558164,-0.759258785846163,
-0.756789568927929,-0.75099352474985,-0.742506502740908,-0.712520149688132,
-0.687505557982705,-0.681603740934655,-0.678046105746995,-0.674816658201571,
-0.670615321973303,-0.661426597907566,-0.648670027263927,-0.626513181060461,
-0.622406803408179,-0.600236589277191,-0.596544402090522,-0.594454126190604,
-0.592633534159041,-0.590162326809779,-0.584354641376705,-0.57584417185639,
-0.545670536684166,-0.520882308009663,-0.514988465362761,-0.511433169593473,
-0.508204312797849,-0.504001592882966,-0.494801114593605,-0.482022249631789,
-0.459859098790976,-0.455687809651332,-0.433590842226422,-0.429899585768213,
-0.427810162328844,-0.425990263346943,-0.423520355790637,-0.41771837945405,
-0.409218889008852,-0.379129430160548,-0.354240075731908,-0.348343606438635,
-0.344788091837284,-0.341559913607819,-0.337359349303703,-0.328169075750749,
-0.315409011071738,-0.293241542476824,-0.289168613256107,-0.266951351457106,
-0.263259952931647,-0.261170606702629,-0.259350665511173,-0.256880704924071,
-0.251079145312153,-0.242580663107586,-0.212499837262792,-0.187582909402351,
-0.181696070158885,-0.178142337625143,-0.174913213247982,-0.170707714485491,
-0.161490703421122,-0.148679700319745,-0.126536537743213,-0.122249519500312,
-0.10031932867716,-0.0966288102038732,-0.0945394845739377,-0.0927194134372372,
-0.0902488872540718,-0.0844437274590148,-0.0759379139851325,-0.0594803364103627),
 .UNSPECIFIED.);
#2792=B_SPLINE_CURVE_WITH_KNOTS('',3,(#108861,#108862,#108863,#108864,#108865,
#108866,#108867,#108868,#108869,#108870,#108871,#108872,#108873,#108874,
#108875,#108876,#108877,#108878,#108879,#108880,#108881,#108882,#108883,
#108884,#108885,#108886,#108887,#108888,#108889,#108890,#108891,#108892,
#108893,#108894,#108895,#108896,#108897,#108898,#108899,#108900,#108901,
#108902,#108903,#108904,#108905,#108906,#108907,#108908,#108909,#108910,
#108911,#108912,#108913,#108914,#108915,#108916,#108917,#108918,#108919,
#108920,#108921,#108922,#108923,#108924,#108925,#108926,#108927,#108928,
#108929,#108930,#108931,#108932,#108933,#108934,#108935,#108936,#108937,
#108938,#108939,#108940,#108941,#108942,#108943,#108944,#108945,#108946,
#108947,#108948,#108949,#108950,#108951,#108952,#108953,#108954,#108955,
#108956,#108957,#108958,#108959,#108960,#108961,#108962,#108963,#108964,
#108965,#108966,#108967,#108968,#108969,#108970,#108971,#108972,#108973,
#108974,#108975,#108976,#108977,#108978,#108979,#108980,#108981,#108982,
#108983,#108984,#108985,#108986,#108987,#108988,#108989,#108990,#108991,
#108992,#108993,#108994,#108995,#108996,#108997,#108998,#108999,#109000,
#109001,#109002,#109003,#109004,#109005,#109006,#109007,#109008,#109009,
#109010,#109011,#109012,#109013,#109014,#109015,#109016,#109017,#109018,
#109019,#109020,#109021,#109022,#109023,#109024,#109025,#109026,#109027,
#109028,#109029,#109030,#109031,#109032,#109033,#109034,#109035,#109036,
#109037,#109038,#109039,#109040,#109041,#109042,#109043,#109044,#109045,
#109046,#109047,#109048,#109049,#109050,#109051,#109052,#109053,#109054,
#109055,#109056,#109057,#109058,#109059,#109060,#109061,#109062,#109063,
#109064,#109065,#109066,#109067,#109068,#109069,#109070,#109071,#109072,
#109073,#109074,#109075,#109076),.UNSPECIFIED.,.F.,.F.,(4,2,2,2,2,2,2,2,
2,2,2,2,2,2,2,2,2,2,2,2,2,2,2,2,2,2,2,2,2,2,2,2,2,2,2,2,2,2,2,2,2,2,2,2,
2,2,2,2,2,2,2,2,2,2,2,2,2,2,2,2,2,2,2,2,2,2,2,2,2,2,2,2,2,2,2,2,2,2,2,2,
2,2,2,2,2,2,2,2,2,2,2,2,2,2,2,2,2,2,2,2,2,2,2,2,2,2,2,4),(-2.04109288767521,
-2.03687409690353,-2.01877604215181,-2.01080122194488,-2.00435292186267,
-2.00067972693583,-1.99747046188616,-1.99346381783989,-1.98714950953611,
-1.94854787787447,-1.92329715138688,-1.91906359849201,-1.91688212668974,
-1.91507433937708,-1.91273878684722,-1.90788492461484,-1.88352805463694,
-1.86135525310743,-1.84856021519006,-1.83935161916744,-1.83514657090432,
-1.83191645493625,-1.82836027830888,-1.82246608040773,-1.79768773004298,
-1.76753019545428,-1.75902273361361,-1.75321573581784,-1.75074429413677,
-1.74892347192538,-1.74683322707306,-1.74314067118672,-1.72114037231852,
-1.71687648042423,-1.69470447950986,-1.68190706046456,-1.67269719927741,
-1.66849191849167,-1.66526175956431,-1.66170567024749,-1.6558119339385,
-1.63104819090398,-1.60087893266394,-1.59236999930377,-1.58656225572344,
-1.58409066292257,-1.58226976601499,-1.58017942139659,-1.57648678065388,
-1.55448186952836,-1.55022240019711,-1.52805146305322,-1.51525674181924,
-1.50604831367855,-1.50184320097003,-1.49861296781623,-1.49505658831395,
-1.4891618634075,-1.46437057717612,-1.43422474338118,-1.42571876013822,
-1.41991248598996,-1.41744114531021,-1.41562038039269,-1.41353028875066,
-1.40983783581059,-1.38780284910498,-1.38356418636957,-1.3613890194487,
-1.34859828616354,-1.33939209720686,-1.33518772461819,-1.33195797531807,
-1.32840205894175,-1.32250797435515,-1.29772093261388,-1.26757120412798,
-1.25906494186905,-1.25325865609181,-1.25078747679406,-1.2489668089471,
-1.24687667366901,-1.24318435855359,-1.22123974221259,-1.21693683767769,
-1.19476953421665,-1.18195680853648,-1.17273882568845,-1.16853209392249,
-1.16530171323064,-1.16174626935345,-1.15585570791226,-1.13119043522373,
-1.10093965540801,-1.09242046631484,-1.0866075501802,-1.08413495980609,
-1.08231362761373,-1.08022280171974,-1.07653011743228,-1.05463307154296,
-1.05046548987067,-1.01182908984538,-1.00551777533215,-1.00151152028973,
-0.998301542668516,-0.994626382112296,-0.991365966097619),.UNSPECIFIED.);
#2793=B_SPLINE_CURVE_WITH_KNOTS('',3,(#109078,#109079,#109080,#109081,#109082,
#109083,#109084,#109085,#109086,#109087,#109088,#109089,#109090,#109091,
#109092,#109093),.UNSPECIFIED.,.F.,.F.,(4,2,2,2,2,2,2,4),(-0.0594803364103627,
-0.034131742218652,-0.0193897135688908,-0.014271326393632,-0.0108796422400385,
-0.0078410923203492,-0.0042584985369012,-0.000493909690971492),
 .UNSPECIFIED.);
#2794=B_SPLINE_CURVE_WITH_KNOTS('',3,(#109094,#109095,#109096,#109097,#109098,
#109099,#109100,#109101,#109102,#109103,#109104,#109105,#109106,#109107,
#109108,#109109,#109110,#109111,#109112,#109113,#109114,#109115,#109116,
#109117,#109118,#109119,#109120,#109121,#109122,#109123,#109124,#109125,
#109126,#109127,#109128,#109129,#109130,#109131,#109132,#109133,#109134,
#109135,#109136,#109137,#109138,#109139,#109140,#109141,#109142,#109143,
#109144,#109145,#109146,#109147,#109148,#109149,#109150,#109151,#109152,
#109153,#109154,#109155,#109156,#109157,#109158,#109159,#109160,#109161,
#109162,#109163,#109164,#109165,#109166,#109167,#109168,#109169,#109170,
#109171,#109172,#109173,#109174,#109175,#109176,#109177,#109178,#109179,
#109180,#109181,#109182,#109183,#109184,#109185,#109186,#109187,#109188,
#109189,#109190,#109191,#109192,#109193,#109194,#109195,#109196,#109197,
#109198,#109199,#109200,#109201,#109202,#109203,#109204,#109205,#109206,
#109207,#109208,#109209,#109210,#109211,#109212,#109213,#109214,#109215,
#109216,#109217,#109218,#109219,#109220,#109221,#109222,#109223,#109224,
#109225,#109226,#109227,#109228,#109229,#109230,#109231,#109232,#109233,
#109234,#109235,#109236,#109237,#109238,#109239,#109240,#109241,#109242,
#109243,#109244,#109245,#109246,#109247,#109248,#109249,#109250,#109251,
#109252,#109253,#109254,#109255,#109256,#109257,#109258,#109259,#109260,
#109261,#109262,#109263,#109264,#109265,#109266,#109267,#109268,#109269,
#109270,#109271,#109272,#109273,#109274,#109275,#109276,#109277,#109278,
#109279,#109280,#109281,#109282,#109283,#109284,#109285,#109286,#109287,
#109288,#109289),.UNSPECIFIED.,.F.,.F.,(4,2,2,2,2,2,2,2,2,2,2,2,2,2,2,2,
2,2,2,2,2,2,2,2,2,2,2,2,2,2,2,2,2,2,2,2,2,2,2,2,2,2,2,2,2,2,2,2,2,2,2,2,
2,2,2,2,2,2,2,2,2,2,2,2,2,2,2,2,2,2,2,2,2,2,2,2,2,2,2,2,2,2,2,2,2,2,2,2,
2,2,2,2,2,2,2,2,2,4),(-2.0995573720879,-2.09249387521299,-2.05186434588951,
-2.03400307225783,-2.02947534543108,-2.02723570969831,-2.02543103320115,
-2.02316381682362,-2.01849392411303,-1.98737166433328,-1.95411421456467,
-1.94952714451913,-1.94533456101474,-1.94210704772032,-1.9385467834496,
-1.93262929074251,-1.9078124325039,-1.87772526984883,-1.86922745731235,
-1.86342568163711,-1.86095566050007,-1.85913558570642,-1.85704591159258,
-1.85335386477429,-1.83124259739022,-1.82705934336081,-1.80487915151732,
-1.79210539935868,-1.78290859214452,-1.77870651814824,-1.77547777804642,
-1.7719222348084,-1.76602706251188,-1.7411715190181,-1.71108226749418,-1.70258421655863,
-1.69678231693862,-1.69431225807351,-1.69249217121317,-1.69040251562105,
-1.68671050274879,-1.66460009727419,-1.66041652985141,-1.63823661501789,
-1.62546276368338,-1.61626593760668,-1.61206389505721,-1.60883519584189,
-1.60527971506497,-1.59938469034904,-1.57453254064439,-1.54444016618074,
-1.53594174974159,-1.53013968733281,-1.52766962667202,-1.52584956212675,
-1.52375995616905,-1.52006810793253,-1.49799387613972,-1.49378264450325,
-1.47160504151074,-1.45882520625341,-1.44962526546874,-1.44542270101988,
-1.44219395683686,-1.43863878204683,-1.43274511042184,-1.40793638725411,
-1.37780671616153,-1.36930363331068,-1.36349926605032,-1.36102883117992,
-1.35920872853993,-1.35711935383474,-1.35342850965987,-1.33159158669275,
-1.32723501167766,-1.30470476004276,-1.29207087331815,-1.28294753169795,
-1.2787583605621,-1.27553131974899,-1.27196941378826,-1.26604400961055,
-1.23992041729621,-1.21091772203325,-1.19851540047147,-1.19528411658948,
-1.19331600925641,-1.1914705182135,-1.18917259443,-1.18337479633972,-1.15093567368114,
-1.12524602335481,-1.11623303348141,-1.1120633137374,-1.10883870020187,
-1.10882129953008),.UNSPECIFIED.);
#2795=B_SPLINE_CURVE_WITH_KNOTS('',3,(#109295,#109296,#109297,#109298,#109299,
#109300,#109301,#109302,#109303,#109304,#109305,#109306,#109307,#109308,
#109309,#109310,#109311,#109312,#109313,#109314,#109315,#109316,#109317,
#109318,#109319,#109320,#109321,#109322,#109323,#109324,#109325,#109326,
#109327,#109328,#109329,#109330,#109331,#109332,#109333,#109334,#109335,
#109336,#109337,#109338,#109339,#109340,#109341,#109342,#109343,#109344,
#109345,#109346,#109347,#109348,#109349,#109350,#109351,#109352,#109353,
#109354,#109355,#109356,#109357,#109358,#109359,#109360,#109361,#109362,
#109363,#109364,#109365,#109366,#109367,#109368,#109369,#109370,#109371,
#109372,#109373,#109374,#109375,#109376,#109377,#109378,#109379,#109380,
#109381,#109382,#109383,#109384,#109385,#109386,#109387,#109388,#109389,
#109390,#109391,#109392,#109393,#109394,#109395,#109396,#109397,#109398,
#109399,#109400,#109401,#109402,#109403,#109404,#109405,#109406,#109407,
#109408,#109409,#109410,#109411,#109412,#109413,#109414,#109415,#109416,
#109417,#109418,#109419,#109420,#109421,#109422,#109423,#109424,#109425,
#109426,#109427,#109428,#109429,#109430,#109431,#109432,#109433,#109434,
#109435,#109436,#109437,#109438,#109439,#109440,#109441,#109442,#109443,
#109444,#109445,#109446,#109447,#109448,#109449,#109450,#109451,#109452,
#109453,#109454,#109455,#109456,#109457,#109458,#109459,#109460,#109461,
#109462,#109463,#109464,#109465,#109466,#109467,#109468,#109469,#109470,
#109471,#109472,#109473,#109474,#109475,#109476,#109477,#109478,#109479,
#109480,#109481,#109482,#109483,#109484,#109485,#109486,#109487,#109488,
#109489,#109490,#109491,#109492,#109493,#109494,#109495,#109496,#109497,
#109498),.UNSPECIFIED.,.F.,.F.,(4,2,2,2,2,2,2,2,2,2,2,2,2,2,2,2,2,2,2,2,
2,2,2,2,2,2,2,2,2,2,2,2,2,2,2,2,2,2,2,2,2,2,2,2,2,2,2,2,2,2,2,2,2,2,2,2,
2,2,2,2,2,2,2,2,2,2,2,2,2,2,2,2,2,2,2,2,2,2,2,2,2,2,2,2,2,2,2,2,2,2,2,2,
2,2,2,2,2,2,2,2,2,4),(-0.991134662338154,-0.989393772578213,-0.985702140833392,
-0.983612358980175,-0.981791924446668,-0.97932092894059,-0.973514811855033,
-0.965007446467625,-0.934855857628895,-0.910050109404556,-0.904155443320496,
-0.900599669208326,-0.897370363333034,-0.893167002313335,-0.883964605623374,
-0.871181968600566,-0.849028653124806,-0.844834692257524,-0.822778552785723,
-0.819087320069484,-0.816997653685516,-0.815177241193076,-0.812706170189455,
-0.806899410365834,-0.798390682843575,-0.768227505857458,-0.743436283209991,
-0.737542169922906,-0.733986561731969,-0.730757300532083,-0.72655384548527,
-0.717350594695106,-0.704566224891441,-0.682414186805858,-0.678212540654213,
-0.656167298020162,-0.652476182021449,-0.650386568364238,-0.648566192208087,
-0.646095157854975,-0.64028842874351,-0.631779696595099,-0.601615710259276,
-0.576826626836023,-0.5709326854297,-0.567377161612114,-0.564147964829037,
-0.559944576101074,-0.550741395741389,-0.537957060115449,-0.515805583759316,
-0.5116031716918,-0.489559557810953,-0.485868522416741,-0.483778952690514,
-0.481958612108759,-0.479487623089475,-0.473680990127681,-0.465172387358052,
-0.435008646302392,-0.410220597040677,-0.404326792668917,-0.400771343799169,
-0.397542210066243,-0.393338896067229,-0.384135847296285,-0.371351667082328,
-0.349200691987352,-0.344997875086687,-0.322955349682106,-0.319264392560079,
-0.317174866231494,-0.31535456618774,-0.312883633761692,-0.307077133325061,
-0.298568727074793,-0.268405757051954,-0.24361798544822,-0.237724302272828,
-0.23416893182949,-0.230939872928728,-0.226736661790037,-0.217533863293973,
-0.204750054967559,-0.182599488272133,-0.158267438953356,-0.153413459536601,
-0.151078327325675,-0.149271106059955,-0.14717966677521,-0.143468180324395,
-0.138511197619789,-0.126878914663252,-0.105635883196703,-0.0772181880988006,
-0.0712212799721465,-0.0676440388692883,-0.0644202939646342,-0.0602596848747935,
-0.0512989436365756,-0.00636782713373653,-0.000492472357443245),
 .UNSPECIFIED.);
#2796=B_SPLINE_CURVE_WITH_KNOTS('',3,(#109499,#109500,#109501,#109502,#109503,
#109504,#109505,#109506,#109507,#109508,#109509,#109510,#109511,#109512,
#109513,#109514,#109515,#109516,#109517,#109518),.UNSPECIFIED.,.F.,.F.,
(4,2,2,2,2,2,2,2,2,4),(-2.09991177729522,-2.09207408138876,-2.08725374609279,
-2.08513462603622,-2.08342457726091,-2.08161050394509,-2.07923825003836,
-2.07406347330844,-2.05735942596725,-2.04109288767521),.UNSPECIFIED.);
#2797=B_SPLINE_CURVE_WITH_KNOTS('',3,(#109519,#109520,#109521,#109522,#109523,
#109524,#109525,#109526,#109527,#109528,#109529,#109530,#109531,#109532,
#109533,#109534,#109535,#109536,#109537,#109538,#109539,#109540,#109541,
#109542,#109543,#109544,#109545,#109546,#109547,#109548,#109549,#109550,
#109551,#109552,#109553,#109554,#109555,#109556,#109557,#109558,#109559,
#109560,#109561,#109562,#109563,#109564,#109565,#109566,#109567,#109568,
#109569,#109570,#109571,#109572,#109573,#109574,#109575,#109576,#109577,
#109578,#109579,#109580,#109581,#109582,#109583,#109584,#109585,#109586,
#109587,#109588,#109589,#109590,#109591,#109592,#109593,#109594,#109595,
#109596,#109597,#109598,#109599,#109600,#109601,#109602,#109603,#109604,
#109605,#109606,#109607,#109608,#109609,#109610,#109611,#109612,#109613,
#109614,#109615,#109616,#109617,#109618,#109619,#109620,#109621,#109622,
#109623,#109624,#109625,#109626,#109627,#109628,#109629,#109630,#109631,
#109632,#109633,#109634,#109635,#109636,#109637,#109638,#109639,#109640,
#109641,#109642,#109643,#109644,#109645,#109646,#109647,#109648,#109649,
#109650,#109651,#109652,#109653,#109654,#109655,#109656,#109657,#109658,
#109659,#109660,#109661,#109662,#109663,#109664,#109665,#109666,#109667,
#109668,#109669,#109670,#109671,#109672,#109673,#109674,#109675,#109676,
#109677,#109678,#109679,#109680,#109681,#109682,#109683,#109684,#109685,
#109686,#109687,#109688,#109689,#109690,#109691,#109692,#109693,#109694,
#109695,#109696,#109697,#109698,#109699,#109700,#109701,#109702,#109703,
#109704,#109705,#109706,#109707,#109708,#109709,#109710,#109711,#109712,
#109713,#109714,#109715,#109716,#109717,#109718,#109719,#109720,#109721,
#109722,#109723,#109724,#109725,#109726),.UNSPECIFIED.,.F.,.F.,(4,2,2,2,
2,2,2,2,2,2,2,2,2,2,2,2,2,2,2,2,2,2,2,2,2,2,2,2,2,2,2,2,2,2,2,2,2,2,2,2,
2,2,2,2,2,2,2,2,2,2,2,2,2,2,2,2,2,2,2,2,2,2,2,2,2,2,2,2,2,2,2,2,2,2,2,2,
2,2,2,2,2,2,2,2,2,2,2,2,2,2,2,2,2,2,2,2,2,2,2,2,2,2,2,4),(-1.10882129953008,
-1.10526679528211,-1.09929416345195,-1.07124182550192,-1.04978224149019,
-1.03261309667385,-1.0290185920319,-1.02695086560713,-1.02512548808884,
-1.02261512611383,-1.01656741095832,-1.00756682415849,-0.973112349166505,
-0.952936237953287,-0.947296295079374,-0.943795112865223,-0.940550166108246,
-0.936229594429629,-0.926332736062728,-0.91218893201069,-0.891751501520659,
-0.890602460875589,-0.866184410411082,-0.86247127304989,-0.860376961154501,
-0.858558047134264,-0.856096498761252,-0.850344969839385,-0.841946925977698,
-0.812645944373628,-0.786842143338621,-0.780922527996549,-0.777361959856718,
-0.774134794994737,-0.769943550320701,-0.760807450656747,-0.748150688772646,
-0.725521448732133,-0.721449722606859,-0.699512946972071,-0.695822540733412,
-0.693733335049984,-0.691913354177291,-0.689442995058895,-0.683638598029587,
-0.675134251720369,-0.645005398979941,-0.620165723773691,-0.61427071306575,
-0.610715419617843,-0.607487015676931,-0.603285532896211,-0.594090498440146,
-0.581321308581274,-0.559159686034164,-0.555024085602284,-0.53288651341158,
-0.529195421161299,-0.527106088192019,-0.52528618289593,-0.522816176147932,
-0.517013707557131,-0.50851318092388,-0.47841381489131,-0.453541472344877,
-0.447645586081739,-0.444090153848873,-0.440861870125438,-0.43666089715462,
-0.427468482464292,-0.414704197444107,-0.392541395749679,-0.388430832861548,
-0.366262335317689,-0.362571202686006,-0.360481886536925,-0.358662024250052,
-0.356192113814487,-0.350390038484483,-0.341890238794491,-0.311795864278021,
-0.286919002007577,-0.281023086493249,-0.277467695171247,-0.274239485627579,
-0.270038662322151,-0.260846801230966,-0.248083475305109,-0.225920888704558,
-0.20154588699152,-0.196697064740808,-0.194363215280882,-0.192556414298842,
-0.190375833504921,-0.1861431979326,-0.160915595012162,-0.122261479818827,
-0.115952019129516,-0.111947990382275,-0.108740547642508,-0.105069173181969,
-0.0986234121112929,-0.0777398413434496,-0.059270592353646),
 .UNSPECIFIED.);
#2798=B_SPLINE_CURVE_WITH_KNOTS('',3,(#109731,#109732,#109733,#109734,#109735,
#109736,#109737,#109738,#109739,#109740,#109741,#109742,#109743,#109744,
#109745,#109746,#109747,#109748,#109749,#109750,#109751,#109752,#109753,
#109754,#109755,#109756,#109757,#109758,#109759,#109760,#109761,#109762,
#109763,#109764,#109765,#109766,#109767,#109768,#109769,#109770,#109771,
#109772,#109773,#109774,#109775,#109776,#109777,#109778,#109779,#109780,
#109781,#109782,#109783,#109784,#109785,#109786,#109787,#109788,#109789,
#109790,#109791,#109792,#109793,#109794,#109795,#109796,#109797,#109798,
#109799,#109800,#109801,#109802,#109803,#109804,#109805,#109806,#109807,
#109808,#109809,#109810,#109811,#109812,#109813,#109814,#109815,#109816,
#109817,#109818,#109819,#109820,#109821,#109822,#109823,#109824,#109825,
#109826,#109827,#109828,#109829,#109830,#109831,#109832,#109833,#109834,
#109835,#109836,#109837,#109838,#109839,#109840,#109841,#109842,#109843,
#109844,#109845,#109846,#109847,#109848,#109849,#109850,#109851,#109852,
#109853,#109854,#109855,#109856,#109857,#109858,#109859,#109860,#109861,
#109862,#109863,#109864,#109865,#109866,#109867,#109868,#109869,#109870,
#109871,#109872,#109873,#109874,#109875,#109876,#109877,#109878,#109879,
#109880,#109881,#109882,#109883,#109884,#109885,#109886,#109887,#109888,
#109889,#109890,#109891,#109892,#109893,#109894,#109895,#109896,#109897,
#109898,#109899,#109900,#109901,#109902,#109903,#109904,#109905,#109906,
#109907,#109908,#109909,#109910,#109911,#109912,#109913,#109914,#109915,
#109916,#109917,#109918,#109919,#109920,#109921,#109922,#109923,#109924,
#109925,#109926,#109927,#109928,#109929,#109930,#109931,#109932,#109933,
#109934,#109935,#109936,#109937,#109938),.UNSPECIFIED.,.F.,.F.,(4,2,2,2,
2,2,2,2,2,2,2,2,2,2,2,2,2,2,2,2,2,2,2,2,2,2,2,2,2,2,2,2,2,2,2,2,2,2,2,2,
2,2,2,2,2,2,2,2,2,2,2,2,2,2,2,2,2,2,2,2,2,2,2,2,2,2,2,2,2,2,2,2,2,2,2,2,
2,2,2,2,2,2,2,2,2,2,2,2,2,2,2,2,2,2,2,2,2,2,2,2,2,2,2,4),(-2.0406532363113,
-2.01879651888547,-1.99238066791252,-1.98657417046703,-1.98410307949025,
-1.98228257015237,-1.98019274581841,-1.97650105154882,-1.95454871727625,
-1.95046807602693,-1.92810477819024,-1.9152929004022,-1.90607597756734,
-1.90186996389921,-1.89864022294136,-1.89508557179966,-1.88919654334807,
-1.86441758445059,-1.8342642856284,-1.82575826484962,-1.81995228083814,
-1.81748128633533,-1.81566080012792,-1.81357094653259,-1.80987908044253,
-1.78787432395361,-1.78361778033117,-1.76144966868946,-1.74865705504362,
-1.73945022254613,-1.73524598260645,-1.7320164868859,-1.72846099132732,
-1.72256791491311,-1.69779327829074,-1.66764318319486,-1.65913759824842,
-1.65333184146872,-1.65086089519909,-1.64904042548142,-1.64695056864638,
-1.64325864911555,-1.62123294175447,-1.61699149170688,-1.59482168700347,
-1.58203367703209,-1.57282927028346,-1.56862547074867,-1.56539604996123,
-1.56184037403629,-1.5559463735015,-1.53114033476139,-1.50101796151513,
-1.49251590193294,-1.48671190598062,-1.48424126358828,-1.48242084262927,
-1.48033083784776,-1.47663821803773,-1.4544137137572,-1.45069200970983,
-1.42326105907623,-1.40818941285548,-1.40316621558188,-1.39979321671459,
-1.39651582226178,-1.39255487107151,-1.38289952391565,-1.34516178337439,
-1.3297452207056,-1.32382287957242,-1.31938965239073,-1.31716844311672,
-1.31536310200235,-1.31307534335792,-1.30829889124567,-1.27819911735721,
-1.26674243556599,-1.25091986982357,-1.24021374006788,-1.23576318522774,
-1.23249727370469,-1.22945906902001,-1.22442397663453,-1.21052500807858,
-1.17090762880138,-1.16048903259338,-1.15377737352765,-1.1511637520117,
-1.14932208000624,-1.14730144340032,-1.14383047825102,-1.12967209877461,
-1.09931381951288,-1.07624190458356,-1.07056687101835,-1.06705771829471,
-1.06381450574458,-1.05958375875845,-1.04995278007793,-1.03633859043345,
-1.0153335574178,-1.01153673043049,-0.991134662338154),.UNSPECIFIED.);
#2799=B_SPLINE_CURVE_WITH_KNOTS('',3,(#109940,#109941,#109942,#109943,#109944,
#109945,#109946,#109947,#109948,#109949,#109950,#109951,#109952,#109953,
#109954,#109955,#109956,#109957,#109958,#109959),.UNSPECIFIED.,.F.,.F.,
(4,2,2,2,2,2,2,2,2,4),(-0.059270592353646,-0.0463606160273744,-0.0324747523360294,
-0.0290287071869147,-0.0270139928621692,-0.0251710208137734,-0.023312781478327,
-0.0207405421945336,-0.0142423352689885,-0.000491546785663075),
 .UNSPECIFIED.);
#2800=B_SPLINE_CURVE_WITH_KNOTS('',3,(#109960,#109961,#109962,#109963,#109964,
#109965,#109966,#109967,#109968,#109969,#109970,#109971,#109972,#109973,
#109974,#109975,#109976,#109977,#109978,#109979,#109980,#109981,#109982,
#109983,#109984,#109985,#109986,#109987,#109988,#109989,#109990,#109991,
#109992,#109993,#109994,#109995,#109996,#109997,#109998,#109999,#110000,
#110001,#110002,#110003,#110004,#110005,#110006,#110007,#110008,#110009,
#110010,#110011,#110012,#110013,#110014,#110015,#110016,#110017,#110018,
#110019,#110020,#110021,#110022,#110023,#110024,#110025,#110026,#110027,
#110028,#110029,#110030,#110031,#110032,#110033,#110034,#110035,#110036,
#110037,#110038,#110039,#110040,#110041,#110042,#110043,#110044,#110045,
#110046,#110047,#110048,#110049,#110050,#110051,#110052,#110053,#110054,
#110055,#110056,#110057,#110058,#110059,#110060,#110061,#110062,#110063,
#110064,#110065,#110066,#110067,#110068,#110069,#110070,#110071,#110072,
#110073,#110074,#110075,#110076,#110077,#110078,#110079,#110080,#110081,
#110082,#110083,#110084,#110085,#110086,#110087,#110088,#110089,#110090,
#110091,#110092,#110093,#110094,#110095,#110096,#110097,#110098,#110099,
#110100,#110101,#110102,#110103,#110104,#110105,#110106,#110107,#110108,
#110109,#110110,#110111,#110112,#110113,#110114,#110115,#110116,#110117,
#110118,#110119,#110120,#110121,#110122,#110123,#110124,#110125,#110126,
#110127,#110128,#110129,#110130,#110131,#110132,#110133,#110134,#110135,
#110136,#110137,#110138,#110139,#110140,#110141,#110142,#110143,#110144,
#110145,#110146,#110147,#110148,#110149,#110150,#110151,#110152,#110153,
#110154,#110155,#110156,#110157,#110158,#110159,#110160,#110161,#110162,
#110163,#110164,#110165,#110166,#110167,#110168,#110169,#110170,#110171,
#110172,#110173,#110174,#110175,#110176,#110177,#110178,#110179,#110180,
#110181,#110182,#110183,#110184,#110185,#110186,#110187,#110188,#110189,
#110190,#110191,#110192,#110193,#110194,#110195,#110196,#110197,#110198,
#110199,#110200,#110201,#110202,#110203,#110204,#110205,#110206,#110207,
#110208,#110209,#110210,#110211,#110212,#110213,#110214,#110215,#110216,
#110217,#110218,#110219),.UNSPECIFIED.,.F.,.F.,(4,2,2,2,2,2,2,2,2,2,2,2,
2,2,2,2,2,2,2,2,2,2,2,2,2,2,2,2,2,2,2,2,2,2,2,2,2,2,2,2,2,2,2,2,2,2,2,2,
2,2,2,2,2,2,2,2,2,2,2,2,2,2,2,2,2,2,2,2,2,2,2,2,2,2,2,2,2,2,2,2,2,2,2,2,
2,2,2,2,2,2,2,2,2,2,2,2,2,2,2,2,2,2,2,2,2,2,2,2,2,2,2,2,2,2,2,2,2,2,2,2,
2,2,2,2,2,2,2,2,2,4),(-2.10016655421883,-2.05915717791619,-2.04966988750992,
-2.04541771109872,-2.04218228650197,-2.03865068287498,-2.03286840012186,
-2.01046722110432,-1.97820115934944,-1.96940940620449,-1.96355303580982,
-1.9611779328342,-1.96116120944313,-1.96114415872831,-1.96112676351043,
-1.96110900550471,-1.961090865398,-1.9610723226097,-1.96105335515769,-1.96103393962189,
-1.96101405095407,-1.96099366237524,-1.9609727452907,-1.96095126897391,
-1.96092920041967,-1.96090650411634,-1.96088314179674,-1.96085907218092,
-1.96083425064338,-1.96080862887707,-1.9607821544609,-1.96075477045221,
-1.96072641487644,-1.96069702003232,-1.96066651196783,-1.96063480962126,
-1.96060182401781,-1.96056745725225,-1.9605316012524,-1.96049413645845,
-1.9604549303156,-1.96041383539265,-1.95860665287326,-1.95627192877903,
-1.95142008391805,-1.92703083938438,-1.90484928473807,-1.89207542889865,
-1.8828784460171,-1.8786762176849,-1.87544733061379,-1.87189159784961,-1.86599604759875,
-1.84113666609858,-1.81104760506436,-1.80254932613724,-1.79674723539548,
-1.79427707655157,-1.79245690570709,-1.79036713775207,-1.78667491571159,
-1.76455923127716,-1.7603785457002,-1.73819718197419,-1.72542333198084,
-1.71622637035485,-1.7120241645721,-1.70879529989845,-1.70523959686264,
-1.69934410795363,-1.67448553005861,-1.64439614462895,-1.63589785878363,
-1.63009577607805,-1.62762562946949,-1.62580547110471,-1.62371572150919,
-1.6200235405967,-1.59791195105464,-1.59372824276747,-1.57154726109244,
-1.55877286929777,-1.54957564222735,-1.5453734090141,-1.54214456033358,
-1.53858891192559,-1.53269360167488,-1.50783975415642,-1.47774662810177,
-1.46924790392769,-1.46344561504617,-1.46097544494368,-1.45915529453949,
-1.45706558350824,-1.45337353408022,-1.43129068858072,-1.42708504511212,
-1.40490593989988,-1.39212684990688,-1.38292718176827,-1.3787245419601,
-1.37549566073552,-1.37194025591082,-1.3660460143265,-1.34122644492246,
-1.31110385504905,-1.30260144689542,-1.29679734046845,-1.29432687819739,
-1.29250670178993,-1.29041718126206,-1.28672594272973,-1.26484282150886,
-1.26065803570967,-1.23803998838052,-1.22538318888839,-1.21624768519038,
-1.21205626812063,-1.20882882540122,-1.20526780822604,-1.19934707303047,
-1.173469953063,-1.14425621295001,-1.13587076886993,-1.13012490576551,-1.12766419633862,
-1.12584524206693,-1.12375016027356,-1.1200340051944,-1.10925371751591),
 .UNSPECIFIED.);
#2801=B_SPLINE_CURVE_WITH_KNOTS('',3,(#110225,#110226,#110227,#110228,#110229,
#110230,#110231,#110232,#110233,#110234,#110235,#110236,#110237,#110238,
#110239,#110240,#110241,#110242,#110243,#110244,#110245,#110246,#110247,
#110248,#110249,#110250,#110251,#110252,#110253,#110254,#110255,#110256,
#110257,#110258,#110259,#110260,#110261,#110262,#110263,#110264,#110265,
#110266,#110267,#110268,#110269,#110270,#110271,#110272,#110273,#110274,
#110275,#110276,#110277,#110278,#110279,#110280,#110281,#110282,#110283,
#110284,#110285,#110286,#110287,#110288,#110289,#110290,#110291,#110292,
#110293,#110294,#110295,#110296,#110297,#110298,#110299,#110300,#110301,
#110302,#110303,#110304,#110305,#110306,#110307,#110308,#110309,#110310,
#110311,#110312,#110313,#110314,#110315,#110316,#110317,#110318,#110319,
#110320,#110321,#110322,#110323,#110324,#110325,#110326,#110327,#110328,
#110329,#110330,#110331,#110332,#110333,#110334,#110335,#110336,#110337,
#110338,#110339,#110340,#110341,#110342,#110343,#110344,#110345,#110346,
#110347,#110348,#110349,#110350,#110351,#110352,#110353,#110354,#110355,
#110356,#110357,#110358,#110359,#110360,#110361,#110362,#110363,#110364,
#110365,#110366,#110367,#110368,#110369,#110370,#110371,#110372,#110373,
#110374,#110375,#110376,#110377,#110378,#110379,#110380,#110381,#110382,
#110383,#110384,#110385,#110386,#110387,#110388,#110389,#110390,#110391,
#110392,#110393,#110394,#110395,#110396,#110397,#110398,#110399,#110400,
#110401,#110402,#110403,#110404,#110405,#110406,#110407,#110408,#110409,
#110410,#110411,#110412,#110413,#110414,#110415,#110416,#110417,#110418,
#110419,#110420,#110421,#110422,#110423,#110424,#110425,#110426,#110427,
#110428,#110429,#110430,#110431,#110432,#110433,#110434,#110435,#110436,
#110437,#110438,#110439,#110440,#110441,#110442,#110443,#110444,#110445,
#110446,#110447,#110448),.UNSPECIFIED.,.F.,.F.,(4,2,2,2,2,2,2,2,2,2,2,2,
2,2,2,2,2,2,2,2,2,2,2,2,2,2,2,2,2,2,2,2,2,2,2,2,2,2,2,2,2,2,2,2,2,2,2,2,
2,2,2,2,2,2,2,2,2,2,2,2,2,2,2,2,2,2,2,2,2,2,2,2,2,2,2,2,2,2,2,2,2,2,2,2,
2,2,2,2,2,2,2,2,2,2,2,2,2,2,2,2,2,2,2,2,2,2,2,2,2,2,2,4),(-0.991198145747101,
-0.979922139387548,-0.973232366071378,-0.969116806922089,-0.965897290328937,
-0.962293127073538,-0.9561727018672,-0.921045055981403,-0.891621506969829,
-0.886838852062437,-0.88454963029269,-0.882743881421336,-0.880523101915277,
-0.876093453497073,-0.870177143769939,-0.854788679461095,-0.817175695968832,
-0.807371148699922,-0.803385048987159,-0.800100848466217,-0.796734956829209,
-0.791749378218907,-0.777019549346137,-0.750729215994269,-0.725134844432903,
-0.720291958278169,-0.717958610530376,-0.716150997953339,-0.713967901386552,
-0.709726061906691,-0.704136351782836,-0.690095693703073,-0.657343598080886,
-0.64238888567584,-0.637237667375068,-0.633838156814175,-0.63054094544253,
-0.625912096471104,-0.614001624710468,-0.595472736993051,-0.568245519300723,
-0.555879485407219,-0.552536464519145,-0.550543540630084,-0.548689034921384,
-0.546002948478418,-0.538790272453764,-0.527231894476751,-0.506004313869084,
-0.477456941445017,-0.471447069061,-0.467866405285966,-0.46464224625417,
-0.460484862635421,-0.451546501851753,-0.425059047755777,-0.391100545075304,
-0.386661277976547,-0.384438648506088,-0.382633036795257,-0.380346051650563,
-0.37557488977765,-0.355546054752669,-0.319809736554227,-0.308122495890007,
-0.303395286082738,-0.300112929251811,-0.296745016497769,-0.291748957244756,
-0.27692509249976,-0.250326697406234,-0.22521380130329,-0.220276037671602,
-0.217957798506011,-0.216151063702564,-0.213955796125457,-0.20965339983341,
-0.184256259388925,-0.14589091042111,-0.13957251014971,-0.135564879815861,
-0.13235580040956,-0.132069740304737,-0.131797747524467,-0.131536018698235,
-0.131326680520065,-0.131154744544695,-0.13101055825957,-0.130887593749863,
-0.130781261702504,-0.130688232298338,-0.130606025406809,-0.130532752426627,
-0.130466947644139,-0.130407454724,-0.130353348164902,-0.130303877767377,
-0.130258428498361,-0.130216490986225,-0.130058621965028,-0.129900736399659,
-0.124978408329008,-0.109896163487368,-0.0823246596791248,-0.0799968337057307,
-0.0566107160938009,-0.0529128640661709,-0.0508215781362848,-0.0490012733873011,
-0.04653238028064,-0.040739670100114,-0.00049225813125148),
 .UNSPECIFIED.);
#2802=B_SPLINE_CURVE_WITH_KNOTS('',3,(#110449,#110450,#110451,#110452,#110453,
#110454,#110455,#110456,#110457,#110458,#110459,#110460,#110461,#110462,
#110463,#110464,#110465,#110466),.UNSPECIFIED.,.F.,.F.,(4,2,2,2,2,2,2,2,
4),(-2.09971007316713,-2.07686154414363,-2.07240379950036,-2.0691316260327,
-2.06583659076626,-2.06283508760716,-2.05800539344515,-2.04562339467567,
-2.0406532363113),.UNSPECIFIED.);
#2803=B_SPLINE_CURVE_WITH_KNOTS('',3,(#110467,#110468,#110469,#110470,#110471,
#110472,#110473,#110474,#110475,#110476,#110477,#110478,#110479,#110480,
#110481,#110482,#110483,#110484,#110485,#110486,#110487,#110488,#110489,
#110490,#110491,#110492,#110493,#110494,#110495,#110496,#110497,#110498,
#110499,#110500,#110501,#110502,#110503,#110504,#110505,#110506,#110507,
#110508,#110509,#110510,#110511,#110512,#110513,#110514,#110515,#110516,
#110517,#110518,#110519,#110520,#110521,#110522,#110523,#110524,#110525,
#110526,#110527,#110528,#110529,#110530,#110531,#110532,#110533,#110534,
#110535,#110536,#110537,#110538,#110539,#110540,#110541,#110542,#110543,
#110544,#110545,#110546,#110547,#110548,#110549,#110550,#110551,#110552,
#110553,#110554,#110555,#110556,#110557,#110558,#110559,#110560,#110561,
#110562,#110563,#110564,#110565,#110566,#110567,#110568,#110569,#110570,
#110571,#110572,#110573,#110574,#110575,#110576,#110577,#110578,#110579,
#110580,#110581,#110582,#110583,#110584,#110585,#110586,#110587,#110588,
#110589,#110590,#110591,#110592,#110593,#110594,#110595,#110596,#110597,
#110598,#110599,#110600,#110601,#110602,#110603,#110604,#110605,#110606,
#110607,#110608,#110609,#110610,#110611,#110612,#110613,#110614,#110615,
#110616,#110617,#110618,#110619,#110620,#110621,#110622,#110623,#110624,
#110625,#110626,#110627,#110628,#110629,#110630,#110631,#110632,#110633,
#110634,#110635,#110636,#110637,#110638,#110639,#110640,#110641,#110642,
#110643,#110644,#110645,#110646,#110647,#110648,#110649,#110650,#110651,
#110652,#110653,#110654,#110655,#110656,#110657,#110658,#110659,#110660,
#110661,#110662),.UNSPECIFIED.,.F.,.F.,(4,2,2,2,2,2,2,2,2,2,2,2,2,2,2,2,
2,2,2,2,2,2,2,2,2,2,2,2,2,2,2,2,2,2,2,2,2,2,2,2,2,2,2,2,2,2,2,2,2,2,2,2,
2,2,2,2,2,2,2,2,2,2,2,2,2,2,2,2,2,2,2,2,2,2,2,2,2,2,2,2,2,2,2,2,2,2,2,2,
2,2,2,2,2,2,2,2,2,4),(-1.10925371751591,-1.09550575347277,-1.07760134236261,
-1.06129650828734,-1.0503670145866,-1.0463295595019,-1.04333238429216,-1.04003441850288,
-1.03539726996905,-1.02342180831539,-1.00473710734787,-0.977124452427724,
-0.965282507648974,-0.961992930843178,-0.960012060857267,-0.958152096937334,
-0.955434246388055,-0.947987646926929,-0.935874901400657,-0.900156364718153,
-0.885232944651148,-0.880085961122931,-0.87668809317706,-0.873391644591205,
-0.868762512047352,-0.856843608831029,-0.838293143269312,-0.811013335325888,
-0.798720539667249,-0.795383983253299,-0.793392883780173,-0.791538434537175,
-0.788850180178022,-0.78161820620513,-0.770013652602038,-0.748839355675297,
-0.720306026606756,-0.714298783809371,-0.710719431158664,-0.707496324550867,
-0.703340153062685,-0.694404035854607,-0.66789503648395,-0.633958123959357,
-0.629516857310411,-0.62729426764726,-0.625489288238946,-0.623203943024099,
-0.618439067109707,-0.598462838181849,-0.562880173529267,-0.55103040634141,
-0.546281146697222,-0.542995478854425,-0.539634097367556,-0.534666702572268,
-0.520087043393112,-0.494275953501948,-0.468025303824664,-0.463176653256218,
-0.460842655797137,-0.459035625313025,-0.456854627929886,-0.452620800670174,
-0.427274460800672,-0.388759280375416,-0.38243442669773,-0.378425603973951,
-0.375217403096375,-0.371548509222647,-0.365116058244221,-0.357166576372186,
-0.339158256166385,-0.305244122311836,-0.297669328822782,-0.29485592966468,
-0.293163719407085,-0.291262116354979,-0.288336762155728,-0.279205017395535,
-0.262630674196795,-0.221534827622289,-0.214918434208845,-0.211172390744529,
-0.208001126639539,-0.20410778017653,-0.196572793331421,-0.186801821689084,
-0.161111208546359,-0.134697968926734,-0.129851213757669,-0.127517758502845,
-0.12571096330473,-0.123530025758696,-0.119668349808246,-0.095716333480646,
-0.0686383347465613,-0.059539451546452),.UNSPECIFIED.);
#2804=B_SPLINE_CURVE_WITH_KNOTS('',3,(#110667,#110668,#110669,#110670,#110671,
#110672,#110673,#110674,#110675,#110676,#110677,#110678,#110679,#110680,
#110681,#110682,#110683,#110684,#110685,#110686,#110687,#110688,#110689,
#110690,#110691,#110692,#110693,#110694,#110695,#110696,#110697,#110698,
#110699,#110700,#110701,#110702,#110703,#110704,#110705,#110706,#110707,
#110708,#110709,#110710,#110711,#110712,#110713,#110714,#110715,#110716,
#110717,#110718,#110719,#110720,#110721,#110722,#110723,#110724,#110725,
#110726,#110727,#110728,#110729,#110730,#110731,#110732,#110733,#110734,
#110735,#110736,#110737,#110738,#110739,#110740,#110741,#110742,#110743,
#110744,#110745,#110746,#110747,#110748,#110749,#110750,#110751,#110752,
#110753,#110754,#110755,#110756,#110757,#110758,#110759,#110760,#110761,
#110762,#110763,#110764,#110765,#110766,#110767,#110768,#110769,#110770,
#110771,#110772,#110773,#110774,#110775,#110776,#110777,#110778,#110779,
#110780,#110781,#110782,#110783,#110784,#110785,#110786,#110787,#110788,
#110789,#110790,#110791,#110792,#110793,#110794,#110795,#110796,#110797,
#110798,#110799,#110800,#110801,#110802,#110803,#110804,#110805,#110806,
#110807,#110808,#110809,#110810,#110811,#110812,#110813,#110814,#110815,
#110816,#110817,#110818,#110819,#110820,#110821,#110822,#110823,#110824,
#110825,#110826,#110827,#110828,#110829,#110830,#110831,#110832,#110833,
#110834,#110835,#110836,#110837,#110838,#110839,#110840,#110841,#110842,
#110843,#110844,#110845,#110846,#110847,#110848,#110849,#110850,#110851,
#110852,#110853,#110854,#110855,#110856,#110857,#110858,#110859,#110860,
#110861,#110862,#110863,#110864,#110865,#110866,#110867,#110868,#110869,
#110870,#110871,#110872,#110873,#110874,#110875,#110876,#110877,#110878,
#110879,#110880,#110881,#110882,#110883,#110884,#110885,#110886,#110887,
#110888,#110889,#110890,#110891,#110892,#110893,#110894,#110895,#110896,
#110897,#110898,#110899,#110900,#110901,#110902),.UNSPECIFIED.,.F.,.F.,
(4,2,2,2,2,2,2,2,2,2,2,2,2,2,2,2,2,2,2,2,2,2,2,2,2,2,2,2,2,2,2,2,2,2,2,
2,2,2,2,2,2,2,2,2,2,2,2,2,2,2,2,2,2,2,2,2,2,2,2,2,2,2,2,2,2,2,2,2,2,2,2,
2,2,2,2,2,2,2,2,2,2,2,2,2,2,2,2,2,2,2,2,2,2,2,2,2,2,2,2,2,2,2,2,2,2,2,2,
2,2,2,2,2,2,2,2,2,2,4),(-2.040918156169,-2.02175067309694,-2.01788165223792,
-1.99046735632266,-1.97542931270169,-1.97051160677594,-1.97035368350289,
-1.97019574120493,-1.97015308637871,-1.97010681483818,-1.97005639631913,
-1.9700011892782,-1.96994040937482,-1.96987308657721,-1.96979800545037,
-1.96971362041797,-1.9696179325652,-1.96950830560969,-1.96938118221942,
-1.96923162994881,-1.9659999595357,-1.96244981971617,-1.95658396976085,
-1.93175403352981,-1.90159550124659,-1.89308797260048,-1.88728095462328,
-1.88480951680331,-1.88298870270076,-1.88089847119671,-1.87720593428999,
-1.85519579285069,-1.85093948269398,-1.82876724466515,-1.81597263871272,
-1.80676431068209,-1.80255934145753,-1.79932926724188,-1.79577311653556,
-1.78987891082858,-1.76509762745267,-1.73494399884569,-1.72643712010952,
-1.72063043561765,-1.71815906373745,-1.7163382683564,-1.71424802358168,
-1.71055538841534,-1.68851223904125,-1.68427982208249,-1.6621049388479,
-1.64931735030738,-1.64011271100341,-1.63590840219731,-1.63267843107337,
-1.62912199039068,-1.62322634437522,-1.59839657334952,-1.56828554296313,
-1.55978406623875,-1.5539800742714,-1.55150916162431,-1.54968843463254,
-1.54759795403942,-1.54390422553654,-1.52155174540561,-1.51756637299942,
-1.4953777226605,-1.48263425390937,-1.47345273724259,-1.46925247885318,
-1.46602304387734,-1.46246461936437,-1.456559552413,-1.43139637668425,-1.40157465600602,
-1.39310994954888,-1.38732424137398,-1.3848563916168,-1.38303606022093,
-1.38094386444565,-1.37724242397059,-1.35355262152704,-1.35154159802529,
-1.33516457613535,-1.31862774103887,-1.31109053263891,-1.30491825651194,
-1.30130316409646,-1.29808570272378,-1.29398899693472,-1.28736469788042,
-1.25363524697903,-1.224200131285,-1.21990163021065,-1.21770705640311,-1.21590015950091,
-1.21358075658974,-1.20863724765885,-1.18219637948464,-1.16748776792177,
-1.15156724093908,-1.1408147202471,-1.13635642719867,-1.13308872434762,
-1.13005158782473,-1.12502471516559,-1.11119907948001,-1.07748349221746,
-1.06317246346268,-1.05485206601686,-1.05202083327608,-1.05013817351247,
-1.04819083116008,-1.04505680342147,-1.03383667143882,-1.01014730675737,
-0.991198145747101),.UNSPECIFIED.);
#2805=B_SPLINE_CURVE_WITH_KNOTS('',3,(#110904,#110905,#110906,#110907,#110908,
#110909,#110910,#110911,#110912,#110913,#110914,#110915,#110916,#110917,
#110918,#110919,#110920,#110921),.UNSPECIFIED.,.F.,.F.,(4,2,2,2,2,2,2,2,
4),(-0.059539451546452,-0.0522753828638611,-0.0469759703147907,-0.0435468468193094,
-0.0402703039018171,-0.0370299854246382,-0.0326579013504971,-0.0227235598706649,
-0.000491884265946706),.UNSPECIFIED.);
#2806=B_SPLINE_CURVE_WITH_KNOTS('',3,(#110922,#110923,#110924,#110925,#110926,
#110927,#110928,#110929,#110930,#110931,#110932,#110933,#110934,#110935,
#110936,#110937,#110938,#110939,#110940,#110941,#110942,#110943,#110944,
#110945,#110946,#110947,#110948,#110949,#110950,#110951,#110952,#110953,
#110954,#110955,#110956,#110957,#110958,#110959,#110960,#110961,#110962,
#110963,#110964,#110965,#110966,#110967,#110968,#110969,#110970,#110971,
#110972,#110973,#110974,#110975,#110976,#110977,#110978,#110979,#110980,
#110981,#110982,#110983,#110984,#110985,#110986,#110987,#110988,#110989,
#110990,#110991,#110992,#110993,#110994,#110995,#110996,#110997,#110998,
#110999,#111000,#111001,#111002,#111003,#111004,#111005,#111006,#111007,
#111008,#111009,#111010,#111011,#111012,#111013,#111014,#111015,#111016,
#111017,#111018,#111019,#111020,#111021,#111022,#111023,#111024,#111025,
#111026,#111027,#111028,#111029,#111030,#111031,#111032,#111033,#111034,
#111035,#111036,#111037,#111038,#111039,#111040,#111041,#111042,#111043,
#111044,#111045,#111046,#111047,#111048,#111049,#111050,#111051,#111052,
#111053,#111054,#111055,#111056,#111057,#111058,#111059,#111060,#111061,
#111062,#111063,#111064,#111065,#111066,#111067,#111068,#111069,#111070,
#111071,#111072,#111073,#111074,#111075,#111076,#111077,#111078,#111079,
#111080,#111081,#111082,#111083,#111084),.UNSPECIFIED.,.F.,.F.,(4,3,3,3,
3,3,3,3,3,3,3,3,3,3,3,3,3,3,3,3,3,3,3,3,3,3,3,3,3,3,3,3,3,3,3,3,3,3,3,3,
3,3,3,3,3,3,3,3,3,3,3,3,3,3,4),(-54.111865720712,-53.9685006349437,-53.8675843506887,
-53.7577897347117,-53.6468205794155,-53.5373284361958,-53.42790328446,-53.3185044306203,
-53.2063874460508,-53.0968489113657,-52.9834427018542,-52.8700364923426,
-52.7602418763655,-52.6492727210694,-52.5397805778495,-52.4303554261137,
-52.3209565722739,-52.2088395877045,-52.0993010530194,-51.9858948435079,
-51.8724886339965,-51.7626940180194,-51.6517248627233,-51.5422327195034,
-51.4328075677676,-51.3234087139277,-51.2112917293584,-51.1017531946732,
-50.9883469851618,-50.8749407756504,-50.7651461596733,-50.6541770043772,
-50.5446848611574,-50.4352597094216,-50.3258608555818,-50.2137438710124,
-50.1042053363273,-49.9907991268158,-49.8773929173043,-49.7675983013272,
-49.6566291460311,-49.5471370028112,-49.4377118510755,-49.3283129972356,
-49.2161960126663,-49.1066574779811,-48.9932512684697,-48.8798450589583,
-48.7700749181116,-48.6604636787953,-48.5509703718697,-48.4415394130417,
-48.3321442536577,-48.2227090186136,-48.1819144021787),.UNSPECIFIED.);
#2807=B_SPLINE_CURVE_WITH_KNOTS('',3,(#111090,#111091,#111092,#111093,#111094,
#111095,#111096,#111097,#111098,#111099,#111100,#111101,#111102,#111103,
#111104,#111105,#111106,#111107,#111108,#111109,#111110,#111111,#111112,
#111113,#111114,#111115,#111116,#111117,#111118,#111119,#111120,#111121,
#111122,#111123,#111124,#111125,#111126,#111127,#111128,#111129,#111130,
#111131,#111132,#111133,#111134,#111135,#111136,#111137,#111138,#111139,
#111140,#111141,#111142,#111143,#111144,#111145,#111146,#111147,#111148,
#111149,#111150,#111151,#111152,#111153,#111154,#111155,#111156,#111157,
#111158,#111159,#111160,#111161,#111162,#111163,#111164,#111165,#111166,
#111167,#111168,#111169,#111170,#111171,#111172,#111173,#111174,#111175,
#111176,#111177,#111178,#111179,#111180,#111181,#111182,#111183,#111184,
#111185,#111186,#111187,#111188,#111189,#111190,#111191,#111192,#111193,
#111194,#111195,#111196,#111197,#111198,#111199,#111200,#111201,#111202,
#111203,#111204,#111205,#111206,#111207,#111208,#111209,#111210,#111211,
#111212,#111213,#111214,#111215,#111216,#111217,#111218,#111219,#111220,
#111221,#111222,#111223,#111224,#111225,#111226,#111227,#111228,#111229,
#111230,#111231,#111232,#111233,#111234,#111235,#111236,#111237,#111238,
#111239,#111240,#111241,#111242,#111243,#111244,#111245,#111246,#111247,
#111248,#111249,#111250,#111251,#111252,#111253,#111254,#111255,#111256,
#111257,#111258,#111259,#111260,#111261,#111262,#111263,#111264,#111265,
#111266,#111267,#111268,#111269,#111270,#111271,#111272,#111273,#111274,
#111275,#111276,#111277,#111278,#111279,#111280,#111281,#111282,#111283,
#111284,#111285,#111286,#111287,#111288,#111289,#111290,#111291,#111292,
#111293,#111294,#111295),.UNSPECIFIED.,.F.,.F.,(4,2,2,2,2,2,2,2,2,2,2,2,
2,2,2,2,2,2,2,2,2,2,2,2,2,2,2,2,2,2,2,2,2,2,2,2,2,2,2,2,2,2,2,2,2,2,2,2,
2,2,2,2,2,2,2,2,2,2,2,2,2,2,2,2,2,2,2,2,2,2,2,2,2,2,2,2,2,2,2,2,2,2,2,2,
2,2,2,2,2,2,2,2,2,2,2,2,2,2,2,2,2,2,4),(-0.991228979995648,-0.983398525141886,
-0.979456642710194,-0.957084543893986,-0.953391681410358,-0.951301487728045,
-0.949480898246093,-0.947009965128886,-0.941205195284152,-0.932700889037199,
-0.902577581866334,-0.877732932348373,-0.871836529632574,-0.868280137956607,
-0.865050543334509,-0.860847197111809,-0.851646496958872,-0.838867619783047,
-0.816709866285661,-0.812536837742524,-0.790450015766714,-0.786758278114422,
-0.784668362291761,-0.782847758306616,-0.780376462084198,-0.774569326542554,
-0.766060187161313,-0.735897780977709,-0.711099256102759,-0.70520436345605,
-0.701648340474268,-0.698418737576984,-0.694214888018101,-0.685010987541685,
-0.67222589551464,-0.650071194126225,-0.645871628579444,-0.623820593002631,
-0.620129064887983,-0.618039222233125,-0.616218649486103,-0.613747352154976,
-0.607940022297441,-0.59943042488059,-0.569263605607128,-0.544471379517814,
-0.538576787116965,-0.535020875847633,-0.531791330477299,-0.527587492722427,
-0.518383349291159,-0.50559769303497,-0.483443794371823,-0.479241132714011,
-0.457194845616134,-0.45350341049653,-0.451413614944705,-0.449593079267466,
-0.447121826948301,-0.441314579481198,-0.432805081653765,-0.402638275129165,
-0.377847270257112,-0.371952822190027,-0.368396989513062,-0.365167510156696,
-0.360963750627403,-0.35175974563816,-0.338974254000734,-0.316820858173598,
-0.312617898578013,-0.290572590536178,-0.286881234186267,-0.28479148255478,
-0.28297098465775,-0.28049978297823,-0.274692651672097,-0.266183321492254,
-0.236017067984694,-0.21121909433528,-0.205328745936947,-0.201773832470939,
-0.198544203804684,-0.194338836121906,-0.185125279874042,-0.172321428276487,
-0.149944620177697,-0.145934869022723,-0.123953039086726,-0.120261997965209,
-0.118172342653606,-0.11635186992887,-0.113880623781306,-0.108073041451337,
-0.0818761625613097,-0.0549676433734573,-0.0424561965430678,-0.037607705320321,
-0.0346029847776142,-0.0313111534385748,-0.0280446219939228,-0.0236019538334248,
-0.000491633709745548),.UNSPECIFIED.);
#2808=B_SPLINE_CURVE_WITH_KNOTS('',3,(#111296,#111297,#111298,#111299,#111300,
#111301,#111302,#111303,#111304,#111305,#111306,#111307,#111308,#111309,
#111310,#111311),.UNSPECIFIED.,.F.,.F.,(4,2,2,2,2,2,2,4),(-2.09972660864104,
-2.05974670160645,-2.05394046144309,-2.05146911933196,-2.04964828326592,
-2.04755791888203,-2.04386491549341,-2.040918156169),.UNSPECIFIED.);
#2809=B_SPLINE_CURVE_WITH_KNOTS('',3,(#111313,#111314,#111315,#111316,#111317,
#111318,#111319,#111320,#111321,#111322,#111323,#111324,#111325),
 .UNSPECIFIED.,.F.,.F.,(4,3,3,3,4),(-48.1819144021787,-48.0723535020162,
-47.9625891120362,-47.8822972006122,-47.8286804139494),.UNSPECIFIED.);
#2810=B_SPLINE_CURVE_WITH_KNOTS('',3,(#111326,#111327,#111328,#111329,#111330,
#111331,#111332,#111333,#111334),.UNSPECIFIED.,.F.,.F.,(4,1,1,1,1,1,4),
(-47.8286738933328,-46.8847493422661,-45.88720148392,-44.8896536255739,
-43.8921057672278,-42.8945579088817,-41.8982186375431),.UNSPECIFIED.);
#2811=B_SPLINE_CURVE_WITH_KNOTS('',3,(#111339,#111340,#111341,#111342,#111343,
#111344,#111345,#111346,#111347,#111348,#111349,#111350,#111351,#111352,
#111353,#111354,#111355,#111356,#111357,#111358,#111359,#111360,#111361,
#111362,#111363,#111364,#111365,#111366,#111367,#111368,#111369,#111370,
#111371,#111372,#111373,#111374,#111375,#111376,#111377,#111378,#111379,
#111380,#111381,#111382,#111383,#111384,#111385,#111386,#111387,#111388,
#111389,#111390,#111391,#111392,#111393,#111394,#111395,#111396,#111397,
#111398,#111399,#111400,#111401,#111402,#111403,#111404,#111405,#111406,
#111407,#111408,#111409,#111410,#111411,#111412,#111413,#111414,#111415,
#111416,#111417,#111418,#111419,#111420,#111421,#111422,#111423,#111424,
#111425,#111426,#111427,#111428,#111429,#111430,#111431,#111432,#111433,
#111434,#111435,#111436,#111437,#111438,#111439,#111440,#111441,#111442,
#111443,#111444,#111445,#111446,#111447,#111448,#111449,#111450,#111451,
#111452,#111453,#111454,#111455,#111456,#111457,#111458,#111459,#111460,
#111461,#111462,#111463,#111464,#111465,#111466,#111467,#111468,#111469,
#111470,#111471,#111472,#111473,#111474,#111475,#111476,#111477,#111478,
#111479,#111480,#111481,#111482,#111483,#111484,#111485,#111486,#111487,
#111488,#111489,#111490,#111491,#111492,#111493,#111494,#111495,#111496,
#111497,#111498,#111499,#111500,#111501,#111502,#111503,#111504,#111505,
#111506,#111507,#111508,#111509,#111510,#111511,#111512,#111513,#111514,
#111515,#111516,#111517,#111518,#111519,#111520,#111521,#111522,#111523,
#111524,#111525,#111526,#111527,#111528,#111529,#111530,#111531,#111532,
#111533,#111534,#111535,#111536,#111537,#111538,#111539,#111540,#111541,
#111542,#111543,#111544),.UNSPECIFIED.,.F.,.F.,(4,2,2,2,2,2,2,2,2,2,2,2,
2,2,2,2,2,2,2,2,2,2,2,2,2,2,2,2,2,2,2,2,2,2,2,2,2,2,2,2,2,2,2,2,2,2,2,2,
2,2,2,2,2,2,2,2,2,2,2,2,2,2,2,2,2,2,2,2,2,2,2,2,2,2,2,2,2,2,2,2,2,2,2,2,
2,2,2,2,2,2,2,2,2,2,2,2,2,2,2,2,2,2,4),(-2.04103609068276,-2.04054941593494,
-2.03638930931414,-2.0331647411395,-2.02958535692507,-2.02358182574604,
-1.99511926535833,-1.97392481751964,-1.96230843101843,-1.95735522553996,
-1.95364416819374,-1.95155528640585,-1.94974748440359,-1.94741148929928,
-1.94255537899236,-1.91820227759977,-1.89602978402057,-1.88323506906757,
-1.87402665648728,-1.86982164406692,-1.86659153486022,-1.86303534382467,
-1.8571410669784,-1.83235929653687,-1.80220552606283,-1.7936985779156,-1.78789184163143,
-1.78542044466259,-1.78359962960099,-1.78150936084036,-1.77781668030054,
-1.75577195471019,-1.75154046932956,-1.72936523983956,-1.71657777544251,
-1.70737317358789,-1.7031688428402,-1.6999388394456,-1.69638234784322,-1.69048658081274,
-1.66565466455493,-1.6355449355966,-1.62704357161517,-1.62123961829485,
-1.61876869564025,-1.61694795087102,-1.6148574377532,-1.61116362569786,
-1.58879882328383,-1.58524470974868,-1.54571246651399,-1.53912333351665,
-1.53542081779393,-1.53221454242607,-1.52824867188314,-1.52207278698063,
-1.48219759365406,-1.4579488398525,-1.45372092376101,-1.4515406349014,-1.44973280232156,
-1.44739587751078,-1.44253495436364,-1.41929935626618,-1.39127773326232,
-1.37603376065766,-1.37099105646683,-1.36761365849837,-1.36433848231425,
-1.359650594565,-1.34819225379622,-1.30874080178992,-1.29615039921359,-1.28850557048288,
-1.28576053342001,-1.28389491523809,-1.28192192195282,-1.27867041630235,
-1.26727492418798,-1.23932148366182,-1.22049444413354,-1.20845951221053,
-1.20381302436367,-1.2005125021138,-1.19711750647856,-1.19198869851601,
-1.17725021657295,-1.13717559364277,-1.12766616554681,-1.12137410099424,
-1.11882423992933,-1.1169924699832,-1.11494287332612,-1.11133911386276,
-1.09484516582397,-1.05022618321615,-1.04074433564576,-1.03653821998532,
-1.03329840457556,-1.02977757796083,-1.02404865308315,-0.999989116222332,
-0.991228979995648),.UNSPECIFIED.);
#2812=B_SPLINE_CURVE_WITH_KNOTS('',3,(#111546,#111547,#111548,#111549,#111550),
 .UNSPECIFIED.,.F.,.F.,(4,1,4),(-41.8982186375431,-41.8970100505357,-41.5455025261802),
 .UNSPECIFIED.);
#2813=B_SPLINE_CURVE_WITH_KNOTS('',3,(#111551,#111552,#111553,#111554,#111555,
#111556,#111557,#111558,#111559,#111560,#111561,#111562,#111563,#111564,
#111565,#111566,#111567,#111568,#111569,#111570,#111571,#111572,#111573,
#111574,#111575,#111576,#111577,#111578,#111579,#111580,#111581,#111582,
#111583,#111584,#111585,#111586,#111587,#111588,#111589,#111590,#111591,
#111592,#111593,#111594,#111595,#111596,#111597,#111598,#111599,#111600,
#111601,#111602,#111603,#111604,#111605,#111606,#111607,#111608,#111609,
#111610,#111611,#111612,#111613,#111614,#111615,#111616,#111617,#111618,
#111619,#111620,#111621,#111622,#111623,#111624,#111625,#111626,#111627,
#111628,#111629,#111630,#111631,#111632,#111633,#111634,#111635,#111636,
#111637,#111638,#111639,#111640,#111641,#111642,#111643,#111644,#111645,
#111646,#111647,#111648,#111649,#111650,#111651,#111652,#111653,#111654,
#111655,#111656,#111657,#111658,#111659,#111660,#111661,#111662,#111663,
#111664,#111665,#111666,#111667,#111668,#111669,#111670,#111671,#111672,
#111673,#111674,#111675,#111676,#111677,#111678,#111679,#111680,#111681,
#111682,#111683,#111684,#111685,#111686,#111687,#111688,#111689,#111690,
#111691,#111692,#111693,#111694,#111695,#111696,#111697,#111698,#111699,
#111700,#111701,#111702,#111703,#111704,#111705,#111706,#111707,#111708,
#111709,#111710,#111711,#111712,#111713,#111714,#111715,#111716,#111717,
#111718,#111719,#111720,#111721,#111722,#111723,#111724,#111725,#111726,
#111727,#111728,#111729,#111730,#111731,#111732),.UNSPECIFIED.,.F.,.F.,
(4,2,2,2,2,2,2,2,2,2,2,2,2,2,2,2,2,2,2,2,2,2,2,2,2,2,2,2,2,2,2,2,2,2,2,
2,2,2,2,2,2,2,2,2,2,2,2,2,2,2,2,2,2,2,2,2,2,2,2,2,2,2,2,2,2,2,2,2,2,2,2,
2,2,2,2,2,2,2,2,2,2,2,2,2,2,2,2,2,2,2,4),(-2.10002519268564,-2.08483697761129,
-2.08076010466194,-2.07762104738156,-2.07451846365738,-2.07098911710212,
-2.06521692955025,-2.0412620342241,-2.01777849298488,-1.99968771820987,
-1.99513344827512,-1.99288873432114,-1.99108424964152,-1.98882263458331,
-1.98418126591821,-1.952465126248,-1.92007509049889,-1.91357429925143,-1.90989107678948,
-1.90668437857483,-1.90269576781476,-1.89643994721236,-1.85729541493937,
-1.8325934643758,-1.82829243893082,-1.82609788722754,-1.82429178973132,
-1.82197449252604,-1.81703932319838,-1.79232357174609,-1.76540498367543,
-1.75048509424041,-1.7454792391055,-1.74211019255397,-1.73883088408269,
-1.73411547576099,-1.72249744487282,-1.68671915254156,-1.66667894727015,
-1.66190728080995,-1.6596207041872,-1.65781576035324,-1.65559446835355,
-1.65115947511068,-1.61714294401893,-1.58677871070461,-1.58024841123671,
-1.5765590208519,-1.57335291429377,-1.56937278509163,-1.56314583015784,
-1.51766815206114,-1.49962009538053,-1.49507069463302,-1.49282688068273,
-1.49102232151892,-1.48875961312834,-1.48411283977927,-1.45250755888057,
-1.41953482703475,-1.41329846734298,-1.40967072118342,-1.40645683990408,
-1.40238490678399,-1.39584357224068,-1.35189453119925,-1.33795738379518,
-1.3297799453804,-1.32696700235239,-1.3250885142317,-1.32313712161813,-1.31998243146455,
-1.3096139964638,-1.27737813414181,-1.26048393738696,-1.24928687557285,
-1.24476223722666,-1.24148431207925,-1.23846428044022,-1.23352737292429,
-1.22038336666716,-1.18604904588521,-1.17156364698001,-1.16317838123143,
-1.160339904387,-1.15845628226542,-1.15651204482705,-1.15338999731221,-1.14332921274324,
-1.110922065625,-1.10898896929382),.UNSPECIFIED.);
#2814=B_SPLINE_CURVE_WITH_KNOTS('',3,(#111738,#111739,#111740,#111741,#111742,
#111743,#111744,#111745,#111746,#111747,#111748,#111749,#111750,#111751,
#111752,#111753,#111754,#111755,#111756,#111757,#111758,#111759,#111760,
#111761,#111762,#111763,#111764,#111765,#111766,#111767,#111768,#111769,
#111770,#111771,#111772,#111773,#111774,#111775,#111776,#111777,#111778,
#111779,#111780,#111781,#111782,#111783,#111784,#111785,#111786,#111787,
#111788,#111789,#111790,#111791,#111792,#111793,#111794,#111795,#111796,
#111797,#111798,#111799,#111800,#111801,#111802,#111803,#111804,#111805,
#111806,#111807,#111808,#111809,#111810,#111811,#111812,#111813,#111814,
#111815,#111816,#111817,#111818,#111819,#111820,#111821,#111822,#111823,
#111824,#111825,#111826,#111827,#111828,#111829,#111830,#111831,#111832,
#111833,#111834,#111835,#111836,#111837,#111838,#111839,#111840,#111841,
#111842,#111843,#111844,#111845,#111846,#111847,#111848,#111849,#111850,
#111851,#111852,#111853,#111854,#111855,#111856,#111857,#111858,#111859,
#111860,#111861,#111862,#111863,#111864,#111865,#111866,#111867,#111868,
#111869,#111870,#111871,#111872,#111873,#111874,#111875,#111876,#111877,
#111878,#111879,#111880,#111881,#111882,#111883,#111884,#111885,#111886,
#111887,#111888,#111889,#111890,#111891,#111892,#111893,#111894,#111895,
#111896,#111897,#111898,#111899,#111900,#111901,#111902,#111903,#111904,
#111905,#111906,#111907,#111908,#111909,#111910,#111911,#111912,#111913,
#111914,#111915,#111916,#111917,#111918,#111919,#111920,#111921,#111922,
#111923,#111924,#111925,#111926,#111927,#111928,#111929,#111930,#111931,
#111932,#111933,#111934,#111935,#111936,#111937,#111938,#111939,#111940,
#111941),.UNSPECIFIED.,.F.,.F.,(4,2,2,2,2,2,2,2,2,2,2,2,2,2,2,2,2,2,2,2,
2,2,2,2,2,2,2,2,2,2,2,2,2,2,2,2,2,2,2,2,2,2,2,2,2,2,2,2,2,2,2,2,2,2,2,2,
2,2,2,2,2,2,2,2,2,2,2,2,2,2,2,2,2,2,2,2,2,2,2,2,2,2,2,2,2,2,2,2,2,2,2,2,
2,2,2,2,2,2,2,2,2,4),(-0.991072633050833,-0.96959646129034,-0.944678711933136,
-0.938779703203733,-0.935222565921512,-0.931992816825189,-0.927790019527473,
-0.918593713735521,-0.905823630266165,-0.883660354338812,-0.879533898535787,
-0.857384837860035,-0.853692567617605,-0.851602427275458,-0.849781682743783,
-0.847310269425852,-0.841503183341829,-0.83299440984175,-0.802838021238123,
-0.778027638027302,-0.772131954079662,-0.768575570929295,-0.765345715084556,
-0.761141642746596,-0.751937708198761,-0.739152951492851,-0.716995831160663,
-0.712801403497338,-0.690741169910172,-0.687049306280662,-0.684959283183059,
-0.683138560034392,-0.680667067635752,-0.674859319450391,-0.66634914526616,
-0.636180864331508,-0.611385362667729,-0.605490241659954,-0.601934026026214,
-0.598704213415621,-0.594500040993152,-0.585295221045302,-0.57250867245532,
-0.550352855042596,-0.546150504741942,-0.524101486558228,-0.520409740294744,
-0.518319769752558,-0.5164990824572,-0.514027625432059,-0.50821990179108,
-0.499709710617032,-0.469540516995256,-0.444747298279119,-0.438852354245613,
-0.435296224142,-0.4320664757741,-0.427862367681426,-0.418657606361045,
-0.405871069855022,-0.383715818262087,-0.379512588450659,-0.357465334068013,
-0.353773669542994,-0.351683743586794,-0.349863093926034,-0.347391686372291,
-0.341584071870001,-0.333074034185266,-0.302905281117464,-0.2781127929516,
-0.272217978172867,-0.268661923461474,-0.265432241932784,-0.261228218498917,
-0.252023632543302,-0.239237331210165,-0.217082553343851,-0.192741218097675,
-0.187889348685176,-0.185554368323922,-0.183746834363978,-0.181565464383872,
-0.177331460424884,-0.152040531888699,-0.113463448222951,-0.107144837200523,
-0.103137301711613,-0.09992843993598,-0.0962569237434189,-0.0898147857437402,
-0.081850296451155,-0.0637884509081943,-0.0434746763101988,-0.0267336396863527,
-0.0214005651163529,-0.0190362188986482,-0.0172232213069115,-0.0155121918094399,
-0.0133884064464265,-0.0085363605493341,-0.000491425429689316),
 .UNSPECIFIED.);
#2815=B_SPLINE_CURVE_WITH_KNOTS('',3,(#111942,#111943,#111944,#111945,#111946,
#111947,#111948,#111949),.UNSPECIFIED.,.F.,.F.,(4,2,2,4),(-2.10007518485579,
-2.07578500626469,-2.04950247907538,-2.04103609068276),.UNSPECIFIED.);
#2816=B_SPLINE_CURVE_WITH_KNOTS('',3,(#111950,#111951,#111952,#111953,#111954,
#111955,#111956,#111957,#111958,#111959,#111960,#111961,#111962,#111963,
#111964,#111965,#111966,#111967,#111968,#111969,#111970,#111971,#111972,
#111973,#111974,#111975,#111976,#111977,#111978,#111979,#111980,#111981,
#111982,#111983,#111984,#111985,#111986,#111987,#111988,#111989,#111990,
#111991,#111992,#111993,#111994,#111995,#111996,#111997,#111998,#111999,
#112000,#112001,#112002,#112003,#112004,#112005,#112006,#112007,#112008,
#112009,#112010,#112011,#112012,#112013,#112014,#112015,#112016,#112017,
#112018,#112019,#112020,#112021,#112022,#112023,#112024,#112025,#112026,
#112027,#112028,#112029,#112030,#112031,#112032,#112033,#112034,#112035,
#112036,#112037,#112038,#112039,#112040,#112041,#112042,#112043,#112044,
#112045,#112046,#112047,#112048,#112049,#112050,#112051,#112052,#112053,
#112054,#112055,#112056,#112057,#112058,#112059,#112060,#112061,#112062,
#112063,#112064,#112065,#112066,#112067,#112068,#112069,#112070,#112071,
#112072,#112073,#112074,#112075,#112076,#112077,#112078,#112079,#112080,
#112081,#112082,#112083,#112084,#112085,#112086,#112087,#112088,#112089,
#112090,#112091,#112092,#112093,#112094,#112095,#112096,#112097,#112098,
#112099,#112100,#112101,#112102,#112103,#112104,#112105,#112106,#112107,
#112108,#112109,#112110,#112111,#112112,#112113,#112114,#112115,#112116,
#112117,#112118,#112119,#112120,#112121,#112122,#112123,#112124,#112125,
#112126,#112127,#112128,#112129,#112130,#112131,#112132,#112133,#112134,
#112135,#112136,#112137,#112138,#112139,#112140,#112141,#112142,#112143,
#112144,#112145,#112146,#112147,#112148,#112149,#112150,#112151,#112152,
#112153,#112154,#112155,#112156,#112157,#112158,#112159,#112160,#112161,
#112162,#112163,#112164,#112165),.UNSPECIFIED.,.F.,.F.,(4,2,2,2,2,2,2,2,
2,2,2,2,2,2,2,2,2,2,2,2,2,2,2,2,2,2,2,2,2,2,2,2,2,2,2,2,2,2,2,2,2,2,2,2,
2,2,2,2,2,2,2,2,2,2,2,2,2,2,2,2,2,2,2,2,2,2,2,2,2,2,2,2,2,2,2,2,2,2,2,2,
2,2,2,2,2,2,2,2,2,2,2,2,2,2,2,2,2,2,2,2,2,2,2,2,2,2,2,4),(-1.10898896929382,
-1.09390414405012,-1.08265174018518,-1.07811894887099,-1.07483967818805,
-1.07141429667589,-1.06613416613628,-1.04996520517984,-1.0212402150986,
-0.998263005053497,-0.994568306464459,-0.992478074967628,-0.990658203159696,
-0.988189333864909,-0.982394339314872,-0.97390909473674,-0.943933036608764,
-0.918914309952309,-0.913013793398772,-0.909457209904748,-0.906228918199669,
-0.902029422570637,-0.892846566427281,-0.88010087628242,-0.857930417791147,
-0.853947411233765,-0.831621684243135,-0.827929712412916,-0.825840116445942,
-0.824020149951253,-0.821550284817142,-0.815749137769432,-0.807251440203605,
-0.777176398388081,-0.752272961871932,-0.746375882345796,-0.742820075919541,
-0.739591670881674,-0.735390853465189,-0.726200112785101,-0.713439275221727,
-0.691273924862846,-0.687186923354377,-0.66498773247137,-0.661296297625461,
-0.659206847631488,-0.657386895388385,-0.654916898488686,-0.649114776814038,
-0.640615050839285,-0.610523207114743,-0.585640316679858,-0.579743951555371,
-0.576188344045373,-0.572959972959557,-0.568758989307938,-0.559566989587237,
-0.546803649935171,-0.524639678165284,-0.52053662343781,-0.498357892991948,
-0.494666607373074,-0.492577216645518,-0.490757298013267,-0.488287322619683,
-0.482485145323523,-0.473985241995247,-0.443891233805176,-0.419012051104974,
-0.413115901939393,-0.409560387486356,-0.406332077382064,-0.40213113934847,
-0.392939095878337,-0.380175574572132,-0.358012207634889,-0.353906715989856,
-0.331731579130073,-0.328040380704382,-0.325951035371735,-0.324131153449181,
-0.321661224087886,-0.315859138247062,-0.307359353831219,-0.27726552517987,
-0.252387354711478,-0.246491341308215,-0.242935902878609,-0.239707658104643,
-0.235506799779487,-0.226314908143842,-0.213551578653512,-0.191388689565356,
-0.167084324828378,-0.162128641449716,-0.159807692922468,-0.158001593951376,
-0.155810528171104,-0.151526072728155,-0.145862038301895,-0.131518066937979,
-0.0976948063532052,-0.0839718135821706,-0.0789591985615271,-0.0759258110012352,
-0.0726585076248189,-0.0681941961652964,-0.0594454700439993),
 .UNSPECIFIED.);
#2817=B_SPLINE_CURVE_WITH_KNOTS('',3,(#112170,#112171,#112172,#112173,#112174,
#112175,#112176,#112177,#112178,#112179,#112180,#112181,#112182,#112183,
#112184,#112185,#112186,#112187,#112188,#112189,#112190,#112191,#112192,
#112193,#112194,#112195,#112196,#112197,#112198,#112199,#112200,#112201,
#112202,#112203,#112204,#112205,#112206,#112207,#112208,#112209,#112210,
#112211,#112212,#112213,#112214,#112215,#112216,#112217,#112218,#112219,
#112220,#112221,#112222,#112223,#112224,#112225,#112226,#112227,#112228,
#112229,#112230,#112231,#112232,#112233,#112234,#112235,#112236,#112237,
#112238,#112239,#112240,#112241,#112242,#112243,#112244,#112245,#112246,
#112247,#112248,#112249,#112250,#112251,#112252,#112253,#112254,#112255,
#112256,#112257,#112258,#112259,#112260,#112261,#112262,#112263,#112264,
#112265,#112266,#112267,#112268,#112269,#112270,#112271,#112272,#112273,
#112274,#112275,#112276,#112277,#112278,#112279,#112280,#112281,#112282,
#112283,#112284,#112285,#112286,#112287,#112288,#112289,#112290,#112291,
#112292,#112293,#112294,#112295,#112296,#112297,#112298,#112299,#112300,
#112301,#112302,#112303,#112304,#112305,#112306,#112307,#112308,#112309,
#112310,#112311,#112312,#112313,#112314,#112315,#112316,#112317,#112318,
#112319,#112320,#112321,#112322,#112323,#112324,#112325,#112326,#112327,
#112328,#112329,#112330,#112331,#112332,#112333,#112334,#112335,#112336,
#112337,#112338,#112339,#112340,#112341,#112342,#112343,#112344,#112345,
#112346,#112347,#112348,#112349,#112350,#112351,#112352,#112353,#112354,
#112355,#112356,#112357,#112358,#112359,#112360,#112361,#112362,#112363,
#112364,#112365,#112366,#112367,#112368,#112369,#112370,#112371,#112372,
#112373,#112374,#112375,#112376,#112377,#112378,#112379,#112380,#112381,
#112382,#112383,#112384,#112385,#112386,#112387),.UNSPECIFIED.,.F.,.F.,
(4,2,2,2,2,2,2,2,2,2,2,2,2,2,2,2,2,2,2,2,2,2,2,2,2,2,2,2,2,2,2,2,2,2,2,
2,2,2,2,2,2,2,2,2,2,2,2,2,2,2,2,2,2,2,2,2,2,2,2,2,2,2,2,2,2,2,2,2,2,2,2,
2,2,2,2,2,2,2,2,2,2,2,2,2,2,2,2,2,2,2,2,2,2,2,2,2,2,2,2,2,2,2,2,2,2,2,2,
2,4),(-2.04074275515961,-2.03567152604733,-2.02716445779139,-2.02135773787919,
-2.01888641574544,-2.01706568248613,-2.01497553868023,-2.01128314570221,
-1.98926911488306,-1.9850164310383,-1.96284472739362,-1.95005174554692,
-1.94084437755,-1.93663968972439,-1.9334097697126,-1.92985372694521,-1.92395955310253,
-1.89918605886234,-1.86902859243381,-1.86052143735779,-1.85471468531573,
-1.85224336822928,-1.85042264604395,-1.84833252351285,-1.84464018655162,
-1.82263444372556,-1.81837603816447,-1.79620522974131,-1.78341054614093,
-1.77420230531716,-1.76999748347622,-1.76676756491554,-1.76321162793297,
-1.75731787718544,-1.73254290960076,-1.70238640492463,-1.69387940337996,
-1.68807273845119,-1.68560144623766,-1.68378073758281,-1.68169062500232,
-1.67799829360566,-1.65598740217461,-1.65173276604165,-1.62956162348202,
-1.6167681999837,-1.60756063565841,-1.60335594954367,-1.60012606690004,
-1.59657010125634,-1.59067614081617,-1.56589319683425,-1.53574400245634,
-1.52723795392019,-1.52143177291809,-1.51896057172024,-1.51713988495493,
-1.51504974491978,-1.51135725184818,-1.48929621441268,-1.48536041100123,
-1.4626987670826,-1.45003044035949,-1.4408884844046,-1.43669526989925,-1.4334668605366,
-1.42990516749844,-1.42398416471475,-1.39813346218269,-1.36890257175063,
-1.36051458655116,-1.3547671903463,-1.35230583284256,-1.35048638025678,
-1.34839062841658,-1.34467298790539,-1.32011159936551,-1.3021563694808,
-1.2859076860515,-1.27500355436319,-1.2705222754074,-1.26725098092633,-1.26380760725131,
-1.25844504228341,-1.24149757322114,-1.20380483139539,-1.18999041672601,
-1.18665648394224,-1.18466552957027,-1.18283127595654,-1.18015610877049,
-1.17350749935577,-1.14182673800396,-1.11243487519151,-1.10595171198221,
-1.10227129981328,-1.09906293422879,-1.0950668440296,-1.08878827885696,
-1.04984422365689,-1.04683088503486,-1.02403579115356,-1.02034098430461,
-1.01825025042474,-1.01642959072702,-1.01395909804104,-1.0081577202863,
-0.999660512452531,-0.991072633050833),.UNSPECIFIED.);
#2818=B_SPLINE_CURVE_WITH_KNOTS('',3,(#112389,#112390,#112391,#112392,#112393,
#112394,#112395,#112396,#112397,#112398),.UNSPECIFIED.,.F.,.F.,(4,2,2,2,
4),(-0.0594454700439993,-0.0573925871556223,-0.0413654807553726,-0.0230001708345523,
-0.000492308184977265),.UNSPECIFIED.);
#2819=B_SPLINE_CURVE_WITH_KNOTS('',3,(#112399,#112400,#112401,#112402,#112403,
#112404,#112405,#112406,#112407,#112408,#112409,#112410,#112411,#112412,
#112413,#112414,#112415,#112416,#112417,#112418,#112419,#112420,#112421,
#112422,#112423,#112424,#112425,#112426,#112427,#112428,#112429,#112430,
#112431,#112432,#112433,#112434,#112435,#112436,#112437,#112438,#112439,
#112440,#112441,#112442,#112443,#112444,#112445,#112446,#112447,#112448,
#112449,#112450,#112451,#112452,#112453,#112454,#112455,#112456,#112457,
#112458,#112459,#112460,#112461,#112462,#112463,#112464,#112465,#112466,
#112467,#112468,#112469,#112470,#112471,#112472,#112473,#112474,#112475,
#112476,#112477,#112478,#112479,#112480,#112481,#112482,#112483,#112484,
#112485,#112486,#112487,#112488,#112489,#112490,#112491,#112492,#112493,
#112494,#112495,#112496,#112497,#112498,#112499,#112500,#112501,#112502,
#112503,#112504,#112505,#112506,#112507,#112508,#112509,#112510,#112511,
#112512,#112513,#112514,#112515,#112516,#112517,#112518,#112519,#112520,
#112521,#112522,#112523,#112524,#112525,#112526,#112527,#112528,#112529,
#112530,#112531,#112532,#112533,#112534,#112535,#112536,#112537,#112538,
#112539,#112540,#112541,#112542,#112543,#112544,#112545,#112546,#112547,
#112548,#112549,#112550,#112551,#112552,#112553,#112554,#112555,#112556,
#112557,#112558,#112559,#112560,#112561,#112562,#112563,#112564,#112565,
#112566,#112567,#112568,#112569,#112570,#112571,#112572,#112573,#112574,
#112575,#112576,#112577,#112578),.UNSPECIFIED.,.F.,.F.,(4,2,2,2,2,2,2,2,
2,2,2,2,2,2,2,2,2,2,2,2,2,2,2,2,2,2,2,2,2,2,2,2,2,2,2,2,2,2,2,2,2,2,2,2,
2,2,2,2,2,2,2,2,2,2,2,2,2,2,2,2,2,2,2,2,2,2,2,2,2,2,2,2,2,2,2,2,2,2,2,2,
2,2,2,2,2,2,2,2,2,4),(-2.10013203330852,-2.09759133984381,-2.09518859571947,
-2.09332411054461,-2.09161915840831,-2.08965654530031,-2.08645037965014,
-2.0755270373007,-2.05064612886903,-2.01943176311094,-2.01318289201795,
-2.00955246284213,-2.0063389283563,-2.00227112178533,-1.99574418275092,
-1.95172132127184,-1.9329171861995,-1.92828117442073,-1.92602048956945,
-1.92421587321082,-1.9219699096027,-1.91740976479451,-1.88478270033251,
-1.85269560506489,-1.84645767066889,-1.84282950840846,-1.83961555528948,
-1.83554393342112,-1.82900394740178,-1.79321394901279,-1.7657959211102,
-1.76142857768398,-1.75922066872306,-1.75741515094544,-1.75511328725454,
-1.75026105181688,-1.72215353043311,-1.68631970579769,-1.67990532972719,
-1.67624006501671,-1.67303120972583,-1.66901651982944,-1.66267215261942,
-1.61774987856709,-1.59941743577169,-1.59483504998088,-1.59258473951846,
-1.59078012093854,-1.58852379390723,-1.58391040438392,-1.5517110974274,
-1.51966212114605,-1.51321232924929,-1.50953957456019,-1.50633146505512,
-1.50232730979013,-1.49601914469461,-1.45736350723146,-1.43223071045562,
-1.42795099687785,-1.42576062150971,-1.42395410072611,-1.42163132223635,
-1.41666728715779,-1.39171226642141,-1.36499522660805,-1.35013547676979,
-1.34513605508485,-1.34176810199038,-1.33848742013393,-1.3345124571801,
-1.32674197855803,-1.28357657343487,-1.27055340575811,-1.26273399565356,
-1.25996646627421,-1.25809685991349,-1.25637384538573,-1.25339846029372,
-1.2446077475669,-1.21144404316211,-1.19391386449296,-1.18243428876635,
-1.17786780202552,-1.17458238365523,-1.17157103797963,-1.16668374991637,
-1.15389899343611,-1.11922703591869,-1.10915862425753),.UNSPECIFIED.);
#2820=B_SPLINE_CURVE_WITH_KNOTS('',3,(#112584,#112585,#112586,#112587,#112588,
#112589,#112590,#112591,#112592,#112593,#112594,#112595,#112596,#112597,
#112598,#112599,#112600,#112601,#112602,#112603,#112604,#112605,#112606,
#112607,#112608,#112609,#112610,#112611,#112612,#112613,#112614,#112615,
#112616,#112617,#112618,#112619,#112620,#112621,#112622,#112623,#112624,
#112625,#112626,#112627,#112628,#112629,#112630,#112631,#112632,#112633,
#112634,#112635,#112636,#112637,#112638,#112639,#112640,#112641,#112642,
#112643,#112644,#112645,#112646,#112647,#112648,#112649,#112650,#112651,
#112652,#112653,#112654,#112655,#112656,#112657,#112658,#112659,#112660,
#112661,#112662,#112663,#112664,#112665,#112666,#112667,#112668,#112669,
#112670,#112671,#112672,#112673,#112674,#112675,#112676,#112677,#112678,
#112679,#112680,#112681,#112682,#112683,#112684,#112685,#112686,#112687,
#112688,#112689,#112690,#112691,#112692,#112693,#112694,#112695,#112696,
#112697,#112698,#112699,#112700,#112701,#112702,#112703,#112704,#112705,
#112706,#112707,#112708,#112709,#112710,#112711,#112712,#112713,#112714,
#112715,#112716,#112717,#112718,#112719,#112720,#112721,#112722,#112723,
#112724,#112725,#112726,#112727,#112728,#112729,#112730,#112731,#112732,
#112733,#112734,#112735,#112736,#112737,#112738,#112739,#112740,#112741,
#112742,#112743,#112744,#112745,#112746,#112747,#112748,#112749,#112750,
#112751,#112752,#112753,#112754,#112755,#112756,#112757,#112758,#112759,
#112760,#112761,#112762,#112763,#112764,#112765,#112766,#112767,#112768,
#112769),.UNSPECIFIED.,.F.,.F.,(4,2,2,2,2,2,2,2,2,2,2,2,2,2,2,2,2,2,2,2,
2,2,2,2,2,2,2,2,2,2,2,2,2,2,2,2,2,2,2,2,2,2,2,2,2,2,2,2,2,2,2,2,2,2,2,2,
2,2,2,2,2,2,2,2,2,2,2,2,2,2,2,2,2,2,2,2,2,2,2,2,2,2,2,2,2,2,2,2,2,2,2,2,
4),(-0.991436796285106,-0.990873237000083,-0.959694946413161,-0.926078997117896,
-0.921600444224151,-0.919369945546251,-0.917564377032642,-0.915285551485311,
-0.910557842618623,-0.890932952857412,-0.856354081040102,-0.843442690479383,
-0.838536579266132,-0.835521133852138,-0.832237100385693,-0.827683376769096,
-0.816297010993809,-0.79898216555433,-0.766179185054227,-0.756857710136171,
-0.753817933684952,-0.752081983920873,-0.750221674330721,-0.747504937187699,
-0.740071449256155,-0.727991669949014,-0.692510586278405,-0.677347736849901,
-0.672174775334541,-0.668770596327473,-0.665476034563454,-0.660862943687471,
-0.64906549850864,-0.630803816212285,-0.604262694454322,-0.59091843245324,
-0.587505034000453,-0.585496666053101,-0.583649279181806,-0.58100373777366,
-0.574076853981764,-0.534863724499452,-0.511962982677311,-0.506149512588472,
-0.502610585636146,-0.499375985242109,-0.495135846774915,-0.485723229113441,
-0.441218178082258,-0.424551201922221,-0.420941449638163,-0.418890514763205,
-0.417059109091292,-0.41451182058211,-0.408236580046016,-0.398761750883128,
-0.359162915599921,-0.343957269007202,-0.338779983990421,-0.335374982044542,
-0.332081120105781,-0.32747151259717,-0.315697938945907,-0.297491903760072,
-0.271096452551978,-0.257545955725953,-0.254119349432689,-0.252108144248591,
-0.250262091054276,-0.247623996452157,-0.240748029607144,-0.197089898625644,
-0.178075038189032,-0.172508447131054,-0.169022087870296,-0.165770138875317,
-0.161408622714191,-0.151266142330518,-0.136625311781776,-0.116709169310579,
-0.0933595528039877,-0.0884373357017265,-0.0861220891024877,-0.0843156172162147,
-0.0821181388438962,-0.0778042765599675,-0.0720898137195765,-0.0575422230559856,
-0.0173414858727192,-0.0084227495550825,-0.00426260359061961,-0.00206331470985932,
-0.000491892551814876),.UNSPECIFIED.);
#2821=B_SPLINE_CURVE_WITH_KNOTS('',3,(#112770,#112771,#112772,#112773,#112774,
#112775,#112776,#112777,#112778,#112779,#112780,#112781),.UNSPECIFIED.,
 .F.,.F.,(4,2,2,2,2,4),(-2.09967868133144,-2.09854857464352,-2.09658609675878,
-2.09129232863807,-2.07408596053682,-2.04074275515961),.UNSPECIFIED.);
#2822=B_SPLINE_CURVE_WITH_KNOTS('',3,(#112782,#112783,#112784,#112785,#112786,
#112787,#112788,#112789,#112790,#112791,#112792,#112793,#112794,#112795,
#112796,#112797,#112798,#112799,#112800,#112801,#112802,#112803,#112804,
#112805,#112806,#112807,#112808,#112809,#112810,#112811,#112812,#112813,
#112814,#112815,#112816,#112817,#112818,#112819,#112820,#112821,#112822,
#112823,#112824,#112825,#112826,#112827,#112828,#112829,#112830,#112831,
#112832,#112833,#112834,#112835,#112836,#112837,#112838,#112839,#112840,
#112841,#112842,#112843,#112844,#112845,#112846,#112847,#112848,#112849,
#112850,#112851,#112852,#112853,#112854,#112855,#112856,#112857,#112858,
#112859,#112860,#112861,#112862,#112863,#112864,#112865,#112866,#112867,
#112868,#112869,#112870,#112871,#112872,#112873,#112874,#112875,#112876,
#112877,#112878,#112879,#112880,#112881,#112882,#112883,#112884,#112885,
#112886,#112887,#112888,#112889,#112890,#112891,#112892,#112893,#112894,
#112895,#112896,#112897,#112898,#112899,#112900,#112901,#112902,#112903,
#112904,#112905,#112906,#112907,#112908,#112909,#112910,#112911,#112912,
#112913,#112914,#112915,#112916,#112917,#112918,#112919,#112920,#112921,
#112922,#112923,#112924,#112925,#112926,#112927,#112928,#112929,#112930,
#112931,#112932,#112933,#112934,#112935,#112936,#112937,#112938,#112939,
#112940,#112941,#112942,#112943,#112944,#112945,#112946,#112947,#112948,
#112949,#112950,#112951,#112952,#112953,#112954,#112955,#112956,#112957,
#112958,#112959,#112960,#112961,#112962,#112963,#112964,#112965,#112966,
#112967,#112968,#112969,#112970,#112971,#112972,#112973,#112974,#112975,
#112976,#112977,#112978,#112979,#112980,#112981,#112982,#112983,#112984,
#112985,#112986,#112987,#112988,#112989,#112990,#112991,#112992,#112993,
#112994,#112995),.UNSPECIFIED.,.F.,.F.,(4,2,2,2,2,2,2,2,2,2,2,2,2,2,2,2,
2,2,2,2,2,2,2,2,2,2,2,2,2,2,2,2,2,2,2,2,2,2,2,2,2,2,2,2,2,2,2,2,2,2,2,2,
2,2,2,2,2,2,2,2,2,2,2,2,2,2,2,2,2,2,2,2,2,2,2,2,2,2,2,2,2,2,2,2,2,2,2,2,
2,2,2,2,2,2,2,2,2,2,2,2,2,2,2,2,2,2,4),(-1.10915862425753,-1.09957210592967,
-1.09484179727824,-1.09256296141637,-1.09075803538217,-1.08852922264832,
-1.08405680732055,-1.05036363381549,-1.02133928243396,-1.01460206567239,
-1.01047363790624,-1.00725366183995,-1.00365891852038,-0.997579277411207,
-0.963305891606409,-0.932875775063358,-0.928144245981082,-0.925865214356625,
-0.924060331650434,-0.921831817932682,-0.91736073514768,-0.911371024271775,
-0.895666606520307,-0.856854632074688,-0.848073379039098,-0.843929396786707,
-0.840699048998021,-0.837149698070751,-0.831283659047388,-0.804123490951329,
-0.787193995873125,-0.764574926695985,-0.760881652399191,-0.758791692521814,
-0.756971675552142,-0.754502098642413,-0.748703198242827,-0.740210208396916,
-0.71017447799593,-0.685222364066652,-0.679323562997927,-0.675767258293627,
-0.672538742150467,-0.668338269719849,-0.659150365976129,-0.64639521976583,
-0.624226550142749,-0.62017969728572,-0.597929761116141,-0.594237932509529,
-0.592148321706141,-0.590328273987628,-0.587858207029735,-0.582056182221982,
-0.57355683436559,-0.543470115374455,-0.518577910446857,-0.512680972733161,
-0.509125111514382,-0.505896568002824,-0.501695443119888,-0.4925034882971,
-0.479740509337504,-0.457574892404385,-0.45347790684298,-0.431290064530191,
-0.427598538235355,-0.425509021254347,-0.423688999964353,-0.421218895037618,
-0.415416456431553,-0.406916209673484,-0.376821623946476,-0.351939660087849,
-0.346043131569558,-0.342487404384609,-0.3392589112882,-0.335057749733842,
-0.325865279395831,-0.31310121748992,-0.290936514004643,-0.286831906161462,
-0.264654111038677,-0.260962695081183,-0.258873228272477,-0.257053240419455,
-0.254583167787781,-0.248780750098684,-0.240280482221082,-0.210184964095294,
-0.185286677485233,-0.17940013856418,-0.175846579580633,-0.172617612476978,
-0.168412324610933,-0.159195857633063,-0.14638583744142,-0.124240829247567,
-0.119957852905529,-0.0980203369861578,-0.0943299017410368,-0.0922406803234062,
-0.0904206881795931,-0.0879503157389445,-0.0821458916829303,-0.0736415108296685,
-0.0594688639043352),.UNSPECIFIED.);
#2823=B_SPLINE_CURVE_WITH_KNOTS('',3,(#113000,#113001,#113002,#113003,#113004,
#113005,#113006,#113007,#113008,#113009,#113010,#113011,#113012,#113013,
#113014,#113015,#113016,#113017,#113018,#113019,#113020,#113021,#113022,
#113023,#113024,#113025,#113026,#113027,#113028,#113029,#113030,#113031,
#113032,#113033,#113034,#113035,#113036,#113037,#113038,#113039,#113040,
#113041,#113042,#113043,#113044,#113045,#113046,#113047,#113048,#113049,
#113050,#113051,#113052,#113053,#113054,#113055,#113056,#113057,#113058,
#113059,#113060,#113061,#113062,#113063,#113064,#113065,#113066,#113067,
#113068,#113069,#113070,#113071,#113072,#113073,#113074,#113075,#113076,
#113077,#113078,#113079,#113080,#113081,#113082,#113083,#113084,#113085,
#113086,#113087,#113088,#113089,#113090,#113091,#113092,#113093,#113094,
#113095,#113096,#113097,#113098,#113099,#113100,#113101,#113102,#113103,
#113104,#113105,#113106,#113107,#113108,#113109,#113110,#113111,#113112,
#113113,#113114,#113115,#113116,#113117,#113118,#113119,#113120,#113121,
#113122,#113123,#113124,#113125,#113126,#113127,#113128,#113129,#113130,
#113131,#113132,#113133,#113134,#113135,#113136,#113137,#113138,#113139,
#113140,#113141,#113142,#113143,#113144,#113145,#113146,#113147,#113148,
#113149,#113150,#113151,#113152,#113153,#113154,#113155,#113156,#113157,
#113158,#113159,#113160,#113161,#113162,#113163,#113164,#113165,#113166,
#113167,#113168,#113169,#113170,#113171,#113172,#113173,#113174,#113175,
#113176,#113177,#113178,#113179,#113180,#113181,#113182,#113183,#113184,
#113185,#113186,#113187,#113188,#113189,#113190,#113191,#113192,#113193,
#113194,#113195,#113196,#113197,#113198,#113199,#113200,#113201),
 .UNSPECIFIED.,.F.,.F.,(4,2,2,2,2,2,2,2,2,2,2,2,2,2,2,2,2,2,2,2,2,2,2,2,
2,2,2,2,2,2,2,2,2,2,2,2,2,2,2,2,2,2,2,2,2,2,2,2,2,2,2,2,2,2,2,2,2,2,2,2,
2,2,2,2,2,2,2,2,2,2,2,2,2,2,2,2,2,2,2,2,2,2,2,2,2,2,2,2,2,2,2,2,2,2,2,2,
2,2,2,2,4),(-2.04139270538101,-2.03966297411823,-2.02143180415736,-2.00964813248972,
-2.00503685889942,-2.00174255800547,-1.99873880357734,-1.99467736075789,
-1.98440851892978,-1.94730249018665,-1.93205365570485,-1.92338634940782,
-1.92051332622025,-1.91862200772741,-1.91691962021657,-1.91405434050606,
-1.90611416035622,-1.87553438979116,-1.84674360174858,-1.8402635075626,
-1.83658349869667,-1.83337472229398,-1.82937712371914,-1.8230941722876,
-1.77786825265898,-1.7596877588869,-1.75512201921192,-1.75287437799442,
-1.75106895911633,-1.74880786954449,-1.74417282306118,-1.71230093028663,
-1.67943786113303,-1.67326966219273,-1.66965522303164,-1.66643730007494,
-1.662338577063,-1.6557079612845,-1.6221760222767,-1.60094644885751,-1.59381020216466,
-1.58870815112307,-1.5863594754392,-1.58472269424159,-1.58262594992414,
-1.57890472223976,-1.55423117001562,-1.53631271472844,-1.52010697864088,
-1.51266553036367,-1.50655413693591,-1.5029517122836,-1.49973158725669,
-1.49561225750841,-1.48688771423292,-1.44790822996209,-1.4321652724848,
-1.42332094406712,-1.42042725510494,-1.4185316067398,-1.41660032053548,
-1.41354051948908,-1.40404758720192,-1.37130702441355,-1.35405837832461,
-1.3427020929498,-1.33815264483204,-1.33486928295805,-1.33185282123776,
-1.32694128349747,-1.31399101295887,-1.27947185340709,-1.26493477226171,
-1.25652928216197,-1.2536875615668,-1.25180268839609,-1.25009442727391,
-1.24719790207228,-1.23902589273424,-1.20546757144143,-1.18769173174651,
-1.17980499814139,-1.17341179203,-1.16974998873271,-1.16653914534787,-1.16251529544889,
-1.15614267358652,-1.11813033375047,-1.09239961558534,-1.08816315014852,
-1.08598099494507,-1.08417310520198,-1.08183801958286,-1.07698710341559,
-1.05053791714071,-1.01457274599916,-1.00803889506752,-1.0039681775919,
-1.00075312290307,-0.997121773519071,-0.991436796285106),.UNSPECIFIED.);
#2824=B_SPLINE_CURVE_WITH_KNOTS('',3,(#113203,#113204,#113205,#113206,#113207,
#113208,#113209,#113210,#113211,#113212,#113213,#113214,#113215,#113216,
#113217,#113218),.UNSPECIFIED.,.F.,.F.,(4,2,2,2,2,2,2,4),(-0.0594688639043352,
-0.0326218974226338,-0.0172456618715315,-0.0121571034009043,-0.00873146617640893,
-0.0056783958676778,-0.00301214665044019,-0.000491717384029574),
 .UNSPECIFIED.);
#2825=B_SPLINE_CURVE_WITH_KNOTS('',3,(#113219,#113220,#113221,#113222,#113223,
#113224,#113225,#113226,#113227,#113228,#113229,#113230,#113231,#113232,
#113233,#113234,#113235,#113236,#113237,#113238,#113239,#113240,#113241,
#113242,#113243,#113244,#113245,#113246,#113247,#113248,#113249,#113250,
#113251,#113252,#113253,#113254,#113255,#113256,#113257,#113258,#113259,
#113260,#113261,#113262,#113263,#113264,#113265,#113266,#113267,#113268,
#113269,#113270,#113271,#113272,#113273,#113274,#113275,#113276,#113277,
#113278,#113279,#113280,#113281,#113282,#113283,#113284,#113285,#113286,
#113287,#113288,#113289,#113290,#113291,#113292,#113293,#113294,#113295,
#113296,#113297,#113298,#113299,#113300,#113301,#113302,#113303,#113304,
#113305,#113306,#113307,#113308,#113309,#113310,#113311,#113312,#113313,
#113314,#113315,#113316,#113317,#113318,#113319,#113320,#113321,#113322,
#113323,#113324,#113325,#113326,#113327,#113328,#113329,#113330,#113331,
#113332,#113333,#113334,#113335,#113336,#113337,#113338,#113339,#113340,
#113341,#113342,#113343,#113344,#113345,#113346,#113347,#113348,#113349,
#113350,#113351,#113352,#113353,#113354,#113355,#113356,#113357,#113358,
#113359,#113360,#113361,#113362,#113363,#113364,#113365,#113366,#113367,
#113368,#113369,#113370,#113371,#113372,#113373,#113374,#113375,#113376,
#113377,#113378,#113379,#113380,#113381,#113382,#113383,#113384,#113385,
#113386,#113387,#113388,#113389,#113390,#113391,#113392,#113393,#113394,
#113395,#113396,#113397,#113398,#113399,#113400,#113401,#113402,#113403,
#113404,#113405,#113406,#113407,#113408,#113409,#113410,#113411,#113412,
#113413,#113414,#113415,#113416),.UNSPECIFIED.,.F.,.F.,(4,2,2,2,2,2,2,2,
2,2,2,2,2,2,2,2,2,2,2,2,2,2,2,2,2,2,2,2,2,2,2,2,2,2,2,2,2,2,2,2,2,2,2,2,
2,2,2,2,2,2,2,2,2,2,2,2,2,2,2,2,2,2,2,2,2,2,2,2,2,2,2,2,2,2,2,2,2,2,2,2,
2,2,2,2,2,2,2,2,2,2,2,2,2,2,2,2,2,2,4),(-2.09998383653095,-2.09276187432922,
-2.04931092824687,-2.03658895661001,-2.02889094500792,-2.02613933279381,
-2.02427283064363,-2.02254617878129,-2.01955204162526,-2.01060856563066,
-1.97753960942744,-1.96007063848493,-1.95226964552112,-1.94767579772682,
-1.94347840532854,-1.94025013518944,-1.93669198300295,-1.9307850344639,
-1.90594868743843,-1.8758586343696,-1.86736023334257,-1.86155808195318,
-1.8590879122204,-1.85726773514597,-1.85517795460678,-1.8514857180737,-1.82936862835452,
-1.82518912950081,-1.80300783675231,-1.79023437904749,-1.78103762161853,
-1.77683543925848,-1.77360656362741,-1.77005081890408,-1.76415518870671,
-1.73929248468774,-1.70920669243844,-1.70070885790683,-1.69490699728263,
-1.69243688480716,-1.69061673545728,-1.6885269901847,-1.6848347622449,-1.66270347852578,
-1.65853515017027,-1.63635304366883,-1.62358165866505,-1.61438602368991,
-1.61018409769296,-1.60695532093096,-1.60339958893912,-1.59750375582772,
-1.57263101302232,-1.54255420729113,-1.5340575657574,-1.52825632492363,
-1.52578634791339,-1.52396623991239,-1.52187646339001,-1.51818406568841,
-1.49600411278805,-1.49187417032022,-1.46968956732065,-1.45692526173437,
-1.44773331499792,-1.44353202078688,-1.44030331261454,-1.43674723900525,
-1.43084984323837,-1.40592346679972,-1.37589430228139,-1.36740369301914,
-1.36160543321638,-1.35913592714686,-1.35731582326821,-1.35522559545671,
-1.35153153995683,-1.3289102431425,-1.31198036598065,-1.29385744310058,
-1.28212104668599,-1.27751751088763,-1.27422548739567,-1.27122163501549,
-1.26715676047054,-1.25686043765124,-1.21606900355127,-1.20331764375839,
-1.19560775446792,-1.19285459455618,-1.19098783047074,-1.1890185731371,
-1.18578181812122,-1.174543811827,-1.14647477958792,-1.12759897919872,-1.11941581829126,
-1.11283811745965,-1.10919012835353),.UNSPECIFIED.);
#2826=B_SPLINE_CURVE_WITH_KNOTS('',3,(#113422,#113423,#113424,#113425,#113426,
#113427,#113428,#113429,#113430,#113431,#113432,#113433,#113434,#113435,
#113436,#113437,#113438,#113439,#113440,#113441),.UNSPECIFIED.,.F.,.F.,
(4,2,2,2,2,2,2,2,2,4),(-0.0593009426660634,-0.0417078351293523,-0.0297985383297815,
-0.0265125915388237,-0.0245388090859083,-0.0228313209054354,-0.020979224624226,
-0.0184296819045016,-0.0123504048007048,-0.000511197579002299),
 .UNSPECIFIED.);
#2827=B_SPLINE_CURVE_WITH_KNOTS('',3,(#113443,#113444,#113445,#113446,#113447,
#113448,#113449,#113450,#113451,#113452,#113453,#113454,#113455,#113456,
#113457,#113458,#113459,#113460,#113461,#113462,#113463,#113464,#113465,
#113466,#113467,#113468,#113469,#113470,#113471,#113472,#113473,#113474,
#113475,#113476,#113477,#113478,#113479,#113480,#113481,#113482,#113483,
#113484,#113485,#113486,#113487,#113488,#113489,#113490,#113491,#113492,
#113493,#113494,#113495,#113496,#113497,#113498,#113499,#113500,#113501,
#113502,#113503,#113504,#113505,#113506,#113507,#113508,#113509,#113510,
#113511,#113512,#113513,#113514,#113515,#113516,#113517,#113518,#113519,
#113520,#113521,#113522,#113523,#113524,#113525,#113526,#113527,#113528,
#113529,#113530,#113531,#113532,#113533,#113534,#113535,#113536,#113537,
#113538,#113539,#113540,#113541,#113542,#113543,#113544,#113545,#113546,
#113547,#113548,#113549,#113550,#113551),.UNSPECIFIED.,.F.,.F.,(4,3,3,3,
3,3,3,3,3,3,3,3,3,3,3,3,3,3,3,3,3,3,3,3,3,3,3,3,3,3,3,3,3,3,3,3,4),(-3.84638326322101,
-3.73817304815445,-3.63008307936253,-3.5220705202799,-3.41409265518859,
-3.30603153662545,-3.1979326333689,-3.08963571181038,-2.99264357503826,
-2.88276587336857,-2.77180710378402,-2.66222615391215,-2.55271033211294,
-2.44321911573495,-2.33118826597426,-2.22155434572583,-2.108325031209,-1.99509571669217,
-1.88634894910193,-1.77524881275745,-1.6668012593166,-1.55841692512387,
-1.45005363583211,-1.3369271914606,-1.22839986838443,-1.11978478227982,
-1.01096831546058,-0.997547858346086,-0.884786287810336,-0.772265546586226,
-0.659886764440191,-0.547616383400315,-0.435420994753685,-0.323232042127002,
-0.211056351513135,-0.0987924848427668,0.),.UNSPECIFIED.);
#2828=B_SPLINE_CURVE_WITH_KNOTS('',3,(#113554,#113555,#113556,#113557,#113558,
#113559,#113560,#113561,#113562,#113563,#113564,#113565,#113566,#113567,
#113568,#113569,#113570,#113571,#113572,#113573,#113574,#113575,#113576,
#113577,#113578,#113579,#113580,#113581,#113582,#113583,#113584,#113585,
#113586,#113587,#113588,#113589,#113590,#113591,#113592,#113593,#113594,
#113595,#113596,#113597,#113598,#113599,#113600,#113601,#113602,#113603,
#113604,#113605,#113606,#113607,#113608,#113609,#113610,#113611,#113612,
#113613,#113614,#113615,#113616,#113617,#113618,#113619,#113620,#113621,
#113622,#113623,#113624,#113625,#113626,#113627,#113628,#113629,#113630,
#113631,#113632,#113633,#113634,#113635,#113636,#113637,#113638,#113639,
#113640,#113641,#113642,#113643,#113644,#113645,#113646,#113647,#113648,
#113649,#113650,#113651,#113652,#113653,#113654,#113655,#113656,#113657,
#113658,#113659,#113660,#113661,#113662,#113663,#113664,#113665,#113666,
#113667,#113668,#113669,#113670,#113671,#113672,#113673,#113674,#113675,
#113676,#113677,#113678,#113679,#113680,#113681,#113682,#113683,#113684,
#113685,#113686,#113687,#113688,#113689,#113690,#113691,#113692,#113693,
#113694,#113695,#113696,#113697,#113698,#113699,#113700,#113701,#113702,
#113703,#113704,#113705,#113706,#113707,#113708,#113709,#113710,#113711,
#113712,#113713,#113714,#113715,#113716,#113717,#113718,#113719,#113720,
#113721,#113722,#113723,#113724,#113725,#113726,#113727),.UNSPECIFIED.,
 .F.,.F.,(4,2,2,2,2,2,2,2,2,2,2,2,2,2,2,2,2,2,2,2,2,2,2,2,2,2,2,2,2,2,2,
2,2,2,2,2,2,2,2,2,2,2,2,2,2,2,2,2,2,2,2,2,2,2,2,2,2,2,2,2,2,2,2,2,2,2,2,
2,2,2,2,2,2,2,2,2,2,2,2,2,2,2,2,2,2,2,4),(-1.97974873256733,-1.97958676484942,
-1.97600317519578,-1.94100267198266,-1.91218505529882,-1.90564031731873,
-1.9019167803576,-1.89866458475273,-1.8946035001476,-1.88819277658925,-1.84516230481906,
-1.8268530631516,-1.8222403185383,-1.81995237340242,-1.81811430865174,-1.81580717439324,
-1.8109982706693,-1.78203085302772,-1.74742922907714,-1.74088809205394,
-1.73718328526767,-1.73395784525245,-1.72994542773198,-1.72365032994016,
-1.67819898302672,-1.66000371616132,-1.65543013307975,-1.65317771385458,
-1.65137444696111,-1.64912511855927,-1.64451610078777,-1.61236237640466,
-1.58034694595528,-1.57386903681223,-1.57020392136783,-1.5670165564695,
-1.56305737434019,-1.55537141625159,-1.50598651336961,-1.49589568419349,
-1.48933969801489,-1.48676018964219,-1.48493100819737,-1.48290460177259,
-1.47940855239251,-1.46481199898505,-1.43463085145165,-1.41942457669491,
-1.40900371157641,-1.40459236030265,-1.40132744991803,-1.39784947166614,
-1.39234398857133,-1.37407308225253,-1.33797363397781,-1.32438480726431,
-1.32105986807721,-1.3190667047929,-1.31722705114186,-1.31496256381588,
-1.30937921898769,-1.27674225740609,-1.25095248133566,-1.24195152052659,
-1.23778188066505,-1.23455497790459,-1.23097808993293,-1.22499105122535,
-1.19589143082964,-1.1693394209813,-1.15744545711871,-1.15425398771316,
-1.15229412002961,-1.1504436913603,-1.14767706816644,-1.14044464862549,
-1.10927529676266,-1.08421404337261,-1.07522899956281,-1.07106527631507,
-1.06784257160284,-1.06427006922935,-1.058290027436,-1.02896945181402,-1.00698497526331,
-0.991250018193274,-0.991241672647406),.UNSPECIFIED.);
#2829=B_SPLINE_CURVE_WITH_KNOTS('',3,(#113733,#113734,#113735,#113736,#113737,
#113738,#113739,#113740,#113741,#113742,#113743,#113744,#113745,#113746,
#113747,#113748,#113749,#113750,#113751,#113752,#113753,#113754,#113755,
#113756,#113757,#113758,#113759,#113760,#113761,#113762,#113763,#113764,
#113765,#113766,#113767,#113768,#113769,#113770,#113771,#113772,#113773,
#113774,#113775,#113776,#113777,#113778,#113779,#113780,#113781,#113782,
#113783,#113784,#113785,#113786,#113787,#113788,#113789,#113790,#113791,
#113792,#113793,#113794,#113795,#113796,#113797,#113798,#113799,#113800,
#113801,#113802,#113803,#113804),.UNSPECIFIED.,.F.,.F.,(4,2,2,2,2,2,2,2,
2,2,2,2,2,2,2,2,2,2,2,2,2,2,2,2,2,2,2,2,2,2,2,2,2,2,2,4),(-0.358760731569834,
-0.357588714416537,-0.340406456573176,-0.336834571924863,-0.334774389493125,
-0.333018019472239,-0.330672679582775,-0.325139584554118,-0.317082275139463,
-0.290068178055794,-0.258861954651025,-0.252959280030101,-0.249499198163838,
-0.246422960364231,-0.242515505307593,-0.234373396072529,-0.201704582837242,
-0.174054602645336,-0.16974968847418,-0.167567493002712,-0.165748347082853,
-0.163743231260215,-0.160392353643154,-0.146811877258289,-0.113203671548509,
-0.086995627305843,-0.0805483037650247,-0.0766221547171091,-0.0730213521738901,
-0.0682621214379093,-0.0572868734598832,-0.0321802295361602,-0.00778597364073482,
-0.0034563959859211,-0.00158264500599872,-5.87679558657036E-5),
 .UNSPECIFIED.);
#2830=B_SPLINE_CURVE_WITH_KNOTS('',3,(#113807,#113808,#113809,#113810,#113811,
#113812,#113813,#113814,#113815,#113816,#113817,#113818,#113819,#113820,
#113821,#113822,#113823,#113824,#113825,#113826,#113827,#113828,#113829,
#113830,#113831,#113832,#113833,#113834,#113835,#113836,#113837,#113838,
#113839,#113840,#113841,#113842,#113843,#113844,#113845,#113846,#113847,
#113848,#113849,#113850,#113851,#113852,#113853,#113854,#113855,#113856,
#113857,#113858,#113859,#113860,#113861,#113862,#113863,#113864,#113865,
#113866,#113867,#113868,#113869,#113870,#113871,#113872,#113873,#113874,
#113875,#113876,#113877,#113878,#113879,#113880,#113881,#113882,#113883,
#113884,#113885,#113886,#113887,#113888,#113889,#113890,#113891,#113892,
#113893,#113894,#113895,#113896,#113897,#113898,#113899,#113900,#113901,
#113902,#113903,#113904,#113905,#113906,#113907,#113908,#113909,#113910,
#113911,#113912,#113913,#113914,#113915,#113916,#113917,#113918,#113919,
#113920,#113921,#113922,#113923,#113924,#113925,#113926),.UNSPECIFIED.,
 .F.,.F.,(4,2,2,2,2,2,2,2,2,2,2,2,2,2,2,2,2,2,2,2,2,2,2,2,2,2,2,2,2,2,2,
2,2,2,2,2,2,2,2,2,2,2,2,2,2,2,2,2,2,2,2,2,2,2,2,2,2,2,2,4),(-1.75478037324913,
-1.75157699880387,-1.72680890478214,-1.70436781523072,-1.69162498350517,
-1.68241391197646,-1.67818088615358,-1.67491705814343,-1.67131004331383,
-1.66529325591384,-1.63706718497493,-1.61632460687294,-1.60530876936184,
-1.59831925399475,-1.59563330166604,-1.59375272143998,-1.59171445466058,
-1.58821527004706,-1.57390064920759,-1.54363468613963,-1.52844718498748,
-1.51803625632712,-1.51361751510249,-1.51034227165868,-1.50684850913675,
-1.50130739417962,-1.4828116871778,-1.44660558241407,-1.43297165383395,
-1.4296425648391,-1.42764863798456,-1.42581830637429,-1.42314642011918,
-1.41647814742639,-1.38016276823827,-1.36286107158849,-1.35149411852575,
-1.34695871618315,-1.34369238877248,-1.34069673237757,-1.33583180407813,
-1.32310319370023,-1.28487643314327,-1.27240852083981,-1.26482026775864,
-1.26209371528085,-1.2602390155936,-1.25826751071241,-1.25502208329052,
-1.24369353186293,-1.21196073855142,-1.19542895810817,-1.1843900026814,
-1.17988418445069,-1.17660488891761,-1.17357302530719,-1.16859195814515,
-1.15515324807121,-1.12121414778627,-1.10916128661629),.UNSPECIFIED.);
#2831=B_SPLINE_CURVE_WITH_KNOTS('',3,(#113931,#113932,#113933,#113934,#113935,
#113936,#113937,#113938,#113939,#113940,#113941,#113942,#113943,#113944,
#113945,#113946,#113947,#113948,#113949,#113950,#113951,#113952,#113953,
#113954,#113955,#113956,#113957,#113958,#113959,#113960,#113961,#113962,
#113963,#113964,#113965,#113966,#113967,#113968,#113969,#113970,#113971,
#113972,#113973,#113974,#113975,#113976,#113977,#113978,#113979,#113980,
#113981,#113982,#113983,#113984,#113985,#113986,#113987,#113988,#113989,
#113990,#113991,#113992,#113993,#113994,#113995,#113996,#113997,#113998,
#113999,#114000,#114001,#114002,#114003,#114004,#114005,#114006,#114007,
#114008,#114009,#114010,#114011,#114012,#114013,#114014,#114015,#114016,
#114017,#114018,#114019,#114020,#114021,#114022,#114023,#114024,#114025,
#114026,#114027,#114028,#114029,#114030,#114031,#114032,#114033,#114034,
#114035,#114036,#114037,#114038,#114039,#114040,#114041,#114042,#114043,
#114044,#114045,#114046,#114047,#114048,#114049,#114050,#114051,#114052,
#114053,#114054,#114055,#114056,#114057,#114058,#114059,#114060,#114061,
#114062,#114063,#114064,#114065,#114066,#114067,#114068,#114069,#114070,
#114071,#114072,#114073,#114074,#114075,#114076,#114077,#114078,#114079,
#114080,#114081,#114082,#114083,#114084,#114085,#114086,#114087,#114088,
#114089,#114090,#114091,#114092,#114093,#114094,#114095,#114096,#114097,
#114098,#114099,#114100,#114101,#114102,#114103,#114104,#114105,#114106,
#114107,#114108,#114109,#114110,#114111,#114112,#114113,#114114,#114115,
#114116,#114117,#114118,#114119,#114120,#114121,#114122,#114123,#114124,
#114125,#114126,#114127,#114128,#114129,#114130,#114131,#114132,#114133,
#114134),.UNSPECIFIED.,.F.,.F.,(4,2,2,2,2,2,2,2,2,2,2,2,2,2,2,2,2,2,2,2,
2,2,2,2,2,2,2,2,2,2,2,2,2,2,2,2,2,2,2,2,2,2,2,2,2,2,2,2,2,2,2,2,2,2,2,2,
2,2,2,2,2,2,2,2,2,2,2,2,2,2,2,2,2,2,2,2,2,2,2,2,2,2,2,2,2,2,2,2,2,2,2,2,
2,2,2,2,2,2,2,2,2,4),(-1.40833512650497,-1.40069098176856,-1.38787474148805,
-1.36573398785996,-1.36142474486855,-1.33952291888054,-1.33583168467958,
-1.33374174701002,-1.33192195928846,-1.3294522385009,-1.32364851669501,
-1.31514499277648,-1.28502396579597,-1.26015341685752,-1.25425797890798,
-1.2507032120157,-1.24747582068171,-1.2432764626835,-1.23408973699226,-1.22133535388231,
-1.19916987032535,-1.19515532407055,-1.17287860500929,-1.1691874323788,
-1.16709828604177,-1.16527782164968,-1.16280676494455,-1.15700274439171,
-1.14850063352328,-1.11840425844881,-1.09350544645594,-1.08760505451081,
-1.08404663296064,-1.08081539307692,-1.07661012370494,-1.06740554943454,
-1.05461967175103,-1.03247886802765,-1.02833096610872,-1.00625015383823,
-1.002556444386,-1.00046480350253,-0.998639633790782,-0.996158960985884,
-0.990319553033095,-0.981749001120184,-0.951072859652514,-0.927051797544536,
-0.921182418045694,-0.917628104023132,-0.91439107207908,-0.910164325254045,
-0.900852081647703,-0.856495923805341,-0.839524843366962,-0.835941140859538,
-0.833875333054979,-0.832057501469606,-0.829560052009865,-0.82353535656955,
-0.814571150674254,-0.780470453505149,-0.759646769933166,-0.753989719912425,
-0.750496765690896,-0.747272530583065,-0.742999853831133,-0.733312013273571,
-0.719565278171568,-0.698733462106393,-0.695051892923753,-0.672835017627635,
-0.669152369497,-0.667069703583026,-0.665247106699071,-0.662770814571849,
-0.656963692222392,-0.648464165926929,-0.61847180994102,-0.593341832579235,
-0.587413589620244,-0.583837432304097,-0.580589073195544,-0.576359462345094,
-0.567087876225144,-0.554183574582817,-0.532300339159159,-0.528708008494463,
-0.506205857281313,-0.502493257712591,-0.500387207557482,-0.498530469081444,
-0.495988404157892,-0.489933486740911,-0.45408616114669,-0.428439332762879,
-0.422521926965401,-0.418935970626578,-0.415666728570026,-0.411391351813892,
-0.401935764996784,-0.358760731569834),.UNSPECIFIED.);
#2832=B_SPLINE_CURVE_WITH_KNOTS('',3,(#114135,#114136,#114137,#114138,#114139,
#114140,#114141,#114142,#114143,#114144,#114145,#114146,#114147,#114148,
#114149,#114150,#114151,#114152,#114153,#114154,#114155,#114156,#114157,
#114158,#114159,#114160,#114161,#114162,#114163,#114164,#114165,#114166,
#114167,#114168,#114169,#114170,#114171,#114172,#114173,#114174,#114175,
#114176,#114177,#114178,#114179,#114180,#114181,#114182,#114183,#114184,
#114185,#114186,#114187,#114188,#114189,#114190,#114191,#114192,#114193,
#114194,#114195,#114196,#114197,#114198,#114199,#114200,#114201,#114202,
#114203,#114204,#114205,#114206,#114207,#114208,#114209,#114210,#114211,
#114212,#114213,#114214,#114215,#114216,#114217,#114218,#114219,#114220,
#114221,#114222,#114223,#114224,#114225,#114226,#114227,#114228,#114229,
#114230,#114231,#114232,#114233,#114234,#114235,#114236,#114237,#114238,
#114239,#114240,#114241,#114242,#114243,#114244,#114245,#114246,#114247,
#114248,#114249,#114250,#114251,#114252,#114253,#114254,#114255,#114256,
#114257,#114258,#114259,#114260,#114261,#114262,#114263,#114264,#114265,
#114266,#114267,#114268,#114269,#114270,#114271,#114272,#114273,#114274,
#114275,#114276,#114277,#114278,#114279,#114280,#114281,#114282,#114283,
#114284,#114285,#114286,#114287,#114288,#114289,#114290,#114291,#114292,
#114293,#114294,#114295,#114296,#114297,#114298,#114299,#114300,#114301,
#114302,#114303,#114304,#114305,#114306,#114307,#114308,#114309,#114310,
#114311,#114312,#114313,#114314,#114315,#114316,#114317,#114318,#114319,
#114320,#114321,#114322,#114323,#114324,#114325,#114326,#114327,#114328,
#114329,#114330,#114331,#114332,#114333,#114334,#114335,#114336,#114337,
#114338,#114339,#114340,#114341,#114342,#114343,#114344,#114345,#114346,
#114347,#114348,#114349,#114350,#114351,#114352),.UNSPECIFIED.,.F.,.F.,
(4,2,2,2,2,2,2,2,2,2,2,2,2,2,2,2,2,2,2,2,2,2,2,2,2,2,2,2,2,2,2,2,2,2,2,
2,2,2,2,2,2,2,2,2,2,2,2,2,2,2,2,2,2,2,2,2,2,2,2,2,2,2,2,2,2,2,2,2,2,2,2,
2,2,2,2,2,2,2,2,2,2,2,2,2,2,2,2,2,2,2,2,2,2,2,2,2,2,2,2,2,2,2,2,2,2,2,2,
2,4),(-1.10916128661629,-1.1068588965783,-1.09852086339214,-1.09568326149892,
-1.09379611024995,-1.09208378124754,-1.08917097179547,-1.08088503629987,
-1.05059279909283,-1.02100922286385,-1.01506309006501,-1.01149527084022,
-1.00826692931509,-1.00415127566961,-0.995201602349336,-0.952436159590886,
-0.939454819477996,-0.931651380621814,-0.928885506458069,-0.927016041622359,
-0.925051224025353,-0.921832934565604,-0.910792820809623,-0.878916105003638,
-0.854168053021811,-0.848277080273857,-0.844723588494016,-0.841496478241594,
-0.837296265876073,-0.828102846067531,-0.81533632466192,-0.793159236903368,
-0.789112411061338,-0.76685967816142,-0.763168754363048,-0.761080091243742,
-0.759260204867692,-0.756790362652809,-0.750991517565072,-0.742499079037655,
-0.712471105207643,-0.68750691684465,-0.681606342784592,-0.678048810090404,
-0.674819040719495,-0.67061668530613,-0.66142315451214,-0.648657768073693,
-0.626502235929794,-0.622360398120677,-0.600235247130315,-0.596543063041667,
-0.594452738884643,-0.592631974565978,-0.590160416588509,-0.584351596258526,
-0.575839087038066,-0.54565089345244,-0.520879544049048,-0.514985742609532,
-0.511430149464382,-0.50820080629351,-0.503997126759067,-0.494793038202192,
-0.482007620330627,-0.459848371053637,-0.455649576826883,-0.433590902091073,
-0.429899478776002,-0.427809829004612,-0.425989620877812,-0.423519099229366,
-0.417714756101117,-0.409210824442457,-0.379088111536539,-0.354238613563417,
-0.348342834854102,-0.344787126252018,-0.341558371680152,-0.337356466024755,
-0.328160622381927,-0.31539037793302,-0.293226968063353,-0.289097820187359,
-0.266951706979895,-0.26326023877772,-0.261170691826645,-0.259350472016111,
-0.256879936560673,-0.251076035023471,-0.24257310800339,-0.212458684830971,
-0.187581296624008,-0.181695527966676,-0.178141746162406,-0.174912124997448,
-0.170705316048839,-0.161482509779152,-0.148660816668445,-0.126636332986425,
-0.122694017829648,-0.100322083409943,-0.0966296442692932,-0.0945397429891191,
-0.092719507624359,-0.0902491906182205,-0.0844464131731029,-0.0759456808677562,
-0.0594792545525924),.UNSPECIFIED.);
#2833=B_SPLINE_CURVE_WITH_KNOTS('',3,(#114357,#114358,#114359,#114360,#114361,
#114362,#114363,#114364,#114365,#114366,#114367,#114368,#114369,#114370,
#114371,#114372,#114373,#114374,#114375,#114376,#114377,#114378,#114379,
#114380,#114381,#114382,#114383,#114384,#114385,#114386,#114387,#114388,
#114389,#114390,#114391,#114392,#114393,#114394,#114395,#114396,#114397,
#114398,#114399,#114400,#114401,#114402,#114403,#114404,#114405,#114406,
#114407,#114408,#114409,#114410,#114411,#114412,#114413,#114414,#114415,
#114416,#114417,#114418,#114419,#114420,#114421,#114422,#114423,#114424,
#114425,#114426,#114427,#114428,#114429,#114430,#114431,#114432,#114433,
#114434,#114435,#114436,#114437,#114438,#114439,#114440,#114441,#114442,
#114443,#114444,#114445,#114446,#114447,#114448,#114449,#114450,#114451,
#114452,#114453,#114454,#114455,#114456,#114457,#114458,#114459,#114460,
#114461,#114462,#114463,#114464,#114465,#114466,#114467,#114468,#114469,
#114470,#114471,#114472,#114473,#114474,#114475,#114476,#114477,#114478,
#114479,#114480,#114481,#114482,#114483,#114484,#114485,#114486,#114487,
#114488,#114489,#114490,#114491,#114492,#114493,#114494,#114495,#114496,
#114497,#114498,#114499,#114500,#114501,#114502,#114503,#114504,#114505,
#114506,#114507,#114508,#114509,#114510,#114511,#114512,#114513,#114514,
#114515,#114516,#114517,#114518,#114519,#114520,#114521,#114522,#114523,
#114524,#114525,#114526,#114527,#114528,#114529,#114530,#114531,#114532,
#114533,#114534,#114535,#114536,#114537,#114538,#114539,#114540,#114541,
#114542,#114543,#114544,#114545,#114546,#114547,#114548,#114549,#114550,
#114551,#114552,#114553,#114554,#114555,#114556,#114557,#114558,#114559,
#114560,#114561,#114562,#114563,#114564,#114565,#114566,#114567,#114568,
#114569,#114570),.UNSPECIFIED.,.F.,.F.,(4,2,2,2,2,2,2,2,2,2,2,2,2,2,2,2,
2,2,2,2,2,2,2,2,2,2,2,2,2,2,2,2,2,2,2,2,2,2,2,2,2,2,2,2,2,2,2,2,2,2,2,2,
2,2,2,2,2,2,2,2,2,2,2,2,2,2,2,2,2,2,2,2,2,2,2,2,2,2,2,2,2,2,2,2,2,2,2,2,
2,2,2,2,2,2,2,2,2,2,2,2,2,2,2,2,2,2,4),(-2.45793897795708,-2.45615588549777,
-2.43177484350015,-2.422770787873,-2.41860144465758,-2.41537554387078,-2.4118005758735,
-2.40581874108697,-2.3757599172176,-2.35166693513045,-2.34279824546252,
-2.33681354770945,-2.33431273065983,-2.33248795396218,-2.33041355500885,
-2.32679191692295,-2.30813529131414,-2.26748366486948,-2.25705557726181,
-2.25297054985888,-2.24996125765374,-2.24667237344482,-2.24209027298485,
-2.23050772719489,-2.21274425295155,-2.17924202763386,-2.17105341531066,
-2.16815489995836,-2.16644635967471,-2.164562085245,-2.16172271163067,-2.15333558004233,
-2.13884522533033,-2.10449960657346,-2.09134549528806,-2.08640611142508,
-2.08338484027012,-2.08010577929559,-2.07557986682592,-2.06438030184675,
-2.0474837375862,-2.0152778102446,-2.00492997510858,-2.00177688807338,-1.99982539359666,
-1.99794570017531,-1.9951292220909,-1.98692889493808,-1.97293182164206,
-1.95227316982027,-1.92671054005153,-1.92079468807121,-1.91723381909934,
-1.91400471938894,-1.9098085300844,-1.90065100469766,-1.88795498508286,
-1.86517631931624,-1.86233811018274,-1.8393949897911,-1.83569957863761,
-1.83360867524846,-1.83178810163029,-1.8293179304999,-1.82351788735836,
-1.81502314868086,-1.78497591757588,-1.76004335518708,-1.7541442494569,
-1.75058722713463,-1.74735768969231,-1.74315531823811,-1.73396055598287,
-1.72119305852158,-1.69903174454589,-1.69491721654909,-1.6727573919502,
-1.66906533783053,-1.66697531287706,-1.6651545875148,-1.662683134092,-1.65687582763822,
-1.64836658292982,-1.6182055819652,-1.59340262799116,-1.58750704379221,
-1.58395055907596,-1.58072049703089,-1.57651597597271,-1.56731015486083,
-1.55452164405268,-1.53237067567287,-1.52816814108077,-1.50612815974973,
-1.50243625349907,-1.50034606538026,-1.49852471174085,-1.49605182893906,
-1.49023903029735,-1.48171913363843,-1.45146950699641,-1.42679775646766,
-1.42090631466174,-1.41735031433094,-1.41411938081594,-1.40991180845125,
-1.40833512650497),.UNSPECIFIED.);
#2834=B_SPLINE_CURVE_WITH_KNOTS('',3,(#114572,#114573,#114574,#114575,#114576,
#114577,#114578,#114579,#114580,#114581,#114582,#114583,#114584,#114585,
#114586,#114587),.UNSPECIFIED.,.F.,.F.,(4,2,2,2,2,2,2,4),(-0.0594792545525924,
-0.0341344864849067,-0.019390033663532,-0.0142709737956861,-0.010878840635614,
-0.00783988566160054,-0.00425775618985681,-0.000493435409444853),
 .UNSPECIFIED.);
#2835=B_SPLINE_CURVE_WITH_KNOTS('',3,(#114588,#114589,#114590,#114591,#114592,
#114593,#114594,#114595,#114596,#114597,#114598,#114599,#114600,#114601,
#114602,#114603,#114604,#114605,#114606,#114607,#114608,#114609,#114610,
#114611,#114612,#114613,#114614,#114615,#114616,#114617,#114618,#114619,
#114620,#114621,#114622,#114623,#114624,#114625,#114626,#114627,#114628,
#114629,#114630,#114631,#114632,#114633,#114634,#114635,#114636,#114637,
#114638,#114639,#114640,#114641,#114642,#114643,#114644,#114645,#114646,
#114647,#114648,#114649,#114650,#114651,#114652,#114653,#114654,#114655,
#114656,#114657,#114658,#114659,#114660,#114661,#114662,#114663,#114664,
#114665,#114666,#114667,#114668,#114669,#114670,#114671,#114672,#114673,
#114674,#114675,#114676,#114677,#114678,#114679,#114680,#114681,#114682,
#114683,#114684,#114685,#114686,#114687,#114688,#114689,#114690,#114691,
#114692,#114693,#114694,#114695,#114696,#114697,#114698,#114699,#114700,
#114701,#114702,#114703,#114704,#114705,#114706,#114707,#114708,#114709,
#114710,#114711,#114712,#114713,#114714,#114715,#114716,#114717,#114718,
#114719,#114720,#114721,#114722,#114723,#114724,#114725,#114726,#114727,
#114728,#114729,#114730,#114731,#114732,#114733,#114734,#114735,#114736,
#114737,#114738,#114739,#114740,#114741,#114742,#114743,#114744,#114745,
#114746,#114747,#114748,#114749,#114750,#114751,#114752,#114753,#114754,
#114755,#114756,#114757,#114758,#114759,#114760,#114761,#114762,#114763,
#114764,#114765,#114766,#114767,#114768,#114769,#114770,#114771,#114772,
#114773,#114774,#114775,#114776,#114777),.UNSPECIFIED.,.F.,.F.,(4,2,2,2,
2,2,2,2,2,2,2,2,2,2,2,2,2,2,2,2,2,2,2,2,2,2,2,2,2,2,2,2,2,2,2,2,2,2,2,2,
2,2,2,2,2,2,2,2,2,2,2,2,2,2,2,2,2,2,2,2,2,2,2,2,2,2,2,2,2,2,2,2,2,2,2,2,
2,2,2,2,2,2,2,2,2,2,2,2,2,2,2,2,2,2,4),(-2.09963543973955,-2.09246016825572,
-2.05214587400277,-2.03411221550204,-2.0295640431354,-2.02732018798611,
-2.02551524420154,-2.02325158294973,-2.01860131270733,-1.98705841801055,
-1.9541653926891,-1.94958605950917,-1.94539874969976,-1.94217144551413,
-1.93860753350505,-1.93267464846004,-1.90794177813569,-1.87780813839569,
-1.86930410252211,-1.86349904491058,-1.86102823590822,-1.85920781240094,
-1.85711798013648,-1.85342612918277,-1.83147633674116,-1.8010425187358,
-1.78514656111749,-1.78003536689141,-1.77664449778827,-1.77338010703456,
-1.76874907804524,-1.75760008563841,-1.71777425874744,-1.70513848736707,
-1.6974754699745,-1.69472835409607,-1.6928626086916,-1.69089090727048,-1.68764412572019,
-1.6762975315996,-1.64458222116772,-1.62808152417664,-1.6205551223639,-1.61438996085163,
-1.61077684469602,-1.60755984276245,-1.60346196095107,-1.59683205799805,
-1.56331925309136,-1.54207957645314,-1.53494210168959,-1.52983971505768,
-1.52749139392588,-1.52585506336916,-1.52375922601036,-1.52004037660899,
-1.4954233957183,-1.49447237304159,-1.47404277590453,-1.4598737595407,-1.4499648701824,
-1.44564178967674,-1.44239598064091,-1.43889483500637,-1.43325706269018,
-1.41312913216072,-1.37865819240984,-1.36965775011106,-1.36360937822551,
-1.36109867339561,-1.35927297595365,-1.35720482846713,-1.35360935419312,
-1.33576538698223,-1.30453320706305,-1.2919951550504,-1.28292211503648,
-1.27874144678629,-1.27551509896906,-1.2719480514783,-1.26599986233491,
-1.23868978064015,-1.21068491649701,-1.19848378036798,-1.195268059158,-1.19330318875485,
-1.19145535674275,-1.18914899894471,-1.18330057417155,-1.15091055774667,
-1.12524857048015,-1.11623326674394,-1.11206281319984,-1.10883774977028,
-1.10881952756263),.UNSPECIFIED.);
#2836=B_SPLINE_CURVE_WITH_KNOTS('',3,(#114782,#114783,#114784,#114785,#114786,
#114787,#114788,#114789,#114790,#114791,#114792,#114793,#114794,#114795,
#114796,#114797,#114798,#114799,#114800,#114801,#114802,#114803,#114804,
#114805,#114806,#114807,#114808,#114809,#114810,#114811,#114812,#114813,
#114814,#114815,#114816,#114817,#114818,#114819,#114820,#114821,#114822,
#114823,#114824,#114825,#114826,#114827,#114828,#114829,#114830,#114831,
#114832,#114833,#114834,#114835,#114836,#114837,#114838,#114839,#114840,
#114841,#114842,#114843,#114844,#114845,#114846,#114847,#114848,#114849,
#114850,#114851,#114852,#114853,#114854,#114855,#114856,#114857,#114858,
#114859,#114860,#114861,#114862,#114863,#114864,#114865,#114866,#114867,
#114868,#114869,#114870,#114871,#114872,#114873,#114874,#114875,#114876,
#114877,#114878,#114879,#114880,#114881,#114882,#114883,#114884,#114885,
#114886,#114887,#114888,#114889,#114890,#114891,#114892,#114893,#114894,
#114895,#114896,#114897,#114898,#114899,#114900,#114901,#114902,#114903,
#114904,#114905,#114906,#114907,#114908,#114909,#114910,#114911,#114912,
#114913,#114914,#114915,#114916,#114917,#114918,#114919,#114920,#114921,
#114922,#114923,#114924,#114925,#114926,#114927,#114928,#114929,#114930,
#114931,#114932,#114933,#114934,#114935,#114936,#114937,#114938,#114939,
#114940,#114941,#114942,#114943,#114944,#114945,#114946,#114947,#114948,
#114949,#114950,#114951,#114952,#114953,#114954,#114955,#114956,#114957,
#114958,#114959,#114960,#114961,#114962,#114963,#114964,#114965,#114966,
#114967,#114968,#114969,#114970,#114971,#114972,#114973,#114974,#114975,
#114976,#114977,#114978,#114979,#114980,#114981),.UNSPECIFIED.,.F.,.F.,
(4,2,2,2,2,2,2,2,2,2,2,2,2,2,2,2,2,2,2,2,2,2,2,2,2,2,2,2,2,2,2,2,2,2,2,
2,2,2,2,2,2,2,2,2,2,2,2,2,2,2,2,2,2,2,2,2,2,2,2,2,2,2,2,2,2,2,2,2,2,2,2,
2,2,2,2,2,2,2,2,2,2,2,2,2,2,2,2,2,2,2,2,2,2,2,2,2,2,2,2,4),(-3.50773961833004,
-3.50421851324702,-3.50140422409568,-3.49952512581685,-3.49781174931706,
-3.49488732096498,-3.48650041962016,-3.45309269569678,-3.43540885820288,
-3.42754817280637,-3.42117159836907,-3.41751368105993,-3.41430296631894,
-3.4102749156194,-3.4038866306081,-3.359189777365,-3.34075014175589,-3.33615510086918,
-3.33390199359663,-3.33209689304258,-3.32984205206654,-3.32523807673874,
-3.2929181834735,-3.2610020422903,-3.25454568610755,-3.25087097401481,-3.24766212901855,
-3.24365828861399,-3.23735299799631,-3.19867971531989,-3.1734976500103,
-3.16926497027186,-3.1670837683819,-3.16527607312614,-3.16294044288485,
-3.1580857852602,-3.13510956096479,-3.1077653779617,-3.091761871451,-3.08663914360522,
-3.08324551126884,-3.07998200934138,-3.07535831287171,-3.06426076892656,
-3.02795873720578,-3.01292965956498,-3.00434285530471,-3.00147959659049,
-2.99959045940212,-2.9976518215459,-2.99455738830669,-2.98475461330809,
-2.95564198409292,-2.93634341310926,-2.92411398166636,-2.91944073329676,
-2.91613541498287,-2.9131437018507,-2.90913185905408,-2.89916841868622,
-2.85339010162891,-2.84349418300337,-2.83702142701227,-2.83444358813303,
-2.83260750499024,-2.83057082863891,-2.82702687572773,-2.81144639395432,
-2.7817423009744,-2.76692582871821,-2.75669858123361,-2.75232310330469,
-2.74906874623193,-2.74558729376446,-2.74004489986829,-2.72107097154034,
-2.67738520586696,-2.67049253016324,-2.6678519606445,-2.66600540600267,
-2.66399501833808,-2.66057239144719,-2.64708876071342,-2.62062747577998,
-2.60239359734701,-2.59438178236599,-2.58791028038803,-2.58423206844143,
-2.58102308927683,-2.57702290942623,-2.57073114778078,-2.52555606454651,
-2.51212497284043,-2.50414335298965,-2.50135431986496,-2.49947999037183,
-2.49776079997681,-2.49480737267149,-2.4861971077323,-2.45793897795708),
 .UNSPECIFIED.);
#2837=B_SPLINE_CURVE_WITH_KNOTS('',3,(#114982,#114983,#114984,#114985,#114986,
#114987,#114988,#114989,#114990,#114991,#114992,#114993,#114994,#114995,
#114996,#114997,#114998,#114999,#115000,#115001,#115002,#115003,#115004,
#115005,#115006,#115007,#115008,#115009,#115010,#115011,#115012,#115013,
#115014,#115015,#115016,#115017,#115018,#115019,#115020,#115021,#115022,
#115023,#115024,#115025,#115026,#115027,#115028,#115029,#115030,#115031,
#115032,#115033,#115034,#115035,#115036,#115037,#115038,#115039,#115040,
#115041,#115042,#115043,#115044,#115045,#115046,#115047,#115048,#115049,
#115050,#115051,#115052,#115053,#115054,#115055,#115056,#115057,#115058,
#115059,#115060,#115061,#115062,#115063,#115064,#115065,#115066,#115067,
#115068,#115069,#115070,#115071,#115072,#115073,#115074,#115075,#115076,
#115077,#115078,#115079,#115080,#115081,#115082,#115083,#115084,#115085,
#115086,#115087,#115088,#115089,#115090,#115091,#115092,#115093,#115094,
#115095,#115096,#115097,#115098,#115099,#115100,#115101,#115102,#115103,
#115104,#115105,#115106,#115107,#115108,#115109,#115110,#115111,#115112,
#115113,#115114,#115115,#115116,#115117,#115118,#115119,#115120,#115121,
#115122,#115123,#115124,#115125,#115126,#115127,#115128,#115129,#115130,
#115131,#115132,#115133,#115134,#115135,#115136,#115137,#115138,#115139,
#115140,#115141,#115142,#115143,#115144,#115145,#115146,#115147,#115148,
#115149,#115150,#115151,#115152,#115153,#115154,#115155,#115156,#115157,
#115158,#115159,#115160,#115161,#115162,#115163,#115164,#115165,#115166,
#115167,#115168,#115169,#115170,#115171,#115172,#115173,#115174,#115175,
#115176,#115177,#115178,#115179,#115180,#115181,#115182,#115183,#115184,
#115185,#115186,#115187,#115188,#115189),.UNSPECIFIED.,.F.,.F.,(4,2,2,2,
2,2,2,2,2,2,2,2,2,2,2,2,2,2,2,2,2,2,2,2,2,2,2,2,2,2,2,2,2,2,2,2,2,2,2,2,
2,2,2,2,2,2,2,2,2,2,2,2,2,2,2,2,2,2,2,2,2,2,2,2,2,2,2,2,2,2,2,2,2,2,2,2,
2,2,2,2,2,2,2,2,2,2,2,2,2,2,2,2,2,2,2,2,2,2,2,2,2,2,2,4),(-1.10881952756263,
-1.10526545399088,-1.09929239582824,-1.07124087827899,-1.04978109997219,
-1.03261241192772,-1.02901764768895,-1.02694969915861,-1.02512405626675,
-1.02261320002931,-1.01656362981476,-1.00755951542083,-0.973073045011544,
-0.952932463075774,-0.94729379316776,-0.943792579956133,-0.940547045415271,
-0.936224833044692,-0.926320057601762,-0.912160792999993,-0.891744393308104,
-0.890671867433004,-0.866186808478679,-0.862471651204054,-0.860376723898788,
-0.858557632186536,-0.856096284592217,-0.850347086728083,-0.841953994196577,
-0.812692423777212,-0.786843576578137,-0.780922568284288,-0.777361404005235,
-0.774133838775332,-0.769942259306126,-0.760806110455771,-0.748149656686722,
-0.725522705128143,-0.721448598660605,-0.6995123715649,-0.695821670641751,
-0.693732235042527,-0.691911994143761,-0.689441167079172,-0.683635108764058,
-0.675127699342708,-0.644976234310481,-0.620163851146711,-0.614269224860633,
-0.610713712917142,-0.607484813396225,-0.603282244222032,-0.59408284925815,
-0.581305735078787,-0.559147509791194,-0.554976486444893,-0.532885759700978,
-0.529194545150015,-0.52710502090039,-0.52528484718224,-0.52281430474735,
-0.517009767680641,-0.50850535761216,-0.478376903370673,-0.453539325064248,
-0.447644039466366,-0.444088434989167,-0.440859644516826,-0.43665749441707,
-0.427460197067178,-0.414686990999679,-0.392527839470723,-0.38837380375174,
-0.366261674775286,-0.362570454821976,-0.360480955412108,-0.358660823271831,
-0.356190363955751,-0.350386139688619,-0.34188229407636,-0.311757544241278,
-0.286916937434843,-0.281021666409002,-0.277466112498312,-0.274237394376277,
-0.270035376372078,-0.260838529656829,-0.248066085519974,-0.225907205357697,
-0.201545621156838,-0.196696607247021,-0.194362544109177,-0.192555507068455,
-0.190374523689871,-0.186140743347986,-0.160758199549301,-0.12229858435053,
-0.11596928382334,-0.111959169966519,-0.108750866326691,-0.10508285304095,
-0.0986545714332097,-0.0777366651724035,-0.0592697367048556),
 .UNSPECIFIED.);
#2838=B_SPLINE_CURVE_WITH_KNOTS('',3,(#115194,#115195,#115196,#115197,#115198,
#115199,#115200,#115201,#115202,#115203,#115204,#115205,#115206,#115207,
#115208,#115209,#115210,#115211,#115212,#115213,#115214,#115215,#115216,
#115217,#115218,#115219,#115220,#115221,#115222,#115223,#115224,#115225,
#115226,#115227,#115228,#115229,#115230,#115231,#115232,#115233,#115234,
#115235,#115236,#115237,#115238,#115239,#115240,#115241,#115242,#115243,
#115244,#115245,#115246,#115247,#115248,#115249,#115250,#115251,#115252,
#115253,#115254,#115255,#115256,#115257,#115258,#115259,#115260,#115261,
#115262,#115263,#115264,#115265,#115266,#115267,#115268,#115269,#115270,
#115271,#115272,#115273,#115274,#115275,#115276,#115277,#115278,#115279,
#115280,#115281,#115282,#115283,#115284,#115285,#115286,#115287,#115288,
#115289,#115290,#115291,#115292,#115293,#115294,#115295,#115296,#115297,
#115298,#115299,#115300,#115301,#115302,#115303,#115304,#115305,#115306,
#115307,#115308,#115309,#115310,#115311,#115312,#115313,#115314,#115315,
#115316,#115317,#115318,#115319,#115320,#115321,#115322,#115323,#115324,
#115325,#115326,#115327,#115328,#115329,#115330,#115331,#115332,#115333,
#115334,#115335,#115336,#115337,#115338,#115339,#115340,#115341,#115342,
#115343,#115344,#115345,#115346,#115347,#115348,#115349,#115350,#115351,
#115352,#115353,#115354,#115355,#115356,#115357,#115358,#115359,#115360,
#115361,#115362,#115363,#115364,#115365,#115366,#115367,#115368,#115369,
#115370,#115371,#115372,#115373,#115374,#115375,#115376,#115377,#115378,
#115379,#115380,#115381,#115382,#115383,#115384,#115385,#115386,#115387,
#115388,#115389,#115390,#115391,#115392,#115393,#115394,#115395,#115396,
#115397),.UNSPECIFIED.,.F.,.F.,(4,2,2,2,2,2,2,2,2,2,2,2,2,2,2,2,2,2,2,2,
2,2,2,2,2,2,2,2,2,2,2,2,2,2,2,2,2,2,2,2,2,2,2,2,2,2,2,2,2,2,2,2,2,2,2,2,
2,2,2,2,2,2,2,2,2,2,2,2,2,2,2,2,2,2,2,2,2,2,2,2,2,2,2,2,2,2,2,2,2,2,2,2,
2,2,2,2,2,2,2,2,2,4),(-4.55723119340549,-4.53542832434012,-4.50896448142615,
-4.50315716589731,-4.50068590262253,-4.49886532687413,-4.49677546896773,
-4.49308377390169,-4.47111463237268,-4.46705960011841,-4.44470686225495,
-4.43188840544058,-4.4226680833791,-4.41846141968583,-4.41523151747225,
-4.41167701522777,-4.40578897923254,-4.38104299002909,-4.35086699346539,
-4.34235836236679,-4.33655110072032,-4.33407985738933,-4.33225929516264,
-4.33016945141772,-4.3264777784293,-4.30450751493001,-4.30023042820911,
-4.27806833262354,-4.26526862974408,-4.25605812824239,-4.2518531905726,
-4.24862352737678,-4.24506820457166,-4.23917623405573,-4.21443515666992,
-4.18426169514232,-4.17575341482362,-4.16994633799681,-4.1674751356603,
-4.16565458884208,-4.16356474556491,-4.15987303635166,-4.13788669860107,
-4.13362061826904,-4.11145693602026,-4.09866131259351,-4.08945296167763,
-4.08524841607183,-4.08201882134212,-4.07846334174193,-4.07257055938531,
-4.04780211202449,-4.01765287466579,-4.00914767472118,-4.00334213740832,
-4.00087120183978,-3.9990506989405,-3.99696072838722,-3.99326841192948,
-3.9711107381612,-3.96730661424229,-3.94463125680002,-3.93196069340678,
-3.92281792141579,-3.91862484134117,-3.915396720625,-3.91183552108742,-3.90591572765924,
-3.88008502814496,-3.85084962367526,-3.84246186834696,-3.83671480575467,
-3.83425366226978,-3.83243438760605,-3.83033883582133,-3.82662150615858,
-3.8020569584203,-3.78411049970614,-3.76786872080134,-3.76041756915105,
-3.75430035560356,-3.75069728500477,-3.74747826158471,-3.74336264926896,
-3.73667133881025,-3.69189773896525,-3.67399856592375,-3.66946614775791,
-3.66722531440779,-3.66542023230273,-3.66315309239069,-3.65848508199062,
-3.6273443310578,-3.59394615017214,-3.58771472518229,-3.58408743406314,
-3.58087247761976,-3.57679712967696,-3.57024583531637,-3.52635959716301,
-3.51240340853765,-3.50773961833004),.UNSPECIFIED.);
#2839=B_SPLINE_CURVE_WITH_KNOTS('',3,(#115399,#115400,#115401,#115402,#115403,
#115404,#115405,#115406,#115407,#115408,#115409,#115410,#115411,#115412,
#115413,#115414,#115415,#115416,#115417,#115418),.UNSPECIFIED.,.F.,.F.,
(4,2,2,2,2,2,2,2,2,4),(-0.0592697367048556,-0.0463583666809266,-0.0324747160269597,
-0.0290285262924044,-0.027013615035921,-0.0251703567530109,-0.0233117892002817,
-0.0207389877446909,-0.0142408263042859,-0.000491288661123149),
 .UNSPECIFIED.);
#2840=B_SPLINE_CURVE_WITH_KNOTS('',3,(#115419,#115420,#115421,#115422,#115423,
#115424,#115425,#115426,#115427,#115428,#115429,#115430,#115431,#115432,
#115433,#115434,#115435,#115436,#115437,#115438,#115439,#115440,#115441,
#115442,#115443,#115444,#115445,#115446,#115447,#115448,#115449,#115450,
#115451,#115452,#115453,#115454,#115455,#115456,#115457,#115458,#115459,
#115460,#115461,#115462,#115463,#115464,#115465,#115466,#115467,#115468,
#115469,#115470,#115471,#115472,#115473,#115474,#115475,#115476,#115477,
#115478,#115479,#115480,#115481,#115482,#115483,#115484,#115485,#115486,
#115487,#115488,#115489,#115490,#115491,#115492,#115493,#115494,#115495,
#115496,#115497,#115498,#115499,#115500,#115501,#115502,#115503,#115504,
#115505,#115506,#115507,#115508,#115509,#115510,#115511,#115512,#115513,
#115514,#115515,#115516,#115517,#115518,#115519,#115520,#115521,#115522,
#115523,#115524,#115525,#115526,#115527,#115528,#115529,#115530,#115531,
#115532,#115533,#115534,#115535,#115536,#115537,#115538,#115539,#115540,
#115541,#115542,#115543,#115544,#115545,#115546,#115547,#115548,#115549,
#115550,#115551,#115552,#115553,#115554,#115555,#115556,#115557,#115558,
#115559,#115560,#115561,#115562,#115563,#115564,#115565,#115566,#115567,
#115568,#115569,#115570,#115571,#115572,#115573,#115574,#115575,#115576,
#115577,#115578,#115579,#115580,#115581,#115582,#115583,#115584,#115585,
#115586,#115587,#115588,#115589,#115590,#115591,#115592,#115593,#115594,
#115595,#115596,#115597,#115598,#115599,#115600,#115601,#115602,#115603,
#115604,#115605,#115606,#115607,#115608,#115609,#115610,#115611,#115612,
#115613,#115614,#115615,#115616,#115617,#115618,#115619,#115620,#115621,
#115622,#115623,#115624,#115625,#115626,#115627,#115628,#115629,#115630,
#115631,#115632,#115633,#115634,#115635,#115636,#115637,#115638,#115639,
#115640,#115641,#115642,#115643,#115644,#115645,#115646,#115647,#115648,
#115649,#115650,#115651,#115652,#115653,#115654,#115655,#115656,#115657,
#115658,#115659,#115660,#115661,#115662,#115663,#115664,#115665,#115666,
#115667,#115668,#115669,#115670,#115671,#115672,#115673,#115674,#115675,
#115676,#115677,#115678),.UNSPECIFIED.,.F.,.F.,(4,2,2,2,2,2,2,2,2,2,2,2,
2,2,2,2,2,2,2,2,2,2,2,2,2,2,2,2,2,2,2,2,2,2,2,2,2,2,2,2,2,2,2,2,2,2,2,2,
2,2,2,2,2,2,2,2,2,2,2,2,2,2,2,2,2,2,2,2,2,2,2,2,2,2,2,2,2,2,2,2,2,2,2,2,
2,2,2,2,2,2,2,2,2,2,2,2,2,2,2,2,2,2,2,2,2,2,2,2,2,2,2,2,2,2,2,2,2,2,2,2,
2,2,2,2,2,2,2,2,2,4),(-2.09994048470851,-2.05894043935947,-2.04944988533331,
-2.04519702509862,-2.04196135890193,-2.03842975304143,-2.03264804227002,
-2.01025775568754,-1.97799440335339,-1.9691977268642,-1.96333889887151,
-1.96096338195135,-1.9609466439916,-1.96092957897279,-1.96091216966876,
-1.96089439783931,-1.96087624407058,-1.9608576877646,-1.96083870708189,
-1.96081927849993,-1.96079937700362,-1.9607789758323,-1.96075804639954,
-1.96073655794338,-1.96071447746922,-1.96069176947358,-1.96066839572713,
-1.96064431499208,-1.96061948256786,-1.96059385023083,-1.96056736555582,
-1.96053997163244,-1.96051160648292,-1.96048220244113,-1.96045168554925,
-1.96041997482767,-1.96038698133963,-1.96035260718332,-1.96031674436325,
-1.96027927338378,-1.96024006176422,-1.96019896214376,-1.95839169712927,
-1.95605694997279,-1.95120528464012,-1.92683135224008,-1.90465539517672,
-1.89187364807633,-1.88267253745642,-1.87846948558848,-1.87524036669506,
-1.87168476754328,-1.86579033211436,-1.84096818824147,-1.81085229888347,
-1.8023508250377,-1.79654714241649,-1.79407665569003,-1.79225637149713,
-1.79016659264472,-1.78647457203492,-1.76441056172453,-1.76019334415021,
-1.73801755634917,-1.72523586766422,-1.71603480541696,-1.71183178040185,
-1.70860268401789,-1.70504711152692,-1.69915272475734,-1.67433098467606,
-1.64421511017746,-1.6357136715291,-1.62991001760038,-1.62743954630897,
-1.62561927475397,-1.62352951188227,-1.61983752268174,-1.59777509026306,
-1.59355683706387,-1.57138130495276,-1.5585994458685,-1.54939831224275,
-1.54519529321184,-1.5419662166612,-1.53841068121885,-1.53251639205084,
-1.50769667405415,-1.47757940530244,-1.46907782412491,-1.46327411065517,
-1.46080364008518,-1.45898337930664,-1.45689364073358,-1.45320172013757,
-1.43115092236588,-1.42692413980631,-1.40474958360488,-1.39196566997983,
-1.3827634789852,-1.37856029415126,-1.37533121543923,-1.37177580261758,
-1.36588201407026,-1.34107759647615,-1.31094736749012,-1.30244418553558,
-1.29663968862182,-1.29416909808649,-1.29234883283046,-1.29025918681035,
-1.28656764000556,-1.2646097013561,-1.26053672195974,-1.23789810131862,
-1.22523632756718,-1.21609820982578,-1.21190623038655,-1.20867858948283,
-1.2051175777133,-1.19919735541953,-1.17334413446036,-1.14411561858126,
-1.13572841400601,-1.12998166527577,-1.12752074458941,-1.12570169168781,
-1.12360653326024,-1.11989028656003,-1.10911089706055),.UNSPECIFIED.);
#2841=B_SPLINE_CURVE_WITH_KNOTS('',3,(#115684,#115685,#115686,#115687,#115688,
#115689,#115690,#115691,#115692,#115693,#115694,#115695,#115696,#115697,
#115698,#115699,#115700,#115701,#115702,#115703,#115704,#115705,#115706,
#115707,#115708,#115709,#115710,#115711,#115712,#115713,#115714,#115715,
#115716,#115717,#115718,#115719,#115720,#115721,#115722,#115723,#115724,
#115725,#115726,#115727,#115728,#115729,#115730,#115731,#115732,#115733,
#115734,#115735,#115736,#115737,#115738,#115739,#115740,#115741,#115742,
#115743,#115744,#115745,#115746,#115747,#115748,#115749,#115750,#115751,
#115752,#115753,#115754,#115755,#115756,#115757,#115758,#115759,#115760,
#115761,#115762,#115763,#115764,#115765,#115766,#115767,#115768,#115769,
#115770,#115771,#115772,#115773,#115774,#115775,#115776,#115777,#115778,
#115779,#115780,#115781,#115782,#115783,#115784,#115785,#115786,#115787,
#115788,#115789,#115790,#115791,#115792,#115793,#115794,#115795,#115796,
#115797,#115798,#115799,#115800,#115801,#115802,#115803,#115804,#115805,
#115806,#115807,#115808,#115809,#115810,#115811,#115812,#115813,#115814,
#115815,#115816,#115817,#115818,#115819,#115820,#115821,#115822,#115823,
#115824,#115825,#115826,#115827,#115828,#115829,#115830,#115831,#115832,
#115833,#115834,#115835,#115836,#115837,#115838,#115839,#115840,#115841,
#115842,#115843,#115844,#115845,#115846,#115847,#115848,#115849,#115850,
#115851,#115852,#115853,#115854,#115855,#115856,#115857,#115858,#115859,
#115860,#115861,#115862,#115863,#115864,#115865,#115866,#115867,#115868,
#115869,#115870,#115871,#115872,#115873,#115874,#115875,#115876,#115877,
#115878,#115879,#115880,#115881,#115882,#115883,#115884,#115885,#115886,
#115887,#115888,#115889),.UNSPECIFIED.,.F.,.F.,(4,2,2,2,2,2,2,2,2,2,2,2,
2,2,2,2,2,2,2,2,2,2,2,2,2,2,2,2,2,2,2,2,2,2,2,2,2,2,2,2,2,2,2,2,2,2,2,2,
2,2,2,2,2,2,2,2,2,2,2,2,2,2,2,2,2,2,2,2,2,2,2,2,2,2,2,2,2,2,2,2,2,2,2,2,
2,2,2,2,2,2,2,2,2,2,2,2,2,2,2,2,2,2,4),(-0.991117350869854,-0.97984114832981,
-0.97315088018324,-0.969034875902649,-0.965814913416383,-0.96221013912214,
-0.956088364065775,-0.922212018621459,-0.89139638286004,-0.886705650402648,
-0.884433775824448,-0.882628151356282,-0.880390653797248,-0.875877129508642,
-0.869813159247332,-0.853790017647763,-0.813718357180651,-0.806027118561792,
-0.802052141548575,-0.798844714949337,-0.795147729252929,-0.788587180245253,
-0.780433524141206,-0.761672250318317,-0.733869798740763,-0.722294141832624,
-0.719026802650053,-0.717050204070622,-0.71518636533546,-0.712451356666229,
-0.704883288898493,-0.692479135787954,-0.654558944539558,-0.641728001349262,
-0.636833076423305,-0.633819537974329,-0.630533689629472,-0.625970175679782,
-0.614517540205833,-0.597052167100155,-0.564022075176314,-0.555081553385852,
-0.552087202000881,-0.550360083667683,-0.54849269948845,-0.545739031266206,
-0.538030256209511,-0.525281516417833,-0.484547396888387,-0.474186772710357,
-0.47011130745134,-0.467104206214309,-0.463813027832059,-0.459218900211225,
-0.44755411924597,-0.429601229977824,-0.395780606180549,-0.388066975755315,
-0.385233144566462,-0.383536612427477,-0.381638432420609,-0.378732291569356,
-0.369778809938577,-0.353723321308674,-0.31351842856002,-0.306607384464841,
-0.302473506591906,-0.299243524743061,-0.295686865876557,-0.289790337620561,
-0.261804282803683,-0.234243515820459,-0.222334976743252,-0.219038586989944,
-0.217055762409074,-0.215195723081021,-0.212480165594264,-0.205054796833161,
-0.192993933742022,-0.157614396084684,-0.142354688441775,-0.137171881433024,
-0.133765755930204,-0.130472649978809,-0.130401637889918,-0.130337722882927,
-0.130279824211306,-0.130227073492749,-0.130178764235331,-0.130134315424739,
-0.12997631229673,-0.12981840149605,-0.124918477348795,-0.110040017949518,
-0.0831589239800696,-0.0584362202721239,-0.0535016838739476,-0.0511839823228503,
-0.0493771883808169,-0.0471812350995658,-0.0428757301979037,-0.0371759277505071,
-0.00039473036140113),.UNSPECIFIED.);
#2842=B_SPLINE_CURVE_WITH_KNOTS('',3,(#115890,#115891,#115892,#115893,#115894,
#115895,#115896,#115897,#115898,#115899,#115900,#115901,#115902,#115903,
#115904,#115905,#115906,#115907),.UNSPECIFIED.,.F.,.F.,(4,2,2,2,2,2,2,2,
4),(-4.61628182467573,-4.59344808068452,-4.58898643506661,-4.58571278198089,
-4.58241685164426,-4.57941610975834,-4.57459111966926,-4.56224152719433,
-4.55723119340549),.UNSPECIFIED.);
#2843=B_SPLINE_CURVE_WITH_KNOTS('',3,(#115908,#115909,#115910,#115911,#115912,
#115913,#115914,#115915,#115916,#115917,#115918,#115919,#115920,#115921,
#115922,#115923,#115924,#115925,#115926,#115927,#115928,#115929,#115930,
#115931,#115932,#115933,#115934,#115935,#115936,#115937,#115938,#115939,
#115940,#115941,#115942,#115943,#115944,#115945,#115946,#115947,#115948,
#115949,#115950,#115951,#115952,#115953,#115954,#115955,#115956,#115957,
#115958,#115959,#115960,#115961,#115962,#115963,#115964,#115965,#115966,
#115967,#115968,#115969,#115970,#115971,#115972,#115973,#115974,#115975,
#115976,#115977,#115978,#115979,#115980,#115981,#115982,#115983,#115984,
#115985,#115986,#115987,#115988,#115989,#115990,#115991,#115992,#115993,
#115994,#115995,#115996,#115997,#115998,#115999,#116000,#116001,#116002,
#116003,#116004,#116005,#116006,#116007,#116008,#116009,#116010,#116011,
#116012,#116013,#116014,#116015,#116016,#116017,#116018,#116019,#116020,
#116021,#116022,#116023,#116024,#116025,#116026,#116027,#116028,#116029,
#116030,#116031,#116032,#116033,#116034,#116035,#116036,#116037,#116038,
#116039,#116040,#116041,#116042,#116043,#116044,#116045,#116046,#116047,
#116048,#116049,#116050,#116051,#116052,#116053,#116054,#116055,#116056,
#116057,#116058,#116059,#116060,#116061,#116062,#116063,#116064,#116065,
#116066,#116067,#116068,#116069,#116070,#116071,#116072,#116073,#116074,
#116075,#116076,#116077,#116078,#116079,#116080,#116081,#116082,#116083,
#116084,#116085,#116086,#116087,#116088,#116089,#116090,#116091,#116092,
#116093,#116094,#116095,#116096,#116097,#116098,#116099,#116100,#116101,
#116102,#116103,#116104,#116105,#116106,#116107),.UNSPECIFIED.,.F.,.F.,
(4,2,2,2,2,2,2,2,2,2,2,2,2,2,2,2,2,2,2,2,2,2,2,2,2,2,2,2,2,2,2,2,2,2,2,
2,2,2,2,2,2,2,2,2,2,2,2,2,2,2,2,2,2,2,2,2,2,2,2,2,2,2,2,2,2,2,2,2,2,2,2,
2,2,2,2,2,2,2,2,2,2,2,2,2,2,2,2,2,2,2,2,2,2,2,2,2,2,2,2,4),(-1.10911089706055,
-1.09536029552188,-1.07745793675764,-1.06115734615668,-1.05022985049061,
-1.04619257319148,-1.04319534546673,-1.03989713287019,-1.03525925835878,
-1.02327938236834,-1.0045839344241,-0.976942564988807,-0.965145595450497,
-0.96185992353093,-0.959879849791299,-0.958019289807807,-0.955298600738319,
-0.94783158868073,-0.935669812887117,-0.899590940595222,-0.885029401543547,
-0.879920000095205,-0.876868450620587,-0.873611642311612,-0.869215130994038,
-0.858850743905504,-0.84375085594157,-0.824247732367925,-0.801248771186571,
-0.796394867994558,-0.794059799098971,-0.792252654269116,-0.790072355452397,
-0.785842137889164,-0.761130010121192,-0.721824007066994,-0.715582876189345,
-0.711598568957438,-0.708392120598604,-0.704705650115049,-0.698189441331689,
-0.690105872516136,-0.671602084187366,-0.644435189368545,-0.631992992293171,
-0.628644872050281,-0.62665131852,-0.624798248140955,-0.622117165970806,
-0.614935723784745,-0.603448560816518,-0.582547219523575,-0.553527797774557,
-0.547543880083569,-0.543969608259826,-0.54074558535044,-0.53658046698623,
-0.527593033377261,-0.502797192499772,-0.472074461225718,-0.464339701664443,
-0.461503676613933,-0.45980727868709,-0.457910810065908,-0.455010014635448,
-0.446096154750107,-0.430150965791991,-0.390388305733253,-0.382348520519313,
-0.378357379187259,-0.375150507862693,-0.371469115056092,-0.36497695357909,
-0.333679093611474,-0.300758822563763,-0.296210472234194,-0.293966957403228,
-0.292162511143119,-0.289899751249717,-0.285252218322695,-0.266342011292558,
-0.245695073367644,-0.220114961852737,-0.21420045061068,-0.210640929160301,
-0.207413425676202,-0.203219885717632,-0.194070840020895,-0.181389305457178,
-0.158661196553583,-0.155314707243115,-0.132807718545252,-0.129115302201541,
-0.127025625334977,-0.125205695777603,-0.122735989446099,-0.11733032510801,
-0.0949096646472632,-0.0681866851383444,-0.0595548159224536),
 .UNSPECIFIED.);
#2844=B_SPLINE_CURVE_WITH_KNOTS('',3,(#116112,#116113,#116114,#116115,#116116,
#116117,#116118,#116119,#116120,#116121,#116122,#116123,#116124,#116125,
#116126,#116127,#116128,#116129,#116130,#116131,#116132,#116133,#116134,
#116135,#116136,#116137,#116138,#116139,#116140,#116141,#116142,#116143,
#116144,#116145,#116146,#116147,#116148,#116149,#116150,#116151,#116152,
#116153,#116154,#116155,#116156,#116157,#116158,#116159,#116160,#116161,
#116162,#116163,#116164,#116165,#116166,#116167,#116168,#116169,#116170,
#116171,#116172,#116173,#116174,#116175,#116176,#116177,#116178,#116179,
#116180,#116181,#116182,#116183,#116184,#116185,#116186,#116187,#116188,
#116189,#116190,#116191,#116192,#116193,#116194,#116195,#116196,#116197,
#116198,#116199,#116200,#116201,#116202,#116203,#116204,#116205,#116206,
#116207,#116208,#116209,#116210,#116211,#116212,#116213,#116214,#116215,
#116216,#116217,#116218,#116219,#116220,#116221,#116222,#116223,#116224,
#116225,#116226,#116227,#116228,#116229,#116230,#116231,#116232,#116233,
#116234,#116235,#116236,#116237,#116238,#116239,#116240,#116241,#116242,
#116243,#116244,#116245,#116246,#116247,#116248,#116249,#116250,#116251,
#116252,#116253,#116254,#116255,#116256,#116257,#116258,#116259,#116260,
#116261,#116262,#116263,#116264,#116265,#116266,#116267,#116268,#116269,
#116270,#116271,#116272,#116273,#116274,#116275,#116276,#116277,#116278,
#116279,#116280,#116281,#116282,#116283,#116284,#116285,#116286,#116287,
#116288,#116289,#116290,#116291,#116292,#116293,#116294,#116295,#116296,
#116297,#116298,#116299,#116300,#116301,#116302,#116303,#116304,#116305,
#116306,#116307,#116308,#116309,#116310,#116311,#116312,#116313,#116314,
#116315,#116316,#116317,#116318,#116319,#116320,#116321,#116322,#116323,
#116324,#116325,#116326,#116327,#116328,#116329,#116330,#116331,#116332,
#116333,#116334,#116335,#116336,#116337,#116338,#116339,#116340,#116341),
 .UNSPECIFIED.,.F.,.F.,(4,2,2,2,2,2,2,2,2,2,2,2,2,2,2,2,2,2,2,2,2,2,2,2,
2,2,2,2,2,2,2,2,2,2,2,2,2,2,2,2,2,2,2,2,2,2,2,2,2,2,2,2,2,2,2,2,2,2,2,2,
2,2,2,2,2,2,2,2,2,2,2,2,2,2,2,2,2,2,2,2,2,2,2,2,2,2,2,2,2,2,2,2,2,2,2,2,
2,2,2,2,2,2,2,2,2,2,2,2,2,2,2,2,2,2,4),(-2.04091987557192,-2.0214364672295,
-2.01795486345245,-1.99048502414608,-1.97542996731522,-1.97050981628791,
-1.97035181158444,-1.97019379604683,-1.97015105764711,-1.97010470448076,
-1.97005420664619,-1.96999892305641,-1.96993806999392,-1.96987067832227,
-1.96979553378446,-1.96971109244413,-1.96961535776459,-1.96950569690538,
-1.96937855768623,-1.96922901564825,-1.9659966455919,-1.96244616112557,
-1.95658071392048,-1.93177799622883,-1.90159286333757,-1.89308148004259,
-1.88727231358038,-1.88480024145603,-1.88297906150313,-1.8808885003324,
-1.87719554210386,-1.85520996783483,-1.85093669278227,-1.82876619989233,
-1.81596410538435,-1.80675149718162,-1.80254530794657,-1.79931456915889,
-1.79575794824884,-1.78986355531596,-1.76510057004488,-1.73492861745318,
-1.72641892425985,-1.72061060729511,-1.71813868693701,-1.71631753638898,
-1.71422691303833,-1.71053363851319,-1.68845667774375,-1.68424910428063,
-1.66207096420474,-1.64928823997298,-1.64008578306475,-1.63588137965813,
-1.63265088769092,-1.62909341550034,-1.62319494011144,-1.59829546438007,
-1.56824268921601,-1.55974806512833,-1.55394724049454,-1.5514765796572,
-1.5496555982326,-1.54756428526641,-1.54386788877696,-1.52095915663146,
-1.51804887530415,-1.4952644517905,-1.48256373641869,-1.4734042903589,-1.46920741993812,
-1.46597791203902,-1.46241671581398,-1.45650059382646,-1.43092008409314,
-1.41028446701765,-1.39138437548358,-1.38673666997502,-1.3844730986558,
-1.38266760104559,-1.38042220123916,-1.37586815433095,-1.34295204710857,
-1.31160807899895,-1.30511190262722,-1.30142839889663,-1.29821976723592,
-1.29422650381571,-1.28795872529718,-1.24890691838106,-1.22401413920869,
-1.21978223072504,-1.21760092102095,-1.21579283991067,-1.2134563302972,
-1.20859861389451,-1.18281016658834,-1.1674554137225,-1.15150727932758,
-1.14074161219738,-1.13628091436378,-1.13301245193946,-1.1299753068327,
-1.12495004358513,-1.11114100498908,-1.07740997159974,-1.06309475938427,
-1.05477253568418,-1.05194083493369,-1.05005789433015,-1.04811026978677,
-1.04497576778931,-1.03375343852834,-1.01005667358214,-0.991117350869854),
 .UNSPECIFIED.);
#2845=B_SPLINE_CURVE_WITH_KNOTS('',3,(#116343,#116344,#116345,#116346,#116347,
#116348,#116349,#116350,#116351,#116352,#116353,#116354,#116355,#116356,
#116357,#116358),.UNSPECIFIED.,.F.,.F.,(4,2,2,2,2,2,2,4),(-0.0595548159224536,
-0.0522110906588228,-0.0469503809994493,-0.0435290859888312,-0.0402475629379682,
-0.0369986128403095,-0.0326031491967441,-0.000491644909933951),
 .UNSPECIFIED.);
#2846=B_SPLINE_CURVE_WITH_KNOTS('',3,(#116359,#116360,#116361,#116362,#116363,
#116364,#116365,#116366,#116367,#116368,#116369,#116370,#116371,#116372,
#116373,#116374,#116375,#116376,#116377,#116378,#116379,#116380,#116381,
#116382,#116383,#116384,#116385,#116386,#116387,#116388,#116389,#116390,
#116391,#116392,#116393,#116394,#116395,#116396,#116397,#116398,#116399,
#116400,#116401,#116402,#116403,#116404,#116405,#116406,#116407,#116408,
#116409,#116410,#116411,#116412,#116413,#116414,#116415,#116416,#116417,
#116418,#116419,#116420,#116421,#116422,#116423,#116424,#116425,#116426,
#116427,#116428,#116429,#116430,#116431,#116432,#116433,#116434,#116435,
#116436,#116437,#116438,#116439,#116440,#116441,#116442,#116443,#116444,
#116445,#116446,#116447,#116448,#116449,#116450,#116451,#116452,#116453,
#116454,#116455,#116456,#116457,#116458,#116459,#116460,#116461,#116462,
#116463,#116464,#116465,#116466,#116467,#116468,#116469,#116470,#116471,
#116472,#116473,#116474,#116475,#116476,#116477,#116478,#116479,#116480,
#116481,#116482,#116483,#116484,#116485,#116486,#116487,#116488,#116489,
#116490,#116491,#116492,#116493,#116494,#116495,#116496,#116497,#116498,
#116499,#116500,#116501,#116502,#116503,#116504,#116505,#116506,#116507,
#116508,#116509,#116510,#116511,#116512,#116513,#116514,#116515,#116516,
#116517,#116518,#116519,#116520,#116521),.UNSPECIFIED.,.F.,.F.,(4,3,3,3,
3,3,3,3,3,3,3,3,3,3,3,3,3,3,3,3,3,3,3,3,3,3,3,3,3,3,3,3,3,3,3,3,3,3,3,3,
3,3,3,3,3,3,3,3,3,3,3,3,3,3,4),(-54.111865720756,-53.9685006350433,-53.8675843506887,
-53.7577897347099,-53.646820579414,-53.5373284361922,-53.4279032844545,
-53.3185044306127,-53.2063874460452,-53.0968489113581,-52.9834427018503,
-52.8700364923426,-52.7602418763656,-52.6492727210695,-52.5397805778498,
-52.4303554261141,-52.3209565722744,-52.208839587705,-52.0993010530199,
-51.9858948435082,-51.8724886339965,-51.76269401802,-51.6517248627238,-51.5422327195046,
-51.4328075677695,-51.3234087139303,-51.2112917293603,-51.1017531946758,
-50.9883469851631,-50.8749407756504,-50.7651461596728,-50.6541770043767,
-50.5446848611563,-50.43525970942,-50.3258608555796,-50.2137438710108,-50.1042053363251,
-49.9907991268147,-49.8773929173043,-49.7675983013272,-49.6566291460311,
-49.5471370028112,-49.4377118510754,-49.3283129972356,-49.2161960126663,
-49.1066574779811,-48.9932512684696,-48.8798450589582,-48.770074918514,
-48.6604636794697,-48.5509703726863,-48.4415394131865,-48.3321442530794,
-48.22270901535,-48.1819103663467),.UNSPECIFIED.);
#2847=B_SPLINE_CURVE_WITH_KNOTS('',3,(#116527,#116528,#116529,#116530,#116531,
#116532,#116533,#116534,#116535,#116536,#116537,#116538,#116539,#116540,
#116541,#116542,#116543,#116544,#116545,#116546,#116547,#116548,#116549,
#116550,#116551,#116552,#116553,#116554,#116555,#116556,#116557,#116558,
#116559,#116560,#116561,#116562,#116563,#116564,#116565,#116566,#116567,
#116568,#116569,#116570,#116571,#116572,#116573,#116574,#116575,#116576,
#116577,#116578,#116579,#116580,#116581,#116582,#116583,#116584,#116585,
#116586,#116587,#116588,#116589,#116590,#116591,#116592,#116593,#116594,
#116595,#116596,#116597,#116598,#116599,#116600,#116601,#116602,#116603,
#116604,#116605,#116606,#116607,#116608,#116609,#116610,#116611,#116612,
#116613,#116614,#116615,#116616,#116617,#116618,#116619,#116620,#116621,
#116622,#116623,#116624,#116625,#116626,#116627,#116628,#116629,#116630,
#116631,#116632,#116633,#116634,#116635,#116636,#116637,#116638,#116639,
#116640,#116641,#116642,#116643,#116644,#116645,#116646,#116647,#116648,
#116649,#116650,#116651,#116652,#116653,#116654,#116655,#116656,#116657,
#116658,#116659,#116660,#116661,#116662,#116663,#116664,#116665,#116666,
#116667,#116668,#116669,#116670,#116671,#116672,#116673,#116674,#116675,
#116676,#116677,#116678,#116679,#116680,#116681,#116682,#116683,#116684,
#116685,#116686,#116687,#116688,#116689,#116690,#116691,#116692,#116693,
#116694,#116695,#116696,#116697,#116698,#116699,#116700,#116701,#116702,
#116703,#116704,#116705,#116706,#116707,#116708,#116709,#116710,#116711,
#116712,#116713,#116714,#116715,#116716,#116717,#116718,#116719,#116720,
#116721,#116722,#116723,#116724,#116725,#116726,#116727,#116728,#116729,
#116730,#116731,#116732),.UNSPECIFIED.,.F.,.F.,(4,2,2,2,2,2,2,2,2,2,2,2,
2,2,2,2,2,2,2,2,2,2,2,2,2,2,2,2,2,2,2,2,2,2,2,2,2,2,2,2,2,2,2,2,2,2,2,2,
2,2,2,2,2,2,2,2,2,2,2,2,2,2,2,2,2,2,2,2,2,2,2,2,2,2,2,2,2,2,2,2,2,2,2,2,
2,2,2,2,2,2,2,2,2,2,2,2,2,2,2,2,2,2,4),(-0.991229013558196,-0.983226807241693,
-0.978905720506465,-0.957081037524643,-0.953390024519641,-0.951300091834927,
-0.949479154193232,-0.947006945545792,-0.941195589161653,-0.932678274344057,
-0.902453257244407,-0.877726437790873,-0.871833252991677,-0.868277265642927,
-0.865047054071154,-0.860841477772183,-0.851629717019773,-0.838830079244984,
-0.816681461932387,-0.8124367997064,-0.790449607248132,-0.786757969855074,
-0.784667923948854,-0.782847059550454,-0.780375180480012,-0.774565613368112,
-0.766051838499369,-0.735854191130525,-0.71109726075852,-0.705203239670551,
-0.701647122844623,-0.698417031180796,-0.694211952144567,-0.685002735411832,
-0.672207860662359,-0.650057696043303,-0.645826704446605,-0.623820542642875,
-0.620128908148945,-0.618038889331176,-0.616218066731327,-0.613746268767549,
-0.607936999666053,-0.599423758636789,-0.569229570716515,-0.544469917019493,
-0.538575918279128,-0.535019854380151,-0.53178983576337,-0.527584887688922,
-0.518376110689972,-0.505581975967506,-0.483432066825163,-0.479202667774492,
-0.457194844287983,-0.453503278898882,-0.451413301976146,-0.449592517856909,
-0.447120774783903,-0.441311646381643,-0.432798622115862,-0.402605373502923,
-0.377845884641074,-0.371951998169329,-0.368396006298207,-0.365166055822773,
-0.36096120035973,-0.351752642818699,-0.338958827043643,-0.316809358516629,
-0.312580212461516,-0.290572617361072,-0.286881128281577,-0.284791194864381,
-0.282970448863579,-0.280498757826556,-0.274689752997988,-0.266176910979542,
-0.235984327366617,-0.211217976131495,-0.205328065501688,-0.201772966766826,
-0.198542873748514,-0.194336462231084,-0.185118648564916,-0.172307031514681,
-0.149932020347275,-0.14597502588274,-0.123953541227381,-0.120262072847819,
-0.118172169834451,-0.116351463683811,-0.11387984463443,-0.108071087843485,
-0.0818781132822752,-0.0549654806149681,-0.0424558181115558,-0.0376072481790382,
-0.0346022506871433,-0.0313099267277518,-0.0280428395245619,-0.0235991964975932,
-0.000491388196465075),.UNSPECIFIED.);
#2848=B_SPLINE_CURVE_WITH_KNOTS('',3,(#116733,#116734,#116735,#116736,#116737,
#116738,#116739,#116740,#116741,#116742,#116743,#116744,#116745,#116746,
#116747,#116748),.UNSPECIFIED.,.F.,.F.,(4,2,2,2,2,2,2,4),(-2.0997315227576,
-2.05974751902068,-2.05394201031784,-2.05147051231299,-2.04964936915767,
-2.0475584005859,-2.04386375467915,-2.04091987557192),.UNSPECIFIED.);
#2849=B_SPLINE_CURVE_WITH_KNOTS('',3,(#116750,#116751,#116752,#116753,#116754,
#116755,#116756,#116757,#116758,#116759,#116760,#116761,#116762),
 .UNSPECIFIED.,.F.,.F.,(4,3,3,3,4),(-48.1819103663467,-48.072349463502,
-47.9625850721489,-47.8822972006122,-47.8286804139494),.UNSPECIFIED.);
#2850=B_SPLINE_CURVE_WITH_KNOTS('',3,(#116763,#116764,#116765,#116766,#116767,
#116768,#116769,#116770,#116771),.UNSPECIFIED.,.F.,.F.,(4,1,1,1,1,1,4),
(-47.8286738455222,-46.8847493422661,-45.88720148392,-44.8896536255739,
-43.8921057672278,-42.8945579088817,-41.8982145706828),.UNSPECIFIED.);
#2851=B_SPLINE_CURVE_WITH_KNOTS('',3,(#116776,#116777,#116778,#116779,#116780,
#116781,#116782,#116783,#116784,#116785,#116786,#116787,#116788,#116789,
#116790,#116791,#116792,#116793,#116794,#116795,#116796,#116797,#116798,
#116799,#116800,#116801,#116802,#116803,#116804,#116805,#116806,#116807,
#116808,#116809,#116810,#116811,#116812,#116813,#116814,#116815,#116816,
#116817,#116818,#116819,#116820,#116821,#116822,#116823,#116824,#116825,
#116826,#116827,#116828,#116829,#116830,#116831,#116832,#116833,#116834,
#116835,#116836,#116837,#116838,#116839,#116840,#116841,#116842,#116843,
#116844,#116845,#116846,#116847,#116848,#116849,#116850,#116851,#116852,
#116853,#116854,#116855,#116856,#116857,#116858,#116859,#116860,#116861,
#116862,#116863,#116864,#116865,#116866,#116867,#116868,#116869,#116870,
#116871,#116872,#116873,#116874,#116875,#116876,#116877,#116878,#116879,
#116880,#116881,#116882,#116883,#116884,#116885,#116886,#116887,#116888,
#116889,#116890,#116891,#116892,#116893,#116894,#116895,#116896,#116897,
#116898,#116899,#116900,#116901,#116902,#116903,#116904,#116905,#116906,
#116907,#116908,#116909,#116910,#116911,#116912,#116913,#116914,#116915,
#116916,#116917,#116918,#116919,#116920,#116921,#116922,#116923,#116924,
#116925,#116926,#116927,#116928,#116929,#116930,#116931,#116932,#116933,
#116934,#116935,#116936,#116937,#116938,#116939,#116940,#116941,#116942,
#116943,#116944,#116945,#116946,#116947,#116948,#116949,#116950,#116951,
#116952,#116953,#116954,#116955,#116956,#116957,#116958,#116959,#116960,
#116961,#116962,#116963,#116964,#116965,#116966,#116967,#116968,#116969,
#116970,#116971,#116972,#116973,#116974,#116975,#116976,#116977,#116978,
#116979,#116980,#116981,#116982,#116983,#116984,#116985,#116986,#116987),
 .UNSPECIFIED.,.F.,.F.,(4,2,2,2,2,2,2,2,2,2,2,2,2,2,2,2,2,2,2,2,2,2,2,2,
2,2,2,2,2,2,2,2,2,2,2,2,2,2,2,2,2,2,2,2,2,2,2,2,2,2,2,2,2,2,2,2,2,2,2,2,
2,2,2,2,2,2,2,2,2,2,2,2,2,2,2,2,2,2,2,2,2,2,2,2,2,2,2,2,2,2,2,2,2,2,2,2,
2,2,2,2,2,2,2,2,2,4),(-2.04102384583476,-2.03717390456845,-2.03386856318245,
-2.03087609430279,-2.02610132939005,-2.01409214424512,-1.97527843971127,
-1.96276676574619,-1.95757056645696,-1.95468374034383,-1.95229856898726,
-1.9522812677756,-1.95226367370402,-1.95224577013204,-1.9504566851066,-1.94845249689006,
-1.9450585732234,-1.93200836201607,-1.90526296711851,-1.88689799636911,
-1.87505751891548,-1.87043815277717,-1.86714234946013,-1.86414009400134,
-1.8593090550742,-1.84692258743775,-1.80853471522224,-1.79607605977328,
-1.78848507236628,-1.78574705589783,-1.78388265434416,-1.78190709148508,
-1.77864436332611,-1.76712279750479,-1.73926078485881,-1.72047168354213,
-1.70845247017219,-1.70380792676097,-1.70050752884884,-1.69711157551711,
-1.69197916848967,-1.67720862078734,-1.64136463985673,-1.62923867236717,
-1.62178538057471,-1.61906592455901,-1.61720504149698,-1.61546965723968,
-1.61243298547157,-1.60313903830861,-1.57028576242051,-1.55296054728561,
-1.54157065124103,-1.53701632864956,-1.53373214880123,-1.53071677533512,
-1.52581117415722,-1.51290293781228,-1.47835134793742,-1.46380613887436,
-1.45809196666741,-1.45377773840045,-1.45157991397355,-1.4497730646489,
-1.44745716595493,-1.44253298524169,-1.41915283243522,-1.39915608757709,
-1.37721353684339,-1.37160533272437,-1.36810973120506,-1.36486045710184,
-1.36059487808944,-1.35115454588705,-1.30919352609576,-1.29630658157641,
-1.28854134334157,-1.28578023304681,-1.28391134998825,-1.28194308352469,
-1.2787139104237,-1.26757167050972,-1.23943731070387,-1.22053611421464,
-1.20847003305595,-1.20381886605605,-1.20051718586692,-1.19712283901868,
-1.19199859608921,-1.17730755383502,-1.13718238987883,-1.12766878359463,
-1.1213746016566,-1.11882422358746,-1.11699219571001,-1.11494241266772,
-1.11133850798002,-1.09484826360241,-1.05022558244646,-1.04074392397264,
-1.03653753341718,-1.03329735228271,-1.02977596482141,-1.02404572578345,
-0.99996913194226,-0.991229013558196),.UNSPECIFIED.);
#2852=B_SPLINE_CURVE_WITH_KNOTS('',3,(#116989,#116990,#116991,#116992,#116993),
 .UNSPECIFIED.,.F.,.F.,(4,1,4),(-41.8982145706828,-41.8970100505356,-41.5455022209794),
 .UNSPECIFIED.);
#2853=B_SPLINE_CURVE_WITH_KNOTS('',3,(#116994,#116995,#116996,#116997,#116998,
#116999,#117000,#117001,#117002,#117003,#117004,#117005,#117006,#117007,
#117008,#117009,#117010,#117011,#117012,#117013,#117014,#117015,#117016,
#117017,#117018,#117019,#117020,#117021,#117022,#117023,#117024,#117025,
#117026,#117027,#117028,#117029,#117030,#117031,#117032,#117033,#117034,
#117035,#117036,#117037,#117038,#117039,#117040,#117041,#117042,#117043,
#117044,#117045,#117046,#117047,#117048,#117049,#117050,#117051,#117052,
#117053,#117054,#117055,#117056,#117057,#117058,#117059,#117060,#117061,
#117062,#117063,#117064,#117065,#117066,#117067,#117068,#117069,#117070,
#117071,#117072,#117073,#117074,#117075,#117076,#117077,#117078,#117079,
#117080,#117081,#117082,#117083,#117084,#117085,#117086,#117087,#117088,
#117089,#117090,#117091,#117092,#117093,#117094,#117095,#117096,#117097,
#117098,#117099,#117100,#117101,#117102,#117103,#117104,#117105,#117106,
#117107,#117108,#117109,#117110,#117111,#117112,#117113,#117114,#117115,
#117116,#117117,#117118,#117119,#117120,#117121,#117122,#117123,#117124,
#117125,#117126,#117127,#117128,#117129,#117130,#117131,#117132,#117133,
#117134,#117135,#117136,#117137,#117138,#117139,#117140,#117141,#117142,
#117143,#117144,#117145,#117146,#117147,#117148,#117149,#117150,#117151,
#117152,#117153,#117154,#117155,#117156,#117157,#117158,#117159,#117160,
#117161,#117162,#117163,#117164,#117165,#117166,#117167,#117168,#117169,
#117170,#117171,#117172,#117173,#117174,#117175,#117176,#117177,#117178,
#117179,#117180,#117181,#117182,#117183,#117184,#117185),.UNSPECIFIED.,
 .F.,.F.,(4,2,2,2,2,2,2,2,2,2,2,2,2,2,2,2,2,2,2,2,2,2,2,2,2,2,2,2,2,2,2,
2,2,2,2,2,2,2,2,2,2,2,2,2,2,2,2,2,2,2,2,2,2,2,2,2,2,2,2,2,2,2,2,2,2,2,2,
2,2,2,2,2,2,2,2,2,2,2,2,2,2,2,2,2,2,2,2,2,2,2,2,2,2,2,2,4),(-2.10009212962413,
-2.08490754922681,-2.08082970724367,-2.07769015352275,-2.07458743933971,
-2.07105810229777,-2.06528703791036,-2.04132892984664,-2.01676155463722,
-2.00413300982311,-1.99647320851046,-1.99372671244327,-1.99186123545881,
-1.98988964740601,-1.98664276414969,-1.97529230046428,-1.94358297681593,
-1.9270860547046,-1.91956103523844,-1.91339689896894,-1.90978424484896,
-1.90656757076755,-1.90246999196441,-1.89584033369671,-1.8617643040054,
-1.83271131688535,-1.82840298143906,-1.82620684143748,-1.82440065117089,
-1.82208475070102,-1.81715775098882,-1.79356838485433,-1.77357042685395,
-1.75909779056585,-1.7490389808044,-1.74469150256002,-1.74144219680918,
-1.7379513106206,-1.7323612416949,-1.71302518102365,-1.66963618258593,-1.66286242183498,
-1.66023972487545,-1.65839664295815,-1.65638005092924,-1.65292722128992,
-1.63894650536415,-1.63524495756845,-1.60109049047854,-1.58432538648303,
-1.57912754172571,-1.57571896554424,-1.57246620255507,-1.56790039549497,
-1.55726104784524,-1.5123446410461,-1.50249967742783,-1.49605079062568,
-1.49347696546924,-1.49164184000464,-1.48960418084608,-1.48605432980396,
-1.47033536664883,-1.44099831528898,-1.4185312217029,-1.41289174465181,
-1.4093902567661,-1.40614461851851,-1.40189702317331,-1.39216355071117,
-1.35427493631468,-1.33881700675578,-1.33007499052363,-1.3271937448826,
-1.3253011060979,-1.32336759872777,-1.32029572815181,-1.31069170443886,
-1.27802107309806,-1.26081908534582,-1.24948433851868,-1.24493894381946,
-1.24165708611289,-1.23864104407536,-1.23372802603151,-1.2207603576303,
-1.18626292302198,-1.17173212778256,-1.16332966745509,-1.16048887435627,
-1.15860460638206,-1.15666060994102,-1.15354043430082,-1.14349926014873,
-1.11108111999421,-1.10913474690605),.UNSPECIFIED.);
#2854=B_SPLINE_CURVE_WITH_KNOTS('',3,(#117191,#117192,#117193,#117194,#117195,
#117196,#117197,#117198,#117199,#117200,#117201,#117202,#117203,#117204,
#117205,#117206,#117207,#117208,#117209,#117210,#117211,#117212,#117213,
#117214,#117215,#117216,#117217,#117218,#117219,#117220,#117221,#117222,
#117223,#117224,#117225,#117226,#117227,#117228,#117229,#117230,#117231,
#117232,#117233,#117234,#117235,#117236,#117237,#117238,#117239,#117240,
#117241,#117242,#117243,#117244,#117245,#117246,#117247,#117248,#117249,
#117250,#117251,#117252,#117253,#117254,#117255,#117256,#117257,#117258,
#117259,#117260,#117261,#117262,#117263,#117264,#117265,#117266,#117267,
#117268,#117269,#117270,#117271,#117272,#117273,#117274,#117275,#117276,
#117277,#117278,#117279,#117280,#117281,#117282,#117283,#117284,#117285,
#117286,#117287,#117288,#117289,#117290,#117291,#117292,#117293,#117294,
#117295,#117296,#117297,#117298,#117299,#117300,#117301,#117302,#117303,
#117304,#117305,#117306,#117307,#117308,#117309,#117310,#117311,#117312,
#117313,#117314,#117315,#117316,#117317,#117318,#117319,#117320,#117321,
#117322,#117323,#117324,#117325,#117326,#117327,#117328,#117329,#117330,
#117331,#117332,#117333,#117334,#117335,#117336,#117337,#117338,#117339,
#117340,#117341,#117342,#117343,#117344,#117345,#117346,#117347,#117348,
#117349,#117350,#117351,#117352,#117353,#117354,#117355,#117356,#117357,
#117358,#117359,#117360,#117361,#117362,#117363,#117364,#117365,#117366,
#117367,#117368,#117369,#117370,#117371,#117372,#117373,#117374,#117375,
#117376,#117377,#117378,#117379,#117380,#117381,#117382,#117383,#117384,
#117385,#117386,#117387,#117388,#117389,#117390,#117391,#117392),
 .UNSPECIFIED.,.F.,.F.,(4,2,2,2,2,2,2,2,2,2,2,2,2,2,2,2,2,2,2,2,2,2,2,2,
2,2,2,2,2,2,2,2,2,2,2,2,2,2,2,2,2,2,2,2,2,2,2,2,2,2,2,2,2,2,2,2,2,2,2,2,
2,2,2,2,2,2,2,2,2,2,2,2,2,2,2,2,2,2,2,2,2,2,2,2,2,2,2,2,2,2,2,2,2,2,2,2,
2,2,2,2,4),(-0.991067550591075,-0.969566444920773,-0.944672893744101,-0.938774257899021,
-0.93521695335431,-0.931986793055493,-0.927783074758645,-0.918583015696578,
-0.905806073276034,-0.883646087270495,-0.879488069453632,-0.857381114331676,
-0.853688774908553,-0.851598484581849,-0.849777516680721,-0.847305643612251,
-0.841496736283739,-0.832984512122551,-0.80280177488619,-0.778023648310773,
-0.772128614964703,-0.768572123824428,-0.765341841835967,-0.761136729971568,
-0.751928357736591,-0.739135429703427,-0.716982499516558,-0.712760451921669,
-0.690739821070485,-0.687047882069024,-0.684957707740074,-0.683136761734768,
-0.680664812413146,-0.674855258847695,-0.666341665386737,-0.636147266425527,
-0.611383750563235,-0.605489277480675,-0.601932953539672,-0.598702715276033,
-0.594497505030695,-0.585288255243221,-0.572493549211428,-0.550341971535362,
-0.546113285198583,-0.524102525380969,-0.520410699398215,-0.518320576787415,
-0.516499667065637,-0.514027755253209,-0.508218238072402,-0.499704651117111,
-0.469509520453648,-0.4447480847128,-0.438853783472498,-0.435297544217477,
-0.432067370851557,-0.42786222782289,-0.418653051607689,-0.405858385644574,
-0.383707370871188,-0.379478042220937,-0.357468771112168,-0.353777026247587,
-0.351686948219359,-0.349866076378106,-0.347394214704811,-0.341584809696551,
-0.333071382001998,-0.302876733591189,-0.278115986605916,-0.272221813941492,
-0.268665650181972,-0.265435544072389,-0.261230486709362,-0.25202149004021,
-0.239227066724125,-0.21707652607314,-0.192746236712413,-0.187894860924606,
-0.185559834444997,-0.183752114101933,-0.181570306669531,-0.177334833101406,
-0.151815053196087,-0.113524426206123,-0.107177305066877,-0.103161200548965,
-0.0999513432637862,-0.0962850354621321,-0.0898689258003784,-0.0672497308052082,
-0.0434761411833771,-0.0267323817985043,-0.0214000897555977,-0.0190357103558771,
-0.0172225145287875,-0.0155112239908774,-0.0133869725079222,-0.00853515704896566,
-0.00049116967053566),.UNSPECIFIED.);
#2855=B_SPLINE_CURVE_WITH_KNOTS('',3,(#117393,#117394,#117395,#117396,#117397,
#117398,#117399,#117400,#117401,#117402),.UNSPECIFIED.,.F.,.F.,(4,2,2,2,
4),(-2.10005510352121,-2.07332448423479,-2.05406114578682,-2.04184561685977,
-2.04102384583476),.UNSPECIFIED.);
#2856=B_SPLINE_CURVE_WITH_KNOTS('',3,(#117403,#117404,#117405,#117406,#117407,
#117408,#117409,#117410,#117411,#117412,#117413,#117414,#117415,#117416,
#117417,#117418,#117419,#117420,#117421,#117422,#117423,#117424,#117425,
#117426,#117427,#117428,#117429,#117430,#117431,#117432,#117433,#117434,
#117435,#117436,#117437,#117438,#117439,#117440,#117441,#117442,#117443,
#117444,#117445,#117446,#117447,#117448,#117449,#117450,#117451,#117452,
#117453,#117454,#117455,#117456,#117457,#117458,#117459,#117460,#117461,
#117462,#117463,#117464,#117465,#117466,#117467,#117468,#117469,#117470,
#117471,#117472,#117473,#117474,#117475,#117476,#117477,#117478,#117479,
#117480,#117481,#117482,#117483,#117484,#117485,#117486,#117487,#117488,
#117489,#117490,#117491,#117492,#117493,#117494,#117495,#117496,#117497,
#117498,#117499,#117500,#117501,#117502,#117503,#117504,#117505,#117506,
#117507,#117508,#117509,#117510,#117511,#117512,#117513,#117514,#117515,
#117516,#117517,#117518,#117519,#117520,#117521,#117522,#117523,#117524,
#117525,#117526,#117527,#117528,#117529,#117530,#117531,#117532,#117533,
#117534,#117535,#117536,#117537,#117538,#117539,#117540,#117541,#117542,
#117543,#117544,#117545,#117546,#117547,#117548,#117549,#117550,#117551,
#117552,#117553,#117554,#117555,#117556,#117557,#117558,#117559,#117560,
#117561,#117562,#117563,#117564,#117565,#117566,#117567,#117568,#117569,
#117570,#117571,#117572,#117573,#117574,#117575,#117576,#117577,#117578,
#117579,#117580,#117581,#117582,#117583,#117584,#117585,#117586,#117587,
#117588,#117589,#117590,#117591,#117592,#117593,#117594,#117595,#117596,
#117597,#117598,#117599,#117600,#117601,#117602,#117603,#117604,#117605,
#117606,#117607,#117608,#117609,#117610,#117611,#117612,#117613,#117614,
#117615,#117616,#117617,#117618),.UNSPECIFIED.,.F.,.F.,(4,2,2,2,2,2,2,2,
2,2,2,2,2,2,2,2,2,2,2,2,2,2,2,2,2,2,2,2,2,2,2,2,2,2,2,2,2,2,2,2,2,2,2,2,
2,2,2,2,2,2,2,2,2,2,2,2,2,2,2,2,2,2,2,2,2,2,2,2,2,2,2,2,2,2,2,2,2,2,2,2,
2,2,2,2,2,2,2,2,2,2,2,2,2,2,2,2,2,2,2,2,2,2,2,2,2,2,2,4),(-1.10913474690605,
-1.09405577864177,-1.08279980310246,-1.07826612582831,-1.07498636782013,
-1.07156060223005,-1.06628011075756,-1.05011160751438,-1.02138896784798,
-0.998409798010556,-0.994714785429516,-0.992624317599637,-0.990804183579028,
-0.988334847959111,-0.982538217590795,-0.97404996881074,-0.944051974893915,
-0.919059796258301,-0.913159581922442,-0.909602758784431,-0.906373970703262,
-0.902173414618555,-0.892986374032505,-0.880233109938923,-0.858065249111541,
-0.854030551272188,-0.831767927548374,-0.82807588384919,-0.82598610590262,
-0.824165865359523,-0.821695438568383,-0.815892081749962,-0.807390221684309,
-0.77728397436924,-0.752417670586788,-0.746521243032921,-0.742965271631544,
-0.7397363515573,-0.735534324979346,-0.726338542003137,-0.713568487318554,
-0.691406728957578,-0.687271479146896,-0.665133878532598,-0.661442369110651,
-0.659352736718786,-0.657532510829956,-0.655061953827518,-0.649257630184002,
-0.640753756560917,-0.610630795677304,-0.585784924543672,-0.579889216925326,
-0.576333445951882,-0.573104559985799,-0.568902365546806,-0.559705311546098,
-0.546932730299792,-0.524772448679891,-0.520623351499045,-0.498503970857649,
-0.494812603522999,-0.492723028981166,-0.490902837341678,-0.488432305215404,
-0.48262794484907,-0.474123931434673,-0.443999094661869,-0.419156604762584,
-0.413261105285596,-0.409705426035708,-0.406476601970075,-0.402274457388477,
-0.393077381776438,-0.380304660344582,-0.358144985515712,-0.353994012833381,
-0.331877601814207,-0.328186319967777,-0.326096790617799,-0.324276636055914,
-0.321806151191492,-0.316001888372612,-0.307498005686736,-0.277373436276523,
-0.252531865444521,-0.246636499845286,-0.243080896543273,-0.239852138409481,
-0.235650075280472,-0.226453159398117,-0.213680644168415,-0.191521447692658,
-0.167222930703103,-0.162272064729742,-0.159951829229269,-0.158145538600874,
-0.1559532972431,-0.151663863205703,-0.14599139004664,-0.131613805531639,
-0.09767025037255,-0.0840808012901606,-0.0790847074119322,-0.0760540389961014,
-0.072784119565897,-0.0683061592401258,-0.0595903483156433),
 .UNSPECIFIED.);
#2857=B_SPLINE_CURVE_WITH_KNOTS('',3,(#117623,#117624,#117625,#117626,#117627,
#117628,#117629,#117630,#117631,#117632,#117633,#117634,#117635,#117636,
#117637,#117638,#117639,#117640,#117641,#117642,#117643,#117644,#117645,
#117646,#117647,#117648,#117649,#117650,#117651,#117652,#117653,#117654,
#117655,#117656,#117657,#117658,#117659,#117660,#117661,#117662,#117663,
#117664,#117665,#117666,#117667,#117668,#117669,#117670,#117671,#117672,
#117673,#117674,#117675,#117676,#117677,#117678,#117679,#117680,#117681,
#117682,#117683,#117684,#117685,#117686,#117687,#117688,#117689,#117690,
#117691,#117692,#117693,#117694,#117695,#117696,#117697,#117698,#117699,
#117700,#117701,#117702,#117703,#117704,#117705,#117706,#117707,#117708,
#117709,#117710,#117711,#117712,#117713,#117714,#117715,#117716,#117717,
#117718,#117719,#117720,#117721,#117722,#117723,#117724,#117725,#117726,
#117727,#117728,#117729,#117730,#117731,#117732,#117733,#117734,#117735,
#117736,#117737,#117738,#117739,#117740,#117741,#117742,#117743,#117744,
#117745,#117746,#117747,#117748,#117749,#117750,#117751,#117752,#117753,
#117754,#117755,#117756,#117757,#117758,#117759,#117760,#117761,#117762,
#117763,#117764,#117765,#117766,#117767,#117768,#117769,#117770,#117771,
#117772,#117773,#117774,#117775,#117776,#117777,#117778,#117779,#117780,
#117781,#117782,#117783,#117784,#117785,#117786,#117787,#117788,#117789,
#117790,#117791,#117792,#117793,#117794,#117795,#117796,#117797,#117798,
#117799,#117800,#117801,#117802,#117803,#117804,#117805,#117806,#117807,
#117808,#117809,#117810,#117811,#117812,#117813,#117814),.UNSPECIFIED.,
 .F.,.F.,(4,2,2,2,2,2,2,2,2,2,2,2,2,2,2,2,2,2,2,2,2,2,2,2,2,2,2,2,2,2,2,
2,2,2,2,2,2,2,2,2,2,2,2,2,2,2,2,2,2,2,2,2,2,2,2,2,2,2,2,2,2,2,2,2,2,2,2,
2,2,2,2,2,2,2,2,2,2,2,2,2,2,2,2,2,2,2,2,2,2,2,2,2,2,2,2,4),(-2.04098006789499,
-2.02522521486599,-2.02086040667168,-2.01865248161769,-2.01684618147899,
-2.01454223012355,-2.00968175907203,-1.9817750950153,-1.94576838995064,
-1.93934734843213,-1.93567977524879,-1.93246971838089,-1.92845456020461,
-1.92211144006445,-1.87718498781505,-1.85885824647768,-1.8542757962952,
-1.85202494365312,-1.85021958394375,-1.84796183626162,-1.8433438518936,
-1.81120632585006,-1.77924205456829,-1.77271612362426,-1.76902653269481,
-1.76581869982293,-1.76183436658643,-1.75559657229383,-1.71016533658795,
-1.69209394211437,-1.68754090276748,-1.6852957337116,-1.68349028122673,
-1.68122658768647,-1.67657807347583,-1.64499021822129,-1.61190735517013,
-1.60572096682812,-1.60210267046644,-1.59888538161607,-1.59479301900264,
-1.58818449594299,-1.55394305729052,-1.525010106732,-1.52070087857754,-1.51850402153859,
-1.51669706348198,-1.51437987167012,-1.50944895745569,-1.48349956513394,
-1.45746841759021,-1.44281857824617,-1.4378416429685,-1.43447722624759,
-1.43119115960431,-1.42644584581865,-1.41462968076956,-1.37903874842166,
-1.35906409526328,-1.35429846704416,-1.35201236213213,-1.35020654161012,
-1.34798251871097,-1.34353705634913,-1.30960304018494,-1.28296758976692,
-1.27409376101385,-1.26994761831544,-1.26672450789409,-1.26313716876311,
-1.25709680652037,-1.22771236752431,-1.20603640852029,-1.19020915967174,
-1.18675406011428,-1.18473657007402,-1.18289298590798,-1.18026990277285,
-1.17397661585752,-1.14198363602638,-1.11242990987644,-1.10594541898531,
-1.10226448200625,-1.09905577707768,-1.09505940613091,-1.08878065242618,
-1.04983758824488,-1.04683110841985,-1.0240300419919,-1.02033498226642,
-1.01824405716327,-1.016423183105,-1.01395230309862,-1.00814954041404,-0.999649762948563,
-0.991067550591075),.UNSPECIFIED.);
#2858=B_SPLINE_CURVE_WITH_KNOTS('',3,(#117816,#117817,#117818,#117819,#117820,
#117821,#117822,#117823,#117824,#117825),.UNSPECIFIED.,.F.,.F.,(4,2,2,2,
4),(-0.0595903483156433,-0.0574176870545041,-0.0412032104811654,-0.0229709702128129,
-0.000637632363922989),.UNSPECIFIED.);
#2859=B_SPLINE_CURVE_WITH_KNOTS('',3,(#117826,#117827,#117828,#117829,#117830,
#117831,#117832,#117833,#117834,#117835,#117836,#117837,#117838,#117839,
#117840,#117841,#117842,#117843,#117844,#117845,#117846,#117847,#117848,
#117849,#117850,#117851,#117852,#117853,#117854,#117855,#117856,#117857,
#117858,#117859,#117860,#117861,#117862,#117863,#117864,#117865,#117866,
#117867,#117868,#117869,#117870,#117871,#117872,#117873,#117874,#117875,
#117876,#117877,#117878,#117879,#117880,#117881,#117882,#117883,#117884,
#117885,#117886,#117887,#117888,#117889,#117890,#117891,#117892,#117893,
#117894,#117895,#117896,#117897,#117898,#117899,#117900,#117901,#117902,
#117903,#117904,#117905,#117906,#117907,#117908,#117909,#117910,#117911,
#117912,#117913,#117914,#117915,#117916,#117917,#117918,#117919,#117920,
#117921,#117922,#117923,#117924,#117925,#117926,#117927,#117928,#117929,
#117930,#117931,#117932,#117933,#117934,#117935,#117936,#117937,#117938,
#117939,#117940,#117941,#117942,#117943,#117944,#117945,#117946,#117947,
#117948,#117949,#117950,#117951,#117952,#117953,#117954,#117955,#117956,
#117957,#117958,#117959,#117960,#117961,#117962,#117963,#117964,#117965,
#117966,#117967,#117968,#117969,#117970,#117971,#117972,#117973,#117974,
#117975,#117976,#117977,#117978,#117979,#117980,#117981,#117982,#117983,
#117984,#117985,#117986,#117987,#117988,#117989,#117990,#117991,#117992,
#117993,#117994,#117995,#117996,#117997,#117998,#117999,#118000,#118001,
#118002,#118003,#118004,#118005,#118006,#118007,#118008,#118009,#118010,
#118011,#118012,#118013,#118014,#118015,#118016,#118017),.UNSPECIFIED.,
 .F.,.F.,(4,2,2,2,2,2,2,2,2,2,2,2,2,2,2,2,2,2,2,2,2,2,2,2,2,2,2,2,2,2,2,
2,2,2,2,2,2,2,2,2,2,2,2,2,2,2,2,2,2,2,2,2,2,2,2,2,2,2,2,2,2,2,2,2,2,2,2,
2,2,2,2,2,2,2,2,2,2,2,2,2,2,2,2,2,2,2,2,2,2,2,2,2,2,2,2,4),(-4.84271254774332,
-4.84012768829738,-4.83777417014381,-4.83590804710275,-4.83420334357131,
-4.83224168845127,-4.8290415726128,-4.81818716236885,-4.79064993423761,
-4.77113401652686,-4.76278265360574,-4.75610047150057,-4.75237866273415,
-4.7491739283282,-4.74523326551119,-4.73914256559883,-4.69853163718669,
-4.68170896766004,-4.67249140236879,-4.66955583113591,-4.66765153314793,
-4.66596008167783,-4.66315345728532,-4.65563211266913,-4.62163345122425,
-4.60359803047165,-4.59189843136318,-4.58729954245183,-4.58400782125478,
-4.58060026889897,-4.575409625978,-4.56007206107721,-4.52478866764198,-4.51274045237939,
-4.50531974472201,-4.5026049912957,-4.500745224134,-4.4987624799809,-4.4954658740778,
-4.48355459791503,-4.45596543489156,-4.43728588230758,-4.42915421528554,
-4.42260810879727,-4.41891459717433,-4.41570760574005,-4.41172985926363,
-4.40551357025942,-4.35996858521503,-4.34194556880708,-4.33739828460921,
-4.33515440472622,-4.33334919027422,-4.33108487220036,-4.3264322554881,
-4.29492302645612,-4.2616947666015,-4.25553988143409,-4.2519285365293,-4.24871055012987,
-4.24460789708212,-4.23796274221672,-4.2049774005901,-4.17498073713445,
-4.17058515702043,-4.16837120942027,-4.16656534220687,-4.16426881425934,
-4.15944717647472,-4.13071733800393,-4.11960641266917,-4.10276015417838,
-4.09513405656174,-4.08890530508023,-4.0852782862359,-4.08206283742387,
-4.0779859024176,-4.07143012023272,-4.02753425890174,-4.01356689740275,
-4.00537696017486,-4.00256179019265,-4.00068235366973,-3.9989689219708,
-3.99604494820572,-3.98766363502708,-3.95423511197276,-3.9365387416129,
-3.92867386204842,-3.92229439490861,-3.91863557603538,-3.91542453955849,
-3.91139674080356,-3.90316849788938,-3.8636243306166,-3.85165705040524),
 .UNSPECIFIED.);
#2860=B_SPLINE_CURVE_WITH_KNOTS('',3,(#118023,#118024,#118025,#118026,#118027,
#118028,#118029,#118030,#118031,#118032,#118033,#118034,#118035,#118036,
#118037,#118038,#118039,#118040,#118041,#118042,#118043,#118044,#118045,
#118046,#118047,#118048,#118049,#118050,#118051,#118052,#118053,#118054,
#118055,#118056,#118057,#118058,#118059,#118060,#118061,#118062,#118063,
#118064,#118065,#118066,#118067,#118068,#118069,#118070,#118071,#118072,
#118073,#118074,#118075,#118076,#118077,#118078,#118079,#118080,#118081,
#118082,#118083,#118084,#118085,#118086,#118087,#118088,#118089,#118090,
#118091,#118092,#118093,#118094,#118095,#118096,#118097,#118098,#118099,
#118100,#118101,#118102,#118103,#118104,#118105,#118106,#118107,#118108,
#118109,#118110,#118111,#118112,#118113,#118114,#118115,#118116,#118117,
#118118,#118119,#118120,#118121,#118122,#118123,#118124,#118125,#118126,
#118127,#118128,#118129,#118130,#118131,#118132,#118133,#118134,#118135,
#118136,#118137,#118138,#118139,#118140,#118141,#118142,#118143,#118144,
#118145,#118146,#118147,#118148,#118149,#118150,#118151,#118152,#118153,
#118154,#118155,#118156,#118157,#118158,#118159,#118160,#118161,#118162,
#118163,#118164,#118165,#118166,#118167,#118168,#118169,#118170,#118171,
#118172,#118173,#118174,#118175,#118176,#118177,#118178,#118179,#118180,
#118181,#118182,#118183,#118184,#118185,#118186,#118187,#118188,#118189,
#118190,#118191,#118192,#118193,#118194,#118195,#118196,#118197,#118198,
#118199,#118200,#118201,#118202,#118203,#118204),.UNSPECIFIED.,.F.,.F.,
(4,2,2,2,2,2,2,2,2,2,2,2,2,2,2,2,2,2,2,2,2,2,2,2,2,2,2,2,2,2,2,2,2,2,2,
2,2,2,2,2,2,2,2,2,2,2,2,2,2,2,2,2,2,2,2,2,2,2,2,2,2,2,2,2,2,2,2,2,2,2,2,
2,2,2,2,2,2,2,2,2,2,2,2,2,2,2,2,2,2,2,4),(-0.991352361073962,-0.990785819095057,
-0.959585665065777,-0.925998326718025,-0.921516348606512,-0.919284995238621,
-0.917479186863969,-0.915200597113129,-0.910475083406357,-0.890872791533548,
-0.856357510059553,-0.843377392364806,-0.838461333403668,-0.835443822219316,
-0.832160681069746,-0.827614016808728,-0.8162781471615,-0.799077934258794,
-0.766442539955367,-0.756836394738463,-0.75376361475442,-0.751829392196886,
-0.749935898574271,-0.747052981652967,-0.738303174683399,-0.722824525338107,
-0.684872011772322,-0.675173622661728,-0.67093078325403,-0.667684848926292,
-0.66417916475887,-0.658524129209144,-0.635813856385057,-0.616312219791162,
-0.593318764350412,-0.58846360436213,-0.586127622592189,-0.584319593906533,
-0.58213793803104,-0.577904195217436,-0.552813301292244,-0.513977098190511,
-0.507683421879438,-0.5036826457543,-0.500473551250248,-0.49679560475275,
-0.490325592592735,-0.460876725520823,-0.429121763263375,-0.42258002933251,
-0.419921706549396,-0.418090261206941,-0.416092750127235,-0.412729337964036,
-0.398469412503287,-0.357073354133918,-0.343504508377478,-0.338509941723328,
-0.335478742611898,-0.332207118541547,-0.327724727981747,-0.316813858900941,
-0.300552487738364,-0.28264373837956,-0.25810368914916,-0.254386489001736,
-0.252290780158785,-0.250471238260137,-0.24800950370595,-0.242260237354865,
-0.233867514389904,-0.204610844989118,-0.178869962029906,-0.172891292784176,
-0.169317285617291,-0.166091685045245,-0.161921924948362,-0.152913474476151,
-0.127226133212799,-0.0947870245274841,-0.0889866339693035,-0.0867034225230636,
-0.0848612479928007,-0.0828855227919735,-0.0796212086708388,-0.066794844031369,
-0.0427074182221363,-0.0122260965999769,-0.00636443773219676,-0.00292236187236719,
-0.000491642045001233),.UNSPECIFIED.);
#2861=B_SPLINE_CURVE_WITH_KNOTS('',3,(#118205,#118206,#118207,#118208,#118209,
#118210,#118211,#118212,#118213,#118214,#118215,#118216),.UNSPECIFIED.,
 .F.,.F.,(4,2,2,2,2,4),(-2.09991228399511,-2.0981766975392,-2.09536860074707,
-2.08896114076016,-2.05232170099698,-2.04098006789499),.UNSPECIFIED.);
#2862=B_SPLINE_CURVE_WITH_KNOTS('',3,(#118217,#118218,#118219,#118220,#118221,
#118222,#118223,#118224,#118225,#118226,#118227,#118228,#118229,#118230,
#118231,#118232,#118233,#118234,#118235,#118236,#118237,#118238,#118239,
#118240,#118241,#118242,#118243,#118244,#118245,#118246,#118247,#118248,
#118249,#118250,#118251,#118252,#118253,#118254,#118255,#118256,#118257,
#118258,#118259,#118260,#118261,#118262,#118263,#118264,#118265,#118266,
#118267,#118268,#118269,#118270,#118271,#118272,#118273,#118274,#118275,
#118276,#118277,#118278,#118279,#118280,#118281,#118282,#118283,#118284,
#118285,#118286,#118287,#118288,#118289,#118290,#118291,#118292,#118293,
#118294,#118295,#118296,#118297,#118298,#118299,#118300,#118301,#118302,
#118303,#118304,#118305,#118306,#118307,#118308,#118309,#118310,#118311,
#118312,#118313,#118314,#118315,#118316,#118317,#118318,#118319,#118320,
#118321,#118322,#118323,#118324,#118325,#118326,#118327,#118328,#118329,
#118330,#118331,#118332,#118333,#118334,#118335,#118336,#118337,#118338,
#118339,#118340,#118341,#118342,#118343,#118344,#118345,#118346,#118347,
#118348,#118349,#118350,#118351,#118352,#118353,#118354,#118355,#118356,
#118357,#118358,#118359,#118360,#118361,#118362,#118363,#118364,#118365,
#118366,#118367,#118368,#118369,#118370,#118371,#118372,#118373,#118374,
#118375,#118376,#118377,#118378,#118379,#118380,#118381,#118382,#118383,
#118384,#118385,#118386,#118387,#118388,#118389,#118390,#118391,#118392,
#118393,#118394,#118395,#118396,#118397,#118398,#118399,#118400,#118401,
#118402,#118403,#118404,#118405,#118406,#118407,#118408,#118409,#118410),
 .UNSPECIFIED.,.F.,.F.,(4,2,2,2,2,2,2,2,2,2,2,2,2,2,2,2,2,2,2,2,2,2,2,2,
2,2,2,2,2,2,2,2,2,2,2,2,2,2,2,2,2,2,2,2,2,2,2,2,2,2,2,2,2,2,2,2,2,2,2,2,
2,2,2,2,2,2,2,2,2,2,2,2,2,2,2,2,2,2,2,2,2,2,2,2,2,2,2,2,2,2,2,2,2,2,2,2,
4),(-3.85165705040524,-3.84773626708953,-3.84170348636172,-3.83720728714827,
-3.83497336099093,-3.83316793769921,-3.83089301598045,-3.82618549112559,
-3.79550069641113,-3.76200603729926,-3.75558970629686,-3.75192316520475,
-3.74871308777263,-3.74469671700828,-3.73834934471633,-3.69342273925938,
-3.67508294657127,-3.6704988670315,-3.66824772085402,-3.66644241898978,
-3.66418518826562,-3.65956975372796,-3.62737305006666,-3.59502640566234,
-3.58873073175417,-3.58508949428779,-3.5818760268942,-3.57782126255208,
-3.57134233279209,-3.52705805416671,-3.50838183381107,-3.50375932557205,
-3.50150069562743,-3.49969534882156,-3.49744548676033,-3.49286816583341,
-3.46018889526995,-3.42823556803621,-3.42195506515446,-3.41831697775172,
-3.41510297692661,-3.41104307937502,-3.4045466152527,-3.36034805304638,
-3.3416255366469,-3.33699773965129,-3.33473805978999,-3.33293267330861,
-3.33068375835262,-3.32611143923264,-3.29337438452813,-3.26191577247669,
-3.25538698090293,-3.25169674423949,-3.24848892995598,-3.24450540488065,
-3.23827053909956,-3.19889354396288,-3.17423895585541,-3.17000794674697,
-3.16782686271051,-3.16601885794631,-3.16368238497483,-3.15882464407283,
-3.13577803230431,-3.10759604463177,-3.09230455359476,-3.08725619975889,
-3.08387736472069,-3.08060255860486,-3.0759183254839,-3.06448126138436,
-3.02850150745686,-3.01355765144878,-3.00500111239543,-3.00214113029365,
-3.00025246372277,-2.99831260667428,-2.99521349854256,-2.9853718913831,
-2.95627064920763,-2.93697235825231,-2.92474164431994,-2.92006767763124,
-2.9167618460622,-2.91376968455636,-2.90899709029393,-2.89700330787531,
-2.85815267040784,-2.84563357950202,-2.83801740928312,-2.83527596055657,
-2.83341087066797,-2.83143641886148,-2.82817892831593,-2.81671901668128,
-2.80139424742162),.UNSPECIFIED.);
#2863=B_SPLINE_CURVE_WITH_KNOTS('',3,(#118415,#118416,#118417,#118418,#118419,
#118420,#118421,#118422,#118423,#118424,#118425,#118426,#118427,#118428,
#118429,#118430,#118431,#118432,#118433,#118434,#118435,#118436,#118437,
#118438,#118439,#118440,#118441,#118442,#118443,#118444,#118445,#118446,
#118447,#118448,#118449,#118450,#118451,#118452,#118453,#118454,#118455,
#118456,#118457,#118458,#118459,#118460,#118461,#118462,#118463,#118464,
#118465,#118466,#118467,#118468,#118469,#118470,#118471,#118472,#118473,
#118474,#118475,#118476,#118477,#118478,#118479,#118480,#118481,#118482,
#118483,#118484,#118485,#118486,#118487,#118488,#118489,#118490,#118491,
#118492,#118493,#118494,#118495,#118496,#118497,#118498,#118499,#118500,
#118501,#118502,#118503,#118504,#118505,#118506,#118507,#118508,#118509,
#118510,#118511,#118512,#118513,#118514,#118515,#118516,#118517,#118518,
#118519,#118520,#118521,#118522,#118523,#118524,#118525,#118526,#118527,
#118528,#118529,#118530,#118531,#118532,#118533,#118534,#118535,#118536,
#118537,#118538,#118539,#118540,#118541,#118542,#118543,#118544,#118545,
#118546,#118547,#118548,#118549,#118550,#118551,#118552,#118553,#118554,
#118555,#118556,#118557,#118558,#118559,#118560,#118561,#118562,#118563,
#118564,#118565,#118566,#118567,#118568,#118569,#118570,#118571,#118572,
#118573,#118574,#118575,#118576,#118577,#118578,#118579,#118580,#118581,
#118582,#118583,#118584,#118585,#118586,#118587,#118588,#118589,#118590,
#118591,#118592,#118593,#118594,#118595,#118596,#118597,#118598,#118599,
#118600,#118601,#118602,#118603,#118604,#118605,#118606,#118607,#118608,
#118609,#118610,#118611,#118612,#118613,#118614,#118615,#118616,#118617,
#118618,#118619,#118620,#118621,#118622),.UNSPECIFIED.,.F.,.F.,(4,2,2,2,
2,2,2,2,2,2,2,2,2,2,2,2,2,2,2,2,2,2,2,2,2,2,2,2,2,2,2,2,2,2,2,2,2,2,2,2,
2,2,2,2,2,2,2,2,2,2,2,2,2,2,2,2,2,2,2,2,2,2,2,2,2,2,2,2,2,2,2,2,2,2,2,2,
2,2,2,2,2,2,2,2,2,2,2,2,2,2,2,2,2,2,2,2,2,2,2,2,2,2,2,4),(-2.04123955694236,
-2.01327501084785,-2.00679074355191,-2.00310945529361,-1.99990017148169,
-1.99590272256132,-1.98962155099611,-1.9506852467667,-1.92569508725374,
-1.92146217165324,-1.91928049978993,-1.91747221512462,-1.91513556324801,
-1.91027792484376,-1.88593457720521,-1.86376311785202,-1.85095801790333,
-1.84174363074351,-1.83753691654822,-1.83430588785183,-1.83074906089007,
-1.82485459557057,-1.80010304267298,-1.76991672286717,-1.76140482883313,
-1.75559528866267,-1.75312304129038,-1.75130172600092,-1.74921100262007,
-1.74551774366588,-1.72352468874556,-1.71925502626877,-1.69708222718193,
-1.68428057181914,-1.67506800306226,-1.67086162494451,-1.66763065960917,
-1.66407370809877,-1.65817857445507,-1.63340415052541,-1.6032382173864,
-1.5947289241423,-1.58892068591823,-1.58644866549858,-1.5846273881578,-1.5825365565741,
-1.57884278307905,-1.55670484848467,-1.55254233311288,-1.53035892953634,
-1.51758528106422,-1.50838738289188,-1.5041835748061,-1.50095295246795,
-1.49739474956413,-1.49149366469679,-1.46651784237616,-1.43652744124927,
-1.42804036269385,-1.4222431656361,-1.41977299473349,-1.41795195925015,
-1.41586010095475,-1.41216169650971,-1.38892565404076,-1.38639127722076,
-1.36357218520573,-1.35086214106202,-1.34169761278491,-1.33749966044732,
-1.33426981455549,-1.33070874082922,-1.32479400527926,-1.29929036373455,
-1.27861601125049,-1.26460256702155,-1.25639487085693,-1.25357719866206,
-1.25169701972495,-1.24998363870439,-1.24706102653929,-1.23869241426644,
-1.20526110597922,-1.18756357370876,-1.17969819538669,-1.17331823412724,
-1.16965889852808,-1.16644724285562,-1.16241841512708,-1.15602972836495,
-1.11818667978574,-1.09231760570813,-1.08808005212805,-1.08589749888602,
-1.08408936332077,-1.08175403657471,-1.07690282671219,-1.05045357632628,
-1.0144885612206,-1.007954313239,-1.0038831925696,-1.00066771132886,-0.997035755158936,
-0.991352361073962),.UNSPECIFIED.);
#2864=B_SPLINE_CURVE_WITH_KNOTS('',3,(#118623,#118624,#118625,#118626,#118627,
#118628,#118629,#118630,#118631,#118632,#118633,#118634,#118635,#118636,
#118637,#118638,#118639,#118640,#118641,#118642,#118643,#118644,#118645,
#118646,#118647,#118648,#118649,#118650,#118651,#118652,#118653,#118654,
#118655,#118656,#118657,#118658,#118659,#118660,#118661,#118662,#118663,
#118664,#118665,#118666,#118667,#118668,#118669,#118670,#118671,#118672,
#118673,#118674,#118675,#118676,#118677,#118678,#118679,#118680,#118681,
#118682,#118683,#118684,#118685,#118686,#118687,#118688,#118689,#118690,
#118691,#118692,#118693,#118694,#118695,#118696,#118697,#118698,#118699,
#118700,#118701,#118702,#118703,#118704,#118705,#118706,#118707,#118708,
#118709,#118710,#118711,#118712,#118713,#118714,#118715,#118716,#118717,
#118718,#118719,#118720,#118721,#118722,#118723,#118724,#118725,#118726,
#118727,#118728,#118729,#118730,#118731,#118732,#118733,#118734,#118735,
#118736,#118737,#118738,#118739,#118740,#118741,#118742,#118743,#118744,
#118745,#118746,#118747,#118748,#118749,#118750,#118751,#118752,#118753,
#118754,#118755,#118756,#118757,#118758,#118759,#118760,#118761,#118762,
#118763,#118764,#118765,#118766,#118767,#118768,#118769,#118770,#118771,
#118772,#118773,#118774,#118775,#118776,#118777,#118778,#118779,#118780,
#118781,#118782,#118783,#118784,#118785,#118786,#118787,#118788,#118789,
#118790,#118791,#118792,#118793,#118794,#118795,#118796,#118797,#118798,
#118799,#118800,#118801,#118802,#118803,#118804,#118805,#118806,#118807,
#118808,#118809,#118810,#118811,#118812,#118813,#118814,#118815,#118816,
#118817,#118818,#118819,#118820,#118821,#118822,#118823,#118824,#118825,
#118826,#118827,#118828,#118829,#118830),.UNSPECIFIED.,.F.,.F.,(4,2,2,2,
2,2,2,2,2,2,2,2,2,2,2,2,2,2,2,2,2,2,2,2,2,2,2,2,2,2,2,2,2,2,2,2,2,2,2,2,
2,2,2,2,2,2,2,2,2,2,2,2,2,2,2,2,2,2,2,2,2,2,2,2,2,2,2,2,2,2,2,2,2,2,2,2,
2,2,2,2,2,2,2,2,2,2,2,2,2,2,2,2,2,2,2,2,2,2,2,2,2,2,2,4),(-2.80139424742162,
-2.78879988481108,-2.76059118451529,-2.75468573714338,-2.75112695351419,
-2.7478971404036,-2.74376640214512,-2.73472788769955,-2.69208714102528,
-2.67912025544343,-2.67132247751412,-2.66855705497056,-2.66668731004663,
-2.66496282540459,-2.66198230834239,-2.65315624447851,-2.62327143071968,
-2.59897543857137,-2.58997243766197,-2.58580315645675,-2.58257717533914,
-2.57900201601199,-2.57301969250743,-2.54358894258563,-2.52138064730654,
-2.51097123635177,-2.50426305974586,-2.5016495181741,-2.49980749003473,
-2.49778603533429,-2.49431287701566,-2.48006188648858,-2.44972465011842,
-2.42668927079624,-2.42101499953902,-2.41750539194453,-2.41426116266904,
-2.40995431598043,-2.40014826329148,-2.38618880427075,-2.36563868474424,
-2.3625331492555,-2.33981071641887,-2.33611569806529,-2.33402482029518,
-2.33220405294256,-2.32973347922363,-2.32393224533036,-2.31543573385929,
-2.28538439452081,-2.26043431254946,-2.25453367291383,-2.25097603889298,
-2.24774616505472,-2.24354369600926,-2.23435035092273,-2.22158656367306,
-2.19941354038118,-2.19533658760213,-2.17311683009265,-2.16942380250306,
-2.1673334092204,-2.16551258808853,-2.1630413201258,-2.15723576975335,-2.14873051427573,
-2.11860951176809,-2.09374024754866,-2.08784205241695,-2.08428496192231,
-2.08105499242064,-2.07685155247179,-2.06765247109752,-2.05487764317136,
-2.03270916866623,-2.02857009567257,-2.00642906012432,-2.00273635625956,
-2.00064603668727,-1.99882515297661,-1.99635364640066,-1.99054693353229,
-1.98203934201765,-1.95189874177632,-1.92705684519228,-1.92115955207053,
-1.91760263146637,-1.9143725745099,-1.91016866896318,-1.90096704712059,
-1.88818741556761,-1.86602095158355,-1.86185377720641,-1.83974773467214,
-1.83605522742889,-1.83396497793084,-1.83214430146993,-1.82967317323945,
-1.82386741517223,-1.815361459849,-1.78523282504622,-1.76037274810103,-1.75447527727419,
-1.75139041054252),.UNSPECIFIED.);
#2865=B_SPLINE_CURVE_WITH_KNOTS('',3,(#118836,#118837,#118838,#118839,#118840,
#118841,#118842,#118843,#118844,#118845,#118846,#118847,#118848,#118849,
#118850,#118851,#118852,#118853,#118854,#118855,#118856,#118857,#118858,
#118859,#118860,#118861,#118862,#118863,#118864,#118865,#118866,#118867,
#118868,#118869,#118870,#118871,#118872,#118873,#118874,#118875,#118876,
#118877,#118878,#118879,#118880,#118881,#118882,#118883,#118884,#118885,
#118886,#118887,#118888,#118889,#118890,#118891,#118892,#118893,#118894,
#118895,#118896,#118897,#118898,#118899,#118900,#118901,#118902,#118903,
#118904,#118905,#118906,#118907,#118908,#118909,#118910,#118911,#118912,
#118913,#118914,#118915,#118916,#118917,#118918,#118919,#118920,#118921,
#118922,#118923,#118924,#118925,#118926,#118927,#118928,#118929,#118930,
#118931,#118932,#118933,#118934,#118935,#118936,#118937,#118938,#118939,
#118940,#118941,#118942,#118943,#118944,#118945,#118946,#118947,#118948,
#118949,#118950,#118951,#118952,#118953,#118954,#118955,#118956,#118957,
#118958,#118959,#118960,#118961,#118962,#118963,#118964,#118965),
 .UNSPECIFIED.,.F.,.F.,(4,2,2,2,2,2,2,2,2,2,2,2,2,2,2,2,2,2,2,2,2,2,2,2,
2,2,2,2,2,2,2,2,2,2,2,2,2,2,2,2,2,2,2,2,2,2,2,2,2,2,2,2,2,2,2,2,2,2,2,2,
2,2,2,2,4),(-0.701622587363262,-0.69782520809542,-0.674829255171103,-0.669922846048609,
-0.667616398149043,-0.665811282498163,-0.663608201244988,-0.659287945074347,
-0.630959998494923,-0.595874548539514,-0.589266617774786,-0.585162989422959,
-0.581929453747833,-0.578284673240364,-0.572030341479378,-0.538732930775711,
-0.507736833265961,-0.503053466152945,-0.500771249654345,-0.498936855248173,
-0.496634187412443,-0.491925021622171,-0.47271714137948,-0.438767709036483,
-0.426269118459773,-0.421396439902457,-0.41836328394742,-0.415028341171548,
-0.410341821925662,-0.398238653475179,-0.379359681618992,-0.35152676465907,
-0.339810678256997,-0.336535629198157,-0.33456067082642,-0.332769732602333,
-0.330225049012681,-0.323393145686127,-0.286831973998349,-0.258805743436394,
-0.252937601621296,-0.249485437965486,-0.246408799842315,-0.242490682540656,
-0.234287538356714,-0.210701559508584,-0.183370211347027,-0.171493461538258,
-0.168263425178072,-0.166329600535944,-0.164466454136752,-0.161776174892017,
-0.154649964298831,-0.116968940589261,-0.0871764818775304,-0.0806335737492376,
-0.0766880313159956,-0.073094175717419,-0.068380569947616,-0.0576891236866487,
-0.0323137982564055,-0.00779173997406027,-0.00345811667600707,-0.00158327751243333,
-5.87629350645707E-5),.UNSPECIFIED.);
#2866=B_SPLINE_CURVE_WITH_KNOTS('',3,(#118968,#118969,#118970,#118971,#118972,
#118973,#118974,#118975,#118976,#118977,#118978,#118979,#118980,#118981,
#118982,#118983,#118984,#118985,#118986,#118987,#118988,#118989,#118990,
#118991,#118992,#118993,#118994,#118995,#118996,#118997,#118998,#118999,
#119000,#119001,#119002,#119003,#119004,#119005,#119006,#119007,#119008,
#119009,#119010,#119011,#119012,#119013,#119014,#119015,#119016,#119017,
#119018,#119019,#119020,#119021,#119022,#119023,#119024,#119025,#119026,
#119027,#119028,#119029,#119030,#119031,#119032,#119033,#119034,#119035,
#119036,#119037,#119038,#119039,#119040,#119041,#119042,#119043,#119044,
#119045,#119046,#119047,#119048,#119049,#119050,#119051,#119052,#119053,
#119054,#119055,#119056,#119057,#119058,#119059,#119060,#119061,#119062,
#119063,#119064,#119065,#119066,#119067,#119068,#119069,#119070,#119071,
#119072,#119073,#119074,#119075,#119076,#119077,#119078,#119079,#119080,
#119081,#119082,#119083,#119084,#119085,#119086,#119087,#119088,#119089,
#119090,#119091,#119092,#119093,#119094,#119095,#119096,#119097,#119098,
#119099,#119100,#119101,#119102,#119103,#119104,#119105,#119106,#119107,
#119108,#119109,#119110,#119111,#119112,#119113,#119114,#119115,#119116,
#119117,#119118,#119119,#119120,#119121,#119122,#119123,#119124,#119125,
#119126,#119127,#119128,#119129,#119130,#119131,#119132,#119133,#119134,
#119135,#119136,#119137,#119138,#119139,#119140,#119141,#119142,#119143,
#119144,#119145,#119146,#119147,#119148,#119149,#119150,#119151,#119152,
#119153,#119154,#119155),.UNSPECIFIED.,.F.,.F.,(4,2,2,2,2,2,2,2,2,2,2,2,
2,2,2,2,2,2,2,2,2,2,2,2,2,2,2,2,2,2,2,2,2,2,2,2,2,2,2,2,2,2,2,2,2,2,2,2,
2,2,2,2,2,2,2,2,2,2,2,2,2,2,2,2,2,2,2,2,2,2,2,2,2,2,2,2,2,2,2,2,2,2,2,2,
2,2,2,2,2,2,2,2,2,4),(-1.97963597789807,-1.97911067462062,-1.97224667709571,
-1.93765234953483,-1.91989061416732,-1.91197821045077,-1.9055506793358,
-1.9018562152793,-1.8986078498892,-1.89452319207106,-1.88801757096771,-1.85356143477461,
-1.8263655964811,-1.82198065731588,-1.81974157734617,-1.81790619020366,
-1.8155529425272,-1.81067156433301,-1.78639735018608,-1.76444854551698,
-1.75161386122014,-1.74237922748276,-1.73815580252188,-1.73490801345122,
-1.73132830795588,-1.7253841935851,-1.699589449833,-1.67019323447981,-1.66177185612889,
-1.65600305061343,-1.65353308438504,-1.65171121529384,-1.6496247175336,
-1.64592526592048,-1.62182019415646,-1.62032066973509,-1.59985864135478,
-1.58571524772036,-1.57582953022289,-1.57152386326298,-1.56829467044939,
-1.56481536620152,-1.55922304091608,-1.53963040587853,-1.49637493856359,
-1.48949938211316,-1.48687155964858,-1.48503396364113,-1.4830266243612,
-1.47961824512937,-1.46635505603671,-1.43972422161585,-1.42141361064092,
-1.40959049038942,-1.40496920547385,-1.40166911105502,-1.39866083063639,
-1.39381505113879,-1.38135377026963,-1.34650958156531,-1.3319022443993,
-1.32617103933515,-1.32184531493975,-1.31964157356574,-1.31783128421811,
-1.31551153706946,-1.31057397859131,-1.28586393467364,-1.25896291674913,
-1.24895028845789,-1.24127410510196,-1.23735060493909,-1.23414477678659,
-1.23040459988526,-1.22382601853695,-1.1824229670469,-1.16601160169481,
-1.15693324864388,-1.15401263966414,-1.15211117226386,-1.15041776427746,
-1.1475982143147,-1.13998043185423,-1.10913161968521,-1.08425772901165,
-1.07526848621783,-1.07110341817376,-1.06787988252065,-1.06430665059646,
-1.05832579086072,-1.02900642671826,-1.00699144824307,-0.991285459946718,
-0.991277804245244),.UNSPECIFIED.);
#2867=B_SPLINE_CURVE_WITH_KNOTS('',3,(#119161,#119162,#119163,#119164,#119165,
#119166,#119167,#119168,#119169,#119170,#119171,#119172,#119173,#119174,
#119175,#119176,#119177,#119178,#119179,#119180,#119181,#119182,#119183,
#119184,#119185,#119186,#119187,#119188,#119189,#119190,#119191,#119192,
#119193,#119194,#119195,#119196,#119197,#119198,#119199,#119200,#119201,
#119202,#119203,#119204,#119205,#119206,#119207,#119208,#119209,#119210,
#119211,#119212,#119213,#119214,#119215,#119216,#119217,#119218,#119219,
#119220,#119221,#119222,#119223,#119224,#119225,#119226,#119227,#119228,
#119229,#119230,#119231,#119232,#119233,#119234),.UNSPECIFIED.,.F.,.F.,
(4,2,2,2,2,2,2,2,2,2,2,2,2,2,2,2,2,2,2,2,2,2,2,2,2,2,2,2,2,2,2,2,2,2,2,
2,4),(-0.358752339019158,-0.35758003104028,-0.340398688796483,-0.336826897283715,
-0.33476676533837,-0.333010439188268,-0.330665170257151,-0.325132231676164,
-0.31707514359999,-0.290061737059928,-0.258856486316567,-0.25295401397713,
-0.249494058015947,-0.246417937613128,-0.242510640506838,-0.234368903731933,
-0.199769648266984,-0.174157594760246,-0.169316644024535,-0.167058190656923,
-0.165265662645593,-0.163073803167974,-0.158845281495978,-0.153310662188677,
-0.139694106829365,-0.103511073302855,-0.0857756328518154,-0.0799370029750358,
-0.0761379594961528,-0.0724812087849253,-0.0673685912890846,-0.0538912888095538,
-0.030966518726725,-0.00771475696196283,-0.00343253357673936,-0.00157316844153016,
-5.8766376665821E-5),.UNSPECIFIED.);
#2868=B_SPLINE_CURVE_WITH_KNOTS('',3,(#119237,#119238,#119239,#119240,#119241,
#119242,#119243,#119244,#119245,#119246,#119247,#119248,#119249,#119250,
#119251,#119252,#119253,#119254,#119255,#119256,#119257,#119258,#119259,
#119260,#119261,#119262,#119263,#119264,#119265,#119266,#119267,#119268,
#119269,#119270,#119271,#119272,#119273,#119274,#119275,#119276,#119277,
#119278,#119279,#119280,#119281,#119282,#119283,#119284,#119285,#119286,
#119287,#119288,#119289,#119290,#119291,#119292,#119293,#119294,#119295,
#119296,#119297,#119298,#119299,#119300,#119301,#119302,#119303,#119304,
#119305,#119306,#119307,#119308,#119309,#119310,#119311,#119312,#119313,
#119314,#119315,#119316,#119317,#119318,#119319,#119320,#119321,#119322,
#119323,#119324,#119325,#119326,#119327,#119328,#119329,#119330,#119331,
#119332,#119333,#119334,#119335,#119336,#119337,#119338,#119339,#119340,
#119341,#119342,#119343,#119344,#119345,#119346,#119347,#119348,#119349,
#119350,#119351,#119352,#119353,#119354,#119355,#119356,#119357,#119358),
 .UNSPECIFIED.,.F.,.F.,(4,2,2,2,2,2,2,2,2,2,2,2,2,2,2,2,2,2,2,2,2,2,2,2,
2,2,2,2,2,2,2,2,2,2,2,2,2,2,2,2,2,2,2,2,2,2,2,2,2,2,2,2,2,2,2,2,2,2,2,2,
4),(-1.75473859914493,-1.75154088040687,-1.72689079662622,-1.70467625101938,
-1.69173746421963,-1.68242362321274,-1.67817272951846,-1.67490672226881,
-1.67130890727376,-1.66533530028674,-1.63676084184676,-1.61487708686701,
-1.5998560152629,-1.59640767418699,-1.59436566649252,-1.59251150052433,
-1.59024704870894,-1.58578837015164,-1.56116797072278,-1.53901736556639,
-1.52648093052477,-1.51740303061522,-1.51320745070685,-1.50996354794196,
-1.50637047787112,-1.50036170283648,-1.47112902592979,-1.44979535915428,
-1.43862692122266,-1.43157598618139,-1.42890757062421,-1.42705372906987,
-1.42506024854931,-1.42168964849452,-1.40884212253478,-1.38191893140923,
-1.36350388087488,-1.35165518326397,-1.34705047948789,-1.34377172622376,
-1.34039291048129,-1.33527761912014,-1.32051306287125,-1.2844406463443,
-1.27225590916121,-1.26478465725884,-1.26207378716518,-1.26022197076231,
-1.25824532632989,-1.25497638312579,-1.24337961458778,-1.21178438857809,
-1.19536079393811,-1.18437122843983,-1.17987288167479,-1.1765948503032,
-1.17356125046985,-1.16857057843087,-1.15505860396329,-1.12118637585851,
-1.10916127312679),.UNSPECIFIED.);
#2869=B_SPLINE_CURVE_WITH_KNOTS('',3,(#119363,#119364,#119365,#119366,#119367,
#119368,#119369,#119370,#119371,#119372,#119373,#119374,#119375,#119376,
#119377,#119378,#119379,#119380,#119381,#119382,#119383,#119384,#119385,
#119386,#119387,#119388,#119389,#119390,#119391,#119392,#119393,#119394,
#119395,#119396,#119397,#119398,#119399,#119400,#119401,#119402,#119403,
#119404,#119405,#119406,#119407,#119408,#119409,#119410,#119411,#119412,
#119413,#119414,#119415,#119416,#119417,#119418,#119419,#119420,#119421,
#119422,#119423,#119424,#119425,#119426,#119427,#119428,#119429,#119430,
#119431,#119432,#119433,#119434,#119435,#119436,#119437,#119438,#119439,
#119440,#119441,#119442,#119443,#119444,#119445,#119446,#119447,#119448,
#119449,#119450,#119451,#119452,#119453,#119454,#119455,#119456,#119457,
#119458,#119459,#119460,#119461,#119462,#119463,#119464,#119465,#119466,
#119467,#119468,#119469,#119470,#119471,#119472,#119473,#119474,#119475,
#119476,#119477,#119478,#119479,#119480,#119481,#119482,#119483,#119484,
#119485,#119486,#119487,#119488,#119489,#119490,#119491,#119492,#119493,
#119494,#119495,#119496,#119497,#119498,#119499,#119500,#119501,#119502,
#119503,#119504,#119505,#119506,#119507,#119508,#119509,#119510,#119511,
#119512,#119513,#119514,#119515,#119516,#119517,#119518,#119519,#119520,
#119521,#119522,#119523,#119524,#119525,#119526,#119527,#119528,#119529,
#119530,#119531,#119532,#119533,#119534,#119535,#119536,#119537,#119538,
#119539,#119540,#119541,#119542,#119543,#119544,#119545,#119546,#119547,
#119548,#119549,#119550,#119551,#119552,#119553,#119554,#119555,#119556,
#119557,#119558,#119559,#119560,#119561,#119562,#119563,#119564,#119565,
#119566),.UNSPECIFIED.,.F.,.F.,(4,2,2,2,2,2,2,2,2,2,2,2,2,2,2,2,2,2,2,2,
2,2,2,2,2,2,2,2,2,2,2,2,2,2,2,2,2,2,2,2,2,2,2,2,2,2,2,2,2,2,2,2,2,2,2,2,
2,2,2,2,2,2,2,2,2,2,2,2,2,2,2,2,2,2,2,2,2,2,2,2,2,2,2,2,2,2,2,2,2,2,2,2,
2,2,2,2,2,2,2,2,2,4),(-1.4082992289097,-1.4006552888223,-1.3878393759836,
-1.36569920472157,-1.36139004195681,-1.33948882989881,-1.33579769323099,
-1.33370781087495,-1.33188807180438,-1.32941841755152,-1.32361485359034,
-1.31511156287969,-1.28499140100962,-1.26012140732392,-1.25422612287674,
-1.25067145026165,-1.24744414566674,-1.24324490224264,-1.23405843495863,
-1.22130441803123,-1.1991395030373,-1.1951252761621,-1.17284887851717,-1.16915780297844,
-1.16706871220799,-1.16524829673333,-1.162777307309,-1.15697344907893,-1.14847158070023,
-1.11837615034095,-1.09347778154855,-1.08757753858206,-1.08401920986116,
-1.08078805620498,-1.07658290187221,-1.0673785916205,-1.05459309089071,
-1.03245285482807,-1.02830520677559,-1.00622478069049,-1.00253116757083,
-1.00043958145166,-0.99861445840005,-0.996133848230994,-0.990294586525929,
-0.981724246627302,-0.951048798860375,-0.927028553861187,-0.921159335391849,
-0.917605115086725,-0.914368165997088,-0.910141523679551,-0.900829494129505,
-0.85647447470958,-0.839503876800746,-0.835920270476699,-0.833854517442367,
-0.832036735584689,-0.829539355501921,-0.823514827105592,-0.814550871432306,
-0.780451195333079,-0.759627894309259,-0.753970985735232,-0.750478125285507,
-0.747253981141342,-0.742981431706823,-0.733293912473096,-0.719547665976067,
-0.698716209736333,-0.695034411371129,-0.672818392628126,-0.66913584587516,
-0.667053237701345,-0.665230692390564,-0.662754472044112,-0.656947526264486,
-0.648448269514703,-0.618457088136563,-0.593327152240948,-0.587399045923802,
-0.583822979777057,-0.580574709162931,-0.576345221812675,-0.567073941984854,
-0.554170094308864,-0.53228738943782,-0.528695248397369,-0.506193517731935,
-0.502481013139736,-0.500375016286649,-0.498518315441251,-0.495976296299316,
-0.489921469046412,-0.454074013905421,-0.428429311324733,-0.422512079111116,
-0.418926209619868,-0.415657034357046,-0.411381726273356,-0.401926205740997,
-0.358752339019158),.UNSPECIFIED.);
#2870=B_SPLINE_CURVE_WITH_KNOTS('',3,(#119567,#119568,#119569,#119570,#119571,
#119572,#119573,#119574,#119575,#119576,#119577,#119578,#119579,#119580,
#119581,#119582,#119583,#119584,#119585,#119586,#119587,#119588,#119589,
#119590,#119591,#119592,#119593,#119594,#119595,#119596,#119597,#119598,
#119599,#119600,#119601,#119602,#119603,#119604,#119605,#119606,#119607,
#119608,#119609,#119610,#119611,#119612,#119613,#119614,#119615,#119616,
#119617,#119618,#119619,#119620,#119621,#119622,#119623,#119624,#119625,
#119626,#119627,#119628,#119629,#119630,#119631,#119632,#119633,#119634,
#119635,#119636,#119637,#119638,#119639,#119640,#119641,#119642,#119643,
#119644,#119645,#119646,#119647,#119648,#119649,#119650,#119651,#119652,
#119653,#119654,#119655,#119656,#119657,#119658,#119659,#119660,#119661,
#119662,#119663,#119664,#119665,#119666,#119667,#119668,#119669,#119670,
#119671,#119672,#119673,#119674,#119675,#119676,#119677,#119678,#119679,
#119680,#119681,#119682,#119683,#119684,#119685,#119686,#119687,#119688,
#119689,#119690,#119691,#119692,#119693,#119694,#119695,#119696,#119697,
#119698,#119699,#119700,#119701,#119702,#119703,#119704,#119705,#119706,
#119707,#119708,#119709,#119710,#119711,#119712,#119713,#119714,#119715,
#119716,#119717,#119718,#119719,#119720,#119721,#119722,#119723,#119724,
#119725,#119726,#119727,#119728,#119729,#119730,#119731,#119732,#119733,
#119734,#119735,#119736,#119737,#119738,#119739,#119740,#119741,#119742,
#119743,#119744,#119745,#119746,#119747,#119748,#119749,#119750,#119751,
#119752,#119753,#119754,#119755,#119756,#119757,#119758,#119759,#119760,
#119761,#119762,#119763,#119764,#119765,#119766,#119767,#119768,#119769,
#119770,#119771,#119772,#119773,#119774,#119775,#119776,#119777,#119778,
#119779,#119780,#119781,#119782,#119783,#119784),.UNSPECIFIED.,.F.,.F.,
(4,2,2,2,2,2,2,2,2,2,2,2,2,2,2,2,2,2,2,2,2,2,2,2,2,2,2,2,2,2,2,2,2,2,2,
2,2,2,2,2,2,2,2,2,2,2,2,2,2,2,2,2,2,2,2,2,2,2,2,2,2,2,2,2,2,2,2,2,2,2,2,
2,2,2,2,2,2,2,2,2,2,2,2,2,2,2,2,2,2,2,2,2,2,2,2,2,2,2,2,2,2,2,2,2,2,2,2,
2,4),(-1.10916127312679,-1.10684992829868,-1.09851897869292,-1.09568224371337,
-1.09379526882295,-1.09208276821439,-1.08916905046944,-1.08087619471203,
-1.05058953079179,-1.02100908595183,-1.01506303853347,-1.01149523805187,
-1.00826689314242,-1.00415120741369,-0.995201347428553,-0.952436126518047,
-0.93945480919547,-0.931651379837895,-0.928885507616449,-0.927016043747836,
-0.925051226932677,-0.921832938457102,-0.910792826002045,-0.878916108873371,
-0.854168052641419,-0.848277081248516,-0.84472359077435,-0.841496482060365,
-0.837296272257313,-0.828102860813718,-0.81533635407929,-0.793159258660976,
-0.789112536219431,-0.766859675684666,-0.763168752377515,-0.761080089928424,
-0.759260204177435,-0.756790363183674,-0.750991523428633,-0.742499095167402,
-0.71247119994093,-0.68750691652322,-0.681606340209787,-0.678048807414275,
-0.67481903875931,-0.670616685451146,-0.661423164336513,-0.64865779563753,
-0.626502259855582,-0.622360491332471,-0.60023525072509,-0.596543066681321,
-0.594452742674484,-0.592631978737739,-0.590160421532918,-0.584351603822365,
-0.575839099370099,-0.545650940385055,-0.520879550394758,-0.514985748646116,
-0.51143015604782,-0.508200813862756,-0.503997136345933,-0.494793055567726,
-0.482007651843694,-0.459848394515748,-0.455649654479213,-0.433590903204346,
-0.429899480218252,-0.42780983088922,-0.425989623366819,-0.423519102918438,
-0.417714764405128,-0.409210841403266,-0.379088193343223,-0.354238617680801,
-0.348342837619647,-0.34478712940166,-0.341558375964348,-0.337356472947442,
-0.328160640260706,-0.315390415839926,-0.293226997624212,-0.289097950171124,
-0.266951707406135,-0.263260239378087,-0.261170692832636,-0.25935047358136,
-0.256879939267643,-0.251076042327961,-0.2425731240137,-0.212458766561942,
-0.18758130092732,-0.181695530236592,-0.178141748568729,-0.174912128415632,
-0.17070532208897,-0.16148252732833,-0.148660855434975,-0.126636360293058,
-0.122694179406678,-0.100322084771383,-0.0966296456084877,-0.0945397446247031,
-0.0927195097909353,-0.0902491939164962,-0.0844464209777026,-0.0759456971816959,
-0.059479256607861),.UNSPECIFIED.);
#2871=B_SPLINE_CURVE_WITH_KNOTS('',3,(#119789,#119790,#119791,#119792,#119793,
#119794,#119795,#119796,#119797,#119798,#119799,#119800,#119801,#119802,
#119803,#119804,#119805,#119806,#119807,#119808,#119809,#119810,#119811,
#119812,#119813,#119814,#119815,#119816,#119817,#119818,#119819,#119820,
#119821,#119822,#119823,#119824,#119825,#119826,#119827,#119828,#119829,
#119830,#119831,#119832,#119833,#119834,#119835,#119836,#119837,#119838,
#119839,#119840,#119841,#119842,#119843,#119844,#119845,#119846,#119847,
#119848,#119849,#119850,#119851,#119852,#119853,#119854,#119855,#119856,
#119857,#119858,#119859,#119860,#119861,#119862,#119863,#119864,#119865,
#119866,#119867,#119868,#119869,#119870,#119871,#119872,#119873,#119874,
#119875,#119876,#119877,#119878,#119879,#119880,#119881,#119882,#119883,
#119884,#119885,#119886,#119887,#119888,#119889,#119890,#119891,#119892,
#119893,#119894,#119895,#119896,#119897,#119898,#119899,#119900,#119901,
#119902,#119903,#119904,#119905,#119906,#119907,#119908,#119909,#119910,
#119911,#119912,#119913,#119914,#119915,#119916,#119917,#119918,#119919,
#119920,#119921,#119922,#119923,#119924,#119925,#119926,#119927,#119928,
#119929,#119930,#119931,#119932,#119933,#119934,#119935,#119936,#119937,
#119938,#119939,#119940,#119941,#119942,#119943,#119944,#119945,#119946,
#119947,#119948,#119949,#119950,#119951,#119952,#119953,#119954,#119955,
#119956,#119957,#119958,#119959,#119960,#119961,#119962,#119963,#119964,
#119965,#119966,#119967,#119968,#119969,#119970,#119971,#119972,#119973,
#119974,#119975,#119976,#119977,#119978,#119979,#119980,#119981,#119982,
#119983,#119984,#119985,#119986,#119987,#119988,#119989,#119990,#119991,
#119992,#119993,#119994,#119995,#119996,#119997,#119998,#119999,#120000,
#120001,#120002),.UNSPECIFIED.,.F.,.F.,(4,2,2,2,2,2,2,2,2,2,2,2,2,2,2,2,
2,2,2,2,2,2,2,2,2,2,2,2,2,2,2,2,2,2,2,2,2,2,2,2,2,2,2,2,2,2,2,2,2,2,2,2,
2,2,2,2,2,2,2,2,2,2,2,2,2,2,2,2,2,2,2,2,2,2,2,2,2,2,2,2,2,2,2,2,2,2,2,2,
2,2,2,2,2,2,2,2,2,2,2,2,2,2,2,2,2,2,4),(-2.45787557075319,-2.4560892806585,
-2.43171211345447,-2.42270830022384,-2.41853906802341,-2.41531325268146,
-2.41173837894919,-2.40575670094468,-2.37569865246704,-2.35160629332699,
-2.34273784398871,-2.33675330716433,-2.33425255668742,-2.33242782833755,
-2.33035348416521,-2.32673194141415,-2.30807580213373,-2.26742523312263,
-2.25699742029425,-2.25291250078726,-2.24990328817644,-2.2466144910873,
-2.24203251229508,-2.23045027627985,-2.21268728113272,-2.17918595748121,
-2.17099751766033,-2.16809907310687,-2.16639057692035,-2.16450635358482,
-2.1616670611253,-2.15328020122357,-2.13879036408145,-2.10444614120628,
-2.09129183178161,-2.08635250401723,-2.08333129942591,-2.08005233564363,
-2.07552660338358,-2.06432774102652,-2.04743252989996,-2.01522869464926,
-2.00487887289385,-2.00172563327065,-1.99977413889167,-1.99789453183547,
-1.9950783105745,-1.98687966763053,-1.97288679736377,-1.95223340085464,
-1.92666144498823,-1.92074551811907,-1.91718469412539,-1.91395569200765,
-1.90975971082744,-1.90060298394815,-1.88790836033308,-1.8651344733792,
-1.8622507540964,-1.8393474606752,-1.83565233377208,-1.83356152749511,-1.83174099303775,
-1.82927081431317,-1.82347048632978,-1.81497508977261,-1.784921688362,-1.75999778692551,
-1.75409907118345,-1.75054219294227,-1.7473127287515,-1.74311037006333,
-1.73391528472747,-1.72114704352049,-1.6989866899069,-1.69486658782451,
-1.6727145166617,-1.66902258671762,-1.66693262314929,-1.66511194493657,
-1.6626405471572,-1.6568333348081,-1.64832419526621,-1.61816304597322,-1.59336181147711,
-1.58746641563755,-1.58391003210748,-1.58068005412256,-1.57647563126804,
-1.56726997763091,-1.55448165977799,-1.532331331972,-1.52812840508173,-1.50608969203846,
-1.50239788585388,-1.5003077536233,-1.49848644795217,-1.49601362949135,
-1.49020097915688,-1.48168129722469,-1.45143239026524,-1.42676137799863,
-1.42087009445924,-1.41731418862032,-1.41408334031537,-1.40987587801174,
-1.4082992289097),.UNSPECIFIED.);
#2872=B_SPLINE_CURVE_WITH_KNOTS('',3,(#120004,#120005,#120006,#120007,#120008,
#120009,#120010,#120011,#120012,#120013,#120014,#120015,#120016,#120017,
#120018,#120019),.UNSPECIFIED.,.F.,.F.,(4,2,2,2,2,2,2,4),(-0.059479256607861,
-0.0341344807334151,-0.0193900327960261,-0.0142709742838432,-0.0108788420291215,
-0.00783988787161742,-0.00425775755582772,-0.000493436327504615),
 .UNSPECIFIED.);
#2873=B_SPLINE_CURVE_WITH_KNOTS('',3,(#120020,#120021,#120022,#120023,#120024,
#120025,#120026,#120027,#120028,#120029,#120030,#120031,#120032,#120033,
#120034,#120035,#120036,#120037,#120038,#120039,#120040,#120041,#120042,
#120043,#120044,#120045,#120046,#120047,#120048,#120049,#120050,#120051,
#120052,#120053,#120054,#120055,#120056,#120057,#120058,#120059,#120060,
#120061,#120062,#120063,#120064,#120065,#120066,#120067,#120068,#120069,
#120070,#120071,#120072,#120073,#120074,#120075,#120076,#120077,#120078,
#120079,#120080,#120081,#120082,#120083,#120084,#120085,#120086,#120087,
#120088,#120089,#120090,#120091,#120092,#120093,#120094,#120095,#120096,
#120097,#120098,#120099,#120100,#120101,#120102,#120103,#120104,#120105,
#120106,#120107,#120108,#120109,#120110,#120111,#120112,#120113,#120114,
#120115,#120116,#120117,#120118,#120119,#120120,#120121,#120122,#120123,
#120124,#120125,#120126,#120127,#120128,#120129,#120130,#120131,#120132,
#120133,#120134,#120135,#120136,#120137,#120138,#120139,#120140,#120141,
#120142,#120143,#120144,#120145,#120146,#120147,#120148,#120149,#120150,
#120151,#120152,#120153,#120154,#120155,#120156,#120157,#120158,#120159,
#120160,#120161,#120162,#120163,#120164,#120165,#120166,#120167,#120168,
#120169,#120170,#120171,#120172,#120173,#120174,#120175,#120176,#120177,
#120178,#120179,#120180,#120181,#120182,#120183,#120184,#120185,#120186,
#120187,#120188,#120189,#120190,#120191,#120192,#120193,#120194,#120195,
#120196,#120197,#120198,#120199,#120200,#120201,#120202,#120203,#120204,
#120205,#120206,#120207),.UNSPECIFIED.,.F.,.F.,(4,2,2,2,2,2,2,2,2,2,2,2,
2,2,2,2,2,2,2,2,2,2,2,2,2,2,2,2,2,2,2,2,2,2,2,2,2,2,2,2,2,2,2,2,2,2,2,2,
2,2,2,2,2,2,2,2,2,2,2,2,2,2,2,2,2,2,2,2,2,2,2,2,2,2,2,2,2,2,2,2,2,2,2,2,
2,2,2,2,2,2,2,2,2,4),(-2.09996244461801,-2.08157373924918,-2.03783073252861,
-2.0309126457687,-2.02826864878956,-2.02642174480607,-2.02441331549537,
-2.02099866755253,-2.00763364657633,-1.98108316517676,-1.95595416763879,
-1.95085521205658,-1.94630520621802,-1.94302229887663,-1.94000685411733,
-1.93509836541476,-1.92216551037023,-1.8876305583691,-1.87308870326431,
-1.86737552789088,-1.86306201100004,-1.86086459686778,-1.85905813002354,
-1.85674286313071,-1.85182065890753,-1.82853418279768,-1.8271798322326,
-1.80018667625805,-1.78524312797341,-1.7802337337003,-1.77686330084659,
-1.77358338025717,-1.76886838053297,-1.75725745698622,-1.72146557792443,
-1.70657460017759,-1.69803818204913,-1.6951810089968,-1.69329320835359,
-1.69135321857799,-1.68825218632507,-1.67838899428806,-1.64931233365744,
-1.62041385138224,-1.61448801535696,-1.61092545065065,-1.60769756211002,
-1.60357663525929,-1.59459088120873,-1.55189552818646,-1.53892445554888,
-1.5311256175077,-1.52836047569698,-1.52649110442872,-1.52476712008828,
-1.52178776512585,-1.51296744161078,-1.47982063791151,-1.4623018971236,
-1.45448665277853,-1.44813857207455,-1.44448663536194,-1.44127517035593,
-1.4372382229071,-1.43081948515339,-1.39332078934756,-1.36727035981716,
-1.36296726884326,-1.36077189181912,-1.3589652331119,-1.35664733329347,
-1.35171124610737,-1.32692131061649,-1.30475451107767,-1.29221393423136,
-1.28313913358878,-1.27895770538371,-1.27573079167078,-1.27216313928785,
-1.26621399152472,-1.23890265707268,-1.21088995053926,-1.19868607597286,
-1.19546974578855,-1.19350452244951,-1.19165637504518,-1.18934964051302,
-1.18350035104981,-1.15110453375573,-1.12543798825827,-1.11642111640819,
-1.11224993677954,-1.10902431162195,-1.10900608777772),.UNSPECIFIED.);
#2874=B_SPLINE_CURVE_WITH_KNOTS('',3,(#120212,#120213,#120214,#120215,#120216,
#120217,#120218,#120219,#120220,#120221,#120222,#120223,#120224,#120225,
#120226,#120227,#120228,#120229,#120230,#120231,#120232,#120233,#120234,
#120235,#120236,#120237,#120238,#120239,#120240,#120241,#120242,#120243,
#120244,#120245,#120246,#120247,#120248,#120249,#120250,#120251,#120252,
#120253,#120254,#120255,#120256,#120257,#120258,#120259,#120260,#120261,
#120262,#120263,#120264,#120265,#120266,#120267,#120268,#120269,#120270,
#120271,#120272,#120273,#120274,#120275,#120276,#120277,#120278,#120279,
#120280,#120281,#120282,#120283,#120284,#120285,#120286,#120287,#120288,
#120289,#120290,#120291,#120292,#120293,#120294,#120295,#120296,#120297,
#120298,#120299,#120300,#120301,#120302,#120303,#120304,#120305,#120306,
#120307,#120308,#120309,#120310,#120311,#120312,#120313,#120314,#120315,
#120316,#120317,#120318,#120319,#120320,#120321,#120322,#120323,#120324,
#120325,#120326,#120327,#120328,#120329,#120330,#120331,#120332,#120333,
#120334,#120335,#120336,#120337,#120338,#120339,#120340,#120341,#120342,
#120343,#120344,#120345,#120346,#120347,#120348,#120349,#120350,#120351,
#120352,#120353,#120354,#120355,#120356,#120357,#120358,#120359,#120360,
#120361,#120362,#120363,#120364,#120365,#120366,#120367,#120368,#120369,
#120370,#120371,#120372,#120373,#120374,#120375,#120376,#120377,#120378,
#120379,#120380,#120381,#120382,#120383,#120384,#120385,#120386,#120387,
#120388,#120389,#120390,#120391,#120392,#120393,#120394,#120395,#120396,
#120397,#120398,#120399,#120400,#120401,#120402,#120403,#120404,#120405,
#120406,#120407,#120408,#120409,#120410,#120411,#120412,#120413,#120414,
#120415,#120416,#120417,#120418,#120419,#120420,#120421,#120422,#120423),
 .UNSPECIFIED.,.F.,.F.,(4,2,2,2,2,2,2,2,2,2,2,2,2,2,2,2,2,2,2,2,2,2,2,2,
2,2,2,2,2,2,2,2,2,2,2,2,2,2,2,2,2,2,2,2,2,2,2,2,2,2,2,2,2,2,2,2,2,2,2,2,
2,2,2,2,2,2,2,2,2,2,2,2,2,2,2,2,2,2,2,2,2,2,2,2,2,2,2,2,2,2,2,2,2,2,2,2,
2,2,2,2,2,2,2,2,2,4),(-3.50758932112955,-3.50326607780528,-3.50079423187189,
-3.49897322688236,-3.49688287624308,-3.49319031109068,-3.47121619820863,
-3.46693706942608,-3.44476974818732,-3.43196655138824,-3.4227536106868,
-3.4185476159197,-3.41531716311827,-3.41176099337353,-3.40586767232834,
-3.38112322683398,-3.35094010361961,-3.34242946150377,-3.3366208272391,
-3.3341489998827,-3.33232800752881,-3.33023767036684,-3.32654512618697,
-3.30457000327504,-3.30029167548298,-3.27812437271735,-3.26532155636205,
-3.25610883190379,-3.25190289283497,-3.24867246587322,-3.24511630768812,
-3.239222965705,-3.21447671298175,-3.18429551574369,-3.17578514806509,-3.16997666091744,
-3.16750486851562,-3.16568389102516,-3.16359355824415,-3.15990099480974,
-3.13791430816717,-3.1336438955831,-3.11147546561411,-3.09867564466832,
-3.08946450349017,-3.08525885760357,-3.08202848634971,-3.07847222038706,
-3.07257829774191,-3.04781217963822,-3.017648669765,-3.00914055926497,-3.00333320283615,
-3.00086160875178,-2.99904066581063,-2.99695024202945,-2.99325723855445,
-2.97114570015141,-2.96696672690247,-2.94478871182247,-2.93201385004535,
-2.9228157857984,-2.91861243426604,-2.91538237316369,-2.91182499855187,
-2.90592578776943,-2.88098154639055,-2.85097333805115,-2.84248487425747,
-2.83668728408946,-2.83421732872331,-2.8323966033404,-2.83030527815063,
-2.8266081963218,-2.80348296664562,-2.77484417510541,-2.75845207107761,
-2.75328979462628,-2.74988782298085,-2.74662925781049,-2.74203469914272,
-2.73115917144329,-2.69464288990083,-2.67955486592204,-2.6709462566399,
-2.66808024234911,-2.66619041807537,-2.66448679822252,-2.66161475329431,
-2.65362442408945,-2.62308648845793,-2.59432929986754,-2.58784992150024,
-2.58417012355828,-2.5809614076584,-2.57696371053926,-2.57068021708651,
-2.52546769247341,-2.51205237661471,-2.50407702746396,-2.50128884125485,
-2.49941471422187,-2.49769540121728,-2.49474118218841,-2.48612426776342,
-2.45787557075319),.UNSPECIFIED.);
#2875=B_SPLINE_CURVE_WITH_KNOTS('',3,(#120424,#120425,#120426,#120427,#120428,
#120429,#120430,#120431,#120432,#120433,#120434,#120435,#120436,#120437,
#120438,#120439,#120440,#120441,#120442,#120443,#120444,#120445,#120446,
#120447,#120448,#120449,#120450,#120451,#120452,#120453,#120454,#120455,
#120456,#120457,#120458,#120459,#120460,#120461,#120462,#120463,#120464,
#120465,#120466,#120467,#120468,#120469,#120470,#120471,#120472,#120473,
#120474,#120475,#120476,#120477,#120478,#120479,#120480,#120481,#120482,
#120483,#120484,#120485,#120486,#120487,#120488,#120489,#120490,#120491,
#120492,#120493,#120494,#120495,#120496,#120497,#120498,#120499,#120500,
#120501,#120502,#120503,#120504,#120505,#120506,#120507,#120508,#120509,
#120510,#120511,#120512,#120513,#120514,#120515,#120516,#120517,#120518,
#120519,#120520,#120521,#120522,#120523,#120524,#120525,#120526,#120527,
#120528,#120529,#120530,#120531,#120532,#120533,#120534,#120535,#120536,
#120537,#120538,#120539,#120540,#120541,#120542,#120543,#120544,#120545,
#120546,#120547,#120548,#120549,#120550,#120551,#120552,#120553,#120554,
#120555,#120556,#120557,#120558,#120559,#120560,#120561,#120562,#120563,
#120564,#120565,#120566,#120567,#120568,#120569,#120570,#120571,#120572,
#120573,#120574,#120575,#120576,#120577,#120578,#120579,#120580,#120581,
#120582,#120583,#120584,#120585,#120586,#120587,#120588,#120589,#120590,
#120591,#120592,#120593,#120594,#120595,#120596,#120597,#120598,#120599,
#120600,#120601,#120602,#120603,#120604,#120605,#120606,#120607,#120608,
#120609,#120610,#120611,#120612,#120613,#120614,#120615,#120616,#120617,
#120618,#120619,#120620,#120621,#120622,#120623),.UNSPECIFIED.,.F.,.F.,
(4,2,2,2,2,2,2,2,2,2,2,2,2,2,2,2,2,2,2,2,2,2,2,2,2,2,2,2,2,2,2,2,2,2,2,
2,2,2,2,2,2,2,2,2,2,2,2,2,2,2,2,2,2,2,2,2,2,2,2,2,2,2,2,2,2,2,2,2,2,2,2,
2,2,2,2,2,2,2,2,2,2,2,2,2,2,2,2,2,2,2,2,2,2,2,2,2,2,2,2,4),(-1.10900608777772,
-1.10545139341803,-1.09947729407191,-1.07142088108024,-1.04995735933683,
-1.03278567515519,-1.02914828651982,-1.02709159286259,-1.02526233148902,
-1.02272801005496,-1.01653354013363,-1.00722847017117,-0.969627029959607,
-0.952560546317377,-0.947183262997452,-0.943736907974779,-0.940467375339906,
-0.935995856459047,-0.925154559814216,-0.909044306241189,-0.891499869558333,
-0.868213455465457,-0.863292167320898,-0.860977130563375,-0.859170727773056,
-0.856973263964287,-0.852659293234556,-0.846944663378402,-0.83239676275621,
-0.797850516980509,-0.784905556412788,-0.779995426927117,-0.776979759363738,
-0.773697247989051,-0.769148938770557,-0.757795148543991,-0.740552733335049,
-0.707857661685441,-0.698356281477206,-0.695296102610414,-0.693365081899662,
-0.691470245806252,-0.688578626646476,-0.679748272137217,-0.664041823595915,
-0.625220852497486,-0.616447547972186,-0.61230472294534,-0.609074158238372,
-0.605523418072018,-0.599652329166598,-0.572369311100458,-0.546032573426438,
-0.532398526305794,-0.528967111313501,-0.526955124571645,-0.525110004392858,
-0.522475610176029,-0.515622730908919,-0.472028954160963,-0.452891447081516,
-0.447339572300788,-0.443856812389304,-0.440604427478022,-0.436236536103075,
-0.42605122199956,-0.411321761042372,-0.38175362970548,-0.365947927471022,
-0.362394686034681,-0.360356400595963,-0.35852174247136,-0.355949922001723,
-0.349513273134975,-0.339693122008154,-0.295231615598122,-0.284190392509096,
-0.279575593646994,-0.276314497194065,-0.272920078327508,-0.267789652890676,
-0.251699059252475,-0.22406652340404,-0.201534498859147,-0.196613723098055,
-0.194299124529777,-0.192493158599055,-0.190296342329874,-0.185983970152466,
-0.180271679975482,-0.16573119296879,-0.13120715471522,-0.118250598598311,
-0.113339620552802,-0.110324326612007,-0.107042918372219,-0.102497431494663,
-0.0911580184665465,-0.0666476919421411,-0.0592664597001961),
 .UNSPECIFIED.);
#2876=B_SPLINE_CURVE_WITH_KNOTS('',3,(#120628,#120629,#120630,#120631,#120632,
#120633,#120634,#120635,#120636,#120637,#120638,#120639,#120640,#120641,
#120642,#120643,#120644,#120645,#120646,#120647,#120648,#120649,#120650,
#120651,#120652,#120653,#120654,#120655,#120656,#120657,#120658,#120659,
#120660,#120661,#120662,#120663,#120664,#120665,#120666,#120667,#120668,
#120669,#120670,#120671,#120672,#120673,#120674,#120675,#120676,#120677,
#120678,#120679,#120680,#120681,#120682,#120683,#120684,#120685,#120686,
#120687,#120688,#120689,#120690,#120691,#120692,#120693,#120694,#120695,
#120696,#120697,#120698,#120699,#120700,#120701,#120702,#120703,#120704,
#120705,#120706,#120707,#120708,#120709,#120710,#120711,#120712,#120713,
#120714,#120715,#120716,#120717,#120718,#120719,#120720,#120721,#120722,
#120723,#120724,#120725,#120726,#120727,#120728,#120729,#120730,#120731,
#120732,#120733,#120734,#120735,#120736,#120737,#120738,#120739,#120740,
#120741,#120742,#120743,#120744,#120745,#120746,#120747,#120748,#120749,
#120750,#120751,#120752,#120753,#120754,#120755,#120756,#120757,#120758,
#120759,#120760,#120761,#120762,#120763,#120764,#120765,#120766,#120767,
#120768,#120769,#120770,#120771,#120772,#120773,#120774,#120775,#120776,
#120777,#120778,#120779,#120780,#120781,#120782,#120783,#120784,#120785,
#120786,#120787,#120788,#120789,#120790,#120791,#120792,#120793,#120794,
#120795,#120796,#120797,#120798,#120799,#120800,#120801,#120802,#120803,
#120804,#120805,#120806,#120807,#120808,#120809,#120810,#120811,#120812,
#120813,#120814,#120815,#120816,#120817,#120818,#120819,#120820,#120821,
#120822,#120823,#120824,#120825,#120826,#120827,#120828,#120829,#120830,
#120831,#120832,#120833,#120834,#120835,#120836,#120837,#120838,#120839),
 .UNSPECIFIED.,.F.,.F.,(4,2,2,2,2,2,2,2,2,2,2,2,2,2,2,2,2,2,2,2,2,2,2,2,
2,2,2,2,2,2,2,2,2,2,2,2,2,2,2,2,2,2,2,2,2,2,2,2,2,2,2,2,2,2,2,2,2,2,2,2,
2,2,2,2,2,2,2,2,2,2,2,2,2,2,2,2,2,2,2,2,2,2,2,2,2,2,2,2,2,2,2,2,2,2,2,2,
2,2,2,2,2,2,2,2,2,4),(-4.55725054622971,-4.53544163392311,-4.50897044576888,
-4.50316152446864,-4.50068957721346,-4.49886849734356,-4.49677806055521,
-4.49308534258128,-4.47111009193486,-4.46705396399047,-4.44469504134589,
-4.43187301532949,-4.4226501294377,-4.41844229892793,-4.4152115020168,-4.41165601637588,
-4.40576635435688,-4.38101369904171,-4.35082916311207,-4.34231815166661,
-4.33650926970097,-4.33403733996817,-4.3322162733169,-4.33012585206608,
-4.32643316231025,-4.30445841021736,-4.30017906553463,-4.2780110038721,
-4.26520734459116,-4.25599407676876,-4.25178793703333,-4.24855737462706,
-4.24500108597025,-4.23910757202739,-4.21436249943664,-4.18417816870753,
-4.1756672150268,-4.16985837247322,-4.16738645950494,-4.16556540520201,
-4.16347499812535,-4.15978233340483,-4.13780773121874,-4.13352841481556,
-4.11136050343049,-4.09855693060044,-4.08934372504939,-4.08513761379573,
-4.08190707328687,-4.07835080875626,-4.07245733484652,-4.04771243253357,
-4.01752830426367,-4.00901740800195,-4.00320860468576,-4.00073670844734,
-3.99891566647474,-3.99682527354528,-3.99313263383623,-3.97115818149917,
-3.9668788936373,-3.94471113281501,-3.93190764680303,-3.92269450371204,
-3.91848842094588,-3.91525790230331,-3.91170166182919,-3.90580822774859,
-3.88106349057684,-3.8508795691259,-3.84236873082204,-3.83655996700689,
-3.83408808753619,-3.83226705791252,-3.83017667917522,-3.82648406450324,
-3.80450975403519,-3.80023049993793,-3.77806288850072,-3.76525949086604,
-3.75604641108258,-3.7518403570185,-3.7486098603463,-3.74505364398424,-3.7391602496926,
-3.71441567341441,-3.68423196219169,-3.67572118231075,-3.66991245825377,
-3.66744059563131,-3.66561957839373,-3.66352921385181,-3.65983662421744,
-3.63786246229042,-3.63358323679476,-3.61141577488531,-3.59861246352816,
-3.58939944589447,-3.58519342029235,-3.58196294551784,-3.5784067533001,
-3.57251339911424,-3.54776899467422,-3.51758548525494,-3.50907476269372,
-3.50758932112955),.UNSPECIFIED.);
#2877=B_SPLINE_CURVE_WITH_KNOTS('',3,(#120841,#120842,#120843,#120844,#120845,
#120846,#120847,#120848,#120849,#120850,#120851,#120852,#120853,#120854,
#120855,#120856,#120857,#120858,#120859,#120860),.UNSPECIFIED.,.F.,.F.,
(4,2,2,2,2,2,2,2,2,4),(-0.0592664597001961,-0.044487464262689,-0.0322596332417712,
-0.0289284677612067,-0.0269386209323888,-0.0250836837176406,-0.0232035109203273,
-0.0205734943312831,-0.0140923816516964,-0.000491289129905891),
 .UNSPECIFIED.);
#2878=B_SPLINE_CURVE_WITH_KNOTS('',3,(#120861,#120862,#120863,#120864,#120865,
#120866,#120867,#120868,#120869,#120870,#120871,#120872,#120873,#120874,
#120875,#120876,#120877,#120878,#120879,#120880,#120881,#120882,#120883,
#120884,#120885,#120886,#120887,#120888,#120889,#120890,#120891,#120892,
#120893,#120894,#120895,#120896,#120897,#120898,#120899,#120900,#120901,
#120902,#120903,#120904,#120905,#120906,#120907,#120908,#120909,#120910,
#120911,#120912,#120913,#120914,#120915,#120916,#120917,#120918,#120919,
#120920,#120921,#120922,#120923,#120924,#120925,#120926,#120927,#120928,
#120929,#120930,#120931,#120932,#120933,#120934,#120935,#120936,#120937,
#120938,#120939,#120940,#120941,#120942,#120943,#120944,#120945,#120946,
#120947,#120948,#120949,#120950,#120951,#120952,#120953,#120954,#120955,
#120956,#120957,#120958,#120959,#120960,#120961,#120962,#120963,#120964,
#120965,#120966,#120967,#120968,#120969,#120970,#120971,#120972,#120973,
#120974,#120975,#120976,#120977,#120978,#120979,#120980,#120981,#120982,
#120983,#120984,#120985,#120986,#120987,#120988,#120989,#120990,#120991,
#120992,#120993,#120994,#120995,#120996,#120997,#120998,#120999,#121000,
#121001,#121002,#121003,#121004,#121005,#121006,#121007,#121008,#121009,
#121010,#121011,#121012,#121013,#121014,#121015,#121016,#121017,#121018,
#121019,#121020,#121021,#121022,#121023,#121024,#121025,#121026,#121027,
#121028,#121029,#121030,#121031,#121032,#121033,#121034,#121035,#121036,
#121037,#121038,#121039,#121040,#121041,#121042,#121043,#121044,#121045,
#121046,#121047,#121048,#121049,#121050,#121051,#121052,#121053,#121054,
#121055,#121056,#121057,#121058,#121059,#121060,#121061,#121062,#121063,
#121064,#121065,#121066,#121067,#121068,#121069,#121070,#121071,#121072,
#121073,#121074,#121075,#121076,#121077,#121078,#121079,#121080,#121081,
#121082,#121083,#121084,#121085,#121086,#121087,#121088,#121089,#121090,
#121091,#121092,#121093,#121094,#121095,#121096,#121097,#121098,#121099,
#121100,#121101,#121102,#121103,#121104,#121105,#121106,#121107,#121108,
#121109,#121110,#121111,#121112,#121113,#121114,#121115,#121116,#121117,
#121118,#121119,#121120),.UNSPECIFIED.,.F.,.F.,(4,2,2,2,2,2,2,2,2,2,2,2,
2,2,2,2,2,2,2,2,2,2,2,2,2,2,2,2,2,2,2,2,2,2,2,2,2,2,2,2,2,2,2,2,2,2,2,2,
2,2,2,2,2,2,2,2,2,2,2,2,2,2,2,2,2,2,2,2,2,2,2,2,2,2,2,2,2,2,2,2,2,2,2,2,
2,2,2,2,2,2,2,2,2,2,2,2,2,2,2,2,2,2,2,2,2,2,2,2,2,2,2,2,2,2,2,2,2,2,2,2,
2,2,2,2,2,2,2,2,2,4),(-2.10010132658151,-2.05909871254268,-2.04960757489194,
-2.04535445155139,-2.04211858461491,-2.03858675912585,-2.03280468762879,
-2.010412986564,-1.97814762227775,-1.96935040867242,-1.96349122128359,-1.9611155574656,
-1.96109881849124,-1.9610817523395,-1.96106434189489,-1.96104656894127,
-1.96102841406951,-1.96100985661037,-1.96099087460414,-1.96097144472476,
-1.96095154193326,-1.96093113946981,-1.96091020873649,-1.96088871894084,
-1.96086663698487,-1.96084392747736,-1.96082055216478,-1.9607964698133,
-1.96077163577537,-1.9607460017532,-1.96071951530737,-1.96069211955835,
-1.96066375252865,-1.9606343465167,-1.96060382759794,-1.9605721147809,-1.96053911910075,
-1.96050474266919,-1.9604688774505,-1.96043140393448,-1.96039218966669,
-1.96035108723155,-1.95854369721215,-1.95620878839875,-1.9513567866793,
-1.92698113559443,-1.90480363110378,-1.89202101462245,-1.88281927504242,
-1.87861593373155,-1.87538659166102,-1.87183074598661,-1.8659359000808,
-1.84111196286137,-1.81099404103307,-1.80249198472382,-1.79668790330436,
-1.79421724612741,-1.79239683609119,-1.79030691253007,-1.78661463583356,
-1.76454900029655,-1.76033155745025,-1.73815422228204,-1.72537166413491,
-1.71616997288781,-1.71196665842624,-1.70873733886666,-1.70518151986088,
-1.69928672264213,-1.67446318993796,-1.64434528239983,-1.63584326122125,
-1.63003920846295,-1.62756856671766,-1.6257481693208,-1.62365826174634,
-1.61996601647707,-1.59790196319905,-1.59368348138443,-1.57150640217843,
-1.55872367291172,-1.54952190991072,-1.54531860136918,-1.54208930163608,
-1.53853351971351,-1.53263882025434,-1.50781731482975,-1.47769800854007,
-1.46919584426651,-1.46339173168703,-1.46092109061689,-1.45910070399122,
-1.45701082074339,-1.45331864420221,-1.43126625813019,-1.42703922213361,
-1.40486312089635,-1.39207833149864,-1.38287550820517,-1.37867203335387,
-1.37544273139674,-1.37188707235244,-1.36599287471854,-1.34118670951267,
-1.31105440836896,-1.30255063895464,-1.2967457407654,-1.29427497937038,
-1.29245458822376,-1.29036479773676,-1.28667299590718,-1.26471371171253,
-1.26064020020926,-1.23800005326314,-1.22533741263083,-1.21619866728069,
-1.21200639864797,-1.20877853460267,-1.20521727619113,-1.1992966428348,
-1.17344158319503,-1.14421107271519,-1.13582329079243,-1.13007614583047,
-1.12761505512968,-1.12579587644223,-1.12370057306247,-1.11998406916987,
-1.10920393116059),.UNSPECIFIED.);
#2879=B_SPLINE_CURVE_WITH_KNOTS('',3,(#121126,#121127,#121128,#121129,#121130,
#121131,#121132,#121133,#121134,#121135,#121136,#121137,#121138,#121139,
#121140,#121141,#121142,#121143,#121144,#121145,#121146,#121147,#121148,
#121149,#121150,#121151,#121152,#121153,#121154,#121155,#121156,#121157,
#121158,#121159,#121160,#121161,#121162,#121163,#121164,#121165,#121166,
#121167,#121168,#121169,#121170,#121171,#121172,#121173,#121174,#121175,
#121176,#121177,#121178,#121179,#121180,#121181,#121182,#121183,#121184,
#121185,#121186,#121187,#121188,#121189,#121190,#121191,#121192,#121193,
#121194,#121195,#121196,#121197,#121198,#121199,#121200,#121201,#121202,
#121203,#121204,#121205,#121206,#121207,#121208,#121209,#121210,#121211,
#121212,#121213,#121214,#121215,#121216,#121217,#121218,#121219,#121220,
#121221,#121222,#121223,#121224,#121225,#121226,#121227,#121228,#121229,
#121230,#121231,#121232,#121233,#121234,#121235,#121236,#121237,#121238,
#121239,#121240,#121241,#121242,#121243,#121244,#121245,#121246,#121247,
#121248,#121249,#121250,#121251,#121252,#121253,#121254,#121255,#121256,
#121257,#121258,#121259,#121260,#121261,#121262,#121263,#121264,#121265,
#121266,#121267,#121268,#121269,#121270,#121271,#121272,#121273,#121274,
#121275,#121276,#121277,#121278,#121279,#121280,#121281,#121282,#121283,
#121284,#121285,#121286,#121287,#121288,#121289,#121290,#121291,#121292,
#121293,#121294,#121295,#121296,#121297,#121298,#121299,#121300,#121301,
#121302,#121303,#121304,#121305,#121306,#121307,#121308,#121309,#121310,
#121311,#121312,#121313,#121314,#121315,#121316,#121317,#121318,#121319,
#121320,#121321,#121322,#121323,#121324,#121325,#121326,#121327,#121328,
#121329,#121330,#121331,#121332,#121333,#121334,#121335,#121336,#121337,
#121338,#121339,#121340,#121341,#121342,#121343,#121344,#121345,#121346,
#121347,#121348,#121349,#121350,#121351,#121352,#121353,#121354,#121355),
 .UNSPECIFIED.,.F.,.F.,(4,2,2,2,2,2,2,2,2,2,2,2,2,2,2,2,2,2,2,2,2,2,2,2,
2,2,2,2,2,2,2,2,2,2,2,2,2,2,2,2,2,2,2,2,2,2,2,2,2,2,2,2,2,2,2,2,2,2,2,2,
2,2,2,2,2,2,2,2,2,2,2,2,2,2,2,2,2,2,2,2,2,2,2,2,2,2,2,2,2,2,2,2,2,2,2,2,
2,2,2,2,2,2,2,2,2,2,2,2,2,2,2,2,2,2,4),(-0.990948248867995,-0.979672455295316,
-0.9729824314885,-0.968866577885365,-0.965646733523735,-0.962042091760025,
-0.955920542585719,-0.948463977709807,-0.932206608285816,-0.914289696023135,
-0.889742600356832,-0.886024818384269,-0.883928817823629,-0.882109048395981,
-0.879647040461974,-0.873897285336823,-0.86550398302534,-0.836247344745194,
-0.810391097282374,-0.804468465538512,-0.800906067000483,-0.79767719191891,
-0.79348360323458,-0.784341535802918,-0.771675142627436,-0.749014066464878,
-0.745144139235457,-0.72305312630508,-0.719360850125708,-0.717270575387693,
-0.715449606649019,-0.712977713232605,-0.707168673574408,-0.698656179402299,
-0.668471262965041,-0.64369567950319,-0.63780073013176,-0.634244259464411,
-0.63101397699056,-0.626808837131111,-0.617600287210655,-0.604807014617657,
-0.582654254540736,-0.578431014816997,-0.556412062067877,-0.552720133122025,
-0.550629962485371,-0.548809018303582,-0.546337069682407,-0.540527510083862,
-0.532013901151589,-0.501819344713932,-0.477056053765409,-0.471161592954264,
-0.467605274252917,-0.46437503941024,-0.460169831734166,-0.450960579806937,
-0.438165864759744,-0.416014312308193,-0.411785558904403,-0.389774911020015,
-0.386083089138364,-0.383992968887352,-0.382172061286059,-0.379700152530363,
-0.373890643459777,-0.365377069540588,-0.335182007953019,-0.310420537464163,
-0.304526240420762,-0.300970004689545,-0.297739835183687,-0.293534698165558,
-0.284325539581565,-0.271530902397935,-0.249379896282433,-0.245150621965675,
-0.22314129192691,-0.219449550512143,-0.21735947469704,-0.215538605008919,
-0.213066746651598,-0.207257351302723,-0.198743939766618,-0.168549385239458,
-0.143733525969834,-0.137868207155276,-0.134318178656801,-0.131086476558862,
-0.130937166136611,-0.130810214512794,-0.130700707519312,-0.130605100312627,
-0.130520765388843,-0.130445710163882,-0.13037839377642,-0.130317604294817,
-0.130262374402493,-0.130211921922581,-0.130165606914334,-0.130122900457604,
-0.129964945395609,-0.129806999613464,-0.124889320967317,-0.10985157029812,
-0.0824337556331517,-0.0786938298884941,-0.0565031873151528,-0.0528107881770321,
-0.0507205723091913,-0.0488997467220234,-0.0464281706108214,-0.0406204185046636,
-0.000394732259851559),.UNSPECIFIED.);
#2880=B_SPLINE_CURVE_WITH_KNOTS('',3,(#121356,#121357,#121358,#121359,#121360,
#121361,#121362,#121363,#121364,#121365,#121366,#121367,#121368,#121369,
#121370,#121371,#121372,#121373),.UNSPECIFIED.,.F.,.F.,(4,2,2,2,2,2,2,2,
4),(-4.61631755219529,-4.59347746858498,-4.58901458892267,-4.58574002981368,
-4.58244318705041,-4.57944161384394,-4.57461528573861,-4.56226226150011,
-4.55725054622971),.UNSPECIFIED.);
#2881=B_SPLINE_CURVE_WITH_KNOTS('',3,(#121374,#121375,#121376,#121377,#121378,
#121379,#121380,#121381,#121382,#121383,#121384,#121385,#121386,#121387,
#121388,#121389,#121390,#121391,#121392,#121393,#121394,#121395,#121396,
#121397,#121398,#121399,#121400,#121401,#121402,#121403,#121404,#121405,
#121406,#121407,#121408,#121409,#121410,#121411,#121412,#121413,#121414,
#121415,#121416,#121417,#121418,#121419,#121420,#121421,#121422,#121423,
#121424,#121425,#121426,#121427,#121428,#121429,#121430,#121431,#121432,
#121433,#121434,#121435,#121436,#121437,#121438,#121439,#121440,#121441,
#121442,#121443,#121444,#121445,#121446,#121447,#121448,#121449,#121450,
#121451,#121452,#121453,#121454,#121455,#121456,#121457,#121458,#121459,
#121460,#121461,#121462,#121463,#121464,#121465,#121466,#121467,#121468,
#121469,#121470,#121471,#121472,#121473,#121474,#121475,#121476,#121477,
#121478,#121479,#121480,#121481,#121482,#121483,#121484,#121485,#121486,
#121487,#121488,#121489,#121490,#121491,#121492,#121493,#121494,#121495,
#121496,#121497,#121498,#121499,#121500,#121501,#121502,#121503,#121504,
#121505,#121506,#121507,#121508,#121509,#121510,#121511,#121512,#121513,
#121514,#121515,#121516,#121517,#121518,#121519,#121520,#121521,#121522,
#121523,#121524,#121525,#121526,#121527,#121528,#121529,#121530,#121531,
#121532,#121533,#121534,#121535,#121536,#121537,#121538,#121539,#121540,
#121541,#121542,#121543,#121544,#121545,#121546,#121547,#121548,#121549,
#121550,#121551,#121552,#121553,#121554,#121555,#121556,#121557,#121558,
#121559,#121560,#121561,#121562,#121563,#121564,#121565,#121566,#121567,
#121568,#121569),.UNSPECIFIED.,.F.,.F.,(4,2,2,2,2,2,2,2,2,2,2,2,2,2,2,2,
2,2,2,2,2,2,2,2,2,2,2,2,2,2,2,2,2,2,2,2,2,2,2,2,2,2,2,2,2,2,2,2,2,2,2,2,
2,2,2,2,2,2,2,2,2,2,2,2,2,2,2,2,2,2,2,2,2,2,2,2,2,2,2,2,2,2,2,2,2,2,2,2,
2,2,2,2,2,2,2,2,2,4),(-1.10920393116059,-1.09545238288575,-1.07754877998225,
-1.06124705181696,-1.05031879527491,-1.04628123799819,-1.04328380279532,
-1.03998536226846,-1.03534716801461,-1.02336647125924,-1.00466975027437,
-0.977026524576556,-0.965228646836615,-0.96194273950729,-0.959962527031071,
-0.958101839391524,-0.955380967614092,-0.94791347960185,-0.935750960576131,
-0.899670325468565,-0.88510704318887,-0.879997210234699,-0.876945435282821,
-0.873688410207201,-0.869291648473138,-0.858926882346821,-0.843826654134602,
-0.824321712371313,-0.801320453629943,-0.796466197493382,-0.794130963671087,
-0.792323693643512,-0.790143246806896,-0.785912750439751,-0.761201507267572,
-0.72188945679387,-0.715648255304336,-0.71166377864048,-0.708457116007543,
-0.704770313589069,-0.698253285582592,-0.690168566300328,-0.671661295578562,
-0.644486982967404,-0.632051739530787,-0.62870399332545,-0.626710434067188,
-0.624857169476173,-0.622175537833955,-0.614991004919582,-0.603497008081052,
-0.58260144584094,-0.553582276257446,-0.547597928525964,-0.544023406016454,
-0.540799160857263,-0.536633760867165,-0.527645742479134,-0.502845970348658,
-0.472117369601396,-0.464386583012527,-0.461550992195022,-0.459854593020427,
-0.457957850420898,-0.455056174332297,-0.446135751111089,-0.430172511085007,
-0.390339533374479,-0.382455664197478,-0.378442682477746,-0.375233945566496,
-0.371567454837926,-0.365147222348091,-0.332841176353624,-0.300920563530067,
-0.296292264495551,-0.294033125964616,-0.292228581255045,-0.289981224950562,
-0.285413647684281,-0.260909675478603,-0.222021586841373,-0.215735631499108,
-0.211738131613172,-0.208530683930541,-0.204853581918325,-0.198382343042951,
-0.170477631411324,-0.141387560819282,-0.131593262330374,-0.128500501728611,
-0.12656267104444,-0.12467417677269,-0.121811716440772,-0.113580981861986,
-0.0993097405969179,-0.0703226089993763,-0.0595389284169461),
 .UNSPECIFIED.);
#2882=B_SPLINE_CURVE_WITH_KNOTS('',3,(#121574,#121575,#121576,#121577,#121578,
#121579,#121580,#121581,#121582,#121583,#121584,#121585,#121586,#121587,
#121588,#121589,#121590,#121591,#121592,#121593,#121594,#121595,#121596,
#121597,#121598,#121599,#121600,#121601,#121602,#121603,#121604,#121605,
#121606,#121607,#121608,#121609,#121610,#121611,#121612,#121613,#121614,
#121615,#121616,#121617,#121618,#121619,#121620,#121621,#121622,#121623,
#121624,#121625,#121626,#121627,#121628,#121629,#121630,#121631,#121632,
#121633,#121634,#121635,#121636,#121637,#121638,#121639,#121640,#121641,
#121642,#121643,#121644,#121645,#121646,#121647,#121648,#121649,#121650,
#121651,#121652,#121653,#121654,#121655,#121656,#121657,#121658,#121659,
#121660,#121661,#121662,#121663,#121664,#121665,#121666,#121667,#121668,
#121669,#121670,#121671,#121672,#121673,#121674,#121675,#121676,#121677,
#121678,#121679,#121680,#121681,#121682,#121683,#121684,#121685,#121686,
#121687,#121688,#121689,#121690,#121691,#121692,#121693,#121694,#121695,
#121696,#121697,#121698,#121699,#121700,#121701,#121702,#121703,#121704,
#121705,#121706,#121707,#121708,#121709,#121710,#121711,#121712,#121713,
#121714,#121715,#121716,#121717,#121718,#121719,#121720,#121721,#121722,
#121723,#121724,#121725,#121726,#121727,#121728,#121729,#121730,#121731,
#121732,#121733,#121734,#121735,#121736,#121737,#121738,#121739,#121740,
#121741,#121742,#121743,#121744,#121745,#121746,#121747,#121748,#121749,
#121750,#121751,#121752,#121753,#121754,#121755,#121756,#121757,#121758,
#121759,#121760,#121761,#121762,#121763,#121764,#121765,#121766,#121767,
#121768,#121769,#121770,#121771,#121772,#121773,#121774,#121775,#121776,
#121777,#121778,#121779,#121780,#121781,#121782,#121783,#121784,#121785,
#121786,#121787,#121788,#121789,#121790,#121791,#121792,#121793),
 .UNSPECIFIED.,.F.,.F.,(4,2,2,2,2,2,2,2,2,2,2,2,2,2,2,2,2,2,2,2,2,2,2,2,
2,2,2,2,2,2,2,2,2,2,2,2,2,2,2,2,2,2,2,2,2,2,2,2,2,2,2,2,2,2,2,2,2,2,2,2,
2,2,2,2,2,2,2,2,2,2,2,2,2,2,2,2,2,2,2,2,2,2,2,2,2,2,2,2,2,2,2,2,2,2,2,2,
2,2,2,2,2,2,2,2,2,2,2,2,2,4),(-2.04079439360869,-2.01832232010227,-1.99049537877606,
-1.97533771893915,-1.9704067674467,-1.97024875981206,-1.97009079499496,
-1.97004916905279,-1.97000408540807,-1.96995504583547,-1.96990144953348,
-1.96984256472043,-1.9697774900404,-1.96970510125454,-1.96962397628702,
-1.96953228694736,-1.96942763891705,-1.96930682773932,-1.96916545357647,
-1.96899728677888,-1.96879316848958,-1.96778835158514,-1.9645712676515,
-1.96047979810822,-1.95387406447519,-1.91929814144932,-1.89069615561188,
-1.88638777793846,-1.8841911447973,-1.8823842508756,-1.88006698821341,-1.87513539421651,
-1.84993687316705,-1.823366335713,-1.80855054804381,-1.80355496652656,-1.80018689839258,
-1.79690402950124,-1.7921754059665,-1.78047978243619,-1.74131194830112,
-1.72875667254374,-1.72112613377165,-1.71838287379085,-1.71651749291244,
-1.71454368155929,-1.71128887113857,-1.69985734884655,-1.67193163462875,
-1.65311654936921,-1.64108655176165,-1.63644055183092,-1.6331399291254,
-1.62974443757469,-1.62461408894545,-1.60986279884279,-1.57696170163996,
-1.55793792431243,-1.55327655566788,-1.55101045008676,-1.54920505897758,
-1.54696243768545,-1.54242211451408,-1.50937094860917,-1.47822566960969,
-1.47168486444353,-1.46799220879308,-1.46478472601858,-1.46080473830769,
-1.45458159127082,-1.40908262477423,-1.39104586784176,-1.38649689377451,
-1.38425254071481,-1.38244711150284,-1.38018265392315,-1.37553006031856,
-1.34403633925316,-1.31144178087576,-1.30493780235371,-1.30125275389038,
-1.2980444103757,-1.2940536354481,-1.28779405904147,-1.24866916810283,-1.22383604239752,
-1.21960461170361,-1.21742344740542,-1.21561542766506,-1.21327892147486,
-1.20842096692003,-1.18263287407177,-1.16727981523855,-1.15133231258097,
-1.1405670616318,-1.13610653068114,-1.13283818872568,-1.12980115431093,
-1.12477607132239,-1.11096750683819,-1.07723772368443,-1.06292303788748,
-1.05460111952307,-1.05176952263733,-1.04988665111793,-1.047939098118,-1.04480471150353,
-1.03358279893802,-1.00988692766837,-0.990948248867995),.UNSPECIFIED.);
#2883=B_SPLINE_CURVE_WITH_KNOTS('',3,(#121795,#121796,#121797,#121798,#121799,
#121800,#121801,#121802,#121803,#121804,#121805,#121806,#121807,#121808,
#121809,#121810,#121811,#121812),.UNSPECIFIED.,.F.,.F.,(4,2,2,2,2,2,2,2,
4),(-0.0595389284169461,-0.0526460477562469,-0.0471652681643023,-0.0436977380443621,
-0.0404394032049224,-0.0372330969659463,-0.032957136393493,-0.0229767669222253,
-0.000491639810663164),.UNSPECIFIED.);
#2884=B_SPLINE_CURVE_WITH_KNOTS('',3,(#121813,#121814,#121815,#121816,#121817,
#121818,#121819,#121820,#121821,#121822,#121823,#121824,#121825,#121826,
#121827,#121828,#121829,#121830,#121831,#121832,#121833,#121834,#121835,
#121836,#121837,#121838,#121839,#121840,#121841,#121842,#121843,#121844,
#121845,#121846,#121847,#121848,#121849,#121850,#121851,#121852,#121853,
#121854,#121855,#121856,#121857,#121858,#121859,#121860,#121861,#121862,
#121863,#121864,#121865,#121866,#121867,#121868,#121869,#121870,#121871,
#121872,#121873,#121874,#121875,#121876,#121877,#121878,#121879,#121880,
#121881,#121882,#121883,#121884,#121885,#121886,#121887,#121888,#121889,
#121890,#121891,#121892,#121893,#121894,#121895,#121896,#121897,#121898,
#121899,#121900,#121901,#121902,#121903,#121904,#121905,#121906,#121907,
#121908,#121909,#121910,#121911,#121912,#121913,#121914,#121915,#121916,
#121917,#121918,#121919,#121920,#121921,#121922,#121923,#121924,#121925,
#121926,#121927,#121928,#121929,#121930,#121931,#121932,#121933,#121934,
#121935,#121936,#121937,#121938,#121939,#121940,#121941,#121942,#121943,
#121944,#121945,#121946,#121947,#121948,#121949,#121950,#121951,#121952,
#121953,#121954,#121955,#121956,#121957,#121958,#121959,#121960,#121961,
#121962,#121963,#121964,#121965,#121966,#121967,#121968,#121969,#121970,
#121971,#121972,#121973,#121974,#121975),.UNSPECIFIED.,.F.,.F.,(4,3,3,3,
3,3,3,3,3,3,3,3,3,3,3,3,3,3,3,3,3,3,3,3,3,3,3,3,3,3,3,3,3,3,3,3,3,3,3,3,
3,3,3,3,3,3,3,3,3,3,3,3,3,3,4),(-54.1118657207559,-53.9685006349923,-53.8675843506887,
-53.7577897347119,-53.6468205794158,-53.5373284361963,-53.4279032844608,
-53.3185044306213,-53.2063874460516,-53.0968489113668,-52.9834427018547,
-52.8700364923426,-52.7602418763654,-52.6492727210693,-52.5397805778494,
-52.4303554261136,-52.3209565722737,-52.2088395877044,-52.0993010530192,
-51.9858948435079,-51.8724886339965,-51.7626940180193,-51.6517248627232,
-51.5422327195032,-51.4328075677673,-51.3234087139274,-51.2112917293581,
-51.1017531946728,-50.9883469851616,-50.8749407756504,-50.7651461596733,
-50.6541770043772,-50.5446848611573,-50.4352597094216,-50.3258608555817,
-50.2137438710124,-50.1042053363272,-49.9907991268158,-49.8773929173043,
-49.7675983013271,-49.656629146031,-49.5471370028111,-49.4377118510753,
-49.3283129972354,-49.2161960126661,-49.1066574779808,-48.9932512684695,
-48.8798450589582,-48.7700749185132,-48.6604636794684,-48.5509703726848,
-48.4415394131861,-48.3321442530804,-48.2227090153558,-48.1819103737702),
 .UNSPECIFIED.);
#2885=B_SPLINE_CURVE_WITH_KNOTS('',3,(#121981,#121982,#121983,#121984,#121985,
#121986,#121987,#121988,#121989,#121990,#121991,#121992,#121993,#121994,
#121995,#121996,#121997,#121998,#121999,#122000,#122001,#122002,#122003,
#122004,#122005,#122006,#122007,#122008,#122009,#122010,#122011,#122012,
#122013,#122014,#122015,#122016,#122017,#122018,#122019,#122020,#122021,
#122022,#122023,#122024,#122025,#122026,#122027,#122028,#122029,#122030,
#122031,#122032,#122033,#122034,#122035,#122036,#122037,#122038,#122039,
#122040,#122041,#122042,#122043,#122044,#122045,#122046,#122047,#122048,
#122049,#122050,#122051,#122052,#122053,#122054,#122055,#122056,#122057,
#122058,#122059,#122060,#122061,#122062,#122063,#122064,#122065,#122066,
#122067,#122068,#122069,#122070,#122071,#122072,#122073,#122074,#122075,
#122076,#122077,#122078,#122079,#122080,#122081,#122082,#122083,#122084,
#122085,#122086,#122087,#122088,#122089,#122090,#122091,#122092,#122093,
#122094,#122095,#122096,#122097,#122098,#122099,#122100,#122101,#122102,
#122103,#122104,#122105,#122106,#122107,#122108,#122109,#122110,#122111,
#122112,#122113,#122114,#122115,#122116,#122117,#122118,#122119,#122120,
#122121,#122122,#122123,#122124,#122125,#122126,#122127,#122128,#122129,
#122130,#122131,#122132,#122133,#122134,#122135,#122136,#122137,#122138,
#122139,#122140,#122141,#122142,#122143,#122144,#122145,#122146,#122147,
#122148,#122149,#122150,#122151,#122152,#122153,#122154,#122155,#122156,
#122157,#122158,#122159,#122160,#122161,#122162,#122163,#122164,#122165,
#122166,#122167,#122168,#122169,#122170,#122171,#122172,#122173,#122174,
#122175,#122176,#122177,#122178,#122179,#122180,#122181,#122182,#122183,
#122184,#122185,#122186),.UNSPECIFIED.,.F.,.F.,(4,2,2,2,2,2,2,2,2,2,2,2,
2,2,2,2,2,2,2,2,2,2,2,2,2,2,2,2,2,2,2,2,2,2,2,2,2,2,2,2,2,2,2,2,2,2,2,2,
2,2,2,2,2,2,2,2,2,2,2,2,2,2,2,2,2,2,2,2,2,2,2,2,2,2,2,2,2,2,2,2,2,2,2,2,
2,2,2,2,2,2,2,2,2,2,2,2,2,2,2,2,2,2,4),(-0.99122901227168,-0.983227268753514,
-0.978906015803561,-0.957081038950441,-0.953390025194915,-0.951300092768376,
-0.949479155878613,-0.947006949049697,-0.941195600594014,-0.932678301015368,
-0.902453400744925,-0.877726444255291,-0.871833256301421,-0.868277269064003,
-0.865047058902015,-0.860841486355785,-0.851629742266183,-0.838830135286176,
-0.816681502993497,-0.812436920807133,-0.790449606973926,-0.786757969892135,
-0.784667924485216,-0.782847060789057,-0.780375183117481,-0.774565621412512,
-0.76605185669774,-0.735854285600317,-0.711097264555212,-0.705203241805246,
-0.701647125408222,-0.69841703507173,-0.694211959148986,-0.685002755409117,
-0.672207904435414,-0.650057728330045,-0.64582680367583,-0.62382054238759,
-0.620128908290396,-0.618038889988993,-0.61621806808448,-0.61374627148331,
-0.607937007578999,-0.59942377628223,-0.569229661290363,-0.544469920718849,
-0.538575920435688,-0.535019856989821,-0.531789839691983,-0.527584894676421,
-0.5183761303656,-0.505582018838782,-0.483432098484161,-0.479202765304772,
-0.457194844110276,-0.453503279123129,-0.451413302716797,-0.4495925192915,
-0.447120777577551,-0.441311654353651,-0.432798639784977,-0.402605463838678,
-0.377845888367626,-0.371952000358812,-0.368396008940593,-0.365166059781741,
-0.360961207371143,-0.351752662490332,-0.338958869860906,-0.316809390129865,
-0.312580309891305,-0.290572617179392,-0.286881128500756,-0.284791195598822,
-0.282970450291284,-0.280498760613538,-0.274689760959446,-0.266176928631103,
-0.235984417645231,-0.211217979187828,-0.205328067355939,-0.201772969145187,
-0.198542877425826,-0.19433646882046,-0.185118667016619,-0.172307071600673,
-0.149932055461014,-0.145974909398137,-0.123953539802761,-0.120262072634282,
-0.11817217031765,-0.116351464819597,-0.113879846807658,-0.108071093268383,
-0.0818781078266959,-0.0549654866670009,-0.0424558191754459,-0.0376072494629689,
-0.0346022527455657,-0.0313099301635705,-0.0280428445143505,-0.0235992042135266,
-0.000491388890533752),.UNSPECIFIED.);
#2886=B_SPLINE_CURVE_WITH_KNOTS('',3,(#122187,#122188,#122189,#122190,#122191,
#122192,#122193,#122194,#122195,#122196,#122197,#122198,#122199,#122200,
#122201,#122202,#122203,#122204),.UNSPECIFIED.,.F.,.F.,(4,2,2,2,2,2,2,2,
4),(-2.0995834550408,-2.06307905068172,-2.05736778314294,-2.05305526557987,
-2.05085783283395,-2.04905103120409,-2.04673484375579,-2.04180884207193,
-2.04079439360869),.UNSPECIFIED.);
#2887=B_SPLINE_CURVE_WITH_KNOTS('',3,(#122206,#122207,#122208,#122209,#122210,
#122211,#122212,#122213,#122214,#122215,#122216,#122217,#122218),
 .UNSPECIFIED.,.F.,.F.,(4,3,3,3,4),(-48.1819103737702,-48.0723494709303,
-47.9625850795796,-47.8822972006122,-47.8286804139494),.UNSPECIFIED.);
#2888=B_SPLINE_CURVE_WITH_KNOTS('',3,(#122219,#122220,#122221,#122222,#122223,
#122224,#122225,#122226,#122227),.UNSPECIFIED.,.F.,.F.,(4,1,1,1,1,1,4),
(-47.8286738456232,-46.8847493422661,-45.88720148392,-44.8896536255739,
-43.8921057672278,-42.8945579088817,-41.8982145781629),.UNSPECIFIED.);
#2889=B_SPLINE_CURVE_WITH_KNOTS('',3,(#122232,#122233,#122234,#122235,#122236,
#122237,#122238,#122239,#122240,#122241,#122242,#122243,#122244,#122245,
#122246,#122247,#122248,#122249,#122250,#122251,#122252,#122253,#122254,
#122255,#122256,#122257,#122258,#122259,#122260,#122261,#122262,#122263,
#122264,#122265,#122266,#122267,#122268,#122269,#122270,#122271,#122272,
#122273,#122274,#122275,#122276,#122277,#122278,#122279,#122280,#122281,
#122282,#122283,#122284,#122285,#122286,#122287,#122288,#122289,#122290,
#122291,#122292,#122293,#122294,#122295,#122296,#122297,#122298,#122299,
#122300,#122301,#122302,#122303,#122304,#122305,#122306,#122307,#122308,
#122309,#122310,#122311,#122312,#122313,#122314,#122315,#122316,#122317,
#122318,#122319,#122320,#122321,#122322,#122323,#122324,#122325,#122326,
#122327,#122328,#122329,#122330,#122331,#122332,#122333,#122334,#122335,
#122336,#122337,#122338,#122339,#122340,#122341,#122342,#122343,#122344,
#122345,#122346,#122347,#122348,#122349,#122350,#122351,#122352,#122353,
#122354,#122355,#122356,#122357,#122358,#122359,#122360,#122361,#122362,
#122363,#122364,#122365,#122366,#122367,#122368,#122369,#122370,#122371,
#122372,#122373,#122374,#122375,#122376,#122377,#122378,#122379,#122380,
#122381,#122382,#122383,#122384,#122385,#122386,#122387,#122388,#122389,
#122390,#122391,#122392,#122393,#122394,#122395,#122396,#122397,#122398,
#122399,#122400,#122401,#122402,#122403,#122404,#122405,#122406,#122407,
#122408,#122409,#122410,#122411,#122412,#122413,#122414,#122415,#122416,
#122417,#122418,#122419,#122420,#122421,#122422,#122423,#122424,#122425,
#122426,#122427,#122428,#122429,#122430,#122431,#122432,#122433,#122434,
#122435,#122436,#122437),.UNSPECIFIED.,.F.,.F.,(4,2,2,2,2,2,2,2,2,2,2,2,
2,2,2,2,2,2,2,2,2,2,2,2,2,2,2,2,2,2,2,2,2,2,2,2,2,2,2,2,2,2,2,2,2,2,2,2,
2,2,2,2,2,2,2,2,2,2,2,2,2,2,2,2,2,2,2,2,2,2,2,2,2,2,2,2,2,2,2,2,2,2,2,2,
2,2,2,2,2,2,2,2,2,2,2,2,2,2,2,2,2,2,4),(-2.04104836935547,-2.03714760643148,
-2.03384845018572,-2.03084882225062,-2.02603457887804,-2.0137649795725,
-1.97860410490939,-1.96388825609362,-1.95813225930661,-1.95503846348167,
-1.95251440409047,-1.95066795756041,-1.94895862152159,-1.94605733496182,
-1.93785136604741,-1.89539815447764,-1.88293084620018,-1.87389455395044,
-1.86971942006444,-1.86649271851588,-1.86292058366996,-1.85695249516301,
-1.82903629522694,-1.80749470991633,-1.79570851325417,-1.78839802852381,
-1.78569813276929,-1.7838408838656,-1.78185241498258,-1.77853061208035,
-1.76643333284362,-1.73899316752314,-1.72037545542265,-1.70842810153789,
-1.70379362613964,-1.70049506138052,-1.69709643016222,-1.69195099152614,
-1.67705435586687,-1.64133739110251,-1.62922903399014,-1.62178308966165,
-1.61906463265654,-1.61720393742357,-1.61546830423004,-1.61243035898823,
-1.60312554052276,-1.57027875748764,-1.55295790183522,-1.54156993263592,
-1.53701589354917,-1.53373176397268,-1.53071633122226,-1.52581039405415,
-1.51289974496388,-1.4783503978887,-1.46380581493756,-1.45809179571037,
-1.45377765578006,-1.45157984942926,-1.44977299960447,-1.44745708076006,
-1.44253279004588,-1.41914693007446,-1.39911833192168,-1.37720930719193,
-1.37160322612921,-1.36810807540033,-1.36485863475455,-1.36059198584682,
-1.35114565726767,-1.3091922065552,-1.2963061283585,-1.28854123950048,-1.28578017549339,
-1.28391130187087,-1.281943021965,-1.27871378539896,-1.26757083438192,-1.2394369833839,
-1.22053599577561,-1.20847000221757,-1.20381884834996,-1.20051717140189,
-1.19712282272305,-1.19199856697369,-1.17730739190922,-1.13718236939856,
-1.1276687747763,-1.1213745987438,-1.11882422211446,-1.11699219495391,-1.11494241242747,
-1.11133850813704,-1.09484825336649,-1.05022558243909,-1.04074392341031,
-1.03653753361252,-1.03329735349281,-1.02977596759147,-1.02404573221537,
-0.999969186069353,-0.99122901227168),.UNSPECIFIED.);
#2890=B_SPLINE_CURVE_WITH_KNOTS('',3,(#122439,#122440,#122441,#122442,#122443),
 .UNSPECIFIED.,.F.,.F.,(4,1,4),(-41.8982145781629,-41.8970100505356,-41.5455022211392),
 .UNSPECIFIED.);
#2891=B_SPLINE_CURVE_WITH_KNOTS('',3,(#122444,#122445,#122446,#122447,#122448,
#122449,#122450,#122451,#122452,#122453,#122454,#122455,#122456,#122457,
#122458,#122459,#122460,#122461,#122462,#122463,#122464,#122465,#122466,
#122467,#122468,#122469,#122470,#122471,#122472,#122473,#122474,#122475,
#122476,#122477,#122478,#122479,#122480,#122481,#122482,#122483,#122484,
#122485,#122486,#122487,#122488,#122489,#122490,#122491,#122492,#122493,
#122494,#122495,#122496,#122497,#122498,#122499,#122500,#122501,#122502,
#122503,#122504,#122505,#122506,#122507,#122508,#122509,#122510,#122511,
#122512,#122513,#122514,#122515,#122516,#122517,#122518,#122519,#122520,
#122521,#122522,#122523,#122524,#122525,#122526,#122527,#122528,#122529,
#122530,#122531,#122532,#122533,#122534,#122535,#122536,#122537,#122538,
#122539,#122540,#122541,#122542,#122543,#122544,#122545,#122546,#122547,
#122548,#122549,#122550,#122551,#122552,#122553,#122554,#122555,#122556,
#122557,#122558,#122559,#122560,#122561,#122562,#122563,#122564,#122565,
#122566,#122567,#122568,#122569,#122570,#122571,#122572,#122573,#122574,
#122575,#122576,#122577,#122578,#122579,#122580,#122581,#122582,#122583,
#122584,#122585,#122586,#122587,#122588,#122589,#122590,#122591,#122592,
#122593,#122594,#122595,#122596,#122597,#122598,#122599,#122600,#122601,
#122602,#122603,#122604,#122605,#122606,#122607,#122608,#122609,#122610,
#122611,#122612,#122613,#122614,#122615,#122616,#122617,#122618,#122619,
#122620,#122621,#122622,#122623,#122624,#122625,#122626,#122627,#122628,
#122629,#122630,#122631,#122632,#122633,#122634,#122635,#122636,#122637,
#122638,#122639,#122640,#122641,#122642,#122643),.UNSPECIFIED.,.F.,.F.,
(4,2,2,2,2,2,2,2,2,2,2,2,2,2,2,2,2,2,2,2,2,2,2,2,2,2,2,2,2,2,2,2,2,2,2,
2,2,2,2,2,2,2,2,2,2,2,2,2,2,2,2,2,2,2,2,2,2,2,2,2,2,2,2,2,2,2,2,2,2,2,2,
2,2,2,2,2,2,2,2,2,2,2,2,2,2,2,2,2,2,2,2,2,2,2,2,2,2,2,2,4),(-2.1000414668587,
-2.08485542041858,-2.08077718866876,-2.07763733435763,-2.07453432238086,
-2.07100464627802,-2.06523302522097,-2.04127262215763,-2.01005811635457,
-2.00155299813749,-1.99574737751126,-1.99327644547223,-1.99145598237474,
-1.98936617189274,-1.98567446947417,-1.96376871100479,-1.95944263777065,
-1.93728236085358,-1.92446023275039,-1.91523781786169,-1.91103086424852,
-1.90780104534508,-1.90424696669279,-1.89836049584397,-1.87352015997578,
-1.8434022656422,-1.83490018635286,-1.82909608462182,-1.82662541561,-1.82480499559872,
-1.82271505912222,-1.81902275646713,-1.79695558933515,-1.79273917895481,
-1.77056162210722,-1.75777924941491,-1.74857764109656,-1.74437432646234,
-1.7411449917458,-1.73758914105032,-1.73169425561274,-1.70686876120012,
-1.6767522709345,-1.66825040207843,-1.66244641603708,-1.6599757769634,-1.65815537142206,
-1.65606544272256,-1.65237313478429,-1.63029759444262,-1.62608763847407,
-1.60390966358946,-1.59112892038175,-1.58192818266925,-1.57772503815865,
-1.57449574428734,-1.57093984885771,-1.56504467583315,-1.54020843369436,
-1.51010166697522,-1.50160105823871,-1.49579770902668,-1.49332718678545,
-1.49150680669156,-1.48941683660854,-1.4857243035667,-1.46358018107037,
-1.4332958309038,-1.41743831176737,-1.4123311420795,-1.40894112918672,-1.40567623321714,
-1.401765487456,-1.39214405565269,-1.35426952809928,-1.33881532900511,-1.33007465122383,
-1.32719356222227,-1.32530095638157,-1.32336741030808,-1.32029536025266,
-1.31068974797531,-1.27802004463933,-1.26081869484812,-1.24948423174351,
-1.24493887957704,-1.24165702995712,-1.23864097985865,-1.2337279134282,
-1.22075989088108,-1.18626278481832,-1.1717320809302,-1.16332965516964,
-1.16048886672462,-1.15860460005043,-1.15666060313107,-1.15354042374703,
-1.14349921037197,-1.11108109221267,-1.10913474556486),.UNSPECIFIED.);
#2892=B_SPLINE_CURVE_WITH_KNOTS('',3,(#122649,#122650,#122651,#122652,#122653,
#122654,#122655,#122656,#122657,#122658,#122659,#122660,#122661,#122662,
#122663,#122664,#122665,#122666,#122667,#122668,#122669,#122670,#122671,
#122672,#122673,#122674,#122675,#122676,#122677,#122678,#122679,#122680,
#122681,#122682,#122683,#122684,#122685,#122686,#122687,#122688,#122689,
#122690,#122691,#122692,#122693,#122694,#122695,#122696,#122697,#122698,
#122699,#122700,#122701,#122702,#122703,#122704,#122705,#122706,#122707,
#122708,#122709,#122710,#122711,#122712,#122713,#122714,#122715,#122716,
#122717,#122718,#122719,#122720,#122721,#122722,#122723,#122724,#122725,
#122726,#122727,#122728,#122729,#122730,#122731,#122732,#122733,#122734,
#122735,#122736,#122737,#122738,#122739,#122740,#122741,#122742,#122743,
#122744,#122745,#122746,#122747,#122748,#122749,#122750,#122751,#122752,
#122753,#122754,#122755,#122756,#122757,#122758,#122759,#122760,#122761,
#122762,#122763,#122764,#122765,#122766,#122767,#122768,#122769,#122770,
#122771,#122772,#122773,#122774,#122775,#122776,#122777,#122778,#122779,
#122780,#122781,#122782,#122783,#122784,#122785,#122786,#122787,#122788,
#122789,#122790,#122791,#122792,#122793,#122794,#122795,#122796,#122797,
#122798,#122799,#122800,#122801,#122802,#122803,#122804,#122805,#122806,
#122807,#122808,#122809,#122810,#122811,#122812,#122813,#122814,#122815,
#122816,#122817,#122818,#122819,#122820,#122821,#122822,#122823,#122824,
#122825,#122826,#122827,#122828,#122829,#122830,#122831,#122832,#122833,
#122834,#122835,#122836,#122837,#122838,#122839,#122840,#122841,#122842,
#122843,#122844,#122845,#122846,#122847,#122848,#122849,#122850),
 .UNSPECIFIED.,.F.,.F.,(4,2,2,2,2,2,2,2,2,2,2,2,2,2,2,2,2,2,2,2,2,2,2,2,
2,2,2,2,2,2,2,2,2,2,2,2,2,2,2,2,2,2,2,2,2,2,2,2,2,2,2,2,2,2,2,2,2,2,2,2,
2,2,2,2,2,2,2,2,2,2,2,2,2,2,2,2,2,2,2,2,2,2,2,2,2,2,2,2,2,2,2,2,2,2,2,2,
2,2,2,2,4),(-0.991067510703159,-0.969566476182921,-0.944672859721234,-0.938774223388853,
-0.935216919650418,-0.931986760811124,-0.927783045495996,-0.91858299783399,
-0.905806075864837,-0.883646082544692,-0.879488147545464,-0.857381082759265,
-0.853688743904557,-0.851598454201426,-0.84977748709762,-0.847305615543153,
-0.841496713817424,-0.832984500027537,-0.802801838660546,-0.778023625108033,
-0.772128590518732,-0.768572100025024,-0.765341819538381,-0.761136710980887,
-0.751928352019178,-0.73913544802847,-0.716982507979576,-0.712760530712895,
-0.690739798845815,-0.687047860436213,-0.68495768673693,-0.683136741528078,
-0.680664793709547,-0.67485524568444,-0.666341662471877,-0.636147338465189,
-0.611383736675271,-0.605489262364102,-0.601932939070134,-0.59870270230495,
-0.594497495356017,-0.585288258792793,-0.572493576715306,-0.550341989050687,
-0.546113369480386,-0.52410251242266,-0.520410687042745,-0.518320565062926,
-0.516499656135749,-0.514027745820546,-0.508218234146404,-0.499704657372448,
-0.469509601148857,-0.444748080051911,-0.438853777598179,-0.435297538992551,
-0.432067367121868,-0.427862227380027,-0.418653064344215,-0.405858422252137,
-0.383707397496495,-0.379478134999086,-0.357468767370291,-0.353777023110643,
-0.351686945712757,-0.349866074664626,-0.347394214486147,-0.341584814974732,
-0.333071397443817,-0.302876823348433,-0.278115991124243,-0.272221817247314,
-0.26866565413597,-0.265435549521099,-0.26123049544298,-0.252021511942407,
-0.239227112477597,-0.217076561846425,-0.192746244043969,-0.187894867516914,
-0.185559841425146,-0.183752121778224,-0.181570315748068,-0.177334846557921,
-0.151815685007491,-0.113524293960377,-0.107177248464375,-0.103161166903685,
-0.0999513126258957,-0.0962849916768693,-0.0898688149715362,-0.0673539059889128,
-0.043476137094742,-0.026732385323984,-0.0214000910904637,-0.0190357117834795,
-0.0172225165109289,-0.0155112267029777,-0.0133869765241974,-0.00853516041908881,
-0.000491170393658215),.UNSPECIFIED.);
#2893=B_SPLINE_CURVE_WITH_KNOTS('',3,(#122851,#122852,#122853,#122854,#122855,
#122856,#122857,#122858,#122859,#122860),.UNSPECIFIED.,.F.,.F.,(4,2,2,2,
4),(-2.10008953608574,-2.07237373101306,-2.05373873006262,-2.04178356612171,
-2.04104836935547),.UNSPECIFIED.);
#2894=B_SPLINE_CURVE_WITH_KNOTS('',3,(#122861,#122862,#122863,#122864,#122865,
#122866,#122867,#122868,#122869,#122870,#122871,#122872,#122873,#122874,
#122875,#122876,#122877,#122878,#122879,#122880,#122881,#122882,#122883,
#122884,#122885,#122886,#122887,#122888,#122889,#122890,#122891,#122892,
#122893,#122894,#122895,#122896,#122897,#122898,#122899,#122900,#122901,
#122902,#122903,#122904,#122905,#122906,#122907,#122908,#122909,#122910,
#122911,#122912,#122913,#122914,#122915,#122916,#122917,#122918,#122919,
#122920,#122921,#122922,#122923,#122924,#122925,#122926,#122927,#122928,
#122929,#122930,#122931,#122932,#122933,#122934,#122935,#122936,#122937,
#122938,#122939,#122940,#122941,#122942,#122943,#122944,#122945,#122946,
#122947,#122948,#122949,#122950,#122951,#122952,#122953,#122954,#122955,
#122956,#122957,#122958,#122959,#122960,#122961,#122962,#122963,#122964,
#122965,#122966,#122967,#122968,#122969,#122970,#122971,#122972,#122973,
#122974,#122975,#122976,#122977,#122978,#122979,#122980,#122981,#122982,
#122983,#122984,#122985,#122986,#122987,#122988,#122989,#122990,#122991,
#122992,#122993,#122994,#122995,#122996,#122997,#122998,#122999,#123000,
#123001,#123002,#123003,#123004,#123005,#123006,#123007,#123008,#123009,
#123010,#123011,#123012,#123013,#123014,#123015,#123016,#123017,#123018,
#123019,#123020,#123021,#123022,#123023,#123024,#123025,#123026,#123027,
#123028,#123029,#123030,#123031,#123032,#123033,#123034,#123035,#123036,
#123037,#123038,#123039,#123040,#123041,#123042,#123043,#123044,#123045,
#123046,#123047,#123048,#123049,#123050,#123051,#123052,#123053,#123054,
#123055,#123056,#123057,#123058,#123059,#123060,#123061,#123062,#123063,
#123064,#123065,#123066,#123067,#123068,#123069,#123070,#123071,#123072,
#123073,#123074,#123075,#123076),.UNSPECIFIED.,.F.,.F.,(4,2,2,2,2,2,2,2,
2,2,2,2,2,2,2,2,2,2,2,2,2,2,2,2,2,2,2,2,2,2,2,2,2,2,2,2,2,2,2,2,2,2,2,2,
2,2,2,2,2,2,2,2,2,2,2,2,2,2,2,2,2,2,2,2,2,2,2,2,2,2,2,2,2,2,2,2,2,2,2,2,
2,2,2,2,2,2,2,2,2,2,2,2,2,2,2,2,2,2,2,2,2,2,2,2,2,2,2,4),(-1.10913474556486,
-1.09405576568703,-1.08279979728913,-1.07826612179371,-1.0749863647678,
-1.07156059995665,-1.06628010922902,-1.05011160521927,-1.0213889613544,
-0.998409794735737,-0.994714782785097,-0.992624315431684,-0.990804181940742,
-0.988334847264225,-0.982538220210314,-0.974049977518646,-0.944052028088183,
-0.919059795644637,-0.913159580686374,-0.909602758030787,-0.906373970953528,
-0.902173417017199,-0.892986384919195,-0.880233136193736,-0.858065269904299,
-0.854030670440583,-0.831767925363533,-0.828075881831663,-0.825986104259027,
-0.824165864269339,-0.821695438602947,-0.815892086195546,-0.807390234433797,
-0.77728404937972,-0.752417671497103,-0.746521242636705,-0.742965271570152,
-0.739736352535635,-0.735534328395455,-0.726338555578801,-0.713568519466804,
-0.691406753585429,-0.687271593018449,-0.665133876505458,-0.66144236726291,
-0.659352735245371,-0.657532509906766,-0.655061954021645,-0.649257634751549,
-0.640753769360755,-0.610630870260464,-0.585784925552515,-0.579889216621454,
-0.576333445978787,-0.573104561047988,-0.568902369041317,-0.559705325191687,
-0.546932762510047,-0.524772473165564,-0.520623460756081,-0.498503968793178,
-0.494812601649143,-0.492723027482836,-0.490902836391282,-0.488432305375315,
-0.482627949343261,-0.474123944083238,-0.443999168495455,-0.419156605698403,
-0.41326110492502,-0.409705426009209,-0.406476602977054,-0.402274460818685,
-0.393077395310913,-0.380304692356088,-0.358145009801013,-0.353994120845126,
-0.331877599673955,-0.328186318020879,-0.326096789046958,-0.324276635032258,
-0.321806151275039,-0.316001892778133,-0.307498018223077,-0.277373509828933,
-0.252531866268621,-0.246636499375252,-0.243080896407582,-0.239852139307401,
-0.235650078599824,-0.226453172809721,-0.213680676034172,-0.191521471838072,
-0.167222933306922,-0.162272064254352,-0.1599518285471,-0.158145538368494,
-0.155953298366559,-0.151663869331122,-0.14599140447005,-0.131613852291793,
-0.0976704140317422,-0.0840808351867522,-0.0790847254395175,-0.0760540547136202,
-0.0727841383799814,-0.0683061924789343,-0.0595903478899269),
 .UNSPECIFIED.);
#2895=B_SPLINE_CURVE_WITH_KNOTS('',3,(#123081,#123082,#123083,#123084,#123085,
#123086,#123087,#123088,#123089,#123090,#123091,#123092,#123093,#123094,
#123095,#123096,#123097,#123098,#123099,#123100,#123101,#123102,#123103,
#123104,#123105,#123106,#123107,#123108,#123109,#123110,#123111,#123112,
#123113,#123114,#123115,#123116,#123117,#123118,#123119,#123120,#123121,
#123122,#123123,#123124,#123125,#123126,#123127,#123128,#123129,#123130,
#123131,#123132,#123133,#123134,#123135,#123136,#123137,#123138,#123139,
#123140,#123141,#123142,#123143,#123144,#123145,#123146,#123147,#123148,
#123149,#123150,#123151,#123152,#123153,#123154,#123155,#123156,#123157,
#123158,#123159,#123160,#123161,#123162,#123163,#123164,#123165,#123166,
#123167,#123168,#123169,#123170,#123171,#123172,#123173,#123174,#123175,
#123176,#123177,#123178,#123179,#123180,#123181,#123182,#123183,#123184,
#123185,#123186,#123187,#123188,#123189,#123190,#123191,#123192,#123193,
#123194,#123195,#123196,#123197,#123198,#123199,#123200,#123201,#123202,
#123203,#123204,#123205,#123206,#123207,#123208,#123209,#123210,#123211,
#123212,#123213,#123214,#123215,#123216,#123217,#123218,#123219,#123220,
#123221,#123222,#123223,#123224,#123225,#123226,#123227,#123228,#123229,
#123230,#123231,#123232,#123233,#123234,#123235,#123236,#123237,#123238,
#123239,#123240,#123241,#123242,#123243,#123244,#123245,#123246,#123247,
#123248,#123249,#123250,#123251,#123252,#123253,#123254,#123255,#123256,
#123257,#123258,#123259,#123260,#123261,#123262,#123263,#123264,#123265,
#123266,#123267,#123268,#123269,#123270,#123271,#123272,#123273,#123274,
#123275,#123276,#123277,#123278,#123279,#123280,#123281,#123282,#123283,
#123284,#123285,#123286),.UNSPECIFIED.,.F.,.F.,(4,2,2,2,2,2,2,2,2,2,2,2,
2,2,2,2,2,2,2,2,2,2,2,2,2,2,2,2,2,2,2,2,2,2,2,2,2,2,2,2,2,2,2,2,2,2,2,2,
2,2,2,2,2,2,2,2,2,2,2,2,2,2,2,2,2,2,2,2,2,2,2,2,2,2,2,2,2,2,2,2,2,2,2,2,
2,2,2,2,2,2,2,2,2,2,2,2,2,2,2,2,2,2,4),(-2.04084412535128,-2.03783344299161,
-2.02809527437528,-2.02169589036857,-2.01912933929048,-2.01729501143891,
-2.01525320173045,-2.01168551557941,-1.99558471766472,-1.9662330821357,
-1.9515417756892,-1.94137540720377,-1.93700972669471,-1.93375687175612,
-1.93027160010572,-1.92471122137928,-1.9057732633403,-1.86208714680868,
-1.85519439216568,-1.85255380240412,-1.85070723674901,-1.84869684021687,
-1.8452742039963,-1.83179062892292,-1.80532919468405,-1.78709524173683,
-1.77908339465956,-1.77261186671085,-1.76893363887402,-1.76572464513885,
-1.76172444617817,-1.75543265269942,-1.71661397467131,-1.69153946808137,
-1.68730677657481,-1.6851253779524,-1.68331740777108,-1.68098127868356,
-1.67612512020677,-1.65311220368238,-1.63359347797964,-1.61848303859685,
-1.60811353163126,-1.60371499750885,-1.6004567341046,-1.59740385141958,
-1.59229217527738,-1.57772052372698,-1.5416740848356,-1.52952015345061,
-1.52205515309274,-1.51933406933972,-1.51747285027636,-1.51573781778083,
-1.51270307408575,-1.50342592679449,-1.47390592434904,-1.4544444405685,
-1.44214780051682,-1.43746488447436,-1.43415740784466,-1.43116683353677,
-1.42640341801443,-1.41446931791054,-1.37899245107612,-1.35905741507545,
-1.35429604918236,-1.35201075564647,-1.35020495714318,-1.34798019687965,
-1.34353099980867,-1.30962977344053,-1.28297203494131,-1.27409521596028,
-1.26994854026439,-1.26672536961805,-1.26313832552059,-1.25709934955502,
-1.22770826950123,-1.20603167292204,-1.19020868362467,-1.18675381386956,
-1.18473637427786,-1.18289277029456,-1.18026956689495,-1.17397521987442,
-1.14198312886049,-1.11242985742344,-1.10594537086438,-1.10226443570444,
-1.09905573203107,-1.09505936225061,-1.08878060967185,-1.04983754644215,
-1.04683104770034,-1.02403000017116,-1.02033494150564,-1.01824401713651,
-1.01642314385123,-1.01395226516392,-1.00814950690654,-0.999649737438738,
-0.991067510703159),.UNSPECIFIED.);
#2896=B_SPLINE_CURVE_WITH_KNOTS('',3,(#123288,#123289,#123290,#123291,#123292,
#123293,#123294,#123295,#123296,#123297),.UNSPECIFIED.,.F.,.F.,(4,2,2,2,
4),(-0.0595903478899269,-0.0574178101975677,-0.0412035277078622,-0.0229711166027303,
-0.000637630673692526),.UNSPECIFIED.);
#2897=B_SPLINE_CURVE_WITH_KNOTS('',3,(#123298,#123299,#123300,#123301,#123302,
#123303,#123304,#123305,#123306,#123307,#123308,#123309,#123310,#123311,
#123312,#123313,#123314,#123315,#123316,#123317,#123318,#123319,#123320,
#123321,#123322,#123323,#123324,#123325,#123326,#123327,#123328,#123329,
#123330,#123331,#123332,#123333,#123334,#123335,#123336,#123337,#123338,
#123339,#123340,#123341,#123342,#123343,#123344,#123345,#123346,#123347,
#123348,#123349,#123350,#123351,#123352,#123353,#123354,#123355,#123356,
#123357,#123358,#123359,#123360,#123361,#123362,#123363,#123364,#123365,
#123366,#123367,#123368,#123369,#123370,#123371,#123372,#123373,#123374,
#123375,#123376,#123377,#123378,#123379,#123380,#123381,#123382,#123383,
#123384,#123385,#123386,#123387,#123388,#123389,#123390,#123391,#123392,
#123393,#123394,#123395,#123396,#123397,#123398,#123399,#123400,#123401,
#123402,#123403,#123404,#123405,#123406,#123407,#123408,#123409,#123410,
#123411,#123412,#123413,#123414,#123415,#123416,#123417,#123418,#123419,
#123420,#123421,#123422,#123423,#123424,#123425,#123426,#123427,#123428,
#123429,#123430,#123431,#123432,#123433,#123434,#123435,#123436,#123437,
#123438,#123439,#123440,#123441,#123442,#123443,#123444,#123445,#123446,
#123447,#123448,#123449,#123450,#123451,#123452,#123453,#123454,#123455,
#123456,#123457,#123458,#123459,#123460,#123461,#123462,#123463,#123464,
#123465,#123466,#123467,#123468,#123469,#123470,#123471,#123472,#123473,
#123474,#123475,#123476,#123477,#123478,#123479,#123480,#123481,#123482,
#123483,#123484,#123485,#123486,#123487,#123488,#123489,#123490,#123491,
#123492,#123493,#123494,#123495),.UNSPECIFIED.,.F.,.F.,(4,2,2,2,2,2,2,2,
2,2,2,2,2,2,2,2,2,2,2,2,2,2,2,2,2,2,2,2,2,2,2,2,2,2,2,2,2,2,2,2,2,2,2,2,
2,2,2,2,2,2,2,2,2,2,2,2,2,2,2,2,2,2,2,2,2,2,2,2,2,2,2,2,2,2,2,2,2,2,2,2,
2,2,2,2,2,2,2,2,2,2,2,2,2,2,2,2,2,2,4),(-4.84275027886607,-4.84016473224924,
-4.83781058688713,-4.8359439682687,-4.83423881191794,-4.83227663570649,
-4.82907566964572,-4.81821837465505,-4.78590128633185,-4.76939626374703,
-4.76186754653844,-4.75570038046285,-4.75208594971086,-4.74886769319487,
-4.74476809788961,-4.7381351756049,-4.70462640946889,-4.67497749940669,
-4.67066585404631,-4.66846839615449,-4.66666133332427,-4.66434458374319,
-4.65941670883551,-4.63505226931717,-4.61286602466617,-4.60007876296943,
-4.59087361610647,-4.58666867067668,-4.58343807736947,-4.57988083516064,
-4.57398362939074,-4.54914776203764,-4.5190201234511,-4.51051501377239,
-4.50470880122425,-4.50223720464507,-4.50041608977555,-4.49832534227604,
-4.49463157816885,-4.47254312207794,-4.46833478111313,-4.44614787245157,
-4.43336290723675,-4.4241589800867,-4.41995426562249,-4.41672372095439,
-4.41316640370285,-4.40726876756833,-4.38241739881447,-4.3523036213571,
-4.34380029404838,-4.33799497763074,-4.33552354112721,-4.3337024571724,
-4.3316116438335,-4.32791754524114,-4.30573021130639,-4.3019450688493,-4.27924799478739,
-4.26656801350084,-4.25741915716489,-4.25322407723578,-4.24999477459079,
-4.24643265670455,-4.24051233517303,-4.21477341083528,-4.18542359623272,
-4.17701837068339,-4.17126189229053,-4.16879863404778,-4.16697857985096,
-4.16488311622511,-4.16116817101942,-4.13674691676291,-4.11776137357766,
-4.09412199189254,-4.08841367945736,-4.08489665642377,-4.08165455002852,
-4.0774372352923,-4.06789238573397,-4.02978623754438,-4.01426865956622,
-4.00550399190194,-4.00261936019934,-4.00072549845072,-3.99879177759986,
-3.99572125639844,-3.98613613015403,-3.95343909709813,-3.93622106346518,
-3.92487771208003,-3.92032989752612,-3.91704662057629,-3.91362310414737,
-3.90835816025227,-3.89235947550556,-3.85363058724457,-3.85161562629314),
 .UNSPECIFIED.);
#2898=B_SPLINE_CURVE_WITH_KNOTS('',3,(#123501,#123502,#123503,#123504,#123505,
#123506,#123507,#123508,#123509,#123510,#123511,#123512,#123513,#123514,
#123515,#123516,#123517,#123518,#123519,#123520,#123521,#123522,#123523,
#123524,#123525,#123526,#123527,#123528,#123529,#123530,#123531,#123532,
#123533,#123534,#123535,#123536,#123537,#123538,#123539,#123540,#123541,
#123542,#123543,#123544,#123545,#123546,#123547,#123548,#123549,#123550,
#123551,#123552,#123553,#123554,#123555,#123556,#123557,#123558,#123559,
#123560,#123561,#123562,#123563,#123564,#123565,#123566,#123567,#123568,
#123569,#123570,#123571,#123572,#123573,#123574,#123575,#123576,#123577,
#123578,#123579,#123580,#123581,#123582,#123583,#123584,#123585,#123586,
#123587,#123588,#123589,#123590,#123591,#123592,#123593,#123594,#123595,
#123596,#123597,#123598,#123599,#123600,#123601,#123602,#123603,#123604,
#123605,#123606,#123607,#123608,#123609,#123610,#123611,#123612,#123613,
#123614,#123615,#123616,#123617,#123618,#123619,#123620,#123621,#123622,
#123623,#123624,#123625,#123626,#123627,#123628,#123629,#123630,#123631,
#123632,#123633,#123634,#123635,#123636,#123637,#123638,#123639,#123640,
#123641,#123642,#123643,#123644,#123645,#123646,#123647,#123648,#123649,
#123650,#123651,#123652,#123653,#123654,#123655,#123656,#123657,#123658,
#123659,#123660,#123661,#123662,#123663,#123664,#123665,#123666,#123667,
#123668,#123669,#123670,#123671,#123672,#123673,#123674,#123675,#123676,
#123677,#123678,#123679,#123680,#123681,#123682,#123683,#123684,#123685,
#123686,#123687,#123688),.UNSPECIFIED.,.F.,.F.,(4,2,2,2,2,2,2,2,2,2,2,2,
2,2,2,2,2,2,2,2,2,2,2,2,2,2,2,2,2,2,2,2,2,2,2,2,2,2,2,2,2,2,2,2,2,2,2,2,
2,2,2,2,2,2,2,2,2,2,2,2,2,2,2,2,2,2,2,2,2,2,2,2,2,2,2,2,2,2,2,2,2,2,2,2,
2,2,2,2,2,2,2,2,2,4),(-0.991269537285924,-0.990703049540231,-0.95950551951661,
-0.925920860047596,-0.921439259655927,-0.919208091960617,-0.917402432588172,
-0.915124029349346,-0.910398897690839,-0.89079815305279,-0.856285529713042,
-0.843306669751067,-0.838391042245147,-0.835373784673303,-0.832090910761312,
-0.827544600475137,-0.816209522722367,-0.799010407219534,-0.766377237774403,
-0.756772664097815,-0.753700225855695,-0.751766182089873,-0.749872828918714,
-0.746990073976569,-0.738240338359172,-0.722761152276517,-0.684804927974626,
-0.675113854394691,-0.670872442820286,-0.667626940805385,-0.664121076440339,
-0.658464295085302,-0.635718332442822,-0.616234319537125,-0.5932677177682,
-0.588413548878501,-0.586077876644514,-0.584270004264512,-0.582088435938074,
-0.577854585990412,-0.552682616179897,-0.513954012550315,-0.507650058425638,
-0.503646446615236,-0.500437376027691,-0.496761961955253,-0.490303135060156,
-0.456188255095197,-0.426416994098503,-0.421610575446495,-0.419316885964097,
-0.417511034148025,-0.415294311147537,-0.410884957570827,-0.405004152691311,
-0.38976535247827,-0.352705900857596,-0.342377724326619,-0.338307306313728,
-0.335301571860482,-0.332009608003629,-0.327410077377925,-0.315706132234414,
-0.297661638587813,-0.280686460663491,-0.258037466083515,-0.25434354042531,
-0.252253047272971,-0.250432399530354,-0.247961626157025,-0.242158231868365,
-0.233656732839965,-0.203554561739876,-0.178684499340552,-0.172790928289895,
-0.169235024933393,-0.166005090441219,-0.161800163308476,-0.152591054755118,
-0.139796141315294,-0.117647405365759,-0.113414453814164,-0.0914124834427105,
-0.0877210490486593,-0.0856311396626544,-0.0838104096785013,-0.0813387338904072,
-0.07552973642375,-0.0670168797564971,-0.0429024945777408,-0.0122258448422594,
-0.00636431777156412,-0.00292231655515231,-0.000491642754462011),
 .UNSPECIFIED.);
#2899=B_SPLINE_CURVE_WITH_KNOTS('',3,(#123689,#123690,#123691,#123692,#123693,
#123694,#123695,#123696,#123697,#123698,#123699,#123700),.UNSPECIFIED.,
 .F.,.F.,(4,2,2,2,2,4),(-2.09975934511255,-2.09808945502736,-2.09537980374138,
-2.08928500501059,-2.06056864970726,-2.04084412535128),.UNSPECIFIED.);
#2900=B_SPLINE_CURVE_WITH_KNOTS('',3,(#123701,#123702,#123703,#123704,#123705,
#123706,#123707,#123708,#123709,#123710,#123711,#123712,#123713,#123714,
#123715,#123716,#123717,#123718,#123719,#123720,#123721,#123722,#123723,
#123724,#123725,#123726,#123727,#123728,#123729,#123730,#123731,#123732,
#123733,#123734,#123735,#123736,#123737,#123738,#123739,#123740,#123741,
#123742,#123743,#123744,#123745,#123746,#123747,#123748,#123749,#123750,
#123751,#123752,#123753,#123754,#123755,#123756,#123757,#123758,#123759,
#123760,#123761,#123762,#123763,#123764,#123765,#123766,#123767,#123768,
#123769,#123770,#123771,#123772,#123773,#123774,#123775,#123776,#123777,
#123778,#123779,#123780,#123781,#123782,#123783,#123784,#123785,#123786,
#123787,#123788,#123789,#123790,#123791,#123792,#123793,#123794,#123795,
#123796,#123797,#123798,#123799,#123800,#123801,#123802,#123803,#123804,
#123805,#123806,#123807,#123808,#123809,#123810,#123811,#123812,#123813,
#123814,#123815,#123816,#123817,#123818,#123819,#123820,#123821,#123822,
#123823,#123824,#123825,#123826,#123827,#123828,#123829,#123830,#123831,
#123832,#123833,#123834,#123835,#123836,#123837,#123838,#123839,#123840,
#123841,#123842,#123843,#123844,#123845,#123846,#123847,#123848,#123849,
#123850,#123851,#123852,#123853,#123854,#123855,#123856,#123857,#123858,
#123859,#123860,#123861,#123862,#123863,#123864,#123865,#123866,#123867,
#123868,#123869,#123870,#123871,#123872,#123873,#123874,#123875,#123876,
#123877,#123878,#123879,#123880,#123881,#123882,#123883,#123884,#123885,
#123886,#123887,#123888,#123889,#123890,#123891,#123892,#123893,#123894,
#123895,#123896,#123897,#123898,#123899,#123900,#123901,#123902),
 .UNSPECIFIED.,.F.,.F.,(4,2,2,2,2,2,2,2,2,2,2,2,2,2,2,2,2,2,2,2,2,2,2,2,
2,2,2,2,2,2,2,2,2,2,2,2,2,2,2,2,2,2,2,2,2,2,2,2,2,2,2,2,2,2,2,2,2,2,2,2,
2,2,2,2,2,2,2,2,2,2,2,2,2,2,2,2,2,2,2,2,2,2,2,2,2,2,2,2,2,2,2,2,2,2,2,2,
2,2,2,2,4),(-3.85161562629314,-3.84422898914919,-3.83798758874284,-3.83544544478692,
-3.83361461612228,-3.83156086629186,-3.82793872235395,-3.81104232570972,
-3.76661694324815,-3.75728141288532,-3.75305420445616,-3.74982106203738,
-3.74627544532569,-3.74043157114328,-3.71695604383362,-3.68562584202229,
-3.67278495216338,-3.66951931682024,-3.66754312803081,-3.66570087304714,
-3.66341793431746,-3.65762050424875,-3.6251407403044,-3.59942500517989,
-3.59041095938543,-3.58623988922321,-3.58301386561286,-3.57944001720798,
-3.5734631783833,-3.54361456492192,-3.51766322693072,-3.50590426735176,
-3.50272387945276,-3.50076633606268,-3.49891296446719,-3.49613569747234,
-3.48883454057117,-3.45771289498189,-3.4326781868821,-3.42368807467503,
-3.41952125061821,-3.41629575074859,-3.41271968558842,-3.40673235307988,
-3.37846980362368,-3.35711780516387,-3.34544249729264,-3.33817898138171,
-3.33548568813289,-3.3336297504521,-3.33163922331026,-3.32830760265149,
-3.31608955147722,-3.28872548937564,-3.27013588463974,-3.25819998694201,
-3.25356726072747,-3.25026918906866,-3.24726975266234,-3.24322596209173,
-3.23306607732978,-3.18752384558539,-3.1776393815424,-3.17117158652448,
-3.16859437418031,-3.16675829128008,-3.16472117835881,-3.16117565342831,
-3.14556988072911,-3.11584778519816,-3.10104078083207,-3.09081751466479,
-3.08644243092351,-3.08318795252335,-3.0797060088438,-3.07416210705314,
-3.05517421163516,-3.0114791587665,-3.0045824383886,-3.0019411378807,-3.00009435699782,
-2.99808410321265,-2.99466253744258,-2.98120061049044,-2.95470942306851,
-2.93646039638031,-2.92466850831725,-2.92005587535993,-2.9167612068738,
-2.91375753592395,-2.90969686342703,-2.89943386723997,-2.85858612601351,
-2.84582565906082,-2.83811110538271,-2.8353565848152,-2.83348895174086,
-2.83151862172262,-2.82828012678467,-2.81703552151411,-2.80145779137746),
 .UNSPECIFIED.);
#2901=B_SPLINE_CURVE_WITH_KNOTS('',3,(#123907,#123908,#123909,#123910,#123911,
#123912,#123913,#123914,#123915,#123916,#123917,#123918,#123919,#123920,
#123921,#123922,#123923,#123924,#123925,#123926,#123927,#123928,#123929,
#123930,#123931,#123932,#123933,#123934,#123935,#123936,#123937,#123938,
#123939,#123940,#123941,#123942,#123943,#123944,#123945,#123946,#123947,
#123948,#123949,#123950,#123951,#123952,#123953,#123954,#123955,#123956,
#123957,#123958,#123959,#123960,#123961,#123962,#123963,#123964,#123965,
#123966,#123967,#123968,#123969,#123970,#123971,#123972,#123973,#123974,
#123975,#123976,#123977,#123978,#123979,#123980,#123981,#123982,#123983,
#123984,#123985,#123986,#123987,#123988,#123989,#123990,#123991,#123992,
#123993,#123994,#123995,#123996,#123997,#123998,#123999,#124000,#124001,
#124002,#124003,#124004,#124005,#124006,#124007,#124008,#124009,#124010,
#124011,#124012,#124013,#124014,#124015,#124016,#124017,#124018,#124019,
#124020,#124021,#124022,#124023,#124024,#124025,#124026,#124027,#124028,
#124029,#124030,#124031,#124032,#124033,#124034,#124035,#124036,#124037,
#124038,#124039,#124040,#124041,#124042,#124043,#124044,#124045,#124046,
#124047,#124048,#124049,#124050,#124051,#124052,#124053,#124054,#124055,
#124056,#124057,#124058,#124059,#124060,#124061,#124062,#124063,#124064,
#124065,#124066,#124067,#124068,#124069,#124070,#124071,#124072,#124073,
#124074,#124075,#124076,#124077,#124078,#124079,#124080,#124081,#124082,
#124083,#124084,#124085,#124086,#124087,#124088,#124089,#124090,#124091,
#124092,#124093,#124094,#124095,#124096,#124097,#124098,#124099,#124100,
#124101,#124102,#124103,#124104,#124105,#124106,#124107,#124108,#124109,
#124110,#124111,#124112,#124113,#124114),.UNSPECIFIED.,.F.,.F.,(4,2,2,2,
2,2,2,2,2,2,2,2,2,2,2,2,2,2,2,2,2,2,2,2,2,2,2,2,2,2,2,2,2,2,2,2,2,2,2,2,
2,2,2,2,2,2,2,2,2,2,2,2,2,2,2,2,2,2,2,2,2,2,2,2,2,2,2,2,2,2,2,2,2,2,2,2,
2,2,2,2,2,2,2,2,2,2,2,2,2,2,2,2,2,2,2,2,2,2,2,2,2,2,2,4),(-2.04107054618519,
-2.01310847198346,-2.00662462122167,-2.00294361178816,-1.99973459518817,
-1.99573751068811,-1.98945697572702,-1.95052272761901,-1.92553552185573,
-1.92130295956127,-1.91912146844143,-1.91731333282856,-1.9149768726701,
-1.91011963004885,-1.88577824426209,-1.86360859074923,-1.85080457342558,
-1.84159095974072,-1.83738459475986,-1.83415383279138,-1.83059729799196,
-1.8247033134626,-1.79995365193905,-1.76976993096714,-1.76125875153898,
-1.75544969655322,-1.75297765404215,-1.75115648906623,-1.74906593760263,
-1.74537298107917,-1.72338130415929,-1.71911228084971,-1.69694125636454,
-1.68414075681005,-1.67492899980363,-1.67072297756311,-1.66749227980551,
-1.66393561713663,-1.65804094865667,-1.63326790790759,-1.60310501672582,
-1.59459649388533,-1.58878876853925,-1.58631695759483,-1.5844958311485,
-1.58240516886669,-1.57871168611666,-1.55657190302086,-1.55241258667971,
-1.53023080902313,-1.51745878609539,-1.50826194567617,-1.50405853636767,
-1.50082818708284,-1.4972702515797,-1.49136953088272,-1.46639150666275,
-1.43640725307171,-1.42792133953288,-1.42212485147269,-1.41965492279101,
-1.4178340423157,-1.41574233471353,-1.41204413776501,-1.38879472627267,
-1.38627809892863,-1.36345942603214,-1.3507500573391,-1.34158608909442,
-1.33738844886172,-1.33415886518938,-1.33059810271997,-1.3246839371242,
-1.29918590247435,-1.27851159046928,-1.26449794602418,-1.25629040763044,
-1.25347290339832,-1.25159286662889,-1.24987964025549,-1.24695733860765,
-1.238589950454,-1.20516104438669,-1.18746475181874,-1.17959996114186,-1.17322048769713,
-1.16956144594394,-1.16635005634423,-1.16232157327202,-1.15593345555153,
-1.11809304305186,-1.09222648107476,-1.08798927861505,-1.08580690576362,
-1.0839989194083,-1.0816637851635,-1.07681297460773,-1.05036589697884,-1.0144038356493,
-1.00787012551006,-1.00379934037544,-1.00058412445147,-0.996952468312172,
-0.991269537285924),.UNSPECIFIED.);
#2902=B_SPLINE_CURVE_WITH_KNOTS('',3,(#124115,#124116,#124117,#124118,#124119,
#124120,#124121,#124122,#124123,#124124,#124125,#124126,#124127,#124128,
#124129,#124130,#124131,#124132,#124133,#124134,#124135,#124136,#124137,
#124138,#124139,#124140,#124141,#124142,#124143,#124144,#124145,#124146,
#124147,#124148,#124149,#124150,#124151,#124152,#124153,#124154,#124155,
#124156,#124157,#124158,#124159,#124160,#124161,#124162,#124163,#124164,
#124165,#124166,#124167,#124168,#124169,#124170,#124171,#124172,#124173,
#124174,#124175,#124176,#124177,#124178,#124179,#124180,#124181,#124182,
#124183,#124184,#124185,#124186,#124187,#124188,#124189,#124190,#124191,
#124192,#124193,#124194,#124195,#124196,#124197,#124198,#124199,#124200,
#124201,#124202,#124203,#124204,#124205,#124206,#124207,#124208,#124209,
#124210,#124211,#124212,#124213,#124214,#124215,#124216,#124217,#124218,
#124219,#124220,#124221,#124222,#124223,#124224,#124225,#124226,#124227,
#124228,#124229,#124230,#124231,#124232,#124233,#124234,#124235,#124236,
#124237,#124238,#124239,#124240,#124241,#124242,#124243,#124244,#124245,
#124246,#124247,#124248,#124249,#124250,#124251,#124252,#124253,#124254,
#124255,#124256,#124257,#124258,#124259,#124260,#124261,#124262,#124263,
#124264,#124265,#124266,#124267,#124268,#124269,#124270,#124271,#124272,
#124273,#124274,#124275,#124276,#124277,#124278,#124279,#124280,#124281,
#124282,#124283,#124284,#124285,#124286,#124287,#124288,#124289,#124290,
#124291,#124292,#124293,#124294,#124295,#124296,#124297,#124298,#124299,
#124300,#124301,#124302,#124303,#124304,#124305,#124306,#124307,#124308,
#124309,#124310,#124311,#124312,#124313,#124314,#124315,#124316,#124317,
#124318,#124319,#124320,#124321,#124322),.UNSPECIFIED.,.F.,.F.,(4,2,2,2,
2,2,2,2,2,2,2,2,2,2,2,2,2,2,2,2,2,2,2,2,2,2,2,2,2,2,2,2,2,2,2,2,2,2,2,2,
2,2,2,2,2,2,2,2,2,2,2,2,2,2,2,2,2,2,2,2,2,2,2,2,2,2,2,2,2,2,2,2,2,2,2,2,
2,2,2,2,2,2,2,2,2,2,2,2,2,2,2,2,2,2,2,2,2,2,2,2,2,2,2,4),(-2.80145779137746,
-2.78896159018484,-2.76065937660977,-2.75475076405021,-2.75119125405688,
-2.74796152760446,-2.74383192612798,-2.73480028451152,-2.69214947388333,
-2.67918126361283,-2.67138289311765,-2.66861735239108,-2.66674755332195,
-2.66502304060338,-2.66204251681594,-2.65321675681465,-2.62333083237893,
-2.59903401702736,-2.59003080747544,-2.58586142906437,-2.58263537253487,
-2.57906012945557,-2.57307766544307,-2.54364620796484,-2.5214373896112,
-2.51102773651572,-2.50431940340741,-2.50170580074452,-2.49986372952664,
-2.4978422275805,-2.49436898823024,-2.48011767320355,-2.44977971349942,
-2.42674378021518,-2.42106937511479,-2.41755968518172,-2.41431538011272,
-2.41000843331411,-2.40020215529185,-2.38624237839934,-2.36569175343155,
-2.36258610885424,-2.33986316981788,-2.33616806478412,-2.33407713804524,
-2.33225632814433,-2.32978569688586,-2.32398432882326,-2.31548762194585,
-2.28543561237568,-2.26048489065247,-2.25458411090553,-2.25102639323188,
-2.24779644399342,-2.24359387765608,-2.23440032340412,-2.22163624925089,
-2.19946269564246,-2.19538573290667,-2.1731653409063,-2.16947222616816,
-2.16738178382152,-2.16556092017402,-2.16308959487641,-2.15728391154746,
-2.14877846310981,-2.11865680998143,-2.09378688310051,-2.08788854710639,
-2.08433137279343,-2.08110132792379,-2.07689779098648,-2.06769850222521,
-2.05492339079155,-2.03275438431432,-2.02861530251389,-2.00647362740441,
-2.00278083635211,-2.00069046769594,-1.99886954142242,-1.99639797741833,
-1.99059113130804,-1.98208334630553,-1.95194209120561,-1.92709953879681,
-1.92120210497237,-1.91764510054041,-1.91441496813857,-1.91021096540058,
-1.90100913527937,-1.88822921860791,-1.86606222275285,-1.86189502278057,
-1.83978835955354,-1.83609576517553,-1.8340054666012,-1.83218474764661,
-1.82971356212138,-1.82390767112326,-1.81540152283688,-1.78527223705395,
-1.7604114978068,-1.75451388622684,-1.75142894609207),.UNSPECIFIED.);
#2903=B_SPLINE_CURVE_WITH_KNOTS('',3,(#124328,#124329,#124330,#124331,#124332,
#124333,#124334,#124335,#124336,#124337,#124338,#124339,#124340,#124341,
#124342,#124343,#124344,#124345,#124346,#124347,#124348,#124349,#124350,
#124351,#124352,#124353,#124354,#124355,#124356,#124357,#124358,#124359,
#124360,#124361,#124362,#124363,#124364,#124365,#124366,#124367,#124368,
#124369,#124370,#124371,#124372,#124373,#124374,#124375,#124376,#124377,
#124378,#124379,#124380,#124381,#124382,#124383,#124384,#124385,#124386,
#124387,#124388,#124389,#124390,#124391,#124392,#124393,#124394,#124395,
#124396,#124397,#124398,#124399,#124400,#124401,#124402,#124403,#124404,
#124405,#124406,#124407,#124408,#124409,#124410,#124411,#124412,#124413,
#124414,#124415,#124416,#124417,#124418,#124419,#124420,#124421,#124422,
#124423,#124424,#124425,#124426,#124427,#124428,#124429,#124430,#124431,
#124432,#124433,#124434,#124435,#124436,#124437,#124438,#124439,#124440,
#124441,#124442,#124443,#124444,#124445,#124446,#124447,#124448,#124449,
#124450,#124451,#124452,#124453,#124454,#124455,#124456,#124457,#124458,
#124459),.UNSPECIFIED.,.F.,.F.,(4,2,2,2,2,2,2,2,2,2,2,2,2,2,2,2,2,2,2,2,
2,2,2,2,2,2,2,2,2,2,2,2,2,2,2,2,2,2,2,2,2,2,2,2,2,2,2,2,2,2,2,2,2,2,2,2,
2,2,2,2,2,2,2,2,2,4),(-0.701636287487779,-0.697839022662261,-0.674842325607004,
-0.669935798104173,-0.667629296920877,-0.665824141089188,-0.663621013114632,
-0.659300671945522,-0.630980069288784,-0.59588492751791,-0.589277207730714,
-0.585173589306852,-0.581939989173495,-0.578295060076084,-0.57204027932623,
-0.538649314979816,-0.507757634175514,-0.503066608646091,-0.500782882059722,
-0.498948465648512,-0.496647185185076,-0.491945406013739,-0.472805016475768,
-0.439048031476098,-0.426344007398241,-0.421441693617695,-0.418403301137768,
-0.415073076198448,-0.410413078920198,-0.398498664926513,-0.380066513848475,
-0.353359115340523,-0.340063944669906,-0.336658492707012,-0.334655043329414,
-0.332872377637875,-0.330400026083402,-0.324064296950665,-0.314351289671585,
-0.272080613631591,-0.257154727894049,-0.252128682248939,-0.248855833352114,
-0.245718104367162,-0.241379608577404,-0.230653790706167,-0.214561853511444,
-0.183199278226535,-0.17147019173188,-0.16825229308572,-0.166320947747948,
-0.164456275517811,-0.161758386229062,-0.154578958792954,-0.116805722640352,
-0.0871659769434536,-0.0806283029311778,-0.0766838441689992,-0.0730896597176575,
-0.0683736923888758,-0.0576675656256708,-0.0323065871038856,-0.00779140283112945,
-0.00345801209014825,-0.00158323791527608,-5.8761756664911E-5),
 .UNSPECIFIED.);
#2904=B_SPLINE_CURVE_WITH_KNOTS('',3,(#124462,#124463,#124464,#124465,#124466,
#124467,#124468,#124469,#124470,#124471,#124472,#124473,#124474,#124475,
#124476,#124477,#124478,#124479,#124480,#124481,#124482,#124483,#124484,
#124485,#124486,#124487,#124488,#124489,#124490,#124491,#124492,#124493,
#124494,#124495,#124496,#124497,#124498,#124499,#124500,#124501,#124502,
#124503,#124504,#124505,#124506,#124507,#124508,#124509,#124510,#124511,
#124512,#124513,#124514,#124515,#124516,#124517,#124518,#124519,#124520,
#124521,#124522,#124523,#124524,#124525,#124526,#124527,#124528,#124529,
#124530,#124531,#124532,#124533,#124534,#124535,#124536,#124537,#124538,
#124539,#124540,#124541,#124542,#124543,#124544,#124545,#124546,#124547,
#124548,#124549,#124550,#124551,#124552,#124553,#124554,#124555,#124556,
#124557,#124558,#124559,#124560,#124561,#124562,#124563,#124564,#124565,
#124566,#124567,#124568,#124569,#124570,#124571,#124572,#124573,#124574,
#124575,#124576,#124577,#124578,#124579,#124580,#124581,#124582,#124583,
#124584,#124585,#124586,#124587,#124588,#124589,#124590,#124591,#124592,
#124593,#124594,#124595,#124596,#124597,#124598,#124599,#124600,#124601,
#124602,#124603,#124604,#124605,#124606,#124607,#124608,#124609,#124610,
#124611,#124612,#124613,#124614,#124615,#124616,#124617,#124618,#124619,
#124620,#124621,#124622,#124623,#124624,#124625,#124626,#124627,#124628,
#124629,#124630,#124631,#124632,#124633,#124634,#124635,#124636,#124637,
#124638,#124639,#124640,#124641,#124642,#124643,#124644,#124645,#124646,
#124647,#124648,#124649),.UNSPECIFIED.,.F.,.F.,(4,2,2,2,2,2,2,2,2,2,2,2,
2,2,2,2,2,2,2,2,2,2,2,2,2,2,2,2,2,2,2,2,2,2,2,2,2,2,2,2,2,2,2,2,2,2,2,2,
2,2,2,2,2,2,2,2,2,2,2,2,2,2,2,2,2,2,2,2,2,2,2,2,2,2,2,2,2,2,2,2,2,2,2,2,
2,2,2,2,2,2,2,2,2,4),(-1.97964531136435,-1.97911906260677,-1.97225183621543,
-1.93766010376271,-1.91989896127257,-1.91198669364148,-1.90555923283692,
-1.90186475831735,-1.8986163535856,-1.89453160537323,-1.88802575250684,
-1.85357382618518,-1.82637417573715,-1.82198916105945,-1.81975004909482,
-1.81791464338252,-1.81556138103437,-1.81067997802214,-1.78640428098552,
-1.76445474780961,-1.75162112186658,-1.74238702862777,-1.73816368383357,
-1.73491589042239,-1.73133611421782,-1.72539172543349,-1.69958592330072,
-1.67019866891438,-1.66177843083949,-1.65601018612154,-1.65354030782054,
-1.65171844439193,-1.64963188226422,-1.64593216701741,-1.62181468261427,
-1.62032922398492,-1.59987229126258,-1.58572494923463,-1.57583725480986,
-1.57153125059668,-1.56830199632932,-1.56482280808428,-1.55923107601898,
-1.539648107259,-1.49638525171747,-1.48950671320994,-1.48687845082069,-1.48504077470034,
-1.48303359177249,-1.47962596458339,-1.46637430092727,-1.43973515849324,
-1.4214213025529,-1.40959677425905,-1.40497527064041,-1.40167512107569,
-1.39866685832657,-1.39382125836553,-1.38136134147017,-1.34651562821764,
-1.3319078439555,-1.32617651666678,-1.32185071527014,-1.31964694934694,
-1.31783664899341,-1.31551689909332,-1.31057937031736,-1.2858478321638,
-1.25896213776951,-1.24895244016569,-1.24127794540381,-1.23735476108039,
-1.23414893049417,-1.23040845522217,-1.22382856709703,-1.18243440748928,
-1.16601811569556,-1.15693804872218,-1.15401723704396,-1.15211571981282,
-1.15042233358238,-1.14760293755012,-1.13998630650627,-1.1091363132709,
-1.08426168631806,-1.07527240257569,-1.0711073135409,-1.06788376091033,
-1.0643105094788,-1.0583296155778,-1.02901015493119,-1.00699503835577,-0.99128888870559,
-0.991281231630979),.UNSPECIFIED.);
#2905=B_SPLINE_CURVE_WITH_KNOTS('',3,(#124652,#124653,#124654,#124655,#124656,
#124657,#124658,#124659,#124660,#124661,#124662,#124663,#124664,#124665,
#124666,#124667,#124668,#124669,#124670,#124671,#124672,#124673,#124674,
#124675,#124676,#124677,#124678,#124679,#124680,#124681,#124682,#124683,
#124684,#124685,#124686,#124687,#124688,#124689,#124690,#124691,#124692,
#124693,#124694,#124695,#124696,#124697,#124698,#124699,#124700,#124701,
#124702,#124703,#124704,#124705,#124706,#124707,#124708,#124709,#124710,
#124711,#124712,#124713,#124714,#124715,#124716,#124717,#124718,#124719,
#124720,#124721,#124722,#124723,#124724,#124725,#124726,#124727,#124728,
#124729,#124730,#124731,#124732,#124733,#124734,#124735,#124736,#124737,
#124738,#124739,#124740,#124741,#124742,#124743,#124744,#124745,#124746,
#124747,#124748,#124749,#124750,#124751,#124752,#124753,#124754,#124755,
#124756,#124757,#124758,#124759,#124760,#124761,#124762,#124763,#124764,
#124765,#124766,#124767,#124768,#124769,#124770,#124771,#124772,#124773,
#124774,#124775,#124776,#124777,#124778,#124779,#124780,#124781,#124782,
#124783,#124784,#124785,#124786,#124787,#124788,#124789,#124790,#124791,
#124792,#124793,#124794,#124795,#124796,#124797,#124798,#124799,#124800,
#124801,#124802,#124803,#124804,#124805,#124806,#124807,#124808,#124809,
#124810,#124811,#124812,#124813,#124814,#124815,#124816,#124817,#124818,
#124819,#124820,#124821,#124822,#124823,#124824,#124825,#124826,#124827,
#124828,#124829,#124830,#124831,#124832,#124833,#124834,#124835,#124836,
#124837,#124838,#124839,#124840,#124841,#124842,#124843,#124844,#124845,
#124846,#124847,#124848,#124849,#124850,#124851,#124852,#124853,#124854,
#124855,#124856,#124857,#124858,#124859,#124860,#124861,#124862,#124863,
#124864,#124865,#124866,#124867,#124868,#124869,#124870,#124871,#124872,
#124873,#124874,#124875,#124876,#124877,#124878,#124879,#124880,#124881,
#124882,#124883,#124884,#124885,#124886,#124887,#124888,#124889,#124890,
#124891,#124892,#124893,#124894,#124895,#124896,#124897,#124898,#124899,
#124900,#124901,#124902,#124903,#124904,#124905,#124906,#124907),
 .UNSPECIFIED.,.F.,.F.,(4,2,2,2,2,2,2,2,2,2,2,2,2,2,2,2,2,2,2,2,2,2,2,2,
2,2,2,2,2,2,2,2,2,2,2,2,2,2,2,2,2,2,2,2,2,2,2,2,2,2,2,2,2,2,2,2,2,2,2,2,
2,2,2,2,2,2,2,2,2,2,2,2,2,2,2,2,2,2,2,2,2,2,2,2,2,2,2,2,2,2,2,2,2,2,2,2,
2,2,2,2,2,2,2,2,2,2,2,2,2,2,2,2,2,2,2,2,2,2,2,2,2,2,2,2,2,2,2,4),(-0.991281231630979,
-0.987841854375976,-0.985827044042622,-0.983983179222014,-0.98135732077623,
-0.974566319623724,-0.931108639327705,-0.911819953225727,-0.906231241791206,
-0.902739454556782,-0.899488089452126,-0.895135911242685,-0.8850558789029,
-0.870542721323148,-0.850460109323952,-0.82708850730907,-0.822165749574291,
-0.819849781275316,-0.818042680006527,-0.815844301721315,-0.811527240667509,
-0.80580748114327,-0.791239087038924,-0.75661318667677,-0.743766727958745,
-0.738869990459187,-0.735856370801476,-0.732571241315397,-0.728010229665721,
-0.716572520714517,-0.699140392147666,-0.666165381766055,-0.657142292836879,
-0.654138218993048,-0.652409390323099,-0.650544039211167,-0.64779948203039,
-0.640156770976696,-0.627569281044651,-0.588167522956102,-0.5766552017642,
-0.571957755024135,-0.568681194006056,-0.565306807515165,-0.560277176713261,
-0.545146916752413,-0.517514277810206,-0.516002232605101,-0.491903183835174,
-0.488196457495654,-0.486103263408001,-0.484283385877947,-0.481817932880979,
-0.476046074904421,-0.467607887531038,-0.438000026011006,-0.412566265076903,
-0.406653986717998,-0.40309413949198,-0.39986525522998,-0.395668327792562,
-0.386504863542936,-0.373796875944327,-0.351624831145559,-0.347995439706742,
-0.32526916214332,-0.321575095137334,-0.319484593450501,-0.31766403004118,
-0.315193446071637,-0.309390695753284,-0.300890308539575,-0.270794594335009,
-0.245927954475505,-0.240031187576714,-0.236474752157447,-0.233245217746195,
-0.229042079835067,-0.219842298474118,-0.20706492889809,-0.184910337920613,
-0.160592686606324,-0.155661279801007,-0.153344353186599,-0.151609418164389,
-0.151583300442266,-0.151541932247801,-0.1515024327774,-0.151464648530632,
-0.151428442165346,-0.151393690519353,-0.151360282819415,-0.151328119031109,
-0.151297108611142,-0.151267169372692,-0.151238226498512,-0.151210211768088,
-0.151183062866975,-0.151156722613911,-0.151131138490097,-0.151106262085664,
-0.151082048741073,-0.151058457392603,-0.151035449836252,-0.151012990563013,
-0.15099104666073,-0.150969587475618,-0.150948584314081,-0.150928010558224,
-0.1509078410711,-0.150888052474096,-0.150868622766498,-0.150849531147258,
-0.150830758147573,-0.15081228521397,-0.150794094974534,-0.148405459333805,
-0.145516080973216,-0.140312230792917,-0.127769787531509,-0.0887276269360894,
-0.0769078943937671,-0.0721628819432224,-0.0688776120374353,-0.0655145066124617,
-0.0605404380655912,-0.0459057461101224,-0.000494228016458911),
 .UNSPECIFIED.);
#2906=B_SPLINE_CURVE_WITH_KNOTS('',3,(#124908,#124909,#124910,#124911,#124912,
#124913,#124914,#124915,#124916,#124917,#124918,#124919,#124920,#124921,
#124922,#124923,#124924,#124925,#124926,#124927),.UNSPECIFIED.,.F.,.F.,
(4,2,2,2,2,2,2,2,2,4),(-2.09990490037868,-2.09043166092189,-2.08804132421848,
-2.08624835223061,-2.08446713995306,-2.0823589812838,-2.07858689204649,
-2.0625197928987,-2.04247110725939,-2.04107054618519),.UNSPECIFIED.);
#2907=B_SPLINE_CURVE_WITH_KNOTS('',3,(#124928,#124929,#124930,#124931,#124932,
#124933,#124934,#124935,#124936,#124937,#124938,#124939,#124940,#124941,
#124942,#124943,#124944,#124945,#124946,#124947,#124948,#124949,#124950,
#124951,#124952,#124953,#124954,#124955,#124956,#124957,#124958,#124959,
#124960,#124961,#124962,#124963,#124964,#124965,#124966,#124967,#124968,
#124969,#124970,#124971,#124972,#124973,#124974,#124975,#124976,#124977,
#124978,#124979,#124980,#124981,#124982,#124983,#124984,#124985,#124986,
#124987,#124988,#124989,#124990,#124991,#124992,#124993,#124994,#124995,
#124996,#124997,#124998,#124999,#125000,#125001,#125002,#125003,#125004,
#125005,#125006,#125007,#125008,#125009,#125010,#125011,#125012,#125013,
#125014,#125015,#125016,#125017,#125018,#125019,#125020,#125021,#125022,
#125023,#125024,#125025,#125026,#125027,#125028,#125029,#125030,#125031,
#125032,#125033,#125034,#125035,#125036,#125037,#125038,#125039,#125040,
#125041,#125042,#125043,#125044,#125045,#125046,#125047,#125048,#125049,
#125050,#125051,#125052,#125053,#125054,#125055,#125056,#125057,#125058,
#125059,#125060,#125061,#125062,#125063,#125064,#125065,#125066,#125067,
#125068,#125069,#125070,#125071,#125072,#125073,#125074,#125075,#125076,
#125077,#125078,#125079,#125080,#125081,#125082,#125083,#125084,#125085,
#125086,#125087,#125088,#125089,#125090,#125091,#125092,#125093,#125094,
#125095,#125096,#125097,#125098,#125099,#125100,#125101,#125102,#125103,
#125104,#125105,#125106,#125107,#125108,#125109,#125110,#125111,#125112,
#125113,#125114,#125115,#125116,#125117,#125118,#125119,#125120,#125121,
#125122,#125123,#125124,#125125,#125126,#125127,#125128,#125129,#125130,
#125131,#125132,#125133,#125134,#125135,#125136,#125137,#125138,#125139,
#125140,#125141,#125142,#125143,#125144,#125145,#125146,#125147),
 .UNSPECIFIED.,.F.,.F.,(4,2,2,2,2,2,2,2,2,2,2,2,2,2,2,2,2,2,2,2,2,2,2,2,
2,2,2,2,2,2,2,2,2,2,2,2,2,2,2,2,2,2,2,2,2,2,2,2,2,2,2,2,2,2,2,2,2,2,2,2,
2,2,2,2,2,2,2,2,2,2,2,2,2,2,2,2,2,2,2,2,2,2,2,2,2,2,2,2,2,2,2,2,2,2,2,2,
2,2,2,2,2,2,2,2,2,2,2,2,2,4),(-1.75142894609207,-1.75095713874224,-1.74772748361246,
-1.74352446718888,-1.73432644337936,-1.72155332420707,-1.69938424111941,
-1.69525426652509,-1.67310192840444,-1.66940942498326,-1.66731927438308,
-1.66549856604467,-1.66302738794025,-1.65722197012572,-1.64871690159625,
-1.61859723219913,-1.59372423678049,-1.58782589978092,-1.58426878683924,
-1.58103883626336,-1.57683547439035,-1.56763675368805,-1.55486241908422,
-1.53269596525806,-1.52856245150482,-1.50641870843793,-1.50272593505734,
-1.50063552704098,-1.49881420938223,-1.49634176309703,-1.49053183263272,
-1.48201809215829,-1.45182576528587,-1.42706593931722,-1.42117109341108,
-1.41761432461896,-1.41438353616731,-1.41017739928,-1.40096528114554,-1.38816631177653,
-1.36600722716564,-1.36174248910034,-1.3397586580243,-1.33606662227047,
-1.33397647904982,-1.3321567252544,-1.32968741846762,-1.32388641432743,
-1.31538873480248,-1.28532212280671,-1.2603663198895,-1.25446772902036,
-1.25091224982781,-1.24768499218589,-1.24348696239449,-1.23430829110508,
-1.22156988424774,-1.19939047269532,-1.19552891957004,-1.17306010274023,
-1.16936774074632,-1.16727830310697,-1.16545789277088,-1.16298740348159,
-1.15718702352554,-1.14869261632144,-1.11866528213641,-1.09366419091909,
-1.08776016999212,-1.08420093187642,-1.0809698469739,-1.07676610057186,
-1.06757072604844,-1.05480303659534,-1.03264531143523,-1.02857602498704,
-1.00637624614241,-1.00268161094015,-1.00058973459417,-0.99876459702422,
-0.996284369391697,-0.990447932930247,-0.981883776358615,-0.951268355677309,
-0.927157000105235,-0.921283515208742,-0.917728276059511,-0.914491424142104,
-0.910266424699868,-0.90096480605169,-0.888000799238241,-0.866041260337691,
-0.861497363765283,-0.839845667046236,-0.836155330683252,-0.834065657641216,
-0.832435350289788,-0.830094796724561,-0.82498563971461,-0.817825118097722,
-0.796437579356522,-0.762792692199946,-0.756158679111235,-0.752070995436364,
-0.748870480093518,-0.745285310224462,-0.739193186305052,-0.731771727027432,
-0.715598489243652,-0.701636287487779),.UNSPECIFIED.);
#2908=B_SPLINE_CURVE_WITH_KNOTS('',3,(#125150,#125151,#125152,#125153,#125154,
#125155,#125156,#125157,#125158,#125159,#125160,#125161,#125162,#125163,
#125164,#125165,#125166,#125167,#125168,#125169,#125170,#125171,#125172,
#125173,#125174,#125175,#125176,#125177,#125178,#125179,#125180,#125181,
#125182,#125183,#125184,#125185,#125186,#125187,#125188,#125189,#125190,
#125191,#125192,#125193,#125194,#125195,#125196,#125197,#125198,#125199,
#125200,#125201,#125202,#125203,#125204,#125205,#125206,#125207,#125208,
#125209,#125210,#125211,#125212,#125213,#125214,#125215,#125216,#125217,
#125218,#125219,#125220,#125221,#125222,#125223,#125224,#125225,#125226,
#125227,#125228,#125229,#125230,#125231,#125232,#125233,#125234,#125235,
#125236,#125237,#125238,#125239,#125240,#125241,#125242,#125243,#125244,
#125245,#125246,#125247,#125248,#125249,#125250,#125251,#125252,#125253,
#125254,#125255,#125256,#125257,#125258,#125259,#125260,#125261,#125262,
#125263,#125264,#125265,#125266,#125267,#125268,#125269,#125270,#125271,
#125272,#125273,#125274,#125275,#125276,#125277,#125278,#125279,#125280,
#125281,#125282,#125283,#125284,#125285,#125286,#125287,#125288,#125289,
#125290,#125291,#125292,#125293,#125294,#125295,#125296,#125297,#125298,
#125299,#125300,#125301,#125302,#125303,#125304,#125305,#125306,#125307,
#125308,#125309,#125310,#125311,#125312,#125313,#125314,#125315,#125316,
#125317,#125318,#125319,#125320,#125321,#125322,#125323,#125324,#125325,
#125326,#125327,#125328,#125329,#125330,#125331,#125332,#125333,#125334,
#125335,#125336,#125337,#125338,#125339,#125340,#125341,#125342,#125343,
#125344,#125345,#125346,#125347,#125348,#125349,#125350,#125351,#125352,
#125353,#125354,#125355,#125356,#125357,#125358,#125359,#125360,#125361,
#125362,#125363,#125364,#125365,#125366,#125367,#125368,#125369,#125370,
#125371,#125372,#125373,#125374,#125375,#125376,#125377,#125378,#125379,
#125380,#125381,#125382,#125383,#125384,#125385,#125386,#125387,#125388,
#125389,#125390,#125391,#125392,#125393,#125394,#125395,#125396,#125397,
#125398,#125399,#125400,#125401,#125402,#125403,#125404,#125405),
 .UNSPECIFIED.,.F.,.F.,(4,2,2,2,2,2,2,2,2,2,2,2,2,2,2,2,2,2,2,2,2,2,2,2,
2,2,2,2,2,2,2,2,2,2,2,2,2,2,2,2,2,2,2,2,2,2,2,2,2,2,2,2,2,2,2,2,2,2,2,2,
2,2,2,2,2,2,2,2,2,2,2,2,2,2,2,2,2,2,2,2,2,2,2,2,2,2,2,2,2,2,2,2,2,2,2,2,
2,2,2,2,2,2,2,2,2,2,2,2,2,2,2,2,2,2,2,2,2,2,2,2,2,2,2,2,2,2,2,4),(-0.991277804245244,
-0.987838448409618,-0.985823649756141,-0.983979794703957,-0.98135394827412,
-0.974562966697378,-0.931105483638177,-0.911816991114433,-0.906228317826688,
-0.902736551807322,-0.899485204675701,-0.895133047792989,-0.885053051592897,
-0.870539933308402,-0.850457508069912,-0.827086044899166,-0.822163315600623,
-0.819847360658439,-0.81804026966992,-0.815841903638442,-0.811524866438444,
-0.805805138274295,-0.791236822040495,-0.756611094699905,-0.743764744147221,
-0.738868039097699,-0.735854437103005,-0.732569325042841,-0.728008334130301,
-0.71657065681125,-0.699138550843459,-0.666163608442,-0.657140782212213,
-0.654136750727445,-0.652407936626109,-0.650542591683229,-0.647798028158866,
-0.640155197245282,-0.627567378870247,-0.588162555419262,-0.576653032048378,
-0.571956112453222,-0.568679661538219,-0.565305172825671,-0.560274972272466,
-0.545139343808745,-0.517488068241534,-0.516247630991732,-0.491911198802518,
-0.488199484486295,-0.48610518199033,-0.484285553773042,-0.481822057758018,
-0.476061839671524,-0.467646997273333,-0.4382190656533,-0.412575153260324,
-0.406658005106013,-0.40309713426503,-0.39986852461374,-0.395673675123066,
-0.386522030649031,-0.373836535048676,-0.35109515600548,-0.347920538781888,
-0.325267942885641,-0.321574187066173,-0.319483759665895,-0.317663188142843,
-0.315192495640078,-0.30938906116643,-0.300887283669319,-0.270780418733576,
-0.245926838186652,-0.240030481959969,-0.236474142258809,-0.233244598582025,
-0.229041310507891,-0.219840611989913,-0.207061471873289,-0.184907685339927,
-0.160592809930546,-0.15566131976479,-0.153344382769017,-0.15160945433713,
-0.151583329528716,-0.151541959998941,-0.151502459357567,-0.151464673950257,
-0.151428466513842,-0.151393713866275,-0.151360305234534,-0.15132814056872,
-0.151297129297126,-0.151267189253574,-0.151238245600769,-0.151210230223545,
-0.151183080707512,-0.151156739847435,-0.151131155108219,-0.151106278201253,
-0.151082064444723,-0.151058472662611,-0.151035464570663,-0.151013004791237,
-0.15099106048062,-0.150969600899822,-0.15094859739742,-0.150928023288037,
-0.150907853609781,-0.150888064783097,-0.150868634772398,-0.150849542917034,
-0.150830769580642,-0.150812296239459,-0.150794105727963,-0.148405476337537,
-0.145516107341229,-0.140312282915775,-0.127769938121448,-0.0887285733398078,
-0.0769081481431902,-0.0721630279763587,-0.0688777371691399,-0.0655146546045517,
-0.0605407041033007,-0.0459070567405313,-0.000494226792898512),
 .UNSPECIFIED.);
#2909=B_SPLINE_CURVE_WITH_KNOTS('',3,(#125406,#125407,#125408,#125409,#125410,
#125411,#125412,#125413,#125414,#125415,#125416,#125417,#125418,#125419,
#125420,#125421,#125422,#125423,#125424,#125425),.UNSPECIFIED.,.F.,.F.,
(4,2,2,2,2,2,2,2,2,4),(-2.1000787529661,-2.09060473924815,-2.08821420497033,
-2.08642108497951,-2.08463972604253,-2.08253139390499,-2.0787589951723,
-2.0626905691525,-2.04262123048289,-2.04123955694236),.UNSPECIFIED.);
#2910=B_SPLINE_CURVE_WITH_KNOTS('',3,(#125426,#125427,#125428,#125429,#125430,
#125431,#125432,#125433,#125434,#125435,#125436,#125437,#125438,#125439,
#125440,#125441,#125442,#125443,#125444,#125445,#125446,#125447,#125448,
#125449,#125450,#125451,#125452,#125453,#125454,#125455,#125456,#125457,
#125458,#125459,#125460,#125461,#125462,#125463,#125464,#125465,#125466,
#125467,#125468,#125469,#125470,#125471,#125472,#125473,#125474,#125475,
#125476,#125477,#125478,#125479,#125480,#125481,#125482,#125483,#125484,
#125485,#125486,#125487,#125488,#125489,#125490,#125491,#125492,#125493,
#125494,#125495,#125496,#125497,#125498,#125499,#125500,#125501,#125502,
#125503,#125504,#125505,#125506,#125507,#125508,#125509,#125510,#125511,
#125512,#125513,#125514,#125515,#125516,#125517,#125518,#125519,#125520,
#125521,#125522,#125523,#125524,#125525,#125526,#125527,#125528,#125529,
#125530,#125531,#125532,#125533,#125534,#125535,#125536,#125537,#125538,
#125539,#125540,#125541,#125542,#125543,#125544,#125545,#125546,#125547,
#125548,#125549,#125550,#125551,#125552,#125553,#125554,#125555,#125556,
#125557,#125558,#125559,#125560,#125561,#125562,#125563,#125564,#125565,
#125566,#125567,#125568,#125569,#125570,#125571,#125572,#125573,#125574,
#125575,#125576,#125577,#125578,#125579,#125580,#125581,#125582,#125583,
#125584,#125585,#125586,#125587,#125588,#125589,#125590,#125591,#125592,
#125593,#125594,#125595,#125596,#125597,#125598,#125599,#125600,#125601,
#125602,#125603,#125604,#125605,#125606,#125607,#125608,#125609,#125610,
#125611,#125612,#125613,#125614,#125615,#125616,#125617,#125618,#125619,
#125620,#125621,#125622,#125623,#125624,#125625,#125626,#125627,#125628,
#125629,#125630,#125631,#125632,#125633,#125634,#125635,#125636,#125637,
#125638,#125639,#125640,#125641,#125642,#125643,#125644,#125645),
 .UNSPECIFIED.,.F.,.F.,(4,2,2,2,2,2,2,2,2,2,2,2,2,2,2,2,2,2,2,2,2,2,2,2,
2,2,2,2,2,2,2,2,2,2,2,2,2,2,2,2,2,2,2,2,2,2,2,2,2,2,2,2,2,2,2,2,2,2,2,2,
2,2,2,2,2,2,2,2,2,2,2,2,2,2,2,2,2,2,2,2,2,2,2,2,2,2,2,2,2,2,2,2,2,2,2,2,
2,2,2,2,2,2,2,2,2,2,2,2,2,4),(-1.75139041054252,-1.75091861351771,-1.74768903365539,
-1.74348611405865,-1.734288297127,-1.72151546056368,-1.69934690996806,-1.69521693622104,
-1.67306524734637,-1.6693728310676,-1.6672827294943,-1.6654620636133,-1.66299094271596,
-1.65718565731196,-1.64868078066227,-1.61856175284192,-1.5936894333588,
-1.58779123767793,-1.58423420864993,-1.58100433341346,-1.57680106832482,
-1.56760255385934,-1.55482850063813,-1.53266257892508,-1.52852906289671,
-1.50638597233275,-1.50269328624427,-1.50060292737515,-1.49878165248302,
-1.49630926403521,-1.49049946810993,-1.48198592353092,-1.45179427085578,
-1.4270350706234,-1.42114036468366,-1.41758367976233,-1.41435296711625,
-1.41014692835945,-1.400935022627,-1.38813634586288,-1.36597779158899,-1.36171313379183,
-1.33972985928813,-1.33603791052661,-1.33394781638972,-1.33212810489372,
-1.329658855026,-1.32385798305222,-1.31536049528632,-1.28529452616742,-1.26033939970604,
-1.25444094943778,-1.2508855535634,-1.24765837059915,-1.2434604365347,-1.23428196817663,
-1.22154383691827,-1.19936495812372,-1.19550325868213,-1.17303525131699,
-1.1693429767004,-1.16725358793298,-1.16543321972153,-1.16296278682649,
-1.15716253556433,-1.14866831284602,-1.11864155909669,-1.09364123173764,
-1.08773735497822,-1.08417820141472,-1.08094719174171,-1.07674354099047,
-1.06754836606575,-1.05478094569836,-1.03262375266717,-1.02855439687768,
-1.00635534843598,-1.00266080118208,-1.00056897439197,-0.99874388084189,
-0.996263713532163,-0.990427419550083,-0.981863473668625,-0.95124884871039,
-0.927137935427773,-0.921264584662462,-0.917709429289234,-0.914472655349134,
-0.91024776020222,-0.900946382214685,-0.887982719896956,-0.866023680170908,
-0.861479939346711,-0.839828679330764,-0.836138429701869,-0.834048805862784,
-0.832418535713938,-0.830078034263107,-0.82496898973213,-0.817808623856327,
-0.796421525510616,-0.762777552759297,-0.756143691609615,-0.752056100635309,
-0.748855657166228,-0.745270566959701,-0.739178575936893,-0.731757276806803,
-0.715584375973475,-0.701622587363262),.UNSPECIFIED.);
#2911=B_SPLINE_CURVE_WITH_KNOTS('',3,(#125648,#125649,#125650,#125651,#125652,
#125653,#125654,#125655,#125656,#125657,#125658,#125659,#125660,#125661,
#125662,#125663,#125664,#125665,#125666,#125667,#125668,#125669,#125670,
#125671,#125672,#125673,#125674,#125675,#125676,#125677,#125678,#125679,
#125680,#125681,#125682,#125683,#125684,#125685,#125686,#125687,#125688,
#125689,#125690,#125691,#125692,#125693,#125694,#125695,#125696,#125697,
#125698,#125699,#125700,#125701,#125702,#125703,#125704,#125705,#125706,
#125707,#125708,#125709,#125710,#125711,#125712,#125713,#125714,#125715,
#125716,#125717,#125718,#125719,#125720,#125721,#125722,#125723,#125724,
#125725,#125726,#125727,#125728,#125729,#125730,#125731,#125732,#125733,
#125734,#125735,#125736,#125737,#125738,#125739,#125740,#125741,#125742,
#125743,#125744,#125745,#125746,#125747,#125748,#125749,#125750,#125751,
#125752,#125753,#125754,#125755,#125756,#125757,#125758,#125759,#125760,
#125761,#125762,#125763,#125764,#125765,#125766,#125767,#125768,#125769,
#125770,#125771,#125772,#125773,#125774,#125775,#125776,#125777,#125778,
#125779,#125780,#125781,#125782,#125783,#125784,#125785,#125786,#125787,
#125788,#125789,#125790,#125791,#125792,#125793,#125794,#125795,#125796,
#125797,#125798,#125799,#125800,#125801,#125802,#125803,#125804,#125805,
#125806,#125807,#125808,#125809,#125810,#125811,#125812,#125813,#125814,
#125815,#125816,#125817,#125818,#125819,#125820,#125821,#125822,#125823,
#125824,#125825,#125826,#125827,#125828,#125829,#125830,#125831,#125832,
#125833,#125834,#125835,#125836,#125837,#125838,#125839,#125840,#125841),
 .UNSPECIFIED.,.F.,.F.,(4,2,2,2,2,2,2,2,2,2,2,2,2,2,2,2,2,2,2,2,2,2,2,2,
2,2,2,2,2,2,2,2,2,2,2,2,2,2,2,2,2,2,2,2,2,2,2,2,2,2,2,2,2,2,2,2,2,2,2,2,
2,2,2,2,2,2,2,2,2,2,2,2,2,2,2,2,2,2,2,2,2,2,2,2,2,2,2,2,2,2,2,2,2,2,2,2,
4),(-0.991241672647406,-0.987801969057869,-0.985787251833555,-0.983943844576314,
-0.98131941668712,-0.974536850515025,-0.931103314466294,-0.911783187657511,
-0.906192464811081,-0.902700439670065,-0.899449543974688,-0.895099050706998,
-0.885028019935898,-0.870532653808531,-0.850424789455911,-0.827053982341092,
-0.822131543385535,-0.819815705223421,-0.818008752444826,-0.815810639713148,
-0.811494104550115,-0.805775079343375,-0.791208931698783,-0.756591530319789,
-0.743737556131094,-0.738840178503933,-0.735826755702091,-0.732542311574434,
-0.727983146023538,-0.716555396200904,-0.699145320780396,-0.666205792614875,
-0.65712477184505,-0.654114006252745,-0.652384056219475,-0.650520149227365,
-0.647782007792058,-0.640185482990252,-0.62771022543606,-0.589215949700183,
-0.576908372559458,-0.572090036841543,-0.569090867154059,-0.565794660217369,
-0.56116750046865,-0.549263264734076,-0.530747045972717,-0.503549298549489,
-0.491149133524473,-0.487804077729745,-0.485811074377502,-0.483957262456012,
-0.48127350053131,-0.474075338245919,-0.462549890183645,-0.441694548303605,
-0.41269008695447,-0.406705223403245,-0.403130210426581,-0.399905387081769,
-0.395739020600716,-0.386747818274057,-0.362152876872644,-0.331764774982016,
-0.323623983186662,-0.3207320817232,-0.319024957349219,-0.317139807864442,
-0.314294952251012,-0.305859814869978,-0.291239717000893,-0.256429593668564,
-0.243779394345411,-0.238911013336089,-0.235902840794419,-0.232614223483765,
-0.228030711621876,-0.216434369678132,-0.198637853958558,-0.165082934194895,
-0.156979916535476,-0.154093190700569,-0.152387132188572,-0.150557471433941,
-0.148033041673921,-0.14494182417323,-0.139191493718343,-0.124495614464095,
-0.0894136332252241,-0.0770511115725383,-0.0722244674544098,-0.069223671106362,
-0.0659284937116466,-0.061308128069644,-0.0494535380316552,-0.0310548575729361,
-0.000494688380018427),.UNSPECIFIED.);
#2912=B_SPLINE_CURVE_WITH_KNOTS('',3,(#125842,#125843,#125844,#125845,#125846,
#125847,#125848,#125849,#125850,#125851,#125852,#125853,#125854,#125855,
#125856,#125857,#125858,#125859),.UNSPECIFIED.,.F.,.F.,(4,2,2,2,2,2,2,2,
4),(-2.1002328439837,-2.09075795692932,-2.08836800179074,-2.0865752450318,
-2.08479410976863,-2.0826860017187,-2.07891367771575,-2.06284869790601,
-2.04139270538101),.UNSPECIFIED.);
#2913=B_SPLINE_CURVE_WITH_KNOTS('',3,(#125860,#125861,#125862,#125863,#125864,
#125865,#125866,#125867,#125868,#125869,#125870,#125871,#125872,#125873,
#125874,#125875,#125876,#125877,#125878,#125879,#125880,#125881,#125882,
#125883,#125884,#125885,#125886,#125887,#125888,#125889,#125890,#125891,
#125892,#125893,#125894,#125895,#125896,#125897,#125898,#125899,#125900,
#125901,#125902,#125903,#125904,#125905,#125906,#125907,#125908,#125909,
#125910,#125911,#125912,#125913,#125914,#125915,#125916,#125917,#125918,
#125919,#125920,#125921,#125922,#125923,#125924,#125925,#125926,#125927,
#125928,#125929,#125930,#125931,#125932,#125933,#125934,#125935,#125936,
#125937,#125938,#125939,#125940,#125941,#125942,#125943,#125944,#125945,
#125946,#125947,#125948,#125949,#125950,#125951,#125952,#125953,#125954,
#125955,#125956,#125957,#125958,#125959,#125960,#125961,#125962,#125963,
#125964,#125965,#125966,#125967,#125968,#125969,#125970,#125971,#125972,
#125973,#125974,#125975,#125976,#125977,#125978,#125979,#125980,#125981,
#125982,#125983,#125984,#125985,#125986,#125987,#125988,#125989,#125990,
#125991,#125992,#125993,#125994,#125995,#125996,#125997,#125998,#125999,
#126000,#126001,#126002,#126003,#126004,#126005,#126006,#126007,#126008,
#126009,#126010,#126011,#126012,#126013,#126014,#126015,#126016,#126017,
#126018,#126019,#126020,#126021,#126022,#126023,#126024,#126025,#126026,
#126027,#126028,#126029,#126030,#126031,#126032,#126033,#126034,#126035,
#126036,#126037,#126038,#126039,#126040,#126041,#126042,#126043,#126044,
#126045,#126046,#126047,#126048,#126049,#126050,#126051,#126052,#126053,
#126054,#126055,#126056,#126057),.UNSPECIFIED.,.F.,.F.,(4,2,2,2,2,2,2,2,
2,2,2,2,2,2,2,2,2,2,2,2,2,2,2,2,2,2,2,2,2,2,2,2,2,2,2,2,2,2,2,2,2,2,2,2,
2,2,2,2,2,2,2,2,2,2,2,2,2,2,2,2,2,2,2,2,2,2,2,2,2,2,2,2,2,2,2,2,2,2,2,2,
2,2,2,2,2,2,2,2,2,2,2,2,2,2,2,2,2,2,4),(-1.10919012835353,-1.10913875417106,
-1.10593342114521,-1.10196645615564,-1.09578448318376,-1.0500864642212,
-1.03072304953975,-1.0270802212056,-1.02500150158327,-1.02317867498968,
-1.02068840394978,-1.01476547192955,-1.00602163637137,-0.981814942237135,
-0.951595900714783,-0.945614220704339,-0.942039871157921,-0.938814911385374,
-0.93464736987415,-0.925649751212604,-0.901338062431275,-0.871421105147256,
-0.862674342874921,-0.859704134962655,-0.85798190232104,-0.856110348158008,
-0.85333607858205,-0.845471552122435,-0.832335192846778,-0.788160082136583,
-0.780385814105817,-0.776394129439986,-0.773185836631225,-0.76950170701144,
-0.763001666553775,-0.730914529150247,-0.698881751937265,-0.694258618415944,
-0.692000232246089,-0.690196236265524,-0.687949721338137,-0.683381333738985,
-0.658877518901604,-0.619939582641716,-0.613655103108357,-0.609659392014902,
-0.606454040653568,-0.60278015979646,-0.59631710004486,-0.588317513035871,
-0.570121671574884,-0.543757980180209,-0.530156781362266,-0.52672900048763,
-0.524718769931408,-0.522874002160885,-0.520239705715888,-0.513387030987529,
-0.469825673898867,-0.450655181612665,-0.445075319115728,-0.441585726434461,
-0.438334197254077,-0.433978473811924,-0.423874383380412,-0.409310896292576,
-0.389308092099506,-0.365945659924148,-0.36108235132119,-0.358743999396581,
-0.356933054192068,-0.354745094212323,-0.350497797610437,-0.344901582146626,
-0.330842171519697,-0.2979484331142,-0.283332375685576,-0.278212655171611,
-0.275155343231835,-0.271892483482143,-0.267487649245627,-0.257101019259404,
-0.241966369841405,-0.211896127282767,-0.197129491172343,-0.193625802333691,
-0.191598252214357,-0.189770593270479,-0.187196905370401,-0.180675249612337,
-0.170656664963624,-0.122908095629107,-0.113977499342045,-0.109881990866413,
-0.106675228360909,-0.103137900339826,-0.0972603476961556,-0.0691137077990027,
-0.0593009426660634),.UNSPECIFIED.);
#2914=B_SPLINE_CURVE_WITH_KNOTS('',3,(#126060,#126061,#126062,#126063,#126064,
#126065,#126066,#126067,#126068,#126069,#126070,#126071,#126072,#126073,
#126074,#126075,#126076,#126077,#126078,#126079,#126080,#126081,#126082,
#126083,#126084,#126085,#126086,#126087,#126088,#126089,#126090,#126091,
#126092,#126093,#126094,#126095,#126096,#126097,#126098,#126099,#126100,
#126101,#126102,#126103,#126104,#126105,#126106,#126107,#126108,#126109,
#126110,#126111,#126112,#126113,#126114,#126115,#126116,#126117,#126118,
#126119,#126120,#126121,#126122,#126123,#126124,#126125,#126126,#126127,
#126128,#126129,#126130,#126131,#126132,#126133,#126134,#126135,#126136,
#126137,#126138,#126139,#126140,#126141,#126142,#126143,#126144,#126145,
#126146,#126147,#126148,#126149,#126150,#126151,#126152,#126153,#126154,
#126155,#126156,#126157,#126158,#126159,#126160,#126161,#126162,#126163,
#126164,#126165,#126166,#126167,#126168,#126169,#126170,#126171,#126172,
#126173,#126174,#126175,#126176,#126177,#126178,#126179,#126180,#126181,
#126182,#126183,#126184,#126185,#126186,#126187,#126188,#126189,#126190,
#126191,#126192,#126193,#126194,#126195,#126196,#126197,#126198,#126199,
#126200,#126201,#126202,#126203,#126204,#126205,#126206,#126207,#126208,
#126209,#126210,#126211,#126212,#126213,#126214,#126215,#126216,#126217,
#126218,#126219,#126220,#126221,#126222,#126223,#126224,#126225,#126226,
#126227,#126228,#126229,#126230,#126231,#126232,#126233,#126234,#126235,
#126236,#126237,#126238,#126239,#126240,#126241,#126242,#126243,#126244,
#126245,#126246,#126247),.UNSPECIFIED.,.F.,.F.,(4,2,2,2,2,2,2,2,2,2,2,2,
2,2,2,2,2,2,2,2,2,2,2,2,2,2,2,2,2,2,2,2,2,2,2,2,2,2,2,2,2,2,2,2,2,2,2,2,
2,2,2,2,2,2,2,2,2,2,2,2,2,2,2,2,2,2,2,2,2,2,2,2,2,2,2,2,2,2,2,2,2,2,2,2,
2,2,2,2,2,2,2,2,2,4),(-0.991403523612787,-0.987963642821703,-0.985948822364639,
-0.984105321973104,-0.981480764294791,-0.974697879765066,-0.931262196775588,
-0.911940967777414,-0.906349950602837,-0.902857745100171,-0.899606683850455,
-0.895255972618923,-0.885184454504479,-0.870688403025017,-0.850579423167714,
-0.827207420967211,-0.822344972442386,-0.820007291415794,-0.818199058221792,
-0.816018537885941,-0.811789534988751,-0.787448795578598,-0.747669641655126,
-0.741481014250267,-0.737511615470875,-0.734305398334489,-0.730606174008498,
-0.724031722976422,-0.68939917349318,-0.660331441517993,-0.655535125391971,
-0.653243639221105,-0.651438286732821,-0.649220721612908,-0.644805316034479,
-0.638913490495356,-0.623626330875805,-0.586388315789502,-0.576234872873496,
-0.572192897897606,-0.569194552209554,-0.565897428171752,-0.561265503200992,
-0.54932785567536,-0.530732586900761,-0.503337572388864,-0.491214431464943,
-0.487891523741086,-0.485903328305085,-0.484046987026729,-0.48134957160757,
-0.474053624903393,-0.46229902588501,-0.440810893855001,-0.412772996888117,
-0.406800605632133,-0.403228189056408,-0.400002682827013,-0.395831152665152,
-0.386811070180518,-0.374374706742553,-0.327302348459393,-0.322323206557624,
-0.319997287952923,-0.31819018476347,-0.316001311014742,-0.311730357115074,
-0.283243699264422,-0.248428409195011,-0.241840072325533,-0.237754078483996,
-0.23453812620516,-0.230917498814929,-0.224717376189783,-0.217136823783367,
-0.200448139197663,-0.168523618213428,-0.15765772047135,-0.154454553250421,
-0.152492343536114,-0.150677171307585,-0.148216037619876,-0.145218916596553,
-0.139725312086273,-0.126066129584397,-0.0814235618930086,-0.0750182323098244,
-0.0709854884195602,-0.0677747342105745,-0.0641207645063932,-0.0577615849681248,
-0.0499291798106559,-0.0323468223698187,-0.000494690693803759),
 .UNSPECIFIED.);
#2915=B_SPLINE_CURVE_WITH_KNOTS('',3,(#126248,#126249,#126250,#126251,#126252,
#126253,#126254,#126255,#126256,#126257,#126258,#126259,#126260,#126261,
#126262,#126263,#126264,#126265),.UNSPECIFIED.,.F.,.F.,(4,2,2,2,2,2,2,2,
4),(-2.10007532875945,-2.0906014191503,-2.08821171307978,-2.08641914292706,
-2.08463819261998,-2.08253030334906,-2.07875836979288,-2.06269506268221,
-2.0412420799731),.UNSPECIFIED.);
#2916=B_SPLINE_CURVE_WITH_KNOTS('',3,(#126266,#126267,#126268,#126269,#126270,
#126271,#126272,#126273,#126274,#126275,#126276,#126277,#126278,#126279,
#126280,#126281,#126282,#126283,#126284,#126285,#126286,#126287,#126288,
#126289,#126290,#126291,#126292,#126293,#126294,#126295,#126296,#126297,
#126298,#126299,#126300,#126301,#126302,#126303,#126304,#126305,#126306,
#126307,#126308,#126309,#126310,#126311,#126312,#126313,#126314,#126315,
#126316,#126317,#126318,#126319,#126320,#126321,#126322,#126323,#126324,
#126325,#126326,#126327,#126328,#126329,#126330,#126331,#126332,#126333,
#126334,#126335,#126336,#126337,#126338,#126339,#126340,#126341,#126342,
#126343,#126344,#126345,#126346,#126347,#126348,#126349,#126350,#126351,
#126352,#126353,#126354,#126355,#126356,#126357,#126358,#126359,#126360,
#126361,#126362,#126363,#126364,#126365,#126366,#126367,#126368,#126369,
#126370,#126371,#126372,#126373,#126374,#126375,#126376,#126377,#126378,
#126379,#126380,#126381,#126382,#126383,#126384,#126385,#126386,#126387,
#126388,#126389,#126390,#126391,#126392,#126393,#126394,#126395,#126396,
#126397,#126398,#126399,#126400,#126401,#126402,#126403,#126404,#126405,
#126406,#126407,#126408,#126409,#126410,#126411,#126412,#126413,#126414,
#126415,#126416,#126417,#126418,#126419,#126420,#126421,#126422,#126423,
#126424,#126425,#126426,#126427,#126428,#126429,#126430,#126431,#126432,
#126433,#126434,#126435,#126436,#126437,#126438,#126439,#126440,#126441,
#126442,#126443,#126444,#126445,#126446,#126447,#126448,#126449,#126450,
#126451,#126452,#126453,#126454,#126455,#126456,#126457,#126458,#126459),
 .UNSPECIFIED.,.F.,.F.,(4,2,2,2,2,2,2,2,2,2,2,2,2,2,2,2,2,2,2,2,2,2,2,2,
2,2,2,2,2,2,2,2,2,2,2,2,2,2,2,2,2,2,2,2,2,2,2,2,2,2,2,2,2,2,2,2,2,2,2,2,
2,2,2,2,2,2,2,2,2,2,2,2,2,2,2,2,2,2,2,2,2,2,2,2,2,2,2,2,2,2,2,2,2,2,2,2,
4),(-1.10915669663231,-1.10910532171049,-1.10590022347286,-1.10193354852953,
-1.09575202659879,-1.05005733740566,-1.03069533293189,-1.02705277091948,
-1.02497420345805,-1.02315151048225,-1.02066142234617,-1.01473892716117,
-1.00599573860429,-0.981790799667696,-0.951573944185358,-0.945592701348895,
-0.942018613321529,-0.938793889716136,-0.934626653734317,-0.925629696316969,
-0.901319497113162,-0.871404258772762,-0.862658720247753,-0.859688802304535,
-0.857966709744681,-0.856095279788858,-0.853321149648226,-0.845456710341012,
-0.832320086986627,-0.788136837005273,-0.780371288386305,-0.776381555805368,
-0.773173617037327,-0.769488561997317,-0.762983280400771,-0.754918204531033,
-0.736487450828257,-0.709514301513081,-0.696783567833986,-0.693413309283975,
-0.691414733393968,-0.689565230657145,-0.686899534787704,-0.679818508622548,
-0.668562553195977,-0.6473706194628,-0.618227667962999,-0.612245495167454,
-0.608673157429048,-0.605451537953733,-0.601290572072463,-0.59231714259212,
-0.566855992752182,-0.534969172607089,-0.528571081335433,-0.525936210195109,
-0.524110051136577,-0.522105620554195,-0.518708344248468,-0.503891324519974,
-0.456498464670831,-0.447464401826884,-0.443334614889865,-0.440105146715298,
-0.436546315642099,-0.430639634673135,-0.402327357768225,-0.374202936201015,
-0.363100614784437,-0.359874221289477,-0.357905864330772,-0.356031190392509,
-0.353257075600444,-0.345425355063952,-0.332373552100607,-0.288782401483648,
-0.280604428910652,-0.276582820453261,-0.273368099744482,-0.269695511161125,
-0.263265941294114,-0.232755830952575,-0.19928539238687,-0.194466407168421,
-0.192170852235826,-0.190371466264548,-0.18817642497511,-0.183824932519784,
-0.156777231243627,-0.120224568449024,-0.113721030701917,-0.109673133659428,
-0.106479523132496,-0.102876701450989,-0.0966903149974414,-0.0631983996702185,
-0.0592977063510342),.UNSPECIFIED.);
#2917=B_SPLINE_CURVE_WITH_KNOTS('',3,(#126462,#126463,#126464,#126465,#126466,
#126467,#126468,#126469,#126470,#126471,#126472,#126473,#126474,#126475,
#126476,#126477,#126478,#126479,#126480,#126481,#126482,#126483,#126484,
#126485,#126486,#126487,#126488,#126489,#126490,#126491,#126492,#126493,
#126494,#126495,#126496,#126497,#126498,#126499,#126500,#126501,#126502,
#126503,#126504,#126505,#126506,#126507,#126508,#126509,#126510,#126511,
#126512,#126513,#126514,#126515,#126516,#126517,#126518,#126519,#126520,
#126521,#126522,#126523,#126524,#126525,#126526,#126527,#126528,#126529,
#126530,#126531,#126532,#126533,#126534,#126535,#126536,#126537,#126538,
#126539,#126540,#126541,#126542,#126543,#126544,#126545,#126546,#126547,
#126548,#126549,#126550,#126551,#126552,#126553,#126554,#126555,#126556,
#126557,#126558,#126559,#126560,#126561,#126562,#126563,#126564,#126565,
#126566,#126567,#126568,#126569,#126570,#126571,#126572,#126573,#126574,
#126575,#126576,#126577,#126578,#126579,#126580,#126581,#126582),
 .UNSPECIFIED.,.F.,.F.,(4,3,3,3,3,3,3,3,3,3,3,3,3,3,3,3,3,3,3,3,3,3,3,3,
3,3,3,3,3,3,3,3,3,3,3,3,3,3,3,3,4),(17.9343865285971,18.0384572998024,18.1423979804763,
18.2462679090633,18.3501018475111,18.4539345090056,18.5578725321006,18.6618645536724,
18.7660437678494,18.8444150126792,18.9485886091815,19.0526067743066,19.1565026798016,
19.2603329942975,19.3641325164526,19.4679360013634,19.5718481070875,19.6758190055391,
19.7799719118523,19.8419628710253,19.9461515595277,20.0501850219937,20.1540964551946,
20.2579424311235,20.3617577250111,20.4655770686522,20.5695050565948,20.6734918745117,
20.7776605862359,20.8395107293714,20.9436986058482,21.0477312846702,21.1516419806614,
21.2554872485236,21.3593018646391,21.4631205619848,21.5670479566075,21.6710342102137,
21.7752024100578,21.8370585877175,21.9911485751285),.UNSPECIFIED.);
#2918=B_SPLINE_CURVE_WITH_KNOTS('',3,(#126583,#126584,#126585,#126586,#126587,
#126588,#126589,#126590,#126591,#126592,#126593,#126594,#126595,#126596,
#126597,#126598,#126599,#126600,#126601,#126602,#126603,#126604,#126605,
#126606,#126607,#126608,#126609,#126610,#126611,#126612,#126613,#126614,
#126615,#126616,#126617,#126618,#126619,#126620,#126621,#126622,#126623,
#126624,#126625,#126626,#126627,#126628,#126629,#126630,#126631,#126632,
#126633,#126634,#126635,#126636,#126637,#126638,#126639,#126640,#126641,
#126642,#126643,#126644,#126645,#126646,#126647,#126648,#126649,#126650,
#126651,#126652),.UNSPECIFIED.,.F.,.F.,(4,3,3,3,3,3,3,3,3,3,3,3,3,3,3,3,
3,3,3,3,3,3,3,4),(21.9911485755009,22.0965808093213,22.1989692644131,22.3012912063502,
22.4035832768669,22.505882070425,22.6082867494055,22.7107561649705,22.8133906742477,
22.8346064460636,22.9387930131769,23.0428243453621,23.1467336457121,23.2505774884119,
23.3543906519354,23.4582078713222,23.5621337592291,23.666118487615,23.7702851493394,
23.8321543044097,23.9363111118011,24.0403323654621,24.1442397578549,24.2175053922168),
 .UNSPECIFIED.);
#2919=B_SPLINE_CURVE_WITH_KNOTS('',3,(#126654,#126655,#126656,#126657,#126658,
#126659,#126660,#126661,#126662,#126663,#126664,#126665,#126666,#126667,
#126668,#126669,#126670,#126671,#126672,#126673,#126674,#126675,#126676,
#126677,#126678,#126679,#126680,#126681,#126682,#126683,#126684,#126685,
#126686,#126687,#126688,#126689,#126690,#126691,#126692,#126693,#126694,
#126695,#126696,#126697,#126698,#126699,#126700,#126701,#126702,#126703,
#126704,#126705,#126706,#126707,#126708,#126709,#126710,#126711,#126712,
#126713,#126714,#126715,#126716,#126717,#126718,#126719,#126720),
 .UNSPECIFIED.,.F.,.F.,(4,3,3,3,3,3,3,3,3,3,3,3,3,3,3,3,3,3,3,3,3,3,4),
(21.9911485755661,22.1068555809328,22.2230357332073,22.3398118814748,22.3785238795456,
22.4827125615403,22.5867460174313,22.6906574439895,22.7945034132374,22.8983187004159,
23.0021380373295,23.1060660185635,23.2100528297722,23.3142215348618,23.3760717378917,
23.4811392289653,23.5851517657021,23.6890597620316,23.7928980829185,23.8988264788089,
24.0026675510491,24.1096396087646,24.2166116664802),.UNSPECIFIED.);
#2920=B_SPLINE_CURVE_WITH_KNOTS('',3,(#126721,#126722,#126723,#126724,#126725,
#126726,#126727,#126728,#126729,#126730,#126731,#126732,#126733,#126734,
#126735,#126736,#126737,#126738,#126739,#126740,#126741,#126742,#126743,
#126744,#126745,#126746,#126747,#126748,#126749,#126750,#126751,#126752,
#126753,#126754,#126755,#126756,#126757,#126758,#126759,#126760,#126761,
#126762,#126763,#126764,#126765,#126766,#126767,#126768,#126769,#126770,
#126771,#126772,#126773,#126774,#126775,#126776,#126777,#126778,#126779,
#126780,#126781,#126782,#126783,#126784,#126785,#126786,#126787,#126788,
#126789,#126790,#126791,#126792,#126793,#126794,#126795,#126796,#126797,
#126798,#126799,#126800,#126801,#126802,#126803,#126804,#126805,#126806,
#126807,#126808,#126809,#126810,#126811,#126812,#126813,#126814,#126815,
#126816,#126817,#126818,#126819,#126820,#126821,#126822,#126823,#126824,
#126825,#126826,#126827,#126828,#126829,#126830,#126831,#126832,#126833,
#126834,#126835,#126836,#126837,#126838,#126839,#126840,#126841,#126842,
#126843,#126844),.UNSPECIFIED.,.F.,.F.,(4,3,3,3,3,3,3,3,3,3,3,3,3,3,3,3,
3,3,3,3,3,3,3,3,3,3,3,3,3,3,3,3,3,3,3,3,3,3,3,3,3,4),(17.9338039591658,
18.0378065512601,18.1419241164839,18.2461084709875,18.3504680705561,18.3883324461612,
18.4924181653028,18.5963471946834,18.7001525240931,18.8038914206691,18.9075988173882,
19.0113096028515,19.1151287668075,19.2190064442924,19.3230666994159,19.3858803045073,
19.4900800737608,19.5941245745256,19.6980469267599,19.8019037417006,19.905729777854,
20.0095597501986,20.1134981178355,20.2174951904896,20.3216738458828,20.3834281628534,
20.4876315786543,20.591680131366,20.6956071218429,20.7994689350635,20.9033003228197,
21.0071359937425,21.1110805544,21.2150841085133,21.3192696347798,21.3809760211995,
21.4863458581892,21.5915494442598,21.6965991972893,21.8015577704351,21.9064689038258,
21.9911485751285),.UNSPECIFIED.);
#2921=B_SPLINE_CURVE_WITH_KNOTS('',3,(#126847,#126848,#126849,#126850,#126851,
#126852,#126853,#126854,#126855,#126856,#126857,#126858,#126859,#126860,
#126861,#126862,#126863,#126864,#126865,#126866,#126867,#126868,#126869,
#126870,#126871,#126872,#126873,#126874,#126875,#126876,#126877,#126878,
#126879,#126880,#126881,#126882,#126883,#126884,#126885,#126886,#126887,
#126888,#126889,#126890,#126891,#126892,#126893,#126894,#126895,#126896,
#126897,#126898,#126899,#126900,#126901,#126902,#126903,#126904,#126905,
#126906,#126907,#126908,#126909,#126910,#126911,#126912,#126913,#126914,
#126915,#126916,#126917,#126918,#126919,#126920,#126921,#126922,#126923,
#126924,#126925,#126926,#126927,#126928,#126929,#126930,#126931,#126932,
#126933,#126934,#126935,#126936,#126937,#126938,#126939,#126940,#126941,
#126942,#126943,#126944,#126945,#126946,#126947,#126948,#126949,#126950,
#126951,#126952,#126953,#126954,#126955,#126956,#126957,#126958,#126959,
#126960,#126961,#126962,#126963,#126964,#126965,#126966,#126967),
 .UNSPECIFIED.,.F.,.F.,(4,3,3,3,3,3,3,3,3,3,3,3,3,3,3,3,3,3,3,3,3,3,3,3,
3,3,3,3,3,3,3,3,3,3,3,3,3,3,3,3,4),(17.9343865323097,18.0384573059669,18.1423979891803,
18.2462679203589,18.350101861447,18.4539345256267,18.5578725514576,18.6618645757981,
18.7660437927651,18.8444150126793,18.9485886051143,19.0526067661076,19.156502667395,
19.2603329776386,19.3641324955029,19.4679359760908,19.5718480774722,19.6758189715633,
19.779971873535,19.8419628710253,19.9461515610579,20.0501850250699,20.1540964598329,
20.2579424373327,20.3617577327979,20.4655770780209,20.5695050675409,20.6734918870352,
20.7776606003195,20.8395107293714,20.9436986062052,21.0477312853947,21.1516419817676,
21.2554872500202,21.359301866534,21.4631205642854,21.5670479593226,21.6710342133488,
21.7752024136171,21.8370585877175,21.9911485751285),.UNSPECIFIED.);
#2922=B_SPLINE_CURVE_WITH_KNOTS('',3,(#126968,#126969,#126970,#126971,#126972,
#126973,#126974,#126975,#126976,#126977,#126978,#126979,#126980,#126981,
#126982,#126983,#126984,#126985,#126986,#126987,#126988,#126989,#126990,
#126991,#126992,#126993,#126994,#126995,#126996,#126997,#126998,#126999,
#127000,#127001,#127002,#127003,#127004,#127005,#127006,#127007,#127008,
#127009,#127010,#127011,#127012,#127013,#127014,#127015,#127016,#127017,
#127018,#127019,#127020,#127021,#127022,#127023,#127024,#127025,#127026,
#127027,#127028,#127029,#127030,#127031,#127032,#127033,#127034,#127035,
#127036,#127037),.UNSPECIFIED.,.F.,.F.,(4,3,3,3,3,3,3,3,3,3,3,3,3,3,3,3,
3,3,3,3,3,3,3,4),(21.9911485755009,22.0965808093213,22.1989692637443,22.3012912050081,
22.4035832748472,22.5058820677243,22.6082867460218,22.7107561609016,22.8133906694953,
22.8346064460636,22.9387930134359,23.042824345883,23.1467336464979,23.250577489464,
23.3543906532553,23.4582078729108,23.5621337610859,23.66611848974,23.77028515173,
23.8321543044097,23.9363111118405,24.0403323655425,24.1442397579785,24.2175053970322),
 .UNSPECIFIED.);
#2923=B_SPLINE_CURVE_WITH_KNOTS('',3,(#127039,#127040,#127041,#127042,#127043,
#127044,#127045,#127046,#127047,#127048,#127049,#127050,#127051,#127052,
#127053,#127054,#127055,#127056,#127057,#127058,#127059,#127060,#127061,
#127062,#127063,#127064,#127065,#127066,#127067,#127068,#127069,#127070,
#127071,#127072,#127073,#127074,#127075,#127076,#127077,#127078,#127079,
#127080,#127081,#127082,#127083,#127084,#127085,#127086,#127087,#127088,
#127089,#127090,#127091,#127092,#127093,#127094,#127095,#127096,#127097,
#127098,#127099,#127100,#127101,#127102,#127103,#127104,#127105),
 .UNSPECIFIED.,.F.,.F.,(4,3,3,3,3,3,3,3,3,3,3,3,3,3,3,3,3,3,3,3,3,3,4),
(21.9911485755662,22.1068555730249,22.2230357171705,22.3398118572522,22.3785238795456,
22.4827125635847,22.5867460215413,22.6906574501864,22.7945034215332,22.8983187108193,
23.0021380498465,23.1060660331879,23.210052846504,23.3142215536779,23.3760717378917,
23.4811392295967,23.5851517668296,23.6890597636676,23.7928980850748,23.898826481689,
24.0026675544749,24.1096396130032,24.2166116715314),.UNSPECIFIED.);
#2924=B_SPLINE_CURVE_WITH_KNOTS('',3,(#127106,#127107,#127108,#127109,#127110,
#127111,#127112,#127113,#127114,#127115,#127116,#127117,#127118,#127119,
#127120,#127121,#127122,#127123,#127124,#127125,#127126,#127127,#127128,
#127129,#127130,#127131,#127132,#127133,#127134,#127135,#127136,#127137,
#127138,#127139,#127140,#127141,#127142,#127143,#127144,#127145,#127146,
#127147,#127148,#127149,#127150,#127151,#127152,#127153,#127154,#127155,
#127156,#127157,#127158,#127159,#127160,#127161,#127162,#127163,#127164,
#127165,#127166,#127167,#127168,#127169,#127170,#127171,#127172,#127173,
#127174,#127175,#127176,#127177,#127178,#127179,#127180,#127181,#127182,
#127183,#127184,#127185,#127186,#127187,#127188,#127189,#127190,#127191,
#127192,#127193,#127194,#127195,#127196,#127197,#127198,#127199,#127200,
#127201,#127202,#127203,#127204,#127205,#127206,#127207,#127208,#127209,
#127210,#127211,#127212,#127213,#127214,#127215,#127216,#127217,#127218,
#127219,#127220,#127221,#127222,#127223,#127224,#127225,#127226,#127227,
#127228,#127229),.UNSPECIFIED.,.F.,.F.,(4,3,3,3,3,3,3,3,3,3,3,3,3,3,3,3,
3,3,3,3,3,3,3,3,3,3,3,3,3,3,3,3,3,3,3,3,3,3,3,3,3,4),(17.9338039635375,
18.0378065699095,18.141924149687,18.2461085189123,18.3504681333591,18.3883324461612,
18.4924181349029,18.5963471334187,18.7001524314161,18.8038912962574,18.907598660964,
19.0113094141818,19.115128545753,19.2190061907243,19.3230664134798,19.3858803045073,
19.4900800856805,19.5941245984907,19.6980469628977,19.8019037900831,19.9057298385346,
20.0095598232127,20.1134982031513,20.2174952881079,20.3216739556707,20.3834281628534,
20.4876315818645,20.5916801378724,20.6956071317597,20.7994689484591,20.9033003397573,
21.0071360142814,21.1110805786052,21.2150841364274,21.3192696664305,21.3809760211995,
21.4863458526797,21.5915494331531,21.6965991804852,21.8015577478801,21.9064688754743,
21.9911485751285),.UNSPECIFIED.);
#2925=B_SPLINE_CURVE_WITH_KNOTS('',3,(#127232,#127233,#127234,#127235,#127236,
#127237,#127238,#127239,#127240,#127241,#127242,#127243,#127244,#127245,
#127246,#127247,#127248,#127249,#127250,#127251,#127252,#127253,#127254,
#127255,#127256,#127257,#127258,#127259,#127260,#127261,#127262,#127263,
#127264,#127265,#127266,#127267,#127268,#127269,#127270,#127271,#127272,
#127273,#127274,#127275,#127276,#127277,#127278,#127279,#127280,#127281,
#127282,#127283,#127284,#127285,#127286,#127287,#127288,#127289,#127290,
#127291,#127292,#127293,#127294,#127295,#127296,#127297,#127298,#127299,
#127300,#127301,#127302,#127303,#127304,#127305,#127306,#127307,#127308,
#127309,#127310,#127311,#127312,#127313,#127314,#127315,#127316,#127317,
#127318,#127319,#127320,#127321,#127322,#127323,#127324,#127325,#127326,
#127327,#127328,#127329,#127330,#127331,#127332,#127333,#127334,#127335,
#127336,#127337,#127338,#127339,#127340,#127341,#127342,#127343,#127344,
#127345,#127346,#127347,#127348,#127349,#127350,#127351,#127352),
 .UNSPECIFIED.,.F.,.F.,(4,3,3,3,3,3,3,3,3,3,3,3,3,3,3,3,3,3,3,3,3,3,3,3,
3,3,3,3,3,3,3,3,3,3,3,3,3,3,3,3,4),(17.9343900068785,18.0384621797793,18.1424043135119,
18.2462757259662,18.3501111769658,18.4539453776036,18.5578849698345,18.6618785800864,
18.766059395221,18.8444150126793,18.9485861780031,19.0526018736708,19.1564952646259,
19.2603230380769,19.3641199963983,19.4679208983768,19.5718304095614,19.6757987029868,
19.7799490157806,19.8419628710253,19.9461525033199,20.0501869193504,20.1540993159731,
20.2579462608792,20.361762527852,20.4655828472436,20.5695118082714,20.6734995992369,
20.7776692733765,20.8395107293714,20.9436988123426,21.0477317039952,21.1516426212559,
21.2554881154862,21.3593029627459,21.4631218956947,21.5670495311687,21.6710360289524,
21.7752044756406,21.8370585877175,21.9911485751285),.UNSPECIFIED.);
#2926=B_SPLINE_CURVE_WITH_KNOTS('',3,(#127353,#127354,#127355,#127356,#127357,
#127358,#127359,#127360,#127361,#127362,#127363,#127364,#127365,#127366,
#127367,#127368,#127369,#127370,#127371,#127372,#127373,#127374,#127375,
#127376,#127377,#127378,#127379,#127380,#127381,#127382,#127383,#127384,
#127385,#127386,#127387,#127388,#127389,#127390,#127391,#127392,#127393,
#127394,#127395,#127396,#127397,#127398,#127399,#127400,#127401,#127402,
#127403,#127404,#127405,#127406,#127407,#127408,#127409,#127410,#127411,
#127412,#127413,#127414,#127415,#127416,#127417,#127418,#127419,#127420,
#127421,#127422),.UNSPECIFIED.,.F.,.F.,(4,3,3,3,3,3,3,3,3,3,3,3,3,3,3,3,
3,3,3,3,3,3,3,4),(21.9911485754958,22.0965808093167,22.1989688491809,22.301290373003,
22.4035820228761,22.5058803936157,22.6082846484721,22.7107536385604,22.8133877234273,
22.8346064460636,22.9387931787213,23.0428246782763,23.1467341478916,23.2505781609339,
23.3543914956235,23.4582088867465,23.5621349460763,23.6661198459672,23.7702866774631,
23.8321543044097,23.9363111340917,24.0403324108138,24.1442398280771,24.2175094731414),
 .UNSPECIFIED.);
#2927=B_SPLINE_CURVE_WITH_KNOTS('',3,(#127424,#127425,#127426,#127427,#127428,
#127429,#127430,#127431,#127432,#127433,#127434,#127435,#127436,#127437,
#127438,#127439,#127440,#127441,#127442,#127443,#127444,#127445,#127446,
#127447,#127448,#127449,#127450,#127451,#127452,#127453,#127454,#127455,
#127456,#127457,#127458,#127459,#127460,#127461,#127462,#127463,#127464,
#127465,#127466,#127467,#127468,#127469,#127470,#127471,#127472,#127473,
#127474,#127475,#127476,#127477,#127478,#127479,#127480,#127481,#127482,
#127483,#127484,#127485,#127486,#127487,#127488,#127489,#127490),
 .UNSPECIFIED.,.F.,.F.,(4,3,3,3,3,3,3,3,3,3,3,3,3,3,3,3,3,3,3,3,3,3,4),
(21.99114857557,22.1068519865695,22.2230284424145,22.3398008663504,22.3785238795456,
22.4827135010409,22.5867479061601,22.6906602917587,22.7945072255769,22.8983234814147,
23.0021437896405,23.1060727395329,23.2100605193632,23.3142301824888,23.3760717378917,
23.4811397540393,23.5851525044163,23.6890607200774,23.7928992656579,23.8988284160114,
24.0026697250665,24.1096427960693,24.2166158670722),.UNSPECIFIED.);
#2928=B_SPLINE_CURVE_WITH_KNOTS('',3,(#127491,#127492,#127493,#127494,#127495,
#127496,#127497,#127498,#127499,#127500,#127501,#127502,#127503,#127504,
#127505,#127506,#127507,#127508,#127509,#127510,#127511,#127512,#127513,
#127514,#127515,#127516,#127517,#127518,#127519,#127520,#127521,#127522,
#127523,#127524,#127525,#127526,#127527,#127528,#127529,#127530,#127531,
#127532,#127533,#127534,#127535,#127536,#127537,#127538,#127539,#127540,
#127541,#127542,#127543,#127544,#127545,#127546,#127547,#127548,#127549,
#127550,#127551,#127552,#127553,#127554,#127555,#127556,#127557,#127558,
#127559,#127560,#127561,#127562,#127563,#127564,#127565,#127566,#127567,
#127568,#127569,#127570,#127571,#127572,#127573,#127574,#127575,#127576,
#127577,#127578,#127579,#127580,#127581,#127582,#127583,#127584,#127585,
#127586,#127587,#127588,#127589,#127590,#127591,#127592,#127593,#127594,
#127595,#127596,#127597,#127598,#127599,#127600,#127601,#127602,#127603,
#127604,#127605,#127606,#127607,#127608,#127609,#127610,#127611,#127612,
#127613,#127614),.UNSPECIFIED.,.F.,.F.,(4,3,3,3,3,3,3,3,3,3,3,3,3,3,3,3,
3,3,3,3,3,3,3,3,3,3,3,3,3,3,3,3,3,3,3,3,3,3,3,3,3,4),(17.9338080230641,
18.037816525777,18.1419401180095,18.2461305705873,18.3504963338971,18.3883324461612,
18.4924050953013,18.5963208567489,18.7001126857905,18.803837945059,18.9075315867694,
19.0112285186248,19.1150337711737,19.2188974829894,19.3229438367761,19.3858803045073,
19.4900853238861,19.5941351297246,19.6980628426444,19.801925049615,19.9057565010466,
20.0095919038493,20.1135356875764,20.2175381763388,20.3217221890141,20.3834281628534,
20.4876329473777,20.5916829062076,20.6956113519136,20.799474649947,20.9033075499886,
21.0071447585888,21.1110908855051,21.2150960243741,21.3192831478159,21.3809760211995,
21.4863434371408,21.5915445630699,21.6965918110537,21.8015478551884,21.9064564387841,
21.9911485751285),.UNSPECIFIED.);
#2929=B_SPLINE_CURVE_WITH_KNOTS('',3,(#127617,#127618,#127619,#127620,#127621,
#127622,#127623,#127624,#127625,#127626,#127627,#127628,#127629,#127630,
#127631,#127632,#127633,#127634,#127635,#127636,#127637,#127638,#127639,
#127640,#127641,#127642,#127643,#127644,#127645,#127646,#127647,#127648,
#127649,#127650,#127651,#127652,#127653,#127654,#127655,#127656,#127657,
#127658,#127659,#127660,#127661,#127662,#127663,#127664,#127665,#127666,
#127667,#127668,#127669,#127670,#127671,#127672,#127673,#127674,#127675,
#127676,#127677,#127678,#127679,#127680,#127681,#127682,#127683,#127684,
#127685,#127686,#127687,#127688,#127689,#127690,#127691,#127692,#127693,
#127694,#127695,#127696,#127697,#127698,#127699,#127700,#127701,#127702,
#127703,#127704,#127705,#127706,#127707,#127708,#127709,#127710,#127711,
#127712,#127713,#127714,#127715,#127716,#127717,#127718,#127719,#127720,
#127721,#127722,#127723,#127724,#127725,#127726,#127727,#127728,#127729,
#127730,#127731,#127732,#127733,#127734,#127735,#127736,#127737),
 .UNSPECIFIED.,.F.,.F.,(4,3,3,3,3,3,3,3,3,3,3,3,3,3,3,3,3,3,3,3,3,3,3,3,
3,3,3,3,3,3,3,3,3,3,3,3,3,3,3,3,4),(17.9343899947098,18.0384621637907,18.1424042935601,
18.2462757019651,18.3501111488352,18.4539453452689,18.5578849332116,18.6618785391202,
18.7660593498775,18.8444150126793,18.9485861849099,19.0526018875928,19.1564952856901,
19.2603230663583,19.3641200319611,19.4679209412748,19.5718304598269,19.6757987606494,
19.779949080807,19.8419628710254,19.9461525005616,20.050186913805,20.1540993076118,
20.2579462496858,20.3617625138143,20.4655828303539,20.5695117885374,20.6734995766586,
20.7776692479848,20.8395107293714,20.9436988117741,21.0477317028403,21.1516426194906,
21.2554881130961,21.3593029597174,21.4631218920152,21.567049526823,21.6710360239309,
21.7752044699356,21.8370585877175,21.9911485751285),.UNSPECIFIED.);
#2930=B_SPLINE_CURVE_WITH_KNOTS('',3,(#127738,#127739,#127740,#127741,#127742,
#127743,#127744,#127745,#127746,#127747,#127748,#127749,#127750,#127751,
#127752,#127753,#127754,#127755,#127756,#127757,#127758,#127759,#127760,
#127761,#127762,#127763,#127764,#127765,#127766,#127767,#127768,#127769,
#127770,#127771,#127772,#127773,#127774,#127775,#127776,#127777,#127778,
#127779,#127780,#127781,#127782,#127783,#127784,#127785,#127786,#127787,
#127788,#127789,#127790,#127791,#127792,#127793,#127794,#127795,#127796,
#127797,#127798,#127799,#127800,#127801,#127802,#127803,#127804,#127805,
#127806,#127807),.UNSPECIFIED.,.F.,.F.,(4,3,3,3,3,3,3,3,3,3,3,3,3,3,3,3,
3,3,3,3,3,3,3,4),(21.9911485754958,22.0965808093167,22.1989688504026,22.3012903754547,
22.4035820265653,22.5058803985488,22.6082846546529,22.7107536459929,22.8133877321084,
22.8346064460636,22.9387931782215,23.0428246772713,23.1467341463756,23.2505781589037,
23.3543914930764,23.458208883681,23.5621349424933,23.6661198418661,23.7702866728494,
23.8321543044097,23.9363111340315,24.0403324106909,24.1442398278863,24.2175094594017),
 .UNSPECIFIED.);
#2931=B_SPLINE_CURVE_WITH_KNOTS('',3,(#127809,#127810,#127811,#127812,#127813,
#127814,#127815,#127816,#127817,#127818,#127819,#127820,#127821,#127822,
#127823,#127824,#127825,#127826,#127827,#127828,#127829,#127830,#127831,
#127832,#127833,#127834,#127835,#127836,#127837,#127838,#127839,#127840,
#127841,#127842,#127843,#127844,#127845,#127846,#127847,#127848,#127849,
#127850,#127851,#127852,#127853,#127854,#127855,#127856,#127857,#127858,
#127859,#127860,#127861,#127862,#127863,#127864,#127865,#127866,#127867,
#127868,#127869,#127870,#127871,#127872,#127873,#127874,#127875),
 .UNSPECIFIED.,.F.,.F.,(4,3,3,3,3,3,3,3,3,3,3,3,3,3,3,3,3,3,3,3,3,3,4),
(21.99114857557,22.1068520005075,22.2230284706919,22.3398009090817,22.3785238795456,
22.4827134973594,22.5867478987589,22.6906602805993,22.7945072106377,22.8983234626795,
23.0021437670992,23.1060727131954,23.2100604892296,23.3142301486006,23.3760717378917,
23.481139752265,23.5851525018523,23.6890607167021,23.7928992614511,23.8988284093079,
24.0026697174858,24.1096427851821,24.2166158528785),.UNSPECIFIED.);
#2932=B_SPLINE_CURVE_WITH_KNOTS('',3,(#127876,#127877,#127878,#127879,#127880,
#127881,#127882,#127883,#127884,#127885,#127886,#127887,#127888,#127889,
#127890,#127891,#127892,#127893,#127894,#127895,#127896,#127897,#127898,
#127899,#127900,#127901,#127902,#127903,#127904,#127905,#127906,#127907,
#127908,#127909,#127910,#127911,#127912,#127913,#127914,#127915,#127916,
#127917,#127918,#127919,#127920,#127921,#127922,#127923,#127924,#127925,
#127926,#127927,#127928,#127929,#127930,#127931,#127932,#127933,#127934,
#127935,#127936,#127937,#127938,#127939,#127940,#127941,#127942,#127943,
#127944,#127945,#127946,#127947,#127948,#127949,#127950,#127951,#127952,
#127953,#127954,#127955,#127956,#127957,#127958,#127959,#127960,#127961,
#127962,#127963,#127964,#127965,#127966,#127967,#127968,#127969,#127970,
#127971,#127972,#127973,#127974,#127975,#127976,#127977,#127978,#127979,
#127980,#127981,#127982,#127983,#127984,#127985,#127986,#127987,#127988,
#127989,#127990,#127991,#127992,#127993,#127994,#127995,#127996,#127997,
#127998,#127999),.UNSPECIFIED.,.F.,.F.,(4,3,3,3,3,3,3,3,3,3,3,3,3,3,3,3,
3,3,3,3,3,3,3,3,3,3,3,3,3,3,3,3,3,3,3,3,3,3,3,3,3,4),(17.9338080088879,
18.0378164903648,18.1419400609392,18.2461304916012,18.3504962327555,18.3883324461612,
18.4924051434582,18.5963209537852,18.7001128325525,18.8038381420455,18.9075318344083,
19.0112288172744,19.115034121039,19.2188978842661,19.3229442892214,19.3858803045073,
19.4900853041056,19.5941350899583,19.6980627826847,19.8019249693451,19.9057564003801,
20.0095917827304,20.113535546061,20.2175380144279,20.3217220069307,20.3834281628534,
20.4876329423721,20.5916828960584,20.6956113364386,20.7994746290363,20.9033075235404,
21.0071447265092,21.1110908476868,21.2150959807482,21.3192830983351,21.3809760211995,
21.4863434462503,21.5915445814378,21.6965918388519,21.8015478925087,21.9064564857074,
21.9911485751285),.UNSPECIFIED.);
#2933=B_SPLINE_CURVE_WITH_KNOTS('',3,(#128002,#128003,#128004,#128005,#128006,
#128007,#128008,#128009,#128010,#128011,#128012,#128013,#128014,#128015,
#128016,#128017,#128018,#128019,#128020,#128021,#128022,#128023,#128024,
#128025,#128026,#128027,#128028,#128029,#128030,#128031,#128032,#128033,
#128034,#128035,#128036,#128037,#128038,#128039,#128040,#128041,#128042,
#128043,#128044,#128045,#128046,#128047,#128048,#128049,#128050,#128051,
#128052,#128053,#128054,#128055,#128056,#128057,#128058,#128059,#128060,
#128061,#128062,#128063,#128064,#128065,#128066,#128067,#128068,#128069,
#128070,#128071,#128072,#128073,#128074,#128075,#128076,#128077,#128078,
#128079,#128080,#128081,#128082,#128083,#128084,#128085,#128086,#128087,
#128088,#128089,#128090,#128091,#128092,#128093,#128094,#128095,#128096,
#128097,#128098,#128099,#128100,#128101,#128102,#128103,#128104,#128105,
#128106,#128107,#128108,#128109,#128110,#128111,#128112,#128113,#128114,
#128115,#128116,#128117,#128118,#128119,#128120,#128121,#128122,#128123,
#128124,#128125,#128126,#128127,#128128,#128129,#128130,#128131,#128132,
#128133,#128134,#128135,#128136,#128137,#128138,#128139,#128140,#128141,
#128142,#128143,#128144,#128145,#128146,#128147,#128148,#128149,#128150,
#128151,#128152,#128153,#128154,#128155,#128156,#128157,#128158,#128159,
#128160,#128161,#128162,#128163,#128164,#128165,#128166,#128167,#128168,
#128169,#128170,#128171,#128172,#128173,#128174,#128175,#128176,#128177,
#128178,#128179,#128180,#128181,#128182,#128183,#128184,#128185,#128186,
#128187,#128188,#128189,#128190,#128191,#128192,#128193),.UNSPECIFIED.,
 .F.,.F.,(4,2,2,2,2,2,2,2,2,2,2,2,2,2,2,2,2,2,2,2,2,2,2,2,2,2,2,2,2,2,2,
2,2,2,2,2,2,2,2,2,2,2,2,2,2,2,2,2,2,2,2,2,2,2,2,2,2,2,2,2,2,2,2,2,2,2,2,
2,2,2,2,2,2,2,2,2,2,2,2,2,2,2,2,2,2,2,2,2,2,2,2,2,2,2,2,4),(-0.991428410285835,
-0.988079051914102,-0.986174702512279,-0.984686720637925,-0.982568327636504,
-0.978057342726682,-0.958846858953674,-0.925949063822915,-0.910796371618096,
-0.905890468462402,-0.90274575578572,-0.89976872626918,-0.895716929755394,
-0.886083974166438,-0.872156372916892,-0.851296795768739,-0.844281720716043,
-0.824951803310466,-0.821511726513893,-0.819587581485021,-0.818101821779044,
-0.816008744738817,-0.811631822475302,-0.793628448958833,-0.761621483382622,
-0.744632225717325,-0.739501522247694,-0.736309326998721,-0.733352816301539,
-0.729428417369128,-0.720564804316846,-0.708149564548891,-0.675417687548301,
-0.658218517705773,-0.654819631418646,-0.652905103656635,-0.65141838021344,
-0.649313192190328,-0.644871404736423,-0.626288555738524,-0.581124760367325,
-0.574882839187131,-0.571124120715254,-0.568182147552947,-0.56494395926655,
-0.559596962681835,-0.536841489904728,-0.505575230366341,-0.491254572171557,
-0.487968880243975,-0.48609905153233,-0.484436286563665,-0.482154321579273,
-0.476712199079443,-0.468741731538051,-0.441496748860293,-0.412387717576688,
-0.406739585552727,-0.403404967233731,-0.400508038898117,-0.396863382055824,
-0.389541116597339,-0.379924474232353,-0.354139622884094,-0.326964804441683,
-0.322224587258243,-0.320087043524696,-0.318437380115702,-0.316504946503874,
-0.312926655053968,-0.308344436582049,-0.26461115235902,-0.244951083691612,
-0.239647439108722,-0.236418664904477,-0.233474418659642,-0.229633554968816,
-0.221247768178535,-0.198872379938102,-0.160140751580241,-0.1559475005551,
-0.153857693129254,-0.152176139033525,-0.150430206099431,-0.14781516987963,
-0.144570044779037,-0.138158827217404,-0.119941501135129,-0.0808892449979691,
-0.0747875341691031,-0.0710287905266305,-0.068094704374682,-0.0648232573106013,
-0.0593202236501849,-0.0332727463327188,-0.000493937522251609),
 .UNSPECIFIED.);
#2934=B_SPLINE_CURVE_WITH_KNOTS('',3,(#128194,#128195,#128196,#128197,#128198,
#128199,#128200,#128201,#128202,#128203,#128204,#128205,#128206,#128207,
#128208,#128209,#128210,#128211,#128212,#128213),.UNSPECIFIED.,.F.,.F.,
(4,2,2,2,2,2,2,2,2,4),(-2.09972702821217,-2.09332876904563,-2.08914070274811,
-2.08717690472677,-2.08561029790526,-2.08408096225861,-2.08202773782795,
-2.07785554176778,-2.06362842930142,-2.04089325283701),.UNSPECIFIED.);
#2935=B_SPLINE_CURVE_WITH_KNOTS('',3,(#128214,#128215,#128216,#128217,#128218,
#128219,#128220,#128221,#128222,#128223,#128224,#128225,#128226,#128227,
#128228,#128229,#128230,#128231,#128232,#128233,#128234,#128235,#128236,
#128237,#128238,#128239,#128240,#128241,#128242,#128243,#128244,#128245,
#128246,#128247,#128248,#128249,#128250,#128251,#128252,#128253,#128254,
#128255,#128256,#128257,#128258,#128259,#128260,#128261,#128262,#128263,
#128264,#128265,#128266,#128267,#128268,#128269,#128270,#128271,#128272,
#128273,#128274,#128275,#128276,#128277,#128278,#128279,#128280,#128281,
#128282,#128283,#128284,#128285,#128286,#128287,#128288,#128289,#128290,
#128291,#128292,#128293,#128294,#128295,#128296,#128297,#128298,#128299,
#128300,#128301,#128302,#128303,#128304,#128305,#128306,#128307,#128308,
#128309,#128310,#128311,#128312,#128313,#128314,#128315,#128316,#128317,
#128318,#128319,#128320,#128321,#128322,#128323,#128324,#128325,#128326,
#128327,#128328,#128329,#128330,#128331,#128332,#128333,#128334,#128335,
#128336,#128337,#128338,#128339,#128340,#128341,#128342,#128343,#128344,
#128345,#128346,#128347,#128348,#128349,#128350,#128351,#128352,#128353,
#128354,#128355,#128356,#128357,#128358,#128359,#128360,#128361,#128362,
#128363,#128364,#128365,#128366,#128367,#128368,#128369,#128370,#128371,
#128372,#128373,#128374,#128375,#128376,#128377,#128378,#128379,#128380,
#128381,#128382,#128383,#128384,#128385,#128386,#128387,#128388,#128389,
#128390,#128391,#128392,#128393,#128394,#128395,#128396,#128397,#128398,
#128399,#128400,#128401,#128402,#128403,#128404,#128405,#128406,#128407,
#128408,#128409,#128410,#128411,#128412,#128413),.UNSPECIFIED.,.F.,.F.,
(4,2,2,2,2,2,2,2,2,2,2,2,2,2,2,2,2,2,2,2,2,2,2,2,2,2,2,2,2,2,2,2,2,2,2,
2,2,2,2,2,2,2,2,2,2,2,2,2,2,2,2,2,2,2,2,2,2,2,2,2,2,2,2,2,2,2,2,2,2,2,2,
2,2,2,2,2,2,2,2,2,2,2,2,2,2,2,2,2,2,2,2,2,2,2,2,2,2,2,2,4),(-1.75137704512006,
-1.75068586141549,-1.74773502972146,-1.74384492978998,-1.73517717150812,
-1.70756333847727,-1.67406144166101,-1.6696848637827,-1.66759229681557,
-1.6659488161001,-1.66395579085683,-1.66008441585536,-1.65501110865308,
-1.64253315520674,-1.60439630157427,-1.59131627393385,-1.58664387665479,
-1.58385831735353,-1.58089453160312,-1.5769185418947,-1.56774476698758,
-1.52303114913358,-1.50580683490755,-1.50240662273871,-1.50049185289282,
-1.4990049665169,-1.49689969713169,-1.49245905629593,-1.47388979843424,
-1.42871407639495,-1.42247706030726,-1.41871950393603,-1.41577738265347,
-1.41253793923695,-1.40718629000793,-1.38435578994611,-1.352638704996,-1.33878463943771,
-1.33552894718525,-1.33366566185352,-1.33200215173781,-1.32970942554851,
-1.32419459703652,-1.31607697962534,-1.28777223434872,-1.25982060941732,
-1.25416928215468,-1.25086734937448,-1.24823352273214,-1.24467544776299,
-1.23778643396667,-1.21272093777518,-1.18670930496516,-1.17216906670648,
-1.16891123022386,-1.16702936965349,-1.16537041375951,-1.16311396155721,
-1.15782516983446,-1.15015885150216,-1.12496725237433,-1.09577693192094,
-1.08865718470918,-1.08500453074326,-1.08207938288981,-1.0787388427316,
-1.07291697071022,-1.03935143486294,-1.00742403873065,-1.00298861170436,
-1.0008532998799,-0.999204598484219,-0.997238008388753,-0.993510036178509,
-0.988681208620626,-0.977124402256908,-0.955825141315264,-0.926759379615489,
-0.921110912166493,-0.917773525313023,-0.914872458758619,-0.911220183221169,
-0.903873501595287,-0.894219283714354,-0.868273613820256,-0.841255103291184,
-0.836525628966603,-0.834390221870311,-0.832744582165012,-0.830824946150585,
-0.827271074801043,-0.798463059903333,-0.761980772425169,-0.755661402129203,
-0.751891185075146,-0.748961058139669,-0.745757486285535,-0.740518802882096,
-0.719296593176995,-0.701455818686197),.UNSPECIFIED.);
#2936=B_SPLINE_CURVE_WITH_KNOTS('',3,(#128416,#128417,#128418,#128419,#128420,
#128421,#128422,#128423,#128424,#128425,#128426,#128427,#128428,#128429,
#128430,#128431,#128432,#128433,#128434,#128435,#128436,#128437,#128438,
#128439,#128440,#128441,#128442,#128443,#128444,#128445,#128446,#128447,
#128448,#128449,#128450,#128451,#128452,#128453,#128454,#128455,#128456,
#128457,#128458,#128459,#128460,#128461,#128462,#128463,#128464,#128465,
#128466,#128467,#128468,#128469,#128470,#128471,#128472,#128473,#128474,
#128475,#128476,#128477,#128478,#128479,#128480,#128481,#128482,#128483,
#128484,#128485,#128486,#128487,#128488,#128489,#128490,#128491,#128492,
#128493,#128494,#128495,#128496,#128497,#128498,#128499,#128500,#128501,
#128502,#128503,#128504,#128505,#128506,#128507,#128508,#128509,#128510,
#128511,#128512,#128513,#128514,#128515,#128516,#128517,#128518,#128519,
#128520,#128521,#128522,#128523,#128524,#128525,#128526,#128527,#128528,
#128529,#128530,#128531,#128532,#128533,#128534,#128535,#128536),
 .UNSPECIFIED.,.F.,.F.,(4,3,3,3,3,3,3,3,3,3,3,3,3,3,3,3,3,3,3,3,3,3,3,3,
3,3,3,3,3,3,3,3,3,3,3,3,3,3,3,3,4),(17.9343860550099,18.0384563012467,18.1423965009774,
18.2462659783595,18.3500994957989,18.4539317669694,18.5578694092301,18.6618610789189,
18.7660398843486,18.8442797453128,18.9484546129248,19.0524740709654,19.1563712946165,
19.2602029425331,19.3640038114039,19.4678086543699,19.5717221204532,19.675694386121,
19.779848640803,19.8418082797494,19.9459968485137,20.0500301930795,20.1539415107437,
20.2577873730439,20.3616025553732,20.46542178969,20.5693496667369,20.6733363761974,
20.7775049695994,20.839336814186,20.9435248555288,21.0475577022467,21.1514685688393,
21.2553140092606,21.3591287996192,21.4629476726207,21.5668752380743,21.6708616635392,
21.7750300200673,21.8368653486226,21.9911485751285),.UNSPECIFIED.);
#2937=B_SPLINE_CURVE_WITH_KNOTS('',3,(#128537,#128538,#128539,#128540,#128541,
#128542,#128543,#128544,#128545,#128546,#128547,#128548,#128549,#128550,
#128551,#128552,#128553,#128554,#128555,#128556,#128557,#128558,#128559,
#128560,#128561,#128562,#128563,#128564,#128565,#128566,#128567,#128568,
#128569,#128570,#128571,#128572,#128573,#128574,#128575,#128576,#128577,
#128578,#128579,#128580,#128581,#128582,#128583,#128584,#128585,#128586,
#128587,#128588,#128589,#128590,#128591,#128592,#128593,#128594,#128595,
#128596,#128597,#128598,#128599,#128600,#128601,#128602,#128603,#128604,
#128605,#128606),.UNSPECIFIED.,.F.,.F.,(4,3,3,3,3,3,3,3,3,3,3,3,3,3,3,3,
3,3,3,3,3,3,3,4),(21.9911485755033,22.0965542389478,22.1989427477135,22.3012648047145,
22.4035570514261,22.5058560821305,22.6082610316386,22.7107307725331,22.8133655493976,
22.8343938830592,22.9385806433496,23.0426121737347,23.1465216778305,23.2503657279729,
23.3541791023172,23.4579965355874,23.5619226348359,23.6659075769415,23.7700744389157,
23.8319224174958,23.9360794349529,24.0401009061163,24.1440085667296,24.2175036368067),
 .UNSPECIFIED.);
#2938=B_SPLINE_CURVE_WITH_KNOTS('',3,(#128608,#128609,#128610,#128611,#128612,
#128613,#128614,#128615,#128616,#128617,#128618,#128619,#128620,#128621,
#128622,#128623,#128624,#128625,#128626,#128627,#128628,#128629,#128630,
#128631,#128632,#128633,#128634,#128635,#128636,#128637,#128638,#128639,
#128640,#128641,#128642,#128643,#128644,#128645,#128646,#128647,#128648,
#128649,#128650,#128651,#128652,#128653,#128654,#128655,#128656,#128657,
#128658,#128659,#128660,#128661,#128662,#128663,#128664,#128665,#128666,
#128667,#128668,#128669,#128670,#128671,#128672,#128673,#128674),
 .UNSPECIFIED.,.F.,.F.,(4,3,3,3,3,3,3,3,3,3,3,3,3,3,3,3,3,3,3,3,3,3,4),
(21.9911485755641,22.1068686936971,22.2230626932475,22.3398531219692,22.3783692882696,
22.4825578617427,22.5865912110659,22.6905025335363,22.7943484006702,22.8981635878534,
23.0019828270372,23.1059107089372,23.2098974232505,23.3140660214517,23.3758978227062,
23.4809869478153,23.5849996243381,23.6889077755763,23.7927462661774,23.8987124055277,
24.0025537182315,24.1095822709052,24.2166108235789),.UNSPECIFIED.);
#2939=B_SPLINE_CURVE_WITH_KNOTS('',3,(#128675,#128676,#128677,#128678,#128679,
#128680,#128681,#128682,#128683,#128684,#128685,#128686,#128687,#128688,
#128689,#128690,#128691,#128692,#128693,#128694,#128695,#128696,#128697,
#128698,#128699,#128700,#128701,#128702,#128703,#128704,#128705,#128706,
#128707,#128708,#128709,#128710,#128711,#128712,#128713,#128714,#128715,
#128716,#128717,#128718,#128719,#128720,#128721,#128722,#128723,#128724,
#128725,#128726,#128727,#128728,#128729,#128730,#128731,#128732,#128733,
#128734,#128735,#128736,#128737,#128738,#128739,#128740,#128741,#128742,
#128743,#128744,#128745,#128746,#128747,#128748,#128749,#128750,#128751,
#128752,#128753,#128754,#128755,#128756,#128757,#128758,#128759,#128760,
#128761,#128762,#128763,#128764,#128765,#128766,#128767,#128768,#128769,
#128770,#128771,#128772,#128773,#128774,#128775,#128776,#128777,#128778,
#128779,#128780,#128781,#128782,#128783,#128784,#128785,#128786,#128787,
#128788,#128789,#128790,#128791,#128792,#128793,#128794,#128795,#128796,
#128797,#128798),.UNSPECIFIED.,.F.,.F.,(4,3,3,3,3,3,3,3,3,3,3,3,3,3,3,3,
3,3,3,3,3,3,3,3,3,3,3,3,3,3,3,3,3,3,3,3,3,3,3,3,3,4),(17.9338028153519,
18.037802986915,18.1419180880466,18.2460999659707,18.3504570297057,18.3882551505232,
18.4923467216465,18.5962816946849,18.7000930752598,18.8038380867795,18.9075516535319,
19.0112686554929,19.1150940593869,19.2189780032249,19.3230444840438,19.3857836849598,
19.4899815455746,19.5940241205743,19.6979445301226,19.8017993933992,19.905623471839,
20.0094514833414,20.113387893203,20.2173830103628,20.3215597202534,20.3833122193964,
20.4875152949366,20.5915634971424,20.6954901224722,20.7993515620656,20.9031825682167,
21.0070178500512,21.1109620069549,21.2149651519192,21.319150249886,21.380840753833,
21.4862078208751,21.5914087085921,21.6964558994253,21.8014119807972,21.9063207971622,
21.9911485751285),.UNSPECIFIED.);
#2940=B_SPLINE_CURVE_WITH_KNOTS('',3,(#128801,#128802,#128803,#128804,#128805,
#128806,#128807,#128808,#128809,#128810,#128811,#128812,#128813,#128814,
#128815,#128816,#128817,#128818,#128819,#128820,#128821,#128822,#128823,
#128824,#128825,#128826,#128827,#128828,#128829,#128830,#128831,#128832,
#128833,#128834,#128835,#128836,#128837,#128838,#128839,#128840,#128841,
#128842,#128843,#128844,#128845,#128846,#128847,#128848,#128849,#128850,
#128851,#128852,#128853,#128854,#128855,#128856,#128857,#128858,#128859,
#128860,#128861,#128862,#128863,#128864,#128865,#128866,#128867,#128868,
#128869,#128870,#128871,#128872,#128873,#128874,#128875,#128876,#128877,
#128878,#128879,#128880,#128881,#128882,#128883,#128884,#128885,#128886,
#128887,#128888,#128889,#128890,#128891,#128892,#128893,#128894,#128895,
#128896,#128897,#128898,#128899,#128900,#128901,#128902,#128903,#128904,
#128905,#128906,#128907,#128908,#128909,#128910,#128911,#128912,#128913,
#128914,#128915,#128916,#128917,#128918,#128919,#128920,#128921,#128922,
#128923,#128924,#128925,#128926,#128927,#128928,#128929,#128930,#128931,
#128932,#128933,#128934,#128935,#128936,#128937,#128938,#128939,#128940,
#128941,#128942,#128943,#128944,#128945,#128946,#128947,#128948,#128949,
#128950,#128951,#128952,#128953,#128954,#128955,#128956,#128957,#128958,
#128959,#128960,#128961,#128962,#128963,#128964,#128965,#128966,#128967,
#128968,#128969,#128970,#128971,#128972,#128973,#128974,#128975,#128976,
#128977,#128978,#128979,#128980,#128981,#128982,#128983,#128984,#128985,
#128986,#128987,#128988,#128989,#128990,#128991,#128992),.UNSPECIFIED.,
 .F.,.F.,(4,2,2,2,2,2,2,2,2,2,2,2,2,2,2,2,2,2,2,2,2,2,2,2,2,2,2,2,2,2,2,
2,2,2,2,2,2,2,2,2,2,2,2,2,2,2,2,2,2,2,2,2,2,2,2,2,2,2,2,2,2,2,2,2,2,2,2,
2,2,2,2,2,2,2,2,2,2,2,2,2,2,2,2,2,2,2,2,2,2,2,2,2,2,2,2,4),(-0.991336294305795,
-0.987987101398143,-0.986082845117753,-0.984594935419473,-0.982476644211697,
-0.97796587170094,-0.958756254912108,-0.925859865691171,-0.910708157934416,
-0.905802519572545,-0.902657965632366,-0.899681078608121,-0.895629463748385,
-0.885996878357646,-0.872069755009444,-0.851211466103253,-0.844196737899769,
-0.824867832965056,-0.821427925970876,-0.819503875272155,-0.818018187896217,
-0.815925212111296,-0.811548499507635,-0.793545971044919,-0.761540534867801,
-0.744552177334396,-0.739421730477923,-0.736229692036535,-0.733273324640428,
-0.729349113007491,-0.720485909664926,-0.708071232202234,-0.67534783706546,
-0.658143341132571,-0.654744275577906,-0.652829763641028,-0.651343124631843,
-0.649238149828613,-0.644797164492093,-0.626220490021437,-0.581048922266406,
-0.57480940999282,-0.571051471845711,-0.568109721197564,-0.56487138004869,
-0.559523195959956,-0.536742575705524,-0.505289792168805,-0.491167620015925,
-0.487892604346136,-0.486025143280338,-0.484361799559493,-0.482075384822308,
-0.476605830689058,-0.468580378857207,-0.440944363429201,-0.412262885621592,
-0.406581292007913,-0.403271345951693,-0.400636251064664,-0.397083063475046,
-0.390226616239235,-0.365430809386113,-0.348165274326103,-0.324988850227267,
-0.321498237784412,-0.31956331640413,-0.317929805578128,-0.315768895589642,
-0.311025822745156,-0.289574163504058,-0.250200258349139,-0.241694054567859,
-0.237873414071076,-0.234922852552908,-0.231715236094792,-0.226510522016004,
-0.206078785196696,-0.184811426749428,-0.160274311105911,-0.155528860473532,
-0.153390586163907,-0.151808624763331,-0.1499682351261,-0.146859212096279,
-0.142857193929927,-0.134136398320465,-0.100900011079064,-0.0785973214288766,
-0.0731311387372958,-0.0698675843457679,-0.0669318734674677,-0.0631589053512889,
-0.0551502767508302,-0.019766497034221,-0.000493928755314768),
 .UNSPECIFIED.);
#2941=B_SPLINE_CURVE_WITH_KNOTS('',3,(#128993,#128994,#128995,#128996,#128997,
#128998,#128999,#129000,#129001,#129002,#129003,#129004,#129005,#129006,
#129007,#129008,#129009,#129010,#129011,#129012,#129013,#129014),
 .UNSPECIFIED.,.F.,.F.,(4,2,2,2,2,2,2,2,2,2,4),(-2.09974145399818,-2.09334315366096,
-2.08915505855463,-2.0871912462299,-2.08562462813712,-2.08409528173233,
-2.08204204294441,-2.0778698186273,-2.06364260288612,-2.04644554779855,
-2.04091635741276),.UNSPECIFIED.);
#2942=B_SPLINE_CURVE_WITH_KNOTS('',3,(#129015,#129016,#129017,#129018,#129019,
#129020,#129021,#129022,#129023,#129024,#129025,#129026,#129027,#129028,
#129029,#129030,#129031,#129032,#129033,#129034,#129035,#129036,#129037,
#129038,#129039,#129040,#129041,#129042,#129043,#129044,#129045,#129046,
#129047,#129048,#129049,#129050,#129051,#129052,#129053,#129054,#129055,
#129056,#129057,#129058,#129059,#129060,#129061,#129062,#129063,#129064,
#129065,#129066,#129067,#129068,#129069,#129070,#129071,#129072,#129073,
#129074,#129075,#129076,#129077,#129078,#129079,#129080,#129081,#129082,
#129083,#129084,#129085,#129086,#129087,#129088,#129089,#129090,#129091,
#129092,#129093,#129094,#129095,#129096,#129097,#129098,#129099,#129100,
#129101,#129102,#129103,#129104,#129105,#129106,#129107,#129108,#129109,
#129110,#129111,#129112,#129113,#129114,#129115,#129116,#129117,#129118,
#129119,#129120,#129121,#129122,#129123,#129124,#129125,#129126,#129127,
#129128,#129129,#129130,#129131,#129132,#129133,#129134,#129135,#129136,
#129137,#129138,#129139,#129140,#129141,#129142,#129143,#129144,#129145,
#129146,#129147,#129148,#129149,#129150,#129151,#129152,#129153,#129154,
#129155,#129156,#129157,#129158,#129159,#129160,#129161,#129162,#129163,
#129164,#129165,#129166,#129167,#129168,#129169,#129170,#129171,#129172,
#129173,#129174,#129175,#129176,#129177,#129178,#129179,#129180,#129181,
#129182,#129183,#129184,#129185,#129186,#129187,#129188,#129189,#129190,
#129191,#129192,#129193,#129194,#129195,#129196,#129197,#129198,#129199,
#129200,#129201,#129202,#129203,#129204,#129205,#129206,#129207,#129208,
#129209,#129210,#129211,#129212,#129213,#129214,#129215,#129216),
 .UNSPECIFIED.,.F.,.F.,(4,2,2,2,2,2,2,2,2,2,2,2,2,2,2,2,2,2,2,2,2,2,2,2,
2,2,2,2,2,2,2,2,2,2,2,2,2,2,2,2,2,2,2,2,2,2,2,2,2,2,2,2,2,2,2,2,2,2,2,2,
2,2,2,2,2,2,2,2,2,2,2,2,2,2,2,2,2,2,2,2,2,2,2,2,2,2,2,2,2,2,2,2,2,2,2,2,
2,2,2,2,4),(-1.75130590682506,-1.75061804629367,-1.74766762561627,-1.74377980457627,
-1.73512470195656,-1.70734178850423,-1.67401985750049,-1.66962622496779,
-1.66753045685401,-1.66588688574552,-1.66389669415773,-1.66003900346778,
-1.65498889582004,-1.64259896704644,-1.60511275082854,-1.59141072418469,
-1.5866644495711,-1.58355435656397,-1.58056081662683,-1.5764066612657,-1.56610809015788,
-1.5507999490363,-1.51866019675941,-1.50539963831284,-1.50218052644649,
-1.50032516243598,-1.49865779364918,-1.49634566606401,-1.49071948012675,
-1.48237815950512,-1.45627308193678,-1.42659499878978,-1.42092049689232,
-1.41761197985444,-1.41497656647377,-1.41142105868874,-1.40455345080713,
-1.37967351499626,-1.36245840759542,-1.33931437673376,-1.33582399778277,
-1.3338892891024,-1.33224112786826,-1.33007316787738,-1.32528507609731,
-1.30336304724814,-1.26250389254157,-1.255379422689,-1.25172840870059,-1.24880663367437,
-1.24547225710487,-1.23966746663796,-1.20514407131681,-1.17423617344591,
-1.17012218360522,-1.16805239224227,-1.16637654611349,-1.16458659938468,
-1.16166646043304,-1.15090593393718,-1.12831455185246,-1.0957114459424,
-1.08863811929518,-1.0849952741147,-1.08207118331994,-1.07872445072472,
-1.07287227130779,-1.03970996496604,-1.00741513181906,-1.00337939226342,
-1.0013274128128,-0.999654052427862,-0.997849692926993,-0.99487632835588,
-0.983526600014533,-0.958531015489666,-0.926759634757129,-0.921055737384536,
-0.917738503173626,-0.915100499254351,-0.911547044420506,-0.904702531898288,
-0.880033831251204,-0.841083278609066,-0.836470880983687,-0.834356776632777,
-0.832713508390733,-0.830779098882874,-0.827154299592165,-0.822488474943991,
-0.811491760080047,-0.789736134853379,-0.759698371655822,-0.754103557698703,
-0.750792344359605,-0.747911395839402,-0.744281645528209,-0.736973319207148,
-0.727366827344797,-0.701574795806025,-0.70148998943205),.UNSPECIFIED.);
#2943=B_SPLINE_CURVE_WITH_KNOTS('',3,(#129219,#129220,#129221,#129222,#129223,
#129224,#129225,#129226,#129227,#129228,#129229,#129230,#129231,#129232,
#129233,#129234,#129235,#129236,#129237,#129238,#129239,#129240,#129241,
#129242,#129243,#129244,#129245,#129246,#129247,#129248,#129249,#129250,
#129251,#129252,#129253,#129254,#129255,#129256,#129257,#129258,#129259,
#129260,#129261,#129262,#129263,#129264,#129265,#129266,#129267,#129268,
#129269,#129270,#129271,#129272,#129273,#129274,#129275,#129276,#129277,
#129278,#129279,#129280,#129281,#129282,#129283,#129284,#129285,#129286,
#129287,#129288,#129289,#129290,#129291,#129292,#129293,#129294,#129295,
#129296,#129297,#129298,#129299,#129300,#129301,#129302,#129303,#129304,
#129305,#129306,#129307,#129308,#129309,#129310,#129311,#129312,#129313,
#129314,#129315,#129316,#129317,#129318,#129319,#129320,#129321,#129322,
#129323,#129324,#129325,#129326,#129327,#129328,#129329,#129330,#129331,
#129332,#129333,#129334,#129335,#129336,#129337,#129338,#129339),
 .UNSPECIFIED.,.F.,.F.,(4,3,3,3,3,3,3,3,3,3,3,3,3,3,3,3,3,3,3,3,3,3,3,3,
3,3,3,3,3,3,3,3,3,3,3,3,3,3,3,3,4),(17.9343860548896,18.0384562993147,18.1423964971713,
18.2462659726421,18.3500994881357,18.4539317573288,18.5578693975759,18.6618610652281,
18.7660398686056,18.844279745313,18.9484546158039,19.0524740767691,19.1563713033989,
19.2602029543261,19.3640038262347,19.4678086722615,19.5717221414199,19.6756944101755,
19.7798486679322,19.8418082797496,19.945996847463,20.0500301909672,20.1539415075587,
20.2577873687803,20.3616025500263,20.465421783257,20.5693496592209,20.6733363675984,
20.7775049599295,20.8393368141862,20.9435248552688,21.0475577017188,21.1514685680337,
21.255314008171,21.3591287982401,21.4629476709467,21.5668752360994,21.6708616612596,
21.7750300174801,21.8368653486228,21.9911485751285),.UNSPECIFIED.);
#2944=B_SPLINE_CURVE_WITH_KNOTS('',3,(#129340,#129341,#129342,#129343,#129344,
#129345,#129346,#129347,#129348,#129349,#129350,#129351,#129352,#129353,
#129354,#129355,#129356,#129357,#129358,#129359,#129360,#129361,#129362,
#129363,#129364,#129365,#129366,#129367,#129368,#129369,#129370,#129371,
#129372,#129373,#129374,#129375,#129376,#129377,#129378,#129379,#129380,
#129381,#129382,#129383,#129384,#129385,#129386,#129387,#129388,#129389,
#129390,#129391,#129392,#129393,#129394,#129395,#129396,#129397,#129398,
#129399,#129400,#129401,#129402,#129403,#129404,#129405,#129406,#129407,
#129408,#129409),.UNSPECIFIED.,.F.,.F.,(4,3,3,3,3,3,3,3,3,3,3,3,3,3,3,3,
3,3,3,3,3,3,3,4),(21.9911485755033,22.0965542389478,22.1989427481708,22.3012648056322,
22.4035570528071,22.5058560839769,22.6082610339522,22.7107307753153,22.8133655526472,
22.8343938830594,22.9385806431776,23.0426121733884,23.1465216773082,23.2503657272733,
23.3541791014396,23.4579965345313,23.5619226336016,23.6659075755289,23.7700744373266,
23.831922417496,23.9360794349241,24.0401009060572,24.1440085666394,24.217503635835),
 .UNSPECIFIED.);
#2945=B_SPLINE_CURVE_WITH_KNOTS('',3,(#129411,#129412,#129413,#129414,#129415,
#129416,#129417,#129418,#129419,#129420,#129421,#129422,#129423,#129424,
#129425,#129426,#129427,#129428,#129429,#129430,#129431,#129432,#129433,
#129434,#129435,#129436,#129437,#129438,#129439,#129440,#129441,#129442,
#129443,#129444,#129445,#129446,#129447,#129448,#129449,#129450,#129451,
#129452,#129453,#129454,#129455,#129456,#129457,#129458,#129459,#129460,
#129461,#129462,#129463,#129464,#129465,#129466,#129467,#129468,#129469,
#129470,#129471,#129472,#129473,#129474,#129475,#129476,#129477),
 .UNSPECIFIED.,.F.,.F.,(4,3,3,3,3,3,3,3,3,3,3,3,3,3,3,3,3,3,3,3,3,3,4),
(21.9911485755641,22.1068686992636,22.2230627045344,22.3398531390132,22.3783692882698,
22.4825578603194,22.5865912082046,22.6905025292221,22.7943483948948,22.8981635806107,
23.0019828183231,23.1059106987561,23.2098974116023,23.3140660083528,23.3758978227064,
23.4809869476749,23.5849996238318,23.6889077746951,23.7927462649133,23.8987124042985,
24.0025537166019,24.109582269528,24.216610822454),.UNSPECIFIED.);
#2946=B_SPLINE_CURVE_WITH_KNOTS('',3,(#129478,#129479,#129480,#129481,#129482,
#129483,#129484,#129485,#129486,#129487,#129488,#129489,#129490,#129491,
#129492,#129493,#129494,#129495,#129496,#129497,#129498,#129499,#129500,
#129501,#129502,#129503,#129504,#129505,#129506,#129507,#129508,#129509,
#129510,#129511,#129512,#129513,#129514,#129515,#129516,#129517,#129518,
#129519,#129520,#129521,#129522,#129523,#129524,#129525,#129526,#129527,
#129528,#129529,#129530,#129531,#129532,#129533,#129534,#129535,#129536,
#129537,#129538,#129539,#129540,#129541,#129542,#129543,#129544,#129545,
#129546,#129547,#129548,#129549,#129550,#129551,#129552,#129553,#129554,
#129555,#129556,#129557,#129558,#129559,#129560,#129561,#129562,#129563,
#129564,#129565,#129566,#129567,#129568,#129569,#129570,#129571,#129572,
#129573,#129574,#129575,#129576,#129577,#129578,#129579,#129580,#129581,
#129582,#129583,#129584,#129585,#129586,#129587,#129588,#129589,#129590,
#129591,#129592,#129593,#129594,#129595,#129596,#129597,#129598,#129599,
#129600,#129601),.UNSPECIFIED.,.F.,.F.,(4,3,3,3,3,3,3,3,3,3,3,3,3,3,3,3,
3,3,3,3,3,3,3,3,3,3,3,3,3,3,3,3,3,3,3,3,3,3,3,3,3,4),(17.9338028151035,
18.0378029754529,18.1419180651585,18.2460999315279,18.350456983587,18.3882551505234,
18.4923467441545,18.5962817400488,18.70009314389,18.8038381789175,18.9075517693863,
19.0112687952391,19.115094223132,19.2189781910668,19.3230446958775,19.38578368496,
19.4899815369513,19.5940241032359,19.6979445039763,19.8017993583924,19.9056234279328,
20.00945143051,20.1133878314687,20.2173829397245,20.321559640807,20.3833122193966,
20.4875152925416,20.5915634922881,20.695490115075,20.7993515520751,20.903182555586,
21.0070178347373,21.1109619889101,21.2149651311122,21.3191502262971,21.3808407538332,
21.4862078248736,21.5914087166519,21.6964559116178,21.8014119971609,21.9063208177285,
21.9911485751285),.UNSPECIFIED.);
#2947=B_SPLINE_CURVE_WITH_KNOTS('',3,(#129603,#129604,#129605,#129606,#129607,
#129608,#129609,#129610,#129611,#129612,#129613,#129614,#129615,#129616,
#129617,#129618,#129619,#129620,#129621,#129622,#129623,#129624,#129625,
#129626,#129627,#129628,#129629,#129630,#129631,#129632,#129633,#129634,
#129635,#129636,#129637,#129638,#129639,#129640,#129641,#129642,#129643,
#129644,#129645,#129646,#129647,#129648,#129649,#129650,#129651,#129652,
#129653,#129654,#129655,#129656,#129657,#129658,#129659,#129660,#129661,
#129662,#129663,#129664,#129665,#129666,#129667,#129668,#129669,#129670,
#129671,#129672,#129673,#129674,#129675,#129676,#129677,#129678,#129679,
#129680,#129681,#129682,#129683,#129684,#129685,#129686,#129687,#129688,
#129689,#129690),.UNSPECIFIED.,.F.,.F.,(4,3,3,3,3,3,3,3,3,3,3,3,3,3,3,3,
3,3,3,3,3,3,3,3,3,3,3,3,3,4),(-0.378621596831377,-0.359800574898229,-0.347867415310614,
-0.339791008828829,-0.335413943756389,-0.315538205554487,-0.301206604784367,
-0.297325827080498,-0.293234930684288,-0.272788407631258,-0.252085100561485,
-0.239312075104769,-0.228816208612987,-0.224508526527948,-0.203203874900672,
-0.200837552551317,-0.179573256408454,-0.15830896026559,-0.154318299386255,
-0.150807254524542,-0.129197322625765,-0.107587390726988,-0.0856207534556525,
-0.0801950788551404,-0.0759413631771757,-0.0534076236452386,-0.0309843347957576,
-0.00876238345449811,-0.0040342792039191,-4.65033222477994E-5),
 .UNSPECIFIED.);
#2948=B_SPLINE_CURVE_WITH_KNOTS('',3,(#129691,#129692,#129693,#129694,#129695,
#129696,#129697,#129698,#129699,#129700,#129701,#129702,#129703,#129704,
#129705,#129706,#129707,#129708,#129709,#129710,#129711,#129712,#129713,
#129714,#129715,#129716,#129717,#129718,#129719,#129720,#129721,#129722,
#129723,#129724,#129725,#129726,#129727,#129728,#129729,#129730,#129731,
#129732,#129733,#129734,#129735,#129736,#129737,#129738,#129739,#129740,
#129741,#129742,#129743,#129744,#129745,#129746,#129747,#129748,#129749,
#129750,#129751,#129752,#129753,#129754,#129755,#129756,#129757,#129758,
#129759,#129760,#129761,#129762,#129763,#129764,#129765,#129766,#129767,
#129768,#129769,#129770,#129771,#129772,#129773,#129774,#129775),
 .UNSPECIFIED.,.F.,.F.,(4,3,3,3,3,3,3,3,3,3,3,3,3,3,3,3,3,3,3,3,3,3,3,3,
3,3,3,3,4),(-0.376940817211572,-0.354434745142103,-0.332914589324204,-0.328066558023255,
-0.30581833788643,-0.290198565614503,-0.28426487902006,-0.278600185330508,
-0.256937232807856,-0.235771146027844,-0.214945582624746,-0.208198463847886,
-0.20440189481038,-0.183824971878735,-0.180862865680233,-0.159776402420874,
-0.140305786244226,-0.136020080940874,-0.132586895718958,-0.112127717435514,
-0.0917629328401109,-0.071833700248866,-0.0676158682049212,-0.0636581831340513,
-0.0440997736349179,-0.0251751445195747,-0.0063477261176011,-0.00328482218945227,
0.),.UNSPECIFIED.);
#2949=B_SPLINE_CURVE_WITH_KNOTS('',3,(#130192,#130193,#130194,#130195,#130196,
#130197,#130198,#130199,#130200,#130201,#130202,#130203,#130204,#130205,
#130206,#130207,#130208,#130209,#130210,#130211,#130212,#130213,#130214,
#130215,#130216,#130217,#130218,#130219,#130220,#130221,#130222,#130223,
#130224,#130225,#130226,#130227,#130228,#130229,#130230,#130231,#130232,
#130233,#130234,#130235,#130236,#130237,#130238,#130239,#130240,#130241,
#130242,#130243,#130244,#130245,#130246,#130247,#130248,#130249,#130250,
#130251,#130252,#130253,#130254,#130255,#130256,#130257,#130258,#130259,
#130260,#130261,#130262,#130263,#130264,#130265,#130266,#130267,#130268,
#130269,#130270,#130271,#130272,#130273),.UNSPECIFIED.,.F.,.F.,(4,3,3,3,
3,3,3,3,3,3,3,3,3,3,3,3,3,3,3,3,3,3,3,3,3,3,3,4),(0.,0.0185942586373532,
0.0384196304941899,0.055766830868922,0.0644671558767212,0.0684494988071322,
0.0886798835323776,0.108910268257623,0.129281600569207,0.133842973757118,
0.137281880988472,0.158357027632817,0.177197233492047,0.197726581113147,
0.205650448408311,0.209125900862407,0.230376280882011,0.251626660901614,
0.273336565247494,0.278315660173636,0.284045110735794,0.306314217788196,
0.322966455755941,0.328173582351109,0.333184502846979,0.355705889915315,
0.372923169659177,0.376894494387216),.UNSPECIFIED.);
#2950=B_SPLINE_CURVE_WITH_KNOTS('',3,(#130691,#130692,#130693,#130694),
 .UNSPECIFIED.,.F.,.F.,(4,4),(-0.015320457083931,0.),.UNSPECIFIED.);
#2951=B_SPLINE_CURVE_WITH_KNOTS('',3,(#130695,#130696,#130697,#130698,#130699,
#130700,#130701,#130702,#130703,#130704,#130705,#130706,#130707,#130708,
#130709,#130710,#130711,#130712,#130713,#130714,#130715,#130716,#130717,
#130718,#130719,#130720,#130721,#130722,#130723,#130724,#130725,#130726,
#130727,#130728,#130729,#130730,#130731,#130732,#130733,#130734,#130735,
#130736,#130737,#130738,#130739,#130740,#130741,#130742,#130743,#130744,
#130745,#130746,#130747,#130748,#130749,#130750,#130751,#130752,#130753,
#130754,#130755,#130756,#130757,#130758,#130759,#130760,#130761,#130762,
#130763,#130764,#130765,#130766,#130767,#130768,#130769,#130770,#130771,
#130772,#130773,#130774,#130775,#130776,#130777,#130778,#130779,#130780,
#130781,#130782),.UNSPECIFIED.,.F.,.F.,(4,3,3,3,3,3,3,3,3,3,3,3,3,3,3,3,
3,3,3,3,3,3,3,3,3,3,3,3,3,4),(0.,0.022076465099833,0.0446500161040329,0.0636175020481042,
0.0720961742632357,0.0767527781954435,0.0810480993262889,0.102995208587912,
0.12460210360104,0.142867742472728,0.150422572110747,0.153916820895177,
0.157566347805364,0.178337891460959,0.197155519647459,0.219426672701599,
0.224328424195588,0.229401239967913,0.250066209825086,0.270727085266657,
0.285675668497039,0.294182634390874,0.299799559450732,0.300624251727421,
0.320446372412837,0.334305514499652,0.338771695116765,0.357798190520139,
0.375324744080579,0.378621596831434),.UNSPECIFIED.);
#2952=B_SPLINE_CURVE_WITH_KNOTS('',3,(#130784,#130785,#130786,#130787,#130788,
#130789,#130790,#130791,#130792,#130793,#130794,#130795,#130796,#130797,
#130798,#130799,#130800,#130801,#130802,#130803,#130804,#130805,#130806,
#130807,#130808,#130809,#130810,#130811,#130812,#130813,#130814,#130815,
#130816,#130817,#130818,#130819,#130820,#130821,#130822,#130823,#130824,
#130825,#130826,#130827,#130828,#130829,#130830,#130831,#130832,#130833,
#130834,#130835,#130836,#130837,#130838,#130839,#130840,#130841,#130842,
#130843,#130844,#130845,#130846,#130847,#130848,#130849,#130850,#130851,
#130852,#130853,#130854,#130855,#130856,#130857,#130858,#130859,#130860,
#130861,#130862,#130863,#130864,#130865,#130866,#130867,#130868,#130869,
#130870,#130871),.UNSPECIFIED.,.F.,.F.,(4,3,3,3,3,3,3,3,3,3,3,3,3,3,3,3,
3,3,3,3,3,3,3,3,3,3,3,3,3,4),(-0.37862159683151,-0.359800569631031,-0.347867401893819,
-0.33979089123365,-0.335413899311082,-0.315538156337577,-0.301206561819263,
-0.297325731230975,-0.293234920420453,-0.272730298566073,-0.252027833031437,
-0.231534606194204,-0.22881619359477,-0.224508521722788,-0.203203870189045,
-0.200837552551386,-0.17957325789842,-0.158308963245454,-0.154318319294633,
-0.15080725817,-0.129484179150672,-0.107552470160347,-0.0856207611700218,
-0.0801950922726167,-0.075941367905241,-0.0534076290690578,-0.0309843400776861,
-0.0087623891159908,-0.0040342792039104,-4.65028613182856E-5),
 .UNSPECIFIED.);
#2953=B_SPLINE_CURVE_WITH_KNOTS('',3,(#130872,#130873,#130874,#130875,#130876,
#130877,#130878,#130879,#130880,#130881,#130882,#130883,#130884,#130885,
#130886,#130887,#130888,#130889,#130890,#130891,#130892,#130893,#130894,
#130895,#130896,#130897,#130898,#130899,#130900,#130901,#130902,#130903,
#130904,#130905,#130906,#130907,#130908,#130909,#130910,#130911,#130912,
#130913,#130914,#130915,#130916,#130917,#130918,#130919,#130920,#130921,
#130922,#130923,#130924,#130925,#130926,#130927,#130928,#130929,#130930,
#130931,#130932,#130933,#130934,#130935,#130936,#130937,#130938,#130939,
#130940,#130941,#130942,#130943,#130944,#130945,#130946,#130947,#130948,
#130949,#130950,#130951,#130952,#130953,#130954,#130955,#130956),
 .UNSPECIFIED.,.F.,.F.,(4,3,3,3,3,3,3,3,3,3,3,3,3,3,3,3,3,3,3,3,3,3,3,3,
3,3,3,3,4),(-0.37694081721158,-0.354434743621784,-0.332914587130445,-0.328066555497701,
-0.305817948776869,-0.290198563389788,-0.284264874081428,-0.278600185634699,
-0.256937233660704,-0.235771147852844,-0.214945584943483,-0.208198462262405,
-0.204401894988106,-0.183824973032507,-0.180862865680225,-0.159776402234228,
-0.14030578623386,-0.136020082340253,-0.132586896844658,-0.11213480581913,
-0.0918985800495415,-0.0718337025226597,-0.0676158747446753,-0.0636581853937461,
-0.0440844999903763,-0.0251601150180132,-0.00634773272082092,-0.00328482218946405,
0.),.UNSPECIFIED.);
#2954=B_SPLINE_CURVE_WITH_KNOTS('',3,(#131373,#131374,#131375,#131376,#131377,
#131378,#131379,#131380,#131381,#131382,#131383,#131384,#131385,#131386,
#131387,#131388,#131389,#131390,#131391,#131392,#131393,#131394,#131395,
#131396,#131397,#131398,#131399,#131400,#131401,#131402,#131403,#131404,
#131405,#131406,#131407,#131408,#131409,#131410,#131411,#131412,#131413,
#131414,#131415,#131416,#131417,#131418,#131419,#131420,#131421,#131422,
#131423,#131424,#131425,#131426,#131427,#131428,#131429,#131430,#131431,
#131432,#131433,#131434,#131435,#131436,#131437,#131438,#131439,#131440,
#131441,#131442,#131443,#131444,#131445,#131446,#131447,#131448,#131449,
#131450,#131451,#131452,#131453,#131454),.UNSPECIFIED.,.F.,.F.,(4,3,3,3,
3,3,3,3,3,3,3,3,3,3,3,3,3,3,3,3,3,3,3,3,3,3,3,4),(0.,0.0185942627018445,
0.0384196340506189,0.0557668339807965,0.0644671612702412,0.0684495001941655,
0.0885013648033302,0.108965744896479,0.125982013797114,0.1338429804339,
0.137281884411352,0.158357030774089,0.17719723349204,0.197726579166287,
0.205650447451187,0.20912590019485,0.230033568486251,0.25139264958201,0.273102086639384,
0.278315662662554,0.284045110154865,0.30631421705641,0.322966455207104,
0.328173581206648,0.33318450226615,0.355705889383306,0.372923169659185,
0.376894494728837),.UNSPECIFIED.);
#2955=B_SPLINE_CURVE_WITH_KNOTS('',3,(#131872,#131873,#131874,#131875),
 .UNSPECIFIED.,.F.,.F.,(4,4),(-0.0153203085855325,0.),.UNSPECIFIED.);
#2956=B_SPLINE_CURVE_WITH_KNOTS('',3,(#131876,#131877,#131878,#131879,#131880,
#131881,#131882,#131883,#131884,#131885,#131886,#131887,#131888,#131889,
#131890,#131891,#131892,#131893,#131894,#131895,#131896,#131897,#131898,
#131899,#131900,#131901,#131902,#131903,#131904,#131905,#131906,#131907,
#131908,#131909,#131910,#131911,#131912,#131913,#131914,#131915,#131916,
#131917,#131918,#131919,#131920,#131921,#131922,#131923,#131924,#131925,
#131926,#131927,#131928,#131929,#131930,#131931,#131932,#131933,#131934,
#131935,#131936,#131937,#131938,#131939,#131940,#131941,#131942,#131943,
#131944,#131945,#131946,#131947,#131948,#131949,#131950,#131951,#131952,
#131953,#131954,#131955,#131956,#131957,#131958,#131959,#131960),
 .UNSPECIFIED.,.F.,.F.,(4,3,3,3,3,3,3,3,3,3,3,3,3,3,3,3,3,3,3,3,3,3,3,3,
3,3,3,3,4),(0.,0.0220764692885148,0.0446500209087305,0.0636175065071147,
0.0720961755907872,0.0767527810215644,0.0810481000867341,0.102973125105672,
0.124771816179149,0.142867742046223,0.150422572478512,0.153916822796493,
0.157566348353921,0.178337890695287,0.197155519647444,0.21942667270158,
0.224328423930133,0.229401239955034,0.25009123940773,0.270727085421763,
0.285678464935528,0.296896068115054,0.300624249977848,0.320446369477332,
0.334305509215125,0.338771690168848,0.357798183302138,0.375324744080529,
0.378621596831382),.UNSPECIFIED.);
#2957=B_SPLINE_CURVE_WITH_KNOTS('',3,(#132392,#132393,#132394,#132395,#132396,
#132397,#132398,#132399,#132400,#132401,#132402,#132403,#132404,#132405,
#132406,#132407,#132408,#132409,#132410,#132411,#132412,#132413,#132414,
#132415,#132416,#132417,#132418,#132419,#132420,#132421,#132422,#132423,
#132424,#132425,#132426,#132427,#132428,#132429,#132430,#132431,#132432,
#132433,#132434,#132435,#132436,#132437,#132438,#132439,#132440,#132441,
#132442,#132443,#132444,#132445,#132446,#132447,#132448,#132449,#132450,
#132451,#132452,#132453,#132454,#132455,#132456,#132457,#132458,#132459,
#132460,#132461,#132462,#132463,#132464,#132465,#132466,#132467,#132468,
#132469,#132470,#132471,#132472,#132473,#132474,#132475,#132476),
 .UNSPECIFIED.,.F.,.F.,(4,3,3,3,3,3,3,3,3,3,3,3,3,3,3,3,3,3,3,3,3,3,3,3,
3,3,3,3,4),(-0.37694081721164,-0.354433306894873,-0.332912068438051,-0.328063707750488,
-0.305815531960939,-0.290195622062823,-0.284258173761416,-0.278600680525688,
-0.256917565609304,-0.235752667545141,-0.214948063833036,-0.208200328709319,
-0.204401454487156,-0.183825513702696,-0.180859240376696,-0.159772587659609,
-0.140301766015443,-0.136001540232934,-0.132615023040107,-0.112155832609778,
-0.0919195811109376,-0.0718621010890796,-0.0660721542666673,-0.0628432174816503,
-0.0432905316599473,-0.0240214811309868,-0.0047524306020263,-0.00327832057784897,
0.),.UNSPECIFIED.);
#2958=B_SPLINE_CURVE_WITH_KNOTS('',3,(#132477,#132478,#132479,#132480,#132481,
#132482,#132483,#132484,#132485,#132486,#132487,#132488,#132489,#132490,
#132491,#132492,#132493,#132494,#132495,#132496,#132497,#132498,#132499,
#132500,#132501,#132502,#132503,#132504,#132505,#132506,#132507,#132508,
#132509,#132510,#132511,#132512,#132513,#132514,#132515,#132516,#132517,
#132518,#132519,#132520,#132521,#132522,#132523,#132524,#132525,#132526,
#132527,#132528,#132529,#132530,#132531,#132532,#132533,#132534,#132535,
#132536,#132537,#132538,#132539,#132540,#132541,#132542,#132543,#132544,
#132545,#132546,#132547,#132548,#132549,#132550,#132551,#132552,#132553,
#132554,#132555,#132556,#132557,#132558),.UNSPECIFIED.,.F.,.F.,(4,3,3,3,
3,3,3,3,3,3,3,3,3,3,3,3,3,3,3,3,3,3,3,3,3,3,3,4),(0.,0.0186893861989584,
0.0380628975178282,0.0557706344050115,0.0644740455004294,0.0684512583734907,
0.0885273404451008,0.108992143028824,0.125987244216384,0.133851910987726,
0.138086378825073,0.158361294974393,0.177200852458616,0.197728340288859,
0.205651029746871,0.209126190448893,0.229948761197729,0.251461698426111,
0.268072642545509,0.278312078768208,0.284045428971702,0.306303003925287,
0.32296858048919,0.328170230546098,0.333183543693291,0.355704946189745,
0.372931104637556,0.376894629385132),.UNSPECIFIED.);
#2959=B_SPLINE_CURVE_WITH_KNOTS('',3,(#132559,#132560,#132561,#132562),
 .UNSPECIFIED.,.F.,.F.,(4,4),(0.,0.0152331259156648),.UNSPECIFIED.);
#2960=B_SPLINE_CURVE_WITH_KNOTS('',3,(#132943,#132944,#132945,#132946,#132947,
#132948,#132949,#132950,#132951,#132952,#132953,#132954,#132955,#132956,
#132957,#132958,#132959,#132960,#132961,#132962,#132963,#132964,#132965,
#132966,#132967,#132968,#132969,#132970,#132971,#132972,#132973,#132974,
#132975,#132976,#132977,#132978,#132979,#132980,#132981,#132982,#132983,
#132984,#132985,#132986,#132987,#132988,#132989,#132990,#132991,#132992,
#132993,#132994,#132995,#132996,#132997,#132998,#132999,#133000,#133001,
#133002,#133003,#133004,#133005,#133006,#133007,#133008,#133009,#133010,
#133011,#133012,#133013,#133014,#133015,#133016,#133017,#133018,#133019,
#133020,#133021,#133022,#133023,#133024,#133025,#133026,#133027,#133028,
#133029,#133030),.UNSPECIFIED.,.F.,.F.,(4,3,3,3,3,3,3,3,3,3,3,3,3,3,3,3,
3,3,3,3,3,3,3,3,3,3,3,3,3,4),(-0.378621596831385,-0.359796914683931,-0.347856916184549,
-0.339696030242093,-0.335370733333621,-0.315491445945434,-0.301165295210856,
-0.29723257379588,-0.293223461848749,-0.272774488137517,-0.252071366520374,
-0.239300846331472,-0.228798122014357,-0.224502765173222,-0.203198222803892,
-0.200833918205808,-0.180346956049432,-0.158306875253142,-0.154304247957037,
-0.150804929022692,-0.129421873498757,-0.107501185980079,-0.0856211676534625,
-0.079697906231664,-0.0759421505311957,-0.0534088813988902,-0.0309855250275342,
-0.00876395290387212,-0.00402630967910949,-3.65615898988344E-5),
 .UNSPECIFIED.);
#2961=B_SPLINE_CURVE_WITH_KNOTS('',3,(#133032,#133033,#133034,#133035),
 .UNSPECIFIED.,.F.,.F.,(4,4),(-0.0152759716381044,0.),.UNSPECIFIED.);
#2962=B_SPLINE_CURVE_WITH_KNOTS('',3,(#133036,#133037,#133038,#133039,#133040,
#133041,#133042,#133043,#133044,#133045,#133046,#133047,#133048,#133049,
#133050,#133051,#133052,#133053,#133054,#133055,#133056,#133057,#133058,
#133059,#133060,#133061,#133062,#133063,#133064,#133065,#133066,#133067,
#133068,#133069,#133070,#133071,#133072,#133073,#133074,#133075,#133076,
#133077,#133078,#133079,#133080,#133081,#133082,#133083,#133084,#133085,
#133086,#133087,#133088,#133089,#133090,#133091,#133092,#133093,#133094,
#133095,#133096,#133097,#133098,#133099,#133100,#133101,#133102,#133103,
#133104,#133105,#133106,#133107,#133108,#133109,#133110,#133111,#133112,
#133113,#133114,#133115,#133116,#133117,#133118,#133119,#133120),
 .UNSPECIFIED.,.F.,.F.,(4,3,3,3,3,3,3,3,3,3,3,3,3,3,3,3,3,3,3,3,3,3,3,3,
3,3,3,3,4),(0.,0.0220793683187804,0.0446533402441453,0.0636210331214285,
0.0720970319424637,0.0767544326890563,0.0810485639074834,0.102973109377672,
0.124771319639633,0.142868280227078,0.150423140460159,0.153919004023562,
0.157566869486277,0.17833745054201,0.197159161989412,0.21943067529714,0.224333068719436,
0.229400005005982,0.250090151731939,0.270725926661941,0.285677006128735,
0.29689344012605,0.300623371473114,0.320444582327625,0.334304749326293,
0.338770888038792,0.357795589733676,0.375331268451236,0.378621596831424),
 .UNSPECIFIED.);
#2963=B_SPLINE_CURVE_WITH_KNOTS('',3,(#133502,#133503,#133504,#133505,#133506,
#133507,#133508,#133509,#133510,#133511,#133512,#133513,#133514,#133515,
#133516,#133517,#133518,#133519,#133520,#133521,#133522,#133523,#133524,
#133525,#133526,#133527,#133528,#133529,#133530,#133531,#133532,#133533,
#133534,#133535,#133536,#133537,#133538,#133539,#133540,#133541,#133542,
#133543,#133544,#133545,#133546,#133547,#133548,#133549,#133550,#133551,
#133552,#133553,#133554,#133555,#133556,#133557,#133558,#133559,#133560,
#133561,#133562,#133563,#133564,#133565,#133566,#133567,#133568,#133569,
#133570,#133571,#133572,#133573,#133574,#133575,#133576,#133577,#133578,
#133579,#133580,#133581,#133582,#133583,#133584,#133585,#133586),
 .UNSPECIFIED.,.F.,.F.,(4,3,3,3,3,3,3,3,3,3,3,3,3,3,3,3,3,3,3,3,3,3,3,3,
3,3,3,3,4),(-0.376940817211642,-0.35463389721075,-0.332912065106493,-0.328063703915442,
-0.305815101391439,-0.290195618764596,-0.284258166436133,-0.278600681034138,
-0.256938276420847,-0.235773098280606,-0.214948067698175,-0.208200326246104,
-0.204401454712377,-0.183825515521996,-0.180859240376695,-0.159772587429043,
-0.140301766028677,-0.136001542949448,-0.132615024954702,-0.112162993959112,
-0.0919266612212684,-0.0718621053887858,-0.066072166338472,-0.0628432204529464,
-0.0432905357930386,-0.0240214863956556,-0.00475243699827259,-0.00327832057784904,
0.),.UNSPECIFIED.);
#2964=B_SPLINE_CURVE_WITH_KNOTS('',3,(#133587,#133588,#133589,#133590,#133591,
#133592,#133593,#133594,#133595,#133596,#133597,#133598,#133599,#133600,
#133601,#133602,#133603,#133604,#133605,#133606,#133607,#133608,#133609,
#133610,#133611,#133612,#133613,#133614,#133615,#133616,#133617,#133618,
#133619,#133620,#133621,#133622,#133623,#133624,#133625,#133626,#133627,
#133628,#133629,#133630,#133631,#133632,#133633,#133634,#133635,#133636,
#133637,#133638,#133639,#133640,#133641,#133642,#133643,#133644,#133645,
#133646,#133647,#133648,#133649,#133650,#133651,#133652,#133653,#133654,
#133655,#133656,#133657,#133658,#133659,#133660,#133661,#133662,#133663,
#133664,#133665,#133666,#133667,#133668),.UNSPECIFIED.,.F.,.F.,(4,3,3,3,
3,3,3,3,3,3,3,3,3,3,3,3,3,3,3,3,3,3,3,3,3,3,3,4),(0.,0.0186893924207011,
0.0380629085124009,0.0557706391965121,0.064474053792627,0.0684512605343887,
0.0885059134327574,0.108970690515085,0.125987250609254,0.133851921051149,
0.137286474827157,0.158361299681457,0.177200852458622,0.197728337128931,
0.20565102804809,0.209126189226868,0.230374857434889,0.25162352564291,0.268072644125497,
0.278312082409732,0.284045428046126,0.306314404619063,0.322968579623693,
0.328170228633061,0.33318354273328,0.355704945255065,0.372931104637582,
0.376894629338845),.UNSPECIFIED.);
#2965=B_SPLINE_CURVE_WITH_KNOTS('',3,(#133669,#133670,#133671,#133672),
 .UNSPECIFIED.,.F.,.F.,(4,4),(0.,0.015233203817751),.UNSPECIFIED.);
#2966=B_SPLINE_CURVE_WITH_KNOTS('',3,(#134053,#134054,#134055,#134056,#134057,
#134058,#134059,#134060,#134061,#134062,#134063,#134064,#134065,#134066,
#134067,#134068,#134069,#134070,#134071,#134072,#134073,#134074,#134075,
#134076,#134077,#134078,#134079,#134080,#134081,#134082,#134083,#134084,
#134085,#134086,#134087,#134088,#134089,#134090,#134091,#134092,#134093,
#134094,#134095,#134096,#134097,#134098,#134099,#134100,#134101,#134102,
#134103,#134104,#134105,#134106,#134107,#134108,#134109,#134110,#134111,
#134112,#134113,#134114,#134115,#134116,#134117,#134118,#134119,#134120,
#134121,#134122,#134123,#134124,#134125,#134126,#134127,#134128,#134129,
#134130,#134131,#134132,#134133,#134134,#134135,#134136,#134137,#134138,
#134139,#134140),.UNSPECIFIED.,.F.,.F.,(4,3,3,3,3,3,3,3,3,3,3,3,3,3,3,3,
3,3,3,3,3,3,3,3,3,3,3,3,3,4),(-0.378621596831399,-0.359796906651946,-0.347856895762323,
-0.339695845366797,-0.335370634830925,-0.315498242912406,-0.301165202324081,
-0.29723236113593,-0.293223432251235,-0.272820719782585,-0.252123121204613,
-0.239300820454911,-0.228798083868718,-0.224502752790907,-0.20319821077641,
-0.200833918205805,-0.18034696156604,-0.158306880080173,-0.154304280740517,
-0.150804935247414,-0.12948390702316,-0.107552543701982,-0.0856211803808043,
-0.0801967363324338,-0.0759421583469307,-0.0533545697894654,-0.0308224381853329,
-0.00876396243776301,-0.00402630967910655,-3.65718562400641E-5),
 .UNSPECIFIED.);
#2967=B_SPLINE_CURVE_WITH_KNOTS('',3,(#134142,#134143,#134144,#134145),
 .UNSPECIFIED.,.F.,.F.,(4,4),(-0.0152760659177977,0.),.UNSPECIFIED.);
#2968=B_SPLINE_CURVE_WITH_KNOTS('',3,(#134146,#134147,#134148,#134149,#134150,
#134151,#134152,#134153,#134154,#134155,#134156,#134157,#134158,#134159,
#134160,#134161,#134162,#134163,#134164,#134165,#134166,#134167,#134168,
#134169,#134170,#134171,#134172,#134173,#134174,#134175,#134176,#134177,
#134178,#134179,#134180,#134181,#134182,#134183,#134184,#134185,#134186,
#134187,#134188,#134189,#134190,#134191,#134192,#134193,#134194,#134195,
#134196,#134197,#134198,#134199,#134200,#134201,#134202,#134203,#134204,
#134205,#134206,#134207,#134208,#134209,#134210,#134211,#134212,#134213,
#134214,#134215,#134216,#134217,#134218,#134219,#134220,#134221,#134222,
#134223,#134224,#134225,#134226,#134227,#134228,#134229,#134230),
 .UNSPECIFIED.,.F.,.F.,(4,3,3,3,3,3,3,3,3,3,3,3,3,3,3,3,3,3,3,3,3,3,3,3,
3,3,3,3,4),(0.,0.0220793746690922,0.0446533474471028,0.0636210397963064,
0.0720970339368394,0.0767544369062487,0.0810485650370603,0.102995575329966,
0.124601454003273,0.14286827936694,0.150423140796222,0.153919006124083,
0.157566870163833,0.178337449110706,0.197159161989394,0.219430675297117,
0.224333068139837,0.229400004999726,0.25009015204505,0.270725926647151,
0.285676999682712,0.296893429032277,0.300623368319006,0.320395536074228,
0.334304739895041,0.338770879251483,0.357795576917732,0.375331268451179,
0.378621596831367),.UNSPECIFIED.);
#2969=B_SPLINE_CURVE_WITH_KNOTS('',3,(#134612,#134613,#134614,#134615,#134616,
#134617,#134618,#134619,#134620,#134621,#134622,#134623,#134624,#134625,
#134626,#134627,#134628,#134629,#134630,#134631,#134632,#134633,#134634,
#134635,#134636,#134637,#134638,#134639,#134640,#134641,#134642,#134643,
#134644,#134645,#134646,#134647,#134648,#134649,#134650,#134651,#134652,
#134653,#134654,#134655,#134656,#134657,#134658,#134659,#134660,#134661,
#134662,#134663,#134664,#134665,#134666,#134667,#134668,#134669,#134670,
#134671,#134672,#134673,#134674,#134675,#134676,#134677,#134678,#134679,
#134680,#134681,#134682,#134683,#134684,#134685,#134686,#134687,#134688,
#134689,#134690,#134691,#134692,#134693,#134694,#134695,#134696),
 .UNSPECIFIED.,.F.,.F.,(4,3,3,3,3,3,3,3,3,3,3,3,3,3,3,3,3,3,3,3,3,3,3,3,
3,3,3,3,4),(-0.376940817211701,-0.35463544655944,-0.332913420786601,-0.328065270514049,
-0.305816652822842,-0.290196976267078,-0.284261180291901,-0.278600481960197,
-0.25691711770642,-0.235699073322327,-0.214946538919852,-0.208201321496629,
-0.204401317171364,-0.183824744173427,-0.180859240376724,-0.159876540755593,
-0.140301763233375,-0.136000503582363,-0.132614278284648,-0.11215519219308,
-0.0917900641439051,-0.0718604732108804,-0.066067545564457,-0.0628420724025775,
-0.0432965324819232,-0.0232874265298861,-0.00474996033762646,-0.00327832057784897,
0.),.UNSPECIFIED.);
#2970=B_SPLINE_CURVE_WITH_KNOTS('',3,(#134697,#134698,#134699,#134700,#134701,
#134702,#134703,#134704,#134705,#134706,#134707,#134708,#134709,#134710,
#134711,#134712,#134713,#134714,#134715,#134716,#134717,#134718,#134719,
#134720,#134721,#134722,#134723,#134724,#134725,#134726,#134727,#134728,
#134729,#134730,#134731,#134732,#134733,#134734,#134735,#134736,#134737,
#134738,#134739,#134740,#134741,#134742,#134743,#134744,#134745,#134746,
#134747,#134748,#134749,#134750,#134751,#134752,#134753,#134754,#134755,
#134756,#134757,#134758,#134759,#134760,#134761,#134762,#134763,#134764,
#134765,#134766,#134767,#134768,#134769,#134770,#134771,#134772,#134773,
#134774,#134775,#134776,#134777,#134778),.UNSPECIFIED.,.F.,.F.,(4,3,3,3,
3,3,3,3,3,3,3,3,3,3,3,3,3,3,3,3,3,3,3,3,3,3,3,4),(0.,0.0185955873360213,
0.0384212454763452,0.0557686963491286,0.0644706897478566,0.0684503846967035,
0.088503222386054,0.108967755523642,0.1259846405568,0.133847808883134,0.137284316290468,
0.158359366945259,0.177200852458612,0.197729598395159,0.205651689526663,
0.20912665907553,0.230133427396579,0.251626259267865,0.268071993510044,
0.278310573550478,0.284045805095789,0.306314875310516,0.322968932642282,
0.328170988094391,0.333183924524744,0.355705311564313,0.372931104637579,
0.376894576726578),.UNSPECIFIED.);
#2971=B_SPLINE_CURVE_WITH_KNOTS('',3,(#134779,#134780,#134781,#134782),
 .UNSPECIFIED.,.F.,.F.,(4,4),(0.,0.0152452198817276),.UNSPECIFIED.);
#2972=B_SPLINE_CURVE_WITH_KNOTS('',3,(#135163,#135164,#135165,#135166,#135167,
#135168,#135169,#135170,#135171,#135172,#135173,#135174,#135175,#135176,
#135177,#135178,#135179,#135180,#135181,#135182,#135183,#135184,#135185,
#135186,#135187,#135188,#135189,#135190,#135191,#135192,#135193,#135194,
#135195,#135196,#135197,#135198,#135199,#135200,#135201,#135202,#135203,
#135204,#135205,#135206,#135207,#135208,#135209,#135210,#135211,#135212,
#135213,#135214,#135215,#135216,#135217,#135218,#135219,#135220,#135221,
#135222,#135223,#135224,#135225,#135226,#135227,#135228,#135229,#135230,
#135231,#135232,#135233,#135234,#135235,#135236,#135237,#135238,#135239,
#135240,#135241,#135242,#135243,#135244,#135245,#135246,#135247,#135248,
#135249,#135250),.UNSPECIFIED.,.F.,.F.,(4,3,3,3,3,3,3,3,3,3,3,3,3,3,3,3,
3,3,3,3,3,3,3,3,3,3,3,3,3,4),(-0.378621596831381,-0.359799334642644,-0.347863072493078,
-0.339751236649128,-0.335397642749941,-0.315527515100311,-0.3011908154885,
-0.297290501565233,-0.293230948264074,-0.27282995282436,-0.252132128052805,
-0.23930757559106,-0.228808049628064,-0.224505962571255,-0.203201329216816,
-0.200833918205823,-0.17956968323802,-0.158305448270218,-0.154294547940623,
-0.150803075770128,-0.129418690026976,-0.10758400477419,-0.0856173806055649,
-0.0801901203801154,-0.0759398217123878,-0.0533520823575455,-0.0308198729383457,
-0.00876113397239242,-0.00402630967911263,-3.42586534900411E-5),
 .UNSPECIFIED.);
#2973=B_SPLINE_CURVE_WITH_KNOTS('',3,(#135252,#135253,#135254,#135255),
 .UNSPECIFIED.,.F.,.F.,(4,4),(-0.015294280875507,0.),.UNSPECIFIED.);
#2974=B_SPLINE_CURVE_WITH_KNOTS('',3,(#135256,#135257,#135258,#135259,#135260,
#135261,#135262,#135263,#135264,#135265,#135266,#135267,#135268,#135269,
#135270,#135271,#135272,#135273,#135274,#135275,#135276,#135277,#135278,
#135279,#135280,#135281,#135282,#135283,#135284,#135285,#135286,#135287,
#135288,#135289,#135290,#135291,#135292,#135293,#135294,#135295,#135296,
#135297,#135298,#135299,#135300,#135301,#135302,#135303,#135304,#135305,
#135306,#135307,#135308,#135309,#135310,#135311,#135312,#135313,#135314,
#135315,#135316,#135317,#135318,#135319,#135320,#135321,#135322,#135323,
#135324,#135325,#135326,#135327,#135328,#135329,#135330,#135331,#135332,
#135333,#135334,#135335,#135336,#135337,#135338,#135339,#135340),
 .UNSPECIFIED.,.F.,.F.,(4,3,3,3,3,3,3,3,3,3,3,3,3,3,3,3,3,3,3,3,3,3,3,3,
3,3,3,3,4),(0.,0.0219645252128417,0.044541845696888,0.0636190102334506,
0.0720964280805716,0.076753153335081,0.0810482200245811,0.102994855000476,
0.124771637962689,0.142868518969364,0.150423017612877,0.153918288000301,
0.157566649003441,0.178337855554218,0.197159161989389,0.219430675297114,
0.224333226672903,0.229400011405901,0.250090054224483,0.270725909831617,
0.285678847355051,0.296896590893469,0.300624275912145,0.320397170032721,
0.334307458733279,0.338773433419682,0.357799291046648,0.375331268451191,
0.378621596831382),.UNSPECIFIED.);
#2975=B_SPLINE_CURVE_WITH_KNOTS('',3,(#135722,#135723,#135724,#135725,#135726,
#135727,#135728,#135729,#135730,#135731,#135732,#135733,#135734,#135735,
#135736,#135737,#135738,#135739,#135740,#135741,#135742,#135743,#135744,
#135745,#135746,#135747,#135748,#135749,#135750,#135751,#135752,#135753,
#135754,#135755,#135756,#135757,#135758,#135759,#135760,#135761,#135762,
#135763,#135764,#135765,#135766,#135767,#135768,#135769,#135770,#135771,
#135772,#135773,#135774,#135775,#135776,#135777,#135778,#135779,#135780,
#135781,#135782,#135783,#135784,#135785,#135786,#135787,#135788,#135789,
#135790,#135791,#135792,#135793,#135794,#135795,#135796,#135797,#135798,
#135799,#135800,#135801,#135802,#135803,#135804,#135805,#135806),
 .UNSPECIFIED.,.F.,.F.,(4,3,3,3,3,3,3,3,3,3,3,3,3,3,3,3,3,3,3,3,3,3,3,3,
3,3,3,3,4),(-0.376940817211664,-0.354635449587131,-0.33291342343583,-0.328065273459223,
-0.305816655761636,-0.290196978838522,-0.28426118601974,-0.278600481540187,
-0.256993860807461,-0.235699071189167,-0.214946535975349,-0.208201323450052,
-0.204401316925529,-0.183824742722166,-0.180859240376722,-0.159876540758328,
-0.140301763235768,-0.136000501696498,-0.132614276957988,-0.112155191085992,
-0.0917900627476849,-0.0718604703137309,-0.0660675372545504,-0.0628420703116484,
-0.0432965295468417,-0.0232874250623442,-0.00474995575000378,-0.00327832057784658,
0.),.UNSPECIFIED.);
#2976=B_SPLINE_CURVE_WITH_KNOTS('',3,(#135807,#135808,#135809,#135810,#135811,
#135812,#135813,#135814,#135815,#135816,#135817,#135818,#135819,#135820,
#135821,#135822,#135823,#135824,#135825,#135826,#135827,#135828,#135829,
#135830,#135831,#135832,#135833,#135834,#135835,#135836,#135837,#135838,
#135839,#135840,#135841,#135842,#135843,#135844,#135845,#135846,#135847,
#135848,#135849,#135850,#135851,#135852,#135853,#135854,#135855,#135856,
#135857,#135858,#135859,#135860,#135861,#135862,#135863,#135864,#135865,
#135866,#135867,#135868,#135869,#135870,#135871,#135872,#135873,#135874,
#135875,#135876,#135877,#135878,#135879,#135880,#135881,#135882,#135883,
#135884,#135885,#135886,#135887,#135888),.UNSPECIFIED.,.F.,.F.,(4,3,3,3,
3,3,3,3,3,3,3,3,3,3,3,3,3,3,3,3,3,3,3,3,3,3,3,4),(0.,0.0185955823964664,
0.038421241154236,0.0557686925672843,0.0644706831960225,0.0684503830038135,
0.0885032171437632,0.108912563113654,0.125984635449896,0.1338478008296,
0.137284312079196,0.158359363131109,0.177200852458623,0.197729600808643,
0.205651690758548,0.209126659942652,0.2301334310946,0.251648890514138,0.268071992223651,
0.278310570548695,0.284045805818415,0.306303539327454,0.322968933321467,
0.328170989556339,0.333183925255598,0.355705312250232,0.372931104637538,
0.376894576477768),.UNSPECIFIED.);
#2977=B_SPLINE_CURVE_WITH_KNOTS('',3,(#135889,#135890,#135891,#135892),
 .UNSPECIFIED.,.F.,.F.,(4,4),(0.,0.0152452936035568),.UNSPECIFIED.);
#2978=B_SPLINE_CURVE_WITH_KNOTS('',3,(#136273,#136274,#136275,#136276,#136277,
#136278,#136279,#136280,#136281,#136282,#136283,#136284,#136285,#136286,
#136287,#136288,#136289,#136290,#136291,#136292,#136293,#136294,#136295,
#136296,#136297,#136298,#136299,#136300,#136301,#136302,#136303,#136304,
#136305,#136306,#136307,#136308,#136309,#136310,#136311,#136312,#136313,
#136314,#136315,#136316,#136317,#136318,#136319,#136320,#136321,#136322,
#136323,#136324,#136325,#136326,#136327,#136328,#136329,#136330,#136331,
#136332,#136333,#136334,#136335,#136336,#136337,#136338,#136339,#136340,
#136341,#136342,#136343,#136344,#136345,#136346,#136347,#136348,#136349,
#136350,#136351,#136352,#136353,#136354,#136355,#136356,#136357,#136358,
#136359,#136360),.UNSPECIFIED.,.F.,.F.,(4,3,3,3,3,3,3,3,3,3,3,3,3,3,3,3,
3,3,3,3,3,3,3,3,3,3,3,3,3,4),(-0.378621596831333,-0.359799340993963,-0.347863088648493,
-0.339751380172106,-0.335397706196632,-0.315527584340703,-0.301190876073838,
-0.297290637950947,-0.29323096453051,-0.272829973526033,-0.252132148232715,
-0.239307590725982,-0.228808071982614,-0.224505969731213,-0.203201336186886,
-0.200833918205781,-0.180345321018525,-0.158305444601098,-0.154294522931056,
-0.150803070963683,-0.129418681789645,-0.107583994998281,-0.0856173707996288,
-0.0801901033259043,-0.0759398156227559,-0.0533919939915826,-0.0308198662669975,
-0.00876112667829501,-0.00402630967910949,-3.42547819880877E-5),
 .UNSPECIFIED.);
#2979=B_SPLINE_CURVE_WITH_KNOTS('',3,(#136362,#136363,#136364,#136365),
 .UNSPECIFIED.,.F.,.F.,(4,4),(-0.0152943911553443,0.),.UNSPECIFIED.);
#2980=B_SPLINE_CURVE_WITH_KNOTS('',3,(#136366,#136367,#136368,#136369,#136370,
#136371,#136372,#136373,#136374,#136375,#136376,#136377,#136378,#136379,
#136380,#136381,#136382,#136383,#136384,#136385,#136386,#136387,#136388,
#136389,#136390,#136391,#136392,#136393,#136394,#136395,#136396,#136397,
#136398,#136399,#136400,#136401,#136402,#136403,#136404,#136405,#136406,
#136407,#136408,#136409,#136410,#136411,#136412,#136413,#136414,#136415,
#136416,#136417,#136418,#136419,#136420,#136421,#136422,#136423,#136424,
#136425,#136426,#136427,#136428,#136429,#136430,#136431,#136432,#136433,
#136434,#136435,#136436,#136437,#136438,#136439,#136440,#136441,#136442,
#136443,#136444,#136445,#136446,#136447,#136448,#136449,#136450),
 .UNSPECIFIED.,.F.,.F.,(4,3,3,3,3,3,3,3,3,3,3,3,3,3,3,3,3,3,3,3,3,3,3,3,
3,3,3,3,4),(0.,0.0219645196906565,0.0445418395961537,0.0636190048953165,
0.0720964264886179,0.0767531499549516,0.0810482191086478,0.102973098393797,
0.124771638719259,0.142868519536808,0.150423017229364,0.153918285920911,
0.15756664838456,0.178337856551124,0.197159161989456,0.219430675297187,
0.224333227042281,0.229400011424028,0.250065016189275,0.270725909719807,
0.285678851884929,0.296896598603033,0.30062427815181,0.320397174054837,
0.334307465475236,0.338773439815346,0.357799300327208,0.375331268451302,
0.378621596831489),.UNSPECIFIED.);
#2981=B_SPLINE_CURVE_WITH_KNOTS('',3,(#136545,#136546,#136547,#136548,#136549,
#136550,#136551,#136552,#136553,#136554,#136555,#136556,#136557,#136558,
#136559,#136560,#136561,#136562,#136563,#136564,#136565,#136566,#136567,
#136568,#136569,#136570,#136571,#136572,#136573,#136574,#136575,#136576,
#136577,#136578,#136579,#136580,#136581,#136582,#136583,#136584,#136585,
#136586,#136587,#136588,#136589,#136590,#136591,#136592,#136593,#136594,
#136595,#136596,#136597,#136598,#136599,#136600,#136601,#136602,#136603,
#136604,#136605,#136606,#136607,#136608,#136609,#136610,#136611,#136612,
#136613,#136614,#136615,#136616,#136617,#136618,#136619,#136620,#136621,
#136622,#136623,#136624,#136625,#136626,#136627,#136628,#136629,#136630,
#136631,#136632,#136633,#136634,#136635,#136636,#136637,#136638,#136639,
#136640,#136641,#136642,#136643,#136644,#136645,#136646,#136647,#136648,
#136649,#136650,#136651,#136652,#136653,#136654,#136655,#136656,#136657,
#136658,#136659,#136660,#136661,#136662,#136663,#136664,#136665,#136666,
#136667,#136668,#136669,#136670,#136671,#136672,#136673,#136674,#136675,
#136676,#136677,#136678,#136679,#136680,#136681,#136682,#136683),
 .UNSPECIFIED.,.F.,.F.,(4,3,3,3,3,3,3,3,3,3,3,3,3,3,3,3,3,3,3,3,3,3,3,3,
3,3,3,3,3,3,3,3,3,3,3,3,3,3,3,3,3,3,3,3,3,3,4),(309.542368439887,309.617837246006,
309.693300130921,309.768771534012,309.844299671964,309.919858116417,309.995504346128,
310.047433937301,310.124855595317,310.202216043453,310.279528349287,310.356805768718,
310.434062635597,310.511320314385,310.545902480609,310.632946223822,310.720200992735,
310.807667881397,310.895195896758,310.982729265011,311.044371023916,311.12037421906,
311.196328916559,311.272249437817,311.34816006007,311.424064195079,311.499995258205,
311.542839567224,311.626842158064,311.710897899939,311.795011601748,311.879134544641,
311.963255773904,312.041308110531,312.120017789723,312.198698595032,312.277361399118,
312.356028358848,312.434696723513,312.513392268518,312.539776653839,312.621199463373,
312.702612292933,312.786520518987,312.867924569884,312.953084883516,313.038245197147),
 .UNSPECIFIED.);
#2982=B_SPLINE_CURVE_WITH_KNOTS('',3,(#136691,#136692,#136693,#136694,#136695,
#136696,#136697,#136698,#136699,#136700,#136701,#136702,#136703,#136704,
#136705,#136706,#136707,#136708,#136709,#136710,#136711,#136712,#136713,
#136714,#136715,#136716,#136717,#136718,#136719,#136720,#136721,#136722,
#136723,#136724,#136725,#136726,#136727,#136728,#136729,#136730,#136731,
#136732,#136733,#136734,#136735,#136736,#136737,#136738,#136739,#136740,
#136741,#136742,#136743,#136744,#136745,#136746,#136747,#136748,#136749,
#136750,#136751,#136752,#136753,#136754,#136755,#136756,#136757,#136758,
#136759,#136760,#136761,#136762,#136763,#136764,#136765,#136766,#136767,
#136768,#136769,#136770,#136771,#136772,#136773,#136774,#136775,#136776,
#136777,#136778,#136779,#136780,#136781,#136782,#136783,#136784,#136785,
#136786,#136787,#136788,#136789,#136790,#136791,#136792,#136793,#136794,
#136795,#136796,#136797,#136798,#136799,#136800,#136801,#136802,#136803,
#136804,#136805,#136806,#136807,#136808,#136809,#136810,#136811,#136812,
#136813,#136814,#136815,#136816,#136817,#136818,#136819,#136820,#136821,
#136822,#136823,#136824,#136825,#136826,#136827,#136828,#136829,#136830,
#136831,#136832,#136833,#136834,#136835,#136836,#136837,#136838,#136839,
#136840,#136841,#136842,#136843,#136844,#136845,#136846,#136847,#136848,
#136849,#136850,#136851,#136852,#136853,#136854,#136855,#136856,#136857,
#136858,#136859,#136860,#136861,#136862,#136863,#136864,#136865,#136866,
#136867,#136868,#136869,#136870,#136871,#136872,#136873,#136874,#136875,
#136876,#136877,#136878,#136879,#136880,#136881,#136882,#136883,#136884,
#136885,#136886,#136887,#136888,#136889,#136890,#136891,#136892,#136893,
#136894,#136895,#136896,#136897,#136898),.UNSPECIFIED.,.F.,.F.,(4,3,3,3,
3,3,3,3,3,3,3,3,3,3,3,3,3,3,3,3,3,3,3,3,3,3,3,3,3,3,3,3,3,3,3,3,3,3,3,3,
3,3,3,3,3,3,3,3,3,3,3,3,3,3,3,3,3,3,3,3,3,3,3,3,3,3,3,3,3,4),(-311.017671895807,
-310.930926646246,-310.844202256897,-310.757594142418,-310.671098411025,
-310.584828273228,-310.545902480609,-310.468642660336,-310.391385417305,
-310.31411775789,-310.236797613467,-310.159447861164,-310.082022859537,
-310.047433937301,-309.970550488847,-309.89373679842,-309.816977853812,
-309.740258681202,-309.663564335473,-309.586862252401,-309.510152478292,
-309.433421487568,-309.35665574544,-309.279790647613,-309.202874370491,
-309.125827334062,-309.050496850686,-308.973403311115,-308.896408861735,
-308.81949842116,-308.742656966525,-308.665869522965,-308.589119125357,
-308.512388285924,-308.435663509342,-308.358931306155,-308.282142911163,
-308.205326891268,-308.128419642196,-308.053559764071,-307.976213241289,
-307.898927080985,-307.821688129199,-307.744482426365,-307.667296324788,
-307.590107731801,-307.555091220763,-307.467982168516,-307.38066246706,
-307.293133530895,-307.205545994981,-307.117958806829,-307.056622677456,
-306.980361985978,-306.904149705518,-306.82797170016,-306.75180442684,-306.675644014599,
-306.599458179872,-306.558154134148,-306.475731516247,-306.393279662411,
-306.309881144518,-306.227367701055,-306.143526645948,-306.059685590841,
-305.977675857624,-305.895686555633,-305.813720207621,-305.801967534929),
 .UNSPECIFIED.);
#2983=B_SPLINE_CURVE_WITH_KNOTS('',3,(#136904,#136905,#136906,#136907,#136908,
#136909,#136910,#136911,#136912,#136913,#136914,#136915,#136916,#136917,
#136918,#136919,#136920,#136921,#136922,#136923,#136924,#136925,#136926,
#136927,#136928,#136929,#136930,#136931,#136932,#136933,#136934,#136935,
#136936,#136937,#136938,#136939,#136940,#136941,#136942,#136943,#136944,
#136945,#136946,#136947,#136948,#136949,#136950,#136951,#136952,#136953,
#136954,#136955,#136956,#136957,#136958,#136959,#136960,#136961,#136962,
#136963,#136964,#136965,#136966,#136967,#136968,#136969,#136970,#136971,
#136972,#136973,#136974,#136975,#136976,#136977,#136978,#136979,#136980,
#136981,#136982,#136983,#136984,#136985,#136986,#136987,#136988,#136989,
#136990,#136991,#136992,#136993,#136994,#136995,#136996,#136997,#136998,
#136999,#137000,#137001,#137002,#137003,#137004,#137005,#137006,#137007,
#137008,#137009,#137010,#137011,#137012,#137013,#137014,#137015,#137016,
#137017,#137018,#137019,#137020,#137021,#137022,#137023,#137024,#137025,
#137026,#137027,#137028,#137029,#137030,#137031,#137032,#137033,#137034,
#137035,#137036,#137037,#137038,#137039,#137040,#137041,#137042,#137043,
#137044,#137045,#137046,#137047,#137048,#137049,#137050,#137051,#137052,
#137053,#137054,#137055,#137056,#137057,#137058,#137059,#137060,#137061,
#137062,#137063,#137064,#137065,#137066,#137067,#137068,#137069,#137070,
#137071,#137072,#137073,#137074,#137075,#137076,#137077,#137078,#137079,
#137080,#137081,#137082,#137083,#137084,#137085,#137086,#137087,#137088,
#137089,#137090,#137091,#137092,#137093,#137094,#137095,#137096,#137097,
#137098,#137099,#137100,#137101,#137102,#137103,#137104,#137105,#137106,
#137107,#137108,#137109,#137110,#137111,#137112,#137113,#137114,#137115,
#137116,#137117,#137118,#137119,#137120,#137121,#137122,#137123,#137124,
#137125,#137126,#137127,#137128,#137129,#137130,#137131,#137132,#137133,
#137134,#137135),.UNSPECIFIED.,.F.,.F.,(4,3,3,3,3,3,3,3,3,3,3,3,3,3,3,3,
3,3,3,3,3,3,3,3,3,3,3,3,3,3,3,3,3,3,3,3,3,3,3,3,3,3,3,3,3,3,3,3,3,3,3,3,
3,3,3,3,3,3,3,3,3,3,3,3,3,3,3,3,3,3,3,3,3,3,3,3,3,4),(303.258525738749,
303.337437675126,303.41630459851,303.497492950898,303.576309928053,303.655119327753,
303.73393166642,303.816901604217,303.895777069118,303.974680900916,304.053645652013,
304.06581141761,304.139959257083,304.214049984434,304.288098768055,304.362129722208,
304.436148605976,304.510192013303,304.564279960918,304.655011624552,304.746226212929,
304.837868512921,304.929604166686,305.021232905757,305.062748504226,305.138664739202,
305.214531642008,305.290363594904,305.366184709726,305.441998765712,305.517839199806,
305.561217047533,305.643117176767,305.725038259918,305.808700092649,305.890676262575,
305.975180926708,306.059685590841,306.142226387424,306.224750819407,306.308101648092,
306.390576093353,306.47436511375,306.558154134148,306.634340306684,306.71050467673,
306.786661344806,306.862847287711,306.939049130345,307.015310892414,307.056622677456,
307.144203357248,307.231804230285,307.319316613453,307.406720170908,307.493865126369,
307.555091220763,307.63228178972,307.709468444206,307.786664267124,307.863911006084,
307.941186435182,308.018536116409,308.053559764071,308.130473946048,308.207318862647,
308.284109489602,308.36086076461,308.43758759697,308.514322633225,308.591065641076,
308.667830114684,308.744629557554,308.821528507859,308.898478773299,308.97555968571,
309.050496850686,309.185189742936),.UNSPECIFIED.);
#2984=B_SPLINE_CURVE_WITH_KNOTS('',3,(#137136,#137137,#137138,#137139,#137140,
#137141,#137142,#137143,#137144,#137145,#137146,#137147,#137148,#137149,
#137150,#137151),.UNSPECIFIED.,.F.,.F.,(4,3,3,3,3,4),(309.18518974306,309.260920311614,
309.33654607352,309.412111555631,309.487623538129,309.542368439887),
 .UNSPECIFIED.);
#2985=B_SPLINE_CURVE_WITH_KNOTS('',3,(#137153,#137154,#137155,#137156,#137157,
#137158,#137159,#137160,#137161,#137162,#137163,#137164,#137165,#137166,
#137167,#137168),.UNSPECIFIED.,.F.,.F.,(4,3,3,3,3,4),(-305.801967534929,
-305.720030109092,-305.638119567349,-305.561217047533,-305.48132141018,
-305.44595019883),.UNSPECIFIED.);
#2986=B_SPLINE_CURVE_WITH_KNOTS('',3,(#137169,#137170,#137171,#137172,#137173,
#137174,#137175,#137176,#137177,#137178,#137179,#137180,#137181,#137182,
#137183,#137184,#137185,#137186,#137187,#137188,#137189,#137190,#137191,
#137192,#137193,#137194,#137195,#137196,#137197,#137198,#137199,#137200,
#137201,#137202,#137203,#137204,#137205,#137206,#137207,#137208,#137209,
#137210,#137211,#137212,#137213,#137214,#137215,#137216,#137217,#137218,
#137219,#137220,#137221,#137222,#137223,#137224,#137225,#137226,#137227,
#137228,#137229,#137230,#137231,#137232,#137233,#137234,#137235,#137236,
#137237,#137238,#137239,#137240,#137241,#137242,#137243,#137244,#137245,
#137246,#137247,#137248,#137249,#137250,#137251,#137252,#137253,#137254,
#137255,#137256,#137257,#137258,#137259,#137260,#137261,#137262,#137263,
#137264,#137265,#137266,#137267,#137268,#137269,#137270,#137271,#137272,
#137273,#137274,#137275,#137276,#137277,#137278,#137279,#137280,#137281,
#137282,#137283,#137284,#137285,#137286,#137287,#137288,#137289,#137290,
#137291,#137292,#137293,#137294,#137295,#137296,#137297,#137298,#137299,
#137300,#137301,#137302,#137303,#137304,#137305,#137306,#137307,#137308,
#137309,#137310,#137311,#137312,#137313,#137314,#137315,#137316,#137317,
#137318,#137319,#137320,#137321,#137322,#137323,#137324,#137325,#137326,
#137327,#137328,#137329,#137330,#137331,#137332,#137333,#137334,#137335,
#137336,#137337,#137338,#137339,#137340,#137341,#137342,#137343,#137344,
#137345,#137346,#137347,#137348,#137349,#137350,#137351,#137352,#137353,
#137354,#137355,#137356,#137357,#137358,#137359,#137360,#137361,#137362,
#137363,#137364,#137365,#137366,#137367,#137368,#137369,#137370,#137371,
#137372,#137373,#137374,#137375,#137376,#137377,#137378,#137379,#137380,
#137381,#137382,#137383,#137384,#137385,#137386,#137387,#137388,#137389,
#137390,#137391,#137392,#137393,#137394,#137395,#137396,#137397,#137398,
#137399,#137400,#137401,#137402,#137403,#137404,#137405,#137406),
 .UNSPECIFIED.,.F.,.F.,(4,3,3,3,3,3,3,3,3,3,3,3,3,3,3,3,3,3,3,3,3,3,3,3,
3,3,3,3,3,3,3,3,3,3,3,3,3,3,3,3,3,3,3,3,3,3,3,3,3,3,3,3,3,3,3,3,3,3,3,3,
3,3,3,3,3,3,3,3,3,3,3,3,3,3,3,3,3,3,3,4),(-305.445950198753,-305.370428452089,
-305.293508465123,-305.217956252189,-305.140352378208,-305.062748504226,
-304.971128629841,-304.879391811904,-304.787810304948,-304.696471890485,
-304.605715271465,-304.564279960918,-304.490236908474,-304.416214556437,
-304.342197836222,-304.268143336115,-304.194069814163,-304.119922631049,
-304.06581141761,-303.986854587823,-303.907951856808,-303.829091603746,
-303.750262240707,-303.671452204277,-303.592635952831,-303.513814364812,
-303.434976919948,-303.35611308886,-303.27717612643,-303.198200446288,-303.119134467816,
-303.068874330995,-302.989891304843,-302.911008376975,-302.832214947182,
-302.753523689414,-302.674892927008,-302.596325213187,-302.570405787688,
-302.491812168687,-302.413168932538,-302.334465713034,-302.255644268394,
-302.176755320595,-302.097744603891,-302.07193724438,-301.992866686455,
-301.913869133847,-301.834932901509,-301.756046350948,-301.677197881843,
-301.598371488275,-301.519557236236,-301.440744613705,-301.3619231109,-301.283055184286,
-301.204163620468,-301.125205184055,-301.075000157765,-301.000893610658,
-300.926844006196,-300.85283616429,-300.778845802293,-300.704867345413,
-300.630863971717,-300.576531614458,-300.485533066705,-300.394030439515,
-300.302087508411,-300.210053528992,-300.118144990757,-300.07806307115,
-300.002353717235,-299.926693034302,-299.851066514759,-299.775449141077,
-299.699837964776,-299.624198364613,-299.579594527842,-299.519174510177),
 .UNSPECIFIED.);
#2987=B_SPLINE_CURVE_WITH_KNOTS('',3,(#137412,#137413,#137414,#137415,#137416,
#137417,#137418,#137419,#137420,#137421,#137422,#137423,#137424,#137425,
#137426,#137427,#137428,#137429,#137430,#137431,#137432,#137433,#137434,
#137435,#137436,#137437,#137438,#137439,#137440,#137441,#137442,#137443,
#137444,#137445,#137446,#137447,#137448,#137449,#137450,#137451,#137452,
#137453,#137454,#137455,#137456,#137457,#137458,#137459,#137460,#137461,
#137462,#137463,#137464,#137465,#137466,#137467,#137468,#137469,#137470,
#137471,#137472,#137473,#137474,#137475,#137476,#137477,#137478,#137479,
#137480,#137481,#137482,#137483,#137484,#137485,#137486,#137487,#137488,
#137489,#137490,#137491,#137492,#137493,#137494,#137495,#137496,#137497,
#137498,#137499,#137500,#137501,#137502,#137503,#137504,#137505,#137506,
#137507,#137508,#137509,#137510,#137511,#137512,#137513,#137514,#137515,
#137516,#137517,#137518,#137519,#137520,#137521,#137522,#137523,#137524,
#137525,#137526,#137527,#137528,#137529,#137530,#137531,#137532,#137533,
#137534,#137535,#137536,#137537,#137538,#137539,#137540,#137541,#137542,
#137543,#137544,#137545,#137546,#137547,#137548,#137549,#137550,#137551,
#137552,#137553,#137554,#137555,#137556,#137557,#137558,#137559,#137560,
#137561,#137562,#137563,#137564,#137565,#137566,#137567,#137568,#137569,
#137570,#137571,#137572,#137573,#137574,#137575,#137576,#137577,#137578,
#137579,#137580,#137581,#137582,#137583,#137584,#137585,#137586,#137587,
#137588,#137589,#137590,#137591,#137592,#137593,#137594,#137595,#137596,
#137597,#137598,#137599,#137600,#137601,#137602,#137603,#137604,#137605,
#137606,#137607,#137608,#137609,#137610,#137611,#137612,#137613,#137614,
#137615,#137616,#137617,#137618,#137619,#137620,#137621,#137622,#137623,
#137624,#137625,#137626,#137627,#137628,#137629,#137630,#137631,#137632,
#137633,#137634,#137635,#137636,#137637,#137638,#137639,#137640,#137641,
#137642,#137643,#137644,#137645,#137646,#137647,#137648,#137649),
 .UNSPECIFIED.,.F.,.F.,(4,3,3,3,3,3,3,3,3,3,3,3,3,3,3,3,3,3,3,3,3,3,3,3,
3,3,3,3,3,3,3,3,3,3,3,3,3,3,3,3,3,3,3,3,3,3,3,3,3,3,3,3,3,3,3,3,3,3,3,3,
3,3,3,3,3,3,3,3,3,3,3,3,3,3,3,3,3,3,3,4),(296.975200039958,297.060326286647,
297.087251811305,297.16135726261,297.235405773649,297.309412524818,297.383401802076,
297.457379176772,297.53138147581,297.585720354612,297.676719322946,297.768222397986,
297.860165787089,297.952200215175,298.044109164971,298.08418889792,298.159898714145,
298.235559860927,298.311186845588,298.386804685189,298.462416328099,298.538056394279,
298.582657441227,298.664935798978,298.747237943652,298.830709953873,298.913064491648,
298.997095238091,299.081125984535,299.16350559355,299.245870382945,299.329301419169,
299.411623981629,299.495609254735,299.579594527842,299.655234312579,299.730850091589,
299.806456335517,299.882090677131,299.957739915546,300.033449887924,300.07806307115,
300.169963088292,300.261995467677,300.353874434312,300.445501240997,300.536521816866,
300.576531614458,300.650534617295,300.724516639125,300.798492759581,300.872506336793,
300.946538714768,301.020644576809,301.075000157765,301.153959490174,301.232864811343,
301.311727734892,301.390559841608,301.469372687813,301.548191830672,301.627016356253,
301.705856778677,301.784723621197,301.863663625607,301.942642365685,302.021711404369,
302.07193724438,302.150936727855,302.229836004384,302.3086456406,302.387352824307,
302.465999328936,302.544582465666,302.570405787688,302.645321251716,302.720281133372,
302.795266419379,302.870323713808,302.902004435651),.UNSPECIFIED.);
#2988=B_SPLINE_CURVE_WITH_KNOTS('',3,(#137650,#137651,#137652,#137653,#137654,
#137655,#137656,#137657,#137658,#137659,#137660,#137661,#137662,#137663,
#137664,#137665),.UNSPECIFIED.,.F.,.F.,(4,3,3,3,3,4),(302.902004435756,
302.997785186833,303.068874330995,303.147952562583,303.22694819009,303.258525738749),
 .UNSPECIFIED.);
#2989=B_SPLINE_CURVE_WITH_KNOTS('',3,(#137667,#137668,#137669,#137670,#137671,
#137672,#137673,#137674,#137675,#137676,#137677,#137678,#137679,#137680,
#137681,#137682),.UNSPECIFIED.,.F.,.F.,(4,3,3,3,3,4),(-299.519174510177,
-299.436768573464,-299.354323050957,-299.271865440741,-299.189388037293,
-299.162764891651),.UNSPECIFIED.);
#2990=B_SPLINE_CURVE_WITH_KNOTS('',3,(#137683,#137684,#137685,#137686,#137687,
#137688,#137689,#137690,#137691,#137692,#137693,#137694,#137695,#137696,
#137697,#137698,#137699,#137700,#137701,#137702,#137703,#137704,#137705,
#137706,#137707,#137708,#137709,#137710,#137711,#137712,#137713,#137714,
#137715,#137716,#137717,#137718,#137719,#137720,#137721,#137722,#137723,
#137724,#137725,#137726,#137727,#137728,#137729,#137730,#137731,#137732,
#137733,#137734,#137735,#137736,#137737,#137738,#137739,#137740,#137741,
#137742,#137743,#137744,#137745,#137746,#137747,#137748,#137749,#137750,
#137751,#137752,#137753,#137754,#137755,#137756,#137757,#137758,#137759,
#137760,#137761,#137762,#137763,#137764,#137765,#137766,#137767,#137768,
#137769,#137770,#137771,#137772,#137773,#137774,#137775,#137776,#137777,
#137778,#137779,#137780,#137781,#137782,#137783,#137784,#137785,#137786,
#137787,#137788,#137789,#137790,#137791,#137792,#137793,#137794,#137795,
#137796,#137797,#137798,#137799,#137800,#137801,#137802,#137803,#137804,
#137805,#137806,#137807,#137808,#137809,#137810,#137811,#137812,#137813,
#137814,#137815,#137816,#137817,#137818,#137819,#137820,#137821,#137822,
#137823,#137824,#137825,#137826,#137827,#137828,#137829,#137830,#137831,
#137832,#137833,#137834,#137835,#137836,#137837,#137838,#137839,#137840,
#137841,#137842,#137843,#137844,#137845,#137846,#137847,#137848,#137849,
#137850,#137851,#137852,#137853,#137854,#137855,#137856,#137857,#137858,
#137859,#137860,#137861,#137862,#137863,#137864,#137865,#137866,#137867,
#137868,#137869,#137870,#137871,#137872,#137873,#137874,#137875,#137876,
#137877,#137878,#137879,#137880,#137881,#137882,#137883,#137884,#137885,
#137886,#137887,#137888,#137889,#137890,#137891,#137892,#137893,#137894,
#137895,#137896,#137897,#137898,#137899,#137900,#137901,#137902,#137903,
#137904,#137905,#137906,#137907,#137908,#137909,#137910,#137911,#137912,
#137913,#137914,#137915,#137916,#137917),.UNSPECIFIED.,.F.,.F.,(4,3,3,3,
3,3,3,3,3,3,3,3,3,3,3,3,3,3,3,3,3,3,3,3,3,3,3,3,3,3,3,3,3,3,3,3,3,3,3,3,
3,3,3,3,3,3,3,3,3,3,3,3,3,3,3,3,3,3,3,3,3,3,3,3,3,3,3,3,3,3,3,3,3,3,3,3,
3,3,4),(-299.162764891524,-299.081125984535,-298.99874738162,-298.916383606438,
-298.832952065135,-298.750630510816,-298.666643976022,-298.582657441227,
-298.507017190406,-298.431400944961,-298.355794234514,-298.28015942751,
-298.20450972403,-298.128799289021,-298.08418889792,-297.992288468792,-297.900255646981,
-297.808376225204,-297.716748972121,-297.625727980528,-297.585720354612,
-297.511718426913,-297.437737485504,-297.363762450475,-297.28974996401,
-297.215718680824,-297.141613915406,-297.087251811305,-297.008290393402,
-296.92938296833,-296.850517927347,-296.771683694538,-296.692868718443,
-296.61404745263,-296.535220811344,-296.456378284779,-296.377509353997,
-296.298567300463,-296.21958653277,-296.140515519565,-296.090314724689,
-296.011322839481,-295.9324310649,-295.853628818892,-295.774928827978,-295.69628939192,
-295.617713119395,-295.591846181382,-295.513259452359,-295.434623279105,
-295.355927279677,-295.277113241945,-295.198231807393,-295.119228707778,
-295.093377638074,-295.014305117287,-294.935305563532,-294.856367296706,
-294.777478683235,-294.698628127702,-294.61979962447,-294.54098325164,-294.462168501499,
-294.383344868565,-294.304474822055,-294.225581144014,-294.146620620199,
-294.096440551459,-294.022335113587,-293.948286615963,-293.874279878189,
-293.800290614271,-293.726313252894,-293.652310967098,-293.597972008152,
-293.506788969109,-293.415204127274,-293.323243588072,-293.23580359734),
 .UNSPECIFIED.);
#2991=B_SPLINE_CURVE_WITH_KNOTS('',3,(#137923,#137924,#137925,#137926,#137927,
#137928,#137929,#137930,#137931,#137932,#137933,#137934,#137935,#137936,
#137937,#137938,#137939,#137940,#137941,#137942,#137943,#137944,#137945,
#137946,#137947,#137948,#137949,#137950,#137951,#137952,#137953,#137954,
#137955,#137956,#137957,#137958,#137959,#137960,#137961,#137962,#137963,
#137964,#137965,#137966,#137967,#137968,#137969,#137970,#137971,#137972,
#137973,#137974,#137975,#137976,#137977,#137978,#137979,#137980,#137981,
#137982,#137983,#137984,#137985,#137986,#137987,#137988,#137989,#137990,
#137991,#137992,#137993,#137994,#137995,#137996,#137997,#137998,#137999,
#138000,#138001,#138002,#138003,#138004,#138005,#138006,#138007,#138008,
#138009,#138010,#138011,#138012,#138013,#138014,#138015,#138016,#138017,
#138018,#138019,#138020,#138021,#138022,#138023,#138024,#138025,#138026,
#138027,#138028,#138029,#138030,#138031,#138032,#138033,#138034,#138035,
#138036,#138037,#138038,#138039,#138040,#138041,#138042,#138043,#138044,
#138045,#138046,#138047,#138048,#138049,#138050,#138051,#138052,#138053,
#138054,#138055,#138056,#138057,#138058,#138059,#138060,#138061,#138062,
#138063,#138064,#138065,#138066,#138067,#138068,#138069,#138070,#138071,
#138072,#138073,#138074,#138075,#138076,#138077,#138078,#138079,#138080,
#138081,#138082,#138083,#138084,#138085,#138086,#138087,#138088,#138089,
#138090,#138091,#138092,#138093,#138094,#138095,#138096,#138097,#138098,
#138099,#138100,#138101,#138102,#138103,#138104,#138105,#138106,#138107,
#138108,#138109,#138110,#138111,#138112,#138113,#138114,#138115,#138116,
#138117,#138118,#138119,#138120,#138121,#138122,#138123,#138124,#138125,
#138126,#138127,#138128,#138129,#138130,#138131,#138132,#138133,#138134,
#138135,#138136,#138137,#138138,#138139,#138140,#138141,#138142,#138143,
#138144,#138145,#138146,#138147,#138148,#138149,#138150,#138151,#138152,
#138153,#138154,#138155,#138156,#138157),.UNSPECIFIED.,.F.,.F.,(4,3,3,3,
3,3,3,3,3,3,3,3,3,3,3,3,3,3,3,3,3,3,3,3,3,3,3,3,3,3,3,3,3,3,3,3,3,3,3,3,
3,3,3,3,3,3,3,3,3,3,3,3,3,3,3,3,3,3,3,3,3,3,3,3,3,3,3,3,3,3,3,3,3,3,3,3,
3,3,4),(290.691188989457,290.782659024431,290.874590100086,290.96662251805,
291.058539304055,291.105629291614,291.18133896279,291.256999964875,291.332626805271,
291.408244501611,291.483856001756,291.559495926441,291.604097834922,291.686376606522,
291.768679169128,291.852150971403,291.934505926045,292.018536152137,292.102566378229,
292.184945389364,292.267309579149,292.350740914746,292.433062888566,292.517048905051,
292.601034921537,292.676675030202,292.752291132552,292.827897699049,292.903532361204,
292.979181919227,293.054892208453,293.099503464844,293.191404036096,293.283437007398,
293.375316578752,293.466943976229,293.557965098977,293.597972008152,293.671973922603,
293.745954850711,293.819929872389,293.893942345456,293.967973615205,294.042078367181,
294.096440551459,294.175401966386,294.254309388427,294.333174426327,294.412008656013,
294.49082362895,294.569644891571,294.648471529648,294.727314052994,294.806182980555,
294.885125030883,294.96410579538,295.043176805432,295.093377638074,295.172369539784,
295.251261330761,295.330063593028,295.408763599925,295.487403051785,295.565979339797,
295.591846181382,295.670432894843,295.749069052265,295.82776503562,295.906579057027,
295.985460475111,296.064463558162,296.09031472469,296.171880226951,296.253354390263,
296.334739943628,296.416006787763,296.497198842002,296.578292418501,296.618819128577),
 .UNSPECIFIED.);
#2992=B_SPLINE_CURVE_WITH_KNOTS('',3,(#138158,#138159,#138160,#138161,#138162,
#138163,#138164,#138165,#138166,#138167,#138168,#138169,#138170,#138171,
#138172,#138173),.UNSPECIFIED.,.F.,.F.,(4,3,3,3,3,4),(296.618819128679,
296.703368262176,296.788149274131,296.873040522573,296.958059703437,296.975200039958),
 .UNSPECIFIED.);
#2993=B_SPLINE_CURVE_WITH_KNOTS('',3,(#138175,#138176,#138177,#138178,#138179,
#138180,#138181,#138182,#138183,#138184,#138185,#138186,#138187,#138188,
#138189,#138190),.UNSPECIFIED.,.F.,.F.,(4,3,3,3,3,4),(-293.23580359734,
-293.143889729308,-293.099503464844,-293.022641471914,-292.94584475079,
-292.879579584471),.UNSPECIFIED.);
#2994=B_SPLINE_CURVE_WITH_KNOTS('',3,(#138191,#138192,#138193,#138194,#138195,
#138196,#138197,#138198,#138199,#138200,#138201,#138202,#138203,#138204,
#138205,#138206,#138207,#138208,#138209,#138210,#138211,#138212,#138213,
#138214,#138215,#138216,#138217,#138218,#138219,#138220,#138221,#138222,
#138223,#138224,#138225,#138226,#138227,#138228,#138229,#138230,#138231,
#138232,#138233,#138234,#138235,#138236,#138237,#138238,#138239,#138240,
#138241,#138242,#138243,#138244,#138245,#138246,#138247,#138248,#138249,
#138250,#138251,#138252,#138253,#138254,#138255,#138256,#138257,#138258,
#138259,#138260,#138261,#138262,#138263,#138264,#138265,#138266,#138267,
#138268,#138269,#138270,#138271,#138272,#138273,#138274,#138275,#138276,
#138277,#138278,#138279,#138280,#138281,#138282,#138283,#138284,#138285,
#138286,#138287,#138288,#138289,#138290,#138291,#138292,#138293,#138294,
#138295,#138296,#138297,#138298,#138299,#138300,#138301,#138302,#138303,
#138304,#138305,#138306,#138307,#138308,#138309,#138310,#138311,#138312,
#138313,#138314,#138315,#138316,#138317,#138318,#138319,#138320,#138321,
#138322,#138323,#138324,#138325,#138326,#138327,#138328,#138329,#138330,
#138331,#138332,#138333,#138334,#138335,#138336,#138337,#138338,#138339,
#138340,#138341,#138342,#138343,#138344,#138345,#138346,#138347,#138348,
#138349,#138350,#138351,#138352,#138353,#138354,#138355,#138356,#138357,
#138358,#138359,#138360,#138361,#138362,#138363,#138364,#138365,#138366,
#138367,#138368,#138369,#138370,#138371,#138372,#138373,#138374,#138375,
#138376,#138377,#138378,#138379,#138380,#138381,#138382,#138383,#138384,
#138385,#138386,#138387,#138388,#138389,#138390,#138391,#138392,#138393,
#138394,#138395,#138396,#138397,#138398,#138399,#138400,#138401,#138402,
#138403,#138404,#138405,#138406,#138407,#138408,#138409,#138410),
 .UNSPECIFIED.,.F.,.F.,(4,3,3,3,3,3,3,3,3,3,3,3,3,3,3,3,3,3,3,3,3,3,3,3,
3,3,3,3,3,3,3,3,3,3,3,3,3,3,3,3,3,3,3,3,3,3,3,3,3,3,3,3,3,3,3,3,3,3,3,3,
3,3,3,3,3,3,3,3,3,3,3,3,3,4),(-292.879579584471,-292.797849710705,-292.716119956935,
-292.634390321493,-292.552660802714,-292.47093139893,-292.389202108476,
-292.304255339957,-292.220635864696,-292.138322943735,-292.056584034668,
-291.974845545282,-291.893107468902,-291.811369798854,-291.729632528466,
-291.647895651063,-291.566159159973,-291.484423048523,-291.402687310041,
-291.320951937854,-291.239216925292,-291.157482265683,-291.075747952356,
-290.99401397864,-290.912280337864,-290.830547023359,-290.748814028455,
-290.667081346481,-290.585348970769,-290.50361689465,-290.421885111455,
-290.340153614514,-290.258422397161,-290.176691452726,-290.094960774541,
-290.01323035594,-289.931500190255,-289.849770270818,-289.768040590963,
-289.686311144023,-289.600882949624,-289.5181243863,-289.436385758736,-289.354647954932,
-289.272910948193,-289.191174711825,-289.109439219139,-289.027704443448,
-288.945970358068,-288.864236936315,-288.78250415151,-288.700771976975,
-288.619040386034,-288.537309352013,-288.45557884824,-288.373848848046,
-288.292119324761,-288.208399924667,-288.126661843638,-288.044925348214,
-287.96319033163,-287.881456687141,-287.799724308024,-287.717993087571,
-287.63626291909,-287.55080616961,-287.469069251391,-287.387335242488,-287.305603715969,
-287.223874245041,-287.142139354565,-287.0604092744,-286.978677845338,-286.95260892325),
 .UNSPECIFIED.);
#2995=B_SPLINE_CURVE_WITH_KNOTS('',3,(#138416,#138417,#138418,#138419,#138420,
#138421,#138422,#138423,#138424,#138425,#138426,#138427,#138428,#138429,
#138430,#138431,#138432,#138433,#138434,#138435,#138436,#138437,#138438,
#138439,#138440,#138441,#138442,#138443,#138444,#138445,#138446,#138447,
#138448,#138449,#138450,#138451,#138452,#138453,#138454,#138455,#138456,
#138457,#138458,#138459,#138460,#138461,#138462,#138463,#138464,#138465,
#138466,#138467,#138468,#138469,#138470,#138471,#138472,#138473,#138474,
#138475,#138476,#138477,#138478,#138479,#138480,#138481,#138482,#138483,
#138484,#138485,#138486,#138487,#138488,#138489,#138490,#138491,#138492,
#138493,#138494,#138495,#138496,#138497,#138498,#138499,#138500,#138501,
#138502,#138503,#138504,#138505,#138506,#138507,#138508,#138509,#138510,
#138511,#138512,#138513,#138514,#138515,#138516,#138517,#138518,#138519,
#138520,#138521,#138522,#138523,#138524,#138525,#138526,#138527,#138528,
#138529,#138530,#138531,#138532,#138533,#138534,#138535,#138536,#138537,
#138538,#138539,#138540,#138541,#138542,#138543,#138544,#138545,#138546,
#138547,#138548,#138549,#138550,#138551,#138552,#138553,#138554,#138555,
#138556,#138557,#138558,#138559,#138560,#138561,#138562,#138563,#138564,
#138565,#138566,#138567,#138568,#138569,#138570,#138571,#138572,#138573,
#138574,#138575,#138576,#138577,#138578,#138579,#138580,#138581,#138582,
#138583,#138584,#138585,#138586,#138587,#138588,#138589,#138590,#138591,
#138592,#138593,#138594,#138595,#138596,#138597,#138598,#138599,#138600,
#138601,#138602,#138603,#138604,#138605,#138606,#138607,#138608,#138609,
#138610,#138611,#138612,#138613,#138614,#138615,#138616,#138617,#138618,
#138619,#138620,#138621,#138622,#138623,#138624,#138625,#138626,#138627,
#138628,#138629,#138630,#138631,#138632,#138633,#138634,#138635,#138636,
#138637,#138638,#138639,#138640,#138641,#138642,#138643,#138644,#138645,
#138646,#138647,#138648,#138649,#138650),.UNSPECIFIED.,.F.,.F.,(4,3,3,3,
3,3,3,3,3,3,3,3,3,3,3,3,3,3,3,3,3,3,3,3,3,3,3,3,3,3,3,3,3,3,3,3,3,3,3,3,
3,3,3,3,3,3,3,3,3,3,3,3,3,3,3,3,3,3,3,3,3,3,3,3,3,3,3,3,3,3,3,3,3,3,3,3,
3,3,4),(284.408859837487,284.484471751109,284.56011303113,284.625538228616,
284.707817000464,284.790119563321,284.873591365472,284.955946320364,285.039976546144,
285.124006771923,285.206385782528,285.28874997178,285.372181307643,285.454503280938,
285.538489298085,285.622475315231,285.698115424451,285.773731527356,285.849338094408,
285.924972757117,286.000622315693,286.076332605469,286.120943858538,286.212844428244,
286.304877397962,286.396756967787,286.488384363818,286.579405485302,286.619412401846,
286.693414316533,286.767395244875,286.841370266786,286.915382740085,286.989414010064,
287.063518762268,287.117880945153,287.1968423611,287.27574978417,287.354614823107,
287.433449053833,287.512264027813,287.591085291473,287.669911930586,287.748754454962,
287.827623383545,287.906565434877,287.985546200366,288.064617211384,288.114818031769,
288.193809927111,288.272701711788,288.351503967835,288.430203968659,288.508843414541,
288.587419696728,288.613286575076,288.691873298233,288.770509465491,288.849205458802,
288.928019490279,289.006900918497,289.085904011706,289.111755118384,289.190827640138,
289.269827194878,289.348765462706,289.427654077192,289.506504633753,289.585333138023,
289.664149511897,289.742964263085,289.821787897067,289.90065794462,289.9795516237,
290.058512148541,290.108692204999,290.190292057889,290.271695048658,290.335633821397),
 .UNSPECIFIED.);
#2996=B_SPLINE_CURVE_WITH_KNOTS('',3,(#138651,#138652,#138653,#138654,#138655,
#138656,#138657,#138658,#138659,#138660,#138661,#138662,#138663,#138664,
#138665,#138666),.UNSPECIFIED.,.F.,.F.,(4,3,3,3,3,4),(290.335633821483,
290.406514795855,290.477380699428,290.548271359671,290.607160748306,290.691188989457),
 .UNSPECIFIED.);
#2997=B_SPLINE_CURVE_WITH_KNOTS('',3,(#138668,#138669,#138670,#138671,#138672,
#138673,#138674,#138675,#138676,#138677,#138678,#138679,#138680,#138681,
#138682,#138683),.UNSPECIFIED.,.F.,.F.,(4,3,3,3,3,4),(-286.95260892325,
-286.870879379414,-286.789144264495,-286.707414027146,-286.625682238195,
-286.596394277292),.UNSPECIFIED.);
#2998=B_SPLINE_CURVE_WITH_KNOTS('',3,(#138684,#138685,#138686,#138687,#138688,
#138689,#138690,#138691,#138692,#138693,#138694,#138695,#138696,#138697,
#138698,#138699,#138700,#138701,#138702,#138703,#138704,#138705,#138706,
#138707,#138708,#138709,#138710,#138711,#138712,#138713,#138714,#138715,
#138716,#138717,#138718,#138719,#138720,#138721,#138722,#138723,#138724,
#138725,#138726,#138727,#138728,#138729,#138730,#138731,#138732,#138733,
#138734,#138735,#138736,#138737,#138738,#138739,#138740,#138741,#138742,
#138743,#138744,#138745,#138746,#138747,#138748,#138749,#138750,#138751,
#138752,#138753,#138754,#138755,#138756,#138757,#138758,#138759,#138760,
#138761,#138762,#138763,#138764,#138765,#138766,#138767,#138768,#138769,
#138770,#138771,#138772,#138773,#138774,#138775,#138776,#138777,#138778,
#138779,#138780,#138781,#138782,#138783,#138784,#138785,#138786,#138787,
#138788,#138789,#138790,#138791,#138792,#138793,#138794,#138795,#138796,
#138797,#138798,#138799,#138800,#138801,#138802,#138803,#138804,#138805,
#138806,#138807,#138808,#138809,#138810,#138811,#138812,#138813,#138814,
#138815,#138816,#138817,#138818,#138819,#138820,#138821,#138822,#138823,
#138824,#138825,#138826,#138827,#138828,#138829,#138830,#138831,#138832,
#138833,#138834,#138835,#138836,#138837,#138838,#138839,#138840,#138841,
#138842,#138843,#138844,#138845,#138846,#138847,#138848,#138849,#138850,
#138851,#138852,#138853,#138854,#138855,#138856,#138857,#138858,#138859,
#138860,#138861,#138862,#138863,#138864,#138865,#138866,#138867,#138868,
#138869,#138870,#138871,#138872,#138873,#138874,#138875,#138876,#138877,
#138878,#138879,#138880,#138881,#138882,#138883,#138884,#138885,#138886,
#138887,#138888,#138889,#138890,#138891,#138892,#138893,#138894,#138895,
#138896,#138897,#138898,#138899,#138900,#138901,#138902,#138903,#138904,
#138905,#138906,#138907,#138908,#138909,#138910,#138911,#138912,#138913,
#138914,#138915,#138916,#138917,#138918),.UNSPECIFIED.,.F.,.F.,(4,3,3,3,
3,3,3,3,3,3,3,3,3,3,3,3,3,3,3,3,3,3,3,3,3,3,3,3,3,3,3,3,3,3,3,3,3,3,3,3,
3,3,3,3,3,3,3,3,3,3,3,3,3,3,3,3,3,3,3,3,3,3,3,3,3,3,3,3,3,3,3,3,3,3,3,3,
3,3,4),(-286.596394277292,-286.505074083817,-286.409041527497,-286.316842690878,
-286.22459197147,-286.132509475947,-286.120943858538,-286.045234187422,
-285.969573185398,-285.893946345062,-285.818328648781,-285.742717148696,
-285.66707722407,-285.622475315231,-285.540196543376,-285.457893980512,
-285.374422178365,-285.292067223465,-285.208036997694,-285.124006771923,
-285.041627761322,-284.959263572073,-284.875832236209,-284.793510262917,
-284.709524245767,-284.625538228616,-284.549898119394,-284.474282016488,
-284.398675449434,-284.323040786724,-284.247391228145,-284.171680938368,
-284.127069685308,-284.035169115606,-283.943136145893,-283.851256576072,
-283.759629180044,-283.668608058564,-283.628601142001,-283.554599227313,
-283.480618298969,-283.406643277056,-283.332630803756,-283.258599533774,
-283.184494781569,-283.130132598693,-283.051171182746,-282.972263759677,
-282.89339872074,-282.814564490015,-282.735749516036,-282.656928252376,
-282.578101613264,-282.499259088887,-282.420390160305,-282.341448108973,
-282.262467343485,-282.183396332467,-282.133195512078,-282.054203616739,
-281.975311832064,-281.896509576019,-281.817809575197,-281.739170129318,
-281.660593847132,-281.63472696877,-281.556140245607,-281.477504078345,
-281.398808085029,-281.319994053547,-281.241112625324,-281.162109532109,
-281.136258425463,-281.05855966127,-280.980933020594,-280.90304644441,-280.825531995737,
-280.747459355796,-280.669386715856),.UNSPECIFIED.);
#2999=B_SPLINE_CURVE_WITH_KNOTS('',3,(#138924,#138925,#138926,#138927,#138928,
#138929,#138930,#138931,#138932,#138933,#138934,#138935,#138936,#138937,
#138938,#138939,#138940,#138941,#138942,#138943,#138944,#138945,#138946,
#138947,#138948,#138949,#138950,#138951,#138952,#138953,#138954,#138955,
#138956,#138957,#138958,#138959,#138960,#138961,#138962,#138963,#138964,
#138965,#138966,#138967,#138968,#138969,#138970,#138971,#138972,#138973,
#138974,#138975,#138976,#138977,#138978,#138979,#138980,#138981,#138982,
#138983,#138984,#138985,#138986,#138987,#138988,#138989,#138990,#138991,
#138992,#138993,#138994,#138995,#138996,#138997,#138998,#138999,#139000,
#139001,#139002,#139003,#139004,#139005,#139006,#139007,#139008,#139009,
#139010,#139011,#139012,#139013,#139014,#139015,#139016,#139017,#139018,
#139019,#139020,#139021,#139022,#139023,#139024,#139025,#139026,#139027,
#139028,#139029,#139030,#139031,#139032,#139033,#139034,#139035,#139036,
#139037,#139038,#139039,#139040,#139041,#139042,#139043,#139044,#139045,
#139046,#139047,#139048,#139049,#139050,#139051,#139052,#139053,#139054,
#139055,#139056,#139057,#139058,#139059,#139060,#139061,#139062,#139063,
#139064,#139065,#139066,#139067,#139068,#139069,#139070,#139071,#139072,
#139073,#139074,#139075,#139076,#139077,#139078,#139079,#139080,#139081,
#139082,#139083,#139084,#139085,#139086,#139087,#139088,#139089,#139090,
#139091,#139092,#139093,#139094,#139095,#139096,#139097,#139098,#139099,
#139100,#139101,#139102,#139103,#139104,#139105,#139106,#139107,#139108,
#139109,#139110,#139111,#139112,#139113,#139114,#139115,#139116,#139117,
#139118,#139119,#139120,#139121,#139122,#139123,#139124,#139125,#139126,
#139127,#139128,#139129,#139130,#139131,#139132,#139133,#139134,#139135,
#139136,#139137,#139138,#139139,#139140,#139141,#139142,#139143,#139144,
#139145,#139146,#139147,#139148,#139149,#139150,#139151,#139152,#139153,
#139154,#139155,#139156,#139157,#139158,#139159,#139160,#139161),
 .UNSPECIFIED.,.F.,.F.,(4,3,3,3,3,3,3,3,3,3,3,3,3,3,3,3,3,3,3,3,3,3,3,3,
3,3,3,3,3,3,3,3,3,3,3,3,3,3,3,3,3,3,3,3,3,3,3,3,3,3,3,3,3,3,3,3,3,3,3,3,
3,3,3,3,3,3,3,3,3,3,3,3,3,3,3,3,3,3,3,4),(278.125459419588,278.145447165617,
278.227826176221,278.310190365473,278.393621701336,278.475943674631,278.559929691778,
278.643915708925,278.719555818145,278.79517192105,278.870778488103,278.946413150811,
279.022062709388,279.097772999164,279.142384252232,279.234284821936,279.32631779165,
279.418197361473,279.509824757503,279.600845878986,279.64085279554,279.714854710229,
279.788835638572,279.862810660485,279.936823133786,280.010854403768,280.084959155973,
280.139321338848,280.218282754795,280.297190177864,280.3760552168,280.454889447526,
280.533704421505,280.612525685165,280.691352324277,280.770194848653,280.849063777236,
280.928005828567,281.006986594055,281.086057605073,281.136258425463,281.215250320801,
281.294142105475,281.372944361519,281.45164436234,281.530283808218,281.608860090403,
281.63472696877,281.713313691934,281.791949859198,281.870645852514,281.949459883998,
282.028341312222,282.107344405438,282.133195512078,282.212268033827,282.291267588562,
282.370205856386,282.449094470868,282.527945027424,282.60677353169,282.685589905558,
282.764404656742,282.843228290719,282.922098338268,283.000992017343,283.07995254218,
283.130132598693,283.204238036795,283.27828653465,283.352293272657,283.426282536809,
283.500259898421,283.574262184455,283.628601142001,283.717952507213,283.807870450816,
283.898002918138,283.988285085807,284.052448514116),.UNSPECIFIED.);
#3000=B_SPLINE_CURVE_WITH_KNOTS('',3,(#139162,#139163,#139164,#139165,#139166,
#139167,#139168,#139169,#139170,#139171,#139172,#139173,#139174,#139175,
#139176,#139177),.UNSPECIFIED.,.F.,.F.,(4,3,3,3,3,4),(284.052448514218,
284.127069685308,284.202777478049,284.278438680736,284.354067936897,284.408859837487),
 .UNSPECIFIED.);
#3001=B_SPLINE_CURVE_WITH_KNOTS('',3,(#139179,#139180,#139181,#139182,#139183,
#139184,#139185,#139186,#139187,#139188,#139189,#139190,#139191,#139192,
#139193,#139194),.UNSPECIFIED.,.F.,.F.,(4,3,3,3,3,4),(-280.669386715856,
-280.591919617408,-280.514418752512,-280.436900105981,-280.359320140393,
-280.313208970232),.UNSPECIFIED.);
#3002=B_SPLINE_CURVE_WITH_KNOTS('',3,(#139195,#139196,#139197,#139198,#139199,
#139200,#139201,#139202,#139203,#139204,#139205,#139206,#139207,#139208,
#139209,#139210,#139211,#139212,#139213,#139214,#139215,#139216,#139217,
#139218,#139219,#139220,#139221,#139222,#139223,#139224,#139225,#139226,
#139227,#139228,#139229,#139230,#139231,#139232,#139233,#139234,#139235,
#139236,#139237,#139238,#139239,#139240,#139241,#139242,#139243,#139244,
#139245,#139246,#139247,#139248,#139249,#139250,#139251,#139252,#139253,
#139254,#139255,#139256,#139257,#139258,#139259,#139260,#139261,#139262,
#139263,#139264,#139265,#139266,#139267,#139268,#139269,#139270,#139271,
#139272,#139273,#139274,#139275,#139276,#139277,#139278,#139279,#139280,
#139281,#139282,#139283,#139284,#139285,#139286,#139287,#139288,#139289,
#139290,#139291,#139292,#139293,#139294,#139295,#139296,#139297,#139298,
#139299,#139300,#139301,#139302,#139303,#139304,#139305,#139306,#139307,
#139308,#139309,#139310,#139311,#139312,#139313,#139314,#139315,#139316,
#139317,#139318,#139319,#139320,#139321,#139322,#139323,#139324,#139325,
#139326,#139327,#139328,#139329,#139330,#139331,#139332,#139333,#139334,
#139335,#139336,#139337,#139338,#139339,#139340,#139341,#139342,#139343,
#139344,#139345,#139346,#139347,#139348,#139349,#139350,#139351,#139352,
#139353,#139354,#139355,#139356,#139357,#139358,#139359,#139360,#139361,
#139362,#139363,#139364,#139365,#139366,#139367,#139368,#139369,#139370,
#139371,#139372,#139373,#139374,#139375,#139376,#139377,#139378,#139379,
#139380,#139381,#139382,#139383,#139384,#139385,#139386,#139387,#139388,
#139389,#139390,#139391,#139392,#139393,#139394,#139395,#139396,#139397,
#139398,#139399,#139400,#139401,#139402,#139403,#139404,#139405,#139406,
#139407,#139408,#139409,#139410,#139411,#139412,#139413,#139414,#139415,
#139416,#139417,#139418,#139419,#139420,#139421,#139422,#139423,#139424,
#139425,#139426,#139427,#139428,#139429),.UNSPECIFIED.,.F.,.F.,(4,3,3,3,
3,3,3,3,3,3,3,3,3,3,3,3,3,3,3,3,3,3,3,3,3,3,3,3,3,3,3,3,3,3,3,3,3,3,3,3,
3,3,3,3,3,3,3,3,3,3,3,3,3,3,3,3,3,3,3,3,3,3,3,3,3,3,3,3,3,3,3,3,3,3,3,3,
3,3,4),(-280.313208970112,-280.171571993323,-280.139321338848,-280.065215900744,
-279.991167402887,-279.917160664878,-279.843171400723,-279.769194039109,
-279.695191753074,-279.64085279554,-279.549853695804,-279.458350478127,
-279.366406939197,-279.274372362018,-279.182463271897,-279.142384252232,
-279.066674581115,-278.99101357909,-278.915386738754,-278.839769042472,
-278.764157542387,-278.68851761776,-278.643915708925,-278.56163693707,-278.479334374206,
-278.395862572059,-278.31350761716,-278.229477391388,-278.145447165617,
-278.063068155016,-277.980703965768,-277.897272629903,-277.814950656611,
-277.730964639461,-277.64697862231,-277.571338513088,-277.495722410181,
-277.420115843127,-277.344481180417,-277.268831621838,-277.193121332061,
-277.148510079002,-277.056609509301,-276.964576539589,-276.872696969768,
-276.781069573741,-276.690048452261,-276.650041535695,-276.576039621006,
-276.502058692663,-276.42808367075,-276.354071197449,-276.280039927468,
-276.205935175262,-276.151572992387,-276.07261157644,-275.99370415337,-275.914839114434,
-275.836004883708,-275.757189909729,-275.678368646069,-275.599542006956,
-275.52069948258,-275.441830553997,-275.362888502666,-275.283907737177,
-275.204836726159,-275.154635905772,-275.075644010434,-274.99675222576,
-274.917949969717,-274.839249968896,-274.760610523018,-274.682034240834,
-274.656167362465,-274.577575184507,-274.498944533264,-274.420231322113,
-274.38703094937),.UNSPECIFIED.);
#3003=B_SPLINE_CURVE_WITH_KNOTS('',3,(#139435,#139436,#139437,#139438,#139439,
#139440,#139441,#139442,#139443,#139444,#139445,#139446,#139447,#139448,
#139449,#139450,#139451,#139452,#139453,#139454,#139455,#139456,#139457,
#139458,#139459,#139460,#139461,#139462,#139463,#139464,#139465,#139466,
#139467,#139468,#139469,#139470,#139471,#139472,#139473,#139474,#139475,
#139476,#139477,#139478,#139479,#139480,#139481,#139482,#139483,#139484,
#139485,#139486,#139487,#139488,#139489,#139490,#139491,#139492,#139493,
#139494,#139495,#139496,#139497,#139498,#139499,#139500,#139501,#139502,
#139503,#139504,#139505,#139506,#139507,#139508,#139509,#139510,#139511,
#139512,#139513,#139514,#139515,#139516,#139517,#139518,#139519,#139520,
#139521,#139522,#139523,#139524,#139525,#139526,#139527,#139528,#139529,
#139530,#139531,#139532,#139533,#139534,#139535,#139536,#139537,#139538,
#139539,#139540,#139541,#139542,#139543,#139544,#139545,#139546,#139547,
#139548,#139549,#139550,#139551,#139552,#139553,#139554,#139555,#139556,
#139557,#139558,#139559,#139560,#139561,#139562,#139563,#139564,#139565,
#139566,#139567,#139568,#139569,#139570,#139571,#139572,#139573,#139574,
#139575,#139576,#139577,#139578,#139579,#139580,#139581,#139582,#139583,
#139584,#139585,#139586,#139587,#139588,#139589,#139590,#139591,#139592,
#139593,#139594,#139595,#139596,#139597,#139598,#139599,#139600,#139601,
#139602,#139603,#139604,#139605,#139606,#139607,#139608,#139609,#139610,
#139611,#139612,#139613,#139614,#139615,#139616,#139617,#139618,#139619,
#139620,#139621,#139622,#139623,#139624,#139625,#139626,#139627,#139628,
#139629,#139630,#139631,#139632,#139633,#139634,#139635,#139636,#139637,
#139638,#139639,#139640,#139641,#139642,#139643,#139644,#139645,#139646,
#139647,#139648,#139649,#139650,#139651,#139652,#139653,#139654,#139655,
#139656,#139657,#139658,#139659,#139660,#139661,#139662,#139663,#139664,
#139665,#139666,#139667,#139668,#139669,#139670,#139671,#139672,#139673,
#139674,#139675),.UNSPECIFIED.,.F.,.F.,(4,3,3,3,3,3,3,3,3,3,3,3,3,3,3,3,
3,3,3,3,3,3,3,3,3,3,3,3,3,3,3,3,3,3,3,3,3,3,3,3,3,3,3,3,3,3,3,3,3,3,3,3,
3,3,3,3,3,3,3,3,3,3,3,3,3,3,3,3,3,3,3,3,3,3,3,3,3,3,3,3,4),(271.842181774342,
271.917788389078,271.993426636706,272.069084165035,272.144799202209,272.163824645927,
272.255725215627,272.347758185338,272.439637755158,272.531265151185,272.622286272665,
272.662293189234,272.736295103923,272.810276032267,272.88425105418,272.958263527481,
273.032294797463,273.106399549668,273.160761732542,273.239723148489,273.318630571558,
273.397495610495,273.47632984122,273.555144815198,273.633966078858,273.712792717971,
273.791635242347,273.87050417093,273.949446222261,274.028426987749,274.107497998767,
274.157698819157,274.236690714496,274.315582499171,274.394384755216,274.473084756038,
274.551724201916,274.630300484102,274.656167362465,274.734754085628,274.813390252891,
274.892086246207,274.970900277689,275.049781705912,275.128784799127,275.154635905772,
275.233708427521,275.312707982256,275.39164625008,275.470534864562,275.549385421118,
275.628213925384,275.707030299253,275.785845050437,275.864668684414,275.943538731962,
276.022432411038,276.101392935875,276.151572992387,276.22567843049,276.299726928345,
276.373733666352,276.447722930505,276.521700292117,276.595702578151,276.650041535695,
276.741040635428,276.832543853103,276.924487392031,277.016521969207,277.108431059326,
277.148510079002,277.22421975012,277.299880752146,277.375507592485,277.451125288767,
277.526736788854,277.602376713482,277.64697862231,277.736638973094,277.769263207038),
 .UNSPECIFIED.);
#3004=B_SPLINE_CURVE_WITH_KNOTS('',3,(#139676,#139677,#139678,#139679,#139680,
#139681,#139682,#139683,#139684,#139685,#139686,#139687,#139688,#139689,
#139690,#139691),.UNSPECIFIED.,.F.,.F.,(4,3,3,3,3,4),(277.769263207152,
277.850658313745,277.932074100619,278.013494947125,278.094934709019,278.125459419588),
 .UNSPECIFIED.);
#3005=B_SPLINE_CURVE_WITH_KNOTS('',3,(#139693,#139694,#139695,#139696,#139697,
#139698,#139699,#139700,#139701,#139702,#139703,#139704,#139705),
 .UNSPECIFIED.,.F.,.F.,(4,3,3,3,4),(-274.38703094937,-274.308189681096,
-274.229211245105,-274.157698819157,-274.030023662932),.UNSPECIFIED.);
#3006=B_SPLINE_CURVE_WITH_KNOTS('',3,(#139706,#139707,#139708,#139709,#139710,
#139711,#139712,#139713,#139714,#139715,#139716,#139717,#139718,#139719,
#139720,#139721,#139722,#139723,#139724,#139725,#139726,#139727,#139728,
#139729,#139730,#139731,#139732,#139733,#139734,#139735,#139736,#139737,
#139738,#139739,#139740,#139741,#139742,#139743,#139744,#139745,#139746,
#139747,#139748,#139749,#139750,#139751,#139752,#139753,#139754,#139755,
#139756,#139757,#139758,#139759,#139760,#139761,#139762,#139763,#139764,
#139765,#139766,#139767,#139768,#139769,#139770,#139771,#139772,#139773,
#139774,#139775,#139776,#139777,#139778,#139779,#139780,#139781,#139782,
#139783,#139784,#139785,#139786,#139787,#139788,#139789,#139790,#139791,
#139792,#139793,#139794,#139795,#139796,#139797,#139798,#139799,#139800,
#139801,#139802,#139803,#139804,#139805,#139806,#139807,#139808,#139809,
#139810,#139811,#139812,#139813,#139814,#139815,#139816,#139817,#139818,
#139819,#139820,#139821,#139822,#139823,#139824,#139825,#139826,#139827,
#139828,#139829,#139830,#139831,#139832,#139833,#139834,#139835,#139836,
#139837,#139838,#139839,#139840,#139841,#139842,#139843,#139844,#139845,
#139846,#139847,#139848,#139849,#139850,#139851,#139852,#139853,#139854,
#139855,#139856,#139857,#139858,#139859,#139860,#139861,#139862,#139863,
#139864,#139865,#139866,#139867,#139868,#139869,#139870,#139871,#139872,
#139873,#139874,#139875,#139876,#139877,#139878,#139879,#139880,#139881,
#139882,#139883,#139884,#139885,#139886,#139887,#139888,#139889,#139890,
#139891,#139892,#139893,#139894,#139895,#139896,#139897,#139898,#139899,
#139900,#139901,#139902,#139903,#139904,#139905,#139906,#139907,#139908,
#139909,#139910,#139911,#139912,#139913,#139914,#139915,#139916,#139917,
#139918,#139919,#139920,#139921,#139922,#139923,#139924,#139925,#139926,
#139927,#139928,#139929,#139930,#139931,#139932,#139933,#139934,#139935,
#139936,#139937),.UNSPECIFIED.,.F.,.F.,(4,3,3,3,3,3,3,3,3,3,3,3,3,3,3,3,
3,3,3,3,3,3,3,3,3,3,3,3,3,3,3,3,3,3,3,3,3,3,3,3,3,3,3,3,3,3,3,3,3,3,3,3,
3,3,3,3,3,3,3,3,3,3,3,3,3,3,3,3,3,3,3,3,3,3,3,3,3,4),(-274.030023662853,
-273.951996221985,-273.874039086137,-273.796138642435,-273.716716528698,
-273.63888579274,-273.561067507186,-273.483249412772,-273.402627492714,
-273.324746987742,-273.242754360142,-273.160761732542,-273.08665629444,
-273.012607796585,-272.938601058577,-272.864611794424,-272.790634432811,
-272.716632146778,-272.662293189234,-272.571294089501,-272.479790871824,
-272.387847332896,-272.295812755718,-272.203903665599,-272.163824645927,
-272.088114974809,-272.012453972782,-271.936827132444,-271.861209436161,
-271.785597936074,-271.709958011445,-271.665356102619,-271.583077330767,
-271.500774767905,-271.417302965757,-271.33494801086,-271.250917785086,
-271.166887559312,-271.08450854871,-271.00214435946,-270.918713023596,-270.836391050303,
-270.752405033154,-270.668419016004,-270.592778906782,-270.517162803874,
-270.44155623682,-270.36592157411,-270.290272015531,-270.214561725753,-270.169950472696,
-270.078049902996,-269.986016933286,-269.894137363467,-269.80250996744,
-269.711488845961,-269.671481929389,-269.5974800147,-269.523499086356,-269.449524064443,
-269.375511591142,-269.30148032116,-269.227375568955,-269.173013386081,
-269.094051970134,-269.015144547065,-268.936279508129,-268.857445277403,
-268.778630303423,-268.699809039763,-268.620982400651,-268.542139876274,
-268.463270947691,-268.38432889636,-268.305348130871,-268.226277119853,
-268.176076299466,-268.102429383984),.UNSPECIFIED.);
#3007=B_SPLINE_CURVE_WITH_KNOTS('',3,(#139943,#139944,#139945,#139946,#139947,
#139948,#139949,#139950,#139951,#139952,#139953,#139954,#139955,#139956,
#139957,#139958,#139959,#139960,#139961,#139962,#139963,#139964,#139965,
#139966,#139967,#139968,#139969,#139970,#139971,#139972,#139973,#139974,
#139975,#139976,#139977,#139978,#139979,#139980,#139981,#139982,#139983,
#139984,#139985,#139986,#139987,#139988,#139989,#139990,#139991,#139992,
#139993,#139994,#139995,#139996,#139997,#139998,#139999,#140000,#140001,
#140002,#140003,#140004,#140005,#140006,#140007,#140008,#140009,#140010,
#140011,#140012,#140013,#140014,#140015,#140016,#140017,#140018,#140019,
#140020,#140021,#140022,#140023,#140024,#140025,#140026,#140027,#140028,
#140029,#140030,#140031,#140032,#140033,#140034,#140035,#140036,#140037,
#140038,#140039,#140040,#140041,#140042,#140043,#140044,#140045,#140046,
#140047,#140048,#140049,#140050,#140051,#140052,#140053,#140054,#140055,
#140056,#140057,#140058,#140059,#140060,#140061,#140062,#140063,#140064,
#140065,#140066,#140067,#140068,#140069,#140070,#140071,#140072,#140073,
#140074,#140075,#140076,#140077,#140078,#140079,#140080,#140081,#140082,
#140083,#140084,#140085,#140086,#140087,#140088,#140089,#140090,#140091,
#140092,#140093,#140094,#140095,#140096,#140097,#140098,#140099,#140100,
#140101,#140102,#140103,#140104,#140105,#140106,#140107,#140108,#140109,
#140110,#140111,#140112,#140113,#140114,#140115,#140116,#140117,#140118,
#140119,#140120,#140121,#140122,#140123,#140124,#140125,#140126,#140127,
#140128,#140129,#140130,#140131,#140132,#140133,#140134,#140135,#140136,
#140137,#140138,#140139,#140140,#140141,#140142,#140143,#140144,#140145,
#140146,#140147,#140148,#140149,#140150,#140151,#140152,#140153,#140154,
#140155,#140156,#140157,#140158,#140159,#140160,#140161,#140162,#140163,
#140164,#140165,#140166,#140167,#140168,#140169,#140170,#140171,#140172,
#140173,#140174,#140175,#140176,#140177,#140178,#140179,#140180),
 .UNSPECIFIED.,.F.,.F.,(4,3,3,3,3,3,3,3,3,3,3,3,3,3,3,3,3,3,3,3,3,3,3,3,
3,3,3,3,3,3,3,3,3,3,3,3,3,3,3,3,3,3,3,3,3,3,3,3,3,3,3,3,3,3,3,3,3,3,3,3,
3,3,3,3,3,3,3,3,3,3,3,3,3,3,3,3,3,3,3,4),(265.559741333664,265.650294523403,
265.683733582928,265.757735497617,265.831716425961,265.905691447874,265.979703921175,
266.053735191157,266.127839943363,266.182202126236,266.261163542183,266.340070965252,
266.418936004189,266.497770234914,266.576585208893,266.655406472553,266.734233111665,
266.813075636041,266.891944564624,266.970886615955,267.049867381444,267.128938392461,
267.179139212851,267.25813110819,267.337022892865,267.41582514891,267.494525149732,
267.57316459561,267.651740877796,267.677607756159,267.756194479322,267.834830646585,
267.9135266399,267.992340671383,268.071222099606,268.150225192821,268.176076299466,
268.255148821215,268.33414837595,268.413086643774,268.491975258256,268.570825814812,
268.649654319077,268.728470692946,268.80728544413,268.886109078107,268.964979125656,
269.043872804731,269.122833329568,269.173013386081,269.247118824183,269.321167322038,
269.395174060045,269.469163324198,269.54314068581,269.617142971843,269.671481929389,
269.762481029126,269.853984246805,269.945927785737,270.037962362917,270.12987145304,
270.169950472697,270.245660143813,270.321321145838,270.396947986175,270.472565682456,
270.548177182542,270.623817107169,270.668419016004,270.750697787859,270.833000350723,
270.91647215287,270.99882710777,271.082857333541,271.166887559312,271.248393466682,
271.329881157949,271.411356799843,271.486077899858),.UNSPECIFIED.);
#3008=B_SPLINE_CURVE_WITH_KNOTS('',3,(#140181,#140182,#140183,#140184,#140185,
#140186,#140187,#140188,#140189,#140190,#140191,#140192,#140193,#140194,
#140195,#140196),.UNSPECIFIED.,.F.,.F.,(4,3,3,3,3,4),(271.486077899858,
271.575717001239,271.665356102619,271.740996288,271.816611901616,271.842181774342),
 .UNSPECIFIED.);
#3009=B_SPLINE_CURVE_WITH_KNOTS('',3,(#140198,#140199,#140200,#140201,#140202,
#140203,#140204,#140205,#140206,#140207,#140208,#140209,#140210,#140211,
#140212,#140213),.UNSPECIFIED.,.F.,.F.,(4,3,3,3,3,4),(-268.102429383984,
-268.022019545821,-267.941766207012,-267.861606921436,-267.781567544259,
-267.74683835584),.UNSPECIFIED.);
#3010=B_SPLINE_CURVE_WITH_KNOTS('',3,(#140214,#140215,#140216,#140217,#140218,
#140219,#140220,#140221,#140222,#140223,#140224,#140225,#140226,#140227,
#140228,#140229,#140230,#140231,#140232,#140233,#140234,#140235,#140236,
#140237,#140238,#140239,#140240,#140241,#140242,#140243,#140244,#140245,
#140246,#140247,#140248,#140249,#140250,#140251,#140252,#140253,#140254,
#140255,#140256,#140257,#140258,#140259,#140260,#140261,#140262,#140263,
#140264,#140265,#140266,#140267,#140268,#140269,#140270,#140271,#140272,
#140273,#140274,#140275,#140276,#140277,#140278,#140279,#140280,#140281,
#140282,#140283,#140284,#140285,#140286,#140287,#140288,#140289,#140290,
#140291,#140292,#140293,#140294,#140295,#140296,#140297,#140298,#140299,
#140300,#140301,#140302,#140303,#140304,#140305,#140306,#140307,#140308,
#140309,#140310,#140311,#140312,#140313,#140314,#140315,#140316,#140317,
#140318,#140319,#140320,#140321,#140322,#140323,#140324,#140325,#140326,
#140327,#140328,#140329,#140330,#140331,#140332,#140333,#140334,#140335,
#140336,#140337,#140338,#140339,#140340,#140341,#140342,#140343,#140344,
#140345,#140346,#140347,#140348,#140349,#140350,#140351,#140352,#140353,
#140354,#140355,#140356,#140357,#140358,#140359,#140360,#140361,#140362,
#140363,#140364,#140365,#140366,#140367,#140368,#140369,#140370,#140371,
#140372,#140373,#140374,#140375,#140376,#140377,#140378,#140379,#140380,
#140381,#140382,#140383,#140384,#140385,#140386,#140387,#140388,#140389,
#140390,#140391,#140392,#140393,#140394,#140395,#140396,#140397,#140398,
#140399,#140400,#140401,#140402,#140403,#140404,#140405,#140406,#140407,
#140408,#140409,#140410,#140411,#140412,#140413,#140414,#140415,#140416,
#140417,#140418,#140419,#140420,#140421,#140422,#140423,#140424,#140425,
#140426,#140427,#140428,#140429,#140430,#140431,#140432,#140433,#140434,
#140435,#140436,#140437,#140438,#140439,#140440,#140441,#140442,#140443,
#140444,#140445,#140446,#140447,#140448),.UNSPECIFIED.,.F.,.F.,(4,3,3,3,
3,3,3,3,3,3,3,3,3,3,3,3,3,3,3,3,3,3,3,3,3,3,3,3,3,3,3,3,3,3,3,3,3,3,3,3,
3,3,3,3,3,3,3,3,3,3,3,3,3,3,3,3,3,3,3,3,3,3,3,3,3,3,3,3,3,3,3,3,3,3,3,3,
3,3,4),(-267.746838355753,-267.677607756159,-267.59902103299,-267.520384865722,
-267.441688872401,-267.362874840913,-267.283993412684,-267.204990319463,
-267.179139212851,-267.100066691102,-267.021067136368,-266.942128868545,
-266.863240254064,-266.784389697509,-266.705561193244,-266.626744819376,
-266.547930068193,-266.469106434217,-266.390236386669,-266.311342707595,
-266.232382182759,-266.182202126236,-266.108096688134,-266.034048190279,
-265.960041452272,-265.886052188119,-265.812074826506,-265.738072540473,
-265.683733582928,-265.592734483193,-265.501231265519,-265.40928772659,
-265.317253149413,-265.225344059293,-265.185265039621,-265.109555368503,
-265.033894366476,-264.958267526138,-264.882649829855,-264.807038329767,
-264.731398405139,-264.686796496313,-264.604517724461,-264.522215161599,
-264.438743359451,-264.356388404554,-264.27235817878,-264.188327953006,
-264.105948942403,-264.023584753153,-263.940153417289,-263.857831443995,
-263.773845426847,-263.689859409698,-263.614219300477,-263.538603197572,
-263.462996630519,-263.38736196781,-263.311712409233,-263.236002119457,
-263.191390866391,-263.099490296686,-263.007457326971,-262.915577757147,
-262.823950361117,-262.732929239634,-262.692922323083,-262.618920408396,
-262.544939480053,-262.470964458141,-262.396951984841,-262.322920714861,
-262.248815962657,-262.194453779776,-262.115994960713,-262.037605868093,
-261.959258290357,-261.880941468947,-261.82024085972),.UNSPECIFIED.);
#3011=B_SPLINE_CURVE_WITH_KNOTS('',3,(#140454,#140455,#140456,#140457,#140458,
#140459,#140460,#140461,#140462,#140463,#140464,#140465,#140466,#140467,
#140468,#140469,#140470,#140471,#140472,#140473,#140474,#140475,#140476,
#140477,#140478,#140479,#140480,#140481,#140482,#140483,#140484,#140485,
#140486,#140487,#140488,#140489,#140490,#140491,#140492,#140493,#140494,
#140495,#140496,#140497,#140498,#140499,#140500,#140501,#140502,#140503,
#140504,#140505,#140506,#140507,#140508,#140509,#140510,#140511,#140512,
#140513,#140514,#140515,#140516,#140517,#140518,#140519,#140520,#140521,
#140522,#140523,#140524,#140525,#140526,#140527,#140528,#140529,#140530,
#140531,#140532,#140533,#140534,#140535,#140536,#140537,#140538,#140539,
#140540,#140541,#140542,#140543,#140544,#140545,#140546,#140547,#140548,
#140549,#140550,#140551,#140552,#140553,#140554,#140555,#140556,#140557,
#140558,#140559,#140560,#140561,#140562,#140563,#140564,#140565,#140566,
#140567,#140568,#140569,#140570,#140571,#140572,#140573,#140574,#140575,
#140576,#140577,#140578,#140579,#140580,#140581,#140582,#140583,#140584,
#140585,#140586,#140587,#140588,#140589,#140590,#140591,#140592,#140593,
#140594,#140595,#140596,#140597,#140598,#140599,#140600,#140601,#140602,
#140603,#140604,#140605,#140606,#140607,#140608,#140609,#140610,#140611,
#140612,#140613,#140614,#140615,#140616,#140617,#140618,#140619,#140620,
#140621,#140622,#140623,#140624,#140625,#140626,#140627,#140628,#140629,
#140630,#140631,#140632,#140633,#140634,#140635,#140636,#140637,#140638,
#140639,#140640,#140641,#140642,#140643,#140644,#140645,#140646,#140647,
#140648,#140649,#140650,#140651,#140652,#140653,#140654,#140655,#140656,
#140657,#140658,#140659,#140660,#140661,#140662,#140663,#140664,#140665,
#140666,#140667,#140668,#140669,#140670,#140671,#140672,#140673,#140674,
#140675,#140676,#140677,#140678,#140679,#140680,#140681,#140682,#140683,
#140684,#140685,#140686,#140687,#140688,#140689,#140690,#140691),
 .UNSPECIFIED.,.F.,.F.,(4,3,3,3,3,3,3,3,3,3,3,3,3,3,3,3,3,3,3,3,3,3,3,3,
3,3,3,3,3,3,3,3,3,3,3,3,3,3,3,3,3,3,3,3,3,3,3,3,3,3,3,3,3,3,3,3,3,3,3,3,
3,3,3,3,3,3,3,3,3,3,3,3,3,3,3,3,3,3,3,4),(259.275636793971,259.354548515047,
259.433416828795,259.512253313696,259.591069523036,259.669890816851,259.74871655884,
259.827557258332,259.906423433194,259.985362535655,260.064339495741,260.143408327936,
260.200579606545,260.279571501884,260.358463286559,260.437265542604,260.515965543426,
260.594604989306,260.673181271491,260.699048149853,260.777634873016,260.856271040278,
260.934967033593,261.013781065075,261.092662493298,261.171665586513,261.19751669316,
261.27658921491,261.355588769645,261.43452703747,261.513415651951,261.592266208508,
261.671094712774,261.749911086643,261.828725837828,261.907549471805,261.986419519354,
262.06531319843,262.144273723268,262.194453779776,262.268559217878,262.342607715732,
262.416614453739,262.490603717892,262.564581079503,262.638583365536,262.692922323083,
262.783921422819,262.875424640497,262.967368179428,263.059402756607,263.151311846729,
263.191390866391,263.267100537508,263.342761539533,263.418388379871,263.494006076152,
263.569617576239,263.645257500866,263.689859409698,263.772138181552,263.854440744416,
263.937912546563,264.020267501462,264.104297727234,264.188327953006,264.270706963607,
264.353071152856,264.43650248872,264.518824462012,264.602810479163,264.686796496313,
264.762436605534,264.83805270844,264.913659275494,264.989293938203,265.064943496781,
265.140653786557,265.185265039621,265.202892592679),.UNSPECIFIED.);
#3012=B_SPLINE_CURVE_WITH_KNOTS('',3,(#140692,#140693,#140694,#140695,#140696,
#140697,#140698,#140699,#140700,#140701,#140702,#140703,#140704),
 .UNSPECIFIED.,.F.,.F.,(4,3,3,3,4),(265.202892592755,265.294397540302,265.385932105706,
265.477236696826,265.559741333664),.UNSPECIFIED.);
#3013=B_SPLINE_CURVE_WITH_KNOTS('',3,(#140706,#140707,#140708,#140709,#140710,
#140711,#140712,#140713,#140714,#140715,#140716,#140717,#140718,#140719,
#140720,#140721),.UNSPECIFIED.,.F.,.F.,(4,3,3,3,3,4),(-261.82024085972,
-261.741950618838,-261.663641105925,-261.585322321214,-261.506958996887,
-261.463653048573),.UNSPECIFIED.);
#3014=B_SPLINE_CURVE_WITH_KNOTS('',3,(#140722,#140723,#140724,#140725,#140726,
#140727,#140728,#140729,#140730,#140731,#140732,#140733,#140734,#140735,
#140736,#140737,#140738,#140739,#140740,#140741,#140742,#140743,#140744,
#140745,#140746,#140747,#140748,#140749,#140750,#140751,#140752,#140753,
#140754,#140755,#140756,#140757,#140758,#140759,#140760,#140761,#140762,
#140763,#140764,#140765,#140766,#140767,#140768,#140769,#140770,#140771,
#140772,#140773,#140774,#140775,#140776,#140777,#140778,#140779,#140780,
#140781,#140782,#140783,#140784,#140785,#140786,#140787,#140788,#140789,
#140790,#140791,#140792,#140793,#140794,#140795,#140796,#140797,#140798,
#140799,#140800,#140801,#140802,#140803,#140804,#140805,#140806,#140807,
#140808,#140809,#140810,#140811,#140812,#140813,#140814,#140815,#140816,
#140817,#140818,#140819,#140820,#140821,#140822,#140823,#140824,#140825,
#140826,#140827,#140828,#140829,#140830,#140831,#140832,#140833,#140834,
#140835,#140836,#140837,#140838,#140839,#140840,#140841,#140842,#140843,
#140844,#140845,#140846,#140847,#140848,#140849,#140850,#140851,#140852,
#140853,#140854,#140855,#140856,#140857,#140858,#140859,#140860,#140861,
#140862,#140863,#140864,#140865,#140866,#140867,#140868,#140869,#140870,
#140871,#140872,#140873,#140874,#140875,#140876,#140877,#140878,#140879,
#140880,#140881,#140882,#140883,#140884,#140885,#140886,#140887,#140888,
#140889,#140890,#140891,#140892,#140893,#140894,#140895,#140896,#140897,
#140898,#140899,#140900,#140901,#140902,#140903,#140904,#140905,#140906,
#140907,#140908,#140909,#140910,#140911,#140912,#140913,#140914,#140915,
#140916,#140917,#140918,#140919,#140920,#140921,#140922,#140923,#140924,
#140925,#140926,#140927,#140928,#140929,#140930,#140931,#140932,#140933,
#140934,#140935,#140936,#140937,#140938,#140939,#140940,#140941,#140942,
#140943,#140944,#140945,#140946,#140947,#140948,#140949,#140950,#140951,
#140952,#140953,#140954,#140955,#140956),.UNSPECIFIED.,.F.,.F.,(4,3,3,3,
3,3,3,3,3,3,3,3,3,3,3,3,3,3,3,3,3,3,3,3,3,3,3,3,3,3,3,3,3,3,3,3,3,3,3,3,
3,3,3,3,3,3,3,3,3,3,3,3,3,3,3,3,3,3,3,3,3,3,3,3,3,3,3,3,3,3,3,3,3,3,3,3,
3,3,4),(-261.463653048459,-261.365739326353,-261.266508210912,-261.19751669316,
-261.118524797823,-261.03963301315,-260.960830757107,-260.882130756287,
-260.80349131041,-260.724915028226,-260.699048149853,-260.620461426688,
-260.541825259424,-260.463129266106,-260.384315234622,-260.305433806398,
-260.22643071318,-260.200579606545,-260.121507084795,-260.04250753006,-259.963569262236,
-259.884680647755,-259.805830091199,-259.727001586933,-259.648185213064,
-259.569370461881,-259.490546827903,-259.411676780355,-259.332783101279,
-259.253822576442,-259.20364251993,-259.129537081829,-259.055488583975,
-258.981481845968,-258.907492581816,-258.833515220205,-258.759512934173,
-258.705173976623,-258.614174876885,-258.522671659206,-258.430728120274,
-258.338693543093,-258.246784452969,-258.206705433315,-258.130995762198,
-258.055334760173,-257.979707919836,-257.904090223555,-257.828478723469,
-257.752838798842,-257.708236890008,-257.625958118154,-257.543655555291,
-257.460183753144,-257.377828798245,-257.293798572473,-257.2097683467,-257.127389336097,
-257.045025146846,-256.961593810982,-256.879271837688,-256.79528582054,
-256.711299803392,-256.635659694172,-256.560043591267,-256.484437024215,
-256.408802361507,-256.33315280293,-256.257442513154,-256.212831260085,
-256.12093069038,-256.028897720663,-255.937018150839,-255.845390754807,
-255.754369633324,-255.714362716777,-255.640362204278,-255.566381661442,
-255.536653192137),.UNSPECIFIED.);
#3015=B_SPLINE_CURVE_WITH_KNOTS('',3,(#140962,#140963,#140964,#140965,#140966,
#140967,#140968,#140969,#140970,#140971,#140972,#140973,#140974,#140975,
#140976,#140977,#140978,#140979,#140980,#140981,#140982,#140983,#140984,
#140985,#140986,#140987,#140988,#140989,#140990,#140991,#140992,#140993,
#140994,#140995,#140996,#140997,#140998,#140999,#141000,#141001,#141002,
#141003,#141004,#141005,#141006,#141007,#141008,#141009,#141010,#141011,
#141012,#141013,#141014,#141015,#141016,#141017,#141018,#141019,#141020,
#141021,#141022,#141023,#141024,#141025,#141026,#141027,#141028,#141029,
#141030,#141031,#141032,#141033,#141034,#141035,#141036,#141037,#141038,
#141039,#141040,#141041,#141042,#141043,#141044,#141045,#141046,#141047,
#141048,#141049,#141050,#141051,#141052,#141053,#141054,#141055,#141056,
#141057,#141058,#141059,#141060,#141061,#141062,#141063,#141064,#141065,
#141066,#141067,#141068,#141069,#141070,#141071,#141072,#141073,#141074,
#141075,#141076,#141077,#141078,#141079,#141080,#141081,#141082,#141083,
#141084,#141085,#141086,#141087,#141088,#141089,#141090,#141091,#141092,
#141093,#141094,#141095,#141096,#141097,#141098,#141099,#141100,#141101,
#141102,#141103,#141104,#141105,#141106,#141107,#141108,#141109,#141110,
#141111,#141112,#141113,#141114,#141115,#141116,#141117,#141118,#141119,
#141120,#141121,#141122,#141123,#141124,#141125,#141126,#141127,#141128,
#141129,#141130,#141131,#141132,#141133,#141134,#141135,#141136,#141137,
#141138,#141139,#141140,#141141,#141142,#141143,#141144,#141145,#141146,
#141147,#141148,#141149,#141150,#141151,#141152,#141153,#141154,#141155,
#141156,#141157,#141158,#141159,#141160,#141161,#141162,#141163,#141164,
#141165,#141166,#141167,#141168,#141169,#141170,#141171,#141172,#141173,
#141174,#141175,#141176,#141177,#141178,#141179,#141180,#141181,#141182,
#141183,#141184,#141185,#141186,#141187,#141188,#141189,#141190,#141191,
#141192,#141193,#141194,#141195,#141196),.UNSPECIFIED.,.F.,.F.,(4,3,3,3,
3,3,3,3,3,3,3,3,3,3,3,3,3,3,3,3,3,3,3,3,3,3,3,3,3,3,3,3,3,3,3,3,3,3,3,3,
3,3,3,3,3,3,3,3,3,3,3,3,3,3,3,3,3,3,3,3,3,3,3,3,3,3,3,3,3,3,3,3,3,3,3,3,
3,3,4),(252.992365321722,253.072326619286,253.152399003248,253.222020000239,
253.301011895578,253.379903680253,253.458705936298,253.53740593712,253.616045382999,
253.694621665185,253.720488543547,253.799075266711,253.877711433975,253.956407427292,
254.035221458775,254.114102887,254.193105980216,254.218957086855,254.298029608604,
254.377029163339,254.455967431163,254.534856045644,254.6137066022,254.692535106466,
254.771351480335,254.850166231518,254.928989865496,255.007859913044,255.086753592119,
255.165714116956,255.21589417347,255.289999611571,255.364048109426,255.438054847432,
255.512044111584,255.586021473196,255.660023759229,255.714362716777,255.805361816515,
255.896865034194,255.988808573126,256.080843150307,256.17275224043,256.212831260085,
256.288540931202,256.364201933227,256.439828773564,256.515446469845,256.591057969931,
256.666697894558,256.711299803392,256.793578575246,256.875881138109,256.959352940256,
257.041707895155,257.125738120927,257.2097683467,257.292147357303,257.374511546554,
257.457942882418,257.540264855712,257.62425087286,257.708236890008,257.783876999228,
257.859493102133,257.935099669185,258.010734331894,258.08638389047,258.162094180246,
258.206705433315,258.298606003021,258.390638972737,258.482518542562,258.574145938593,
258.665167060077,258.705173976623,258.775894354609,258.847800819991,258.919707285374),
 .UNSPECIFIED.);
#3016=B_SPLINE_CURVE_WITH_KNOTS('',3,(#141197,#141198,#141199,#141200,#141201,
#141202,#141203,#141204,#141205,#141206,#141207,#141208,#141209,#141210,
#141211,#141212),.UNSPECIFIED.,.F.,.F.,(4,3,3,3,3,4),(258.919707285499,
258.998551910999,259.077463224529,259.156505125832,259.20364251993,259.275636793971),
 .UNSPECIFIED.);
#3017=B_SPLINE_CURVE_WITH_KNOTS('',3,(#141214,#141215,#141216,#141217,#141218,
#141219,#141220,#141221,#141222,#141223,#141224,#141225,#141226,#141227,
#141228,#141229,#141230,#141231,#141232),.UNSPECIFIED.,.F.,.F.,(4,3,3,3,
3,3,4),(-255.536653192137,-255.462676298287,-255.388657906524,-255.3146152606,
-255.240504027705,-255.21589417347,-255.180467741394),.UNSPECIFIED.);
#3018=B_SPLINE_CURVE_WITH_KNOTS('',3,(#141233,#141234,#141235,#141236,#141237,
#141238,#141239,#141240,#141241,#141242,#141243,#141244,#141245,#141246,
#141247,#141248,#141249,#141250,#141251,#141252,#141253,#141254,#141255,
#141256,#141257,#141258,#141259,#141260,#141261,#141262,#141263,#141264,
#141265,#141266,#141267,#141268,#141269,#141270,#141271,#141272,#141273,
#141274,#141275,#141276,#141277,#141278,#141279,#141280,#141281,#141282,
#141283,#141284,#141285,#141286,#141287,#141288,#141289,#141290,#141291,
#141292,#141293,#141294,#141295,#141296,#141297,#141298,#141299,#141300,
#141301,#141302,#141303,#141304,#141305,#141306,#141307,#141308,#141309,
#141310,#141311,#141312,#141313,#141314,#141315,#141316,#141317,#141318,
#141319,#141320,#141321,#141322,#141323,#141324,#141325,#141326,#141327,
#141328,#141329,#141330,#141331,#141332,#141333,#141334,#141335,#141336,
#141337,#141338,#141339,#141340,#141341,#141342,#141343,#141344,#141345,
#141346,#141347,#141348,#141349,#141350,#141351,#141352,#141353,#141354,
#141355,#141356,#141357,#141358,#141359,#141360,#141361,#141362,#141363,
#141364,#141365,#141366,#141367,#141368,#141369,#141370,#141371,#141372,
#141373,#141374,#141375,#141376,#141377,#141378,#141379,#141380,#141381,
#141382,#141383,#141384,#141385,#141386,#141387,#141388,#141389,#141390,
#141391,#141392,#141393,#141394,#141395,#141396,#141397,#141398,#141399,
#141400,#141401,#141402,#141403,#141404,#141405,#141406,#141407,#141408,
#141409,#141410,#141411,#141412,#141413,#141414,#141415,#141416,#141417,
#141418,#141419,#141420,#141421,#141422,#141423,#141424,#141425,#141426,
#141427,#141428,#141429,#141430,#141431,#141432,#141433,#141434,#141435,
#141436,#141437,#141438,#141439,#141440,#141441,#141442,#141443,#141444,
#141445,#141446,#141447,#141448,#141449,#141450,#141451,#141452,#141453,
#141454,#141455,#141456,#141457,#141458,#141459,#141460,#141461,#141462,
#141463,#141464,#141465,#141466,#141467,#141468,#141469,#141470),
 .UNSPECIFIED.,.F.,.F.,(4,3,3,3,3,3,3,3,3,3,3,3,3,3,3,3,3,3,3,3,3,3,3,3,
3,3,3,3,3,3,3,3,3,3,3,3,3,3,3,3,3,3,3,3,3,3,3,3,3,3,3,3,3,3,3,3,3,3,3,3,
3,3,3,3,3,3,3,3,3,3,3,3,3,3,3,3,3,3,3,4),(-255.180467741312,-255.101973116499,
-255.023538197481,-254.9451503052,-254.866796796049,-254.7858168324,-254.707481506871,
-254.6291405407,-254.550782482535,-254.472395872106,-254.393936405803,-254.315434389609,
-254.236847990182,-254.218957086855,-254.139965191516,-254.061073406842,
-253.982271150797,-253.903571149976,-253.824931704097,-253.746355421912,
-253.720488543547,-253.641901820383,-253.563265653119,-253.484569659802,
-253.405755628319,-253.326874200094,-253.247871106878,-253.222020000239,
-253.14294747849,-253.063947923755,-252.985009655931,-252.90612104145,-252.827270484893,
-252.748441980628,-252.669625606759,-252.590810855576,-252.511987221598,
-252.43311717405,-252.354223494975,-252.275262970138,-252.225082913624,
-252.150977475523,-252.076928977668,-252.002922239662,-251.92893297551,
-251.854955613898,-251.780953327865,-251.726614370317,-251.63561527058,
-251.544112052901,-251.452168513969,-251.360133936788,-251.268224846665,
-251.228145827009,-251.152436155892,-251.076775153867,-251.00114831353,
-250.925530617249,-250.849919117163,-250.774279192536,-250.729677283702,
-250.647398511848,-250.565095948984,-250.481624146836,-250.399269191937,
-250.315238966166,-250.231208740394,-250.148829729793,-250.066465540544,
-249.98303420468,-249.900712231388,-249.816726214238,-249.732740197087,
-249.657100291293,-249.581484716781,-249.50587900288,-249.43024848262,-249.35460320045,
-249.278904741001,-249.253903437549),.UNSPECIFIED.);
#3019=B_SPLINE_CURVE_WITH_KNOTS('',3,(#141476,#141477,#141478,#141479,#141480,
#141481,#141482,#141483,#141484,#141485,#141486,#141487,#141488,#141489,
#141490,#141491,#141492,#141493,#141494,#141495,#141496,#141497,#141498,
#141499,#141500,#141501,#141502,#141503,#141504,#141505,#141506,#141507,
#141508,#141509,#141510,#141511,#141512,#141513,#141514,#141515,#141516,
#141517,#141518,#141519,#141520,#141521,#141522,#141523,#141524,#141525,
#141526,#141527,#141528,#141529,#141530,#141531,#141532,#141533,#141534,
#141535,#141536,#141537,#141538,#141539,#141540,#141541,#141542,#141543,
#141544,#141545,#141546,#141547,#141548,#141549,#141550,#141551,#141552,
#141553,#141554,#141555,#141556,#141557,#141558,#141559,#141560,#141561,
#141562,#141563,#141564,#141565,#141566,#141567,#141568,#141569,#141570,
#141571,#141572,#141573,#141574,#141575,#141576,#141577,#141578,#141579,
#141580,#141581,#141582,#141583,#141584,#141585,#141586,#141587,#141588,
#141589,#141590,#141591,#141592,#141593,#141594,#141595,#141596,#141597,
#141598,#141599,#141600,#141601,#141602,#141603,#141604,#141605,#141606,
#141607,#141608,#141609,#141610,#141611,#141612,#141613,#141614,#141615,
#141616,#141617,#141618,#141619,#141620,#141621,#141622,#141623,#141624,
#141625,#141626,#141627,#141628,#141629,#141630,#141631,#141632,#141633,
#141634,#141635,#141636,#141637,#141638,#141639,#141640,#141641,#141642,
#141643,#141644,#141645,#141646,#141647,#141648,#141649,#141650,#141651,
#141652,#141653,#141654,#141655,#141656,#141657,#141658,#141659,#141660,
#141661,#141662,#141663,#141664,#141665,#141666,#141667,#141668,#141669,
#141670,#141671,#141672,#141673,#141674,#141675,#141676,#141677,#141678,
#141679,#141680,#141681,#141682,#141683,#141684,#141685,#141686,#141687,
#141688,#141689,#141690,#141691,#141692,#141693,#141694,#141695,#141696,
#141697,#141698,#141699,#141700,#141701,#141702,#141703,#141704,#141705,
#141706,#141707,#141708,#141709,#141710),.UNSPECIFIED.,.F.,.F.,(4,3,3,3,
3,3,3,3,3,3,3,3,3,3,3,3,3,3,3,3,3,3,3,3,3,3,3,3,3,3,3,3,3,3,3,3,3,3,3,3,
3,3,3,3,3,3,3,3,3,3,3,3,3,3,3,3,3,3,3,3,3,3,3,3,3,3,3,3,3,3,3,3,3,3,3,3,
3,3,4),(246.709703796838,246.741928937241,246.820515660405,246.899151827669,
246.977847820986,247.05666185247,247.135543280694,247.214546373911,247.240397480549,
247.319470002299,247.398469557034,247.477407824858,247.556296439339,247.635146995895,
247.71397550016,247.792791874029,247.871606625213,247.95043025919,248.029300306738,
248.108193985814,248.187154510651,248.237334567164,248.311440005265,248.385488503119,
248.459495241126,248.533484505278,248.60746186689,248.681464152923,248.735803110471,
248.826802210207,248.918305427884,249.010248966815,249.102283543994,249.194192634116,
249.234271653779,249.309981324897,249.385642326925,249.461269167263,249.536886863547,
249.612498363634,249.688138288263,249.732740197087,249.815018968939,249.897321531799,
249.980793333948,250.063148288844,250.147178514619,250.231208740394,250.313587750997,
250.395951940248,250.479383276112,250.561705249406,250.645691266554,250.729677283702,
250.805317392922,250.880933495828,250.95654006288,251.032174725589,251.107824284166,
251.183534573942,251.228145827009,251.320046396713,251.412079366429,251.503958936253,
251.595586332285,251.686607453767,251.726614370317,251.800616285004,251.874597213347,
251.948572235259,252.022584708558,252.096615978538,252.170720730742,252.225082913624,
252.31338252294,252.401525174677,252.489509903532,252.577143865673,252.636521978204),
 .UNSPECIFIED.);
#3020=B_SPLINE_CURVE_WITH_KNOTS('',3,(#141711,#141712,#141713,#141714,#141715,
#141716,#141717,#141718,#141719,#141720,#141721,#141722,#141723,#141724,
#141725,#141726),.UNSPECIFIED.,.F.,.F.,(4,3,3,3,3,4),(252.63652197832,252.716213408794,
252.795966776382,252.875752384699,252.955608181191,252.992365321722),
 .UNSPECIFIED.);
#3021=B_SPLINE_CURVE_WITH_KNOTS('',3,(#141728,#141729,#141730,#141731,#141732,
#141733,#141734,#141735,#141736,#141737,#141738,#141739,#141740,#141741,
#141742,#141743),.UNSPECIFIED.,.F.,.F.,(4,3,3,3,3,4),(-249.253903437549,
-249.234271653779,-249.139112369578,-249.043810942917,-248.94881027079,
-248.897282434214),.UNSPECIFIED.);
#3022=B_SPLINE_CURVE_WITH_KNOTS('',3,(#141744,#141745,#141746,#141747,#141748,
#141749,#141750,#141751,#141752,#141753,#141754,#141755,#141756,#141757,
#141758,#141759,#141760,#141761,#141762,#141763,#141764,#141765,#141766,
#141767,#141768,#141769,#141770,#141771,#141772,#141773,#141774,#141775,
#141776,#141777,#141778,#141779,#141780,#141781,#141782,#141783,#141784,
#141785,#141786,#141787,#141788,#141789,#141790,#141791,#141792,#141793,
#141794,#141795,#141796,#141797,#141798,#141799,#141800,#141801,#141802,
#141803,#141804,#141805,#141806,#141807,#141808,#141809,#141810,#141811,
#141812,#141813,#141814,#141815,#141816,#141817,#141818,#141819,#141820,
#141821,#141822,#141823,#141824,#141825,#141826,#141827,#141828,#141829,
#141830,#141831,#141832,#141833,#141834,#141835,#141836,#141837,#141838,
#141839,#141840,#141841,#141842,#141843,#141844,#141845,#141846,#141847,
#141848,#141849,#141850,#141851,#141852,#141853,#141854,#141855,#141856,
#141857,#141858,#141859,#141860,#141861,#141862,#141863,#141864,#141865,
#141866,#141867,#141868,#141869,#141870,#141871,#141872,#141873,#141874,
#141875,#141876,#141877,#141878,#141879,#141880,#141881,#141882,#141883,
#141884,#141885,#141886,#141887,#141888,#141889,#141890,#141891,#141892,
#141893,#141894,#141895,#141896,#141897,#141898,#141899,#141900,#141901,
#141902,#141903,#141904,#141905,#141906,#141907,#141908,#141909,#141910,
#141911,#141912,#141913,#141914,#141915,#141916,#141917,#141918,#141919,
#141920,#141921,#141922,#141923,#141924,#141925,#141926,#141927,#141928,
#141929,#141930,#141931,#141932,#141933,#141934,#141935,#141936,#141937,
#141938,#141939,#141940,#141941,#141942,#141943,#141944,#141945,#141946,
#141947,#141948,#141949,#141950,#141951,#141952,#141953,#141954,#141955,
#141956,#141957,#141958,#141959,#141960,#141961,#141962,#141963),
 .UNSPECIFIED.,.F.,.F.,(4,3,3,3,3,3,3,3,3,3,3,3,3,3,3,3,3,3,3,3,3,3,3,3,
3,3,3,3,3,3,3,3,3,3,3,3,3,3,3,3,3,3,3,3,3,3,3,3,3,3,3,3,3,3,3,3,3,3,3,3,
3,3,3,3,3,3,3,3,3,3,3,3,3,4),(-248.897282434214,-248.815552560448,-248.733822806678,
-248.652093171236,-248.570363652457,-248.488634248674,-248.406904958219,
-248.3219581897,-248.238338714439,-248.156025793479,-248.074286884412,-247.992548395025,
-247.910810318645,-247.829072648598,-247.747335378209,-247.665598500806,
-247.583862009716,-247.502125898266,-247.420390159784,-247.338654787598,
-247.256919775036,-247.175185115427,-247.093450802099,-247.011716828383,
-246.929983187607,-246.848249873102,-246.766516878198,-246.684784196225,
-246.603051820513,-246.521319744394,-246.439587961198,-246.357856464257,
-246.276125246904,-246.194394302469,-246.112663624285,-246.030933205684,
-245.949203039999,-245.867473120562,-245.785743440707,-245.704013993766,
-245.618585799367,-245.535827236043,-245.45408860848,-245.372350804676,
-245.290613797936,-245.208877561568,-245.127142068883,-245.045407293192,
-244.963673207811,-244.881939786059,-244.800207001254,-244.718474826718,
-244.636743235777,-244.555012201756,-244.473281697984,-244.391551697789,
-244.309822174504,-244.22610277441,-244.144364693382,-244.062628197957,
-243.980893181373,-243.899159536884,-243.817427157767,-243.735695937314,
-243.653965768834,-243.568509019354,-243.486772101135,-243.405038092231,
-243.323306565712,-243.241577094784,-243.159842204308,-243.078112124143,
-242.996380695082,-242.970311772993),.UNSPECIFIED.);
#3023=B_SPLINE_CURVE_WITH_KNOTS('',3,(#141969,#141970,#141971,#141972,#141973,
#141974,#141975,#141976,#141977,#141978,#141979,#141980,#141981,#141982,
#141983,#141984,#141985,#141986,#141987,#141988,#141989,#141990,#141991,
#141992,#141993,#141994,#141995,#141996,#141997,#141998,#141999,#142000,
#142001,#142002,#142003,#142004,#142005,#142006,#142007,#142008,#142009,
#142010,#142011,#142012,#142013,#142014,#142015,#142016,#142017,#142018,
#142019,#142020,#142021,#142022,#142023,#142024,#142025,#142026,#142027,
#142028,#142029,#142030,#142031,#142032,#142033,#142034,#142035,#142036,
#142037,#142038,#142039,#142040,#142041,#142042,#142043,#142044,#142045,
#142046,#142047,#142048,#142049,#142050,#142051,#142052,#142053,#142054,
#142055,#142056,#142057,#142058,#142059,#142060,#142061,#142062,#142063,
#142064,#142065,#142066,#142067,#142068,#142069,#142070,#142071,#142072,
#142073,#142074,#142075,#142076,#142077,#142078,#142079,#142080,#142081,
#142082,#142083,#142084,#142085,#142086,#142087,#142088,#142089,#142090,
#142091,#142092,#142093,#142094,#142095,#142096,#142097,#142098,#142099,
#142100,#142101,#142102,#142103,#142104,#142105,#142106,#142107,#142108,
#142109,#142110,#142111,#142112,#142113,#142114,#142115,#142116,#142117,
#142118,#142119,#142120,#142121,#142122,#142123,#142124,#142125,#142126,
#142127,#142128,#142129,#142130,#142131,#142132,#142133,#142134,#142135,
#142136,#142137,#142138,#142139,#142140,#142141,#142142,#142143,#142144,
#142145,#142146,#142147,#142148,#142149,#142150,#142151,#142152,#142153,
#142154,#142155,#142156,#142157,#142158,#142159,#142160,#142161,#142162,
#142163,#142164,#142165,#142166,#142167,#142168,#142169,#142170,#142171,
#142172,#142173,#142174,#142175,#142176,#142177,#142178,#142179,#142180,
#142181,#142182,#142183,#142184,#142185,#142186,#142187,#142188,#142189,
#142190,#142191,#142192,#142193,#142194,#142195,#142196,#142197,#142198,
#142199,#142200),.UNSPECIFIED.,.F.,.F.,(4,3,3,3,3,3,3,3,3,3,3,3,3,3,3,3,
3,3,3,3,3,3,3,3,3,3,3,3,3,3,3,3,3,3,3,3,3,3,3,3,3,3,3,3,3,3,3,3,3,3,3,3,
3,3,3,3,3,3,3,3,3,3,3,3,3,3,3,3,3,3,3,3,3,3,3,3,3,4),(240.426626170505,
240.505559763057,240.584444689868,240.663292543497,240.742119607048,240.820935434143,
240.899750532045,240.97857540635,241.057447086753,241.136343221325,241.215305082781,
241.258774960858,241.33288039896,241.406928896815,241.480935634822,241.554924898975,
241.628902260588,241.702904546621,241.757243504166,241.8482426039,241.939745821575,
242.031689360503,242.12372393768,242.215633027799,242.255712047473,242.331421718591,
242.407082720618,242.482709560957,242.55832725724,242.633938757327,242.709578681956,
242.754180590781,242.836459362633,242.918761925495,243.002233727643,243.08458868254,
243.168618908314,243.252649134088,243.335028144691,243.417392333942,243.500823669805,
243.583145643099,243.667131660248,243.751117677396,243.826757786617,243.902373889522,
243.977980456575,244.053615119284,244.129264677861,244.204974967637,244.249586220703,
244.341486790406,244.433519760121,244.525399329943,244.617026725973,244.708047847455,
244.748054764011,244.8220566787,244.896037607043,244.970012628957,245.044025102257,
245.118056372239,245.192161124444,245.246523307319,245.325484723266,245.404392146335,
245.483257185272,245.562091415997,245.640906389976,245.719727653636,245.798554292748,
245.877396817124,245.956265745707,246.035207797038,246.114188562527,246.193259573544,
246.243460393934,246.35333667114),.UNSPECIFIED.);
#3024=B_SPLINE_CURVE_WITH_KNOTS('',3,(#142201,#142202,#142203,#142204,#142205,
#142206,#142207,#142208,#142209,#142210,#142211,#142212,#142213,#142214,
#142215,#142216),.UNSPECIFIED.,.F.,.F.,(4,3,3,3,3,4),(246.353336671251,
246.429405639111,246.505380470581,246.581301005019,246.657176301325,246.709703796838),
 .UNSPECIFIED.);
#3025=B_SPLINE_CURVE_WITH_KNOTS('',3,(#142218,#142219,#142220,#142221,#142222,
#142223,#142224,#142225,#142226,#142227,#142228,#142229,#142230,#142231,
#142232,#142233),.UNSPECIFIED.,.F.,.F.,(4,3,3,3,3,4),(-242.970311772993,
-242.888582229157,-242.806847114238,-242.725116876889,-242.643385087938,
-242.614097127035),.UNSPECIFIED.);
#3026=B_SPLINE_CURVE_WITH_KNOTS('',3,(#142234,#142235,#142236,#142237,#142238,
#142239,#142240,#142241,#142242,#142243,#142244,#142245,#142246,#142247,
#142248,#142249,#142250,#142251,#142252,#142253,#142254,#142255,#142256,
#142257,#142258,#142259,#142260,#142261,#142262,#142263,#142264,#142265,
#142266,#142267,#142268,#142269,#142270,#142271,#142272,#142273,#142274,
#142275,#142276,#142277,#142278,#142279,#142280,#142281,#142282,#142283,
#142284,#142285,#142286,#142287,#142288,#142289,#142290,#142291,#142292,
#142293,#142294,#142295,#142296,#142297,#142298,#142299,#142300,#142301,
#142302,#142303,#142304,#142305,#142306,#142307,#142308,#142309,#142310,
#142311,#142312,#142313,#142314,#142315,#142316,#142317,#142318,#142319,
#142320,#142321,#142322,#142323,#142324,#142325,#142326,#142327,#142328,
#142329,#142330,#142331,#142332,#142333,#142334,#142335,#142336,#142337,
#142338,#142339,#142340,#142341,#142342,#142343,#142344,#142345,#142346,
#142347,#142348,#142349,#142350,#142351,#142352,#142353,#142354,#142355,
#142356,#142357,#142358,#142359,#142360,#142361,#142362,#142363,#142364,
#142365,#142366,#142367,#142368,#142369,#142370,#142371,#142372,#142373,
#142374,#142375,#142376,#142377,#142378,#142379,#142380,#142381,#142382,
#142383,#142384,#142385,#142386,#142387,#142388,#142389,#142390,#142391,
#142392,#142393,#142394,#142395,#142396,#142397,#142398,#142399,#142400,
#142401,#142402,#142403,#142404,#142405,#142406,#142407,#142408,#142409,
#142410,#142411,#142412,#142413,#142414,#142415,#142416,#142417,#142418,
#142419,#142420,#142421,#142422,#142423,#142424,#142425,#142426,#142427,
#142428,#142429,#142430,#142431,#142432,#142433,#142434,#142435,#142436,
#142437,#142438,#142439,#142440,#142441,#142442,#142443,#142444,#142445,
#142446,#142447,#142448,#142449,#142450,#142451,#142452,#142453,#142454,
#142455,#142456,#142457,#142458,#142459,#142460,#142461,#142462,#142463,
#142464,#142465,#142466,#142467,#142468,#142469,#142470,#142471),
 .UNSPECIFIED.,.F.,.F.,(4,3,3,3,3,3,3,3,3,3,3,3,3,3,3,3,3,3,3,3,3,3,3,3,
3,3,3,3,3,3,3,3,3,3,3,3,3,3,3,3,3,3,3,3,3,3,3,3,3,3,3,3,3,3,3,3,3,3,3,3,
3,3,3,3,3,3,3,3,3,3,3,3,3,3,3,3,3,3,3,4),(-242.614097127035,-242.53872344443,
-242.463324904272,-242.387914432477,-242.3124425137,-242.255712047473,-242.163811477774,
-242.071778508064,-241.979898938246,-241.88827154222,-241.797250420742,
-241.757243504166,-241.683241589477,-241.609260661133,-241.53528563922,
-241.461273165919,-241.387241895937,-241.313137143731,-241.258774960858,
-241.179813544911,-241.100906121842,-241.022041082906,-240.94320685218,
-240.864391878201,-240.785570614541,-240.706743975429,-240.627901451053,
-240.54903252247,-240.470090471139,-240.391109705651,-240.312038694633,
-240.261837874243,-240.182845978904,-240.103954194229,-240.025151938184,
-239.946451937363,-239.867812491484,-239.789236209298,-239.763369330935,
-239.684782607772,-239.606146440509,-239.527450447193,-239.448636415711,
-239.369754987488,-239.290751894272,-239.264900787628,-239.185828265879,
-239.106828711144,-239.02789044332,-238.949001828839,-238.870151272282,
-238.791322768017,-238.712506394148,-238.633691642964,-238.554868008987,
-238.475997961439,-238.397104282363,-238.318143757526,-238.267963701013,
-238.19385826291,-238.119809765055,-238.045803027048,-237.971813762894,
-237.897836401282,-237.823834115248,-237.769495157705,-237.678496057971,
-237.586992840297,-237.495049301369,-237.403014724192,-237.311105634074,
-237.271026614398,-237.19531694328,-237.119655941254,-237.044029100915,
-236.968411404632,-236.892799904545,-236.817159979917,-236.77255807109,
-236.687327340016),.UNSPECIFIED.);
#3027=B_SPLINE_CURVE_WITH_KNOTS('',3,(#142477,#142478,#142479,#142480,#142481,
#142482,#142483,#142484,#142485,#142486,#142487,#142488,#142489,#142490,
#142491,#142492,#142493,#142494,#142495,#142496,#142497,#142498,#142499,
#142500,#142501,#142502,#142503,#142504,#142505,#142506,#142507,#142508,
#142509,#142510,#142511,#142512,#142513,#142514,#142515,#142516,#142517,
#142518,#142519,#142520,#142521,#142522,#142523,#142524,#142525,#142526,
#142527,#142528,#142529,#142530,#142531,#142532,#142533,#142534,#142535,
#142536,#142537,#142538,#142539,#142540,#142541,#142542,#142543,#142544,
#142545,#142546,#142547,#142548,#142549,#142550,#142551,#142552,#142553,
#142554,#142555,#142556,#142557,#142558,#142559,#142560,#142561,#142562,
#142563,#142564,#142565,#142566,#142567,#142568,#142569,#142570,#142571,
#142572,#142573,#142574,#142575,#142576,#142577,#142578,#142579,#142580,
#142581,#142582,#142583,#142584,#142585,#142586,#142587,#142588,#142589,
#142590,#142591,#142592,#142593,#142594,#142595,#142596,#142597,#142598,
#142599,#142600,#142601,#142602,#142603,#142604,#142605,#142606,#142607,
#142608,#142609,#142610,#142611,#142612,#142613,#142614,#142615,#142616,
#142617,#142618,#142619,#142620,#142621,#142622,#142623,#142624,#142625,
#142626,#142627,#142628,#142629,#142630,#142631,#142632,#142633,#142634,
#142635,#142636,#142637,#142638,#142639,#142640,#142641,#142642,#142643,
#142644,#142645,#142646,#142647,#142648,#142649,#142650,#142651,#142652,
#142653,#142654,#142655,#142656,#142657,#142658,#142659,#142660,#142661,
#142662,#142663,#142664,#142665,#142666,#142667,#142668,#142669,#142670,
#142671,#142672,#142673,#142674,#142675,#142676,#142677,#142678,#142679,
#142680,#142681,#142682,#142683,#142684,#142685,#142686,#142687,#142688,
#142689,#142690,#142691,#142692,#142693,#142694,#142695,#142696,#142697,
#142698,#142699,#142700,#142701,#142702,#142703,#142704,#142705,#142706,
#142707,#142708,#142709,#142710,#142711),.UNSPECIFIED.,.F.,.F.,(4,3,3,3,
3,3,3,3,3,3,3,3,3,3,3,3,3,3,3,3,3,3,3,3,3,3,3,3,3,3,3,3,3,3,3,3,3,3,3,3,
3,3,3,3,3,3,3,3,3,3,3,3,3,3,3,3,3,3,3,3,3,3,3,3,3,3,3,3,3,3,3,3,3,3,3,3,
3,3,4),(234.143309340879,234.227320887716,234.280215354552,234.354320792655,
234.42836929051,234.502376028518,234.576365292671,234.650342654284,234.724344940318,
234.77868389786,234.869682997594,234.961186215269,235.053129754197,235.145164331373,
235.237073421492,235.277152441167,235.352862112285,235.428523114311,235.504149954649,
235.579767650931,235.655379151018,235.731019075646,235.775620984475,235.857899756329,
235.940202319193,236.023674121341,236.10602907624,236.190059302011,236.274089527783,
236.356468538383,236.438832727631,236.522264063496,236.604586036787,236.688572053938,
236.77255807109,236.848198180312,236.923814283219,236.999420850274,237.075055512984,
237.150705071563,237.226415361341,237.271026614398,237.362927184098,237.45496015381,
237.54683972363,237.638467119658,237.729488241138,237.769495157705,237.843497072394,
237.917478000738,237.991453022651,238.065465495951,238.139496765933,238.213601518138,
238.267963701013,238.34692511696,238.42583254003,238.504697578966,238.583531809693,
238.662346783672,238.741168047332,238.819994686445,238.898837210821,238.977706139405,
239.056648190736,239.135628956225,239.214699967243,239.264900787628,239.343892682965,
239.422784467639,239.501586723681,239.580286724501,239.658926170379,239.737502452563,
239.763369330935,239.84006483917,239.914714461518,239.992432912695,240.070151363873),
 .UNSPECIFIED.);
#3028=B_SPLINE_CURVE_WITH_KNOTS('',3,(#142712,#142713,#142714,#142715,#142716,
#142717,#142718,#142719,#142720,#142721,#142722,#142723,#142724),
 .UNSPECIFIED.,.F.,.F.,(4,3,3,3,4),(240.070151363961,240.165994619102,240.261837874243,
240.344232022374,240.426626170505),.UNSPECIFIED.);
#3029=B_SPLINE_CURVE_WITH_KNOTS('',3,(#142726,#142727,#142728,#142729,#142730,
#142731,#142732,#142733,#142734,#142735,#142736,#142737,#142738,#142739,
#142740,#142741),.UNSPECIFIED.,.F.,.F.,(4,3,3,3,3,4),(-236.687327340016,
-236.605018875511,-236.522672705988,-236.440315080971,-236.35793754469,
-236.330911819855),.UNSPECIFIED.);
#3030=B_SPLINE_CURVE_WITH_KNOTS('',3,(#142742,#142743,#142744,#142745,#142746,
#142747,#142748,#142749,#142750,#142751,#142752,#142753,#142754,#142755,
#142756,#142757,#142758,#142759,#142760,#142761,#142762,#142763,#142764,
#142765,#142766,#142767,#142768,#142769,#142770,#142771,#142772,#142773,
#142774,#142775,#142776,#142777,#142778,#142779,#142780,#142781,#142782,
#142783,#142784,#142785,#142786,#142787,#142788,#142789,#142790,#142791,
#142792,#142793,#142794,#142795,#142796,#142797,#142798,#142799,#142800,
#142801,#142802,#142803,#142804,#142805,#142806,#142807,#142808,#142809,
#142810,#142811,#142812,#142813,#142814,#142815,#142816,#142817,#142818,
#142819,#142820,#142821,#142822,#142823,#142824,#142825,#142826,#142827,
#142828,#142829,#142830,#142831,#142832,#142833,#142834,#142835,#142836,
#142837,#142838,#142839,#142840,#142841,#142842,#142843,#142844,#142845,
#142846,#142847,#142848,#142849,#142850,#142851,#142852,#142853,#142854,
#142855,#142856,#142857,#142858,#142859,#142860,#142861,#142862,#142863,
#142864,#142865,#142866,#142867,#142868,#142869,#142870,#142871,#142872,
#142873,#142874,#142875,#142876,#142877,#142878,#142879,#142880,#142881,
#142882,#142883,#142884,#142885,#142886,#142887,#142888,#142889,#142890,
#142891,#142892,#142893,#142894,#142895,#142896,#142897,#142898,#142899,
#142900,#142901,#142902,#142903,#142904,#142905,#142906,#142907,#142908,
#142909,#142910,#142911,#142912,#142913,#142914,#142915,#142916,#142917,
#142918,#142919,#142920,#142921,#142922,#142923,#142924,#142925,#142926,
#142927,#142928,#142929,#142930,#142931,#142932,#142933,#142934,#142935,
#142936,#142937,#142938,#142939,#142940,#142941,#142942,#142943,#142944,
#142945,#142946,#142947,#142948,#142949,#142950,#142951,#142952,#142953,
#142954,#142955,#142956,#142957,#142958,#142959,#142960,#142961,#142962,
#142963,#142964,#142965,#142966,#142967,#142968,#142969,#142970,#142971,
#142972,#142973,#142974,#142975,#142976,#142977,#142978,#142979),
 .UNSPECIFIED.,.F.,.F.,(4,3,3,3,3,3,3,3,3,3,3,3,3,3,3,3,3,3,3,3,3,3,3,3,
3,3,3,3,3,3,3,3,3,3,3,3,3,3,3,3,3,3,3,3,3,3,3,3,3,3,3,3,3,3,3,3,3,3,3,3,
3,3,3,3,3,3,3,3,3,3,3,3,3,3,3,3,3,3,3,4),(-236.330911819752,-236.274089527782,
-236.191710517193,-236.109346327957,-236.025914992087,-235.943593018808,
-235.859607001641,-235.775620984475,-235.69998087525,-235.62436477234,-235.548758205282,
-235.473123542569,-235.397473983987,-235.321763694207,-235.277152441167,
-235.185251871468,-235.093218901759,-235.001339331941,-234.909711935916,
-234.818690814438,-234.77868389786,-234.704681983171,-234.630701054827,
-234.556726032914,-234.482713559614,-234.408682289632,-234.334577537427,
-234.280215354552,-234.201253938605,-234.122346515535,-234.043481476598,
-233.964647245872,-233.885832271893,-233.807011008233,-233.728184369121,
-233.649341844744,-233.570472916161,-233.491530864829,-233.412550099341,
-233.333479088322,-233.283278267937,-233.2042863726,-233.125394587926,-233.046592331883,
-232.967892331062,-232.889252885185,-232.810676603001,-232.78480972463,
-232.706223001466,-232.627586834202,-232.548890840884,-232.470076809401,
-232.391195381176,-232.312192287959,-232.286341181322,-232.207268659573,
-232.128269104838,-232.049330837014,-231.970442222533,-231.891591665977,
-231.812763161711,-231.733946787842,-231.655132036659,-231.576308402681,
-231.497438355133,-231.418544676057,-231.339584151221,-231.289404094707,
-231.215298656605,-231.14125015875,-231.067243420743,-230.99325415659,-230.919276794977,
-230.845274508944,-230.790935551399,-230.700035430836,-230.608423997618,
-230.516541195554,-230.424506658068,-230.403871264419),.UNSPECIFIED.);
#3031=B_SPLINE_CURVE_WITH_KNOTS('',3,(#142985,#142986,#142987,#142988,#142989,
#142990,#142991,#142992,#142993,#142994,#142995,#142996,#142997,#142998,
#142999,#143000,#143001,#143002,#143003,#143004,#143005,#143006,#143007,
#143008,#143009,#143010,#143011,#143012,#143013,#143014,#143015,#143016,
#143017,#143018,#143019,#143020,#143021,#143022,#143023,#143024,#143025,
#143026,#143027,#143028,#143029,#143030,#143031,#143032,#143033,#143034,
#143035,#143036,#143037,#143038,#143039,#143040,#143041,#143042,#143043,
#143044,#143045,#143046,#143047,#143048,#143049,#143050,#143051,#143052,
#143053,#143054,#143055,#143056,#143057,#143058,#143059,#143060,#143061,
#143062,#143063,#143064,#143065,#143066,#143067,#143068,#143069,#143070,
#143071,#143072,#143073,#143074,#143075,#143076,#143077,#143078,#143079,
#143080,#143081,#143082,#143083,#143084,#143085,#143086,#143087,#143088,
#143089,#143090,#143091,#143092,#143093,#143094,#143095,#143096,#143097,
#143098,#143099,#143100,#143101,#143102,#143103,#143104,#143105,#143106,
#143107,#143108,#143109,#143110,#143111,#143112,#143113,#143114,#143115,
#143116,#143117,#143118,#143119,#143120,#143121,#143122,#143123,#143124,
#143125,#143126,#143127,#143128,#143129,#143130,#143131,#143132,#143133,
#143134,#143135,#143136,#143137,#143138,#143139,#143140,#143141,#143142,
#143143,#143144,#143145,#143146,#143147,#143148,#143149,#143150,#143151,
#143152,#143153,#143154,#143155,#143156,#143157,#143158,#143159,#143160,
#143161,#143162,#143163,#143164,#143165,#143166,#143167,#143168,#143169,
#143170,#143171,#143172,#143173,#143174,#143175,#143176,#143177,#143178,
#143179,#143180,#143181,#143182,#143183,#143184,#143185,#143186,#143187,
#143188,#143189,#143190,#143191,#143192,#143193,#143194,#143195,#143196,
#143197,#143198,#143199,#143200,#143201,#143202,#143203,#143204,#143205,
#143206,#143207,#143208,#143209,#143210,#143211,#143212,#143213,#143214,
#143215,#143216,#143217,#143218,#143219),.UNSPECIFIED.,.F.,.F.,(4,3,3,3,
3,3,3,3,3,3,3,3,3,3,3,3,3,3,3,3,3,3,3,3,3,3,3,3,3,3,3,3,3,3,3,3,3,3,3,3,
3,3,3,3,3,3,3,3,3,3,3,3,3,3,3,3,3,3,3,3,3,3,3,3,3,3,3,3,3,3,3,3,3,3,3,3,
3,3,4),(227.859336579383,227.950680999062,228.042561426182,228.134579702056,
228.226520588781,228.298592834862,228.374302505979,228.449963508003,228.52559034834,
228.601208044621,228.676819544707,228.752459469334,228.797061378169,228.879340150024,
228.961642712888,229.045114515035,229.127469469934,229.211499695706,229.295529921477,
229.377908932078,229.460273121326,229.543704457191,229.626026430483,229.710012447633,
229.793998464784,229.869638574006,229.945254676912,230.020861243967,230.096495906677,
230.172145465256,230.247855755033,230.292467008092,230.384367577794,230.476400547506,
230.568280117326,230.659907513352,230.750928634833,230.790935551399,230.864937466087,
230.938918394431,231.012893416344,231.086905889644,231.160937159626,231.235041911832,
231.289404094707,231.368365510654,231.447272933724,231.52613797266,231.604972203387,
231.683787177365,231.762608441025,231.841435080137,231.920277604514,231.999146533096,
232.078088584428,232.157069349917,232.236140360935,232.286341181322,232.365333076661,
232.444224861336,232.523027117381,232.601727118202,232.68036656408,232.758942846266,
232.78480972463,232.863396447793,232.942032615055,233.02072860837,233.099542639852,
233.178424068074,233.257427161289,233.283278267937,233.365646306409,233.447916375147,
233.532678795556,233.614707660166,233.700836858474,233.782651577588,233.786966056781),
 .UNSPECIFIED.);
#3032=B_SPLINE_CURVE_WITH_KNOTS('',3,(#143220,#143221,#143222,#143223,#143224,
#143225,#143226,#143227,#143228,#143229,#143230,#143231,#143232,#143233,
#143234,#143235),.UNSPECIFIED.,.F.,.F.,(4,3,3,3,3,4),(233.786966674316,
233.870479334874,233.954172167115,234.0379522201,234.121843783026,234.143309340879),
 .UNSPECIFIED.);
#3033=B_SPLINE_CURVE_WITH_KNOTS('',3,(#143237,#143238,#143239,#143240,#143241,
#143242,#143243,#143244,#143245,#143246,#143247,#143248,#143249,#143250,
#143251,#143252,#143253,#143254,#143255),.UNSPECIFIED.,.F.,.F.,(4,3,3,3,
3,3,4),(-230.403871264419,-230.311987089053,-230.292467008092,-230.215986240579,
-230.139557082451,-230.063172142902,-230.047726512675),.UNSPECIFIED.);
#3034=B_SPLINE_CURVE_WITH_KNOTS('',3,(#143256,#143257,#143258,#143259,#143260,
#143261,#143262,#143263,#143264,#143265,#143266,#143267,#143268,#143269,
#143270,#143271,#143272,#143273,#143274,#143275,#143276,#143277,#143278,
#143279,#143280,#143281,#143282,#143283,#143284,#143285,#143286,#143287,
#143288,#143289,#143290,#143291,#143292,#143293,#143294,#143295,#143296,
#143297,#143298,#143299,#143300,#143301,#143302,#143303,#143304,#143305,
#143306,#143307,#143308,#143309,#143310,#143311,#143312,#143313,#143314,
#143315,#143316,#143317,#143318,#143319,#143320,#143321,#143322,#143323,
#143324,#143325,#143326,#143327,#143328,#143329,#143330,#143331,#143332,
#143333,#143334,#143335,#143336,#143337,#143338,#143339,#143340,#143341,
#143342,#143343,#143344,#143345,#143346,#143347,#143348,#143349,#143350,
#143351,#143352,#143353,#143354,#143355,#143356,#143357,#143358,#143359,
#143360,#143361,#143362,#143363,#143364,#143365,#143366,#143367,#143368,
#143369,#143370,#143371,#143372,#143373,#143374,#143375,#143376,#143377,
#143378,#143379,#143380,#143381,#143382,#143383,#143384,#143385,#143386,
#143387,#143388,#143389,#143390,#143391,#143392,#143393,#143394,#143395,
#143396,#143397,#143398,#143399,#143400,#143401,#143402,#143403,#143404,
#143405,#143406,#143407,#143408,#143409,#143410,#143411,#143412,#143413,
#143414,#143415,#143416,#143417,#143418,#143419,#143420,#143421,#143422,
#143423,#143424,#143425,#143426,#143427,#143428,#143429,#143430,#143431,
#143432,#143433,#143434,#143435,#143436,#143437,#143438,#143439,#143440,
#143441,#143442,#143443,#143444,#143445,#143446,#143447,#143448,#143449,
#143450,#143451,#143452,#143453,#143454,#143455,#143456,#143457,#143458,
#143459,#143460,#143461,#143462,#143463,#143464,#143465,#143466,#143467,
#143468,#143469,#143470,#143471,#143472,#143473,#143474,#143475),
 .UNSPECIFIED.,.F.,.F.,(4,3,3,3,3,3,3,3,3,3,3,3,3,3,3,3,3,3,3,3,3,3,3,3,
3,3,3,3,3,3,3,3,3,3,3,3,3,3,3,3,3,3,3,3,3,3,3,3,3,3,3,3,3,3,3,3,3,3,3,3,
3,3,3,3,3,3,3,3,3,3,3,3,3,4),(-230.047726512675,-229.965996638909,-229.884266885139,
-229.802537249697,-229.720807730918,-229.639078327135,-229.557349036681,
-229.472402268161,-229.3887827929,-229.30646987194,-229.224730962873,-229.142992473487,
-229.061254397107,-228.979516727059,-228.897779456671,-228.816042579268,
-228.734306088178,-228.652569976728,-228.570834238246,-228.489098866059,
-228.407363853497,-228.325629193888,-228.243894880561,-228.162160906845,
-228.080427266069,-227.998693951564,-227.91696095666,-227.835228274686,
-227.753495898974,-227.671763822855,-227.59003203966,-227.508300542719,
-227.426569325366,-227.344838380931,-227.263107702746,-227.181377284145,
-227.09964711846,-227.017917199024,-226.936187519169,-226.854458072228,
-226.769029877829,-226.686271314505,-226.604532686942,-226.522794883138,
-226.441057876398,-226.35932164003,-226.277586147345,-226.195851371654,
-226.114117286273,-226.032383864521,-225.950651079716,-225.86891890518,
-225.787187314239,-225.705456280218,-225.623725776446,-225.541995776251,
-225.460266252966,-225.376546852872,-225.294808771843,-225.213072276419,
-225.131337259834,-225.049603615346,-224.967871236229,-224.886140015776,
-224.804409847296,-224.718953097815,-224.637216179596,-224.555482170693,
-224.473750644174,-224.392021173245,-224.310286282769,-224.228556202604,
-224.146824773543,-224.120755851454),.UNSPECIFIED.);
#3035=B_SPLINE_CURVE_WITH_KNOTS('',3,(#143481,#143482,#143483,#143484,#143485,
#143486,#143487,#143488,#143489,#143490,#143491,#143492,#143493,#143494,
#143495,#143496,#143497,#143498,#143499,#143500,#143501,#143502,#143503,
#143504,#143505,#143506,#143507,#143508,#143509,#143510,#143511,#143512,
#143513,#143514,#143515,#143516,#143517,#143518,#143519,#143520,#143521,
#143522,#143523,#143524,#143525,#143526,#143527,#143528,#143529,#143530,
#143531,#143532,#143533,#143534,#143535,#143536,#143537,#143538,#143539,
#143540,#143541,#143542,#143543,#143544,#143545,#143546,#143547,#143548,
#143549,#143550,#143551,#143552,#143553,#143554,#143555,#143556,#143557,
#143558,#143559,#143560,#143561,#143562,#143563,#143564,#143565,#143566,
#143567,#143568,#143569,#143570,#143571,#143572,#143573,#143574,#143575,
#143576,#143577,#143578,#143579,#143580,#143581,#143582,#143583,#143584,
#143585,#143586,#143587,#143588,#143589,#143590,#143591,#143592,#143593,
#143594,#143595,#143596,#143597,#143598,#143599,#143600,#143601,#143602,
#143603,#143604,#143605,#143606,#143607,#143608,#143609,#143610,#143611,
#143612,#143613,#143614,#143615,#143616,#143617,#143618,#143619,#143620,
#143621,#143622,#143623,#143624,#143625,#143626,#143627,#143628,#143629,
#143630,#143631,#143632,#143633,#143634,#143635,#143636,#143637,#143638,
#143639,#143640,#143641,#143642,#143643,#143644,#143645,#143646,#143647,
#143648,#143649,#143650,#143651,#143652,#143653,#143654,#143655,#143656,
#143657,#143658,#143659,#143660,#143661,#143662,#143663,#143664,#143665,
#143666,#143667,#143668,#143669,#143670,#143671,#143672,#143673,#143674,
#143675,#143676,#143677,#143678,#143679,#143680,#143681,#143682,#143683,
#143684,#143685,#143686,#143687,#143688,#143689,#143690,#143691,#143692,
#143693,#143694,#143695,#143696,#143697,#143698,#143699,#143700,#143701,
#143702,#143703,#143704,#143705,#143706,#143707,#143708,#143709,#143710,
#143711,#143712,#143713,#143714,#143715,#143716,#143717,#143718),
 .UNSPECIFIED.,.F.,.F.,(4,3,3,3,3,3,3,3,3,3,3,3,3,3,3,3,3,3,3,3,3,3,3,3,
3,3,3,3,3,3,3,3,3,3,3,3,3,3,3,3,3,3,3,3,3,3,3,3,3,3,3,3,3,3,3,3,3,3,3,3,
3,3,3,3,3,3,3,3,3,3,3,3,3,3,3,3,3,3,3,4),(221.577058603984,221.652672288649,
221.728284922499,221.80392501773,221.818501771863,221.900780543719,221.983083106584,
222.066554908731,222.148909863632,222.232940089401,222.316970315171,222.399349325771,
222.481713515019,222.565144850884,222.647466824175,222.731452841327,222.815438858478,
222.891078967699,222.966695070606,223.04230163766,223.117936300369,223.193585858948,
223.269296148725,223.313907401786,223.405807971491,223.497840941208,223.589720511032,
223.681347907064,223.772369028547,223.812375945094,223.886377859781,223.960358788123,
224.034333810035,224.108346283333,224.182377553314,224.256482305518,224.310844488401,
224.389805904348,224.468713327418,224.547578366354,224.62641259708,224.705227571059,
224.78404883472,224.862875473832,224.941717998208,225.020586926792,225.099528978123,
225.178509743612,225.25758075463,225.307781575016,225.386773470355,225.46566525503,
225.544467511075,225.623167511897,225.701806957777,225.780383239963,225.806250118324,
225.884836841487,225.963473008749,226.042169002064,226.120983033547,226.199864461769,
226.278867554984,226.304718661631,226.383791183381,226.462790738116,226.54172900594,
226.620617620421,226.699468176978,226.778296681244,226.857113055113,226.935927806296,
227.014751440274,227.093621487822,227.172515166897,227.251475691734,227.301655748246,
227.384641264441,227.467394863404,227.503780749601),.UNSPECIFIED.);
#3036=B_SPLINE_CURVE_WITH_KNOTS('',3,(#143719,#143720,#143721,#143722,#143723,
#143724,#143725,#143726,#143727,#143728,#143729,#143730,#143731,#143732,
#143733,#143734,#143735,#143736,#143737),.UNSPECIFIED.,.F.,.F.,(4,3,3,3,
3,3,4),(227.503780749711,227.577866635172,227.648878133573,227.719884644627,
227.790914707643,227.800124291554,227.859336579383),.UNSPECIFIED.);
#3037=B_SPLINE_CURVE_WITH_KNOTS('',3,(#143739,#143740,#143741,#143742,#143743,
#143744,#143745,#143746,#143747,#143748,#143749,#143750,#143751,#143752,
#143753,#143754),.UNSPECIFIED.,.F.,.F.,(4,3,3,3,3,4),(-224.120755851454,
-224.039026307618,-223.957291192699,-223.87556095535,-223.793829166399,
-223.764541205496),.UNSPECIFIED.);
#3038=B_SPLINE_CURVE_WITH_KNOTS('',3,(#143755,#143756,#143757,#143758,#143759,
#143760,#143761,#143762,#143763,#143764,#143765,#143766,#143767,#143768,
#143769,#143770,#143771,#143772,#143773,#143774,#143775,#143776,#143777,
#143778,#143779,#143780,#143781,#143782,#143783,#143784,#143785,#143786,
#143787,#143788,#143789,#143790,#143791,#143792,#143793,#143794,#143795,
#143796,#143797,#143798,#143799,#143800,#143801,#143802,#143803,#143804,
#143805,#143806,#143807,#143808,#143809,#143810,#143811,#143812,#143813,
#143814,#143815,#143816,#143817,#143818,#143819,#143820,#143821,#143822,
#143823,#143824,#143825,#143826,#143827,#143828,#143829,#143830,#143831,
#143832,#143833,#143834,#143835,#143836,#143837,#143838,#143839,#143840,
#143841,#143842,#143843,#143844,#143845,#143846,#143847,#143848,#143849,
#143850,#143851,#143852,#143853,#143854,#143855,#143856,#143857,#143858,
#143859,#143860,#143861,#143862,#143863,#143864,#143865,#143866,#143867,
#143868,#143869,#143870,#143871,#143872,#143873,#143874,#143875,#143876,
#143877,#143878,#143879,#143880,#143881,#143882,#143883,#143884,#143885,
#143886,#143887,#143888,#143889,#143890,#143891,#143892,#143893,#143894,
#143895,#143896,#143897,#143898,#143899,#143900,#143901,#143902,#143903,
#143904,#143905,#143906,#143907,#143908,#143909,#143910,#143911,#143912,
#143913,#143914,#143915,#143916,#143917,#143918,#143919,#143920,#143921,
#143922,#143923,#143924,#143925,#143926,#143927,#143928,#143929,#143930,
#143931,#143932,#143933,#143934,#143935,#143936,#143937,#143938,#143939,
#143940,#143941,#143942,#143943,#143944,#143945,#143946,#143947,#143948,
#143949,#143950,#143951,#143952,#143953,#143954,#143955,#143956,#143957,
#143958,#143959,#143960,#143961,#143962,#143963,#143964,#143965,#143966,
#143967,#143968,#143969,#143970,#143971,#143972,#143973,#143974,#143975,
#143976,#143977,#143978,#143979,#143980,#143981,#143982,#143983,#143984,
#143985,#143986,#143987,#143988,#143989),.UNSPECIFIED.,.F.,.F.,(4,3,3,3,
3,3,3,3,3,3,3,3,3,3,3,3,3,3,3,3,3,3,3,3,3,3,3,3,3,3,3,3,3,3,3,3,3,3,3,3,
3,3,3,3,3,3,3,3,3,3,3,3,3,3,3,3,3,3,3,3,3,3,3,3,3,3,3,3,3,3,3,3,3,3,3,3,
3,3,4),(-223.764541205496,-223.672803714405,-223.580435572842,-223.487896573484,
-223.395424020174,-223.313907401786,-223.238197730668,-223.162536728641,
-223.086909888302,-223.011292192019,-222.935680691932,-222.860040767303,
-222.815438858478,-222.733160086626,-222.650857523765,-222.567385721616,
-222.48503076672,-222.401000540945,-222.316970315171,-222.234591304568,
-222.152227115317,-222.068795779453,-221.986473806159,-221.902487789011,
-221.818501771863,-221.742861662642,-221.667245559737,-221.591638992684,
-221.516004329975,-221.440354771398,-221.364644481622,-221.320033228556,
-221.228132658852,-221.136099689136,-221.044220119313,-220.952592723282,
-220.861571601799,-220.821564685248,-220.74756277056,-220.673581842218,
-220.599606820306,-220.525594347006,-220.451563077025,-220.377458324821,
-220.323096141941,-220.244134725994,-220.165227302924,-220.086362263987,
-220.007528033261,-219.928713059282,-219.849891795622,-219.771065156509,
-219.692222632132,-219.613353703549,-219.534411652218,-219.455430886729,
-219.37635987571,-219.326159055325,-219.247167159987,-219.168275375312,
-219.089473119268,-219.010773118447,-218.932133672568,-218.853557390383,
-218.827690512018,-218.749103788854,-218.670467621591,-218.591771628275,
-218.512957596792,-218.434076168568,-218.355073075352,-218.32922196871,
-218.251485982939,-218.173821811482,-218.096216627412,-218.018663395878,
-217.941140397265,-217.863632607374,-217.837561537579),.UNSPECIFIED.);
#3039=B_SPLINE_CURVE_WITH_KNOTS('',3,(#143995,#143996,#143997,#143998,#143999,
#144000,#144001,#144002,#144003,#144004,#144005,#144006,#144007,#144008,
#144009,#144010,#144011,#144012,#144013,#144014,#144015,#144016,#144017,
#144018,#144019,#144020,#144021,#144022,#144023,#144024,#144025,#144026,
#144027,#144028,#144029,#144030,#144031,#144032,#144033,#144034,#144035,
#144036,#144037,#144038,#144039,#144040,#144041,#144042,#144043,#144044,
#144045,#144046,#144047,#144048,#144049,#144050,#144051,#144052,#144053,
#144054,#144055,#144056,#144057,#144058,#144059,#144060,#144061,#144062,
#144063,#144064,#144065,#144066,#144067,#144068,#144069,#144070,#144071,
#144072,#144073,#144074,#144075,#144076,#144077,#144078,#144079,#144080,
#144081,#144082,#144083,#144084,#144085,#144086,#144087,#144088,#144089,
#144090,#144091,#144092,#144093,#144094,#144095,#144096,#144097,#144098,
#144099,#144100,#144101,#144102,#144103,#144104,#144105,#144106,#144107,
#144108,#144109,#144110,#144111,#144112,#144113,#144114,#144115,#144116,
#144117,#144118,#144119,#144120,#144121,#144122,#144123,#144124,#144125,
#144126,#144127,#144128,#144129,#144130,#144131,#144132,#144133,#144134,
#144135,#144136,#144137,#144138,#144139,#144140,#144141,#144142,#144143,
#144144,#144145,#144146,#144147,#144148,#144149,#144150,#144151,#144152,
#144153,#144154,#144155,#144156,#144157,#144158,#144159,#144160,#144161,
#144162,#144163,#144164,#144165,#144166,#144167,#144168,#144169,#144170,
#144171,#144172,#144173,#144174,#144175,#144176,#144177,#144178,#144179,
#144180,#144181,#144182,#144183,#144184,#144185,#144186,#144187,#144188,
#144189,#144190,#144191,#144192,#144193,#144194,#144195,#144196,#144197,
#144198,#144199,#144200,#144201,#144202,#144203,#144204,#144205,#144206,
#144207,#144208,#144209,#144210,#144211,#144212,#144213,#144214,#144215,
#144216,#144217,#144218,#144219,#144220,#144221,#144222,#144223,#144224,
#144225,#144226,#144227,#144228,#144229,#144230,#144231,#144232),
 .UNSPECIFIED.,.F.,.F.,(4,3,3,3,3,3,3,3,3,3,3,3,3,3,3,3,3,3,3,3,3,3,3,3,
3,3,3,3,3,3,3,3,3,3,3,3,3,3,3,3,3,3,3,3,3,3,3,3,3,3,3,3,3,3,3,3,3,3,3,3,
3,3,3,3,3,3,3,3,3,3,3,3,3,3,3,3,3,3,3,4),(215.293584957643,215.338410708865,
215.420789719468,215.503153908718,215.586585244582,215.668907217876,215.752893235024,
215.836879252173,215.912519361393,215.988135464298,216.063742031351,216.13937669406,
216.215026252636,216.290736542412,216.33534779548,216.427248365185,216.519281334901,
216.611160904726,216.702788300757,216.793809422241,216.833816338788,216.907818253476,
216.981799181818,217.05577420373,217.12978667703,217.20381794701,217.277922699215,
217.332284882095,217.411246298042,217.490153721111,217.569018760048,217.647852990774,
217.726667964752,217.805489228412,217.884315867525,217.963158391901,218.042027320484,
218.120969371815,218.199950137304,218.279021148322,218.32922196871,218.408213864049,
218.487105648724,218.565907904768,218.64460790559,218.723247351469,218.801823633655,
218.827690512018,218.906277235182,218.984913402445,219.063609395762,219.142423427246,
219.22130485547,219.300307948686,219.326159055326,219.405231577075,219.48423113181,
219.563169399634,219.642058014116,219.720908570672,219.799737074937,219.878553448806,
219.95736819999,220.036191833967,220.115061881515,220.193955560591,220.272916085428,
220.323096141941,220.397201580042,220.471250077897,220.545256815903,220.619246080055,
220.693223441667,220.767225727699,220.821564685248,220.910526452492,221.000020868658,
221.08972837351,221.179600242886,221.220595442298),.UNSPECIFIED.);
#3040=B_SPLINE_CURVE_WITH_KNOTS('',3,(#144233,#144234,#144235,#144236,#144237,
#144238,#144239,#144240,#144241,#144242,#144243,#144244,#144245,#144246,
#144247,#144248),.UNSPECIFIED.,.F.,.F.,(4,3,3,3,3,4),(221.220595442422,
221.320033228556,221.395742383023,221.47140477704,221.547032011141,221.577058603984),
 .UNSPECIFIED.);
#3041=B_SPLINE_CURVE_WITH_KNOTS('',3,(#144250,#144251,#144252,#144253,#144254,
#144255,#144256,#144257,#144258,#144259,#144260,#144261,#144262,#144263,
#144264,#144265),.UNSPECIFIED.,.F.,.F.,(4,3,3,3,3,4),(-217.837561537579,
-217.760053293282,-217.682505293837,-217.604936121589,-217.527300607496,
-217.481355898413),.UNSPECIFIED.);
#3042=B_SPLINE_CURVE_WITH_KNOTS('',3,(#144266,#144267,#144268,#144269,#144270,
#144271,#144272,#144273,#144274,#144275,#144276,#144277,#144278,#144279,
#144280,#144281,#144282,#144283,#144284,#144285,#144286,#144287,#144288,
#144289,#144290,#144291,#144292,#144293,#144294,#144295,#144296,#144297,
#144298,#144299,#144300,#144301,#144302,#144303,#144304,#144305,#144306,
#144307,#144308,#144309,#144310,#144311,#144312,#144313,#144314,#144315,
#144316,#144317,#144318,#144319,#144320,#144321,#144322,#144323,#144324,
#144325,#144326,#144327,#144328,#144329,#144330,#144331,#144332,#144333,
#144334,#144335,#144336,#144337,#144338,#144339,#144340,#144341,#144342,
#144343,#144344,#144345,#144346,#144347,#144348,#144349,#144350,#144351,
#144352,#144353,#144354,#144355,#144356,#144357,#144358,#144359,#144360,
#144361,#144362,#144363,#144364,#144365,#144366,#144367,#144368,#144369,
#144370,#144371,#144372,#144373,#144374,#144375,#144376,#144377,#144378,
#144379,#144380,#144381,#144382,#144383,#144384,#144385,#144386,#144387,
#144388,#144389,#144390,#144391,#144392,#144393,#144394,#144395,#144396,
#144397,#144398,#144399,#144400,#144401,#144402,#144403,#144404,#144405,
#144406,#144407,#144408,#144409,#144410,#144411,#144412,#144413,#144414,
#144415,#144416,#144417,#144418,#144419,#144420,#144421,#144422,#144423,
#144424,#144425,#144426,#144427,#144428,#144429,#144430,#144431,#144432,
#144433,#144434,#144435,#144436,#144437,#144438,#144439,#144440,#144441,
#144442,#144443,#144444,#144445,#144446,#144447,#144448,#144449,#144450,
#144451,#144452,#144453,#144454,#144455,#144456,#144457,#144458,#144459,
#144460,#144461,#144462,#144463,#144464,#144465,#144466,#144467,#144468,
#144469,#144470,#144471,#144472,#144473,#144474,#144475,#144476,#144477,
#144478,#144479,#144480,#144481,#144482,#144483,#144484,#144485,#144486,
#144487,#144488,#144489,#144490,#144491,#144492,#144493,#144494,#144495,
#144496,#144497),.UNSPECIFIED.,.F.,.F.,(4,3,3,3,3,3,3,3,3,3,3,3,3,3,3,3,
3,3,3,3,3,3,3,3,3,3,3,3,3,3,3,3,3,3,3,3,3,3,3,3,3,3,3,3,3,3,3,3,3,3,3,3,
3,3,3,3,3,3,3,3,3,3,3,3,3,3,3,3,3,3,3,3,3,3,3,3,3,4),(-217.481355898316,
-217.332284882095,-217.258179443994,-217.18413094614,-217.110124208134,
-217.036134943982,-216.96215758237,-216.888155296338,-216.833816338788,
-216.74281723905,-216.651314021371,-216.559370482438,-216.467335905257,
-216.375426815133,-216.33534779548,-216.259638124363,-216.183977122338,
-216.108350282001,-216.03273258572,-215.957121085634,-215.881481161007,
-215.836879252173,-215.754600480319,-215.672297917456,-215.588826115309,
-215.50647116041,-215.422440934638,-215.338410708865,-215.256031698262,
-215.173667509011,-215.090236173147,-215.007914199853,-214.923928182705,
-214.839942165557,-214.764302056337,-214.688685953432,-214.613079386379,
-214.537444723671,-214.461795165095,-214.386084875319,-214.34147362225,
-214.249573052545,-214.157540082829,-214.065660513004,-213.974033116973,
-213.88301199549,-213.843005078942,-213.769003164254,-213.695022235912,
-213.621047214,-213.5470347407,-213.473003470719,-213.398898718515,-213.344536535635,
-213.265575119688,-213.186667696619,-213.107802657682,-213.028968426957,
-212.950153452978,-212.871332189318,-212.792505550206,-212.713663025829,
-212.634794097247,-212.555852045915,-212.476871280426,-212.397800269408,
-212.34759944902,-212.268607553681,-212.189715769005,-212.11091351296,-212.032213512137,
-211.953574066258,-211.874997784072,-211.849130905712,-211.770531646682,
-211.69189389683,-211.613163329234,-211.555186956847),.UNSPECIFIED.);
#3043=B_SPLINE_CURVE_WITH_KNOTS('',3,(#144503,#144504,#144505,#144506,#144507,
#144508,#144509,#144510,#144511,#144512,#144513,#144514,#144515,#144516,
#144517,#144518,#144519,#144520,#144521,#144522,#144523,#144524,#144525,
#144526,#144527,#144528,#144529,#144530,#144531,#144532,#144533,#144534,
#144535,#144536,#144537,#144538,#144539,#144540,#144541,#144542,#144543,
#144544,#144545,#144546,#144547,#144548,#144549,#144550,#144551,#144552,
#144553,#144554,#144555,#144556,#144557,#144558,#144559,#144560,#144561,
#144562,#144563,#144564,#144565,#144566,#144567,#144568,#144569,#144570,
#144571,#144572,#144573,#144574,#144575,#144576,#144577,#144578,#144579,
#144580,#144581,#144582,#144583,#144584,#144585,#144586,#144587,#144588,
#144589,#144590,#144591,#144592,#144593,#144594,#144595,#144596,#144597,
#144598,#144599,#144600,#144601,#144602,#144603,#144604,#144605,#144606,
#144607,#144608,#144609,#144610,#144611,#144612,#144613,#144614,#144615,
#144616,#144617,#144618,#144619,#144620,#144621,#144622,#144623,#144624,
#144625,#144626,#144627,#144628,#144629,#144630,#144631,#144632,#144633,
#144634,#144635,#144636,#144637,#144638,#144639,#144640,#144641,#144642,
#144643,#144644,#144645,#144646,#144647,#144648,#144649,#144650,#144651,
#144652,#144653,#144654,#144655,#144656,#144657,#144658,#144659,#144660,
#144661,#144662,#144663,#144664,#144665,#144666,#144667,#144668,#144669,
#144670,#144671,#144672,#144673,#144674,#144675,#144676,#144677,#144678,
#144679,#144680,#144681,#144682,#144683,#144684,#144685,#144686,#144687,
#144688,#144689,#144690,#144691,#144692,#144693,#144694,#144695,#144696,
#144697,#144698,#144699,#144700,#144701,#144702,#144703,#144704,#144705,
#144706,#144707,#144708,#144709,#144710,#144711,#144712,#144713,#144714,
#144715,#144716,#144717,#144718,#144719,#144720,#144721,#144722,#144723,
#144724,#144725,#144726,#144727,#144728,#144729,#144730,#144731,#144732,
#144733,#144734,#144735,#144736,#144737,#144738,#144739,#144740,#144741,
#144742,#144743),.UNSPECIFIED.,.F.,.F.,(4,3,3,3,3,3,3,3,3,3,3,3,3,3,3,3,
3,3,3,3,3,3,3,3,3,3,3,3,3,3,3,3,3,3,3,3,3,3,3,3,3,3,3,3,3,3,3,3,3,3,3,3,
3,3,3,3,3,3,3,3,3,3,3,3,3,3,3,3,3,3,3,3,3,3,3,3,3,3,3,3,4),(209.010381503964,
209.085988047285,209.161622800332,209.237272587392,209.312982998961,209.356788189174,
209.448688758878,209.540721728594,209.632601298418,209.724228694449,209.815249815932,
209.855256732482,209.92925864717,210.003239575514,210.077214597427,210.151227070727,
210.225258340709,210.299363092915,210.35372527579,210.432686691737,210.511594114806,
210.590459153743,210.669293384468,210.748108358447,210.826929622107,210.905756261219,
210.984598785595,211.063467714177,211.142409765509,211.221390530997,211.300461542015,
211.350662362405,211.429654257743,211.508546042417,211.587348298461,211.666048299282,
211.74468774516,211.823264027345,211.849130905712,211.927717628876,212.00635379614,
212.085049789458,212.163863820941,212.242745249165,212.321748342382,212.34759944902,
212.42667197077,212.505671525505,212.584609793329,212.66349840781,212.742348964366,
212.821177468632,212.8999938425,212.978808593684,213.057632227662,213.13650227521,
213.215395954286,213.294356479123,213.344536535635,213.418641973736,213.49269047159,
213.566697209596,213.640686473748,213.71466383536,213.788666121392,213.843005078942,
213.93400417868,214.025507396355,214.117450935285,214.209485512466,214.301394602588,
214.34147362225,214.417183293369,214.492844295396,214.568471135735,214.644088832019,
214.719700332106,214.795340256735,214.839942165558,214.930975113248,214.937410135242),
 .UNSPECIFIED.);
#3044=B_SPLINE_CURVE_WITH_KNOTS('',3,(#144744,#144745,#144746,#144747,#144748,
#144749,#144750,#144751,#144752,#144753,#144754,#144755,#144756,#144757,
#144758,#144759),.UNSPECIFIED.,.F.,.F.,(4,3,3,3,3,4),(214.937410135318,
215.018871014483,215.100353018709,215.181840116616,215.263345603113,215.293584957643),
 .UNSPECIFIED.);
#3045=B_SPLINE_CURVE_WITH_KNOTS('',3,(#144761,#144762,#144763,#144764,#144765,
#144766,#144767,#144768,#144769,#144770,#144771,#144772,#144773,#144774,
#144775,#144776),.UNSPECIFIED.,.F.,.F.,(4,3,3,3,3,4),(-211.555186956847,
-211.476324236877,-211.39733291139,-211.350662362405,-211.217629850047,
-211.198170591137),.UNSPECIFIED.);
#3046=B_SPLINE_CURVE_WITH_KNOTS('',3,(#144777,#144778,#144779,#144780,#144781,
#144782,#144783,#144784,#144785,#144786,#144787,#144788,#144789,#144790,
#144791,#144792,#144793,#144794,#144795,#144796,#144797,#144798,#144799,
#144800,#144801,#144802,#144803,#144804,#144805,#144806,#144807,#144808,
#144809,#144810,#144811,#144812,#144813,#144814,#144815,#144816,#144817,
#144818,#144819,#144820,#144821,#144822,#144823,#144824,#144825,#144826,
#144827,#144828,#144829,#144830,#144831,#144832,#144833,#144834,#144835,
#144836,#144837,#144838,#144839,#144840,#144841,#144842,#144843,#144844,
#144845,#144846,#144847,#144848,#144849,#144850,#144851,#144852,#144853,
#144854,#144855,#144856,#144857,#144858,#144859,#144860,#144861,#144862,
#144863,#144864,#144865,#144866,#144867,#144868,#144869,#144870,#144871,
#144872,#144873,#144874,#144875,#144876,#144877,#144878,#144879,#144880,
#144881,#144882,#144883,#144884,#144885,#144886,#144887,#144888,#144889,
#144890,#144891,#144892,#144893,#144894,#144895,#144896,#144897,#144898,
#144899,#144900,#144901,#144902,#144903,#144904,#144905,#144906,#144907,
#144908,#144909,#144910,#144911,#144912,#144913,#144914,#144915,#144916,
#144917,#144918,#144919,#144920,#144921,#144922,#144923,#144924,#144925,
#144926,#144927,#144928,#144929,#144930,#144931,#144932,#144933,#144934,
#144935,#144936,#144937,#144938,#144939,#144940,#144941,#144942,#144943,
#144944,#144945,#144946,#144947,#144948,#144949,#144950,#144951,#144952,
#144953,#144954,#144955,#144956,#144957,#144958,#144959,#144960,#144961,
#144962,#144963,#144964,#144965,#144966,#144967,#144968,#144969,#144970,
#144971,#144972,#144973,#144974,#144975,#144976,#144977,#144978,#144979,
#144980,#144981,#144982,#144983,#144984,#144985,#144986,#144987,#144988,
#144989,#144990,#144991,#144992,#144993,#144994,#144995,#144996,#144997,
#144998,#144999,#145000,#145001,#145002,#145003,#145004,#145005,#145006,
#145007,#145008,#145009,#145010,#145011),.UNSPECIFIED.,.F.,.F.,(4,3,3,3,
3,3,3,3,3,3,3,3,3,3,3,3,3,3,3,3,3,3,3,3,3,3,3,3,3,3,3,3,3,3,3,3,3,3,3,3,
3,3,3,3,3,3,3,3,3,3,3,3,3,3,3,3,3,3,3,3,3,3,3,3,3,3,3,3,3,3,3,3,3,3,3,3,
3,3,4),(-211.198170591051,-211.120197743593,-211.042291363753,-210.96443779742,
-210.886623209151,-210.8088299744,-210.731045779471,-210.653258318129,-210.575426098554,
-210.497571869303,-210.419643103381,-210.353725275789,-210.279619837687,
-210.205571339833,-210.131564601827,-210.057575337674,-209.983597976063,
-209.90959569003,-209.855256732482,-209.764257632745,-209.672754415067,
-209.580810876135,-209.488776298956,-209.396867208834,-209.356788189174,
-209.281078518057,-209.205417516032,-209.129790675694,-209.054172979413,
-208.978561479327,-208.9029215547,-208.858319645867,-208.776040874013,-208.693738311149,
-208.610266509002,-208.527911554103,-208.443881328331,-208.359851102559,
-208.277472091958,-208.195107902709,-208.111676566845,-208.029354593553,
-207.945368576402,-207.861382559252,-207.78574245003,-207.710126347124,
-207.63451978007,-207.55888511736,-207.483235558781,-207.407525269004,-207.362914015944,
-207.271013446243,-207.17898047653,-207.087100906709,-206.995473510682,
-206.904452389201,-206.864445472637,-206.790443557949,-206.716462629605,
-206.642487607692,-206.568475134392,-206.49444386441,-206.420339112205,
-206.365976929329,-206.287015513382,-206.208108090313,-206.129243051376,
-206.05040882065,-205.971593846672,-205.892772583012,-205.813945943899,
-205.735103419523,-205.65623449094,-205.577292439608,-205.49831167412,-205.419240663102,
-205.369039842714,-205.289130625658,-205.27050831412),.UNSPECIFIED.);
#3047=B_SPLINE_CURVE_WITH_KNOTS('',3,(#145017,#145018,#145019,#145020,#145021,
#145022,#145023,#145024,#145025,#145026,#145027,#145028,#145029,#145030,
#145031,#145032,#145033,#145034,#145035,#145036,#145037,#145038,#145039,
#145040,#145041,#145042,#145043,#145044,#145045,#145046,#145047,#145048,
#145049,#145050,#145051,#145052,#145053,#145054,#145055,#145056,#145057,
#145058,#145059,#145060,#145061,#145062,#145063,#145064,#145065,#145066,
#145067,#145068,#145069,#145070,#145071,#145072,#145073,#145074,#145075,
#145076,#145077,#145078,#145079,#145080,#145081,#145082,#145083,#145084,
#145085,#145086,#145087,#145088,#145089,#145090,#145091,#145092,#145093,
#145094,#145095,#145096,#145097,#145098,#145099,#145100,#145101,#145102,
#145103,#145104,#145105,#145106,#145107,#145108,#145109,#145110,#145111,
#145112,#145113,#145114,#145115,#145116,#145117,#145118,#145119,#145120,
#145121,#145122,#145123,#145124,#145125,#145126,#145127,#145128,#145129,
#145130,#145131,#145132,#145133,#145134,#145135,#145136,#145137,#145138,
#145139,#145140,#145141,#145142,#145143,#145144,#145145,#145146,#145147,
#145148,#145149,#145150,#145151,#145152,#145153,#145154,#145155,#145156,
#145157,#145158,#145159,#145160,#145161,#145162,#145163,#145164,#145165,
#145166,#145167,#145168,#145169,#145170,#145171,#145172,#145173,#145174,
#145175,#145176,#145177,#145178,#145179,#145180,#145181,#145182,#145183,
#145184,#145185,#145186,#145187,#145188,#145189,#145190,#145191,#145192,
#145193,#145194,#145195,#145196,#145197,#145198,#145199,#145200,#145201,
#145202,#145203,#145204,#145205,#145206,#145207,#145208,#145209,#145210,
#145211,#145212,#145213,#145214,#145215,#145216,#145217,#145218,#145219,
#145220,#145221,#145222,#145223,#145224,#145225,#145226,#145227,#145228,
#145229,#145230,#145231,#145232,#145233,#145234,#145235,#145236,#145237,
#145238,#145239,#145240,#145241,#145242,#145243,#145244,#145245,#145246,
#145247,#145248,#145249,#145250,#145251,#145252,#145253,#145254),
 .UNSPECIFIED.,.F.,.F.,(4,3,3,3,3,3,3,3,3,3,3,3,3,3,3,3,3,3,3,3,3,3,3,3,
3,3,3,3,3,3,3,3,3,3,3,3,3,3,3,3,3,3,3,3,3,3,3,3,3,3,3,3,3,3,3,3,3,3,3,3,
3,3,3,3,3,3,3,3,3,3,3,3,3,3,3,3,3,3,3,4),(202.727851097702,202.818931905915,
202.876697126176,202.950699040865,203.024679969209,203.098654991122,203.172667464423,
203.246698734404,203.32080348661,203.375165669484,203.454127085431,203.5330345085,
203.611899547437,203.690733778163,203.769548752142,203.848370015802,203.927196654914,
204.00603917929,204.084908107873,204.163850159204,204.242830924693,204.321901935711,
204.372102756099,204.451094651437,204.529986436111,204.608788692154,204.687488692975,
204.766128138853,204.844704421037,204.870571299406,204.94915802257,205.027794189834,
205.106490183151,205.185304214635,205.264185642859,205.343188736076,205.369039842714,
205.448112364463,205.527111919198,205.606050187022,205.684938801503,205.76378935806,
205.842617862325,205.921434236194,206.000248987378,206.079072621355,206.157942668903,
206.236836347979,206.315796872816,206.365976929329,206.440082367431,206.514130865286,
206.588137603294,206.662126867447,206.736104229059,206.810106515092,206.864445472637,
206.955444572371,207.046947790046,207.138891328975,207.230925906152,207.322834996271,
207.362914015944,207.438623687062,207.514284689089,207.589911529427,207.66552922571,
207.741140725798,207.816780650426,207.861382559252,207.943661331104,208.025963893966,
208.109435696114,208.191790651011,208.275820876785,208.359851102559,208.441480017848,
208.523091015779,208.604687165193,208.654224828063),.UNSPECIFIED.);
#3048=B_SPLINE_CURVE_WITH_KNOTS('',3,(#145255,#145256,#145257,#145258,#145259,
#145260,#145261,#145262,#145263,#145264,#145265,#145266,#145267,#145268,
#145269,#145270),.UNSPECIFIED.,.F.,.F.,(4,3,3,3,3,4),(208.654224828187,
208.740497929717,208.826719004093,208.858319645867,208.934350574915,209.010381503964),
 .UNSPECIFIED.);
#3049=B_SPLINE_CURVE_WITH_KNOTS('',3,(#145272,#145273,#145274,#145275,#145276,
#145277,#145278,#145279,#145280,#145281,#145282,#145283,#145284,#145285,
#145286,#145287),.UNSPECIFIED.,.F.,.F.,(4,3,3,3,3,4),(-205.27050831412,
-205.190744529819,-205.11111727546,-205.031571299999,-204.952123552818,
-204.914985284074),.UNSPECIFIED.);
#3050=B_SPLINE_CURVE_WITH_KNOTS('',3,(#145288,#145289,#145290,#145291,#145292,
#145293,#145294,#145295,#145296,#145297,#145298,#145299,#145300,#145301,
#145302,#145303,#145304,#145305,#145306,#145307,#145308,#145309,#145310,
#145311,#145312,#145313,#145314,#145315,#145316,#145317,#145318,#145319,
#145320,#145321,#145322,#145323,#145324,#145325,#145326,#145327,#145328,
#145329,#145330,#145331,#145332,#145333,#145334,#145335,#145336,#145337,
#145338,#145339,#145340,#145341,#145342,#145343,#145344,#145345,#145346,
#145347,#145348,#145349,#145350,#145351,#145352,#145353,#145354,#145355,
#145356,#145357,#145358,#145359,#145360,#145361,#145362,#145363,#145364,
#145365,#145366,#145367,#145368,#145369,#145370,#145371,#145372,#145373,
#145374,#145375,#145376,#145377,#145378,#145379,#145380,#145381,#145382,
#145383,#145384,#145385,#145386,#145387,#145388,#145389,#145390,#145391,
#145392,#145393,#145394,#145395,#145396,#145397,#145398,#145399,#145400,
#145401,#145402,#145403,#145404,#145405,#145406,#145407,#145408,#145409,
#145410,#145411,#145412,#145413,#145414,#145415,#145416,#145417,#145418,
#145419,#145420,#145421,#145422,#145423,#145424,#145425,#145426,#145427,
#145428,#145429,#145430,#145431,#145432,#145433,#145434,#145435,#145436,
#145437,#145438,#145439,#145440,#145441,#145442,#145443,#145444,#145445,
#145446,#145447,#145448,#145449,#145450,#145451,#145452,#145453,#145454,
#145455,#145456,#145457,#145458,#145459,#145460,#145461,#145462,#145463,
#145464,#145465,#145466,#145467,#145468,#145469,#145470,#145471,#145472,
#145473,#145474,#145475,#145476,#145477,#145478,#145479,#145480,#145481,
#145482,#145483,#145484,#145485,#145486,#145487,#145488,#145489,#145490,
#145491,#145492,#145493,#145494,#145495,#145496,#145497,#145498,#145499,
#145500,#145501,#145502,#145503,#145504,#145505,#145506,#145507,#145508,
#145509,#145510,#145511,#145512,#145513,#145514,#145515,#145516,#145517,
#145518,#145519,#145520,#145521,#145522),.UNSPECIFIED.,.F.,.F.,(4,3,3,3,
3,3,3,3,3,3,3,3,3,3,3,3,3,3,3,3,3,3,3,3,3,3,3,3,3,3,3,3,3,3,3,3,3,3,3,3,
3,3,3,3,3,3,3,3,3,3,3,3,3,3,3,3,3,3,3,3,3,3,3,3,3,3,3,3,3,3,3,3,3,3,3,3,
3,3,4),(-204.914985283957,-204.870571299406,-204.791984576244,-204.713348408983,
-204.634652415668,-204.555838384187,-204.476956955965,-204.397953862751,
-204.372102756099,-204.293030234349,-204.214030679614,-204.13509241179,
-204.056203797308,-203.977353240752,-203.898524736486,-203.819708362616,
-203.740893611432,-203.662069977454,-203.583199929906,-203.50430625083,
-203.425345725992,-203.375165669484,-203.301060231382,-203.227011733527,
-203.153004995519,-203.079015731366,-203.005038369754,-202.93103608372,
-202.876697126176,-202.785698026443,-202.694194808769,-202.602251269841,
-202.510216692664,-202.418307602545,-202.378228582869,-202.302518911751,
-202.226857909725,-202.151231069388,-202.075613373105,-202.000001873018,
-201.92436194839,-201.879760039561,-201.797481267707,-201.715178704842,
-201.631706902695,-201.549351947796,-201.465321722024,-201.381291496253,
-201.298912485652,-201.216548296405,-201.13311696054,-201.050794987249,
-200.966808970097,-200.882822952946,-200.807182843724,-200.731566740817,
-200.655960173762,-200.580325511052,-200.504675952473,-200.428965662696,
-200.384354409638,-200.292453839936,-200.200420870225,-200.108541300405,
-200.016913904378,-199.925892782898,-199.885885866331,-199.811883951642,
-199.737903023298,-199.663928001386,-199.589915528085,-199.515884258103,
-199.441779505898,-199.387417323023,-199.309170163293,-199.22899001696,
-199.15085344188,-199.069651509919,-198.988449577959),.UNSPECIFIED.);
#3051=B_SPLINE_CURVE_WITH_KNOTS('',3,(#145528,#145529,#145530,#145531,#145532,
#145533,#145534,#145535,#145536,#145537,#145538,#145539,#145540,#145541,
#145542,#145543,#145544,#145545,#145546,#145547,#145548,#145549,#145550,
#145551,#145552,#145553,#145554,#145555,#145556,#145557,#145558,#145559,
#145560,#145561,#145562,#145563,#145564,#145565,#145566,#145567,#145568,
#145569,#145570,#145571,#145572,#145573,#145574,#145575,#145576,#145577,
#145578,#145579,#145580,#145581,#145582,#145583,#145584,#145585,#145586,
#145587,#145588,#145589,#145590,#145591,#145592,#145593,#145594,#145595,
#145596,#145597,#145598,#145599,#145600,#145601,#145602,#145603,#145604,
#145605,#145606,#145607,#145608,#145609,#145610,#145611,#145612,#145613,
#145614,#145615,#145616,#145617,#145618,#145619,#145620,#145621,#145622,
#145623,#145624,#145625,#145626,#145627,#145628,#145629,#145630,#145631,
#145632,#145633,#145634,#145635,#145636,#145637,#145638,#145639,#145640,
#145641,#145642,#145643,#145644,#145645,#145646,#145647,#145648,#145649,
#145650,#145651,#145652,#145653,#145654,#145655,#145656,#145657,#145658,
#145659,#145660,#145661,#145662,#145663,#145664,#145665,#145666,#145667,
#145668,#145669,#145670,#145671,#145672,#145673,#145674,#145675,#145676,
#145677,#145678,#145679,#145680,#145681,#145682,#145683,#145684,#145685,
#145686,#145687,#145688,#145689,#145690,#145691,#145692,#145693,#145694,
#145695,#145696,#145697,#145698,#145699,#145700,#145701,#145702,#145703,
#145704,#145705,#145706,#145707,#145708,#145709,#145710,#145711,#145712,
#145713,#145714,#145715,#145716,#145717,#145718,#145719,#145720,#145721,
#145722,#145723,#145724,#145725,#145726,#145727,#145728,#145729,#145730,
#145731,#145732,#145733,#145734,#145735,#145736,#145737,#145738,#145739,
#145740,#145741,#145742,#145743,#145744,#145745,#145746,#145747,#145748,
#145749,#145750,#145751,#145752,#145753,#145754,#145755,#145756,#145757,
#145758,#145759,#145760,#145761,#145762),.UNSPECIFIED.,.F.,.F.,(4,3,3,3,
3,3,3,3,3,3,3,3,3,3,3,3,3,3,3,3,3,3,3,3,3,3,3,3,3,3,3,3,3,3,3,3,3,3,3,3,
3,3,3,3,3,3,3,3,3,3,3,3,3,3,3,3,3,3,3,3,3,3,3,3,3,3,3,3,3,3,3,3,3,3,3,3,
3,3,4),(196.443737963822,196.522665757598,196.601546491101,196.680391752479,
196.759213102051,196.838504358019,196.917327604243,196.996162560754,197.07501974207,
197.154650594001,197.233615182068,197.313579165931,197.393543149793,197.472535045132,
197.551426829808,197.630229085853,197.708929086675,197.787568532554,197.86614481474,
197.892011693101,197.970598416264,198.049234583526,198.127930576842,198.206744608324,
198.285626036547,198.364629129762,198.390480236408,198.469552758158,198.548552312893,
198.627490580717,198.706379195198,198.785229751754,198.86405825602,198.942874629889,
199.021689381072,199.10051301505,199.179383062598,199.258276741674,199.337237266511,
199.387417323023,199.461522761125,199.535571258981,199.609577996988,199.683567261141,
199.757544622754,199.831546908788,199.885885866331,199.976884966065,200.06838818374,
200.160331722668,200.252366299845,200.344275389964,200.384354409638,200.460064080756,
200.535725082783,200.611351923121,200.686969619404,200.762581119492,200.83822104412,
200.882822952946,200.965101724798,201.04740428766,201.130876089808,201.213231044705,
201.297261270479,201.381291496253,201.463670506856,201.546034696106,201.62946603197,
201.711788005263,201.795774022412,201.879760039561,201.955357754018,202.030931327645,
202.106495255714,202.182086177459,202.257691990731,202.333355910857,202.371039520793),
 .UNSPECIFIED.);
#3052=B_SPLINE_CURVE_WITH_KNOTS('',3,(#145763,#145764,#145765,#145766,#145767,
#145768,#145769,#145770,#145771,#145772,#145773,#145774,#145775,#145776,
#145777,#145778),.UNSPECIFIED.,.F.,.F.,(4,3,3,3,3,4),(202.371039520883,
202.378228582869,202.470178269923,202.562210817129,202.654076209428,202.727851097702),
 .UNSPECIFIED.);
#3053=B_SPLINE_CURVE_WITH_KNOTS('',3,(#145780,#145781,#145782,#145783,#145784,
#145785,#145786,#145787,#145788,#145789,#145790,#145791,#145792,#145793,
#145794,#145795),.UNSPECIFIED.,.F.,.F.,(4,3,3,3,3,4),(-198.988449577959,
-198.910364452514,-198.832250522121,-198.754121808537,-198.675939145095,
-198.631799976778),.UNSPECIFIED.);
#3054=B_SPLINE_CURVE_WITH_KNOTS('',3,(#145796,#145797,#145798,#145799,#145800,
#145801,#145802,#145803,#145804,#145805,#145806,#145807,#145808,#145809,
#145810,#145811,#145812,#145813,#145814,#145815,#145816,#145817,#145818,
#145819,#145820,#145821,#145822,#145823,#145824,#145825,#145826,#145827,
#145828,#145829,#145830,#145831,#145832,#145833,#145834,#145835,#145836,
#145837,#145838,#145839,#145840,#145841,#145842,#145843,#145844,#145845,
#145846,#145847,#145848,#145849,#145850,#145851,#145852,#145853,#145854,
#145855,#145856,#145857,#145858,#145859,#145860,#145861,#145862,#145863,
#145864,#145865,#145866,#145867,#145868,#145869,#145870,#145871,#145872,
#145873,#145874,#145875,#145876,#145877,#145878,#145879,#145880,#145881,
#145882,#145883,#145884,#145885,#145886,#145887,#145888,#145889,#145890,
#145891,#145892,#145893,#145894,#145895,#145896,#145897,#145898,#145899,
#145900,#145901,#145902,#145903,#145904,#145905,#145906,#145907,#145908,
#145909,#145910,#145911,#145912,#145913,#145914,#145915,#145916,#145917,
#145918,#145919,#145920,#145921,#145922,#145923,#145924,#145925,#145926,
#145927,#145928,#145929,#145930,#145931,#145932,#145933,#145934,#145935,
#145936,#145937,#145938,#145939,#145940,#145941,#145942,#145943,#145944,
#145945,#145946,#145947,#145948,#145949,#145950,#145951,#145952,#145953,
#145954,#145955,#145956,#145957,#145958,#145959,#145960,#145961,#145962,
#145963,#145964,#145965,#145966,#145967,#145968,#145969,#145970,#145971,
#145972,#145973,#145974,#145975,#145976,#145977,#145978,#145979,#145980,
#145981,#145982,#145983,#145984,#145985,#145986,#145987,#145988,#145989,
#145990,#145991,#145992,#145993,#145994,#145995,#145996,#145997,#145998,
#145999,#146000,#146001,#146002,#146003,#146004,#146005,#146006,#146007,
#146008,#146009,#146010,#146011,#146012,#146013,#146014,#146015,#146016,
#146017,#146018,#146019,#146020,#146021,#146022,#146023,#146024,#146025,
#146026,#146027,#146028,#146029,#146030),.UNSPECIFIED.,.F.,.F.,(4,3,3,3,
3,3,3,3,3,3,3,3,3,3,3,3,3,3,3,3,3,3,3,3,3,3,3,3,3,3,3,3,3,3,3,3,3,3,3,3,
3,3,3,3,3,3,3,3,3,3,3,3,3,3,3,3,3,3,3,3,3,3,3,3,3,3,3,3,3,3,3,3,3,3,3,3,
3,3,4),(-198.631799976686,-198.530223734246,-198.42689683786,-198.390480236408,
-198.311488341069,-198.232596556394,-198.15379430035,-198.075094299528,
-197.996454853649,-197.917878571464,-197.8920116931,-197.813424969937,-197.734788802675,
-197.656092809359,-197.577278777877,-197.498397349654,-197.419394256439,
-197.393543149793,-197.314470628043,-197.235471073308,-197.156532805484,
-197.077644191003,-196.998793634447,-196.919965130181,-196.841148756312,
-196.762334005128,-196.683510371151,-196.604640323602,-196.525746644527,
-196.44678611969,-196.396606063178,-196.322500625076,-196.24845212722,-196.174445389213,
-196.10045612506,-196.026478763447,-195.952476477413,-195.89813751987,-195.807138420136,
-195.715635202461,-195.623691663533,-195.531657086357,-195.439747996238,
-195.399668976563,-195.323959305445,-195.248298303418,-195.17267146308,
-195.097053766797,-195.021442266709,-194.945802342081,-194.901200433255,
-194.818921661403,-194.736619098541,-194.653147296393,-194.570792341496,
-194.486762115722,-194.402731889948,-194.320352879346,-194.237988690096,
-194.154557354232,-194.072235380939,-193.988249363789,-193.90426334664,
-193.828623237418,-193.753007134511,-193.677400567456,-193.601765904746,
-193.526116346167,-193.450406056389,-193.405794803332,-193.313894233632,
-193.221861263921,-193.129981694102,-193.038354298076,-192.947333176598,
-192.907326260025,-192.833325706021,-192.759340356795,-192.704890585279),
 .UNSPECIFIED.);
#3055=B_SPLINE_CURVE_WITH_KNOTS('',3,(#146036,#146037,#146038,#146039,#146040,
#146041,#146042,#146043,#146044,#146045,#146046,#146047,#146048,#146049,
#146050,#146051,#146052,#146053,#146054,#146055,#146056,#146057,#146058,
#146059,#146060,#146061,#146062,#146063,#146064,#146065,#146066,#146067,
#146068,#146069,#146070,#146071,#146072,#146073,#146074,#146075,#146076,
#146077,#146078,#146079,#146080,#146081,#146082,#146083,#146084,#146085,
#146086,#146087,#146088,#146089,#146090,#146091,#146092,#146093,#146094,
#146095,#146096,#146097,#146098,#146099,#146100,#146101,#146102,#146103,
#146104,#146105,#146106,#146107,#146108,#146109,#146110,#146111,#146112,
#146113,#146114,#146115,#146116,#146117,#146118,#146119,#146120,#146121,
#146122,#146123,#146124,#146125,#146126,#146127,#146128,#146129,#146130,
#146131,#146132,#146133,#146134,#146135,#146136,#146137,#146138,#146139,
#146140,#146141,#146142,#146143,#146144,#146145,#146146,#146147,#146148,
#146149,#146150,#146151,#146152,#146153,#146154,#146155,#146156,#146157,
#146158,#146159,#146160,#146161,#146162,#146163,#146164,#146165,#146166,
#146167,#146168,#146169,#146170,#146171,#146172,#146173,#146174,#146175,
#146176,#146177,#146178,#146179,#146180,#146181,#146182,#146183,#146184,
#146185,#146186,#146187,#146188,#146189,#146190,#146191,#146192,#146193,
#146194,#146195,#146196,#146197,#146198,#146199,#146200,#146201,#146202,
#146203,#146204,#146205,#146206,#146207,#146208,#146209,#146210,#146211,
#146212,#146213,#146214,#146215,#146216,#146217,#146218,#146219,#146220,
#146221,#146222,#146223,#146224,#146225,#146226,#146227,#146228,#146229,
#146230,#146231,#146232,#146233,#146234,#146235,#146236,#146237,#146238,
#146239,#146240,#146241,#146242,#146243,#146244,#146245,#146246,#146247,
#146248,#146249,#146250,#146251,#146252,#146253,#146254,#146255,#146256,
#146257,#146258,#146259,#146260,#146261,#146262,#146263,#146264,#146265,
#146266,#146267,#146268,#146269,#146270,#146271,#146272,#146273),
 .UNSPECIFIED.,.F.,.F.,(4,3,3,3,3,3,3,3,3,3,3,3,3,3,3,3,3,3,3,3,3,3,3,3,
3,3,3,3,3,3,3,3,3,3,3,3,3,3,3,3,3,3,3,3,3,3,3,3,3,3,3,3,3,3,3,3,3,3,3,3,
3,3,3,3,3,3,3,3,3,3,3,3,3,3,3,3,3,3,3,4),(190.160514847461,190.239950536493,
190.319437569548,190.399017127351,190.414983543487,190.493975438826,190.572867223502,
190.651669479548,190.73036948037,190.809008926249,190.887585208435,190.913452086795,
190.992038809958,191.07067497722,191.149370970535,191.228185002017,191.30706643024,
191.386069523455,191.411920630102,191.490993151852,191.569992706587,191.648930974411,
191.727819588892,191.806670145448,191.885498649714,191.964315023583,192.043129774766,
192.121953408744,192.200823456292,192.279717135367,192.358677660204,192.408857716717,
192.482963154819,192.557011652674,192.631018390681,192.705007654834,192.778985016446,
192.85298730248,192.907326260025,192.998325359763,193.089828577442,193.181772116374,
193.273806693554,193.365715783677,193.405794803333,193.481504474449,193.557165476474,
193.63279231681,193.708410013091,193.784021513177,193.859661437804,193.90426334664,
193.986542118494,194.068844681359,194.152316483506,194.234671438406,194.318701664177,
194.402731889948,194.485110900549,194.567475089797,194.650906425662,194.733228398954,
194.817214416104,194.901200433255,194.976840542477,195.052456645383,195.128063212437,
195.203697875147,195.279347433726,195.355057723503,195.399668976563,195.491569546264,
195.583602515976,195.675482085796,195.767109481821,195.8581306033,195.89813751987,
195.968852952326,196.039554024148,196.087854213605),.UNSPECIFIED.);
#3056=B_SPLINE_CURVE_WITH_KNOTS('',3,(#146274,#146275,#146276,#146277,#146278,
#146279,#146280,#146281,#146282,#146283,#146284,#146285,#146286,#146287,
#146288,#146289),.UNSPECIFIED.,.F.,.F.,(4,3,3,3,3,4),(196.087854213704,
196.16581340922,196.243822506616,196.321954292725,196.396606063178,196.443737963822),
 .UNSPECIFIED.);
#3057=B_SPLINE_CURVE_WITH_KNOTS('',3,(#146291,#146292,#146293,#146294,#146295,
#146296,#146297,#146298,#146299,#146300,#146301,#146302,#146303,#146304,
#146305,#146306),.UNSPECIFIED.,.F.,.F.,(4,3,3,3,3,4),(-192.704890585279,
-192.630880807372,-192.556855814682,-192.482753841835,-192.408857716717,
-192.348614669598),.UNSPECIFIED.);
#3058=B_SPLINE_CURVE_WITH_KNOTS('',3,(#146307,#146308,#146309,#146310,#146311,
#146312,#146313,#146314,#146315,#146316,#146317,#146318,#146319,#146320,
#146321,#146322,#146323,#146324,#146325,#146326,#146327,#146328,#146329,
#146330,#146331,#146332,#146333,#146334,#146335,#146336,#146337,#146338,
#146339,#146340,#146341,#146342,#146343,#146344,#146345,#146346,#146347,
#146348,#146349,#146350,#146351,#146352,#146353,#146354,#146355,#146356,
#146357,#146358,#146359,#146360,#146361,#146362,#146363,#146364,#146365,
#146366,#146367,#146368,#146369,#146370,#146371,#146372,#146373,#146374,
#146375,#146376,#146377,#146378,#146379,#146380,#146381,#146382,#146383,
#146384,#146385,#146386,#146387,#146388,#146389,#146390,#146391,#146392,
#146393,#146394,#146395,#146396,#146397,#146398,#146399,#146400,#146401,
#146402,#146403,#146404,#146405,#146406,#146407,#146408,#146409,#146410,
#146411,#146412,#146413,#146414,#146415,#146416,#146417,#146418,#146419,
#146420,#146421,#146422,#146423,#146424,#146425,#146426,#146427,#146428,
#146429,#146430,#146431,#146432,#146433,#146434,#146435,#146436,#146437,
#146438,#146439,#146440,#146441,#146442,#146443,#146444,#146445,#146446,
#146447,#146448,#146449,#146450,#146451,#146452,#146453,#146454,#146455,
#146456,#146457,#146458,#146459,#146460,#146461,#146462,#146463,#146464,
#146465,#146466,#146467,#146468,#146469,#146470,#146471,#146472,#146473,
#146474,#146475,#146476,#146477,#146478,#146479,#146480,#146481,#146482,
#146483,#146484,#146485,#146486,#146487,#146488,#146489,#146490,#146491,
#146492,#146493,#146494,#146495,#146496,#146497,#146498,#146499,#146500,
#146501,#146502,#146503,#146504,#146505,#146506,#146507,#146508,#146509,
#146510,#146511,#146512,#146513,#146514,#146515,#146516,#146517,#146518,
#146519,#146520,#146521,#146522,#146523,#146524,#146525,#146526,#146527,
#146528,#146529,#146530,#146531,#146532,#146533,#146534,#146535,#146536,
#146537,#146538,#146539,#146540,#146541,#146542,#146543,#146544),
 .UNSPECIFIED.,.F.,.F.,(4,3,3,3,3,3,3,3,3,3,3,3,3,3,3,3,3,3,3,3,3,3,3,3,
3,3,3,3,3,3,3,3,3,3,3,3,3,3,3,3,3,3,3,3,3,3,3,3,3,3,3,3,3,3,3,3,3,3,3,3,
3,3,3,3,3,3,3,3,3,3,3,3,3,3,3,3,3,3,3,4),(-192.348614669501,-192.270390617134,
-192.192227777621,-192.11411295072,-192.036032971698,-191.957965294289,
-191.879903180881,-191.801834718374,-191.723747991729,-191.645592249413,
-191.567402408137,-191.489114269976,-191.411920630102,-191.332928734764,
-191.25403695009,-191.175234694046,-191.096534693225,-191.017895247347,
-190.939318965163,-190.913452086795,-190.834865363631,-190.756229196367,
-190.67753320305,-190.598719171567,-190.519837743343,-190.440834650126,
-190.414983543487,-190.335911021738,-190.256911467003,-190.177973199179,
-190.099084584697,-190.020234028141,-189.941405523876,-189.862589150007,
-189.783774398823,-189.704950764846,-189.626080717298,-189.547187038222,
-189.468226513385,-189.418046456872,-189.34394101877,-189.269892520915,
-189.195885782908,-189.121896518755,-189.047919157142,-188.973916871109,
-188.919577913564,-188.82857881383,-188.737075596154,-188.645132057226,
-188.553097480049,-188.461188389929,-188.421109370257,-188.345399699139,
-188.269738697112,-188.194111856774,-188.118494160491,-188.042882660403,
-187.967242735775,-187.922640826949,-187.840362055097,-187.758059492235,
-187.674587690087,-187.59223273519,-187.508202509416,-187.424172283642,
-187.341793273039,-187.259429083788,-187.175997747925,-187.093675774631,
-187.009689757482,-186.925703740334,-186.850063631113,-186.774447528207,
-186.698840961154,-186.623206298445,-186.547556739867,-186.471846450091,
-186.427235197027,-186.42200373843),.UNSPECIFIED.);
#3059=B_SPLINE_CURVE_WITH_KNOTS('',3,(#146550,#146551,#146552,#146553,#146554,
#146555,#146556,#146557,#146558,#146559,#146560,#146561,#146562,#146563,
#146564,#146565,#146566,#146567,#146568,#146569,#146570,#146571,#146572,
#146573,#146574,#146575,#146576,#146577,#146578,#146579,#146580,#146581,
#146582,#146583,#146584,#146585,#146586,#146587,#146588,#146589,#146590,
#146591,#146592,#146593,#146594,#146595,#146596,#146597,#146598,#146599,
#146600,#146601,#146602,#146603,#146604,#146605,#146606,#146607,#146608,
#146609,#146610,#146611,#146612,#146613,#146614,#146615,#146616,#146617,
#146618,#146619,#146620,#146621,#146622,#146623,#146624,#146625,#146626,
#146627,#146628,#146629,#146630,#146631,#146632,#146633,#146634,#146635,
#146636,#146637,#146638,#146639,#146640,#146641,#146642,#146643,#146644,
#146645,#146646,#146647,#146648,#146649,#146650,#146651,#146652,#146653,
#146654,#146655,#146656,#146657,#146658,#146659,#146660,#146661,#146662,
#146663,#146664,#146665,#146666,#146667,#146668,#146669,#146670,#146671,
#146672,#146673,#146674,#146675,#146676,#146677,#146678,#146679,#146680,
#146681,#146682,#146683,#146684,#146685,#146686,#146687,#146688,#146689,
#146690,#146691,#146692,#146693,#146694,#146695,#146696,#146697,#146698,
#146699,#146700,#146701,#146702,#146703,#146704,#146705,#146706,#146707,
#146708,#146709,#146710,#146711,#146712,#146713,#146714,#146715,#146716,
#146717,#146718,#146719,#146720,#146721,#146722,#146723,#146724,#146725,
#146726,#146727,#146728,#146729,#146730,#146731,#146732,#146733,#146734,
#146735,#146736,#146737,#146738,#146739,#146740,#146741,#146742,#146743,
#146744,#146745,#146746,#146747,#146748,#146749,#146750,#146751,#146752,
#146753,#146754,#146755,#146756,#146757,#146758,#146759,#146760,#146761,
#146762,#146763,#146764,#146765,#146766,#146767,#146768,#146769,#146770,
#146771,#146772,#146773,#146774,#146775,#146776,#146777,#146778,#146779,
#146780,#146781,#146782,#146783,#146784),.UNSPECIFIED.,.F.,.F.,(4,3,3,3,
3,3,3,3,3,3,3,3,3,3,3,3,3,3,3,3,3,3,3,3,3,3,3,3,3,3,3,3,3,3,3,3,3,3,3,3,
3,3,3,3,3,3,3,3,3,3,3,3,3,3,3,3,3,3,3,3,3,3,3,3,3,3,3,3,3,3,3,3,3,3,3,3,
3,3,4),(183.87796157873,183.934892480489,184.013479203651,184.092115370914,
184.170811364229,184.249625395711,184.328506823934,184.407509917149,184.433361023796,
184.512433545546,184.591433100282,184.670371368106,184.749259982587,184.828110539145,
184.906939043411,184.98575541728,185.064570168464,185.143393802442,185.222263849991,
185.301157529067,185.380118053904,185.430298110412,185.504403548514,185.578452046368,
185.652458784375,185.726448048528,185.80042541014,185.874427696173,185.928766653719,
186.019765753455,186.111268971133,186.203212510064,186.295247087243,186.387156177364,
186.427235197027,186.502944868144,186.578605870169,186.654232710506,186.729850406788,
186.805461906874,186.881101831501,186.925703740334,187.007982512188,187.090285075052,
187.173756877199,187.256111832098,187.34014205787,187.424172283642,187.506551294243,
187.588915483491,187.672346819356,187.754668792648,187.838654809798,187.922640826949,
187.99828093617,188.073897039077,188.14950360613,188.225138268839,188.300787827417,
188.376498117194,188.421109370257,188.513009939962,188.605042909677,188.696922479502,
188.788549875532,188.879570997015,188.919577913565,188.993579828252,189.067560756595,
189.141535778506,189.215548251805,189.289579521785,189.363684273989,189.418046456872,
189.508079469988,189.597935928296,189.687584901263,189.776793207838,189.804668906392),
 .UNSPECIFIED.);
#3060=B_SPLINE_CURVE_WITH_KNOTS('',3,(#146785,#146786,#146787,#146788,#146789,
#146790,#146791,#146792,#146793,#146794,#146795,#146796,#146797,#146798,
#146799,#146800),.UNSPECIFIED.,.F.,.F.,(4,3,3,3,3,4),(189.804668906524,
189.883885148564,189.963143028557,190.042422162795,190.121758264539,190.160514847461),
 .UNSPECIFIED.);
#3061=B_SPLINE_CURVE_WITH_KNOTS('',3,(#146802,#146803,#146804,#146805,#146806,
#146807,#146808,#146809,#146810,#146811,#146812,#146813,#146814),
 .UNSPECIFIED.,.F.,.F.,(4,3,3,3,4),(-186.42200373843,-186.32760531351,-186.233107414807,
-186.138937815505,-186.065429362419),.UNSPECIFIED.);
#3062=B_SPLINE_CURVE_WITH_KNOTS('',3,(#146815,#146816,#146817,#146818,#146819,
#146820,#146821,#146822,#146823,#146824,#146825,#146826,#146827,#146828,
#146829,#146830,#146831,#146832,#146833,#146834,#146835,#146836,#146837,
#146838,#146839,#146840,#146841,#146842,#146843,#146844,#146845,#146846,
#146847,#146848,#146849,#146850,#146851,#146852,#146853,#146854,#146855,
#146856,#146857,#146858,#146859,#146860,#146861,#146862,#146863,#146864,
#146865,#146866,#146867,#146868,#146869,#146870,#146871,#146872,#146873,
#146874,#146875,#146876,#146877,#146878,#146879,#146880,#146881,#146882,
#146883,#146884,#146885,#146886,#146887,#146888,#146889,#146890,#146891,
#146892,#146893,#146894,#146895,#146896,#146897,#146898,#146899,#146900,
#146901,#146902,#146903,#146904,#146905,#146906,#146907,#146908,#146909,
#146910,#146911,#146912,#146913,#146914,#146915,#146916,#146917,#146918,
#146919,#146920,#146921,#146922,#146923,#146924,#146925,#146926,#146927,
#146928,#146929,#146930,#146931,#146932,#146933,#146934,#146935,#146936,
#146937,#146938,#146939,#146940,#146941,#146942,#146943,#146944,#146945,
#146946,#146947,#146948,#146949,#146950,#146951,#146952,#146953,#146954,
#146955,#146956,#146957,#146958,#146959,#146960,#146961,#146962,#146963,
#146964,#146965,#146966,#146967,#146968,#146969,#146970,#146971,#146972,
#146973,#146974,#146975,#146976,#146977,#146978,#146979,#146980,#146981,
#146982,#146983,#146984,#146985,#146986,#146987,#146988,#146989,#146990,
#146991,#146992,#146993,#146994,#146995,#146996,#146997,#146998,#146999,
#147000,#147001,#147002,#147003,#147004,#147005,#147006,#147007,#147008,
#147009,#147010,#147011,#147012,#147013,#147014,#147015,#147016,#147017,
#147018,#147019,#147020,#147021,#147022,#147023,#147024,#147025,#147026,
#147027,#147028,#147029,#147030,#147031,#147032,#147033,#147034),
 .UNSPECIFIED.,.F.,.F.,(4,3,3,3,3,3,3,3,3,3,3,3,3,3,3,3,3,3,3,3,3,3,3,3,
3,3,3,3,3,3,3,3,3,3,3,3,3,3,3,3,3,3,3,3,3,3,3,3,3,3,3,3,3,3,3,3,3,3,3,3,
3,3,3,3,3,3,3,3,3,3,3,3,3,4),(-186.065429362419,-185.983699488653,-185.901969734882,
-185.820240099441,-185.738510580662,-185.656781176878,-185.575051886423,
-185.490105117904,-185.406485642643,-185.324172721683,-185.242433812616,
-185.16069532323,-185.07895724685,-184.997219576802,-184.915482306414,-184.833745429011,
-184.75200893792,-184.67027282647,-184.588537087988,-184.506801715802,-184.42506670324,
-184.343332043631,-184.261597730303,-184.179863756587,-184.098130115812,
-184.016396801307,-183.934663806402,-183.852931124429,-183.771198748717,
-183.689466672597,-183.607734889402,-183.526003392461,-183.444272175108,
-183.362541230673,-183.280810552488,-183.199080133888,-183.117349968202,
-183.035620048765,-182.95389036891,-182.87216092197,-182.786732727571,-182.703974164247,
-182.622235536683,-182.540497732879,-182.45876072614,-182.377024489772,
-182.295288997086,-182.213554221395,-182.131820136015,-182.050086714262,
-181.968353929457,-181.886621754922,-181.80489016398,-181.72315912996,-181.641428626187,
-181.559698625992,-181.477969102708,-181.394249702613,-181.312511621585,
-181.23077512616,-181.149040109576,-181.067306465087,-180.98557408597,-180.903842865517,
-180.822112697037,-180.736655947557,-180.654919029338,-180.573185020435,
-180.491453493915,-180.409724022987,-180.327989132511,-180.246259052346,
-180.164527623284,-180.138458701197),.UNSPECIFIED.);
#3063=B_SPLINE_CURVE_WITH_KNOTS('',3,(#147040,#147041,#147042,#147043,#147044,
#147045,#147046,#147047,#147048,#147049,#147050,#147051,#147052,#147053,
#147054,#147055,#147056,#147057,#147058,#147059,#147060,#147061,#147062,
#147063,#147064,#147065,#147066,#147067,#147068,#147069,#147070,#147071,
#147072,#147073,#147074,#147075,#147076,#147077,#147078,#147079,#147080,
#147081,#147082,#147083,#147084,#147085,#147086,#147087,#147088,#147089,
#147090,#147091,#147092,#147093,#147094,#147095,#147096,#147097,#147098,
#147099,#147100,#147101,#147102,#147103,#147104,#147105,#147106,#147107,
#147108,#147109,#147110,#147111,#147112,#147113,#147114,#147115,#147116,
#147117,#147118,#147119,#147120,#147121,#147122,#147123,#147124,#147125,
#147126,#147127,#147128,#147129,#147130,#147131,#147132,#147133,#147134,
#147135,#147136,#147137,#147138,#147139,#147140,#147141,#147142,#147143,
#147144,#147145,#147146,#147147,#147148,#147149,#147150,#147151,#147152,
#147153,#147154,#147155,#147156,#147157,#147158,#147159,#147160,#147161,
#147162,#147163,#147164,#147165,#147166,#147167,#147168,#147169,#147170,
#147171,#147172,#147173,#147174,#147175,#147176,#147177,#147178,#147179,
#147180,#147181,#147182,#147183,#147184,#147185,#147186,#147187,#147188,
#147189,#147190,#147191,#147192,#147193,#147194,#147195,#147196,#147197,
#147198,#147199,#147200,#147201,#147202,#147203,#147204,#147205,#147206,
#147207,#147208,#147209,#147210,#147211,#147212,#147213,#147214,#147215,
#147216,#147217,#147218,#147219,#147220,#147221,#147222,#147223,#147224,
#147225,#147226,#147227,#147228,#147229,#147230,#147231,#147232,#147233,
#147234,#147235,#147236,#147237,#147238,#147239,#147240,#147241,#147242,
#147243,#147244,#147245,#147246,#147247,#147248,#147249,#147250,#147251,
#147252,#147253,#147254,#147255,#147256,#147257,#147258,#147259,#147260,
#147261,#147262,#147263,#147264,#147265,#147266,#147267,#147268,#147269,
#147270,#147271),.UNSPECIFIED.,.F.,.F.,(4,3,3,3,3,3,3,3,3,3,3,3,3,3,3,3,
3,3,3,3,3,3,3,3,3,3,3,3,3,3,3,3,3,3,3,3,3,3,3,3,3,3,3,3,3,3,3,3,3,3,3,3,
3,3,3,3,3,3,3,3,3,3,3,3,3,3,3,3,3,3,3,3,3,3,3,3,3,4),(177.594716365316,
177.673667692144,177.752566694605,177.831424976149,177.910257755466,177.989075987583,
178.06789018167,178.146710843128,178.225576826486,178.304464218069,178.38342159048,
178.451738504106,178.525843942414,178.599892440475,178.673899178688,178.747888443046,
178.821865804863,178.8958680911,178.950207047413,179.041206146889,179.13270936428,
179.224652902903,179.316687479773,179.408596569598,179.448675590721,179.524385261863,
179.600046263912,179.675673104274,179.75129080058,179.826902300691,179.902542225342,
179.947144134028,180.029422905902,180.111725468786,180.195197270924,180.277552225844,
180.36158245159,180.445612677336,180.527991687909,180.610355877129,180.693787213008,
180.776109186271,180.860095203457,180.944081220644,181.019721329879,181.095337432798,
181.170943999866,181.246578662589,181.32222822118,181.397938510971,181.442549763951,
181.534450333637,181.626483303333,181.718362873137,181.809990269148,181.901011390613,
181.941018307259,182.015020221949,182.089001150295,182.162976172209,182.236988645512,
182.311019915495,182.385124667702,182.439486850566,182.518448266513,182.597355689582,
182.676220728518,182.755054959244,182.833869933222,182.912691196882,182.991517835994,
183.070360360371,183.149229288953,183.228171340284,183.307152105773,183.38622311679,
183.436423937181,183.521483599344),.UNSPECIFIED.);
#3064=B_SPLINE_CURVE_WITH_KNOTS('',3,(#147272,#147273,#147274,#147275,#147276,
#147277,#147278,#147279,#147280,#147281,#147282,#147283,#147284,#147285,
#147286,#147287),.UNSPECIFIED.,.F.,.F.,(4,3,3,3,3,4),(183.521483599436,
183.598089530995,183.674591230521,183.751032931773,183.827419279678,183.87796157873),
 .UNSPECIFIED.);
#3065=B_SPLINE_CURVE_WITH_KNOTS('',3,(#147289,#147290,#147291,#147292,#147293,
#147294,#147295,#147296,#147297,#147298,#147299,#147300,#147301,#147302,
#147303,#147304),.UNSPECIFIED.,.F.,.F.,(4,3,3,3,3,4),(-180.138458701197,
-180.056729157361,-179.974994042442,-179.893263805093,-179.811532016142,
-179.782244055239),.UNSPECIFIED.);
#3066=B_SPLINE_CURVE_WITH_KNOTS('',3,(#147305,#147306,#147307,#147308,#147309,
#147310,#147311,#147312,#147313,#147314,#147315,#147316,#147317,#147318,
#147319,#147320,#147321,#147322,#147323,#147324,#147325,#147326,#147327,
#147328,#147329,#147330,#147331,#147332,#147333,#147334,#147335,#147336,
#147337,#147338,#147339,#147340,#147341,#147342,#147343,#147344,#147345,
#147346,#147347,#147348,#147349,#147350,#147351,#147352,#147353,#147354,
#147355,#147356,#147357,#147358,#147359,#147360,#147361,#147362,#147363,
#147364,#147365,#147366,#147367,#147368,#147369,#147370,#147371,#147372,
#147373,#147374,#147375,#147376,#147377,#147378,#147379,#147380,#147381,
#147382,#147383,#147384,#147385,#147386,#147387,#147388,#147389,#147390,
#147391,#147392,#147393,#147394,#147395,#147396,#147397,#147398,#147399,
#147400,#147401,#147402,#147403,#147404,#147405,#147406,#147407,#147408,
#147409,#147410,#147411,#147412,#147413,#147414,#147415,#147416,#147417,
#147418,#147419,#147420,#147421,#147422,#147423,#147424,#147425,#147426,
#147427,#147428,#147429,#147430,#147431,#147432,#147433,#147434,#147435,
#147436,#147437,#147438,#147439,#147440,#147441,#147442,#147443,#147444,
#147445,#147446,#147447,#147448,#147449,#147450,#147451,#147452,#147453,
#147454,#147455,#147456,#147457,#147458,#147459,#147460,#147461,#147462,
#147463,#147464,#147465,#147466,#147467,#147468,#147469,#147470,#147471,
#147472,#147473,#147474,#147475,#147476,#147477,#147478,#147479,#147480,
#147481,#147482,#147483,#147484,#147485,#147486,#147487,#147488,#147489,
#147490,#147491,#147492,#147493,#147494,#147495,#147496,#147497,#147498,
#147499,#147500,#147501,#147502,#147503,#147504,#147505,#147506,#147507,
#147508,#147509,#147510,#147511,#147512,#147513,#147514,#147515,#147516,
#147517,#147518,#147519,#147520,#147521,#147522,#147523,#147524,#147525,
#147526,#147527,#147528,#147529,#147530,#147531,#147532,#147533,#147534,
#147535,#147536,#147537,#147538,#147539,#147540,#147541,#147542,#147543,
#147544,#147545),.UNSPECIFIED.,.F.,.F.,(4,3,3,3,3,3,3,3,3,3,3,3,3,3,3,3,
3,3,3,3,3,3,3,3,3,3,3,3,3,3,3,3,3,3,3,3,3,3,3,3,3,3,3,3,3,3,3,3,3,3,3,3,
3,3,3,3,3,3,3,3,3,3,3,3,3,3,3,3,3,3,3,3,3,3,3,3,3,3,3,3,4),(-179.782244055239,
-179.70674937923,-179.631225012669,-179.555683642121,-179.480083302716,
-179.448675590721,-179.356775021314,-179.264742051907,-179.172862482386,
-179.081235086644,-178.990213965419,-178.950207047413,-178.876205132521,
-178.802224203973,-178.728249181856,-178.65423670835,-178.580205438163,
-178.506100685752,-178.451738504106,-178.37277708835,-178.293869665473,
-178.21500462673,-178.136170396199,-178.057355422415,-177.978534158949,
-177.89970752003,-177.820864995846,-177.741996067454,-177.66305401631,-177.584073251007,
-177.505002240169,-177.454801417491,-177.375809521819,-177.296917736817,
-177.218115480452,-177.13941547932,-177.060776033139,-176.982199750662,
-176.956332874183,-176.87774615106,-176.799109983836,-176.720413990555,
-176.641599959103,-176.562718530908,-176.483715437716,-176.457864330876,
-176.378791810217,-176.299792256578,-176.220853989855,-176.141965376475,
-176.063114821019,-175.984286317844,-175.90546994506,-175.826655194952,
-175.747831562039,-175.668961515531,-175.590067837481,-175.511107313639,
-175.46092724426,-175.386821801255,-175.312773298522,-175.238766555663,
-175.164777286706,-175.090799920313,-175.016797629551,-174.962458700953,
-174.871459625913,-174.779956434837,-174.688012923564,-174.595978373746,
-174.504069309141,-174.463990157645,-174.388280473823,-174.312619459148,
-174.236992606224,-174.161374897479,-174.085763384994,-174.010123448111,
-173.965521614338,-173.883281692548,-173.855477722695),.UNSPECIFIED.);
#3067=B_SPLINE_CURVE_WITH_KNOTS('',3,(#147551,#147552,#147553,#147554,#147555,
#147556,#147557,#147558,#147559,#147560,#147561,#147562,#147563,#147564,
#147565,#147566,#147567,#147568,#147569,#147570,#147571,#147572,#147573,
#147574,#147575,#147576,#147577,#147578,#147579,#147580,#147581,#147582,
#147583,#147584,#147585,#147586,#147587,#147588,#147589,#147590,#147591,
#147592,#147593,#147594,#147595,#147596,#147597,#147598,#147599,#147600,
#147601,#147602,#147603,#147604,#147605,#147606,#147607,#147608,#147609,
#147610,#147611,#147612,#147613,#147614,#147615,#147616,#147617,#147618,
#147619,#147620,#147621,#147622,#147623,#147624,#147625,#147626,#147627,
#147628,#147629,#147630,#147631,#147632,#147633,#147634,#147635,#147636,
#147637,#147638,#147639,#147640,#147641,#147642,#147643,#147644,#147645,
#147646,#147647,#147648,#147649,#147650,#147651,#147652,#147653,#147654,
#147655,#147656,#147657,#147658,#147659,#147660,#147661,#147662,#147663,
#147664,#147665,#147666,#147667,#147668,#147669,#147670,#147671,#147672,
#147673,#147674,#147675,#147676,#147677,#147678,#147679,#147680,#147681,
#147682,#147683,#147684,#147685,#147686,#147687,#147688,#147689,#147690,
#147691,#147692,#147693,#147694,#147695,#147696,#147697,#147698,#147699,
#147700,#147701,#147702,#147703,#147704,#147705,#147706,#147707,#147708,
#147709,#147710,#147711,#147712,#147713,#147714,#147715,#147716,#147717,
#147718,#147719,#147720,#147721,#147722,#147723,#147724,#147725,#147726,
#147727,#147728,#147729,#147730,#147731,#147732,#147733,#147734,#147735,
#147736,#147737,#147738,#147739,#147740,#147741,#147742,#147743,#147744,
#147745,#147746,#147747,#147748,#147749,#147750,#147751,#147752,#147753,
#147754,#147755,#147756,#147757,#147758,#147759,#147760,#147761,#147762,
#147763,#147764,#147765,#147766,#147767,#147768,#147769,#147770,#147771,
#147772,#147773,#147774,#147775,#147776,#147777,#147778,#147779,#147780,
#147781,#147782,#147783,#147784,#147785),.UNSPECIFIED.,.F.,.F.,(4,3,3,3,
3,3,3,3,3,3,3,3,3,3,3,3,3,3,3,3,3,3,3,3,3,3,3,3,3,3,3,3,3,3,3,3,3,3,3,3,
3,3,3,3,3,3,3,3,3,3,3,3,3,3,3,3,3,3,3,3,3,3,3,3,3,3,3,3,3,3,3,3,3,3,3,3,
3,3,4),(171.311431343321,171.394462023174,171.4731788978,171.547284682488,
171.621333526952,171.695340611491,171.769330221457,171.843307928735,171.917310559088,
171.971647441108,172.062645935509,172.154148482996,172.246091299276,172.338125146677,
172.430033533839,172.470115984415,172.545825784847,172.621486916478,172.697113886636,
172.772731712749,172.848343342738,172.923983396916,172.968584527723,173.050863244669,
173.133165751679,173.216637581517,173.298992479751,173.383022775391,173.46705307103,
173.549432078143,173.631796263722,173.715227601376,173.79754957065,173.881535592494,
173.965521614338,174.04116173582,174.116777851093,174.192384430612,174.268019105903,
174.343668677136,174.419378979628,174.463990157645,174.555890701794,174.647923644425,
174.739803186861,174.831430556288,174.92245165336,174.962458700953,175.036460620371,
175.110441553481,175.184416580198,175.258429058346,175.332460333206,175.406565090317,
175.46092724426,175.539888659215,175.618796081269,175.697661119169,175.776495348841,
175.855310321749,175.934131584323,176.01295822234,176.091800745614,176.170669673091,
176.249611723317,176.3285924877,176.407663497624,176.457864330876,176.536856226191,
176.615748010839,176.694550266853,176.773250267641,176.851889713482,176.930465995628,
176.956332874183,177.030702036272,177.105081017374,177.17952040767,177.238298292035),
 .UNSPECIFIED.);
#3068=B_SPLINE_CURVE_WITH_KNOTS('',3,(#147786,#147787,#147788,#147789,#147790,
#147791,#147792,#147793,#147794,#147795,#147796,#147797,#147798,#147799,
#147800,#147801),.UNSPECIFIED.,.F.,.F.,(4,3,3,3,3,4),(177.238298292165,
177.328651471841,177.419665567986,177.454801417491,177.533869140457,177.594716365316),
 .UNSPECIFIED.);
#3069=B_SPLINE_CURVE_WITH_KNOTS('',3,(#147803,#147804,#147805,#147806,#147807,
#147808,#147809,#147810,#147811,#147812,#147813,#147814,#147815,#147816,
#147817,#147818),.UNSPECIFIED.,.F.,.F.,(4,3,3,3,3,4),(-173.855477722695,
-173.773204617602,-173.690895316582,-173.608575252747,-173.526235864634,
-173.499058748059),.UNSPECIFIED.);
#3070=B_SPLINE_CURVE_WITH_KNOTS('',3,(#147819,#147820,#147821,#147822,#147823,
#147824,#147825,#147826,#147827,#147828,#147829,#147830,#147831,#147832,
#147833,#147834,#147835,#147836,#147837,#147838,#147839,#147840,#147841,
#147842,#147843,#147844,#147845,#147846,#147847,#147848,#147849,#147850,
#147851,#147852,#147853,#147854,#147855,#147856,#147857,#147858,#147859,
#147860,#147861,#147862,#147863,#147864,#147865,#147866,#147867,#147868,
#147869,#147870,#147871,#147872,#147873,#147874,#147875,#147876,#147877,
#147878,#147879,#147880,#147881,#147882,#147883,#147884,#147885,#147886,
#147887,#147888,#147889,#147890,#147891,#147892,#147893,#147894,#147895,
#147896,#147897,#147898,#147899,#147900,#147901,#147902,#147903,#147904,
#147905,#147906,#147907,#147908,#147909,#147910,#147911,#147912,#147913,
#147914,#147915,#147916,#147917,#147918,#147919,#147920,#147921,#147922,
#147923,#147924,#147925,#147926,#147927,#147928,#147929,#147930,#147931,
#147932,#147933,#147934,#147935,#147936,#147937,#147938,#147939,#147940,
#147941,#147942,#147943,#147944,#147945,#147946,#147947,#147948,#147949,
#147950,#147951,#147952,#147953,#147954,#147955,#147956,#147957,#147958,
#147959,#147960,#147961,#147962,#147963,#147964,#147965,#147966,#147967,
#147968,#147969,#147970,#147971,#147972,#147973,#147974,#147975,#147976,
#147977,#147978,#147979,#147980,#147981,#147982,#147983,#147984,#147985,
#147986,#147987,#147988,#147989,#147990,#147991,#147992,#147993,#147994,
#147995,#147996,#147997,#147998,#147999,#148000,#148001,#148002,#148003,
#148004,#148005,#148006,#148007,#148008,#148009,#148010,#148011,#148012,
#148013,#148014,#148015,#148016,#148017,#148018,#148019,#148020,#148021,
#148022,#148023,#148024,#148025,#148026,#148027,#148028,#148029,#148030,
#148031,#148032,#148033,#148034,#148035,#148036,#148037,#148038,#148039,
#148040,#148041,#148042,#148043,#148044,#148045,#148046,#148047,#148048,
#148049,#148050,#148051,#148052,#148053,#148054,#148055,#148056),
 .UNSPECIFIED.,.F.,.F.,(4,3,3,3,3,3,3,3,3,3,3,3,3,3,3,3,3,3,3,3,3,3,3,3,
3,3,3,3,3,3,3,3,3,3,3,3,3,3,3,3,3,3,3,3,3,3,3,3,3,3,3,3,3,3,3,3,3,3,3,3,
3,3,3,3,3,3,3,3,3,3,3,3,3,3,3,3,3,3,3,4),(-173.499058747929,-173.46705307103,
-173.384674116491,-173.302309983779,-173.218878619765,-173.13655670272,
-173.052570615222,-172.968584527723,-172.892944288927,-172.817328056207,
-172.741721359174,-172.666086566588,-172.590436878105,-172.514726458919,
-172.470115984415,-172.378216119382,-172.28618387761,-172.194305017949,
-172.102678297202,-172.011657774091,-171.971647441108,-171.897645181924,
-171.823663908182,-171.749688540053,-171.675675720032,-171.60164410271,
-171.527539003634,-171.4731788978,-171.394217594986,-171.315310285976,-171.236445361765,
-171.157611246176,-171.078796387488,-170.99997523868,-170.921148713993,
-170.842306303387,-170.763437487691,-170.684495547107,-170.605514891192,
-170.526443986869,-170.476241811185,-170.397250490465,-170.318359277892,
-170.239557590234,-170.160858149801,-170.082219258926,-170.003643522044,
-169.977773267877,-169.899184973782,-169.820547207909,-169.741849591751,
-169.663033911633,-169.584150820255,-169.505146053935,-169.47930472457,
-169.400234194684,-169.321236642535,-169.242300383456,-169.163413779317,
-169.084565230139,-169.005738717276,-168.9269243219,-168.848111532234,-168.76928983873,
-168.690421686318,-168.611529876873,-168.532571165133,-168.482367637955,
-168.408257109661,-168.334203555212,-168.260191795563,-168.18619757205,
-168.112215282172,-168.038208133164,-167.983899094647,-167.892990978227,
-167.801368859447,-167.70948624669,-167.617471027762,-167.571942423577),
 .UNSPECIFIED.);
#3071=B_SPLINE_CURVE_WITH_KNOTS('',3,(#148062,#148063,#148064,#148065,#148066,
#148067,#148068,#148069,#148070,#148071,#148072,#148073,#148074,#148075,
#148076,#148077,#148078,#148079,#148080,#148081,#148082,#148083,#148084,
#148085,#148086,#148087,#148088,#148089,#148090,#148091,#148092,#148093,
#148094,#148095,#148096,#148097,#148098,#148099,#148100,#148101,#148102,
#148103,#148104,#148105,#148106,#148107,#148108,#148109,#148110,#148111,
#148112,#148113,#148114,#148115,#148116,#148117,#148118,#148119,#148120,
#148121,#148122,#148123,#148124,#148125,#148126,#148127,#148128,#148129,
#148130,#148131,#148132,#148133,#148134,#148135,#148136,#148137,#148138,
#148139,#148140,#148141,#148142,#148143,#148144,#148145,#148146,#148147,
#148148,#148149,#148150,#148151,#148152,#148153,#148154,#148155,#148156,
#148157,#148158,#148159,#148160,#148161,#148162,#148163,#148164,#148165,
#148166,#148167,#148168,#148169,#148170,#148171,#148172,#148173,#148174,
#148175,#148176,#148177,#148178,#148179,#148180,#148181,#148182,#148183,
#148184,#148185,#148186,#148187,#148188,#148189,#148190,#148191,#148192,
#148193,#148194,#148195,#148196,#148197,#148198,#148199,#148200,#148201,
#148202,#148203,#148204,#148205,#148206,#148207,#148208,#148209,#148210,
#148211,#148212,#148213,#148214,#148215,#148216,#148217,#148218,#148219,
#148220,#148221,#148222,#148223,#148224,#148225,#148226,#148227,#148228,
#148229,#148230,#148231,#148232,#148233,#148234,#148235,#148236,#148237,
#148238,#148239,#148240,#148241,#148242,#148243,#148244,#148245,#148246,
#148247,#148248,#148249,#148250,#148251,#148252,#148253,#148254,#148255,
#148256,#148257,#148258,#148259,#148260,#148261,#148262,#148263,#148264,
#148265,#148266,#148267,#148268,#148269,#148270,#148271,#148272,#148273,
#148274,#148275,#148276,#148277,#148278,#148279,#148280,#148281,#148282,
#148283,#148284,#148285,#148286,#148287,#148288,#148289,#148290,#148291,
#148292,#148293),.UNSPECIFIED.,.F.,.F.,(4,3,3,3,3,3,3,3,3,3,3,3,3,3,3,3,
3,3,3,3,3,3,3,3,3,3,3,3,3,3,3,3,3,3,3,3,3,3,3,3,3,3,3,3,3,3,3,3,3,3,3,3,
3,3,3,3,3,3,3,3,3,3,3,3,3,3,3,3,3,3,3,3,3,3,3,3,3,4),(165.02754145477,165.117918435358,
165.211327921046,165.302367295196,165.396961836652,165.491556378109,165.567514022134,
165.643423783486,165.719300013385,165.795167433697,165.871028965888,165.946918501106,
165.990024921417,166.072127026197,166.15424939746,166.237810414276,166.319981292175,
166.404237378449,166.488493464724,166.570935886981,166.653364296468,166.736763724359,
166.819150225261,166.903056116646,166.986962008032,167.062596601454,167.138207188958,
167.21380824425,167.289437415811,167.365081491186,167.440786333058,167.48543055134,
167.57731665728,167.669334116649,167.761197748819,167.852809518232,167.943816086182,
167.983899094647,168.057905873878,168.131891713771,168.205871692892,168.279889182454,
168.353925506678,168.428035352154,168.482367637955,168.561327246203,168.64023281893,
168.719095969567,168.797928278697,168.876741302422,168.955560584526,169.034385225545,
169.113225739348,169.192092648921,169.271032682423,169.350011430197,169.429080442211,
169.47930472457,169.558298286639,169.637191727285,169.71599562514,169.794697239726,
169.873338280972,169.951916126491,169.977773267877,170.056359443274,170.13499505431,
170.21369048415,170.292503944947,170.371384798467,170.450387315026,170.476241811185,
170.559521333102,170.642694489389,170.725698825545,170.808594331111,170.891316876558,
170.955112984985),.UNSPECIFIED.);
#3072=B_SPLINE_CURVE_WITH_KNOTS('',3,(#148294,#148295,#148296,#148297,#148298,
#148299,#148300,#148301,#148302,#148303,#148304,#148305,#148306,#148307,
#148308,#148309),.UNSPECIFIED.,.F.,.F.,(4,3,3,3,3,4),(170.95511468872,171.037715426029,
171.120454088486,171.203260261769,171.286161630498,171.311431343321),
 .UNSPECIFIED.);
#3073=B_SPLINE_CURVE_WITH_KNOTS('',3,(#148311,#148312,#148313,#148314,#148315,
#148316,#148317,#148318,#148319,#148320,#148321,#148322,#148323,#148324,
#148325,#148326),.UNSPECIFIED.,.F.,.F.,(4,3,3,3,3,4),(-167.571942423577,
-167.485430551339,-167.409258995797,-167.333137055842,-167.257054247403,
-167.21587344088),.UNSPECIFIED.);
#3074=B_SPLINE_CURVE_WITH_KNOTS('',3,(#148327,#148328,#148329,#148330,#148331,
#148332,#148333,#148334,#148335,#148336,#148337,#148338,#148339,#148340,
#148341,#148342,#148343,#148344,#148345,#148346,#148347,#148348,#148349,
#148350,#148351,#148352,#148353,#148354,#148355,#148356,#148357,#148358,
#148359,#148360,#148361,#148362,#148363,#148364,#148365,#148366,#148367,
#148368,#148369,#148370,#148371,#148372,#148373,#148374,#148375,#148376,
#148377,#148378,#148379,#148380,#148381,#148382,#148383,#148384,#148385,
#148386,#148387,#148388,#148389,#148390,#148391,#148392,#148393,#148394,
#148395,#148396,#148397,#148398,#148399,#148400,#148401,#148402,#148403,
#148404,#148405,#148406,#148407,#148408,#148409,#148410,#148411,#148412,
#148413,#148414,#148415,#148416,#148417,#148418,#148419,#148420,#148421,
#148422,#148423,#148424,#148425,#148426,#148427,#148428,#148429,#148430,
#148431,#148432,#148433,#148434,#148435,#148436,#148437,#148438,#148439,
#148440,#148441,#148442,#148443,#148444,#148445,#148446,#148447,#148448,
#148449,#148450,#148451,#148452,#148453,#148454,#148455,#148456,#148457,
#148458,#148459,#148460,#148461,#148462,#148463,#148464,#148465,#148466,
#148467,#148468,#148469,#148470,#148471,#148472,#148473,#148474,#148475,
#148476,#148477,#148478,#148479,#148480,#148481,#148482,#148483,#148484,
#148485,#148486,#148487,#148488,#148489,#148490,#148491,#148492,#148493,
#148494,#148495,#148496,#148497,#148498,#148499,#148500,#148501,#148502,
#148503,#148504,#148505,#148506,#148507,#148508,#148509,#148510,#148511,
#148512,#148513,#148514,#148515,#148516,#148517,#148518,#148519,#148520,
#148521,#148522,#148523,#148524,#148525,#148526,#148527,#148528,#148529,
#148530,#148531,#148532,#148533,#148534,#148535,#148536,#148537,#148538,
#148539,#148540,#148541,#148542,#148543,#148544,#148545,#148546),
 .UNSPECIFIED.,.F.,.F.,(4,3,3,3,3,3,3,3,3,3,3,3,3,3,3,3,3,3,3,3,3,3,3,3,
3,3,3,3,3,3,3,3,3,3,3,3,3,3,3,3,3,3,3,3,3,3,3,3,3,3,3,3,3,3,3,3,3,3,3,3,
3,3,3,3,3,3,3,3,3,3,3,3,3,4),(-167.21587344088,-167.134143567114,-167.052413813343,
-166.970684177902,-166.888954659123,-166.807225255339,-166.725495964884,
-166.640549196365,-166.556929721104,-166.474616800144,-166.392877891077,
-166.31113940169,-166.229401325311,-166.147663655263,-166.065926384875,
-165.984189507472,-165.902453016381,-165.820716904931,-165.738981166449,
-165.657245794263,-165.575510781701,-165.493776122092,-165.412041808764,
-165.330307835048,-165.248574194272,-165.166840879767,-165.085107884863,
-165.003375202889,-164.921642827178,-164.839910751058,-164.758178967863,
-164.676447470922,-164.594716253569,-164.512985309134,-164.431254630949,
-164.349524212349,-164.267794046663,-164.186064127227,-164.104334447371,
-164.022605000431,-163.937176806032,-163.854418242708,-163.772679615145,
-163.690941811341,-163.609204804601,-163.527468568233,-163.445733075548,
-163.363998299857,-163.282264214476,-163.200530792723,-163.118798007918,
-163.037065833383,-162.955334242442,-162.873603208421,-162.791872704648,
-162.710142704454,-162.628413181169,-162.544693781075,-162.462955700046,
-162.381219204622,-162.299484188037,-162.217750543549,-162.136018164432,
-162.054286943979,-161.972556775498,-161.887100026018,-161.805363107799,
-161.723629098896,-161.641897572377,-161.560168101449,-161.478433210973,
-161.396703130808,-161.314971701746,-161.288902779658),.UNSPECIFIED.);
#3075=B_SPLINE_CURVE_WITH_KNOTS('',3,(#148552,#148553,#148554,#148555,#148556,
#148557,#148558,#148559,#148560,#148561,#148562,#148563,#148564,#148565,
#148566,#148567,#148568,#148569,#148570,#148571,#148572,#148573,#148574,
#148575,#148576,#148577,#148578,#148579,#148580,#148581,#148582,#148583,
#148584,#148585,#148586,#148587,#148588,#148589,#148590,#148591,#148592,
#148593,#148594,#148595,#148596,#148597,#148598,#148599,#148600,#148601,
#148602,#148603,#148604,#148605,#148606,#148607,#148608,#148609,#148610,
#148611,#148612,#148613,#148614,#148615,#148616,#148617,#148618,#148619,
#148620,#148621,#148622,#148623,#148624,#148625,#148626,#148627,#148628,
#148629,#148630,#148631,#148632,#148633,#148634,#148635,#148636,#148637,
#148638,#148639,#148640,#148641,#148642,#148643,#148644,#148645,#148646,
#148647,#148648,#148649,#148650,#148651,#148652,#148653,#148654,#148655,
#148656,#148657,#148658,#148659,#148660,#148661,#148662,#148663,#148664,
#148665,#148666,#148667,#148668,#148669,#148670,#148671,#148672,#148673,
#148674,#148675,#148676,#148677,#148678,#148679,#148680,#148681,#148682,
#148683,#148684,#148685,#148686,#148687,#148688,#148689,#148690,#148691,
#148692,#148693,#148694,#148695,#148696,#148697,#148698,#148699,#148700,
#148701,#148702,#148703,#148704,#148705,#148706,#148707,#148708,#148709,
#148710,#148711,#148712,#148713,#148714,#148715,#148716,#148717,#148718,
#148719,#148720,#148721,#148722,#148723,#148724,#148725,#148726,#148727,
#148728,#148729,#148730,#148731,#148732,#148733,#148734,#148735,#148736,
#148737,#148738,#148739,#148740,#148741,#148742,#148743,#148744,#148745,
#148746,#148747,#148748,#148749,#148750,#148751,#148752,#148753,#148754,
#148755,#148756,#148757,#148758,#148759,#148760,#148761,#148762,#148763,
#148764,#148765,#148766,#148767,#148768,#148769,#148770,#148771),
 .UNSPECIFIED.,.F.,.F.,(4,3,3,3,3,3,3,3,3,3,3,3,3,3,3,3,3,3,3,3,3,3,3,3,
3,3,3,3,3,3,3,3,3,3,3,3,3,3,3,3,3,3,3,3,3,3,3,3,3,3,3,3,3,3,3,3,3,3,3,3,
3,3,3,3,3,3,3,3,3,3,3,3,3,4),(158.744957016583,158.82668689035,158.90841664412,
158.990146279561,159.07187579834,159.153605202124,159.235334492578,159.320281261098,
159.403900736359,159.486213657319,159.567952566386,159.649691055772,159.731429132152,
159.8131668022,159.894904072588,159.976640949991,160.058377441081,160.140113552531,
160.221849291013,160.3035846632,160.385319675762,160.467054335371,160.548788648698,
160.630522622414,160.71225626319,160.793989577695,160.8757225726,160.957455254573,
161.039187630285,161.120919706404,161.2026514896,161.28438298654,161.366114203894,
161.447845148329,161.529575826513,161.611306245114,161.693036410799,161.774766330236,
161.856496010091,161.938225457032,162.023653651431,162.106412214755,162.188150842318,
162.269888646122,162.351625652862,162.43336188923,162.515097381915,162.596832157606,
162.678566242987,162.76029966474,162.842032449545,162.92376462408,163.005496215021,
163.087227249042,163.168957752814,163.250687753009,163.332417276294,163.416136676388,
163.497874757417,163.579611252841,163.661346269426,163.743079913914,163.824812293031,
163.906543513484,163.988273681965,164.073730431445,164.155467349664,164.237201358567,
164.318932885086,164.400662356015,164.48239724649,164.564127326655,164.645858755717,
164.671927677806),.UNSPECIFIED.);
#3076=B_SPLINE_CURVE_WITH_KNOTS('',3,(#148772,#148773,#148774,#148775,#148776,
#148777,#148778,#148779,#148780,#148781,#148782,#148783,#148784,#148785,
#148786,#148787,#148788,#148789,#148790),.UNSPECIFIED.,.F.,.F.,(4,3,3,3,
3,3,4),(164.672427783019,164.744041659808,164.8156404277,164.88722929276,
164.958841893886,164.993087834802,165.02754145477),.UNSPECIFIED.);
#3077=B_SPLINE_CURVE_WITH_KNOTS('',3,(#148792,#148793,#148794,#148795,#148796,
#148797,#148798,#148799,#148800,#148801,#148802,#148803,#148804,#148805,
#148806,#148807),.UNSPECIFIED.,.F.,.F.,(4,3,3,3,3,4),(-161.288902779658,
-161.207173235822,-161.125438120903,-161.043707883554,-160.961976094603,
-160.9326881337),.UNSPECIFIED.);
#3078=B_SPLINE_CURVE_WITH_KNOTS('',3,(#148808,#148809,#148810,#148811,#148812,
#148813,#148814,#148815,#148816,#148817,#148818,#148819,#148820,#148821,
#148822,#148823,#148824,#148825,#148826,#148827,#148828,#148829,#148830,
#148831,#148832,#148833,#148834,#148835,#148836,#148837,#148838,#148839,
#148840,#148841,#148842,#148843,#148844,#148845,#148846,#148847,#148848,
#148849,#148850,#148851,#148852,#148853,#148854,#148855,#148856,#148857,
#148858,#148859,#148860,#148861,#148862,#148863,#148864,#148865,#148866,
#148867,#148868,#148869,#148870,#148871,#148872,#148873,#148874,#148875,
#148876,#148877,#148878,#148879,#148880,#148881,#148882,#148883,#148884,
#148885,#148886,#148887,#148888,#148889,#148890,#148891,#148892,#148893,
#148894,#148895,#148896,#148897,#148898,#148899,#148900,#148901,#148902,
#148903,#148904,#148905,#148906,#148907,#148908,#148909,#148910,#148911,
#148912,#148913,#148914,#148915,#148916,#148917,#148918,#148919,#148920,
#148921,#148922,#148923,#148924,#148925,#148926,#148927,#148928,#148929,
#148930,#148931,#148932,#148933,#148934,#148935,#148936,#148937,#148938,
#148939,#148940,#148941,#148942,#148943,#148944,#148945,#148946,#148947,
#148948,#148949,#148950,#148951,#148952,#148953,#148954,#148955,#148956,
#148957,#148958,#148959,#148960,#148961,#148962,#148963,#148964,#148965,
#148966,#148967,#148968,#148969,#148970,#148971,#148972,#148973,#148974,
#148975,#148976,#148977,#148978,#148979,#148980,#148981,#148982,#148983,
#148984,#148985,#148986,#148987,#148988,#148989,#148990,#148991,#148992,
#148993,#148994,#148995,#148996,#148997,#148998,#148999,#149000,#149001,
#149002,#149003,#149004,#149005,#149006,#149007,#149008,#149009,#149010,
#149011,#149012,#149013,#149014,#149015,#149016,#149017,#149018,#149019,
#149020,#149021,#149022,#149023,#149024,#149025,#149026,#149027,#149028,
#149029,#149030,#149031,#149032,#149033,#149034,#149035,#149036,#149037,
#149038,#149039,#149040,#149041,#149042,#149043,#149044,#149045),
 .UNSPECIFIED.,.F.,.F.,(4,3,3,3,3,3,3,3,3,3,3,3,3,3,3,3,3,3,3,3,3,3,3,3,
3,3,3,3,3,3,3,3,3,3,3,3,3,3,3,3,3,3,3,3,3,3,3,3,3,3,3,3,3,3,3,3,3,3,3,3,
3,3,3,3,3,3,3,3,3,3,3,3,3,3,3,3,3,3,3,4),(-160.9326881337,-160.851753714582,
-160.770640585143,-160.689254829997,-160.607715595427,-160.525950020712,
-160.506870945034,-160.429026496388,-160.351272650518,-160.273595290889,
-160.195980354179,-160.118413820932,-160.040878611182,-159.963359829769,
-159.885844826791,-159.808320956824,-159.730742760459,-159.653137126767,
-159.575447421521,-159.509933858419,-159.431228794851,-159.352592103808,
-159.274012702095,-159.195486763226,-159.116992780832,-159.038519564958,
-159.011465315111,-158.929812605011,-158.848093681957,-158.764319454419,
-158.682430650419,-158.597713711111,-158.512996771803,-158.431594055443,
-158.350260504194,-158.266327435269,-158.185145307839,-158.099836768167,
-158.014528228496,-157.935506745639,-157.856463939296,-157.777390015581,
-157.698242168605,-157.619052686286,-157.53978064037,-157.516059685188,
-157.438550009036,-157.361107114613,-157.283716716122,-157.206364564723,
-157.129036439365,-157.051701752493,-156.974360228904,-156.896998990283,
-156.819605149562,-156.74211896366,-156.664584530957,-156.586930454071,
-156.519122598573,-156.443888371344,-156.368748377998,-156.293686181249,
-156.218685427187,-156.143729825913,-156.066036786669,-155.991108027357,
-155.916172470055,-155.841215430626,-155.76622220858,-155.691136858506,
-155.615996739876,-155.54074829231,-155.522185511958,-155.444955082429,
-155.367811457943,-155.290741127077,-155.213741865405,-155.13678410832,
-155.059853433246,-155.005663677983),.UNSPECIFIED.);
#3079=B_SPLINE_CURVE_WITH_KNOTS('',3,(#149051,#149052,#149053,#149054,#149055,
#149056,#149057,#149058,#149059,#149060,#149061,#149062,#149063,#149064,
#149065,#149066,#149067,#149068,#149069,#149070,#149071,#149072,#149073,
#149074,#149075,#149076,#149077,#149078,#149079,#149080,#149081,#149082,
#149083,#149084,#149085,#149086,#149087,#149088,#149089,#149090,#149091,
#149092,#149093,#149094,#149095,#149096,#149097,#149098,#149099,#149100,
#149101,#149102,#149103,#149104,#149105,#149106,#149107,#149108,#149109,
#149110,#149111,#149112,#149113,#149114,#149115,#149116,#149117,#149118,
#149119,#149120,#149121,#149122,#149123,#149124,#149125,#149126,#149127,
#149128,#149129,#149130,#149131,#149132,#149133,#149134,#149135,#149136,
#149137,#149138,#149139,#149140,#149141,#149142,#149143,#149144,#149145,
#149146,#149147,#149148,#149149,#149150,#149151,#149152,#149153,#149154,
#149155,#149156,#149157,#149158,#149159,#149160,#149161,#149162,#149163,
#149164,#149165,#149166,#149167,#149168,#149169,#149170,#149171,#149172,
#149173,#149174,#149175,#149176,#149177,#149178,#149179,#149180,#149181,
#149182,#149183,#149184,#149185,#149186,#149187,#149188,#149189,#149190,
#149191,#149192,#149193,#149194,#149195,#149196,#149197,#149198,#149199,
#149200,#149201,#149202,#149203,#149204,#149205,#149206,#149207,#149208,
#149209,#149210,#149211,#149212,#149213,#149214,#149215,#149216,#149217,
#149218,#149219,#149220,#149221,#149222,#149223,#149224,#149225,#149226,
#149227,#149228,#149229,#149230,#149231,#149232,#149233,#149234,#149235,
#149236,#149237,#149238,#149239,#149240,#149241,#149242,#149243,#149244,
#149245,#149246,#149247,#149248,#149249,#149250,#149251,#149252,#149253,
#149254,#149255,#149256,#149257,#149258,#149259,#149260,#149261,#149262,
#149263,#149264,#149265,#149266,#149267,#149268,#149269,#149270,#149271,
#149272,#149273,#149274,#149275,#149276,#149277,#149278,#149279,#149280,
#149281,#149282,#149283,#149284,#149285,#149286,#149287,#149288,#149289,
#149290,#149291),.UNSPECIFIED.,.F.,.F.,(4,3,3,3,3,3,3,3,3,3,3,3,3,3,3,3,
3,3,3,3,3,3,3,3,3,3,3,3,3,3,3,3,3,3,3,3,3,3,3,3,3,3,3,3,3,3,3,3,3,3,3,3,
3,3,3,3,3,3,3,3,3,3,3,3,3,3,3,3,3,3,3,3,3,3,3,3,3,3,3,3,4),(152.461872548045,
152.531374252113,152.608905049108,152.686380993047,152.76381497896,152.841222846017,
152.918615169387,152.996015244036,153.02984279542,153.108966009833,153.188092851743,
153.267233018585,153.346420626813,153.425634399544,153.50490824031,153.528311338728,
153.613266920936,153.698202335754,153.783065063921,153.867859507684,153.952513587944,
154.026779882035,154.104294440241,154.181804546132,154.259322876478,154.336889387948,
154.414483072056,154.492147142944,154.525248425343,154.603042406765,154.680774851418,
154.758459588496,154.836110412816,154.913741093835,154.991382886643,155.069034149677,
155.146707365294,155.224415026398,155.302215990995,155.380066106682,155.458034270177,
155.522185511958,155.597418690668,155.672557806474,155.747619295678,155.822619511427,
155.897574743044,155.975268224986,156.050197038596,156.125132807108,156.200090214791,
156.275083962399,156.350170069209,156.425311080461,156.50056061365,156.519122598573,
156.596785594421,156.674356120084,156.751848550961,156.829277208533,156.906656369881,
156.984003284394,157.061333319959,157.138659355257,157.215994264305,157.293384539171,
157.37080265027,157.448307120662,157.516059685188,157.595324306327,157.674520101997,
157.753656985933,157.83273536786,157.911778254531,157.990793017878,158.014528228496,
158.093583812149,158.172704056942,158.251857104928,158.331092251217,158.388376241259),
 .UNSPECIFIED.);
#3080=B_SPLINE_CURVE_WITH_KNOTS('',3,(#149292,#149293,#149294,#149295,#149296,
#149297,#149298,#149299,#149300,#149301,#149302,#149303,#149304,#149305,
#149306,#149307),.UNSPECIFIED.,.F.,.F.,(4,3,3,3,3,4),(158.388742370626,
158.470471914462,158.552207029381,158.63393726673,158.715669055681,158.744957016583),
 .UNSPECIFIED.);
#3081=B_SPLINE_CURVE_WITH_KNOTS('',3,(#149309,#149310,#149311,#149312,#149313,
#149314,#149315,#149316,#149317,#149318,#149319,#149320,#149321,#149322,
#149323,#149324),.UNSPECIFIED.,.F.,.F.,(4,3,3,3,3,4),(-155.005663677983,
-154.928750365625,-154.851804570041,-154.77484175986,-154.697816546421,
-154.649502826602),.UNSPECIFIED.);
#3082=B_SPLINE_CURVE_WITH_KNOTS('',3,(#149325,#149326,#149327,#149328,#149329,
#149330,#149331,#149332,#149333,#149334,#149335,#149336,#149337,#149338,
#149339,#149340,#149341,#149342,#149343,#149344,#149345,#149346,#149347,
#149348,#149349,#149350,#149351,#149352,#149353,#149354,#149355,#149356,
#149357,#149358,#149359,#149360,#149361,#149362,#149363,#149364,#149365,
#149366,#149367,#149368,#149369,#149370,#149371,#149372,#149373,#149374,
#149375,#149376,#149377,#149378,#149379,#149380,#149381,#149382,#149383,
#149384,#149385,#149386,#149387,#149388,#149389,#149390,#149391,#149392,
#149393,#149394,#149395,#149396,#149397,#149398,#149399,#149400,#149401,
#149402,#149403,#149404,#149405,#149406,#149407,#149408,#149409,#149410,
#149411,#149412,#149413,#149414,#149415,#149416,#149417,#149418,#149419,
#149420,#149421,#149422,#149423,#149424,#149425,#149426,#149427,#149428,
#149429,#149430,#149431,#149432,#149433,#149434,#149435,#149436,#149437,
#149438,#149439,#149440,#149441,#149442,#149443,#149444,#149445,#149446,
#149447,#149448,#149449,#149450,#149451,#149452,#149453,#149454,#149455,
#149456,#149457,#149458,#149459,#149460,#149461,#149462,#149463,#149464,
#149465,#149466,#149467,#149468,#149469,#149470,#149471,#149472,#149473,
#149474,#149475,#149476,#149477,#149478,#149479,#149480,#149481,#149482,
#149483,#149484,#149485,#149486,#149487,#149488,#149489,#149490,#149491,
#149492,#149493,#149494,#149495,#149496,#149497,#149498,#149499,#149500,
#149501,#149502,#149503,#149504,#149505,#149506,#149507,#149508,#149509,
#149510,#149511,#149512,#149513,#149514,#149515,#149516,#149517,#149518,
#149519,#149520,#149521,#149522,#149523,#149524,#149525,#149526,#149527,
#149528,#149529,#149530,#149531,#149532,#149533,#149534,#149535,#149536,
#149537,#149538,#149539,#149540,#149541,#149542,#149543,#149544,#149545,
#149546,#149547,#149548,#149549,#149550,#149551,#149552,#149553,#149554,
#149555,#149556,#149557,#149558,#149559,#149560,#149561,#149562),
 .UNSPECIFIED.,.F.,.F.,(4,3,3,3,3,3,3,3,3,3,3,3,3,3,3,3,3,3,3,3,3,3,3,3,
3,3,3,3,3,3,3,3,3,3,3,3,3,3,3,3,3,3,3,3,3,3,3,3,3,3,3,3,3,3,3,3,3,3,3,3,
3,3,3,3,3,3,3,3,3,3,3,3,3,3,3,3,3,3,3,4),(-154.649502826521,-154.525248425343,
-154.447587709264,-154.369984567194,-154.29242625479,-154.214898763173,
-154.137389544905,-154.059877070554,-154.026779882035,-153.942155713893,
-153.857420741895,-153.772553364838,-153.687641000974,-153.602685811278,
-153.528311338728,-153.449042151582,-153.369823495967,-153.290645602546,
-153.211499792603,-153.132374156501,-153.053254885006,-153.02984279542,
-152.952441049764,-152.875047326639,-152.797648790269,-152.720206658767,
-152.642740007134,-152.565206289548,-152.531374252113,-152.441611266669,
-152.351813698248,-152.262177425072,-152.172732395101,-152.083727450608,
-152.032905708805,-151.958589664459,-151.884292438208,-151.809999042985,
-151.735665740119,-151.661311952551,-151.586883380113,-151.534437165498,
-151.455503202959,-151.376623859828,-151.297787454988,-151.218982340526,
-151.140196893334,-151.061405591473,-150.982609139477,-150.903796964785,
-150.824958485864,-150.746046820653,-150.667096413218,-150.588055433093,
-150.537500078883,-150.458590748963,-150.379781364379,-150.301061176057,
-150.222442401086,-150.143883589462,-150.065386817239,-150.039031535575,
-149.960384680215,-149.881686893022,-149.802927930414,-149.724049334714,
-149.645102435641,-149.566032998171,-149.540562992267,-149.461498149583,
-149.382507986401,-149.29998865198,-149.221122885299,-149.142291855357,
-149.063484993942,-148.984691749771,-148.905888638323,-148.827080945834,
-148.748242150062,-148.722353311028),.UNSPECIFIED.);
#3083=B_SPLINE_CURVE_WITH_KNOTS('',3,(#149568,#149569,#149570,#149571,#149572,
#149573,#149574,#149575,#149576,#149577,#149578,#149579,#149580,#149581,
#149582,#149583,#149584,#149585,#149586,#149587,#149588,#149589,#149590,
#149591,#149592,#149593,#149594,#149595,#149596,#149597,#149598,#149599,
#149600,#149601,#149602,#149603,#149604,#149605,#149606,#149607,#149608,
#149609,#149610,#149611,#149612,#149613,#149614,#149615,#149616,#149617,
#149618,#149619,#149620,#149621,#149622,#149623,#149624,#149625,#149626,
#149627,#149628,#149629,#149630,#149631,#149632,#149633,#149634,#149635,
#149636,#149637,#149638,#149639,#149640,#149641,#149642,#149643,#149644,
#149645,#149646,#149647,#149648,#149649,#149650,#149651,#149652,#149653,
#149654,#149655,#149656,#149657,#149658,#149659,#149660,#149661,#149662,
#149663,#149664,#149665,#149666,#149667,#149668,#149669,#149670,#149671,
#149672,#149673,#149674,#149675,#149676,#149677,#149678,#149679,#149680,
#149681,#149682,#149683,#149684,#149685,#149686,#149687,#149688,#149689,
#149690,#149691,#149692,#149693,#149694,#149695,#149696,#149697,#149698,
#149699,#149700,#149701,#149702,#149703,#149704,#149705,#149706,#149707,
#149708,#149709,#149710,#149711,#149712,#149713,#149714,#149715,#149716,
#149717,#149718,#149719,#149720,#149721,#149722,#149723,#149724,#149725,
#149726,#149727,#149728,#149729,#149730,#149731,#149732,#149733,#149734,
#149735,#149736,#149737,#149738,#149739,#149740,#149741,#149742,#149743,
#149744,#149745,#149746,#149747,#149748,#149749,#149750,#149751,#149752,
#149753,#149754,#149755,#149756,#149757,#149758,#149759,#149760,#149761,
#149762,#149763,#149764,#149765,#149766,#149767,#149768,#149769,#149770,
#149771,#149772,#149773,#149774,#149775,#149776,#149777,#149778,#149779,
#149780,#149781,#149782,#149783,#149784,#149785,#149786,#149787),
 .UNSPECIFIED.,.F.,.F.,(4,3,3,3,3,3,3,3,3,3,3,3,3,3,3,3,3,3,3,3,3,3,3,3,
3,3,3,3,3,3,3,3,3,3,3,3,3,3,3,3,3,3,3,3,3,3,3,3,3,3,3,3,3,3,3,3,3,3,3,3,
3,3,3,3,3,3,3,3,3,3,3,3,3,4),(146.178586402224,146.260316275991,146.342046029761,
146.423775665203,146.505505183982,146.587234587766,146.66896387822,146.753910646739,
146.837530122,146.91984304296,147.001581952028,147.083320441414,147.165058517794,
147.246796187842,147.32853345823,147.410270335633,147.492006826723,147.573742938173,
147.655478676655,147.737214048842,147.818949061404,147.900683721013,147.98241803434,
148.064152008057,148.145885648832,148.227618963337,148.309351958242,148.391084640215,
148.472817015927,148.554549092046,148.636280875242,148.718012372182,148.799743589536,
148.881474533971,148.963205212155,149.044935630756,149.126665796441,149.208395715878,
149.290125395733,149.371854842673,149.457283037073,149.540041600397,149.62178022796,
149.703518031764,149.785255038504,149.866991274872,149.948726767557,150.030461543248,
150.112195628629,150.193929050381,150.275661835186,150.357394009722,150.439125600663,
150.520856634684,150.602587138456,150.684317138651,150.766046661936,150.84976606203,
150.931504143059,151.013240638483,151.094975655068,151.176709299556,151.258441678673,
151.340172899126,151.421903067606,151.507359817086,151.589096735305,151.670830744209,
151.752562270728,151.834291741656,151.916026632132,151.997756712297,152.079488141359,
152.105557063447),.UNSPECIFIED.);
#3084=B_SPLINE_CURVE_WITH_KNOTS('',3,(#149788,#149789,#149790,#149791,#149792,
#149793,#149794,#149795,#149796,#149797,#149798,#149799,#149800),
 .UNSPECIFIED.,.F.,.F.,(4,3,3,3,4),(152.105557063447,152.195632841689,152.285955846226,
152.37647093208,152.461872548045),.UNSPECIFIED.);
#3085=B_SPLINE_CURVE_WITH_KNOTS('',3,(#149802,#149803,#149804,#149805,#149806,
#149807,#149808,#149809,#149810,#149811,#149812,#149813,#149814,#149815,
#149816,#149817),.UNSPECIFIED.,.F.,.F.,(4,3,3,3,3,4),(-148.722353311028,
-148.643465082527,-148.564514557937,-148.543625905652,-148.454971712497,
-148.366317519341),.UNSPECIFIED.);
#3086=B_SPLINE_CURVE_WITH_KNOTS('',3,(#149818,#149819,#149820,#149821,#149822,
#149823,#149824,#149825,#149826,#149827,#149828,#149829,#149830,#149831,
#149832,#149833,#149834,#149835,#149836,#149837,#149838,#149839,#149840,
#149841,#149842,#149843,#149844,#149845,#149846,#149847,#149848,#149849,
#149850,#149851,#149852,#149853,#149854,#149855,#149856,#149857,#149858,
#149859,#149860,#149861,#149862,#149863,#149864,#149865,#149866,#149867,
#149868,#149869,#149870,#149871,#149872,#149873,#149874,#149875,#149876,
#149877,#149878,#149879,#149880,#149881,#149882,#149883,#149884,#149885,
#149886,#149887,#149888,#149889,#149890,#149891,#149892,#149893,#149894,
#149895,#149896,#149897,#149898,#149899,#149900,#149901,#149902,#149903,
#149904,#149905,#149906,#149907,#149908,#149909,#149910,#149911,#149912,
#149913,#149914,#149915,#149916,#149917,#149918,#149919,#149920,#149921,
#149922,#149923,#149924,#149925,#149926,#149927,#149928,#149929,#149930,
#149931,#149932,#149933,#149934,#149935,#149936,#149937,#149938,#149939,
#149940,#149941,#149942,#149943,#149944,#149945,#149946,#149947,#149948,
#149949,#149950,#149951,#149952,#149953,#149954,#149955,#149956,#149957,
#149958,#149959,#149960,#149961,#149962,#149963,#149964,#149965,#149966,
#149967,#149968,#149969,#149970,#149971,#149972,#149973,#149974,#149975,
#149976,#149977,#149978,#149979,#149980,#149981,#149982,#149983,#149984,
#149985,#149986,#149987,#149988,#149989,#149990,#149991,#149992,#149993,
#149994,#149995,#149996,#149997,#149998,#149999,#150000,#150001,#150002,
#150003,#150004,#150005,#150006,#150007,#150008,#150009,#150010,#150011,
#150012,#150013,#150014,#150015,#150016,#150017,#150018,#150019,#150020,
#150021,#150022,#150023,#150024,#150025,#150026,#150027,#150028,#150029,
#150030,#150031,#150032,#150033,#150034,#150035,#150036,#150037,#150038,
#150039,#150040,#150041,#150042,#150043,#150044,#150045,#150046,#150047,
#150048,#150049,#150050,#150051,#150052,#150053,#150054,#150055),
 .UNSPECIFIED.,.F.,.F.,(4,3,3,3,3,3,3,3,3,3,3,3,3,3,3,3,3,3,3,3,3,3,3,3,
3,3,3,3,3,3,3,3,3,3,3,3,3,3,3,3,3,3,3,3,3,3,3,3,3,3,3,3,3,3,3,3,3,3,3,3,
3,3,3,3,3,3,3,3,3,3,3,3,3,3,3,3,3,3,3,4),(-148.36631751921,-148.295097778499,
-148.223893167673,-148.152698698807,-148.081479920567,-148.045157362345,
-147.954159342607,-147.862657150356,-147.770714478799,-147.678680645011,
-147.586772073684,-147.546688819037,-147.470982507544,-147.395324882409,
-147.319701434226,-147.244087145053,-147.168479062259,-147.092842558515,
-147.04822027573,-146.965936488568,-146.883628796585,-146.800159530544,
-146.717799306148,-146.633775519285,-146.549751732422,-146.467376065816,
-146.385015272141,-146.301582251385,-146.219263712141,-146.135273450628,
-146.051283189114,-145.97564198174,-145.90002477354,-145.824417094708,-145.748781313446,
-145.673130631722,-145.597419216424,-145.552814645807,-145.46091508944,
-145.368883184751,-145.277004679384,-145.185378310241,-145.094358120478,
-145.054346102499,-144.980344107589,-144.906363098792,-144.832387996217,
-144.758375442111,-144.684344091165,-144.610239258084,-144.555877559192,
-144.476916121412,-144.398008675984,-144.319143614219,-144.240309360249,
-144.161494362667,-144.082673075002,-144.00384641167,-143.925003862908,
-143.846134909821,-143.767192833972,-143.688212043952,-143.609141008602,
-143.558940472577,-143.479948660699,-143.401056959162,-143.322254785764,
-143.243554866504,-143.16491550145,-143.086339298753,-143.060471929269,
-142.981885159439,-142.903248944468,-142.824552902507,-142.745738821302,
-142.666857342744,-142.587854198644,-142.562003385962,-142.478726056179,
-142.439142960337),.UNSPECIFIED.);
#3087=B_SPLINE_CURVE_WITH_KNOTS('',3,(#150061,#150062,#150063,#150064,#150065,
#150066,#150067,#150068,#150069,#150070,#150071,#150072,#150073,#150074,
#150075,#150076,#150077,#150078,#150079,#150080,#150081,#150082,#150083,
#150084,#150085,#150086,#150087,#150088,#150089,#150090,#150091,#150092,
#150093,#150094,#150095,#150096,#150097,#150098,#150099,#150100,#150101,
#150102,#150103,#150104,#150105,#150106,#150107,#150108,#150109,#150110,
#150111,#150112,#150113,#150114,#150115,#150116,#150117,#150118,#150119,
#150120,#150121,#150122,#150123,#150124,#150125,#150126,#150127,#150128,
#150129,#150130,#150131,#150132,#150133,#150134,#150135,#150136,#150137,
#150138,#150139,#150140,#150141,#150142,#150143,#150144,#150145,#150146,
#150147,#150148,#150149,#150150,#150151,#150152,#150153,#150154,#150155,
#150156,#150157,#150158,#150159,#150160,#150161,#150162,#150163,#150164,
#150165,#150166,#150167,#150168,#150169,#150170,#150171,#150172,#150173,
#150174,#150175,#150176,#150177,#150178,#150179,#150180,#150181,#150182,
#150183,#150184,#150185,#150186,#150187,#150188,#150189,#150190,#150191,
#150192,#150193,#150194,#150195,#150196,#150197,#150198,#150199,#150200,
#150201,#150202,#150203,#150204,#150205,#150206,#150207,#150208,#150209,
#150210,#150211,#150212,#150213,#150214,#150215,#150216,#150217,#150218,
#150219,#150220,#150221,#150222,#150223,#150224,#150225,#150226,#150227,
#150228,#150229,#150230,#150231,#150232,#150233,#150234,#150235,#150236,
#150237,#150238,#150239,#150240,#150241,#150242,#150243,#150244,#150245,
#150246,#150247,#150248,#150249,#150250,#150251,#150252,#150253,#150254,
#150255,#150256,#150257,#150258,#150259,#150260,#150261,#150262,#150263,
#150264,#150265,#150266,#150267,#150268,#150269,#150270,#150271,#150272,
#150273,#150274,#150275,#150276,#150277,#150278,#150279,#150280,#150281,
#150282,#150283,#150284,#150285,#150286,#150287,#150288,#150289,#150290,
#150291,#150292,#150293,#150294,#150295,#150296,#150297,#150298,#150299,
#150300,#150301),.UNSPECIFIED.,.F.,.F.,(4,3,3,3,3,3,3,3,3,3,3,3,3,3,3,3,
3,3,3,3,3,3,3,3,3,3,3,3,3,3,3,3,3,3,3,3,3,3,3,3,3,3,3,3,3,3,3,3,3,3,3,3,
3,3,3,3,3,3,3,3,3,3,3,3,3,3,3,3,3,3,3,3,3,3,3,3,3,3,3,3,4),(139.895602067557,
139.977901874986,140.060171044567,140.069660669424,140.145300773922,140.220916872101,
140.296523434427,140.372158092422,140.447807646289,140.52351793138,140.568129212731,
140.660029796919,140.752062781502,140.843942365698,140.935569775318,141.02659090873,
141.066597756039,141.140599667601,141.214580592822,141.288555611617,141.362568081812,
141.436599348694,141.51070409782,141.565066299346,141.644027707974,141.722935123658,
141.80180015516,141.88063437842,141.959449344918,142.038270601121,142.117097232801,
142.195939749784,142.27480867103,142.353750715161,142.432731473525,142.511802477606,
142.562003385962,142.640995331965,142.719887166777,142.79868947233,142.877389521512,
142.95602901502,143.034605343613,143.060471929269,143.139058572594,143.217694658848,
143.296390570157,143.37520451866,143.454085863362,143.533088872827,143.558940472577,
143.638013018572,143.717012597661,143.795950889894,143.874839528783,143.953690109694,
144.032518638095,144.11133503593,144.19014981086,144.268973468316,144.347843538777,
144.426737240448,144.505697787184,144.555877559192,144.629983078104,144.704031656759,
144.778038475533,144.852027820258,144.926005262392,145.000007628607,145.054346102499,
145.145344259658,145.236846452989,145.328788914312,145.420822418235,145.512730496857,
145.552814645807,145.628975917023,145.705087664326,145.781160440953,145.822371756267),
 .UNSPECIFIED.);
#3088=B_SPLINE_CURVE_WITH_KNOTS('',3,(#150302,#150303,#150304,#150305,#150306,
#150307,#150308,#150309,#150310,#150311,#150312,#150313,#150314,#150315,
#150316,#150317),.UNSPECIFIED.,.F.,.F.,(4,3,3,3,3,4),(145.822371756267,
145.904101300103,145.985836415022,146.067566652371,146.149298441322,146.178586402224),
 .UNSPECIFIED.);
#3089=B_SPLINE_CURVE_WITH_KNOTS('',3,(#150319,#150320,#150321,#150322,#150323,
#150324,#150325,#150326,#150327,#150328,#150329,#150330,#150331,#150332,
#150333,#150334),.UNSPECIFIED.,.F.,.F.,(4,3,3,3,3,4),(-142.439142960337,
-142.356023082934,-142.273070385938,-142.190228256313,-142.107546608186,
-142.083132212162),.UNSPECIFIED.);
#3090=B_SPLINE_CURVE_WITH_KNOTS('',3,(#150335,#150336,#150337,#150338,#150339,
#150340,#150341,#150342,#150343,#150344,#150345,#150346,#150347,#150348,
#150349,#150350,#150351,#150352,#150353,#150354,#150355,#150356,#150357,
#150358,#150359,#150360,#150361,#150362,#150363,#150364,#150365,#150366,
#150367,#150368,#150369,#150370,#150371,#150372,#150373,#150374,#150375,
#150376,#150377,#150378,#150379,#150380,#150381,#150382,#150383,#150384,
#150385,#150386,#150387,#150388,#150389,#150390,#150391,#150392,#150393,
#150394,#150395,#150396,#150397,#150398,#150399,#150400,#150401,#150402,
#150403,#150404,#150405,#150406,#150407,#150408,#150409,#150410,#150411,
#150412,#150413,#150414,#150415,#150416,#150417,#150418,#150419,#150420,
#150421,#150422,#150423,#150424,#150425,#150426,#150427,#150428,#150429,
#150430,#150431,#150432,#150433,#150434,#150435,#150436,#150437,#150438,
#150439,#150440,#150441,#150442,#150443,#150444,#150445,#150446,#150447,
#150448,#150449,#150450,#150451,#150452,#150453,#150454,#150455,#150456,
#150457,#150458,#150459,#150460,#150461,#150462,#150463,#150464,#150465,
#150466,#150467,#150468,#150469,#150470,#150471,#150472,#150473,#150474,
#150475,#150476,#150477,#150478,#150479,#150480,#150481,#150482,#150483,
#150484,#150485,#150486,#150487,#150488,#150489,#150490,#150491,#150492,
#150493,#150494,#150495,#150496,#150497,#150498,#150499,#150500,#150501,
#150502,#150503,#150504,#150505,#150506,#150507,#150508,#150509,#150510,
#150511,#150512,#150513,#150514,#150515,#150516,#150517,#150518,#150519,
#150520,#150521,#150522,#150523,#150524,#150525,#150526,#150527,#150528,
#150529,#150530,#150531,#150532,#150533,#150534,#150535,#150536,#150537,
#150538,#150539,#150540,#150541,#150542,#150543,#150544,#150545,#150546,
#150547,#150548,#150549,#150550,#150551,#150552,#150553,#150554,#150555,
#150556,#150557,#150558,#150559,#150560,#150561,#150562,#150563,#150564,
#150565,#150566,#150567,#150568,#150569),.UNSPECIFIED.,.F.,.F.,(4,3,3,3,
3,3,3,3,3,3,3,3,3,3,3,3,3,3,3,3,3,3,3,3,3,3,3,3,3,3,3,3,3,3,3,3,3,3,3,3,
3,3,3,3,3,3,3,3,3,3,3,3,3,3,3,3,3,3,3,3,3,3,3,3,3,3,3,3,3,3,3,3,3,3,3,3,
3,3,4),(-142.083130505234,-142.000499302849,-141.917779667378,-141.834977613084,
-141.752059853652,-141.66908716499,-141.586038721683,-141.565066299346,
-141.490960864321,-141.416912369555,-141.342905634648,-141.268916373607,
-141.194939015116,-141.120936732207,-141.066597756039,-140.975598644234,
-140.884095413094,-140.792151859509,-140.700117267453,-140.608208162886,
-140.568129212731,-140.492419546296,-140.416758548968,-140.341131713343,
-140.265514021781,-140.189902526422,-140.114262606517,-140.069660669424,
-139.98738189348,-139.90507932644,-139.821607526359,-139.739252567185,-139.65522234665,
-139.571192126116,-139.488813117401,-139.406448930065,-139.323017593251,
-139.240695621887,-139.156709602348,-139.072723582809,-138.997083473201,
-138.921467369906,-138.845860802462,-138.770226139361,-138.69457658039,
-138.61886629022,-138.574255039501,-138.482354469857,-138.390321500201,
-138.298441930429,-138.206814534445,-138.115793412998,-138.075786496194,
-138.001784581558,-137.927803653267,-137.853828631407,-137.779816158162,
-137.705784888235,-137.631680136085,-137.577317952886,-137.498356536905,
-137.419449113802,-137.34058407483,-137.261749844069,-137.182934870054,
-137.104113606357,-137.025286967207,-136.946444442794,-136.867575514174,
-136.788633462805,-136.709652697279,-136.630581686223,-136.580380866271,
-136.501378523423,-136.422477075346,-136.343694796591,-136.264982735704,
-136.186348045329,-136.155837210071),.UNSPECIFIED.);
#3091=B_SPLINE_CURVE_WITH_KNOTS('',3,(#150575,#150576,#150577,#150578,#150579,
#150580,#150581,#150582,#150583,#150584,#150585,#150586,#150587,#150588,
#150589,#150590,#150591,#150592,#150593,#150594,#150595,#150596,#150597,
#150598,#150599,#150600,#150601,#150602,#150603,#150604,#150605,#150606,
#150607,#150608,#150609,#150610,#150611,#150612,#150613,#150614,#150615,
#150616,#150617,#150618,#150619,#150620,#150621,#150622,#150623,#150624,
#150625,#150626,#150627,#150628,#150629,#150630,#150631,#150632,#150633,
#150634,#150635,#150636,#150637,#150638,#150639,#150640,#150641,#150642,
#150643,#150644,#150645,#150646,#150647,#150648,#150649,#150650,#150651,
#150652,#150653,#150654,#150655,#150656,#150657,#150658,#150659,#150660,
#150661,#150662,#150663,#150664,#150665,#150666,#150667,#150668,#150669,
#150670,#150671,#150672,#150673,#150674,#150675,#150676,#150677,#150678,
#150679,#150680,#150681,#150682,#150683,#150684,#150685,#150686,#150687,
#150688,#150689,#150690,#150691,#150692,#150693,#150694,#150695,#150696,
#150697,#150698,#150699,#150700,#150701,#150702,#150703,#150704,#150705,
#150706,#150707,#150708,#150709,#150710,#150711,#150712,#150713,#150714,
#150715,#150716,#150717,#150718,#150719,#150720,#150721,#150722,#150723,
#150724,#150725,#150726,#150727,#150728,#150729,#150730,#150731,#150732,
#150733,#150734,#150735,#150736,#150737,#150738,#150739,#150740,#150741,
#150742,#150743,#150744,#150745,#150746,#150747,#150748,#150749,#150750,
#150751,#150752,#150753,#150754,#150755,#150756,#150757,#150758,#150759,
#150760,#150761,#150762,#150763,#150764,#150765,#150766,#150767,#150768,
#150769,#150770,#150771,#150772,#150773,#150774,#150775,#150776,#150777,
#150778,#150779,#150780,#150781,#150782,#150783,#150784,#150785,#150786,
#150787,#150788,#150789,#150790,#150791,#150792,#150793,#150794,#150795,
#150796,#150797,#150798,#150799,#150800,#150801,#150802,#150803,#150804,
#150805,#150806,#150807,#150808,#150809,#150810,#150811,#150812),
 .UNSPECIFIED.,.F.,.F.,(4,3,3,3,3,3,3,3,3,3,3,3,3,3,3,3,3,3,3,3,3,3,3,3,
3,3,3,3,3,3,3,3,3,3,3,3,3,3,3,3,3,3,3,3,3,3,3,3,3,3,3,3,3,3,3,3,3,3,3,3,
3,3,3,3,3,3,3,3,3,3,3,3,3,3,3,3,3,3,3,4),(133.611894774878,133.703844055645,
133.799892579167,133.891713018518,133.983244652198,134.074173849049,134.088038149733,
134.162040064416,134.236020992754,134.309996014661,134.384008487955,134.458039757931,
134.532144510131,134.586506693041,134.665468108988,134.744375532057,134.823240570993,
134.902074801719,134.980889775697,135.059711039357,135.138537678469,135.217380202845,
135.296249131428,135.375191182759,135.454171948247,135.533242959265,135.583443779656,
135.662435675016,135.741327459713,135.820129715778,135.898829716621,135.97746916252,
136.056045444726,136.081912322963,136.160499046081,136.239135213299,136.317831206568,
136.396645238004,136.47552666618,136.554529759348,136.580380866271,136.659453388058,
136.73845294283,136.817391210691,136.89627982521,136.975130381803,137.053958886106,
137.132775260011,137.211590011231,137.290413645245,137.369283692828,137.448177371938,
137.527137896809,137.577317952886,137.651423390933,137.725471888733,137.799478626685,
137.873467890785,137.947445252344,138.021447538325,138.075786496194,138.166785595894,
138.258288813528,138.350232352405,138.442266929528,138.53417601959,138.574255039501,
138.649964711011,138.725625713429,138.801252554159,138.876870250831,138.952481751307,
139.028121676321,139.072723582809,139.154965444528,139.237231094181,139.319536624453,
139.401853127536,139.484193158093,139.539186449088),.UNSPECIFIED.);
#3092=B_SPLINE_CURVE_WITH_KNOTS('',3,(#150813,#150814,#150815,#150816,#150817,
#150818,#150819,#150820,#150821,#150822,#150823,#150824,#150825,#150826,
#150827,#150828),.UNSPECIFIED.,.F.,.F.,(4,3,3,3,3,4),(139.539186449218,
139.571192126116,139.653573056315,139.735937288415,139.818282645486,139.895602067557),
 .UNSPECIFIED.);
#3093=B_SPLINE_CURVE_WITH_KNOTS('',3,(#150830,#150831,#150832,#150833,#150834,
#150835,#150836,#150837,#150838,#150839,#150840,#150841,#150842,#150843,
#150844,#150845),.UNSPECIFIED.,.F.,.F.,(4,3,3,3,3,4),(-136.155837210071,
-136.081912322963,-136.007543160793,-135.933164179611,-135.85872478924,
-135.799946905112),.UNSPECIFIED.);
#3094=B_SPLINE_CURVE_WITH_KNOTS('',3,(#150846,#150847,#150848,#150849,#150850,
#150851,#150852,#150853,#150854,#150855,#150856,#150857,#150858,#150859,
#150860,#150861,#150862,#150863,#150864,#150865,#150866,#150867,#150868,
#150869,#150870,#150871,#150872,#150873,#150874,#150875,#150876,#150877,
#150878,#150879,#150880,#150881,#150882,#150883,#150884,#150885,#150886,
#150887,#150888,#150889,#150890,#150891,#150892,#150893,#150894,#150895,
#150896,#150897,#150898,#150899,#150900,#150901,#150902,#150903,#150904,
#150905,#150906,#150907,#150908,#150909,#150910,#150911,#150912,#150913,
#150914,#150915,#150916,#150917,#150918,#150919,#150920,#150921,#150922,
#150923,#150924,#150925,#150926,#150927,#150928,#150929,#150930,#150931,
#150932,#150933,#150934,#150935,#150936,#150937,#150938,#150939,#150940,
#150941,#150942,#150943,#150944,#150945,#150946,#150947,#150948,#150949,
#150950,#150951,#150952,#150953,#150954,#150955,#150956,#150957,#150958,
#150959,#150960,#150961,#150962,#150963,#150964,#150965,#150966,#150967,
#150968,#150969,#150970,#150971,#150972,#150973,#150974,#150975,#150976,
#150977,#150978,#150979,#150980,#150981,#150982,#150983,#150984,#150985,
#150986,#150987,#150988,#150989,#150990,#150991,#150992,#150993,#150994,
#150995,#150996,#150997,#150998,#150999,#151000,#151001,#151002,#151003,
#151004,#151005,#151006,#151007,#151008,#151009,#151010,#151011,#151012,
#151013,#151014,#151015,#151016,#151017,#151018,#151019,#151020,#151021,
#151022,#151023,#151024,#151025,#151026,#151027,#151028,#151029,#151030,
#151031,#151032,#151033,#151034,#151035,#151036,#151037,#151038,#151039,
#151040,#151041,#151042,#151043,#151044,#151045,#151046,#151047,#151048,
#151049,#151050,#151051,#151052,#151053,#151054,#151055,#151056,#151057,
#151058,#151059,#151060,#151061,#151062,#151063,#151064,#151065,#151066,
#151067,#151068,#151069,#151070,#151071,#151072,#151073,#151074,#151075,
#151076,#151077,#151078,#151079,#151080),.UNSPECIFIED.,.F.,.F.,(4,3,3,3,
3,3,3,3,3,3,3,3,3,3,3,3,3,3,3,3,3,3,3,3,3,3,3,3,3,3,3,3,3,3,3,3,3,3,3,3,
3,3,3,3,3,3,3,3,3,3,3,3,3,3,3,3,3,3,3,3,3,3,3,3,3,3,3,3,3,3,3,3,3,3,3,3,
3,3,4),(-135.799946904982,-135.709593726747,-135.618579632177,-135.583443779656,
-135.504371257906,-135.425371703171,-135.346433435348,-135.267544820866,
-135.18869426431,-135.109865760044,-135.031049386175,-134.952234634992,
-134.873411001014,-134.794540953466,-134.71564727439,-134.636686749553,
-134.586506693041,-134.512401254945,-134.438352757096,-134.364346019095,
-134.290356754948,-134.216379393341,-134.142377107314,-134.088038149733,
-133.997039049987,-133.905535832298,-133.813592293355,-133.721557716163,
-133.629648626029,-133.589569606426,-133.513859935311,-133.438198933289,
-133.362572092954,-133.286954396674,-133.211342896591,-133.135702971966,
-133.091101063118,-133.008822291261,-132.926519728395,-132.843047926249,
-132.760692971348,-132.676662745579,-132.59263251981,-132.51025350921,-132.427889319963,
-132.344457984098,-132.262136010807,-132.178149993655,-132.094163976503,
-132.018523867281,-131.942907764374,-131.867301197319,-131.791666534609,
-131.716016976031,-131.640306686253,-131.595695433195,-131.503794863493,
-131.411761893781,-131.31988232396,-131.228254927932,-131.137233806452,
-131.097226889888,-131.0232249752,-130.949244046856,-130.875269024943,-130.801256551643,
-130.727225281661,-130.653120529456,-130.59875834658,-130.519788908694,
-130.438987933081,-130.360125171892,-130.281291165063,-130.202475388716,
-130.120201817486,-130.041376296381,-129.962540678799,-129.883669978161,
-129.873381103796),.UNSPECIFIED.);
#3095=B_SPLINE_CURVE_WITH_KNOTS('',3,(#151086,#151087,#151088,#151089,#151090,
#151091,#151092,#151093,#151094,#151095,#151096,#151097,#151098,#151099,
#151100,#151101,#151102,#151103,#151104,#151105,#151106,#151107,#151108,
#151109,#151110,#151111,#151112,#151113,#151114,#151115,#151116,#151117,
#151118,#151119,#151120,#151121,#151122,#151123,#151124,#151125,#151126,
#151127,#151128,#151129,#151130,#151131,#151132,#151133,#151134,#151135,
#151136,#151137,#151138,#151139,#151140,#151141,#151142,#151143,#151144,
#151145,#151146,#151147,#151148,#151149,#151150,#151151,#151152,#151153,
#151154,#151155,#151156,#151157,#151158,#151159,#151160,#151161,#151162,
#151163,#151164,#151165,#151166,#151167,#151168,#151169,#151170,#151171,
#151172,#151173,#151174,#151175,#151176,#151177,#151178,#151179,#151180,
#151181,#151182,#151183,#151184,#151185,#151186,#151187,#151188,#151189,
#151190,#151191,#151192,#151193,#151194,#151195,#151196,#151197,#151198,
#151199,#151200,#151201,#151202,#151203,#151204,#151205,#151206,#151207,
#151208,#151209,#151210,#151211,#151212,#151213,#151214,#151215,#151216,
#151217,#151218,#151219,#151220,#151221,#151222,#151223,#151224,#151225,
#151226,#151227,#151228,#151229,#151230,#151231,#151232,#151233,#151234,
#151235,#151236,#151237,#151238,#151239,#151240,#151241,#151242,#151243,
#151244,#151245,#151246,#151247,#151248,#151249,#151250,#151251,#151252,
#151253,#151254,#151255,#151256,#151257,#151258,#151259,#151260,#151261,
#151262,#151263,#151264,#151265,#151266,#151267,#151268,#151269,#151270,
#151271,#151272,#151273,#151274,#151275,#151276,#151277,#151278,#151279,
#151280,#151281,#151282,#151283,#151284,#151285,#151286,#151287,#151288,
#151289,#151290,#151291,#151292,#151293,#151294,#151295,#151296,#151297,
#151298,#151299,#151300,#151301,#151302,#151303,#151304,#151305),
 .UNSPECIFIED.,.F.,.F.,(4,3,3,3,3,3,3,3,3,3,3,3,3,3,3,3,3,3,3,3,3,3,3,3,
3,3,3,3,3,3,3,3,3,3,3,3,3,3,3,3,3,3,3,3,3,3,3,3,3,3,3,3,3,3,3,3,3,3,3,3,
3,3,3,3,3,3,3,3,3,3,3,3,3,4),(127.329030480685,127.410760354451,127.492490108222,
127.574219743663,127.655949262443,127.737678666226,127.819407956681,127.9043547252,
127.987974200461,128.070287121421,128.152026030488,128.233764519875,128.315502596255,
128.397240266302,128.47897753669,128.560714414093,128.642450905183,128.724187016634,
128.805922755116,128.887658127302,128.969393139864,129.051127799473,129.132862112801,
129.214596086517,129.296329727292,129.378063041797,129.459796036702,129.541528718675,
129.623261094387,129.704993170506,129.786724953702,129.868456450642,129.950187667996,
130.031918612431,130.113649290615,130.195379709216,130.277109874901,130.358839794338,
130.440569474193,130.522298921133,130.607727115532,130.690485678857,130.77222430642,
130.853962110224,130.935699116964,131.017435353331,131.099170846017,131.180905621708,
131.262639707089,131.344373128841,131.426105913646,131.507838088182,131.589569679123,
131.671300713144,131.753031216916,131.834761217111,131.916490740395,132.00021014049,
132.081948221518,132.163684716943,132.245419733527,132.327153378016,132.408885757133,
132.490616977586,132.572347146066,132.657803895546,132.739540813765,132.821274822668,
132.903006349188,132.984735820116,133.066470710592,133.148200790757,133.229932219818,
133.256001141908),.UNSPECIFIED.);
#3096=B_SPLINE_CURVE_WITH_KNOTS('',3,(#151306,#151307,#151308,#151309,#151310,
#151311,#151312,#151313,#151314,#151315,#151316,#151317,#151318,#151319,
#151320,#151321,#151322,#151323,#151324),.UNSPECIFIED.,.F.,.F.,(4,3,3,3,
3,3,4),(133.256001141908,133.331495817858,133.407020184361,133.482561554849,
133.558161894196,133.589569606426,133.611894774878),.UNSPECIFIED.);
#3097=B_SPLINE_CURVE_WITH_KNOTS('',3,(#151326,#151327,#151328,#151329,#151330,
#151331,#151332,#151333,#151334,#151335,#151336,#151337,#151338,#151339,
#151340,#151341),.UNSPECIFIED.,.F.,.F.,(4,3,3,3,3,4),(-129.873381103796,
-129.794432154857,-129.715442567629,-129.636366301135,-129.601821259965,
-129.516761597802),.UNSPECIFIED.);
#3098=B_SPLINE_CURVE_WITH_KNOTS('',3,(#151342,#151343,#151344,#151345,#151346,
#151347,#151348,#151349,#151350,#151351,#151352,#151353,#151354,#151355,
#151356,#151357,#151358,#151359,#151360,#151361,#151362,#151363,#151364,
#151365,#151366,#151367,#151368,#151369,#151370,#151371,#151372,#151373,
#151374,#151375,#151376,#151377,#151378,#151379,#151380,#151381,#151382,
#151383,#151384,#151385,#151386,#151387,#151388,#151389,#151390,#151391,
#151392,#151393,#151394,#151395,#151396,#151397,#151398,#151399,#151400,
#151401,#151402,#151403,#151404,#151405,#151406,#151407,#151408,#151409,
#151410,#151411,#151412,#151413,#151414,#151415,#151416,#151417,#151418,
#151419,#151420,#151421,#151422,#151423,#151424,#151425,#151426,#151427,
#151428,#151429,#151430,#151431,#151432,#151433,#151434,#151435,#151436,
#151437,#151438,#151439,#151440,#151441,#151442,#151443,#151444,#151445,
#151446,#151447,#151448,#151449,#151450,#151451,#151452,#151453,#151454,
#151455,#151456,#151457,#151458,#151459,#151460,#151461,#151462,#151463,
#151464,#151465,#151466,#151467,#151468,#151469,#151470,#151471,#151472,
#151473,#151474,#151475,#151476,#151477,#151478,#151479,#151480,#151481,
#151482,#151483,#151484,#151485,#151486,#151487,#151488,#151489,#151490,
#151491,#151492,#151493,#151494,#151495,#151496,#151497,#151498,#151499,
#151500,#151501,#151502,#151503,#151504,#151505,#151506,#151507,#151508,
#151509,#151510,#151511,#151512,#151513,#151514,#151515,#151516,#151517,
#151518,#151519,#151520,#151521,#151522,#151523,#151524,#151525,#151526,
#151527,#151528,#151529,#151530,#151531,#151532,#151533,#151534,#151535,
#151536,#151537,#151538,#151539,#151540,#151541,#151542,#151543,#151544,
#151545,#151546,#151547,#151548,#151549,#151550,#151551,#151552,#151553,
#151554,#151555,#151556,#151557,#151558,#151559,#151560,#151561,#151562,
#151563,#151564,#151565,#151566,#151567,#151568,#151569,#151570,#151571,
#151572,#151573,#151574,#151575,#151576,#151577,#151578,#151579),
 .UNSPECIFIED.,.F.,.F.,(4,3,3,3,3,3,3,3,3,3,3,3,3,3,3,3,3,3,3,3,3,3,3,3,
3,3,3,3,3,3,3,3,3,3,3,3,3,3,3,3,3,3,3,3,3,3,3,3,3,3,3,3,3,3,3,3,3,3,3,3,
3,3,3,3,3,3,3,3,3,3,3,3,3,3,3,3,3,3,3,4),(-129.51676159771,-129.440162129166,
-129.3636436382,-129.287207051255,-129.210817745977,-129.134465961583,-129.103352716657,
-129.024765993494,-128.946129826232,-128.867433832917,-128.788619801435,
-128.709738373212,-128.630735279997,-128.60488417335,-128.5258116516,-128.446812096865,
-128.367873829041,-128.28898521456,-128.210134658003,-128.131306153737,
-128.052489779869,-127.973675028685,-127.894851394707,-127.815981347159,
-127.737087668083,-127.658127143246,-127.607947086735,-127.533841648633,
-127.459793150777,-127.38578641277,-127.311797148617,-127.237819787004,
-127.16381750097,-127.109478543427,-127.018479443693,-126.926976226018,
-126.83503268709,-126.742998109913,-126.651089019794,-126.61101000012,-126.535300329002,
-126.459639326975,-126.384012486637,-126.308394790354,-126.232783290266,
-126.157143365638,-126.112541456812,-126.03026268496,-125.947960122098,
-125.86448831995,-125.782133365053,-125.698103139279,-125.614072913505,
-125.531693902902,-125.449329713651,-125.365898377787,-125.283576404493,
-125.199590387345,-125.115604370197,-125.039964260976,-124.964348158071,
-124.888741591018,-124.813106928309,-124.737457369732,-124.661747079956,
-124.61713582689,-124.525235257187,-124.433202287472,-124.34132271765,-124.24969532162,
-124.158674200137,-124.118667283582,-124.044665368893,-123.970684440549,
-123.896709418635,-123.822696945334,-123.748665675352,-123.674560923147,
-123.620198740274,-123.590150617738),.UNSPECIFIED.);
#3099=B_SPLINE_CURVE_WITH_KNOTS('',3,(#151585,#151586,#151587,#151588,#151589,
#151590,#151591,#151592,#151593,#151594,#151595,#151596,#151597,#151598,
#151599,#151600,#151601,#151602,#151603,#151604,#151605,#151606,#151607,
#151608,#151609,#151610,#151611,#151612,#151613,#151614,#151615,#151616,
#151617,#151618,#151619,#151620,#151621,#151622,#151623,#151624,#151625,
#151626,#151627,#151628,#151629,#151630,#151631,#151632,#151633,#151634,
#151635,#151636,#151637,#151638,#151639,#151640,#151641,#151642,#151643,
#151644,#151645,#151646,#151647,#151648,#151649,#151650,#151651,#151652,
#151653,#151654,#151655,#151656,#151657,#151658,#151659,#151660,#151661,
#151662,#151663,#151664,#151665,#151666,#151667,#151668,#151669,#151670,
#151671,#151672,#151673,#151674,#151675,#151676,#151677,#151678,#151679,
#151680,#151681,#151682,#151683,#151684,#151685,#151686,#151687,#151688,
#151689,#151690,#151691,#151692,#151693,#151694,#151695,#151696,#151697,
#151698,#151699,#151700,#151701,#151702,#151703,#151704,#151705,#151706,
#151707,#151708,#151709,#151710,#151711,#151712,#151713,#151714,#151715,
#151716,#151717,#151718,#151719,#151720,#151721,#151722,#151723,#151724,
#151725,#151726,#151727,#151728,#151729,#151730,#151731,#151732,#151733,
#151734,#151735,#151736,#151737,#151738,#151739,#151740,#151741,#151742,
#151743,#151744,#151745,#151746,#151747,#151748,#151749,#151750,#151751,
#151752,#151753,#151754,#151755,#151756,#151757,#151758,#151759,#151760,
#151761,#151762,#151763,#151764,#151765,#151766,#151767,#151768,#151769,
#151770,#151771,#151772,#151773,#151774,#151775,#151776,#151777,#151778,
#151779,#151780,#151781,#151782,#151783,#151784,#151785,#151786,#151787,
#151788,#151789,#151790,#151791,#151792,#151793,#151794,#151795,#151796,
#151797,#151798,#151799,#151800,#151801,#151802,#151803,#151804,#151805,
#151806,#151807,#151808,#151809,#151810,#151811,#151812,#151813,#151814,
#151815,#151816,#151817,#151818,#151819),.UNSPECIFIED.,.F.,.F.,(4,3,3,3,
3,3,3,3,3,3,3,3,3,3,3,3,3,3,3,3,3,3,3,3,3,3,3,3,3,3,3,3,3,3,3,3,3,3,3,3,
3,3,3,3,3,3,3,3,3,3,3,3,3,3,3,3,3,3,3,3,3,3,3,3,3,3,3,3,3,3,3,3,3,3,3,3,
3,3,4),(121.04580412481,121.123867226472,121.20193141621,121.280008607331,
121.35811071905,121.436284155121,121.51449773961,121.59279954696,121.626324567044,
121.705316462383,121.784208247058,121.863010503103,121.941710503926,122.020349949805,
122.098926231991,122.124793110352,122.203379833515,122.282016000777,122.360711994093,
122.439526025575,122.518407453798,122.597410547013,122.623261653659,122.702334175409,
122.781333730144,122.860271997968,122.939160612449,123.018011169005,123.096839673271,
123.17565604714,123.254470798323,123.333294432301,123.412164479849,123.491058158925,
123.570018683762,123.620198740274,123.694304178376,123.768352676231,123.842359414238,
123.916348678391,123.990326040003,124.064328326036,124.118667283582,124.209666383319,
124.301169600998,124.39311313993,124.48514771711,124.577056807233,124.61713582689,
124.692845498007,124.768506500031,124.844133340368,124.919751036649,124.995362536735,
125.071002461362,125.115604370197,125.197883142052,125.280185704916,125.363657507063,
125.446012461962,125.530042687734,125.614072913505,125.696451924106,125.778816113354,
125.862247449219,125.94456942251,126.028555439661,126.112541456812,126.188181566034,
126.263797668941,126.339404235995,126.415038898706,126.490688457284,126.566398747061,
126.61101000012,126.705396416608,126.799894665305,126.894075848052,126.972815834728),
 .UNSPECIFIED.);
#3100=B_SPLINE_CURVE_WITH_KNOTS('',3,(#151820,#151821,#151822,#151823,#151824,
#151825,#151826,#151827,#151828,#151829,#151830,#151831,#151832,#151833,
#151834,#151835),.UNSPECIFIED.,.F.,.F.,(4,3,3,3,3,4),(126.972815834728,
127.054545378564,127.136280493483,127.218010730832,127.299742519783,127.329030480685),
 .UNSPECIFIED.);
#3101=B_SPLINE_CURVE_WITH_KNOTS('',3,(#151837,#151838,#151839,#151840,#151841,
#151842,#151843,#151844,#151845,#151846,#151847,#151848,#151849),
 .UNSPECIFIED.,.F.,.F.,(4,3,3,3,4),(-123.590150617738,-123.500202190511,
-123.410405737001,-123.321051447307,-123.233576290755),.UNSPECIFIED.);
#3102=B_SPLINE_CURVE_WITH_KNOTS('',3,(#151850,#151851,#151852,#151853,#151854,
#151855,#151856,#151857,#151858,#151859,#151860,#151861,#151862,#151863,
#151864,#151865,#151866,#151867,#151868,#151869,#151870,#151871,#151872,
#151873,#151874,#151875,#151876,#151877,#151878,#151879,#151880,#151881,
#151882,#151883,#151884,#151885,#151886,#151887,#151888,#151889,#151890,
#151891,#151892,#151893,#151894,#151895,#151896,#151897,#151898,#151899,
#151900,#151901,#151902,#151903,#151904,#151905,#151906,#151907,#151908,
#151909,#151910,#151911,#151912,#151913,#151914,#151915,#151916,#151917,
#151918,#151919,#151920,#151921,#151922,#151923,#151924,#151925,#151926,
#151927,#151928,#151929,#151930,#151931,#151932,#151933,#151934,#151935,
#151936,#151937,#151938,#151939,#151940,#151941,#151942,#151943,#151944,
#151945,#151946,#151947,#151948,#151949,#151950,#151951,#151952,#151953,
#151954,#151955,#151956,#151957,#151958,#151959,#151960,#151961,#151962,
#151963,#151964,#151965,#151966,#151967,#151968,#151969,#151970,#151971,
#151972,#151973,#151974,#151975,#151976,#151977,#151978,#151979,#151980,
#151981,#151982,#151983,#151984,#151985,#151986,#151987,#151988,#151989,
#151990,#151991,#151992,#151993,#151994,#151995,#151996,#151997,#151998,
#151999,#152000,#152001,#152002,#152003,#152004,#152005,#152006,#152007,
#152008,#152009,#152010,#152011,#152012,#152013,#152014,#152015,#152016,
#152017,#152018,#152019,#152020,#152021,#152022,#152023,#152024,#152025,
#152026,#152027,#152028,#152029,#152030,#152031,#152032,#152033,#152034,
#152035,#152036,#152037,#152038,#152039,#152040,#152041,#152042,#152043,
#152044,#152045,#152046,#152047,#152048,#152049,#152050,#152051,#152052,
#152053,#152054,#152055,#152056,#152057,#152058,#152059,#152060,#152061,
#152062,#152063,#152064,#152065,#152066,#152067,#152068,#152069,#152070,
#152071,#152072,#152073,#152074,#152075,#152076,#152077,#152078,#152079,
#152080,#152081,#152082,#152083,#152084),.UNSPECIFIED.,.F.,.F.,(4,3,3,3,
3,3,3,3,3,3,3,3,3,3,3,3,3,3,3,3,3,3,3,3,3,3,3,3,3,3,3,3,3,3,3,3,3,3,3,3,
3,3,3,3,3,3,3,3,3,3,3,3,3,3,3,3,3,3,3,3,3,3,3,3,3,3,3,3,3,3,3,3,3,3,3,3,
3,3,4),(-123.233576290623,-123.154340788253,-123.075085132784,-122.99580002089,
-122.916476130551,-122.837062311739,-122.757601429428,-122.678037844198,
-122.623261653659,-122.544269758321,-122.465377973647,-122.386575717604,
-122.307875716783,-122.229236270906,-122.150659988722,-122.124793110352,
-122.046206387188,-121.967570219925,-121.888874226607,-121.810060195124,
-121.731178766899,-121.652175673683,-121.626324567044,-121.547252045294,
-121.46825249056,-121.389314222736,-121.310425608255,-121.231575051698,
-121.152746547433,-121.073930173564,-120.99511542238,-120.916291788403,
-120.837421740854,-120.758528061779,-120.679567536942,-120.629387480429,
-120.555282042327,-120.481233544472,-120.407226806465,-120.333237542312,
-120.259260180699,-120.185257894666,-120.130918937121,-120.039919837387,
-119.948416619712,-119.856473080783,-119.764438503607,-119.672529413488,
-119.632450393814,-119.556740722696,-119.481079720669,-119.40545288033,
-119.329835184047,-119.25422368396,-119.178583759332,-119.133981850506,
-119.051703078654,-118.969400515792,-118.885928713644,-118.803573758747,
-118.719543532973,-118.635513307199,-118.553134296596,-118.470770107346,
-118.387338771482,-118.305016798188,-118.22103078104,-118.137044763891,
-118.06140465467,-117.985788551765,-117.910181984712,-117.834547322003,
-117.758897763426,-117.68318747365,-117.638576220584,-117.54663341521,-117.454600059247,
-117.362706616229,-117.306038383074),.UNSPECIFIED.);
#3103=B_SPLINE_CURVE_WITH_KNOTS('',3,(#152090,#152091,#152092,#152093,#152094,
#152095,#152096,#152097,#152098,#152099,#152100,#152101,#152102,#152103,
#152104,#152105,#152106,#152107,#152108,#152109,#152110,#152111,#152112,
#152113,#152114,#152115,#152116,#152117,#152118,#152119,#152120,#152121,
#152122,#152123,#152124,#152125,#152126,#152127,#152128,#152129,#152130,
#152131,#152132,#152133,#152134,#152135,#152136,#152137,#152138,#152139,
#152140,#152141,#152142,#152143,#152144,#152145,#152146,#152147,#152148,
#152149,#152150,#152151,#152152,#152153,#152154,#152155,#152156,#152157,
#152158,#152159,#152160,#152161,#152162,#152163,#152164,#152165,#152166,
#152167,#152168,#152169,#152170,#152171,#152172,#152173,#152174,#152175,
#152176,#152177,#152178,#152179,#152180,#152181,#152182,#152183,#152184,
#152185,#152186,#152187,#152188,#152189,#152190,#152191,#152192,#152193,
#152194,#152195,#152196,#152197,#152198,#152199,#152200,#152201,#152202,
#152203,#152204,#152205,#152206,#152207,#152208,#152209,#152210,#152211,
#152212,#152213,#152214,#152215,#152216,#152217,#152218,#152219,#152220,
#152221,#152222,#152223,#152224,#152225,#152226,#152227,#152228,#152229,
#152230,#152231,#152232,#152233,#152234,#152235,#152236,#152237,#152238,
#152239,#152240,#152241,#152242,#152243,#152244,#152245,#152246,#152247,
#152248,#152249,#152250,#152251,#152252,#152253,#152254,#152255,#152256,
#152257,#152258,#152259,#152260,#152261,#152262,#152263,#152264,#152265,
#152266,#152267,#152268,#152269,#152270,#152271,#152272,#152273,#152274,
#152275,#152276,#152277,#152278,#152279,#152280,#152281,#152282,#152283,
#152284,#152285,#152286,#152287,#152288,#152289,#152290,#152291,#152292,
#152293,#152294,#152295,#152296,#152297,#152298,#152299,#152300,#152301,
#152302,#152303,#152304,#152305,#152306,#152307,#152308,#152309,#152310,
#152311,#152312,#152313,#152314,#152315,#152316,#152317,#152318,#152319,
#152320,#152321,#152322,#152323,#152324),.UNSPECIFIED.,.F.,.F.,(4,3,3,3,
3,3,3,3,3,3,3,3,3,3,3,3,3,3,3,3,3,3,3,3,3,3,3,3,3,3,3,3,3,3,3,3,3,3,3,3,
3,3,3,3,3,3,3,3,3,3,3,3,3,3,3,3,3,3,3,3,3,3,3,3,3,3,3,3,3,3,3,3,3,3,3,3,
3,3,4),(114.763381035136,114.842229958887,114.920966376191,114.999637094917,
115.078236134955,115.146233504046,115.224820227208,115.30345639447,115.382152387785,
115.460966419266,115.539847847488,115.618850940703,115.644702047353,115.723774569103,
115.802774123839,115.881712391663,115.960601006145,116.039451562701,116.118280066968,
116.197096440837,116.275911192021,116.354734825999,116.433604873548,116.512498552624,
116.591459077462,116.641639133969,116.715744572071,116.789793069925,116.863799807932,
116.937789072085,117.011766433696,117.08576871973,117.140107677276,117.231106777012,
117.32260999469,117.414553533621,117.5065881108,117.598497200922,117.638576220584,
117.714285891701,117.789946893726,117.865573734064,117.941191430345,118.016802930432,
118.092442855059,118.137044763891,118.219323535745,118.301626098609,118.385097900756,
118.467452855655,118.551483081427,118.635513307199,118.7178923178,118.800256507049,
118.883687842913,118.966009816205,119.049995833355,119.133981850506,119.209621959727,
119.285238062634,119.360844629687,119.436479292397,119.512128850974,119.587839140751,
119.632450393814,119.724350963519,119.816383933236,119.90826350306,119.999890899091,
120.090912020574,120.130918937122,120.204920851809,120.278901780151,120.352876802063,
120.426889275362,120.500920545342,120.575025297546,120.629387480429,120.689630527549),
 .UNSPECIFIED.);
#3104=B_SPLINE_CURVE_WITH_KNOTS('',3,(#152325,#152326,#152327,#152328,#152329,
#152330,#152331,#152332,#152333,#152334,#152335,#152336,#152337,#152338,
#152339,#152340),.UNSPECIFIED.,.F.,.F.,(4,3,3,3,3,4),(120.689630527646,
120.767862687141,120.846020793888,120.924135361203,121.002215288158,121.04580412481),
 .UNSPECIFIED.);
#3105=B_SPLINE_CURVE_WITH_KNOTS('',3,(#152342,#152343,#152344,#152345,#152346,
#152347,#152348,#152349,#152350,#152351,#152352,#152353,#152354,#152355,
#152356,#152357),.UNSPECIFIED.,.F.,.F.,(4,3,3,3,3,4),(-117.306038383074,
-117.21490246554,-117.140107677276,-117.069392244814,-116.998691172987,
-116.950390983542),.UNSPECIFIED.);
#3106=B_SPLINE_CURVE_WITH_KNOTS('',3,(#152358,#152359,#152360,#152361,#152362,
#152363,#152364,#152365,#152366,#152367,#152368,#152369,#152370,#152371,
#152372,#152373,#152374,#152375,#152376,#152377,#152378,#152379,#152380,
#152381,#152382,#152383,#152384,#152385,#152386,#152387,#152388,#152389,
#152390,#152391,#152392,#152393,#152394,#152395,#152396,#152397,#152398,
#152399,#152400,#152401,#152402,#152403,#152404,#152405,#152406,#152407,
#152408,#152409,#152410,#152411,#152412,#152413,#152414,#152415,#152416,
#152417,#152418,#152419,#152420,#152421,#152422,#152423,#152424,#152425,
#152426,#152427,#152428,#152429,#152430,#152431,#152432,#152433,#152434,
#152435,#152436,#152437,#152438,#152439,#152440,#152441,#152442,#152443,
#152444,#152445,#152446,#152447,#152448,#152449,#152450,#152451,#152452,
#152453,#152454,#152455,#152456,#152457,#152458,#152459,#152460,#152461,
#152462,#152463,#152464,#152465,#152466,#152467,#152468,#152469,#152470,
#152471,#152472,#152473,#152474,#152475,#152476,#152477,#152478,#152479,
#152480,#152481,#152482,#152483,#152484,#152485,#152486,#152487,#152488,
#152489,#152490,#152491,#152492,#152493,#152494,#152495,#152496,#152497,
#152498,#152499,#152500,#152501,#152502,#152503,#152504,#152505,#152506,
#152507,#152508,#152509,#152510,#152511,#152512,#152513,#152514,#152515,
#152516,#152517,#152518,#152519,#152520,#152521,#152522,#152523,#152524,
#152525,#152526,#152527,#152528,#152529,#152530,#152531,#152532,#152533,
#152534,#152535,#152536,#152537,#152538,#152539,#152540,#152541,#152542,
#152543,#152544,#152545,#152546,#152547,#152548,#152549,#152550,#152551,
#152552,#152553,#152554,#152555,#152556,#152557,#152558,#152559,#152560,
#152561,#152562,#152563,#152564,#152565,#152566,#152567,#152568,#152569,
#152570,#152571,#152572,#152573,#152574,#152575,#152576,#152577,#152578,
#152579,#152580,#152581,#152582,#152583,#152584,#152585,#152586,#152587,
#152588,#152589,#152590,#152591,#152592),.UNSPECIFIED.,.F.,.F.,(4,3,3,3,
3,3,3,3,3,3,3,3,3,3,3,3,3,3,3,3,3,3,3,3,3,3,3,3,3,3,3,3,3,3,3,3,3,3,3,3,
3,3,3,3,3,3,3,3,3,3,3,3,3,3,3,3,3,3,3,3,3,3,3,3,3,3,3,3,3,3,3,3,3,3,3,3,
3,3,4),(-116.950390983443,-116.872431787928,-116.794422690535,-116.716290904427,
-116.641639133969,-116.562677718021,-116.483770294951,-116.404905256013,
-116.326071025286,-116.247256051307,-116.168434787645,-116.089608148532,
-116.010765624155,-115.931896695571,-115.852954644239,-115.773973878749,
-115.69490286773,-115.644702047353,-115.565710152015,-115.486818367341,
-115.408016111297,-115.329316110476,-115.250676664598,-115.172100382413,
-115.146233504046,-115.067646780882,-114.989010613619,-114.910314620303,
-114.831500588819,-114.752619160596,-114.67361606738,-114.647764960738,
-114.568692438988,-114.489692884253,-114.410754616429,-114.331866001947,
-114.253015445391,-114.174186941125,-114.095370567256,-114.016555816072,
-113.937732182094,-113.858862134546,-113.77996845547,-113.701007930633,
-113.650827874123,-113.576722436022,-113.502673938168,-113.428667200161,
-113.354677936009,-113.280700574398,-113.206698288365,-113.152359330816,
-113.061360231079,-112.9698570134,-112.877913474468,-112.785878897287,-112.693969807164,
-112.653890787508,-112.578181116391,-112.502520114366,-112.426893274029,
-112.351275577748,-112.275664077662,-112.200024153035,-112.155422244201,
-112.073143472347,-111.990840909484,-111.907369107336,-111.825014152438,
-111.740983926666,-111.656953700893,-111.57457469029,-111.492210501039,
-111.408779165175,-111.326457191881,-111.242471174733,-111.158485157585,
-111.082886699848,-111.023443944257),.UNSPECIFIED.);
#3107=B_SPLINE_CURVE_WITH_KNOTS('',3,(#152598,#152599,#152600,#152601,#152602,
#152603,#152604,#152605,#152606,#152607,#152608,#152609,#152610,#152611,
#152612,#152613,#152614,#152615,#152616,#152617,#152618,#152619,#152620,
#152621,#152622,#152623,#152624,#152625,#152626,#152627,#152628,#152629,
#152630,#152631,#152632,#152633,#152634,#152635,#152636,#152637,#152638,
#152639,#152640,#152641,#152642,#152643,#152644,#152645,#152646,#152647,
#152648,#152649,#152650,#152651,#152652,#152653,#152654,#152655,#152656,
#152657,#152658,#152659,#152660,#152661,#152662,#152663,#152664,#152665,
#152666,#152667,#152668,#152669,#152670,#152671,#152672,#152673,#152674,
#152675,#152676,#152677,#152678,#152679,#152680,#152681,#152682,#152683,
#152684,#152685,#152686,#152687,#152688,#152689,#152690,#152691,#152692,
#152693,#152694,#152695,#152696,#152697,#152698,#152699,#152700,#152701,
#152702,#152703,#152704,#152705,#152706,#152707,#152708,#152709,#152710,
#152711,#152712,#152713,#152714,#152715,#152716,#152717,#152718,#152719,
#152720,#152721,#152722,#152723,#152724,#152725,#152726,#152727,#152728,
#152729,#152730,#152731,#152732,#152733,#152734,#152735,#152736,#152737,
#152738,#152739,#152740,#152741,#152742,#152743,#152744,#152745,#152746,
#152747,#152748,#152749,#152750,#152751,#152752,#152753,#152754,#152755,
#152756,#152757,#152758,#152759,#152760,#152761,#152762,#152763,#152764,
#152765,#152766,#152767,#152768,#152769,#152770,#152771,#152772,#152773,
#152774,#152775,#152776,#152777,#152778,#152779,#152780,#152781,#152782,
#152783,#152784,#152785,#152786,#152787,#152788,#152789,#152790,#152791,
#152792,#152793,#152794,#152795,#152796,#152797,#152798,#152799,#152800,
#152801,#152802,#152803,#152804,#152805,#152806,#152807,#152808,#152809,
#152810,#152811,#152812,#152813,#152814,#152815,#152816,#152817,#152818,
#152819,#152820,#152821,#152822,#152823,#152824,#152825,#152826,#152827,
#152828,#152829,#152830,#152831,#152832),.UNSPECIFIED.,.F.,.F.,(4,3,3,3,
3,3,3,3,3,3,3,3,3,3,3,3,3,3,3,3,3,3,3,3,3,3,3,3,3,3,3,3,3,3,3,3,3,3,3,3,
3,3,3,3,3,3,3,3,3,3,3,3,3,3,3,3,3,3,3,3,3,3,3,3,3,3,3,3,3,3,3,3,3,3,3,3,
3,3,4),(108.478674260886,108.557552281005,108.636553196501,108.666142441048,
108.745214962797,108.824214517533,108.903152785357,108.982041399838,109.060891956394,
109.13972046066,109.218536834529,109.297351585712,109.376175219689,109.455045267237,
109.533938946313,109.61289947115,109.663079527663,109.737184965764,109.811233463619,
109.885240201625,109.959229465777,110.033206827389,110.107209113421,110.16154807097,
110.252547170709,110.344050388387,110.43599392732,110.5280285045,110.619937594623,
110.660016614278,110.735726285395,110.81138728742,110.887014127756,110.962631824038,
111.038243324123,111.11388324875,111.158485157585,111.240763929439,111.323066492301,
111.406538294449,111.488893249347,111.57292347512,111.656953700893,111.739332711496,
111.821696900748,111.905128236611,111.987450209905,112.071436227053,112.155422244201,
112.231062353421,112.306678456326,112.382285023379,112.457919686087,112.533569244663,
112.609279534439,112.653890787508,112.745791357214,112.837824326931,112.929703896756,
113.021331292787,113.112352414271,113.152359330816,113.226361245503,113.300342173846,
113.374317195758,113.448329669058,113.522360939038,113.596465691242,113.650827874123,
113.72907653155,113.80726520934,113.885402422488,113.96351040033,114.041600985793,
114.119686009305,114.197799010695,114.275925669416,114.354107310553,114.406445220369),
 .UNSPECIFIED.);
#3108=B_SPLINE_CURVE_WITH_KNOTS('',3,(#152833,#152834,#152835,#152836,#152837,
#152838,#152839,#152840,#152841,#152842,#152843,#152844,#152845,#152846,
#152847,#152848),.UNSPECIFIED.,.F.,.F.,(4,3,3,3,3,4),(114.406445220461,
114.508021462892,114.611348359269,114.647764960738,114.726761857662,114.763381035136),
 .UNSPECIFIED.);
#3109=B_SPLINE_CURVE_WITH_KNOTS('',3,(#152850,#152851,#152852,#152853,#152854,
#152855,#152856,#152857,#152858,#152859,#152860,#152861,#152862,#152863,
#152864,#152865),.UNSPECIFIED.,.F.,.F.,(4,3,3,3,3,4),(-111.023443944257,
-110.947879173554,-110.872289747824,-110.796688202473,-110.721026482249,
-110.667205676354),.UNSPECIFIED.);
#3110=B_SPLINE_CURVE_WITH_KNOTS('',3,(#152866,#152867,#152868,#152869,#152870,
#152871,#152872,#152873,#152874,#152875,#152876,#152877,#152878,#152879,
#152880,#152881,#152882,#152883,#152884,#152885,#152886,#152887,#152888,
#152889,#152890,#152891,#152892,#152893,#152894,#152895,#152896,#152897,
#152898,#152899,#152900,#152901,#152902,#152903,#152904,#152905,#152906,
#152907,#152908,#152909,#152910,#152911,#152912,#152913,#152914,#152915,
#152916,#152917,#152918,#152919,#152920,#152921,#152922,#152923,#152924,
#152925,#152926,#152927,#152928,#152929,#152930,#152931,#152932,#152933,
#152934,#152935,#152936,#152937,#152938,#152939,#152940,#152941,#152942,
#152943,#152944,#152945,#152946,#152947,#152948,#152949,#152950,#152951,
#152952,#152953,#152954,#152955,#152956,#152957,#152958,#152959,#152960,
#152961,#152962,#152963,#152964,#152965,#152966,#152967,#152968,#152969,
#152970,#152971,#152972,#152973,#152974,#152975,#152976,#152977,#152978,
#152979,#152980,#152981,#152982,#152983,#152984,#152985,#152986,#152987,
#152988,#152989,#152990,#152991,#152992,#152993,#152994,#152995,#152996,
#152997,#152998,#152999,#153000,#153001,#153002,#153003,#153004,#153005,
#153006,#153007,#153008,#153009,#153010,#153011,#153012,#153013,#153014,
#153015,#153016,#153017,#153018,#153019,#153020,#153021,#153022,#153023,
#153024,#153025,#153026,#153027,#153028,#153029,#153030,#153031,#153032,
#153033,#153034,#153035,#153036,#153037,#153038,#153039,#153040,#153041,
#153042,#153043,#153044,#153045,#153046,#153047,#153048,#153049,#153050,
#153051,#153052,#153053,#153054,#153055,#153056,#153057,#153058,#153059,
#153060,#153061,#153062,#153063,#153064,#153065,#153066,#153067,#153068,
#153069,#153070,#153071,#153072,#153073,#153074,#153075,#153076,#153077,
#153078,#153079,#153080,#153081,#153082,#153083,#153084,#153085,#153086,
#153087,#153088,#153089,#153090,#153091,#153092,#153093,#153094,#153095,
#153096,#153097,#153098,#153099,#153100,#153101,#153102,#153103,#153104,
#153105,#153106),.UNSPECIFIED.,.F.,.F.,(4,3,3,3,3,3,3,3,3,3,3,3,3,3,3,3,
3,3,3,3,3,3,3,3,3,3,3,3,3,3,3,3,3,3,3,3,3,3,3,3,3,3,3,3,3,3,3,3,3,3,3,3,
3,3,3,3,3,3,3,3,3,3,3,3,3,3,3,3,3,3,3,3,3,3,3,3,3,3,3,3,4),(-110.667205676264,
-110.660016614278,-110.568116044574,-110.476083074859,-110.384203505036,
-110.292576109006,-110.201554987524,-110.16154807097,-110.087546156283,
-110.01356522794,-109.939590206028,-109.865577732729,-109.791546462748,
-109.717441710544,-109.663079527663,-109.584118111716,-109.505210688647,
-109.42634564971,-109.347511418984,-109.268696445006,-109.189875181345,
-109.111048542233,-109.032206017857,-108.953337089274,-108.874395037942,
-108.795414272454,-108.716343261435,-108.666142441048,-108.587150545709,
-108.508258761033,-108.429456504988,-108.350756504166,-108.272117058286,
-108.1935407761,-108.16767389774,-108.089087174578,-108.010451007316,-107.931755014,
-107.852940982519,-107.774059554296,-107.695056461082,-107.669205354433,
-107.590132832683,-107.511133277947,-107.432195010123,-107.353306395641,
-107.274455839085,-107.195627334818,-107.116810960949,-107.037996209765,
-106.959172575787,-106.880302528238,-106.801408849162,-106.722448324325,
-106.672268267817,-106.598162829715,-106.524114331861,-106.450107593854,
-106.376118329702,-106.30214096809,-106.228138682057,-106.17379972451,-106.082800624774,
-105.991297407096,-105.899353868165,-105.807319290985,-105.715410200864,
-105.675331181202,-105.599621510085,-105.523960508059,-105.448333667722,
-105.37271597144,-105.297104471354,-105.221464546727,-105.176862637895,
-105.094588492349,-105.012289926871,-104.929953560671,-104.847605501347,
-104.765237375343,-104.740291169727),.UNSPECIFIED.);
#3111=B_SPLINE_CURVE_WITH_KNOTS('',3,(#153112,#153113,#153114,#153115,#153116,
#153117,#153118,#153119,#153120,#153121,#153122,#153123,#153124,#153125,
#153126,#153127,#153128,#153129,#153130,#153131,#153132,#153133,#153134,
#153135,#153136,#153137,#153138,#153139,#153140,#153141,#153142,#153143,
#153144,#153145,#153146,#153147,#153148,#153149,#153150,#153151,#153152,
#153153,#153154,#153155,#153156,#153157,#153158,#153159,#153160,#153161,
#153162,#153163,#153164,#153165,#153166,#153167,#153168,#153169,#153170,
#153171,#153172,#153173,#153174,#153175,#153176,#153177,#153178,#153179,
#153180,#153181,#153182,#153183,#153184,#153185,#153186,#153187,#153188,
#153189,#153190,#153191,#153192,#153193,#153194,#153195,#153196,#153197,
#153198,#153199,#153200,#153201,#153202,#153203,#153204,#153205,#153206,
#153207,#153208,#153209,#153210,#153211,#153212,#153213,#153214,#153215,
#153216,#153217,#153218,#153219,#153220,#153221,#153222,#153223,#153224,
#153225,#153226,#153227,#153228,#153229,#153230,#153231,#153232,#153233,
#153234,#153235,#153236,#153237,#153238,#153239,#153240,#153241,#153242,
#153243,#153244,#153245,#153246,#153247,#153248,#153249,#153250,#153251,
#153252,#153253,#153254,#153255,#153256,#153257,#153258,#153259,#153260,
#153261,#153262,#153263,#153264,#153265,#153266,#153267,#153268,#153269,
#153270,#153271,#153272,#153273,#153274,#153275,#153276,#153277,#153278,
#153279,#153280,#153281,#153282,#153283,#153284,#153285,#153286,#153287,
#153288,#153289,#153290,#153291,#153292,#153293,#153294,#153295,#153296,
#153297,#153298,#153299,#153300,#153301,#153302,#153303,#153304,#153305,
#153306,#153307,#153308,#153309,#153310,#153311,#153312,#153313,#153314,
#153315,#153316,#153317,#153318,#153319,#153320,#153321,#153322,#153323,
#153324,#153325,#153326,#153327,#153328,#153329,#153330,#153331,#153332,
#153333,#153334,#153335,#153336,#153337,#153338,#153339,#153340,#153341,
#153342,#153343,#153344,#153345,#153346),.UNSPECIFIED.,.F.,.F.,(4,3,3,3,
3,3,3,3,3,3,3,3,3,3,3,3,3,3,3,3,3,3,3,3,3,3,3,3,3,3,3,3,3,3,3,3,3,3,3,3,
3,3,3,3,3,3,3,3,3,3,3,3,3,3,3,3,3,3,3,3,3,3,3,3,3,3,3,3,3,3,3,3,3,3,3,3,
3,3,4),(102.196903430706,102.274689906697,102.352474506175,102.430269534311,
102.508113205017,102.585985365738,102.663924460471,102.684519921357,102.758625359459,
102.832673857315,102.906680595322,102.980669859475,103.054647221088,103.128649507121,
103.182988464665,103.273987564398,103.365490782074,103.457434321002,103.549468898179,
103.641377988298,103.681457007972,103.75716667909,103.832827681117,103.908454521455,
103.984072217738,104.059683717825,104.135323642454,104.17992555128,104.262204323132,
104.344506885994,104.427978688142,104.510333643039,104.594363868813,104.678394094587,
104.76077310519,104.84313729444,104.926568630304,105.008890603598,105.092876620746,
105.176862637895,105.252502747116,105.328118850021,105.403725417074,105.479360079783,
105.55500963836,105.630719928136,105.675331181202,105.767231750907,105.859264720624,
105.951144290448,106.042771686478,106.133792807961,106.17379972451,106.247801639198,
106.32178256754,106.395757589452,106.469770062751,106.543801332732,106.617906084937,
106.672268267817,106.751229683765,106.830137106834,106.909002145771,106.987836376498,
107.066651350477,107.145472614138,107.224299253251,107.303141777627,107.382010706211,
107.460952757542,107.539933523032,107.61900453405,107.669205354433,107.749104703786,
107.82889315808,107.908540526475,107.988104779652,108.06756570541,108.123259913073),
 .UNSPECIFIED.);
#3112=B_SPLINE_CURVE_WITH_KNOTS('',3,(#153347,#153348,#153349,#153350,#153351,
#153352,#153353,#153354,#153355,#153356,#153357,#153358,#153359,#153360,
#153361,#153362),.UNSPECIFIED.,.F.,.F.,(4,3,3,3,3,4),(108.12325991319,108.16767389774,
108.24627820679,108.324921018778,108.403664244961,108.478674260886),
 .UNSPECIFIED.);
#3113=B_SPLINE_CURVE_WITH_KNOTS('',3,(#153364,#153365,#153366,#153367,#153368,
#153369,#153370,#153371,#153372,#153373,#153374,#153375,#153376,#153377,
#153378,#153379),.UNSPECIFIED.,.F.,.F.,(4,3,3,3,3,4),(-104.740291169727,
-104.678394094587,-104.596765179296,-104.515154181363,-104.433558031947,
-104.384020369084),.UNSPECIFIED.);
#3114=B_SPLINE_CURVE_WITH_KNOTS('',3,(#153380,#153381,#153382,#153383,#153384,
#153385,#153386,#153387,#153388,#153389,#153390,#153391,#153392,#153393,
#153394,#153395,#153396,#153397,#153398,#153399,#153400,#153401,#153402,
#153403,#153404,#153405,#153406,#153407,#153408,#153409,#153410,#153411,
#153412,#153413,#153414,#153415,#153416,#153417,#153418,#153419,#153420,
#153421,#153422,#153423,#153424,#153425,#153426,#153427,#153428,#153429,
#153430,#153431,#153432,#153433,#153434,#153435,#153436,#153437,#153438,
#153439,#153440,#153441,#153442,#153443,#153444,#153445,#153446,#153447,
#153448,#153449,#153450,#153451,#153452,#153453,#153454,#153455,#153456,
#153457,#153458,#153459,#153460,#153461,#153462,#153463,#153464,#153465,
#153466,#153467,#153468,#153469,#153470,#153471,#153472,#153473,#153474,
#153475,#153476,#153477,#153478,#153479,#153480,#153481,#153482,#153483,
#153484,#153485,#153486,#153487,#153488,#153489,#153490,#153491,#153492,
#153493,#153494,#153495,#153496,#153497,#153498,#153499,#153500,#153501,
#153502,#153503,#153504,#153505,#153506,#153507,#153508,#153509,#153510,
#153511,#153512,#153513,#153514,#153515,#153516,#153517,#153518,#153519,
#153520,#153521,#153522,#153523,#153524,#153525,#153526,#153527,#153528,
#153529,#153530,#153531,#153532,#153533,#153534,#153535,#153536,#153537,
#153538,#153539,#153540,#153541,#153542,#153543,#153544,#153545,#153546,
#153547,#153548,#153549,#153550,#153551,#153552,#153553,#153554,#153555,
#153556,#153557,#153558,#153559,#153560,#153561,#153562,#153563,#153564,
#153565,#153566,#153567,#153568,#153569,#153570,#153571,#153572,#153573,
#153574,#153575,#153576,#153577,#153578,#153579,#153580,#153581,#153582,
#153583,#153584,#153585,#153586,#153587,#153588,#153589,#153590,#153591,
#153592,#153593,#153594,#153595,#153596,#153597,#153598,#153599,#153600,
#153601,#153602,#153603,#153604,#153605,#153606,#153607,#153608,#153609,
#153610,#153611,#153612,#153613,#153614,#153615,#153616,#153617,#153618,
#153619,#153620),.UNSPECIFIED.,.F.,.F.,(4,3,3,3,3,3,3,3,3,3,3,3,3,3,3,3,
3,3,3,3,3,3,3,3,3,3,3,3,3,3,3,3,3,3,3,3,3,3,3,3,3,3,3,3,3,3,3,3,3,3,3,3,
3,3,3,3,3,3,3,3,3,3,3,3,3,3,3,3,3,3,3,3,3,3,3,3,3,3,3,3,4),(-104.38402036896,
-104.297747267439,-104.211526193072,-104.17992555128,-104.104285442056,
-104.028669339147,-103.953062772091,-103.877428109379,-103.801778550799,
-103.72606826102,-103.681457007972,-103.589556438273,-103.497523468563,
-103.405643898744,-103.314016502719,-103.222995381241,-103.182988464665,
-103.108986549976,-103.035005621632,-102.961030599719,-102.887018126419,
-102.812986856437,-102.738882104231,-102.684519921357,-102.60555850541,
-102.526651082341,-102.447786043404,-102.368951812678,-102.290136838699,
-102.211315575039,-102.132488935927,-102.05364641155,-101.974777482967,
-101.895835431636,-101.816854666147,-101.737783655129,-101.687582834742,
-101.608590939403,-101.529699154728,-101.450896898683,-101.372196897862,
-101.293557451984,-101.214981169798,-101.189114291434,-101.110527568271,
-101.031891401009,-100.953195407692,-100.87438137621,-100.795499947987,
-100.716496854772,-100.690645748127,-100.611573226377,-100.532573671642,
-100.453635403818,-100.374746789337,-100.29589623278,-100.217067728515,
-100.138251354646,-100.059436603462,-99.9806129694843,-99.9017429219359,
-99.8228492428599,-99.7438887180229,-99.6937086615116,-99.6196032234094,
-99.5455547255546,-99.4715479875472,-99.3975587233941,-99.323581361782,
-99.2495790757487,-99.195240118204,-99.1042410184677,-99.0127378007954,
-98.9207942618662,-98.8287596846874,-98.7368505945678,-98.6967715748965,
-98.6210612370815,-98.5453977770355,-98.469770943029,-98.4567671119247),
 .UNSPECIFIED.);
#3115=B_SPLINE_CURVE_WITH_KNOTS('',3,(#153626,#153627,#153628,#153629,#153630,
#153631,#153632,#153633,#153634,#153635,#153636,#153637,#153638,#153639,
#153640,#153641,#153642,#153643,#153644,#153645,#153646,#153647,#153648,
#153649,#153650,#153651,#153652,#153653,#153654,#153655,#153656,#153657,
#153658,#153659,#153660,#153661,#153662,#153663,#153664,#153665,#153666,
#153667,#153668,#153669,#153670,#153671,#153672,#153673,#153674,#153675,
#153676,#153677,#153678,#153679,#153680,#153681,#153682,#153683,#153684,
#153685,#153686,#153687,#153688,#153689,#153690,#153691,#153692,#153693,
#153694,#153695,#153696,#153697,#153698,#153699,#153700,#153701,#153702,
#153703,#153704,#153705,#153706,#153707,#153708,#153709,#153710,#153711,
#153712,#153713,#153714,#153715,#153716,#153717,#153718,#153719,#153720,
#153721,#153722,#153723,#153724,#153725,#153726,#153727,#153728,#153729,
#153730,#153731,#153732,#153733,#153734,#153735,#153736,#153737,#153738,
#153739,#153740,#153741,#153742,#153743,#153744,#153745,#153746,#153747,
#153748,#153749,#153750,#153751,#153752,#153753,#153754,#153755,#153756,
#153757,#153758,#153759,#153760,#153761,#153762,#153763,#153764,#153765,
#153766,#153767,#153768,#153769,#153770,#153771,#153772,#153773,#153774,
#153775,#153776,#153777,#153778,#153779,#153780,#153781,#153782,#153783,
#153784,#153785,#153786,#153787,#153788,#153789,#153790,#153791,#153792,
#153793,#153794,#153795,#153796,#153797,#153798,#153799,#153800,#153801,
#153802,#153803,#153804,#153805,#153806,#153807,#153808,#153809,#153810,
#153811,#153812,#153813,#153814,#153815,#153816,#153817,#153818,#153819,
#153820,#153821,#153822,#153823,#153824,#153825,#153826,#153827,#153828,
#153829,#153830,#153831,#153832,#153833,#153834,#153835,#153836,#153837,
#153838,#153839,#153840,#153841,#153842,#153843,#153844,#153845,#153846,
#153847,#153848,#153849,#153850,#153851,#153852,#153853,#153854,#153855,
#153856,#153857,#153858,#153859,#153860),.UNSPECIFIED.,.F.,.F.,(4,3,3,3,
3,3,3,3,3,3,3,3,3,3,3,3,3,3,3,3,3,3,3,3,3,3,3,3,3,3,3,3,3,3,3,3,3,3,3,3,
3,3,3,3,3,3,3,3,3,3,3,3,3,3,3,3,3,3,3,3,3,3,3,3,3,3,3,3,3,3,3,3,3,3,3,3,
3,3,4),(95.9134562041998,95.9874494352425,96.0614280794984,96.1354322403172,
96.2044288583587,96.2954279580946,96.3869311757722,96.4788747147027,96.5709092918821,
96.6628183820036,96.7028974016663,96.7786070727838,96.8542680748096,96.9298949151471,
97.0055126114294,97.0811241115159,97.1567640361435,97.2013659449738,97.2836447168271,
97.3659472796899,97.4494190818378,97.5317740367358,97.6158042625086,97.6998344882814,
97.7822134988835,97.8645776881333,97.9480090239972,98.0303309972902,98.1143170144396,
98.198303031589,98.2739431408102,98.3495592437161,98.4251658107696,98.5008004734788,
98.5764500320564,98.6521603218331,98.6967715748965,98.7886721445999,98.8807051143141,
98.9725846841366,99.0642120801662,99.1552332016479,99.1952401182041,99.269242032892,
99.3432229612353,99.4171979831476,99.4912104564474,99.5652417264285,99.6393464786333,
99.6937086615116,99.772670077459,99.8515775005284,99.9304425394651,100.009276770191,
100.08809174417,100.16691300783,100.245739646943,100.324582171319,100.403451099902,
100.482393151234,100.561373916723,100.640444927741,100.690645748127,100.769637643465,
100.848529428139,100.927331684183,101.006031685004,101.084671130883,101.163247413067,
101.189114291434,101.267701014598,101.346337181861,101.425033175179,101.503847206662,
101.582728634886,101.661731728102,101.687582834742,101.820615347273,101.84007460601),
 .UNSPECIFIED.);
#3116=B_SPLINE_CURVE_WITH_KNOTS('',3,(#153861,#153862,#153863,#153864,#153865,
#153866,#153867,#153868,#153869,#153870,#153871,#153872,#153873,#153874,
#153875,#153876),.UNSPECIFIED.,.F.,.F.,(4,3,3,3,3,4),(101.840074606096,
101.918052868575,101.995951121691,102.073802611243,102.151615518596,102.196903430706),
 .UNSPECIFIED.);
#3117=B_SPLINE_CURVE_WITH_KNOTS('',3,(#153878,#153879,#153880,#153881,#153882,
#153883,#153884,#153885,#153886,#153887,#153888,#153889,#153890,#153891,
#153892,#153893,#153894,#153895,#153896),.UNSPECIFIED.,.F.,.F.,(4,3,3,3,
3,3,4),(-98.4567671119247,-98.3811514041528,-98.3055396637728,-98.2298999732549,
-98.1983030315889,-98.1072700840541,-98.1008350619045),.UNSPECIFIED.);
#3118=B_SPLINE_CURVE_WITH_KNOTS('',3,(#153897,#153898,#153899,#153900,#153901,
#153902,#153903,#153904,#153905,#153906,#153907,#153908,#153909,#153910,
#153911,#153912,#153913,#153914,#153915,#153916,#153917,#153918,#153919,
#153920,#153921,#153922,#153923,#153924,#153925,#153926,#153927,#153928,
#153929,#153930,#153931,#153932,#153933,#153934,#153935,#153936,#153937,
#153938,#153939,#153940,#153941,#153942,#153943,#153944,#153945,#153946,
#153947,#153948,#153949,#153950,#153951,#153952,#153953,#153954,#153955,
#153956,#153957,#153958,#153959,#153960,#153961,#153962,#153963,#153964,
#153965,#153966,#153967,#153968,#153969,#153970,#153971,#153972,#153973,
#153974,#153975,#153976,#153977,#153978,#153979,#153980,#153981,#153982,
#153983,#153984,#153985,#153986,#153987,#153988,#153989,#153990,#153991,
#153992,#153993,#153994,#153995,#153996,#153997,#153998,#153999,#154000,
#154001,#154002,#154003,#154004,#154005,#154006,#154007,#154008,#154009,
#154010,#154011,#154012,#154013,#154014,#154015,#154016,#154017,#154018,
#154019,#154020,#154021,#154022,#154023,#154024,#154025,#154026,#154027,
#154028,#154029,#154030,#154031,#154032,#154033,#154034,#154035,#154036,
#154037,#154038,#154039,#154040,#154041,#154042,#154043,#154044,#154045,
#154046,#154047,#154048,#154049,#154050,#154051,#154052,#154053,#154054,
#154055,#154056,#154057,#154058,#154059,#154060,#154061,#154062,#154063,
#154064,#154065,#154066,#154067,#154068,#154069,#154070,#154071,#154072,
#154073,#154074,#154075,#154076,#154077,#154078,#154079,#154080,#154081,
#154082,#154083,#154084,#154085,#154086,#154087,#154088,#154089,#154090,
#154091,#154092,#154093,#154094,#154095,#154096,#154097,#154098,#154099,
#154100,#154101,#154102,#154103,#154104,#154105,#154106,#154107,#154108,
#154109,#154110,#154111,#154112,#154113,#154114,#154115,#154116,#154117,
#154118,#154119,#154120,#154121,#154122,#154123,#154124,#154125,#154126,
#154127,#154128,#154129,#154130,#154131,#154132,#154133,#154134),
 .UNSPECIFIED.,.F.,.F.,(4,3,3,3,3,3,3,3,3,3,3,3,3,3,3,3,3,3,3,3,3,3,3,3,
3,3,3,3,3,3,3,3,3,3,3,3,3,3,3,3,3,3,3,3,3,3,3,3,3,3,3,3,3,3,3,3,3,3,3,3,
3,3,3,3,3,3,3,3,3,3,3,3,3,3,3,3,3,3,3,4),(-98.1008350618282,-98.0193723107643,
-97.9378849353233,-97.8563932604577,-97.7748767781644,-97.6998344882814,
-97.6174554776792,-97.5350912884297,-97.4516599525657,-97.3693379792726,
-97.2853519621232,-97.2013659449738,-97.1257258357525,-97.0501097328464,
-96.9745031657927,-96.8988685030833,-96.8232189445056,-96.7475086547288,
-96.7028974016662,-96.6109968319633,-96.5189638622495,-96.4270842924274,
-96.3354568963981,-96.2444357749168,-96.2044288583587,-96.1304269436705,
-96.0564460153271,-95.9824709934147,-95.9084585201146,-95.8344272501333,
-95.7603224979283,-95.7059603150511,-95.6269988991039,-95.5480914760347,
-95.4692264370982,-95.3903922063724,-95.3115772323937,-95.2327559687335,
-95.1539293296212,-95.0750868052449,-94.9962178766622,-94.9172758253308,
-94.838295059842,-94.7592240488239,-94.709023228436,-94.6300313330974,-94.5511395484225,
-94.4723372923782,-94.3936372915567,-94.314997845678,-94.2364215634927,
-94.2105546851284,-94.1319679619649,-94.053331794702,-93.9746358013858,
-93.895821769903,-93.8169403416795,-93.7379372484637,-93.7120861418209,
-93.6330136200713,-93.5540140653362,-93.4750757975122,-93.3961871830309,
-93.3173366264747,-93.238508122209,-93.1596917483401,-93.0808769971564,
-93.0020533631788,-92.9231833156305,-92.8442896365547,-92.7653291117177,
-92.7151490552058,-92.6410436171038,-92.5669951192492,-92.4929883812423,
-92.4189991170896,-92.3450217554775,-92.2710194694443,-92.2166805118982,
-92.1745156025595),.UNSPECIFIED.);
#3119=B_SPLINE_CURVE_WITH_KNOTS('',3,(#154140,#154141,#154142,#154143,#154144,
#154145,#154146,#154147,#154148,#154149,#154150,#154151,#154152,#154153,
#154154,#154155,#154156,#154157,#154158,#154159,#154160,#154161,#154162,
#154163,#154164,#154165,#154166,#154167,#154168,#154169,#154170,#154171,
#154172,#154173,#154174,#154175,#154176,#154177,#154178,#154179,#154180,
#154181,#154182,#154183,#154184,#154185,#154186,#154187,#154188,#154189,
#154190,#154191,#154192,#154193,#154194,#154195,#154196,#154197,#154198,
#154199,#154200,#154201,#154202,#154203,#154204,#154205,#154206,#154207,
#154208,#154209,#154210,#154211,#154212,#154213,#154214,#154215,#154216,
#154217,#154218,#154219,#154220,#154221,#154222,#154223,#154224,#154225,
#154226,#154227,#154228,#154229,#154230,#154231,#154232,#154233,#154234,
#154235,#154236,#154237,#154238,#154239,#154240,#154241,#154242,#154243,
#154244,#154245,#154246,#154247,#154248,#154249,#154250,#154251,#154252,
#154253,#154254,#154255,#154256,#154257,#154258,#154259,#154260,#154261,
#154262,#154263,#154264,#154265,#154266,#154267,#154268,#154269,#154270,
#154271,#154272,#154273,#154274,#154275,#154276,#154277,#154278,#154279,
#154280,#154281,#154282,#154283,#154284,#154285,#154286,#154287,#154288,
#154289,#154290,#154291,#154292,#154293,#154294,#154295,#154296,#154297,
#154298,#154299,#154300,#154301,#154302,#154303,#154304,#154305,#154306,
#154307,#154308,#154309,#154310,#154311,#154312,#154313,#154314,#154315,
#154316,#154317,#154318,#154319,#154320,#154321,#154322,#154323,#154324,
#154325,#154326,#154327,#154328,#154329,#154330,#154331,#154332,#154333,
#154334,#154335,#154336,#154337,#154338,#154339,#154340,#154341,#154342,
#154343,#154344,#154345,#154346,#154347,#154348,#154349,#154350,#154351,
#154352,#154353,#154354,#154355,#154356,#154357,#154358,#154359,#154360,
#154361,#154362,#154363,#154364,#154365,#154366,#154367,#154368,#154369,
#154370,#154371,#154372,#154373,#154374),.UNSPECIFIED.,.F.,.F.,(4,3,3,3,
3,3,3,3,3,3,3,3,3,3,3,3,3,3,3,3,3,3,3,3,3,3,3,3,3,3,3,3,3,3,3,3,3,3,3,3,
3,3,3,3,3,3,3,3,3,3,3,3,3,3,3,3,3,3,3,3,3,3,3,3,3,3,3,3,3,3,3,3,3,3,3,3,
3,3,4),(89.6300395101817,89.7243377953605,89.8000474664779,89.8757084685036,
89.9513353088409,90.0269530051231,90.1025645052098,90.1782044298374,90.222806338668,
90.3050851105214,90.3873876733842,90.4708594755321,90.5532144304302,90.6372446562029,
90.7212748819756,90.8036538925775,90.8860180818271,90.9694494176911,91.0517713909838,
91.1357574081335,91.2197434252831,91.2953835345044,91.3709996374104,91.4466062044641,
91.5222408671736,91.5978904257513,91.6736007155281,91.7182119685907,91.8101125382937,
91.9021455080077,91.9940250778299,92.0856524738591,92.1766735953405,92.2166805118982,
92.2906824265863,92.3646633549297,92.4386383768422,92.5126508501422,92.5866821201235,
92.6607868723284,92.7151490552058,92.794110471153,92.8730178942222,92.9518829331587,
93.0307171638846,93.1095321378633,93.1883534015235,93.2671800406358,93.3460225650122,
93.424891493595,93.5038335449265,93.5828143104152,93.6618853214333,93.7120861418209,
93.7910780371595,93.8699698218343,93.9487720778786,94.0274720787001,94.1061115245789,
94.1846878067641,94.2105546851285,94.289141408292,94.3677775755548,94.4464735688713,
94.525287600354,94.6041690285776,94.6831721217933,94.709023228436,94.786765196696,
94.8644314260667,94.9420360592962,95.0195897015247,95.0971148667966,95.1746242892932,
95.2521306918767,95.3296741511598,95.4072349269498,95.4848662150954,95.5568892987335),
 .UNSPECIFIED.);
#3120=B_SPLINE_CURVE_WITH_KNOTS('',3,(#154375,#154376,#154377,#154378,#154379,
#154380,#154381,#154382,#154383,#154384,#154385,#154386,#154387),
 .UNSPECIFIED.,.F.,.F.,(4,3,3,3,4),(95.5568892988304,95.7059603150512,95.7800702622623,
95.8541168037861,95.9134562041998),.UNSPECIFIED.);
#3121=B_SPLINE_CURVE_WITH_KNOTS('',3,(#154389,#154390,#154391,#154392,#154393,
#154394,#154395,#154396,#154397,#154398,#154399,#154400,#154401),
 .UNSPECIFIED.,.F.,.F.,(4,3,3,3,4),(-92.1745156025595,-92.0851629640592,
-91.9955575606049,-91.9057144617474,-91.817649754849),.UNSPECIFIED.);
#3122=B_SPLINE_CURVE_WITH_KNOTS('',3,(#154402,#154403,#154404,#154405,#154406,
#154407,#154408,#154409,#154410,#154411,#154412,#154413,#154414,#154415,
#154416,#154417,#154418,#154419,#154420,#154421,#154422,#154423,#154424,
#154425,#154426,#154427,#154428,#154429,#154430,#154431,#154432,#154433,
#154434,#154435,#154436,#154437,#154438,#154439,#154440,#154441,#154442,
#154443,#154444,#154445,#154446,#154447,#154448,#154449,#154450,#154451,
#154452,#154453,#154454,#154455,#154456,#154457,#154458,#154459,#154460,
#154461,#154462,#154463,#154464,#154465,#154466,#154467,#154468,#154469,
#154470,#154471,#154472,#154473,#154474,#154475,#154476,#154477,#154478,
#154479,#154480,#154481,#154482,#154483,#154484,#154485,#154486,#154487,
#154488,#154489,#154490,#154491,#154492,#154493,#154494,#154495,#154496,
#154497,#154498,#154499,#154500,#154501,#154502,#154503,#154504,#154505,
#154506,#154507,#154508,#154509,#154510,#154511,#154512,#154513,#154514,
#154515,#154516,#154517,#154518,#154519,#154520,#154521,#154522,#154523,
#154524,#154525,#154526,#154527,#154528,#154529,#154530,#154531,#154532,
#154533,#154534,#154535,#154536,#154537,#154538,#154539,#154540,#154541,
#154542,#154543,#154544,#154545,#154546,#154547,#154548,#154549,#154550,
#154551,#154552,#154553,#154554,#154555,#154556,#154557,#154558,#154559,
#154560,#154561,#154562,#154563,#154564,#154565,#154566,#154567,#154568,
#154569,#154570,#154571,#154572,#154573,#154574,#154575,#154576,#154577,
#154578,#154579,#154580,#154581,#154582,#154583,#154584,#154585,#154586,
#154587,#154588,#154589,#154590,#154591,#154592,#154593,#154594,#154595,
#154596,#154597,#154598,#154599,#154600,#154601,#154602,#154603,#154604,
#154605,#154606,#154607,#154608,#154609,#154610,#154611,#154612,#154613,
#154614,#154615,#154616,#154617,#154618,#154619,#154620,#154621,#154622,
#154623,#154624,#154625,#154626,#154627,#154628,#154629,#154630,#154631,
#154632,#154633,#154634,#154635,#154636),.UNSPECIFIED.,.F.,.F.,(4,3,3,3,
3,3,3,3,3,3,3,3,3,3,3,3,3,3,3,3,3,3,3,3,3,3,3,3,3,3,3,3,3,3,3,3,3,3,3,3,
3,3,3,3,3,3,3,3,3,3,3,3,3,3,3,3,3,3,3,3,3,3,3,3,3,3,3,3,3,3,3,3,3,3,3,3,
3,3,4),(-91.8176497547249,-91.7182119685907,-91.6425022974724,-91.5668412954458,
-91.4912144551078,-91.4155967588247,-91.3399852587375,-91.2643453341091,
-91.2197434252831,-91.1374646534299,-91.0551620905675,-90.9716902884195,
-90.889335333522,-90.8053051077488,-90.7212748819755,-90.6388958713735,
-90.5565316821242,-90.4731003462601,-90.3907783729674,-90.3067923558177,
-90.222806338668,-90.1471662294466,-90.0715501265406,-89.995943559487,-89.9203088967776,
-89.8446593381999,-89.7689490484231,-89.7243377953604,-89.6324372256577,
-89.5404042559442,-89.4485246861222,-89.3568972900923,-89.2658761686112,
-89.2258692520529,-89.1518673373648,-89.0778864090216,-89.0039113871093,
-88.9298989138093,-88.8558676438278,-88.7817628916227,-88.7274007087453,
-88.6484392927982,-88.569531869729,-88.4906668307924,-88.4118326000669,
-88.3330176260878,-88.2541963624276,-88.1753697233152,-88.0965271989387,
-88.0176582703557,-87.9387162190243,-87.8597354535355,-87.7806644425174,
-87.7304636221302,-87.6514717267914,-87.5725799421166,-87.4937776860723,
-87.4150776852505,-87.3364382393722,-87.2578619571867,-87.2319950788226,
-87.1534083556589,-87.0747721883961,-86.9960761950799,-86.9172621635974,
-86.8383807353739,-86.7593776421582,-86.7335265355151,-86.6544473002854,
-86.5754422403857,-86.4964996701987,-86.4176158351969,-86.3387667922288,
-86.2599420069206,-86.1811309618265,-86.1023075062359,-86.0234798687421,
-85.9446144097895,-85.8904867273958),.UNSPECIFIED.);
#3123=B_SPLINE_CURVE_WITH_KNOTS('',3,(#154642,#154643,#154644,#154645,#154646,
#154647,#154648,#154649,#154650,#154651,#154652,#154653,#154654,#154655,
#154656,#154657,#154658,#154659,#154660,#154661,#154662,#154663,#154664,
#154665,#154666,#154667,#154668,#154669,#154670,#154671,#154672,#154673,
#154674,#154675,#154676,#154677,#154678,#154679,#154680,#154681,#154682,
#154683,#154684,#154685,#154686,#154687,#154688,#154689,#154690,#154691,
#154692,#154693,#154694,#154695,#154696,#154697,#154698,#154699,#154700,
#154701,#154702,#154703,#154704,#154705,#154706,#154707,#154708,#154709,
#154710,#154711,#154712,#154713,#154714,#154715,#154716,#154717,#154718,
#154719,#154720,#154721,#154722,#154723,#154724,#154725,#154726,#154727,
#154728,#154729,#154730,#154731,#154732,#154733,#154734,#154735,#154736,
#154737,#154738,#154739,#154740,#154741,#154742,#154743,#154744,#154745,
#154746,#154747,#154748,#154749,#154750,#154751,#154752,#154753,#154754,
#154755,#154756,#154757,#154758,#154759,#154760,#154761,#154762,#154763,
#154764,#154765,#154766,#154767,#154768,#154769,#154770,#154771,#154772,
#154773,#154774,#154775,#154776,#154777,#154778,#154779,#154780,#154781,
#154782,#154783,#154784,#154785,#154786,#154787,#154788,#154789,#154790,
#154791,#154792,#154793,#154794,#154795,#154796,#154797,#154798,#154799,
#154800,#154801,#154802,#154803,#154804,#154805,#154806,#154807,#154808,
#154809,#154810,#154811,#154812,#154813,#154814,#154815,#154816,#154817,
#154818,#154819,#154820,#154821,#154822,#154823,#154824,#154825,#154826,
#154827,#154828,#154829,#154830,#154831,#154832,#154833,#154834,#154835,
#154836,#154837,#154838,#154839,#154840,#154841,#154842,#154843,#154844,
#154845,#154846,#154847,#154848,#154849,#154850,#154851,#154852,#154853,
#154854,#154855,#154856,#154857,#154858,#154859,#154860,#154861),
 .UNSPECIFIED.,.F.,.F.,(4,3,3,3,3,3,3,3,3,3,3,3,3,3,3,3,3,3,3,3,3,3,3,3,
3,3,3,3,3,3,3,3,3,3,3,3,3,3,3,3,3,3,3,3,3,3,3,3,3,3,3,3,3,3,3,3,3,3,3,3,
3,3,3,3,3,3,3,3,3,3,3,3,3,4),(83.3467333304285,83.4284632041948,83.5101929579649,
83.5919225934066,83.6736521121857,83.7553815159691,83.8371108064235,83.9220575749427,
84.0056770502037,84.0879899711638,84.1697288802311,84.2514673696174,84.3332054459974,
84.4149431160448,84.4966803864333,84.5784172638362,84.6601537549263,84.7418898663764,
84.8236256048585,84.9053609770448,84.9870959896069,85.0688306492161,85.1505649625434,
85.2322989362597,85.3140325770352,85.3957658915402,85.4774988864446,85.5592315684181,
85.6409639441299,85.7226960202491,85.8044278034446,85.8861593003851,85.9678905177387,
86.0496214621738,86.1313521403579,86.2130825589589,86.2948127246442,86.3765426440807,
86.4582723239359,86.5400017708761,86.6254299652753,86.7081885285996,86.7899271561628,
86.8716649599667,86.9534019667064,87.0351382030743,87.11687369576,87.1986084714508,
87.2803425568315,87.3620759785842,87.4438087633892,87.5255409379243,87.6072725288654,
87.6890035628865,87.7707340666591,87.8524640668536,87.9341935901381,88.0179129902326,
88.099651071261,88.1813875666854,88.2631225832699,88.3448562277583,88.4265886068752,
88.5083198273283,88.5900499958087,88.6755067452889,88.7572436635079,88.8389776724112,
88.9207091989303,89.0024386698586,89.0841735603345,89.1659036404995,89.247635069561,
89.2737039916508),.UNSPECIFIED.);
#3124=B_SPLINE_CURVE_WITH_KNOTS('',3,(#154862,#154863,#154864,#154865,#154866,
#154867,#154868,#154869,#154870,#154871,#154872,#154873,#154874),
 .UNSPECIFIED.,.F.,.F.,(4,3,3,3,4),(89.2737039916508,89.3656387825245,89.4579312834165,
89.5504795579867,89.6300395101817),.UNSPECIFIED.);
#3125=B_SPLINE_CURVE_WITH_KNOTS('',3,(#154876,#154877,#154878,#154879,#154880,
#154881,#154882,#154883,#154884,#154885,#154886,#154887,#154888,#154889,
#154890,#154891),.UNSPECIFIED.,.F.,.F.,(4,3,3,3,3,4),(-85.8904867273958,
-85.8115303384309,-85.7365894489,-85.6536039327013,-85.5708503337389,-85.5344644475453),
 .UNSPECIFIED.);
#3126=B_SPLINE_CURVE_WITH_KNOTS('',3,(#154892,#154893,#154894,#154895,#154896,
#154897,#154898,#154899,#154900,#154901,#154902,#154903,#154904,#154905,
#154906,#154907,#154908,#154909,#154910,#154911,#154912,#154913,#154914,
#154915,#154916,#154917,#154918,#154919,#154920,#154921,#154922,#154923,
#154924,#154925,#154926,#154927,#154928,#154929,#154930,#154931,#154932,
#154933,#154934,#154935,#154936,#154937,#154938,#154939,#154940,#154941,
#154942,#154943,#154944,#154945,#154946,#154947,#154948,#154949,#154950,
#154951,#154952,#154953,#154954,#154955,#154956,#154957,#154958,#154959,
#154960,#154961,#154962,#154963,#154964,#154965,#154966,#154967,#154968,
#154969,#154970,#154971,#154972,#154973,#154974,#154975,#154976,#154977,
#154978,#154979,#154980,#154981,#154982,#154983,#154984,#154985,#154986,
#154987,#154988,#154989,#154990,#154991,#154992,#154993,#154994,#154995,
#154996,#154997,#154998,#154999,#155000,#155001,#155002,#155003,#155004,
#155005,#155006,#155007,#155008,#155009,#155010,#155011,#155012,#155013,
#155014,#155015,#155016,#155017,#155018,#155019,#155020,#155021,#155022,
#155023,#155024,#155025,#155026,#155027,#155028,#155029,#155030,#155031,
#155032,#155033,#155034,#155035,#155036,#155037,#155038,#155039,#155040,
#155041,#155042,#155043,#155044,#155045,#155046,#155047,#155048,#155049,
#155050,#155051,#155052,#155053,#155054,#155055,#155056,#155057,#155058,
#155059,#155060,#155061,#155062,#155063,#155064,#155065,#155066,#155067,
#155068,#155069,#155070,#155071,#155072,#155073,#155074,#155075,#155076,
#155077,#155078,#155079,#155080,#155081,#155082,#155083,#155084,#155085,
#155086,#155087,#155088,#155089,#155090,#155091,#155092,#155093,#155094,
#155095,#155096,#155097,#155098,#155099,#155100,#155101,#155102,#155103,
#155104,#155105,#155106,#155107,#155108,#155109,#155110,#155111,#155112,
#155113,#155114,#155115,#155116,#155117,#155118,#155119,#155120,#155121,
#155122,#155123,#155124,#155125,#155126,#155127,#155128,#155129),
 .UNSPECIFIED.,.F.,.F.,(4,3,3,3,3,3,3,3,3,3,3,3,3,3,3,3,3,3,3,3,3,3,3,3,
3,3,3,3,3,3,3,3,3,3,3,3,3,3,3,3,3,3,3,3,3,3,3,3,3,3,3,3,3,3,3,3,3,3,3,3,
3,3,3,3,3,3,3,3,3,3,3,3,3,3,3,3,3,3,3,4),(-85.534464447435,-85.4603785619744,
-85.389367063574,-85.3183605525203,-85.2473304895041,-85.2381209055924,
-85.1471218058569,-85.0556185881807,-84.9636750492508,-84.8716404720719,
-84.7797313819514,-84.7396523622849,-84.6639426911673,-84.5882816891414,
-84.5126548488037,-84.4370371525214,-84.3614256524346,-84.2857857278067,
-84.2411838189773,-84.1589050471238,-84.0766024842607,-83.993130682113,
-83.910775727215,-83.8267455014424,-83.7427152756697,-83.6603362650678,
-83.5779720758183,-83.4945407399542,-83.4122187666616,-83.3282327495119,
-83.2442467323622,-83.1686066231408,-83.0929905202347,-83.0173839531808,
-82.9417492904714,-82.8660997318935,-82.7903894421167,-82.7457781890546,
-82.6538776193516,-82.561844649637,-82.469965079815,-82.3783376837873,-82.2873165623051,
-82.2473096457471,-82.1733077310589,-82.0993268027156,-82.0253517808033,
-81.9513393075032,-81.8773080375218,-81.8032032853168,-81.7488411024395,
-81.6698796864922,-81.5909722634228,-81.5121072244858,-81.4332729937596,
-81.3544580197812,-81.2756367561211,-81.1968101170086,-81.1179675926322,
-81.0390986640493,-80.9601566127179,-80.8811758472291,-80.802104836211,
-80.7519040158244,-80.6729121204856,-80.5940203358109,-80.5152180797672,
-80.4365180789458,-80.3578786330677,-80.2793023508825,-80.2534354725168,
-80.1748487493532,-80.0962125820902,-80.0175165887737,-79.9387025572909,
-79.8598211290667,-79.7808180358505,-79.7549669292093,-79.67261042862,-79.6072239344785),
 .UNSPECIFIED.);
#3127=B_SPLINE_CURVE_WITH_KNOTS('',3,(#155135,#155136,#155137,#155138,#155139,
#155140,#155141,#155142,#155143,#155144,#155145,#155146,#155147,#155148,
#155149,#155150,#155151,#155152,#155153,#155154,#155155,#155156,#155157,
#155158,#155159,#155160,#155161,#155162,#155163,#155164,#155165,#155166,
#155167,#155168,#155169,#155170,#155171,#155172,#155173,#155174,#155175,
#155176,#155177,#155178,#155179,#155180,#155181,#155182,#155183,#155184,
#155185,#155186,#155187,#155188,#155189,#155190,#155191,#155192,#155193,
#155194,#155195,#155196,#155197,#155198,#155199,#155200,#155201,#155202,
#155203,#155204,#155205,#155206,#155207,#155208,#155209,#155210,#155211,
#155212,#155213,#155214,#155215,#155216,#155217,#155218,#155219,#155220,
#155221,#155222,#155223,#155224,#155225,#155226,#155227,#155228,#155229,
#155230,#155231,#155232,#155233,#155234,#155235,#155236,#155237,#155238,
#155239,#155240,#155241,#155242,#155243,#155244,#155245,#155246,#155247,
#155248,#155249,#155250,#155251,#155252,#155253,#155254,#155255,#155256,
#155257,#155258,#155259,#155260,#155261,#155262,#155263,#155264,#155265,
#155266,#155267,#155268,#155269,#155270,#155271,#155272,#155273,#155274,
#155275,#155276,#155277,#155278,#155279,#155280,#155281,#155282,#155283,
#155284,#155285,#155286,#155287,#155288,#155289,#155290,#155291,#155292,
#155293,#155294,#155295,#155296,#155297,#155298,#155299,#155300,#155301,
#155302,#155303,#155304,#155305,#155306,#155307,#155308,#155309,#155310,
#155311,#155312,#155313,#155314,#155315,#155316,#155317,#155318,#155319,
#155320,#155321,#155322,#155323,#155324,#155325,#155326,#155327,#155328,
#155329,#155330,#155331,#155332,#155333,#155334,#155335,#155336,#155337,
#155338,#155339,#155340,#155341,#155342,#155343,#155344,#155345,#155346,
#155347,#155348,#155349,#155350,#155351,#155352,#155353,#155354,#155355,
#155356,#155357,#155358,#155359,#155360,#155361,#155362,#155363,#155364,
#155365,#155366,#155367,#155368,#155369,#155370,#155371,#155372,#155373,
#155374,#155375),.UNSPECIFIED.,.F.,.F.,(4,3,3,3,3,3,3,3,3,3,3,3,3,3,3,3,
3,3,3,3,3,3,3,3,3,3,3,3,3,3,3,3,3,3,3,3,3,3,3,3,3,3,3,3,3,3,3,3,3,3,3,3,
3,3,3,3,3,3,3,3,3,3,3,3,3,3,3,3,3,3,3,3,3,3,3,3,3,3,3,3,4),(77.0637438066728,
77.1460509018794,77.2283272461551,77.2626242126715,77.3382643218935,77.4138804248002,
77.4894869918545,77.5651216545645,77.640771213143,77.7164815029205,77.7610927559791,
77.8529933256816,77.9450262953949,78.0369058652165,78.128533261245,78.2195543827259,
78.2595612992866,78.3335632139748,78.4075441423182,78.4815191642309,78.5555316375308,
78.6295629075121,78.7036676597172,78.7580298425942,78.8369912585414,78.9158986816107,
78.9947637205473,79.0735979512731,79.1524129252519,79.2312341889121,79.3100608280245,
79.3889033524008,79.4677722809837,79.5467143323151,79.625695097804,79.7047661088221,
79.7549669292093,79.8339588245478,79.9128506092226,79.9916528652669,80.0703528660884,
80.1489923119669,80.2275685941521,80.2534354725169,80.3320221956804,80.4106583629434,
80.4893543562597,80.5681683877424,80.647049815966,80.7260529091818,80.7519040158244,
80.830976537574,80.9099760923091,80.9889143601331,81.0678029746144,81.1466535311706,
81.2254820354363,81.3042984093052,81.3831131604889,81.4619367944664,81.5408068420147,
81.6197005210906,81.6986610459276,81.7488411024395,81.8229465405415,81.896995038396,
81.9710017764029,82.0449910405556,82.1189684021677,82.1929706882008,82.2473096457471,
82.338308745483,82.4298119631601,82.5217555020904,82.6137900792692,82.7056991693903,
82.7457781890547,82.8222589565696,82.8986881147001,82.9750730542511,82.9905186844712),
 .UNSPECIFIED.);
#3128=B_SPLINE_CURVE_WITH_KNOTS('',3,(#155376,#155377,#155378,#155379,#155380,
#155381,#155382,#155383,#155384,#155385,#155386,#155387,#155388,#155389,
#155390,#155391),.UNSPECIFIED.,.F.,.F.,(4,3,3,3,3,4),(82.9905186844712,
83.0722482283072,83.1539833432262,83.2357135805754,83.3174453695265,83.3467333304285),
 .UNSPECIFIED.);
#3129=B_SPLINE_CURVE_WITH_KNOTS('',3,(#155393,#155394,#155395,#155396,#155397,
#155398,#155399,#155400,#155401,#155402,#155403,#155404,#155405,#155406,
#155407,#155408),.UNSPECIFIED.,.F.,.F.,(4,3,3,3,3,4),(-79.6072239344785,
-79.5250325657862,-79.4429820957931,-79.3610225518867,-79.2791885693329,
-79.2512791403658),.UNSPECIFIED.);
#3130=B_SPLINE_CURVE_WITH_KNOTS('',3,(#155409,#155410,#155411,#155412,#155413,
#155414,#155415,#155416,#155417,#155418,#155419,#155420,#155421,#155422,
#155423,#155424,#155425,#155426,#155427,#155428,#155429,#155430,#155431,
#155432,#155433,#155434,#155435,#155436,#155437,#155438,#155439,#155440,
#155441,#155442,#155443,#155444,#155445,#155446,#155447,#155448,#155449,
#155450,#155451,#155452,#155453,#155454,#155455,#155456,#155457,#155458,
#155459,#155460,#155461,#155462,#155463,#155464,#155465,#155466,#155467,
#155468,#155469,#155470,#155471,#155472,#155473,#155474,#155475,#155476,
#155477,#155478,#155479,#155480,#155481,#155482,#155483,#155484,#155485,
#155486,#155487,#155488,#155489,#155490,#155491,#155492,#155493,#155494,
#155495,#155496,#155497,#155498,#155499,#155500,#155501,#155502,#155503,
#155504,#155505,#155506,#155507,#155508,#155509,#155510,#155511,#155512,
#155513,#155514,#155515,#155516,#155517,#155518,#155519,#155520,#155521,
#155522,#155523,#155524,#155525,#155526,#155527,#155528,#155529,#155530,
#155531,#155532,#155533,#155534,#155535,#155536,#155537,#155538,#155539,
#155540,#155541,#155542,#155543,#155544,#155545,#155546,#155547,#155548,
#155549,#155550,#155551,#155552,#155553,#155554,#155555,#155556,#155557,
#155558,#155559,#155560,#155561,#155562,#155563,#155564,#155565,#155566,
#155567,#155568,#155569,#155570,#155571,#155572,#155573,#155574,#155575,
#155576,#155577,#155578,#155579,#155580,#155581,#155582,#155583,#155584,
#155585,#155586,#155587,#155588,#155589,#155590,#155591,#155592,#155593,
#155594,#155595,#155596,#155597,#155598,#155599,#155600,#155601,#155602,
#155603,#155604,#155605,#155606,#155607,#155608,#155609,#155610,#155611,
#155612,#155613,#155614,#155615,#155616,#155617,#155618,#155619,#155620,
#155621,#155622,#155623,#155624,#155625,#155626,#155627,#155628,#155629,
#155630,#155631,#155632,#155633,#155634,#155635,#155636,#155637,#155638,
#155639,#155640),.UNSPECIFIED.,.F.,.F.,(4,3,3,3,3,3,3,3,3,3,3,3,3,3,3,3,
3,3,3,3,3,3,3,3,3,3,3,3,3,3,3,3,3,3,3,3,3,3,3,3,3,3,3,3,3,3,3,3,3,3,3,3,
3,3,3,3,3,3,3,3,3,3,3,3,3,3,3,3,3,3,3,3,3,3,3,3,3,4),(-79.2512785228306,
-79.1677334496107,-79.0840691932055,-79.0002387934004,-78.9163372798076,
-78.8323326741379,-78.7580298425942,-78.6839244044922,-78.6098759066377,
-78.5358691686304,-78.4618799044777,-78.3879025428657,-78.3139002568326,
-78.2595612992866,-78.1685621995506,-78.0770589818738,-77.9851154429436,
-77.8930808657643,-77.8011717756431,-77.761092755979,-77.6853830848615,
-77.6097220828355,-77.5340952424979,-77.4584775462156,-77.382866046129,
-77.3072261215013,-77.2626242126715,-77.180345440818,-77.0980428779547,
-77.014571075807,-76.9322161209089,-76.8481858951364,-76.7641556693639,
-76.681776658762,-76.5994124695124,-76.5159811336484,-76.4336591603557,
-76.349673143206,-76.2656871260564,-76.1900470168349,-76.1144309139291,
-76.0388243468752,-75.9631896841656,-75.8875401255878,-75.8118298358109,
-75.7672185827488,-75.6753180130453,-75.5832850433304,-75.4914054735083,
-75.3997780774793,-75.3087569559981,-75.2687500394412,-75.1947481247532,
-75.1207671964098,-75.0467921744976,-74.9727797011978,-74.8987484312166,
-74.8246436790119,-74.7702814961337,-74.6913200801863,-74.6124126571173,
-74.5335476181811,-74.4547133874553,-74.3758984134772,-74.2970771498171,
-74.2182505107048,-74.1394079863288,-74.0605390577459,-73.9815970064143,
-73.9026162409256,-73.8235452299075,-73.7733444095186,-73.6943456368794,
-73.6154474967274,-73.5366695691337,-73.4579618401987,-73.3793327385231,
-73.3240852745455),.UNSPECIFIED.);
#3131=B_SPLINE_CURVE_WITH_KNOTS('',3,(#155646,#155647,#155648,#155649,#155650,
#155651,#155652,#155653,#155654,#155655,#155656,#155657,#155658,#155659,
#155660,#155661,#155662,#155663,#155664,#155665,#155666,#155667,#155668,
#155669,#155670,#155671,#155672,#155673,#155674,#155675,#155676,#155677,
#155678,#155679,#155680,#155681,#155682,#155683,#155684,#155685,#155686,
#155687,#155688,#155689,#155690,#155691,#155692,#155693,#155694,#155695,
#155696,#155697,#155698,#155699,#155700,#155701,#155702,#155703,#155704,
#155705,#155706,#155707,#155708,#155709,#155710,#155711,#155712,#155713,
#155714,#155715,#155716,#155717,#155718,#155719,#155720,#155721,#155722,
#155723,#155724,#155725,#155726,#155727,#155728,#155729,#155730,#155731,
#155732,#155733,#155734,#155735,#155736,#155737,#155738,#155739,#155740,
#155741,#155742,#155743,#155744,#155745,#155746,#155747,#155748,#155749,
#155750,#155751,#155752,#155753,#155754,#155755,#155756,#155757,#155758,
#155759,#155760,#155761,#155762,#155763,#155764,#155765,#155766,#155767,
#155768,#155769,#155770,#155771,#155772,#155773,#155774,#155775,#155776,
#155777,#155778,#155779,#155780,#155781,#155782,#155783,#155784,#155785,
#155786,#155787,#155788,#155789,#155790,#155791,#155792,#155793,#155794,
#155795,#155796,#155797,#155798,#155799,#155800,#155801,#155802,#155803,
#155804,#155805,#155806,#155807,#155808,#155809,#155810,#155811,#155812,
#155813,#155814,#155815,#155816,#155817,#155818,#155819,#155820,#155821,
#155822,#155823,#155824,#155825,#155826,#155827,#155828,#155829,#155830,
#155831,#155832,#155833,#155834,#155835,#155836,#155837,#155838,#155839,
#155840,#155841,#155842,#155843,#155844,#155845,#155846,#155847,#155848,
#155849,#155850,#155851,#155852,#155853,#155854,#155855,#155856,#155857,
#155858,#155859,#155860,#155861,#155862,#155863,#155864,#155865,#155866,
#155867,#155868,#155869,#155870,#155871,#155872,#155873,#155874,#155875,
#155876,#155877,#155878,#155879,#155880,#155881,#155882,#155883,#155884,
#155885,#155886),.UNSPECIFIED.,.F.,.F.,(4,3,3,3,3,3,3,3,3,3,3,3,3,3,3,3,
3,3,3,3,3,3,3,3,3,3,3,3,3,3,3,3,3,3,3,3,3,3,3,3,3,3,3,3,3,3,3,3,3,3,3,3,
3,3,3,3,3,3,3,3,3,3,3,3,3,3,3,3,3,3,3,3,3,3,3,3,3,3,3,3,4),(70.7799867132232,
70.7825331496733,70.8744337193759,70.9664666890899,71.058346258912,71.1499736549409,
71.2409947764223,71.2810016929808,71.355003607669,71.4289845360125,71.5029595579251,
71.5769720312251,71.6510033012064,71.7251080534115,71.7794702362884,71.8584316522356,
71.9373390753048,72.0162041142414,72.0950383449674,72.1738533189461,72.2526745826062,
72.3315012217186,72.4103437460949,72.4892126746776,72.568154726009,72.6471354914978,
72.726206502516,72.7764073229035,72.855399218242,72.9342910029167,73.0130932589609,
73.0917932597823,73.1704327056608,73.249008987846,73.274875866211,73.3534625893746,
73.4320987566377,73.5107947499542,73.5896087814371,73.6684902096608,73.7474933028768,
73.7733444095186,73.8524169312682,73.9314164860032,74.0103547538272,74.0892433683085,
74.1680939248648,74.2469224291305,74.3257388029993,74.4045535541831,74.4833771881605,
74.5622472357088,74.6411409147846,74.7201014396216,74.7702814961337,74.8443869342357,
74.9184354320902,74.9924421700973,75.06643143425,75.1404087958621,75.2144110818953,
75.2687500394413,75.359749139177,75.4512523568538,75.5431958957836,75.6352304729624,
75.7271395630831,75.7672185827488,75.8429282538665,75.9185892558926,75.9942160962305,
76.0698337925129,76.1454452925997,76.2210852172276,76.2656871260564,76.3479703571948,
76.4302779995685,76.5126237436815,76.5949809727244,76.6773585381553,76.7073333772916),
 .UNSPECIFIED.);
#3132=B_SPLINE_CURVE_WITH_KNOTS('',3,(#155887,#155888,#155889,#155890,#155891,
#155892,#155893,#155894,#155895,#155896,#155897,#155898,#155899,#155900,
#155901,#155902),.UNSPECIFIED.,.F.,.F.,(4,3,3,3,3,4),(76.7073333773951,
76.764155669364,76.8465358442871,76.9289000222271,77.0112452878717,77.0637438066728),
 .UNSPECIFIED.);
#3133=B_SPLINE_CURVE_WITH_KNOTS('',3,(#155904,#155905,#155906,#155907,#155908,
#155909,#155910,#155911,#155912,#155913,#155914,#155915,#155916,#155917,
#155918,#155919),.UNSPECIFIED.,.F.,.F.,(4,3,3,3,3,4),(-73.3240852745455,
-73.274875866211,-73.1981803579767,-73.1235307356291,-73.0458122844514,
-72.9680938332738),.UNSPECIFIED.);
#3134=B_SPLINE_CURVE_WITH_KNOTS('',3,(#155920,#155921,#155922,#155923,#155924,
#155925,#155926,#155927,#155928,#155929,#155930,#155931,#155932,#155933,
#155934,#155935,#155936,#155937,#155938,#155939,#155940,#155941,#155942,
#155943,#155944,#155945,#155946,#155947,#155948,#155949,#155950,#155951,
#155952,#155953,#155954,#155955,#155956,#155957,#155958,#155959,#155960,
#155961,#155962,#155963,#155964,#155965,#155966,#155967,#155968,#155969,
#155970,#155971,#155972,#155973,#155974,#155975,#155976,#155977,#155978,
#155979,#155980,#155981,#155982,#155983,#155984,#155985,#155986,#155987,
#155988,#155989,#155990,#155991,#155992,#155993,#155994,#155995,#155996,
#155997,#155998,#155999,#156000,#156001,#156002,#156003,#156004,#156005,
#156006,#156007,#156008,#156009,#156010,#156011,#156012,#156013,#156014,
#156015,#156016,#156017,#156018,#156019,#156020,#156021,#156022,#156023,
#156024,#156025,#156026,#156027,#156028,#156029,#156030,#156031,#156032,
#156033,#156034,#156035,#156036,#156037,#156038,#156039,#156040,#156041,
#156042,#156043,#156044,#156045,#156046,#156047,#156048,#156049,#156050,
#156051,#156052,#156053,#156054,#156055,#156056,#156057,#156058,#156059,
#156060,#156061,#156062,#156063,#156064,#156065,#156066,#156067,#156068,
#156069,#156070,#156071,#156072,#156073,#156074,#156075,#156076,#156077,
#156078,#156079,#156080,#156081,#156082,#156083,#156084,#156085,#156086,
#156087,#156088,#156089,#156090,#156091,#156092,#156093,#156094,#156095,
#156096,#156097,#156098,#156099,#156100,#156101,#156102,#156103,#156104,
#156105,#156106,#156107,#156108,#156109,#156110,#156111,#156112,#156113,
#156114,#156115,#156116,#156117,#156118,#156119,#156120,#156121,#156122,
#156123,#156124,#156125,#156126,#156127,#156128,#156129,#156130,#156131,
#156132,#156133,#156134,#156135,#156136,#156137,#156138,#156139,#156140,
#156141,#156142,#156143,#156144,#156145,#156146,#156147,#156148,#156149,
#156150,#156151),.UNSPECIFIED.,.F.,.F.,(4,3,3,3,3,3,3,3,3,3,3,3,3,3,3,3,
3,3,3,3,3,3,3,3,3,3,3,3,3,3,3,3,3,3,3,3,3,3,3,3,3,3,3,3,3,3,3,3,3,3,3,3,
3,3,3,3,3,3,3,3,3,3,3,3,3,3,3,3,3,3,3,3,3,3,3,3,3,4),(-72.9680938331862,
-72.8722505780449,-72.7764073229035,-72.6973348011539,-72.6183352464187,
-72.5393969785947,-72.4605083641133,-72.3816578075571,-72.3028293032914,
-72.2240129294225,-72.1451981782387,-72.0663745442612,-71.9875044967129,
-71.908610817637,-71.8296502928,-71.7794702362883,-71.7053647981864,-71.6313163003318,
-71.5573095623247,-71.4833202981721,-71.4093429365601,-71.3353406505269,
-71.2810016929808,-71.1900025932449,-71.0984993755676,-71.0065558366373,
-70.9145212594584,-70.8226121693373,-70.7825331496732,-70.7068234785557,
-70.6311624765299,-70.5555356361924,-70.4799179399102,-70.4043064398236,
-70.3286665151959,-70.2840646063657,-70.2017858345122,-70.1194832716494,
-70.0360114695015,-69.9536565146034,-69.8696262888308,-69.7855960630581,
-69.7032170524562,-69.6208528632067,-69.5374215273427,-69.4550995540499,
-69.3711135369003,-69.2871275197506,-69.2114874105292,-69.1358713076231,
-69.0602647405694,-68.98463007786,-68.9089805192822,-68.8332702295053,-68.788658976443,
-68.69675840674,-68.6047254370263,-68.5128458672042,-68.4212184711754,-68.3301973496942,
-68.2901904331355,-68.2161885184473,-68.1422075901039,-68.0682325681916,
-67.9942200948916,-67.9201888249102,-67.8460840727052,-67.7917218898279,
-67.7127532835095,-67.6338405959854,-67.5549769868227,-67.4761421238226,
-67.3973254830067,-67.3185165534304,-67.2396875472761,-67.160849079403,
-67.0819685455894,-67.0415072947074),.UNSPECIFIED.);
#3135=B_SPLINE_CURVE_WITH_KNOTS('',3,(#156157,#156158,#156159,#156160,#156161,
#156162,#156163,#156164,#156165,#156166,#156167,#156168,#156169,#156170,
#156171,#156172,#156173,#156174,#156175,#156176,#156177,#156178,#156179,
#156180,#156181,#156182,#156183,#156184,#156185,#156186,#156187,#156188,
#156189,#156190,#156191,#156192,#156193,#156194,#156195,#156196,#156197,
#156198,#156199,#156200,#156201,#156202,#156203,#156204,#156205,#156206,
#156207,#156208,#156209,#156210,#156211,#156212,#156213,#156214,#156215,
#156216,#156217,#156218,#156219,#156220,#156221,#156222,#156223,#156224,
#156225,#156226,#156227,#156228,#156229,#156230,#156231,#156232,#156233,
#156234,#156235,#156236,#156237,#156238,#156239,#156240,#156241,#156242,
#156243,#156244,#156245,#156246,#156247,#156248,#156249,#156250,#156251,
#156252,#156253,#156254,#156255,#156256,#156257,#156258,#156259,#156260,
#156261,#156262,#156263,#156264,#156265,#156266,#156267,#156268,#156269,
#156270,#156271,#156272,#156273,#156274,#156275,#156276,#156277,#156278,
#156279,#156280,#156281,#156282,#156283,#156284,#156285,#156286,#156287,
#156288,#156289,#156290,#156291,#156292,#156293,#156294,#156295,#156296,
#156297,#156298,#156299,#156300,#156301,#156302,#156303,#156304,#156305,
#156306,#156307,#156308,#156309,#156310,#156311,#156312,#156313,#156314,
#156315,#156316,#156317,#156318,#156319,#156320,#156321,#156322,#156323,
#156324,#156325,#156326,#156327,#156328,#156329,#156330,#156331,#156332,
#156333,#156334,#156335,#156336,#156337,#156338,#156339,#156340,#156341,
#156342,#156343,#156344,#156345,#156346,#156347,#156348,#156349,#156350,
#156351,#156352,#156353,#156354,#156355,#156356,#156357,#156358,#156359,
#156360,#156361,#156362,#156363,#156364,#156365,#156366,#156367,#156368,
#156369,#156370,#156371,#156372,#156373,#156374,#156375,#156376),
 .UNSPECIFIED.,.F.,.F.,(4,3,3,3,3,3,3,3,3,3,3,3,3,3,3,3,3,3,3,3,3,3,3,3,
3,3,3,3,3,3,3,3,3,3,3,3,3,3,3,3,3,3,3,3,3,3,3,3,3,3,3,3,3,3,3,3,3,3,3,3,
3,3,3,3,3,3,3,3,3,3,3,3,3,4),(64.4971774088899,64.5789072826559,64.6606370364263,
64.7423666718676,64.8240961906468,64.9058255944302,64.9875548848845,65.0725016534037,
65.1561211286648,65.2384340496249,65.3201729586921,65.4019114480785,65.4836495244585,
65.5653871945059,65.6471244648944,65.7288613422973,65.8105978333875,65.8923339448375,
65.9740696833197,66.055805055506,66.1375400680681,66.2192747276772,66.3010090410045,
66.3827430147207,66.4644766554963,66.5462099700013,66.6279429649057,66.7096756468792,
66.7914080225911,66.8731400987103,66.9548718819059,67.0366033788464,67.1183345962,
67.200065540635,67.2817962188191,67.3635266374201,67.4452568031052,67.5269867225418,
67.6087164023969,67.6904458493373,67.7758740437365,67.8586326070607,67.940371234624,
68.0221090384279,68.1038460451676,68.1855822815355,68.2673177742213,68.3490525499121,
68.4307866352927,68.5125200570455,68.5942528418505,68.6759850163858,68.757716607327,
68.839447641348,68.9211781451206,69.0029081453151,69.0846376685999,69.1683570686944,
69.2500951497228,69.3318316451472,69.4135666617318,69.4953003062201,69.5770326853371,
69.6587639057902,69.7404940742708,69.8259508237509,69.9076877419699,69.9894217508731,
70.0711532773924,70.1528827483207,70.2346176387967,70.3163477189616,70.3980791480231,
70.4241480701121),.UNSPECIFIED.);
#3136=B_SPLINE_CURVE_WITH_KNOTS('',3,(#156377,#156378,#156379,#156380,#156381,
#156382,#156383,#156384,#156385,#156386,#156387,#156388,#156389,#156390,
#156391,#156392),.UNSPECIFIED.,.F.,.F.,(4,3,3,3,3,4),(70.4241480701121,
70.4995216491135,70.5749196434235,70.6503295519316,70.7257998391169,70.7799867132232),
 .UNSPECIFIED.);
#3137=B_SPLINE_CURVE_WITH_KNOTS('',3,(#156394,#156395,#156396,#156397,#156398,
#156399,#156400,#156401,#156402,#156403,#156404,#156405,#156406,#156407,
#156408,#156409),.UNSPECIFIED.,.F.,.F.,(4,3,3,3,3,4),(-67.0415072947074,
-66.9625466064109,-66.8835422217944,-66.8044565762651,-66.7947848032128,
-66.6849085260066),.UNSPECIFIED.);
#3138=B_SPLINE_CURVE_WITH_KNOTS('',3,(#156410,#156411,#156412,#156413,#156414,
#156415,#156416,#156417,#156418,#156419,#156420,#156421,#156422,#156423,
#156424,#156425,#156426,#156427,#156428,#156429,#156430,#156431,#156432,
#156433,#156434,#156435,#156436,#156437,#156438,#156439,#156440,#156441,
#156442,#156443,#156444,#156445,#156446,#156447,#156448,#156449,#156450,
#156451,#156452,#156453,#156454,#156455,#156456,#156457,#156458,#156459,
#156460,#156461,#156462,#156463,#156464,#156465,#156466,#156467,#156468,
#156469,#156470,#156471,#156472,#156473,#156474,#156475,#156476,#156477,
#156478,#156479,#156480,#156481,#156482,#156483,#156484,#156485,#156486,
#156487,#156488,#156489,#156490,#156491,#156492,#156493,#156494,#156495,
#156496,#156497,#156498,#156499,#156500,#156501,#156502,#156503,#156504,
#156505,#156506,#156507,#156508,#156509,#156510,#156511,#156512,#156513,
#156514,#156515,#156516,#156517,#156518,#156519,#156520,#156521,#156522,
#156523,#156524,#156525,#156526,#156527,#156528,#156529,#156530,#156531,
#156532,#156533,#156534,#156535,#156536,#156537,#156538,#156539,#156540,
#156541,#156542,#156543,#156544,#156545,#156546,#156547,#156548,#156549,
#156550,#156551,#156552,#156553,#156554,#156555,#156556,#156557,#156558,
#156559,#156560,#156561,#156562,#156563,#156564,#156565,#156566,#156567,
#156568,#156569,#156570,#156571,#156572,#156573,#156574,#156575,#156576,
#156577,#156578,#156579,#156580,#156581,#156582,#156583,#156584,#156585,
#156586,#156587,#156588,#156589,#156590,#156591,#156592,#156593,#156594,
#156595,#156596,#156597,#156598,#156599,#156600,#156601,#156602,#156603,
#156604,#156605,#156606,#156607,#156608,#156609,#156610,#156611,#156612,
#156613,#156614,#156615,#156616,#156617,#156618,#156619,#156620,#156621,
#156622,#156623,#156624,#156625,#156626,#156627,#156628,#156629,#156630,
#156631,#156632,#156633,#156634,#156635,#156636,#156637,#156638,#156639,
#156640,#156641,#156642,#156643,#156644),.UNSPECIFIED.,.F.,.F.,(4,3,3,3,
3,3,3,3,3,3,3,3,3,3,3,3,3,3,3,3,3,3,3,3,3,3,3,3,3,3,3,3,3,3,3,3,3,3,3,3,
3,3,3,3,3,3,3,3,3,3,3,3,3,3,3,3,3,3,3,3,3,3,3,3,3,3,3,3,3,3,3,3,3,3,3,3,
3,3,4),(-66.6849085258952,-66.6088428877483,-66.5307112307875,-66.454794221533,
-66.3755552407191,-66.2963162599052,-66.217729536742,-66.1390933694789,
-66.0603973761627,-65.98158334468,-65.9027019164564,-65.8236988232405,-65.7978477165977,
-65.718775194848,-65.639775640113,-65.5608373722887,-65.4819487578074,-65.4030982012506,
-65.3242696969848,-65.2454533231158,-65.1666385719322,-65.0878149379551,
-65.0089448904068,-64.9300512113308,-64.8510906864937,-64.8009106299825,
-64.7268051918805,-64.6527566940262,-64.5787499560192,-64.5047606918665,
-64.4307833302543,-64.3567810442212,-64.302442086675,-64.2114429869394,
-64.1199397692619,-64.0279962303319,-63.9359616531531,-63.8440525630324,
-63.8039735433674,-63.7282638722498,-63.6526028702242,-63.5769760298864,
-63.501358333604,-63.4257468335173,-63.3501069088897,-63.3055050000599,
-63.2232262282068,-63.1409236653438,-63.0574518631959,-62.975096908298,
-62.8910666825251,-62.8070364567523,-62.7246574461501,-62.6422932569008,
-62.5588619210368,-62.4765399477438,-62.3925539305943,-62.3085679134447,
-62.2329278042234,-62.1573117013175,-62.081705134264,-62.0060704715546,
-61.9304209129773,-61.8547106232006,-61.8100993701372,-61.7181988004331,
-61.6261658307195,-61.534286260897,-61.4426588648701,-61.3516377433887,
-61.3116308268296,-61.2376289121415,-61.1636479837985,-61.0896729618857,
-61.0156604885858,-60.9416292186042,-60.8675244663993,-60.8131622835221,
-60.7582306085734),.UNSPECIFIED.);
#3139=B_SPLINE_CURVE_WITH_KNOTS('',3,(#156650,#156651,#156652,#156653,#156654,
#156655,#156656,#156657,#156658,#156659,#156660,#156661,#156662,#156663,
#156664,#156665,#156666,#156667,#156668,#156669,#156670,#156671,#156672,
#156673,#156674,#156675,#156676,#156677,#156678,#156679,#156680,#156681,
#156682,#156683,#156684,#156685,#156686,#156687,#156688,#156689,#156690,
#156691,#156692,#156693,#156694,#156695,#156696,#156697,#156698,#156699,
#156700,#156701,#156702,#156703,#156704,#156705,#156706,#156707,#156708,
#156709,#156710,#156711,#156712,#156713,#156714,#156715,#156716,#156717,
#156718,#156719,#156720,#156721,#156722,#156723,#156724,#156725,#156726,
#156727,#156728,#156729,#156730,#156731,#156732,#156733,#156734,#156735,
#156736,#156737,#156738,#156739,#156740,#156741,#156742,#156743,#156744,
#156745,#156746,#156747,#156748,#156749,#156750,#156751,#156752,#156753,
#156754,#156755,#156756,#156757,#156758,#156759,#156760,#156761,#156762,
#156763,#156764,#156765,#156766,#156767,#156768,#156769,#156770,#156771,
#156772,#156773,#156774,#156775,#156776,#156777,#156778,#156779,#156780,
#156781,#156782,#156783,#156784,#156785,#156786,#156787,#156788,#156789,
#156790,#156791,#156792,#156793,#156794,#156795,#156796,#156797,#156798,
#156799,#156800,#156801,#156802,#156803,#156804,#156805,#156806,#156807,
#156808,#156809,#156810,#156811,#156812,#156813,#156814,#156815,#156816,
#156817,#156818,#156819,#156820,#156821,#156822,#156823,#156824,#156825,
#156826,#156827,#156828,#156829,#156830,#156831,#156832,#156833,#156834,
#156835,#156836,#156837,#156838,#156839,#156840,#156841,#156842,#156843,
#156844,#156845,#156846,#156847,#156848,#156849,#156850,#156851,#156852,
#156853,#156854,#156855,#156856,#156857,#156858,#156859,#156860,#156861,
#156862,#156863,#156864,#156865,#156866,#156867,#156868,#156869,#156870,
#156871,#156872,#156873,#156874,#156875,#156876,#156877,#156878,#156879,
#156880,#156881,#156882,#156883,#156884),.UNSPECIFIED.,.F.,.F.,(4,3,3,3,
3,3,3,3,3,3,3,3,3,3,3,3,3,3,3,3,3,3,3,3,3,3,3,3,3,3,3,3,3,3,3,3,3,3,3,3,
3,3,3,3,3,3,3,3,3,3,3,3,3,3,3,3,3,3,3,3,3,3,3,3,3,3,3,3,3,3,3,3,3,3,3,3,
3,3,4),(58.2138923057233,58.2922290577518,58.3705658184217,58.4489140372679,
58.5272851692979,58.6057275535383,58.6842073400998,58.7627801355672,58.8192881102919,
58.8982800056304,58.9771717903052,59.0559740463494,59.1346740471708,59.2133134930495,
59.2918897752347,59.3177566535994,59.3963433767629,59.474979544026,59.5536755373422,
59.6324895688251,59.7113709970488,59.7903740902648,59.816225196907,59.8952977186566,
59.9742972733916,60.0532355412157,60.132124155697,60.2109747122533,60.289803216519,
60.3686195903879,60.4474343415717,60.5262579755491,60.6051280230974,60.6840217021733,
60.7629822270103,60.8131622835221,60.887267721624,60.9613162194785,61.0353229574855,
61.1093122216381,61.1832895832501,61.2572918692832,61.3116308268296,61.4026299265654,
61.4941331442422,61.5860766831724,61.6781112603513,61.7700203504723,61.8100993701372,
61.8858090412549,61.9614700432808,62.0370968836184,62.1127145799009,62.1883260799876,
62.2639660046154,62.3085679134448,62.390846685298,62.4731492481605,62.5566210503085,
62.6389760052064,62.7230062309794,62.8070364567523,62.8894154673545,62.9717796566043,
63.0552109924682,63.1375329657612,63.2215189829106,63.3055050000599,63.3811451092811,
63.4567612121871,63.5323677792406,63.6080024419499,63.6836520005274,63.7593622903041,
63.8039735433674,63.8991328275661,63.9944342542252,64.0894349263504,64.1409627629325),
 .UNSPECIFIED.);
#3140=B_SPLINE_CURVE_WITH_KNOTS('',3,(#156885,#156886,#156887,#156888,#156889,
#156890,#156891,#156892,#156893,#156894,#156895,#156896,#156897,#156898,
#156899,#156900),.UNSPECIFIED.,.F.,.F.,(4,3,3,3,3,4),(64.1409627629325,
64.2226923067685,64.3044274216875,64.3861576590365,64.4678894479876,64.4971774088899),
 .UNSPECIFIED.);
#3141=B_SPLINE_CURVE_WITH_KNOTS('',3,(#156902,#156903,#156904,#156905,#156906,
#156907,#156908,#156909,#156910,#156911,#156912,#156913,#156914),
 .UNSPECIFIED.,.F.,.F.,(4,3,3,3,4),(-60.7582306085734,-60.6691037611657,
-60.5810548876563,-60.4913890532995,-60.4017232189426),.UNSPECIFIED.);
#3142=B_SPLINE_CURVE_WITH_KNOTS('',3,(#156915,#156916,#156917,#156918,#156919,
#156920,#156921,#156922,#156923,#156924,#156925,#156926,#156927,#156928,
#156929,#156930,#156931,#156932,#156933,#156934,#156935,#156936,#156937,
#156938,#156939,#156940,#156941,#156942,#156943,#156944,#156945,#156946,
#156947,#156948,#156949,#156950,#156951,#156952,#156953,#156954,#156955,
#156956,#156957,#156958,#156959,#156960,#156961,#156962,#156963,#156964,
#156965,#156966,#156967,#156968,#156969,#156970,#156971,#156972,#156973,
#156974,#156975,#156976,#156977,#156978,#156979,#156980,#156981,#156982,
#156983,#156984,#156985,#156986,#156987,#156988,#156989,#156990,#156991,
#156992,#156993,#156994,#156995,#156996,#156997,#156998,#156999,#157000,
#157001,#157002,#157003,#157004,#157005,#157006,#157007,#157008,#157009,
#157010,#157011,#157012,#157013,#157014,#157015,#157016,#157017,#157018,
#157019,#157020,#157021,#157022,#157023,#157024,#157025,#157026,#157027,
#157028,#157029,#157030,#157031,#157032,#157033,#157034,#157035,#157036,
#157037,#157038,#157039,#157040,#157041,#157042,#157043,#157044,#157045,
#157046,#157047,#157048,#157049,#157050,#157051,#157052,#157053,#157054,
#157055,#157056,#157057,#157058,#157059,#157060,#157061,#157062,#157063,
#157064,#157065,#157066,#157067,#157068,#157069,#157070,#157071,#157072,
#157073,#157074,#157075,#157076,#157077,#157078,#157079,#157080,#157081,
#157082,#157083,#157084,#157085,#157086,#157087,#157088,#157089,#157090,
#157091,#157092,#157093,#157094,#157095,#157096,#157097,#157098,#157099,
#157100,#157101,#157102,#157103,#157104,#157105,#157106,#157107,#157108,
#157109,#157110,#157111,#157112,#157113,#157114,#157115,#157116,#157117,
#157118,#157119,#157120,#157121,#157122,#157123,#157124,#157125,#157126,
#157127,#157128,#157129,#157130,#157131,#157132,#157133,#157134,#157135,
#157136,#157137,#157138,#157139,#157140,#157141,#157142,#157143,#157144,
#157145,#157146,#157147,#157148,#157149),.UNSPECIFIED.,.F.,.F.,(4,3,3,3,
3,3,3,3,3,3,3,3,3,3,3,3,3,3,3,3,3,3,3,3,3,3,3,3,3,3,3,3,3,3,3,3,3,3,3,3,
3,3,3,3,3,3,3,3,3,3,3,3,3,3,3,3,3,3,3,3,3,3,3,3,3,3,3,3,3,3,3,3,3,3,3,3,
3,3,4),(-60.401723218827,-60.3220092933395,-60.2422614639156,-60.1624718065184,
-60.0826323710433,-60.002695033114,-59.9227035170359,-59.8426133993631,
-59.816225196907,-59.7372333015685,-59.6583415168936,-59.5795392608493,
-59.5008392600278,-59.4221998141494,-59.3436235319641,-59.3177566535994,
-59.2391699304359,-59.1605337631728,-59.0818377698565,-59.0030237383736,
-58.9241423101499,-58.845139216934,-58.8192881102918,-58.7402155885422,
-58.6612160338072,-58.5822777659832,-58.5033891515018,-58.4245385949456,
-58.3457100906799,-58.2668937168111,-58.1880789656273,-58.1092553316499,
-58.0303852841016,-57.9514916050257,-57.8725310801887,-57.8223510236767,
-57.7482455855748,-57.6741970877203,-57.6001903497133,-57.5262010855606,
-57.4522237239486,-57.3782214379155,-57.3238824803692,-57.2328833806335,
-57.1413801629565,-57.0494366240264,-56.9574020468475,-56.8654929567266,
-56.8254139370616,-56.7497042659439,-56.674043263918,-56.5984164235803,
-56.5227987272979,-56.4471872272111,-56.3715473025833,-56.326945393754,
-56.2446666219008,-56.1623640590383,-56.0788922568903,-55.9965373019925,
-55.9125070762195,-55.8284768504465,-55.7460978398443,-55.6637336505946,
-55.5803023147307,-55.4979803414377,-55.4139943242883,-55.3300083071389,
-55.2543681979176,-55.1787520950117,-55.103145527958,-55.0275108652487,
-54.9518613066711,-54.8761510168944,-54.8315397638314,-54.7395871468826,
-54.6475551712311,-54.5557033213318,-54.4741437745622),.UNSPECIFIED.);
#3143=B_SPLINE_CURVE_WITH_KNOTS('',3,(#157155,#157156,#157157,#157158,#157159,
#157160,#157161,#157162,#157163,#157164,#157165,#157166,#157167,#157168,
#157169,#157170,#157171,#157172,#157173,#157174,#157175,#157176,#157177,
#157178,#157179,#157180,#157181,#157182,#157183,#157184,#157185,#157186,
#157187,#157188,#157189,#157190,#157191,#157192,#157193,#157194,#157195,
#157196,#157197,#157198,#157199,#157200,#157201,#157202,#157203,#157204,
#157205,#157206,#157207,#157208,#157209,#157210,#157211,#157212,#157213,
#157214,#157215,#157216,#157217,#157218,#157219,#157220,#157221,#157222,
#157223,#157224,#157225,#157226,#157227,#157228,#157229,#157230,#157231,
#157232,#157233,#157234,#157235,#157236,#157237,#157238,#157239,#157240,
#157241,#157242,#157243,#157244,#157245,#157246,#157247,#157248,#157249,
#157250,#157251,#157252,#157253,#157254,#157255,#157256,#157257,#157258,
#157259,#157260,#157261,#157262,#157263,#157264,#157265,#157266,#157267,
#157268,#157269,#157270,#157271,#157272,#157273,#157274,#157275,#157276,
#157277,#157278,#157279,#157280,#157281,#157282,#157283,#157284,#157285,
#157286,#157287,#157288,#157289,#157290,#157291,#157292,#157293,#157294,
#157295,#157296,#157297,#157298,#157299,#157300,#157301,#157302,#157303,
#157304,#157305,#157306,#157307,#157308,#157309,#157310,#157311,#157312,
#157313,#157314,#157315,#157316,#157317,#157318,#157319,#157320,#157321,
#157322,#157323,#157324,#157325,#157326,#157327,#157328,#157329,#157330,
#157331,#157332,#157333,#157334,#157335,#157336,#157337,#157338,#157339,
#157340,#157341,#157342,#157343,#157344,#157345,#157346,#157347,#157348,
#157349,#157350,#157351,#157352,#157353,#157354,#157355,#157356,#157357,
#157358,#157359,#157360,#157361,#157362,#157363,#157364,#157365,#157366,
#157367,#157368,#157369,#157370,#157371,#157372,#157373,#157374,#157375,
#157376,#157377,#157378,#157379,#157380,#157381,#157382,#157383,#157384,
#157385,#157386,#157387,#157388,#157389,#157390,#157391,#157392),
 .UNSPECIFIED.,.F.,.F.,(4,3,3,3,3,3,3,3,3,3,3,3,3,3,3,3,3,3,3,3,3,3,3,3,
3,3,3,3,3,3,3,3,3,3,3,3,3,3,3,3,3,3,3,3,3,3,3,3,3,3,3,3,3,3,3,3,3,3,3,3,
3,3,3,3,3,3,3,3,3,3,3,3,3,3,3,3,3,3,3,4),(51.9314713010136,52.010349088432,
52.0925610781474,52.1712486835971,52.2498775775425,52.3284465749947,52.3391970472936,
52.4177837704572,52.4964199377203,52.575115931037,52.6539299625199,52.7328113907437,
52.8118144839596,52.8376655906012,52.9167381123508,52.9957376670859,53.0746759349099,
53.1535645493913,53.2324151059476,53.3112436102133,53.3900599840822,53.4688747352658,
53.5476983692433,53.6265684167916,53.7054620958675,53.7844226207045,53.8346026772163,
53.9087081153182,53.9827566131727,54.0567633511797,54.1307526153323,54.2047299769443,
54.2787322629774,54.3330712205238,54.4240703202597,54.5155735379368,54.6075170768671,
54.6995516540461,54.7914607441672,54.8315397638314,54.9072494349489,54.9829104369747,
55.0585372773123,55.1341549735946,55.2097664736812,55.2854063983089,55.3300083071389,
55.4122870789922,55.494589641855,55.5780614440028,55.6604163989009,55.7444466246737,
55.8284768504465,55.9108558610486,55.9932200502983,56.0766513861622,56.1589733594553,
56.2429593766047,56.3269453937541,56.4025855029753,56.4782016058812,56.5538081729345,
56.6294428356438,56.7050923942214,56.780802683998,56.8254139370616,56.9173145067649,
57.009347476479,57.1012270463014,57.1928544423309,57.2838755638127,57.3238824803692,
57.3978843950572,57.4718653234005,57.5458403453128,57.6198528186127,57.6938840885939,
57.7679888407988,57.8223510236767,57.8577774557529),.UNSPECIFIED.);
#3144=B_SPLINE_CURVE_WITH_KNOTS('',3,(#157393,#157394,#157395,#157396,#157397,
#157398,#157399,#157400,#157401,#157402,#157403,#157404,#157405,#157406,
#157407,#157408),.UNSPECIFIED.,.F.,.F.,(4,3,3,3,3,4),(57.8577774558344,
57.9362807382,58.014711565424,58.0930995598951,58.17145295758,58.2138923057233),
 .UNSPECIFIED.);
#3145=B_SPLINE_CURVE_WITH_KNOTS('',3,(#157410,#157411,#157412,#157413,#157414,
#157415,#157416,#157417,#157418,#157419,#157420,#157421,#157422,#157423,
#157424,#157425),.UNSPECIFIED.,.F.,.F.,(4,3,3,3,3,4),(-54.4741437745622,
-54.3830887300197,-54.3330712205238,-54.2623508425394,-54.1904443771559,
-54.1185379117723),.UNSPECIFIED.);
#3146=B_SPLINE_CURVE_WITH_KNOTS('',3,(#157426,#157427,#157428,#157429,#157430,
#157431,#157432,#157433,#157434,#157435,#157436,#157437,#157438,#157439,
#157440,#157441,#157442,#157443,#157444,#157445,#157446,#157447,#157448,
#157449,#157450,#157451,#157452,#157453,#157454,#157455,#157456,#157457,
#157458,#157459,#157460,#157461,#157462,#157463,#157464,#157465,#157466,
#157467,#157468,#157469,#157470,#157471,#157472,#157473,#157474,#157475,
#157476,#157477,#157478,#157479,#157480,#157481,#157482,#157483,#157484,
#157485,#157486,#157487,#157488,#157489,#157490,#157491,#157492,#157493,
#157494,#157495,#157496,#157497,#157498,#157499,#157500,#157501,#157502,
#157503,#157504,#157505,#157506,#157507,#157508,#157509,#157510,#157511,
#157512,#157513,#157514,#157515,#157516,#157517,#157518,#157519,#157520,
#157521,#157522,#157523,#157524,#157525,#157526,#157527,#157528,#157529,
#157530,#157531,#157532,#157533,#157534,#157535,#157536,#157537,#157538,
#157539,#157540,#157541,#157542,#157543,#157544,#157545,#157546,#157547,
#157548,#157549,#157550,#157551,#157552,#157553,#157554,#157555,#157556,
#157557,#157558,#157559,#157560,#157561,#157562,#157563,#157564,#157565,
#157566,#157567,#157568,#157569,#157570,#157571,#157572,#157573,#157574,
#157575,#157576,#157577,#157578,#157579,#157580,#157581,#157582,#157583,
#157584,#157585,#157586,#157587,#157588,#157589,#157590,#157591,#157592,
#157593,#157594,#157595,#157596,#157597,#157598,#157599,#157600,#157601,
#157602,#157603,#157604,#157605,#157606,#157607,#157608,#157609,#157610,
#157611,#157612,#157613,#157614,#157615,#157616,#157617,#157618,#157619,
#157620,#157621,#157622,#157623,#157624,#157625,#157626,#157627,#157628,
#157629,#157630,#157631,#157632,#157633,#157634,#157635,#157636,#157637,
#157638,#157639,#157640,#157641,#157642,#157643,#157644,#157645,#157646,
#157647,#157648,#157649,#157650,#157651,#157652,#157653,#157654,#157655,
#157656,#157657,#157658,#157659,#157660,#157661,#157662,#157663),
 .UNSPECIFIED.,.F.,.F.,(4,3,3,3,3,3,3,3,3,3,3,3,3,3,3,3,3,3,3,3,3,3,3,3,
3,3,3,3,3,3,3,3,3,3,3,3,3,3,3,3,3,3,3,3,3,3,3,3,3,3,3,3,3,3,3,3,3,3,3,3,
3,3,3,3,3,3,3,3,3,3,3,3,3,3,3,3,3,3,3,4),(-54.1185379116474,-54.0396932861478,
-53.9607819726184,-53.881740071316,-53.8346026772163,-53.755641261269,-53.6767338381998,
-53.5978687992631,-53.5190345685371,-53.4402195945583,-53.3613983308981,
-53.2825716917857,-53.2037291674094,-53.1248602388266,-53.0459181874951,
-52.9669374220063,-52.8878664109882,-52.8376655906011,-52.7586736952626,
-52.6797819105877,-52.6009796545436,-52.5222796537221,-52.4436402078436,
-52.3650639256585,-52.3391970472936,-52.2606103241301,-52.1819741568671,
-52.1032781635508,-52.024464132068,-51.9455827038444,-51.8665796106285,
-51.840728503986,-51.7616559822364,-51.6826564275014,-51.6037181596773,
-51.524829545196,-51.4459789886397,-51.367150484374,-51.2883341105051,-51.2095193593214,
-51.1306957253439,-51.0518256777956,-50.9729319987198,-50.8939714738828,
-50.8437914173709,-50.7696859792689,-50.6956374814144,-50.6216307434073,
-50.5476414792546,-50.4736641176425,-50.3996618316093,-50.3453228740633,
-50.2543237743278,-50.162820556651,-50.0708770177211,-49.9788424405425,
-49.8869333504217,-49.8468543307558,-49.7711446596381,-49.6954836576122,
-49.6198568172745,-49.544239120992,-49.4686276209053,-49.3929876962775,
-49.3483857874482,-49.266107015595,-49.1838044527324,-49.1003326505845,
-49.0179776956867,-48.9339474699137,-48.8499172441407,-48.7675382335386,
-48.685174044289,-48.601742708425,-48.519420735132,-48.4354347179826,-48.3514487008331,
-48.2758079681556,-48.2001936861576,-48.1916415759627),.UNSPECIFIED.);
#3147=B_SPLINE_CURVE_WITH_KNOTS('',3,(#157669,#157670,#157671,#157672,#157673,
#157674,#157675,#157676,#157677,#157678,#157679,#157680,#157681,#157682,
#157683,#157684,#157685,#157686,#157687,#157688,#157689,#157690,#157691,
#157692,#157693,#157694,#157695,#157696,#157697,#157698,#157699,#157700,
#157701,#157702,#157703,#157704,#157705,#157706,#157707,#157708,#157709,
#157710,#157711,#157712,#157713,#157714,#157715,#157716,#157717,#157718,
#157719,#157720,#157721,#157722,#157723,#157724,#157725,#157726,#157727,
#157728,#157729,#157730,#157731,#157732,#157733,#157734,#157735,#157736,
#157737,#157738,#157739,#157740,#157741,#157742,#157743,#157744,#157745,
#157746,#157747,#157748,#157749,#157750,#157751,#157752,#157753,#157754,
#157755,#157756,#157757,#157758,#157759,#157760,#157761,#157762,#157763,
#157764,#157765,#157766,#157767,#157768,#157769,#157770,#157771,#157772,
#157773,#157774,#157775,#157776,#157777,#157778,#157779,#157780,#157781,
#157782,#157783,#157784,#157785,#157786,#157787,#157788,#157789,#157790,
#157791,#157792,#157793,#157794,#157795,#157796,#157797,#157798,#157799,
#157800,#157801,#157802,#157803,#157804,#157805,#157806,#157807,#157808,
#157809,#157810,#157811,#157812,#157813,#157814,#157815,#157816,#157817,
#157818,#157819,#157820,#157821,#157822,#157823,#157824,#157825,#157826,
#157827,#157828,#157829,#157830,#157831,#157832,#157833,#157834,#157835,
#157836,#157837,#157838,#157839,#157840,#157841,#157842,#157843,#157844,
#157845,#157846,#157847,#157848,#157849,#157850,#157851,#157852,#157853,
#157854,#157855,#157856,#157857,#157858,#157859,#157860,#157861,#157862,
#157863,#157864,#157865,#157866,#157867,#157868,#157869,#157870,#157871,
#157872,#157873,#157874,#157875,#157876,#157877,#157878,#157879,#157880,
#157881,#157882,#157883,#157884,#157885,#157886,#157887,#157888,#157889,
#157890,#157891,#157892,#157893,#157894,#157895,#157896,#157897,#157898,
#157899,#157900,#157901,#157902,#157903),.UNSPECIFIED.,.F.,.F.,(4,3,3,3,
3,3,3,3,3,3,3,3,3,3,3,3,3,3,3,3,3,3,3,3,3,3,3,3,3,3,3,3,3,3,3,3,3,3,3,3,
3,3,3,3,3,3,3,3,3,3,3,3,3,3,3,3,3,3,3,3,3,3,3,3,3,3,3,3,3,3,3,3,3,3,3,3,
3,3,4),(45.6468212085296,45.7256771159923,45.8046642745895,45.8591059842953,
45.938178506045,46.0171780607802,46.0961163286042,46.1750049430857,46.2538554996418,
46.3326840039076,46.4115003777766,46.4903151289606,46.5691387629384,46.6480088104868,
46.7269024895627,46.8058630143996,46.8560430709105,46.9301485090125,47.004197006867,
47.0782037448741,47.1521930090267,47.2261703706386,47.3001726566718,47.354511614218,
47.4455107139543,47.5370139316309,47.6289574705612,47.7209920477399,47.8129011378603,
47.8529801575256,47.9286898286431,48.0043508306691,48.0799776710068,48.1555953672892,
48.2312068673758,48.3068467920036,48.3514487008331,48.4337274726864,48.5160300355491,
48.599501837697,48.681856792595,48.7658870183678,48.8499172441407,48.9322962547427,
49.0146604439924,49.0980917798564,49.1804137531494,49.2643997702988,49.3483857874483,
49.4240258966695,49.4996419995754,49.5752485666291,49.6508832293383,49.726532787916,
49.8022430776929,49.8468543307558,49.9387549004592,50.030787870172,50.1226674399944,
50.2142948360256,50.3053159575074,50.3453228740634,50.4193247887513,50.4933057170947,
50.5672807390074,50.6412932123071,50.7153244822882,50.789429234493,50.8437914173709,
50.9222508834037,51.0037935415499,51.0821383235146,51.1604532036749,51.2387496665986,
51.3170391836195,51.3953501369081,51.4736731259674,51.552038685281,51.5745921485733),
 .UNSPECIFIED.);
#3148=B_SPLINE_CURVE_WITH_KNOTS('',3,(#157904,#157905,#157906,#157907,#157908,
#157909,#157910,#157911,#157912,#157913,#157914,#157915,#157916,#157917,
#157918,#157919),.UNSPECIFIED.,.F.,.F.,(4,3,3,3,3,4),(51.5745921486873,
51.6725058707897,51.7717369862272,51.8407285039861,51.9197400789197,51.9314713010136),
 .UNSPECIFIED.);
#3149=B_SPLINE_CURVE_WITH_KNOTS('',3,(#157921,#157922,#157923,#157924,#157925,
#157926,#157927,#157928,#157929,#157930,#157931,#157932,#157933,#157934,
#157935,#157936,#157937,#157938,#157939),.UNSPECIFIED.,.F.,.F.,(4,3,3,3,
3,3,4),(-48.1916415759627,-48.1160351770241,-48.0403994804095,-47.964747421664,
-47.8890357469598,-47.8529801575256,-47.8353526044678),.UNSPECIFIED.);
#3150=B_SPLINE_CURVE_WITH_KNOTS('',3,(#157940,#157941,#157942,#157943,#157944,
#157945,#157946,#157947,#157948,#157949,#157950,#157951,#157952,#157953,
#157954,#157955,#157956,#157957,#157958,#157959,#157960,#157961,#157962,
#157963,#157964,#157965,#157966,#157967,#157968,#157969,#157970,#157971,
#157972,#157973,#157974,#157975,#157976,#157977,#157978,#157979,#157980,
#157981,#157982,#157983,#157984,#157985,#157986,#157987,#157988,#157989,
#157990,#157991,#157992,#157993,#157994,#157995,#157996,#157997,#157998,
#157999,#158000,#158001,#158002,#158003,#158004,#158005,#158006,#158007,
#158008,#158009,#158010,#158011,#158012,#158013,#158014,#158015,#158016,
#158017,#158018,#158019,#158020,#158021,#158022,#158023,#158024,#158025,
#158026,#158027,#158028,#158029,#158030,#158031,#158032,#158033,#158034,
#158035,#158036,#158037,#158038,#158039,#158040,#158041,#158042,#158043,
#158044,#158045,#158046,#158047,#158048,#158049,#158050,#158051,#158052,
#158053,#158054,#158055,#158056,#158057,#158058,#158059,#158060,#158061,
#158062,#158063,#158064,#158065,#158066,#158067,#158068,#158069,#158070,
#158071,#158072,#158073,#158074,#158075,#158076,#158077,#158078,#158079,
#158080,#158081,#158082,#158083,#158084,#158085,#158086,#158087,#158088,
#158089,#158090,#158091,#158092,#158093,#158094,#158095,#158096,#158097,
#158098,#158099,#158100,#158101,#158102,#158103,#158104,#158105,#158106,
#158107,#158108,#158109,#158110,#158111,#158112,#158113,#158114,#158115,
#158116,#158117,#158118,#158119,#158120,#158121,#158122,#158123,#158124,
#158125,#158126,#158127,#158128,#158129,#158130,#158131,#158132,#158133,
#158134,#158135,#158136,#158137,#158138,#158139,#158140,#158141,#158142,
#158143,#158144,#158145,#158146,#158147,#158148,#158149,#158150,#158151,
#158152,#158153,#158154,#158155,#158156,#158157,#158158,#158159,#158160,
#158161,#158162,#158163,#158164,#158165,#158166,#158167,#158168,#158169,
#158170,#158171,#158172,#158173,#158174,#158175,#158176,#158177),
 .UNSPECIFIED.,.F.,.F.,(4,3,3,3,3,3,3,3,3,3,3,3,3,3,3,3,3,3,3,3,3,3,3,3,
3,3,3,3,3,3,3,3,3,3,3,3,3,3,3,3,3,3,3,3,3,3,3,3,3,3,3,3,3,3,3,3,3,3,3,3,
3,3,3,3,3,3,3,3,3,3,3,3,3,3,3,3,3,3,3,4),(-47.8353526043918,-47.7438818493918,
-47.6523361208125,-47.5609865054093,-47.4698969508807,-47.3793718635444,
-47.354511614218,-47.2805096995299,-47.2065287711865,-47.132553749274,-47.0585412759741,
-46.9845100059928,-46.9104052537878,-46.8560430709104,-46.7770816549632,
-46.698174231894,-46.6193091929574,-46.5404749622316,-46.4616599882529,
-46.3828387245927,-46.3040120854804,-46.225169561104,-46.1463006325212,
-46.0673585811898,-45.9883778157009,-45.9093068046828,-45.8591059842953,
-45.7801140889568,-45.7012223042821,-45.622420048238,-45.5437200474165,
-45.4650806015379,-45.3865043193528,-45.3606374409878,-45.2820507178242,
-45.2034145505611,-45.1247185572446,-45.0459045257617,-44.967023097538,
-44.888020004322,-44.8621688976802,-44.7830963759306,-44.7040968211956,
-44.6251585533716,-44.5462699388903,-44.467419382334,-44.3885908780683,
-44.3097745041995,-44.2309597530157,-44.1521361190383,-44.07326607149,-43.9943723924142,
-43.9154118675772,-43.8652318110651,-43.7911263729631,-43.7170778751086,
-43.6430711371015,-43.5690818729488,-43.4951045113367,-43.4211022253034,
-43.3667632677575,-43.2757641680218,-43.184260950345,-43.0923174114152,
-43.0002828342366,-42.9083737441158,-42.86829472445,-42.7925850533323,-42.7169240513064,
-42.6412972109688,-42.5656795146863,-42.4900680145996,-42.4144280899718,
-42.3698261811424,-42.2875502010023,-42.2052500532836,-42.1229103589057,
-42.0405596721461,-41.9581865681693,-41.9084162677792),.UNSPECIFIED.);
#3151=B_SPLINE_CURVE_WITH_KNOTS('',3,(#158183,#158184,#158185,#158186,#158187,
#158188,#158189,#158190,#158191,#158192,#158193,#158194,#158195,#158196,
#158197,#158198,#158199,#158200,#158201,#158202,#158203,#158204,#158205,
#158206,#158207,#158208,#158209,#158210,#158211,#158212,#158213,#158214,
#158215,#158216,#158217,#158218,#158219,#158220,#158221,#158222,#158223,
#158224,#158225,#158226,#158227,#158228,#158229,#158230,#158231,#158232,
#158233,#158234,#158235,#158236,#158237,#158238,#158239,#158240,#158241,
#158242,#158243,#158244,#158245,#158246,#158247,#158248,#158249,#158250,
#158251,#158252,#158253,#158254,#158255,#158256,#158257,#158258,#158259,
#158260,#158261,#158262,#158263,#158264,#158265,#158266,#158267,#158268,
#158269,#158270,#158271,#158272,#158273,#158274,#158275,#158276,#158277,
#158278,#158279,#158280,#158281,#158282,#158283,#158284,#158285,#158286,
#158287,#158288,#158289,#158290,#158291,#158292,#158293,#158294,#158295,
#158296,#158297,#158298,#158299,#158300,#158301,#158302,#158303,#158304,
#158305,#158306,#158307,#158308,#158309,#158310,#158311,#158312,#158313,
#158314,#158315,#158316,#158317,#158318,#158319,#158320,#158321,#158322,
#158323,#158324,#158325,#158326,#158327,#158328,#158329,#158330,#158331,
#158332,#158333,#158334,#158335,#158336,#158337,#158338,#158339,#158340,
#158341,#158342,#158343,#158344,#158345,#158346,#158347,#158348,#158349,
#158350,#158351,#158352,#158353,#158354,#158355,#158356,#158357,#158358,
#158359,#158360,#158361,#158362,#158363,#158364,#158365,#158366,#158367,
#158368,#158369,#158370,#158371,#158372,#158373,#158374,#158375,#158376,
#158377,#158378,#158379,#158380,#158381,#158382,#158383,#158384,#158385,
#158386,#158387,#158388,#158389,#158390,#158391,#158392,#158393,#158394,
#158395,#158396,#158397,#158398,#158399,#158400,#158401,#158402,#158403,
#158404,#158405,#158406,#158407,#158408,#158409,#158410,#158411,#158412,
#158413,#158414,#158415,#158416,#158417),.UNSPECIFIED.,.F.,.F.,(4,3,3,3,
3,3,3,3,3,3,3,3,3,3,3,3,3,3,3,3,3,3,3,3,3,3,3,3,3,3,3,3,3,3,3,3,3,3,3,3,
3,3,3,3,3,3,3,3,3,3,3,3,3,3,3,3,3,3,3,3,3,3,3,3,3,3,3,3,3,3,3,3,3,3,3,3,
3,3,4),(39.3650750661798,39.4428973253601,39.520713993561,39.5985373278778,
39.6764073153725,39.7543022948959,39.8322681440181,39.8774834646046,39.9515889027065,
40.025637400561,40.0996441385683,40.173633402721,40.247610764333,40.3216130503661,
40.3759520079122,40.4669511076482,40.5584543253243,40.6503978642546,40.7424324414336,
40.8343415315547,40.8744205512198,40.9501302223373,41.025791224363,41.1014180647006,
41.1770357609829,41.2526472610696,41.3282871856971,41.3728890945273,41.4551678663805,
41.5374704292436,41.6209422313914,41.7032971862895,41.7873274120622,41.8713576378349,
41.9537366484368,42.0361008376866,42.1195321735505,42.2018541468433,42.2858401639928,
42.3698261811424,42.4454662903638,42.5210823932697,42.5966889603235,42.672323623033,
42.7479731816105,42.8236834713872,42.86829472445,42.9601952941527,43.0522282638671,
43.1441078336892,43.2357352297184,43.3267563511995,43.3667632677576,43.4407651824456,
43.5147461107889,43.5887211327014,43.6627336060013,43.7367648759821,43.810869628187,
43.8652318110651,43.9441932270122,44.0231006500812,44.1019656890176,44.1807999197432,
44.2596148937224,44.3384361573826,44.4172627964949,44.4961053208715,44.5749742494545,
44.653916300786,44.732897066275,44.8119680772932,44.8621688976802,44.9426880221432,
45.0230879351252,45.1033329860329,45.183484530017,45.2635184145895,45.2914068413062),
 .UNSPECIFIED.);
#3152=B_SPLINE_CURVE_WITH_KNOTS('',3,(#158418,#158419,#158420,#158421,#158422,
#158423,#158424,#158425,#158426,#158427,#158428,#158429,#158430,#158431,
#158432,#158433),.UNSPECIFIED.,.F.,.F.,(4,3,3,3,3,4),(45.2914068413937,
45.3606374409878,45.4392344513366,45.5178699470115,45.5965949508927,45.6468212085296),
 .UNSPECIFIED.);
#3153=B_SPLINE_CURVE_WITH_KNOTS('',3,(#158435,#158436,#158437,#158438,#158439,
#158440,#158441,#158442,#158443,#158444,#158445,#158446,#158447,#158448,
#158449,#158450),.UNSPECIFIED.,.F.,.F.,(4,3,3,3,3,4),(-41.9084162677792,
-41.8713576378349,-41.7898517304649,-41.7083640391987,-41.6268883973049,
-41.5521672972882),.UNSPECIFIED.);
#3154=B_SPLINE_CURVE_WITH_KNOTS('',3,(#158451,#158452,#158453,#158454,#158455,
#158456,#158457,#158458,#158459,#158460,#158461,#158462,#158463,#158464,
#158465,#158466,#158467,#158468,#158469,#158470,#158471,#158472,#158473,
#158474,#158475,#158476,#158477,#158478,#158479,#158480,#158481,#158482,
#158483,#158484,#158485,#158486,#158487,#158488,#158489,#158490,#158491,
#158492,#158493,#158494,#158495,#158496,#158497,#158498,#158499,#158500,
#158501,#158502,#158503,#158504,#158505,#158506,#158507,#158508,#158509,
#158510,#158511,#158512,#158513,#158514,#158515,#158516,#158517,#158518,
#158519,#158520,#158521,#158522,#158523,#158524,#158525,#158526,#158527,
#158528,#158529,#158530,#158531,#158532,#158533,#158534,#158535,#158536,
#158537,#158538,#158539,#158540,#158541,#158542,#158543,#158544,#158545,
#158546,#158547,#158548,#158549,#158550,#158551,#158552,#158553,#158554,
#158555,#158556,#158557,#158558,#158559,#158560,#158561,#158562,#158563,
#158564,#158565,#158566,#158567,#158568,#158569,#158570,#158571,#158572,
#158573,#158574,#158575,#158576,#158577,#158578,#158579,#158580,#158581,
#158582,#158583,#158584,#158585,#158586,#158587,#158588,#158589,#158590,
#158591,#158592,#158593,#158594,#158595,#158596,#158597,#158598,#158599,
#158600,#158601,#158602,#158603,#158604,#158605,#158606,#158607,#158608,
#158609,#158610,#158611,#158612,#158613,#158614,#158615,#158616,#158617,
#158618,#158619,#158620,#158621,#158622,#158623,#158624,#158625,#158626,
#158627,#158628,#158629,#158630,#158631,#158632,#158633,#158634,#158635,
#158636,#158637,#158638,#158639,#158640,#158641,#158642,#158643,#158644,
#158645,#158646,#158647,#158648,#158649,#158650,#158651,#158652,#158653,
#158654,#158655,#158656,#158657,#158658,#158659,#158660,#158661,#158662,
#158663,#158664,#158665,#158666,#158667,#158668,#158669,#158670,#158671,
#158672,#158673,#158674,#158675,#158676,#158677,#158678,#158679,#158680,
#158681,#158682,#158683,#158684,#158685,#158686,#158687,#158688),
 .UNSPECIFIED.,.F.,.F.,(4,3,3,3,3,3,3,3,3,3,3,3,3,3,3,3,3,3,3,3,3,3,3,3,
3,3,3,3,3,3,3,3,3,3,3,3,3,3,3,3,3,3,3,3,3,3,3,3,3,3,3,3,3,3,3,3,3,3,3,3,
3,3,3,3,3,3,3,3,3,3,3,3,3,3,3,3,3,3,3,4),(-41.5521672972882,-41.4625281959078,
-41.3728890945273,-41.2972489853062,-41.2216328824004,-41.1460263153471,
-41.0703916526379,-40.9947420940603,-40.9190318042837,-40.8744205512198,
-40.7825199815166,-40.6904870118016,-40.5986074419793,-40.5069800459494,
-40.4159589244676,-40.3759520079122,-40.3019500932241,-40.2279691648807,
-40.1539941429681,-40.0799816696681,-40.0059503996867,-39.9318456474817,
-39.8774834646046,-39.7985220486573,-39.7196146255882,-39.6407495866517,
-39.5619153559262,-39.4831003819476,-39.4042791182875,-39.3254524791752,
-39.2466099547988,-39.1677410262161,-39.0887989748847,-39.0098182093957,
-38.9307471983775,-38.8805463779895,-38.801554482651,-38.7226626979764,
-38.6438604419319,-38.5651604411105,-38.4865209952314,-38.4079447130463,
-38.382077834682,-38.3034911115186,-38.2248549442554,-38.1461589509396,
-38.0673449194569,-37.9884634912329,-37.9094603980172,-37.8836092913744,
-37.8045367696248,-37.7255372148899,-37.6465989470658,-37.5677103325842,
-37.4888597760277,-37.410031271762,-37.3312148978932,-37.2524001467095,
-37.1735765127321,-37.0947064651839,-37.0158127861082,-36.9368522612713,
-36.8866722047593,-36.8125667666573,-36.7385182688028,-36.6645115307967,
-36.590522266644,-36.5165449050318,-36.4425426189986,-36.3882036614517,
-36.2972045617156,-36.2057013440403,-36.1137578051107,-36.0217232279321,
-35.9298141378113,-35.8897351181442,-35.814026435445,-35.7383644598627,
-35.6627367767685,-35.6249640953535),.UNSPECIFIED.);
#3155=B_SPLINE_CURVE_WITH_KNOTS('',3,(#158694,#158695,#158696,#158697,#158698,
#158699,#158700,#158701,#158702,#158703,#158704,#158705,#158706,#158707,
#158708,#158709,#158710,#158711,#158712,#158713,#158714,#158715,#158716,
#158717,#158718,#158719,#158720,#158721,#158722,#158723,#158724,#158725,
#158726,#158727,#158728,#158729,#158730,#158731,#158732,#158733,#158734,
#158735,#158736,#158737,#158738,#158739,#158740,#158741,#158742,#158743,
#158744,#158745,#158746,#158747,#158748,#158749,#158750,#158751,#158752,
#158753,#158754,#158755,#158756,#158757,#158758,#158759,#158760,#158761,
#158762,#158763,#158764,#158765,#158766,#158767,#158768,#158769,#158770,
#158771,#158772,#158773,#158774,#158775,#158776,#158777,#158778,#158779,
#158780,#158781,#158782,#158783,#158784,#158785,#158786,#158787,#158788,
#158789,#158790,#158791,#158792,#158793,#158794,#158795,#158796,#158797,
#158798,#158799,#158800,#158801,#158802,#158803,#158804,#158805,#158806,
#158807,#158808,#158809,#158810,#158811,#158812,#158813,#158814,#158815,
#158816,#158817,#158818,#158819,#158820,#158821,#158822,#158823,#158824,
#158825,#158826,#158827,#158828,#158829,#158830,#158831,#158832,#158833,
#158834,#158835,#158836,#158837,#158838,#158839,#158840,#158841,#158842,
#158843,#158844,#158845,#158846,#158847,#158848,#158849,#158850,#158851,
#158852,#158853,#158854,#158855,#158856,#158857,#158858,#158859,#158860,
#158861,#158862,#158863,#158864,#158865,#158866,#158867,#158868,#158869,
#158870,#158871,#158872,#158873,#158874,#158875,#158876,#158877,#158878,
#158879,#158880,#158881,#158882,#158883,#158884,#158885,#158886,#158887,
#158888,#158889,#158890,#158891,#158892,#158893,#158894,#158895,#158896,
#158897,#158898,#158899,#158900,#158901,#158902,#158903,#158904,#158905,
#158906,#158907,#158908,#158909,#158910,#158911,#158912,#158913,#158914,
#158915,#158916,#158917,#158918,#158919,#158920,#158921,#158922,#158923,
#158924,#158925,#158926,#158927,#158928),.UNSPECIFIED.,.F.,.F.,(4,3,3,3,
3,3,3,3,3,3,3,3,3,3,3,3,3,3,3,3,3,3,3,3,3,3,3,3,3,3,3,3,3,3,3,3,3,3,3,3,
3,3,3,3,3,3,3,3,3,3,3,3,3,3,3,3,3,3,3,3,3,3,3,3,3,3,3,3,3,3,3,3,3,3,3,3,
3,3,4),(33.0816676322956,33.1556600429916,33.2296420595945,33.3036185021859,
33.3776189751015,33.3973924016064,33.4883915013423,33.5798947190199,33.6718382579498,
33.7638728351289,33.8557819252498,33.895860944914,33.9715706160315,34.0472316180573,
34.1228584583949,34.1984761546772,34.2740876547638,34.3497275793915,34.3943294882215,
34.4766082600749,34.5589108229377,34.6423826250856,34.7247375799837,34.8087678057564,
34.8927980315291,34.975177042131,35.0575412313805,35.1409725672445,35.2232945405373,
35.3072805576869,35.3912665748366,35.466906684058,35.5425227869641,35.6181293540178,
35.6937640167273,35.769413575305,35.8451238650819,35.8897351181442,35.981635687847,
36.0736686575608,36.1655482273828,36.2571756234118,36.3481967448931,36.3882036614517,
36.4622055761398,36.5361865044833,36.6101615263958,36.6841739996958,36.7582052696771,
36.8323100218821,36.8866722047593,36.9656336207065,37.0445410437757,37.1234060827122,
37.2022403134381,37.2810552874168,37.359876551077,37.4387031901894,37.5175457145658,
37.5964146431485,37.6753566944799,37.7543374599686,37.8334084709867,37.8836092913744,
37.962601186713,38.0414929713878,38.120295227432,38.1989952282536,38.2776346741321,
38.3562109563174,38.382077834682,38.4606645578453,38.5393007251084,38.6179967184244,
38.696810749907,38.7756921781308,38.8546952713465,38.8805463779895,39.0082215342141),
 .UNSPECIFIED.);
#3156=B_SPLINE_CURVE_WITH_KNOTS('',3,(#158929,#158930,#158931,#158932,#158933,
#158934,#158935,#158936,#158937,#158938,#158939,#158940,#158941,#158942,
#158943,#158944),.UNSPECIFIED.,.F.,.F.,(4,3,3,3,3,4),(39.0082215342936,
39.0862558873874,39.1642044673432,39.2421030021683,39.3199578461465,39.3650750661798),
 .UNSPECIFIED.);
#3157=B_SPLINE_CURVE_WITH_KNOTS('',3,(#158946,#158947,#158948,#158949,#158950,
#158951,#158952,#158953,#158954,#158955,#158956,#158957,#158958,#158959,
#158960,#158961),.UNSPECIFIED.,.F.,.F.,(4,3,3,3,3,4),(-35.6249640953535,
-35.5493511139821,-35.4703088444094,-35.3912665748366,-35.3016062240681,
-35.2689819901086),.UNSPECIFIED.);
#3158=B_SPLINE_CURVE_WITH_KNOTS('',3,(#158962,#158963,#158964,#158965,#158966,
#158967,#158968,#158969,#158970,#158971,#158972,#158973,#158974,#158975,
#158976,#158977,#158978,#158979,#158980,#158981,#158982,#158983,#158984,
#158985,#158986,#158987,#158988,#158989,#158990,#158991,#158992,#158993,
#158994,#158995,#158996,#158997,#158998,#158999,#159000,#159001,#159002,
#159003,#159004,#159005,#159006,#159007,#159008,#159009,#159010,#159011,
#159012,#159013,#159014,#159015,#159016,#159017,#159018,#159019,#159020,
#159021,#159022,#159023,#159024,#159025,#159026,#159027,#159028,#159029,
#159030,#159031,#159032,#159033,#159034,#159035,#159036,#159037,#159038,
#159039,#159040,#159041,#159042,#159043,#159044,#159045,#159046,#159047,
#159048,#159049,#159050,#159051,#159052,#159053,#159054,#159055,#159056,
#159057,#159058,#159059,#159060,#159061,#159062,#159063,#159064,#159065,
#159066,#159067,#159068,#159069,#159070,#159071,#159072,#159073,#159074,
#159075,#159076,#159077,#159078,#159079,#159080,#159081,#159082,#159083,
#159084,#159085,#159086,#159087,#159088,#159089,#159090,#159091,#159092,
#159093,#159094,#159095,#159096,#159097,#159098,#159099,#159100,#159101,
#159102,#159103,#159104,#159105,#159106,#159107,#159108,#159109,#159110,
#159111,#159112,#159113,#159114,#159115,#159116,#159117,#159118,#159119,
#159120,#159121,#159122,#159123,#159124,#159125,#159126,#159127,#159128,
#159129,#159130,#159131,#159132,#159133,#159134,#159135,#159136,#159137,
#159138,#159139,#159140,#159141,#159142,#159143,#159144,#159145,#159146,
#159147,#159148,#159149,#159150,#159151,#159152,#159153,#159154,#159155,
#159156,#159157,#159158,#159159,#159160,#159161,#159162,#159163,#159164,
#159165,#159166,#159167,#159168,#159169,#159170,#159171,#159172,#159173,
#159174,#159175,#159176,#159177,#159178,#159179,#159180,#159181,#159182,
#159183,#159184,#159185,#159186,#159187,#159188,#159189,#159190,#159191,
#159192,#159193,#159194,#159195,#159196,#159197,#159198,#159199),
 .UNSPECIFIED.,.F.,.F.,(4,3,3,3,3,3,3,3,3,3,3,3,3,3,3,3,3,3,3,3,3,3,3,3,
3,3,3,3,3,3,3,3,3,3,3,3,3,3,3,3,3,3,3,3,3,3,3,3,3,3,3,3,3,3,3,3,3,3,3,3,
3,3,3,3,3,3,3,3,3,3,3,3,3,3,3,3,3,3,3,4),(-35.2689819899945,-35.1875860810853,
-35.1061679575443,-35.0247451134917,-34.9433006085595,-34.8927980315291,
-34.8104190209271,-34.7280548316773,-34.6446234958133,-34.5623015225204,
-34.4783155053709,-34.3943294882215,-34.3186893790001,-34.243073276094,
-34.1674667090403,-34.0918320463309,-34.0161824877531,-33.9404721979762,
-33.8958609449139,-33.803960375211,-33.7119274054973,-33.6200478356754,
-33.5284204396465,-33.4373993181653,-33.3973924016064,-33.3233904869182,
-33.2494095585748,-33.1754345366622,-33.1014220633622,-33.0273907933808,
-32.9532860411758,-32.8989238582988,-32.8199624423516,-32.7410550192824,
-32.6621899803458,-32.5833557496199,-32.5045407756412,-32.425719511981,
-32.3468928728687,-32.2680503484923,-32.1891814199096,-32.1102393685781,
-32.0312586030894,-31.9521875920712,-31.9019867716837,-31.8229948763452,
-31.7441030916705,-31.6653008356263,-31.5866008348049,-31.5079613889263,
-31.4293851067412,-31.4035182283762,-31.3249315052126,-31.2462953379495,
-31.1675993446332,-31.0887853131503,-31.0099038849267,-30.9309007917107,
-30.9050496850686,-30.825977163319,-30.746977608584,-30.66803934076,-30.5891507262786,
-30.5103001697224,-30.4314716654567,-30.3526552915878,-30.2738405404041,
-30.1950169064267,-30.1161468588784,-30.0372531798026,-29.9582926549656,
-29.9081125984535,-29.8340071603516,-29.7599586624969,-29.6859519244899,
-29.6119626603372,-29.5379852987251,-29.463983012692,-29.4096440551459,
-29.3426756889445),.UNSPECIFIED.);
#3159=B_SPLINE_CURVE_WITH_KNOTS('',3,(#159205,#159206,#159207,#159208,#159209,
#159210,#159211,#159212,#159213,#159214,#159215,#159216,#159217,#159218,
#159219,#159220,#159221,#159222,#159223,#159224,#159225,#159226,#159227,
#159228,#159229,#159230,#159231,#159232,#159233,#159234,#159235,#159236,
#159237,#159238,#159239,#159240,#159241,#159242,#159243,#159244,#159245,
#159246,#159247,#159248,#159249,#159250,#159251,#159252,#159253,#159254,
#159255,#159256,#159257,#159258,#159259,#159260,#159261,#159262,#159263,
#159264,#159265,#159266,#159267,#159268,#159269,#159270,#159271,#159272,
#159273,#159274,#159275,#159276,#159277,#159278,#159279,#159280,#159281,
#159282,#159283,#159284,#159285,#159286,#159287,#159288,#159289,#159290,
#159291,#159292,#159293,#159294,#159295,#159296,#159297,#159298,#159299,
#159300,#159301,#159302,#159303,#159304,#159305,#159306,#159307,#159308,
#159309,#159310,#159311,#159312,#159313,#159314,#159315,#159316,#159317,
#159318,#159319,#159320,#159321,#159322,#159323,#159324,#159325,#159326,
#159327,#159328,#159329,#159330,#159331,#159332,#159333,#159334,#159335,
#159336,#159337,#159338,#159339,#159340,#159341,#159342,#159343,#159344,
#159345,#159346,#159347,#159348,#159349,#159350,#159351,#159352,#159353,
#159354,#159355,#159356,#159357,#159358,#159359,#159360,#159361,#159362,
#159363,#159364,#159365,#159366,#159367,#159368,#159369,#159370,#159371,
#159372,#159373,#159374,#159375,#159376,#159377,#159378,#159379,#159380,
#159381,#159382,#159383,#159384,#159385,#159386,#159387,#159388,#159389,
#159390,#159391,#159392,#159393,#159394,#159395,#159396,#159397,#159398,
#159399,#159400,#159401,#159402,#159403,#159404,#159405,#159406,#159407,
#159408,#159409,#159410,#159411,#159412,#159413,#159414,#159415,#159416,
#159417,#159418,#159419,#159420,#159421,#159422,#159423,#159424,#159425,
#159426,#159427,#159428,#159429,#159430,#159431,#159432,#159433,#159434,
#159435,#159436,#159437,#159438,#159439,#159440,#159441,#159442),
 .UNSPECIFIED.,.F.,.F.,(4,3,3,3,3,3,3,3,3,3,3,3,3,3,3,3,3,3,3,3,3,3,3,3,
3,3,3,3,3,3,3,3,3,3,3,3,3,3,3,3,3,3,3,3,3,3,3,3,3,3,3,3,3,3,3,3,3,3,3,3,
3,3,3,3,3,3,3,3,3,3,3,3,3,3,3,3,3,3,3,4),(26.7981096470418,26.8902131063854,
26.9173013386081,26.9930110097253,27.0686720117508,27.1442988520881,27.2199165483701,
27.2955280484565,27.3711679730839,27.4157698819157,27.4980486537694,27.5803512166326,
27.6638230187803,27.7461779736786,27.830208199451,27.9142384252233,27.9966174358251,
28.0789816250744,28.1624129609385,28.2447349342312,28.328720951381,28.4127069685308,
28.4883470777522,28.5639631806583,28.6395697477119,28.7152044104214,28.7908539689992,
28.866564258776,28.9111755118384,29.0030760815413,29.0951090512552,29.1869886210773,
29.2786160171064,29.3696371385877,29.4096440551459,29.483645969834,29.5576268981774,
29.6316019200899,29.7056143933899,29.7796456633712,29.8537504155762,29.9081125984535,
29.9870740144007,30.0659814374699,30.1448464764065,30.2236807071324,30.302495681111,
30.3813169447712,30.4601435838836,30.5389861082599,30.6178550368427,30.6967970881741,
30.7757778536629,30.8548488646811,30.9050496850686,30.9840415804072,31.062933365082,
31.1417356211263,31.2204356219479,31.2990750678265,31.3776513500118,31.4035182283762,
31.4821049515397,31.5607411188028,31.6394371121192,31.7182511436019,31.7971325718255,
31.8761356650413,31.9019867716837,31.9796905707252,32.0573184284515,32.1348845444677,
32.2123990485688,32.289884947382,32.3673550257151,32.4448220569819,32.5223226907332,
32.5998408827482,32.6774206041791,32.7250362269146),.UNSPECIFIED.);
#3160=B_SPLINE_CURVE_WITH_KNOTS('',3,(#159443,#159444,#159445,#159446,#159447,
#159448,#159449,#159450,#159451,#159452,#159453,#159454,#159455,#159456,
#159457,#159458),.UNSPECIFIED.,.F.,.F.,(4,3,3,3,3,4),(32.7250362270345,
32.8666732039272,32.8989238582988,32.9730371102414,33.0470853245701,33.0816676322956),
 .UNSPECIFIED.);
#3161=B_SPLINE_CURVE_WITH_KNOTS('',3,(#159460,#159461,#159462,#159463,#159464,
#159465,#159466,#159467,#159468,#159469,#159470,#159471,#159472),
 .UNSPECIFIED.,.F.,.F.,(4,3,3,3,4),(-29.3426756889445,-29.252824355409,
-29.1627373608491,-29.0724643622336,-28.9857966830313),.UNSPECIFIED.);
#3162=B_SPLINE_CURVE_WITH_KNOTS('',3,(#159473,#159474,#159475,#159476,#159477,
#159478,#159479,#159480,#159481,#159482,#159483,#159484,#159485,#159486,
#159487,#159488,#159489,#159490,#159491,#159492,#159493,#159494,#159495,
#159496,#159497,#159498,#159499,#159500,#159501,#159502,#159503,#159504,
#159505,#159506,#159507,#159508,#159509,#159510,#159511,#159512,#159513,
#159514,#159515,#159516,#159517,#159518,#159519,#159520,#159521,#159522,
#159523,#159524,#159525,#159526,#159527,#159528,#159529,#159530,#159531,
#159532,#159533,#159534,#159535,#159536,#159537,#159538,#159539,#159540,
#159541,#159542,#159543,#159544,#159545,#159546,#159547,#159548,#159549,
#159550,#159551,#159552,#159553,#159554,#159555,#159556,#159557,#159558,
#159559,#159560,#159561,#159562,#159563,#159564,#159565,#159566,#159567,
#159568,#159569,#159570,#159571,#159572,#159573,#159574,#159575,#159576,
#159577,#159578,#159579,#159580,#159581,#159582,#159583,#159584,#159585,
#159586,#159587,#159588,#159589,#159590,#159591,#159592,#159593,#159594,
#159595,#159596,#159597,#159598,#159599,#159600,#159601,#159602,#159603,
#159604,#159605,#159606,#159607,#159608,#159609,#159610,#159611,#159612,
#159613,#159614,#159615,#159616,#159617,#159618,#159619,#159620,#159621,
#159622,#159623,#159624,#159625,#159626,#159627,#159628,#159629,#159630,
#159631,#159632,#159633,#159634,#159635,#159636,#159637,#159638,#159639,
#159640,#159641,#159642,#159643,#159644,#159645,#159646,#159647,#159648,
#159649,#159650,#159651,#159652,#159653,#159654,#159655,#159656,#159657,
#159658,#159659,#159660,#159661,#159662,#159663,#159664,#159665,#159666,
#159667,#159668,#159669,#159670,#159671,#159672,#159673,#159674,#159675,
#159676,#159677,#159678,#159679,#159680,#159681,#159682,#159683,#159684,
#159685,#159686,#159687,#159688,#159689,#159690,#159691,#159692,#159693,
#159694,#159695,#159696,#159697,#159698,#159699,#159700,#159701,#159702,
#159703,#159704,#159705,#159706,#159707),.UNSPECIFIED.,.F.,.F.,(4,3,3,3,
3,3,3,3,3,3,3,3,3,3,3,3,3,3,3,3,3,3,3,3,3,3,3,3,3,3,3,3,3,3,3,3,3,3,3,3,
3,3,3,3,3,3,3,3,3,3,3,3,3,3,3,3,3,3,3,3,3,3,3,3,3,3,3,3,3,3,3,3,3,3,3,3,
3,3,4),(-28.985796682929,-28.9111755118384,-28.8354658407202,-28.7598048386937,
-28.6841779983556,-28.6085603020726,-28.5329488019854,-28.4573088773571,
-28.4127069685308,-28.3304281966777,-28.2481256338155,-28.1646538316674,
-28.0822988767698,-27.9982686509965,-27.9142384252232,-27.8318594146209,
-27.7494952253709,-27.6660638895071,-27.583741916214,-27.4997558990649,
-27.4157698819157,-27.3401297726947,-27.2645136697891,-27.1889071027363,
-27.1132724400273,-27.0376228814498,-26.9619125916734,-26.9173013386081,
-26.8254007689034,-26.7333677991868,-26.641488229363,-26.5498608333321,
-26.458839711849,-26.4188327953006,-26.3448308806132,-26.2708499522705,
-26.1968749303587,-26.1228624570593,-26.0488311870786,-25.9747264348744,
-25.920364251993,-25.8414028360458,-25.7624954129767,-25.6836303740406,
-25.6047961433149,-25.5259811693365,-25.4471599056764,-25.3683332665642,
-25.289490742188,-25.2106218136058,-25.1316797622744,-25.0526989967857,
-24.9736279857675,-24.9234271653779,-24.8444352700362,-24.7655434853584,
-24.6867412293113,-24.6080412284866,-24.5294017826055,-24.4508255004176,
-24.4249586220703,-24.3463718989129,-24.2677357316562,-24.1890397383471,
-24.1102257068707,-24.0313442786536,-23.9523411854441,-23.9264900787628,
-23.8474119781529,-23.7684078578114,-23.6894660330283,-23.610582322527,
-23.5317331437529,-23.4529079627478,-23.3740962622646,-23.295225741387,
-23.216394325695,-23.1375042522246,-23.0586141787543),.UNSPECIFIED.);
#3163=B_SPLINE_CURVE_WITH_KNOTS('',3,(#159713,#159714,#159715,#159716,#159717,
#159718,#159719,#159720,#159721,#159722,#159723,#159724,#159725,#159726,
#159727,#159728,#159729,#159730,#159731,#159732,#159733,#159734,#159735,
#159736,#159737,#159738,#159739,#159740,#159741,#159742,#159743,#159744,
#159745,#159746,#159747,#159748,#159749,#159750,#159751,#159752,#159753,
#159754,#159755,#159756,#159757,#159758,#159759,#159760,#159761,#159762,
#159763,#159764,#159765,#159766,#159767,#159768,#159769,#159770,#159771,
#159772,#159773,#159774,#159775,#159776,#159777,#159778,#159779,#159780,
#159781,#159782,#159783,#159784,#159785,#159786,#159787,#159788,#159789,
#159790,#159791,#159792,#159793,#159794,#159795,#159796,#159797,#159798,
#159799,#159800,#159801,#159802,#159803,#159804,#159805,#159806,#159807,
#159808,#159809,#159810,#159811,#159812,#159813,#159814,#159815,#159816,
#159817,#159818,#159819,#159820,#159821,#159822,#159823,#159824,#159825,
#159826,#159827,#159828,#159829,#159830,#159831,#159832,#159833,#159834,
#159835,#159836,#159837,#159838,#159839,#159840,#159841,#159842,#159843,
#159844,#159845,#159846,#159847,#159848,#159849,#159850,#159851,#159852,
#159853,#159854,#159855,#159856,#159857,#159858,#159859,#159860,#159861,
#159862,#159863,#159864,#159865,#159866,#159867,#159868,#159869,#159870,
#159871,#159872,#159873,#159874,#159875,#159876,#159877,#159878,#159879,
#159880,#159881,#159882,#159883,#159884,#159885,#159886,#159887,#159888,
#159889,#159890,#159891,#159892,#159893,#159894,#159895,#159896,#159897,
#159898,#159899,#159900,#159901,#159902,#159903,#159904,#159905,#159906,
#159907,#159908,#159909,#159910,#159911,#159912,#159913,#159914,#159915,
#159916,#159917,#159918,#159919,#159920,#159921,#159922,#159923,#159924,
#159925,#159926,#159927,#159928,#159929,#159930,#159931,#159932),
 .UNSPECIFIED.,.F.,.F.,(4,3,3,3,3,3,3,3,3,3,3,3,3,3,3,3,3,3,3,3,3,3,3,3,
3,3,3,3,3,3,3,3,3,3,3,3,3,3,3,3,3,3,3,3,3,3,3,3,3,3,3,3,3,3,3,3,3,3,3,3,
3,3,3,3,3,3,3,3,3,3,3,3,3,4),(20.5148802586327,20.5966101323988,20.6783398861692,
20.7600695216108,20.8417990403898,20.9235284441734,21.0052577346279,21.0902045031471,
21.1738239784081,21.2561368993682,21.3378758084354,21.4196142978218,21.5013523742017,
21.5830900442492,21.6648273146377,21.7465641920405,21.8283006831307,21.9100367945807,
21.9917725330629,22.0735079052492,22.1552429178113,22.2369775774205,22.3187118907478,
22.400445864464,22.4821795052395,22.5639128197445,22.645645814649,22.7273784966224,
22.8091108723342,22.8908429484535,22.972574731649,23.0543062285894,23.136037445943,
23.217768390378,23.2994990685622,23.3812294871632,23.4629596528485,23.5446895722853,
23.6264192521404,23.7081486990807,23.7935768934799,23.8763354568041,23.9580740843673,
24.0398118881713,24.121548894911,24.2032851312789,24.2850206239646,24.3667553996553,
24.4484894850359,24.5302229067887,24.6119556915937,24.6936878661289,24.7754194570701,
24.8571504910911,24.9388809948637,25.0206109950583,25.1023405183429,25.1860599184374,
25.2677979994658,25.3495344948902,25.4312695114747,25.513003155963,25.5947355350801,
25.6764667555333,25.7581969240138,25.8436536734939,25.9253905917129,26.0071246006162,
26.0888561271355,26.1705855980639,26.2523204885399,26.334050568705,26.4157819977665,
26.4418509198549),.UNSPECIFIED.);
#3164=B_SPLINE_CURVE_WITH_KNOTS('',3,(#159933,#159934,#159935,#159936,#159937,
#159938,#159939,#159940,#159941,#159942,#159943,#159944,#159945),
 .UNSPECIFIED.,.F.,.F.,(4,3,3,3,4),(26.4418509198549,26.5333568795253,26.6252438530259,
26.7174516395712,26.7981096470418),.UNSPECIFIED.);
#3165=B_SPLINE_CURVE_WITH_KNOTS('',3,(#159947,#159948,#159949,#159950,#159951,
#159952,#159953,#159954,#159955,#159956,#159957,#159958,#159959,#159960,
#159961,#159962),.UNSPECIFIED.,.F.,.F.,(4,3,3,3,3,4),(-23.0586141787543,
-22.9796536386338,-22.9295529921477,-22.8479531392553,-22.7665501484863,
-22.7026113757494),.UNSPECIFIED.);
#3166=B_SPLINE_CURVE_WITH_KNOTS('',3,(#159963,#159964,#159965,#159966,#159967,
#159968,#159969,#159970,#159971,#159972,#159973,#159974,#159975,#159976,
#159977,#159978,#159979,#159980,#159981,#159982,#159983,#159984,#159985,
#159986,#159987,#159988,#159989,#159990,#159991,#159992,#159993,#159994,
#159995,#159996,#159997,#159998,#159999,#160000,#160001,#160002,#160003,
#160004,#160005,#160006,#160007,#160008,#160009,#160010,#160011,#160012,
#160013,#160014,#160015,#160016,#160017,#160018,#160019,#160020,#160021,
#160022,#160023,#160024,#160025,#160026,#160027,#160028,#160029,#160030,
#160031,#160032,#160033,#160034,#160035,#160036,#160037,#160038,#160039,
#160040,#160041,#160042,#160043,#160044,#160045,#160046,#160047,#160048,
#160049,#160050,#160051,#160052,#160053,#160054,#160055,#160056,#160057,
#160058,#160059,#160060,#160061,#160062,#160063,#160064,#160065,#160066,
#160067,#160068,#160069,#160070,#160071,#160072,#160073,#160074,#160075,
#160076,#160077,#160078,#160079,#160080,#160081,#160082,#160083,#160084,
#160085,#160086,#160087,#160088,#160089,#160090,#160091,#160092,#160093,
#160094,#160095,#160096,#160097,#160098,#160099,#160100,#160101,#160102,
#160103,#160104,#160105,#160106,#160107,#160108,#160109,#160110,#160111,
#160112,#160113,#160114,#160115,#160116,#160117,#160118,#160119,#160120,
#160121,#160122,#160123,#160124,#160125,#160126,#160127,#160128,#160129,
#160130,#160131,#160132,#160133,#160134,#160135,#160136,#160137,#160138,
#160139,#160140,#160141,#160142,#160143,#160144,#160145,#160146,#160147,
#160148,#160149,#160150,#160151,#160152,#160153,#160154,#160155,#160156,
#160157,#160158,#160159,#160160,#160161,#160162,#160163,#160164,#160165,
#160166,#160167,#160168,#160169,#160170,#160171,#160172,#160173,#160174,
#160175,#160176,#160177,#160178,#160179,#160180,#160181,#160182,#160183,
#160184,#160185,#160186,#160187,#160188,#160189,#160190,#160191,#160192,
#160193,#160194,#160195,#160196,#160197,#160198,#160199,#160200),
 .UNSPECIFIED.,.F.,.F.,(4,3,3,3,3,3,3,3,3,3,3,3,3,3,3,3,3,3,3,3,3,3,3,3,
3,3,3,3,3,3,3,3,3,3,3,3,3,3,3,3,3,3,3,3,3,3,3,3,3,3,3,3,3,3,3,3,3,3,3,3,
3,3,3,3,3,3,3,3,3,3,3,3,3,3,3,3,3,3,3,4),(-22.7026113756635,-22.63173040129,
-22.5608644977156,-22.4899738374718,-22.4310844488401,-22.3400853491217,
-22.2485821314641,-22.156638592555,-22.0646040153979,-21.9726949252976,
-21.9326159055326,-21.8569062343569,-21.7812452322732,-21.7056183918778,
-21.6300006955379,-21.5543891953937,-21.4787492707089,-21.434147362225,
-21.3518685906234,-21.2695660280155,-21.1860942257409,-21.103739271098,
-21.0197090450077,-20.9356788189174,-20.853299807784,-20.7709356180008,
-20.6875042824031,-20.6051823085844,-20.5211962920972,-20.4372102756099,
-20.3615701669439,-20.2859540645933,-20.2103474980945,-20.134712835939,
-20.0590632779147,-19.9833529886882,-19.9387417323023,-19.8468411610517,
-19.754808189751,-19.662928618399,-19.5713012209253,-19.4802800981782,-19.4402731889948,
-19.3662712745431,-19.2922903464352,-19.218315324757,-19.1443028516895,
-19.0702715819395,-18.9961668299636,-18.9418046456872,-18.8628432307598,
-18.7839358087192,-18.7050707708183,-18.6262365411328,-18.5474215681963,
-18.468600305575,-18.3897736674978,-18.3109311441513,-18.2320622165907,
-18.1531201662622,-18.0741394017655,-17.9950683917138,-17.9448675590721,
-17.8658756573626,-17.7869838663843,-17.7081816041176,-17.6294815972208,
-17.5508421453608,-17.4722658573496,-17.4463990157645,-17.3678123023036,
-17.2891761448826,-17.2104801615263,-17.1316661401196,-17.0527847220363,
-16.9737816389859,-16.947930472457,-16.866341548056,-16.7848569941609,-16.7753213308628),
 .UNSPECIFIED.);
#3167=B_SPLINE_CURVE_WITH_KNOTS('',3,(#160206,#160207,#160208,#160209,#160210,
#160211,#160212,#160213,#160214,#160215,#160216,#160217,#160218,#160219,
#160220,#160221,#160222,#160223,#160224,#160225,#160226,#160227,#160228,
#160229,#160230,#160231,#160232,#160233,#160234,#160235,#160236,#160237,
#160238,#160239,#160240,#160241,#160242,#160243,#160244,#160245,#160246,
#160247,#160248,#160249,#160250,#160251,#160252,#160253,#160254,#160255,
#160256,#160257,#160258,#160259,#160260,#160261,#160262,#160263,#160264,
#160265,#160266,#160267,#160268,#160269,#160270,#160271,#160272,#160273,
#160274,#160275,#160276,#160277,#160278,#160279,#160280,#160281,#160282,
#160283,#160284,#160285,#160286,#160287,#160288,#160289,#160290,#160291,
#160292,#160293,#160294,#160295,#160296,#160297,#160298,#160299,#160300,
#160301,#160302,#160303,#160304,#160305,#160306,#160307,#160308,#160309,
#160310,#160311,#160312,#160313,#160314,#160315,#160316,#160317,#160318,
#160319,#160320,#160321,#160322,#160323,#160324,#160325,#160326,#160327,
#160328,#160329,#160330,#160331,#160332,#160333,#160334,#160335,#160336,
#160337,#160338,#160339,#160340,#160341,#160342,#160343,#160344,#160345,
#160346,#160347,#160348,#160349,#160350,#160351,#160352,#160353,#160354,
#160355,#160356,#160357,#160358,#160359,#160360,#160361,#160362,#160363,
#160364,#160365,#160366,#160367,#160368,#160369,#160370,#160371,#160372,
#160373,#160374,#160375,#160376,#160377,#160378,#160379,#160380,#160381,
#160382,#160383,#160384,#160385,#160386,#160387,#160388,#160389,#160390,
#160391,#160392,#160393,#160394,#160395,#160396,#160397,#160398,#160399,
#160400,#160401,#160402,#160403,#160404,#160405,#160406,#160407,#160408,
#160409,#160410,#160411,#160412,#160413,#160414,#160415,#160416,#160417,
#160418,#160419,#160420,#160421,#160422,#160423,#160424,#160425,#160426,
#160427,#160428,#160429,#160430,#160431,#160432,#160433,#160434,#160435,
#160436,#160437,#160438,#160439,#160440,#160441,#160442,#160443),
 .UNSPECIFIED.,.F.,.F.,(4,3,3,3,3,3,3,3,3,3,3,3,3,3,3,3,3,3,3,3,3,3,3,3,
3,3,3,3,3,3,3,3,3,3,3,3,3,3,3,3,3,3,3,3,3,3,3,3,3,3,3,3,3,3,3,3,3,3,3,3,
3,3,3,3,3,3,3,3,3,3,3,3,3,3,3,3,3,3,3,4),(14.231883480232,14.3141973780922,
14.3964809558168,14.4555877559192,14.5312280067413,14.6068442521871,14.6824509626349,
14.7580857696397,14.8337354731209,14.9094459081311,14.9540562992267,15.0459567283529,
15.1379895501617,15.2298689719367,15.3214962250171,15.4125172166086,15.4525248425343,
15.5265267702345,15.6005077116442,15.6744827466736,15.7484952331392,15.8225265163264,
15.8966312817451,15.9509933858419,16.0299548037444,16.1088622288164,16.1877272697983,
16.2665615026073,16.345376478702,16.424197744515,16.5030243858,16.5818669123645,
16.6607358431467,16.7396778966799,16.8186586643724,16.8977296775774,16.947930472457,
17.0269223576651,17.1058141322463,17.1846163782545,17.2633163691684,17.3419558052269,
17.4205320777516,17.4463990157645,17.5249857447869,17.6036219180417,17.6823179174691,
17.7611319552012,17.8400133897525,17.9190164893673,17.9448675590721,18.0239400798595,
18.1029396336136,18.1818779004403,18.2607665139104,18.3396170694441,18.4184455726759,
18.4972619455054,18.5760766956466,18.6549003285804,18.7337703750903,18.8126640531305,
18.8916245769453,18.9418046456872,19.0159100835603,19.0899585811844,19.1639653189595,
19.2379545828783,19.3119319442551,19.385934230052,19.4402731889948,19.5312722900101,
19.6227755091177,19.7147190496085,19.8067536283734,19.8986627200372,19.9387417323023,
20.0156037252305,20.0924004463538,20.1586656126753),.UNSPECIFIED.);
#3168=B_SPLINE_CURVE_WITH_KNOTS('',3,(#160444,#160445,#160446,#160447,#160448,
#160449,#160450,#160451,#160452,#160453,#160454,#160455,#160456,#160457,
#160458,#160459),.UNSPECIFIED.,.F.,.F.,(4,3,3,3,3,4),(20.1586656126753,
20.2403951565113,20.3221302714303,20.4038605087794,20.4855922977304,20.5148802586327),
 .UNSPECIFIED.);
#3169=B_SPLINE_CURVE_WITH_KNOTS('',3,(#160461,#160462,#160463,#160464,#160465,
#160466,#160467,#160468,#160469,#160470,#160471,#160472,#160473,#160474,
#160475,#160476),.UNSPECIFIED.,.F.,.F.,(4,3,3,3,3,4),(-16.7753213308628,
-16.6939460132947,-16.6126881417199,-16.5315046550008,-16.4504174865027,
-16.4194260685698),.UNSPECIFIED.);
#3170=B_SPLINE_CURVE_WITH_KNOTS('',3,(#160477,#160478,#160479,#160480,#160481,
#160482,#160483,#160484,#160485,#160486,#160487,#160488,#160489,#160490,
#160491,#160492,#160493,#160494,#160495,#160496,#160497,#160498,#160499,
#160500,#160501,#160502,#160503,#160504,#160505,#160506,#160507,#160508,
#160509,#160510,#160511,#160512,#160513,#160514,#160515,#160516,#160517,
#160518,#160519,#160520,#160521,#160522,#160523,#160524,#160525,#160526,
#160527,#160528,#160529,#160530,#160531,#160532,#160533,#160534,#160535,
#160536,#160537,#160538,#160539,#160540,#160541,#160542,#160543,#160544,
#160545,#160546,#160547,#160548,#160549,#160550,#160551,#160552,#160553,
#160554,#160555,#160556,#160557,#160558,#160559,#160560,#160561,#160562,
#160563,#160564,#160565,#160566,#160567,#160568,#160569,#160570,#160571,
#160572,#160573,#160574,#160575,#160576,#160577,#160578,#160579,#160580,
#160581,#160582,#160583,#160584,#160585,#160586,#160587,#160588,#160589,
#160590,#160591,#160592,#160593,#160594,#160595,#160596,#160597,#160598,
#160599,#160600,#160601,#160602,#160603,#160604,#160605,#160606,#160607,
#160608,#160609,#160610,#160611,#160612,#160613,#160614,#160615,#160616,
#160617,#160618,#160619,#160620,#160621,#160622,#160623,#160624,#160625,
#160626,#160627,#160628,#160629,#160630,#160631,#160632,#160633,#160634,
#160635,#160636,#160637,#160638,#160639,#160640,#160641,#160642,#160643,
#160644,#160645,#160646,#160647,#160648,#160649,#160650,#160651,#160652,
#160653,#160654,#160655,#160656,#160657,#160658,#160659,#160660,#160661,
#160662,#160663,#160664,#160665,#160666,#160667,#160668,#160669,#160670,
#160671,#160672,#160673,#160674,#160675,#160676,#160677,#160678,#160679,
#160680,#160681,#160682,#160683,#160684,#160685,#160686,#160687,#160688,
#160689,#160690,#160691,#160692,#160693,#160694,#160695,#160696,#160697,
#160698,#160699,#160700,#160701,#160702,#160703,#160704,#160705,#160706,
#160707,#160708),.UNSPECIFIED.,.F.,.F.,(4,3,3,3,3,3,3,3,3,3,3,3,3,3,3,3,
3,3,3,3,3,3,3,3,3,3,3,3,3,3,3,3,3,3,3,3,3,3,3,3,3,3,3,3,3,3,3,3,3,3,3,3,
3,3,3,3,3,3,3,3,3,3,3,3,3,3,3,3,3,3,3,3,3,3,3,3,3,4),(-16.4194260684678,
-16.3348432118268,-16.2501027335155,-16.1651650733611,-16.0801426234198,
-15.9950222397046,-15.9509933858419,-15.8768879345363,-15.8028394234964,
-15.728832672326,-15.6548433950672,-15.5808660203712,-15.506863721332,-15.4525248425343,
-15.3615258742025,-15.270022799166,-15.1780794100646,-15.0860449819812,
-14.9941360321871,-14.9540562992267,-14.8783464830015,-14.8026853362177,
-14.7270583515563,-14.6514405119547,-14.5758288690443,-14.5001888028641,
-14.4555877559192,-14.3733093981691,-14.2910072534959,-14.2075352432749,
-14.1251807055008,-14.0411499590562,-13.9571192126116,-13.8747396035953,
-13.7923748141998,-13.7089437779758,-13.6266212155157,-13.5426359424099,
-13.4586506693041,-13.3830108845675,-13.3073951055576,-13.2317888616295,
-13.1561545200157,-13.0805052816012,-13.0047953092234,-12.9601821259965,
-12.868282108857,-12.7762497294734,-12.6843707628409,-12.5927439561573,
-12.5017233802903,-12.4617135826889,-12.3877105798512,-12.3137285580205,
-12.2397524375635,-12.1657388603515,-12.0917064823757,-12.0176006203337,
-11.9632450393814,-11.8842857069725,-11.8053803858034,-11.7265174622548,
-11.6476853555399,-11.5688725093352,-11.4900533664762,-11.4112288408948,
-11.3323884184719,-11.2535215759515,-11.1745815715412,-11.0956028314634,
-11.0165337927795,-10.9663079527663,-10.8873050792045,-10.8084026717488,
-10.72938700255,-10.6506762921222,-10.5715081435379,-10.4923399949537),
 .UNSPECIFIED.);
#3171=B_SPLINE_CURVE_WITH_KNOTS('',3,(#160714,#160715,#160716,#160717,#160718,
#160719,#160720,#160721,#160722,#160723,#160724,#160725,#160726),
 .UNSPECIFIED.,.F.,.F.,(4,3,3,3,4),(-4.2102189925341,-4.13326383456533,
-4.05618009768139,-3.98774834646046,-3.85305545421067),.UNSPECIFIED.);
#3172=B_SPLINE_CURVE_WITH_KNOTS('',3,(#160728,#160729,#160730,#160731,#160732,
#160733,#160734,#160735,#160736,#160737,#160738,#160739,#160740,#160741,
#160742,#160743,#160744,#160745,#160746,#160747,#160748,#160749,#160750,
#160751,#160752,#160753,#160754,#160755,#160756,#160757,#160758,#160759,
#160760,#160761,#160762,#160763,#160764,#160765,#160766,#160767,#160768,
#160769,#160770,#160771,#160772,#160773,#160774,#160775,#160776,#160777,
#160778,#160779,#160780,#160781,#160782,#160783,#160784,#160785,#160786,
#160787,#160788,#160789,#160790,#160791,#160792,#160793,#160794,#160795,
#160796,#160797,#160798,#160799,#160800,#160801,#160802,#160803,#160804,
#160805,#160806,#160807,#160808,#160809,#160810,#160811,#160812,#160813,
#160814,#160815,#160816,#160817,#160818,#160819,#160820,#160821,#160822,
#160823,#160824,#160825,#160826,#160827,#160828,#160829,#160830,#160831,
#160832,#160833,#160834,#160835,#160836,#160837,#160838,#160839,#160840,
#160841,#160842,#160843,#160844,#160845,#160846,#160847,#160848,#160849,
#160850,#160851,#160852,#160853,#160854,#160855,#160856,#160857,#160858,
#160859,#160860,#160861,#160862,#160863,#160864,#160865,#160866,#160867,
#160868,#160869,#160870,#160871,#160872,#160873,#160874,#160875,#160876,
#160877,#160878,#160879,#160880,#160881),.UNSPECIFIED.,.F.,.F.,(4,3,3,3,
3,3,3,3,3,3,3,3,3,3,3,3,3,3,3,3,3,3,3,3,3,3,3,3,3,3,3,3,3,3,3,3,3,3,3,3,
3,3,3,3,3,3,3,3,3,3,3,4),(-3.85305545408635,-3.77733322152493,-3.70169587286144,
-3.62612730711408,-3.54671280120549,-3.47123186819023,-3.39576658341081,
-3.32030250466635,-3.24482519243858,-3.16928858882332,-3.09371744426421,
-3.01806353171231,-2.99081125984535,-2.91338960182974,-2.83602915369424,
-2.75871684786117,-2.68143942843154,-2.604182561553,-2.52692488276581,-2.49234271653779,
-2.40529897332284,-2.31804420440917,-2.23057731574574,-2.14304930038302,
-2.05551593212837,-1.99387417323023,-1.91787097808727,-1.84191628058941,
-1.76599575933275,-1.69008513708016,-1.61418100207181,-1.53824993894703,
-1.49540562992267,-1.41140303908181,-1.32734729720491,-1.24323359539477,
-1.15911065250105,-1.07498942323625,-0.996937086615118,-0.918227407423238,
-0.839546602114508,-0.760883798027845,-0.682216838298316,-0.60354847363303,
-0.524852928628286,-0.498468543307558,-0.417045733774206,-0.335632904215115,
-0.251724678161337,-0.170320627264329,-0.0851603136321654,-1.82627892504507E-15),
 .UNSPECIFIED.);
#3173=B_SPLINE_CURVE_WITH_KNOTS('',3,(#160885,#160886,#160887,#160888,#160889,
#160890,#160891,#160892,#160893,#160894,#160895,#160896,#160897,#160898,
#160899,#160900,#160901,#160902,#160903,#160904,#160905,#160906,#160907,
#160908,#160909,#160910,#160911,#160912,#160913,#160914,#160915,#160916,
#160917,#160918,#160919,#160920,#160921,#160922,#160923,#160924,#160925,
#160926,#160927,#160928,#160929,#160930,#160931,#160932,#160933,#160934,
#160935,#160936,#160937,#160938,#160939,#160940,#160941,#160942,#160943,
#160944,#160945,#160946,#160947,#160948,#160949,#160950,#160951,#160952,
#160953,#160954,#160955,#160956,#160957,#160958,#160959,#160960,#160961,
#160962,#160963,#160964,#160965,#160966,#160967,#160968,#160969,#160970,
#160971,#160972,#160973,#160974,#160975,#160976,#160977,#160978,#160979,
#160980,#160981,#160982,#160983,#160984,#160985,#160986,#160987,#160988,
#160989,#160990,#160991,#160992,#160993,#160994,#160995,#160996,#160997,
#160998,#160999,#161000,#161001,#161002,#161003,#161004,#161005,#161006,
#161007,#161008,#161009,#161010,#161011,#161012,#161013,#161014,#161015,
#161016,#161017,#161018,#161019,#161020,#161021,#161022,#161023,#161024,
#161025,#161026,#161027,#161028,#161029,#161030,#161031,#161032,#161033,
#161034,#161035,#161036,#161037,#161038,#161039,#161040,#161041,#161042,
#161043,#161044,#161045,#161046,#161047,#161048,#161049,#161050,#161051,
#161052,#161053,#161054,#161055,#161056,#161057,#161058,#161059,#161060,
#161061,#161062,#161063,#161064,#161065,#161066,#161067,#161068,#161069,
#161070,#161071,#161072,#161073,#161074,#161075,#161076,#161077,#161078,
#161079,#161080,#161081,#161082,#161083,#161084,#161085,#161086,#161087,
#161088,#161089,#161090,#161091,#161092,#161093,#161094,#161095,#161096,
#161097,#161098,#161099,#161100,#161101,#161102,#161103,#161104),
 .UNSPECIFIED.,.F.,.F.,(4,3,3,3,3,3,3,3,3,3,3,3,3,3,3,3,3,3,3,3,3,3,3,3,
3,3,3,3,3,3,3,3,3,3,3,3,3,3,3,3,3,3,3,3,3,3,3,3,3,3,3,3,3,3,3,3,3,3,3,3,
3,3,3,3,3,3,3,3,3,3,3,3,3,4),(2.02057330133861,2.10731855090179,2.19404294025265,
2.28065105473334,2.36714678612864,2.45341692392646,2.49234271653779,2.56960253681016,
2.64685977983922,2.72412743925298,2.80144758367556,2.87879733597736,2.95622233760274,
2.99081125984535,3.06769470829953,3.14450839872675,3.22126734333478,3.29798651594428,
3.37468086167416,3.45138294474633,3.5280927188547,3.60482370957874,3.68158945170787,
3.75845454953412,3.83537082665699,3.91241786308591,3.98774834646046,4.0648418860315,
4.14183633541153,4.21874677598679,4.29558823062224,4.37237567418249,4.44912607179099,
4.52585691122378,4.602581687806,4.6793138909937,4.7561022859856,4.83291830588097,
4.90982555495308,4.98468543307558,5.06203195585688,5.13931811616054,5.21655706794557,
5.29376277077859,5.37094887235525,5.44813746534129,5.48315397638314,5.57026302863232,
5.65758273008965,5.74511166625669,5.8326992021723,5.92028639032618,5.9816225196907,
6.05788321116819,6.13409549162699,6.21027349698447,6.28644077030324,6.36260118254298,
6.4387870172689,6.48009106299825,6.5625136809008,6.64496553473764,6.72836405262968,
6.81087749609412,6.89471855119997,6.97855960630581,7.06056935141231,7.14255800395656,
7.22617554037076,7.30811590022636,7.39257202491986,7.47702814961337,7.55692378696674,
7.59229499831615),.UNSPECIFIED.);
#3174=B_SPLINE_CURVE_WITH_KNOTS('',3,(#161105,#161106,#161107,#161108,#161109,
#161110,#161111,#161112,#161113,#161114,#161115,#161116,#161117,#161118,
#161119,#161120),.UNSPECIFIED.,.F.,.F.,(4,3,3,3,3,4),(7.59229499839287,
7.66781581452666,7.74335395647864,7.81890012251005,7.89450003993217,7.94810021833352),
 .UNSPECIFIED.);
#3175=B_SPLINE_CURVE_WITH_KNOTS('',3,(#161123,#161124,#161125,#161126,#161127,
#161128,#161129,#161130,#161131,#161132,#161133,#161134,#161135,#161136,
#161137,#161138,#161139,#161140,#161141,#161142,#161143,#161144,#161145,
#161146,#161147,#161148,#161149,#161150,#161151,#161152,#161153,#161154,
#161155,#161156,#161157,#161158,#161159,#161160,#161161,#161162,#161163,
#161164,#161165,#161166,#161167,#161168,#161169,#161170,#161171,#161172,
#161173,#161174,#161175,#161176,#161177,#161178,#161179,#161180,#161181,
#161182,#161183,#161184,#161185,#161186,#161187,#161188,#161189,#161190,
#161191,#161192,#161193,#161194,#161195,#161196,#161197,#161198,#161199,
#161200,#161201,#161202,#161203,#161204,#161205,#161206,#161207,#161208,
#161209,#161210,#161211,#161212,#161213,#161214,#161215,#161216,#161217,
#161218,#161219,#161220,#161221,#161222,#161223,#161224,#161225,#161226,
#161227,#161228,#161229,#161230,#161231,#161232,#161233,#161234,#161235,
#161236,#161237,#161238,#161239,#161240,#161241,#161242,#161243,#161244,
#161245,#161246,#161247,#161248,#161249,#161250,#161251,#161252,#161253,
#161254,#161255,#161256,#161257,#161258,#161259,#161260,#161261,#161262,
#161263,#161264,#161265,#161266,#161267,#161268,#161269,#161270,#161271,
#161272,#161273,#161274,#161275,#161276,#161277,#161278,#161279,#161280,
#161281,#161282,#161283,#161284,#161285,#161286,#161287,#161288,#161289,
#161290,#161291,#161292,#161293,#161294,#161295,#161296,#161297,#161298,
#161299,#161300,#161301,#161302,#161303,#161304,#161305,#161306,#161307,
#161308,#161309,#161310,#161311,#161312,#161313,#161314,#161315,#161316,
#161317,#161318,#161319,#161320,#161321,#161322,#161323,#161324,#161325,
#161326,#161327,#161328,#161329,#161330,#161331,#161332,#161333,#161334,
#161335,#161336,#161337,#161338,#161339,#161340,#161341,#161342,#161343,
#161344,#161345,#161346,#161347,#161348,#161349,#161350,#161351,#161352,
#161353,#161354,#161355,#161356,#161357,#161358,#161359,#161360),
 .UNSPECIFIED.,.F.,.F.,(4,3,3,3,3,3,3,3,3,3,3,3,3,3,3,3,3,3,3,3,3,3,3,3,
3,3,3,3,3,3,3,3,3,3,3,3,3,3,3,3,3,3,3,3,3,3,3,3,3,3,3,3,3,3,3,3,3,3,3,3,
3,3,3,3,3,3,3,3,3,3,3,3,3,3,3,3,3,3,3,4),(7.94810021833352,7.97549669292093,
8.06711656730402,8.15885338523794,8.25043489219158,8.34177330665132,8.43252992566801,
8.47396523622849,8.54800828867236,8.62203064070959,8.69604736092453,8.77010186103058,
8.84417538298251,8.91832256609645,8.97243377953604,9.05139060932345,9.13029334033861,
9.20915359340074,9.28798295643997,9.36679299287031,9.44560924431697,9.52443083233563,
9.60326827720018,9.68213210828826,9.76106907071863,9.84004475086048,9.91911072933346,
9.96937086615116,10.048353892304,10.1272368201723,10.206030249966,10.2847215077339,
10.3633522701407,10.4419199839626,10.4678394094587,10.5464330284591,10.6250762646076,
10.7037794841114,10.7826009287505,10.8614898765492,10.9405005932523,10.9663079527663,
11.0453785106916,11.1243760632993,11.2033122956374,11.2821988461979,11.3610473153034,
11.4398737088712,11.5186879609097,11.5975005834405,11.6763220862447,11.7551900128592,
11.8340815766776,11.9130400130903,11.9632450393814,12.0373515864893,12.1114011909516,
12.1854090328583,12.2593993948568,12.333377851737,12.4073812254331,12.461713582689,
12.5527121304417,12.6442147576327,12.7361576887354,12.8281916681528,12.9201002063867,
12.9601821259965,13.0358914799109,13.1115521628426,13.1871786823854,13.2627960560663,
13.3384072323673,13.4140468325296,13.4586506693041,13.5410375115435,13.6246482100316,
13.7070972633513,13.7912887844235,13.8754803054957),.UNSPECIFIED.);
#3176=B_SPLINE_CURVE_WITH_KNOTS('',3,(#161361,#161362,#161363,#161364,#161365,
#161366,#161367,#161368,#161369,#161370,#161371,#161372,#161373,#161374,
#161375,#161376),.UNSPECIFIED.,.F.,.F.,(4,3,3,3,3,4),(13.8754803056222,
13.9571192126116,14.0394983452062,14.1218621763033,14.2042074048479,14.231883480232),
 .UNSPECIFIED.);
#3177=B_SPLINE_CURVE_WITH_KNOTS('',3,(#161378,#161379,#161380,#161381,#161382,
#161383,#161384,#161385,#161386,#161387,#161388,#161389,#161390,#161391,
#161392,#161393,#161394,#161395,#161396),.UNSPECIFIED.,.F.,.F.,(4,3,3,3,
3,3,4),(-10.4923399949537,-10.4678394094587,-10.3929239454309,-10.3179640637741,
-10.2429787777672,-10.1679214833374,-10.1362407614956),.UNSPECIFIED.);
#3178=B_SPLINE_CURVE_WITH_KNOTS('',3,(#161397,#161398,#161399,#161400,#161401,
#161402,#161403,#161404,#161405,#161406,#161407,#161408,#161409,#161410,
#161411,#161412,#161413,#161414,#161415,#161416,#161417,#161418,#161419,
#161420,#161421,#161422,#161423,#161424,#161425,#161426,#161427,#161428,
#161429,#161430,#161431,#161432,#161433,#161434,#161435,#161436,#161437,
#161438,#161439,#161440,#161441,#161442,#161443,#161444,#161445,#161446,
#161447,#161448,#161449,#161450,#161451,#161452,#161453,#161454,#161455,
#161456,#161457,#161458,#161459,#161460,#161461,#161462,#161463,#161464,
#161465,#161466,#161467,#161468,#161469,#161470,#161471,#161472,#161473,
#161474,#161475,#161476,#161477,#161478,#161479,#161480,#161481,#161482,
#161483,#161484,#161485,#161486,#161487,#161488,#161489,#161490,#161491,
#161492,#161493,#161494,#161495,#161496,#161497,#161498,#161499,#161500,
#161501,#161502,#161503,#161504,#161505,#161506,#161507,#161508,#161509,
#161510,#161511,#161512,#161513,#161514,#161515,#161516,#161517,#161518,
#161519,#161520,#161521,#161522,#161523,#161524,#161525,#161526,#161527,
#161528,#161529,#161530,#161531,#161532,#161533,#161534,#161535,#161536,
#161537,#161538,#161539,#161540,#161541,#161542,#161543,#161544,#161545,
#161546,#161547,#161548,#161549,#161550,#161551,#161552,#161553,#161554,
#161555,#161556,#161557,#161558,#161559,#161560,#161561,#161562,#161563,
#161564,#161565,#161566,#161567,#161568,#161569,#161570,#161571,#161572,
#161573,#161574,#161575,#161576,#161577,#161578,#161579,#161580,#161581,
#161582,#161583,#161584,#161585,#161586,#161587,#161588,#161589,#161590,
#161591,#161592,#161593,#161594,#161595,#161596,#161597,#161598,#161599,
#161600,#161601,#161602,#161603,#161604,#161605,#161606,#161607,#161608,
#161609,#161610,#161611,#161612,#161613,#161614,#161615,#161616,#161617,
#161618,#161619,#161620,#161621,#161622,#161623,#161624,#161625,#161626,
#161627,#161628),.UNSPECIFIED.,.F.,.F.,(4,3,3,3,3,3,3,3,3,3,3,3,3,3,3,3,
3,3,3,3,3,3,3,3,3,3,3,3,3,3,3,3,3,3,3,3,3,3,3,3,3,3,3,3,3,3,3,3,3,3,3,3,
3,3,3,3,3,3,3,3,3,3,3,3,3,3,3,3,3,3,3,3,3,3,3,3,3,4),(-10.1362407613902,
-10.0404600103124,-9.96937086615116,-9.8903033587492,-9.81130884994392,
-9.73237564784757,-9.6534921071148,-9.57464662055245,-9.49582315096894,
-9.41701178211171,-9.33820199578966,-9.25938327602393,-9.18051803145294,
-9.10162909268758,-9.02267316761131,-8.97243377953605,-8.89828594006323,
-8.82419521271217,-8.75014642909095,-8.67611547493831,-8.60209659116966,
-8.5280531838428,-8.47396523622849,-8.38323357259632,-8.29201898422131,
-8.20037668423165,-8.10864103046863,-8.01701229140009,-7.97549669292093,
-7.89958045794402,-7.8237135551364,-7.7478816022398,-7.67206048741651,-7.59624643142938,
-7.52040599733432,-7.47702814961337,-7.39512802038051,-7.31320693723104,
-7.22954510449973,-7.14756893457477,-7.06306427044029,-6.97855960630581,
-6.89601880972164,-6.8134943777379,-6.73014354905299,-6.64766910379144,
-6.56388008339485,-6.48009106299825,-6.40390489046263,-6.32774052041723,
-6.25158385234168,-6.17539790943762,-6.09919606680476,-6.02293430473634,
-5.9816225196907,-5.89404183989763,-5.80644096685919,-5.71892858368981,
-5.63152502623376,-5.54438007077154,-5.48315397638314,-5.40596340742709,
-5.32877675294137,-5.25158093002387,-5.17433419106375,-5.09705876196652,
-5.01970908073965,-4.98468543307558,-4.90776221233483,-4.83091062748332,
-4.75332417311467,-4.67657256393022,-4.59984318628236,-4.52312254376973,
-4.44489665596082,-4.36812994750742,-4.28917447002076,-4.2102189925341),
 .UNSPECIFIED.);
#3179=B_SPLINE_CURVE_WITH_KNOTS('',3,(#161632,#161633,#161634,#161635,#161636,
#161637,#161638,#161639,#161640,#161641,#161642,#161643,#161644,#161645,
#161646,#161647,#161648,#161649,#161650,#161651,#161652,#161653,#161654,
#161655,#161656,#161657,#161658,#161659,#161660,#161661,#161662,#161663,
#161664,#161665,#161666,#161667,#161668,#161669,#161670,#161671,#161672,
#161673,#161674,#161675,#161676,#161677,#161678,#161679,#161680,#161681,
#161682,#161683,#161684,#161685,#161686),.UNSPECIFIED.,.F.,.F.,(4,3,3,3,
3,3,3,3,3,3,3,3,3,3,3,3,3,3,4),(14.3988535768134,14.4773090887871,14.5557627497234,
14.6342164121779,14.7126808485184,14.7911453674607,14.8696199926236,14.897322120121,
14.9731691685373,15.0489941245849,15.1248067164951,15.2006302452213,15.2764581123458,
15.3523191565515,15.3957906634286,15.4769611354302,15.5581346632558,15.639296551796,
15.7079632679496),.UNSPECIFIED.);
#3180=B_SPLINE_CURVE_WITH_KNOTS('',3,(#161690,#161691,#161692,#161693,#161694,
#161695,#161696,#161697),.UNSPECIFIED.,.F.,.F.,(4,2,2,4),(13.8754803054958,
14.7048380819337,15.5341958583716,15.7079632679496),.UNSPECIFIED.);
#3181=B_SPLINE_CURVE_WITH_KNOTS('',3,(#161699,#161700,#161701,#161702,#161703,
#161704,#161705,#161706,#161707,#161708,#161709,#161710,#161711,#161712,
#161713),.UNSPECIFIED.,.F.,.F.,(4,1,1,1,1,1,1,1,1,1,1,1,4),(15.7079632679496,
15.8426561601993,16.8395932468144,17.338061790122,17.8365303334295,18.3349988767371,
18.8334674200446,19.3319359633522,19.8304045066598,20.3288730499673,20.8273415932749,
21.82427867989,21.9911485751291),.UNSPECIFIED.);
#3182=B_SPLINE_CURVE_WITH_KNOTS('',3,(#161715,#161716,#161717,#161718,#161719,
#161720,#161721,#161722,#161723,#161724,#161725,#161726,#161727,#161728,
#161729,#161730,#161731,#161732,#161733,#161734,#161735,#161736,#161737,
#161738,#161739,#161740,#161741,#161742,#161743,#161744,#161745,#161746,
#161747,#161748,#161749,#161750,#161751,#161752,#161753,#161754,#161755,
#161756,#161757,#161758,#161759,#161760,#161761,#161762,#161763,#161764,
#161765,#161766,#161767,#161768,#161769,#161770,#161771,#161772,#161773,
#161774,#161775,#161776,#161777,#161778,#161779,#161780,#161781,#161782,
#161783,#161784,#161785,#161786,#161787,#161788,#161789,#161790,#161791,
#161792,#161793,#161794,#161795,#161796,#161797,#161798,#161799,#161800,
#161801,#161802,#161803,#161804,#161805,#161806,#161807,#161808,#161809,
#161810,#161811,#161812,#161813,#161814,#161815,#161816,#161817,#161818,
#161819,#161820,#161821,#161822,#161823,#161824,#161825,#161826,#161827,
#161828,#161829,#161830,#161831,#161832,#161833,#161834,#161835,#161836,
#161837,#161838,#161839,#161840,#161841,#161842,#161843,#161844,#161845,
#161846,#161847,#161848,#161849,#161850,#161851,#161852,#161853,#161854,
#161855,#161856,#161857,#161858,#161859,#161860,#161861,#161862,#161863,
#161864,#161865,#161866,#161867,#161868,#161869,#161870,#161871,#161872,
#161873,#161874,#161875,#161876,#161877,#161878,#161879,#161880,#161881,
#161882,#161883,#161884,#161885,#161886,#161887,#161888,#161889,#161890,
#161891,#161892,#161893,#161894,#161895,#161896,#161897,#161898,#161899,
#161900,#161901,#161902,#161903,#161904,#161905,#161906,#161907,#161908,
#161909,#161910,#161911,#161912,#161913,#161914,#161915,#161916,#161917,
#161918,#161919,#161920,#161921,#161922,#161923,#161924,#161925,#161926,
#161927,#161928,#161929,#161930,#161931,#161932,#161933,#161934,#161935,
#161936,#161937,#161938,#161939,#161940,#161941,#161942,#161943,#161944,
#161945,#161946,#161947,#161948,#161949,#161950,#161951,#161952,#161953,
#161954,#161955,#161956,#161957,#161958,#161959,#161960,#161961,#161962,
#161963,#161964,#161965,#161966,#161967,#161968,#161969,#161970),
 .UNSPECIFIED.,.F.,.F.,(4,3,3,3,3,3,3,3,3,3,3,3,3,3,3,3,3,3,3,3,3,3,3,3,
3,3,3,3,3,3,3,3,3,3,3,3,3,3,3,3,3,3,3,3,3,3,3,3,3,3,3,3,3,3,3,3,3,3,3,3,
3,3,3,3,3,3,3,3,3,3,3,3,3,3,3,3,3,3,3,3,3,3,3,3,3,4),(21.9911485751291,
22.063496052357,22.1357752717274,22.2080149164767,22.28022855992,22.3227472231976,
22.3984962342701,22.4742911622871,22.5501412873131,22.6261033785794,22.702127044247,
22.7782701758204,22.8212157665051,22.8974244542329,22.9735651300765,23.0496482567728,
23.1256842565747,23.2016835182255,23.2787421850874,23.3547054036644,23.4306649451627,
23.5066302188929,23.5845108774497,23.6605386368451,23.7393457449827,23.8181528531202,
23.8895771968369,23.9609483903943,24.0322800260588,24.1035944219084,24.1748961647337,
24.2462226946391,24.3166213964278,24.4043263537643,24.4925021480966,24.5811059728463,
24.669805701723,24.7584014261205,24.8150899397353,24.8880590784629,24.9609827620746,
25.0338739797433,25.1067558678726,25.1796304740047,25.2525331111681,25.3135584830429,
25.3928598158705,25.4721833074765,25.5515264797574,25.6309001340357,25.7102823939454,
25.7896797474913,25.8120270263505,25.8914240280869,25.9708073030149,26.0501743520023,
26.1295191321404,26.2088417487659,26.2881355804246,26.310495569658,26.3833981064024,
26.4562781007974,26.5291485083777,26.6020449917875,26.6749537871511,26.7479222399894,
26.8089641129656,26.8975383090898,26.9862385321724,27.0748052013842,27.1631484764552,
27.2509180668742,27.3074326562731,27.3787561671641,27.4500599299111,27.5213574458225,
27.5926899541536,27.6640383256156,27.7354589933113,27.8059011995807,27.8879447479105,
27.9699232619414,28.0517634418163,28.1335007431438,28.2150493567445,28.2743338822451),
 .UNSPECIFIED.);
#3183=B_SPLINE_CURVE_WITH_KNOTS('',3,(#161972,#161973,#161974,#161975,#161976,
#161977,#161978,#161979,#161980,#161981,#161982,#161983,#161984,#161985,
#161986,#161987,#161988,#161989,#161990,#161991,#161992,#161993,#161994,
#161995,#161996,#161997,#161998,#161999,#162000,#162001,#162002,#162003,
#162004,#162005,#162006,#162007,#162008,#162009,#162010,#162011,#162012,
#162013,#162014,#162015,#162016,#162017,#162018,#162019,#162020,#162021,
#162022,#162023,#162024,#162025,#162026,#162027,#162028,#162029,#162030,
#162031,#162032,#162033,#162034,#162035,#162036,#162037,#162038,#162039,
#162040,#162041,#162042,#162043,#162044,#162045,#162046,#162047,#162048,
#162049,#162050,#162051,#162052,#162053,#162054,#162055,#162056,#162057,
#162058,#162059,#162060,#162061,#162062,#162063,#162064,#162065,#162066,
#162067,#162068,#162069,#162070,#162071,#162072,#162073,#162074,#162075,
#162076,#162077,#162078,#162079,#162080,#162081,#162082,#162083,#162084,
#162085,#162086,#162087,#162088,#162089,#162090,#162091,#162092,#162093,
#162094,#162095,#162096,#162097,#162098,#162099,#162100,#162101,#162102,
#162103,#162104,#162105,#162106,#162107,#162108,#162109,#162110,#162111,
#162112,#162113,#162114,#162115,#162116,#162117,#162118,#162119,#162120,
#162121,#162122,#162123,#162124,#162125,#162126,#162127,#162128,#162129,
#162130,#162131,#162132,#162133,#162134,#162135,#162136,#162137,#162138,
#162139,#162140,#162141,#162142,#162143,#162144,#162145,#162146,#162147,
#162148,#162149,#162150,#162151,#162152,#162153,#162154,#162155,#162156,
#162157,#162158,#162159,#162160,#162161,#162162,#162163,#162164,#162165,
#162166,#162167,#162168,#162169,#162170,#162171,#162172,#162173,#162174,
#162175,#162176,#162177,#162178,#162179,#162180,#162181,#162182,#162183,
#162184,#162185,#162186,#162187,#162188,#162189,#162190,#162191,#162192,
#162193,#162194,#162195,#162196,#162197,#162198,#162199,#162200,#162201,
#162202,#162203,#162204,#162205,#162206,#162207,#162208,#162209,#162210,
#162211,#162212,#162213,#162214,#162215,#162216,#162217,#162218,#162219,
#162220,#162221,#162222,#162223,#162224,#162225,#162226,#162227),
 .UNSPECIFIED.,.F.,.F.,(4,3,3,3,3,3,3,3,3,3,3,3,3,3,3,3,3,3,3,3,3,3,3,3,
3,3,3,3,3,3,3,3,3,3,3,3,3,3,3,3,3,3,3,3,3,3,3,3,3,3,3,3,3,3,3,3,3,3,3,3,
3,3,3,3,3,3,3,3,3,3,3,3,3,3,3,3,3,3,3,3,3,3,3,3,3,4),(28.2743338823087,
28.3524992901552,28.4307348821981,28.5090430266781,28.5874765565581,28.6659730322945,
28.7445841671321,28.8028382861958,28.8789711486772,28.9550108400185,29.030966835712,
29.1068252686922,29.1826263227681,29.2583656341798,29.3013068295034,29.3770491999729,
29.452837326493,29.5286805032169,29.604635467491,29.6806519059134,29.7567877075728,
29.7997753728109,29.8759859523571,29.9521285556643,30.0282136410446,30.1042516263436,
30.1802528959144,30.2573103413534,30.3332756024773,30.4092371933377,30.4852045193935,
30.5630815044016,30.6391113008366,30.7179118801313,30.796712459426,30.8681357340553,
30.9395058607466,31.0108364320444,31.0821497693047,31.1534504559005,31.2247759371654,
31.2951810027336,31.3828864933078,31.4710628571004,31.5596672692188,31.6483675776298,
31.7369638390569,31.7936495460412,31.8666189899611,31.9395429805229,32.0124345067303,
32.0853167051164,32.1581916226244,32.2310945717994,32.2921180893487,32.3714188737895,
32.4507418047674,32.530084407287,32.6094574849733,32.6888391664853,32.7682359441056,
32.7905866326563,32.8699840270845,32.9493677006684,33.0287351520635,33.1080803356296,
33.1874033546504,33.2666975840301,33.2890551759638,33.3619575762874,33.4348374333879,
33.5077077028764,33.5806040473371,33.6535127031778,33.7264810161821,33.7875237192714,
33.8760980508646,33.9647984163178,34.053365228401,34.141708641946,34.2294783585552,
34.2859922625789,34.3543180996439,34.4226219070607,34.4909372077778,34.5575191894883),
 .UNSPECIFIED.);
#3184=B_SPLINE_CURVE_WITH_KNOTS('',3,(#162229,#162230,#162231,#162232,#162233,
#162234,#162235,#162236,#162237,#162238,#162239,#162240,#162241,#162242,
#162243,#162244,#162245,#162246,#162247,#162248,#162249,#162250,#162251,
#162252,#162253,#162254,#162255,#162256,#162257,#162258,#162259,#162260,
#162261,#162262,#162263,#162264,#162265,#162266,#162267,#162268,#162269,
#162270,#162271,#162272,#162273,#162274,#162275,#162276,#162277,#162278,
#162279,#162280,#162281,#162282,#162283,#162284,#162285,#162286,#162287,
#162288,#162289,#162290,#162291,#162292,#162293,#162294,#162295,#162296,
#162297,#162298,#162299,#162300,#162301,#162302,#162303,#162304,#162305,
#162306,#162307,#162308,#162309,#162310,#162311,#162312,#162313,#162314,
#162315,#162316,#162317,#162318,#162319,#162320,#162321,#162322,#162323,
#162324,#162325,#162326,#162327,#162328,#162329,#162330,#162331,#162332,
#162333,#162334,#162335,#162336,#162337,#162338,#162339,#162340,#162341,
#162342,#162343,#162344,#162345,#162346,#162347,#162348,#162349,#162350,
#162351,#162352,#162353,#162354,#162355,#162356,#162357,#162358,#162359,
#162360,#162361,#162362,#162363,#162364,#162365,#162366,#162367,#162368,
#162369,#162370,#162371,#162372,#162373,#162374,#162375,#162376,#162377,
#162378,#162379,#162380,#162381,#162382,#162383,#162384,#162385,#162386,
#162387,#162388,#162389,#162390,#162391,#162392,#162393,#162394,#162395,
#162396,#162397,#162398,#162399,#162400,#162401,#162402,#162403,#162404,
#162405,#162406,#162407,#162408,#162409,#162410,#162411,#162412,#162413,
#162414,#162415,#162416,#162417,#162418,#162419,#162420,#162421,#162422,
#162423,#162424,#162425,#162426,#162427,#162428,#162429,#162430,#162431,
#162432,#162433,#162434,#162435,#162436,#162437,#162438,#162439,#162440,
#162441,#162442,#162443,#162444,#162445,#162446,#162447,#162448,#162449,
#162450,#162451,#162452,#162453,#162454,#162455,#162456,#162457,#162458,
#162459,#162460,#162461,#162462,#162463,#162464,#162465,#162466,#162467,
#162468,#162469,#162470,#162471,#162472,#162473,#162474,#162475,#162476,
#162477,#162478,#162479,#162480,#162481,#162482,#162483,#162484,#162485,
#162486,#162487,#162488,#162489,#162490,#162491,#162492,#162493,#162494,
#162495,#162496,#162497,#162498,#162499,#162500,#162501,#162502,#162503,
#162504,#162505,#162506,#162507,#162508,#162509,#162510,#162511,#162512,
#162513,#162514,#162515,#162516,#162517,#162518,#162519,#162520,#162521,
#162522,#162523,#162524,#162525,#162526,#162527,#162528,#162529,#162530,
#162531,#162532,#162533,#162534,#162535,#162536,#162537,#162538,#162539,
#162540,#162541,#162542,#162543,#162544,#162545,#162546,#162547,#162548,
#162549,#162550,#162551,#162552,#162553,#162554,#162555,#162556,#162557,
#162558,#162559,#162560,#162561,#162562,#162563,#162564,#162565,#162566,
#162567,#162568,#162569,#162570,#162571,#162572,#162573,#162574,#162575,
#162576,#162577,#162578,#162579,#162580,#162581,#162582,#162583,#162584,
#162585,#162586,#162587,#162588,#162589,#162590,#162591,#162592,#162593,
#162594,#162595,#162596,#162597,#162598,#162599,#162600,#162601,#162602,
#162603,#162604,#162605,#162606,#162607,#162608,#162609,#162610,#162611,
#162612,#162613,#162614,#162615,#162616,#162617,#162618,#162619,#162620,
#162621,#162622,#162623,#162624,#162625,#162626,#162627,#162628,#162629,
#162630,#162631,#162632,#162633,#162634,#162635,#162636,#162637,#162638,
#162639,#162640,#162641,#162642,#162643,#162644,#162645,#162646,#162647,
#162648,#162649,#162650,#162651,#162652,#162653,#162654,#162655,#162656,
#162657,#162658,#162659,#162660,#162661,#162662,#162663,#162664,#162665,
#162666,#162667,#162668,#162669,#162670,#162671,#162672,#162673,#162674,
#162675,#162676,#162677,#162678,#162679,#162680,#162681,#162682,#162683,
#162684,#162685,#162686,#162687,#162688,#162689,#162690,#162691,#162692,
#162693,#162694,#162695,#162696,#162697,#162698,#162699,#162700,#162701,
#162702,#162703,#162704,#162705,#162706,#162707,#162708,#162709,#162710,
#162711,#162712,#162713,#162714,#162715,#162716,#162717,#162718,#162719,
#162720,#162721,#162722,#162723,#162724,#162725,#162726,#162727,#162728,
#162729,#162730,#162731,#162732,#162733,#162734,#162735,#162736,#162737,
#162738,#162739,#162740,#162741,#162742,#162743,#162744,#162745,#162746,
#162747,#162748,#162749,#162750,#162751,#162752,#162753,#162754,#162755,
#162756,#162757,#162758,#162759,#162760,#162761,#162762,#162763,#162764,
#162765,#162766,#162767,#162768,#162769,#162770,#162771,#162772,#162773,
#162774,#162775,#162776,#162777,#162778,#162779,#162780,#162781,#162782,
#162783,#162784,#162785,#162786,#162787,#162788,#162789,#162790,#162791,
#162792,#162793,#162794,#162795,#162796,#162797,#162798,#162799,#162800,
#162801,#162802,#162803,#162804,#162805,#162806,#162807,#162808,#162809,
#162810,#162811,#162812,#162813,#162814,#162815,#162816,#162817,#162818,
#162819,#162820,#162821,#162822,#162823,#162824,#162825,#162826,#162827,
#162828,#162829,#162830,#162831,#162832,#162833,#162834,#162835,#162836,
#162837,#162838,#162839,#162840,#162841,#162842,#162843,#162844,#162845,
#162846,#162847,#162848,#162849,#162850,#162851,#162852,#162853,#162854,
#162855,#162856,#162857,#162858,#162859,#162860,#162861,#162862,#162863,
#162864,#162865,#162866,#162867,#162868,#162869,#162870,#162871,#162872,
#162873,#162874,#162875,#162876,#162877,#162878,#162879,#162880,#162881,
#162882,#162883,#162884,#162885,#162886,#162887,#162888,#162889,#162890,
#162891,#162892,#162893,#162894,#162895,#162896,#162897,#162898,#162899,
#162900,#162901,#162902,#162903,#162904,#162905,#162906,#162907,#162908,
#162909,#162910,#162911,#162912,#162913,#162914,#162915,#162916,#162917,
#162918,#162919,#162920,#162921,#162922,#162923,#162924,#162925,#162926,
#162927,#162928,#162929,#162930,#162931,#162932,#162933,#162934),
 .UNSPECIFIED.,.F.,.F.,(4,2,2,2,2,2,2,2,2,2,2,2,2,2,2,2,2,2,2,2,2,2,2,2,
2,2,2,2,2,2,2,2,2,2,2,2,2,2,2,2,2,2,2,2,2,2,2,2,2,2,2,2,2,2,2,2,2,2,2,2,
2,2,2,2,2,2,2,2,2,2,2,2,2,2,2,2,2,2,2,2,2,2,2,2,2,2,2,2,2,2,2,2,2,2,2,2,
2,2,2,2,2,2,2,2,2,2,2,2,2,2,2,2,2,2,2,2,2,2,2,2,2,2,2,2,2,2,2,2,2,2,2,2,
2,2,2,2,2,2,2,2,2,2,2,2,2,2,2,2,2,2,2,2,2,2,2,2,2,2,2,2,2,2,2,2,2,2,2,2,
2,2,2,2,2,2,2,2,2,2,2,2,2,2,2,2,2,2,2,2,2,2,2,2,2,2,2,2,2,2,2,2,2,2,2,2,
2,2,2,2,2,2,2,2,2,2,2,2,2,2,2,2,2,2,2,2,2,2,2,2,2,2,2,2,2,2,2,2,2,2,2,2,
2,2,2,2,2,2,2,2,2,2,2,2,2,2,2,2,2,2,2,2,2,2,2,2,2,2,2,2,2,2,2,2,2,2,2,2,
2,2,2,2,2,2,2,2,2,2,2,2,2,2,2,2,2,2,2,2,2,2,2,2,2,2,2,2,2,2,2,2,2,2,2,2,
2,2,2,2,2,2,2,2,2,2,2,2,2,2,2,2,2,2,2,2,2,2,2,2,2,2,2,2,2,2,2,2,2,2,2,2,
2,2,2,2,4),(0.0017515687772967,0.138325053356595,0.151276780243772,0.155417338248591,
0.159555236496333,0.162228688491512,0.164324512341607,0.166279619726446,
0.168343676188257,0.171236107367478,0.178859989943288,0.286447337701843,
0.306422960151675,0.337450622805883,0.381798567778655,0.483543771061002,
0.552589452192858,0.587426297663754,0.593869037401524,0.597335588765897,
0.599930739551836,0.602778066778233,0.6078501347858,0.62299837233455,0.88925622396032,
0.966227315679684,0.996167927523107,1.01353649868113,1.01789582511869,1.0200448176947,
1.02229467168772,1.02488615663501,1.02926826985985,1.0450887399084,1.16611709033031,
1.3093237217122,1.36123288072709,1.38592794762347,1.39573370032208,1.40257220206871,
1.40924126413931,1.41795089558398,1.43266333782643,1.55754294091557,1.71762008710786,
1.76930642454278,1.77894991119294,1.78246797805769,1.78458335780597,1.78685804959934,
1.78979118646403,1.79608054282211,1.85896281509135,2.06879091335953,2.19079911093772,
2.20049647818805,2.20459181449844,2.20754914304387,2.21024052938154,2.21383347180757,
2.22257891539509,2.30606328763443,2.40162405827975,2.51628376135754,2.61951894546772,
2.63366657267915,2.63762610262992,2.640028241587,2.64218952728719,2.6449398560019,
2.64929451210425,2.6711444683841,2.76498742292603,2.93502751766293,3.05473296397257,
3.0834464034837,3.09752924238869,3.10880083224543,3.1216989272624,3.14370797869731,
3.26255241531138,3.38249007778415,3.40709068860276,3.42416763503091,3.43135831811938,
3.43636855510755,3.44193711502854,3.45221546534293,3.5018559733613,3.54515239928105,
3.58332661591931,3.61042988000154,3.62352680689319,3.6330475862313,3.64488421775403,
3.66524744499144,3.758830697354,3.80476408814399,3.82956825981784,3.83778725084525,
3.84371036254889,3.85037319087125,3.86168670320928,3.91027566677167,3.9129985584667,
3.91368009540159,3.91779784471794,4.01435332239539,4.06897923977882,4.09050616813681,
4.10696608988951,4.12612287126621,4.19034722147345,4.22948196296821,4.24279877693456,
4.2561098056066,4.28990075193618,4.33635578632061,4.35846208144909,4.37794013402896,
4.39436665437786,4.41509029525811,4.46205924034342,4.487048611373,4.58626846791351,
4.6128945658258,4.63105975539313,4.63905473275387,4.64504281643948,4.65160163012007,
4.66452176213023,4.7205301054893,4.79074110597474,4.81028622731075,4.83668892242472,
4.84969338544162,4.86021928284336,4.87249061078675,4.89446875201819,4.98252906666981,
5.01724332579486,5.03807694217747,5.04612645537648,5.05184511077815,5.05786608123225,
5.0685289742,5.11472989385464,5.23691881353043,5.27772913550408,5.3461004621232,
5.36611083947209,5.37845710219832,5.38984318575178,5.40493041891499,5.43943120713386,
5.62925048650287,5.75652278427547,5.83353688349086,5.83952285080448,5.84242323059355,
5.84449009585872,5.84666379680256,5.84950935941345,5.85557763469844,5.95740276971331,
6.02263446905738,6.10472251589366,6.26147037625291,6.27125445803611,6.27505948910482,
6.27780537262738,6.2807243592377,6.2845956769982,6.29304455380973,6.44850059962419,
6.68156938000003,6.69379067055946,6.69780794539533,6.70004380724059,6.70229680535922,
6.70509137168914,6.71052801700793,6.74742507824072,6.8482799829783,7.03844185882802,
7.06470219409981,7.07492136391038,7.08114810646387,7.08772294922664,7.09591661711547,
7.11211867733351,7.2921261147837,7.34270829555601,7.45286986577465,7.45987475668961,
7.46266516599736,7.46497423176599,7.46732637697601,7.47073288629693,7.47957714845698,
7.51965030796423,7.54473192479103,7.69220648587477,7.86843571804428,7.87949254280103,
7.88350069772908,7.88630163968428,7.88890837742962,7.89247223464457,7.89936987780593,
7.94439721742122,8.05083804224671,8.19808001189696,8.30788654712594,8.31529884038834,
8.31815775804147,8.320213434276,8.32239191784763,8.32526866233631,8.33137560922606,
8.38385747816661,8.44272943600845,8.53370538440831,8.72343406498634,8.75905557155854,
8.77320749174054,8.78477657451478,8.79531839325679,8.81059912094329,8.84893515011331,
8.90440066059995,8.98993905574617,9.02152384109188,9.06993198504814,9.09958347649567,
9.10888413783582,9.11408272678337,9.11876512707595,9.11878073989593,9.11879631953773,
9.11881186501636,9.1188273767727,9.11884285512973,9.11885830041947,9.11887371297768,
9.11888909317892,9.11890444133229,9.11891975775977,9.11893504289695,9.11895029703402,
9.11896552050978,9.11898071368812,9.1189958768656,9.119011010385,9.11902611459777,
9.11904118976973,9.11905623627824,9.11907125448075,9.11908624461243,9.11910120699744,
9.11911614193394,9.11913104967132,9.11914593063062,9.11916078510116,9.11917561337012,
9.11919041571846,9.11920519247744,9.11921994397121,9.11923467049878,9.11924937232786,
9.11926404973785,9.11927870301223,9.11929333243354,9.11930793832082,9.11932252092869,
9.11933708044505,9.11935161719383,9.11936613150718,9.11938062365889,9.11939509398288,
9.11940954269116,9.1194239700672,9.11943837637845,9.11945276187849,9.11946712679392,
9.1194814714212,9.11949579605101,9.11951010091221,9.11952438627004,9.11953865241671,
9.12513615870805,9.13307319168024,9.14667555097134,9.17821235740199,9.26435424754514,
9.290813057662,9.3037988742816,9.31360821167378,9.31384830845949,9.314072301997,
9.31428127100334,9.3144762254085,9.3146581096178,9.31482780594748,9.31498613808514,
9.3151338745275,9.31527173195236,9.31540037847771,9.31552043679201,9.31563248713119,
9.31573707011319,9.31583468940297,9.31592581422803,9.3160108817309,9.31609029918427,
9.31616444604063,9.31628967332175,9.31641312126722,9.31653482283826,9.31665481348598,
9.31677312663185,9.32844945619472,9.35354311887971,9.38726251861441,9.44199029596007,
9.44931792646235,9.50578435580815,9.51596452740012,9.52148073677252,9.52707785530135,
9.53481458275568,9.55287949424507,9.57963179856445,9.68000740471447,9.74617233089887,
9.76659357125358,9.78173234185024,9.79750085548905,9.8152918680815,9.82367586210791,
9.84619224069513,9.90827042514558,9.91839595744867,9.92930854127623,9.94149638644303,
9.96101002456414,10.0154532726687,10.0460807300154,10.0618751072877,10.0772264137265,
10.0932476479946,10.1148962593431,10.2289668597367),.UNSPECIFIED.);
#3185=B_SPLINE_CURVE_WITH_KNOTS('',3,(#162936,#162937,#162938,#162939,#162940,
#162941,#162942,#162943,#162944,#162945,#162946,#162947,#162948,#162949,
#162950,#162951,#162952,#162953,#162954,#162955,#162956,#162957,#162958,
#162959,#162960,#162961,#162962,#162963,#162964,#162965,#162966,#162967,
#162968,#162969,#162970,#162971,#162972,#162973,#162974,#162975,#162976,
#162977,#162978,#162979,#162980,#162981,#162982,#162983,#162984,#162985,
#162986,#162987,#162988,#162989,#162990,#162991,#162992,#162993,#162994,
#162995,#162996,#162997,#162998,#162999,#163000,#163001,#163002,#163003,
#163004,#163005,#163006,#163007,#163008,#163009,#163010,#163011,#163012,
#163013,#163014,#163015,#163016,#163017,#163018,#163019,#163020,#163021,
#163022,#163023,#163024,#163025,#163026,#163027,#163028,#163029,#163030,
#163031,#163032,#163033,#163034,#163035,#163036,#163037,#163038,#163039,
#163040,#163041,#163042,#163043,#163044,#163045,#163046,#163047,#163048,
#163049,#163050,#163051,#163052,#163053,#163054,#163055,#163056,#163057,
#163058,#163059,#163060,#163061,#163062,#163063,#163064,#163065,#163066,
#163067,#163068,#163069,#163070,#163071,#163072,#163073,#163074,#163075,
#163076,#163077,#163078,#163079,#163080,#163081,#163082,#163083,#163084,
#163085,#163086,#163087,#163088,#163089,#163090,#163091,#163092,#163093,
#163094,#163095,#163096,#163097,#163098,#163099,#163100,#163101,#163102,
#163103,#163104,#163105,#163106,#163107,#163108,#163109,#163110,#163111,
#163112,#163113,#163114,#163115,#163116,#163117,#163118,#163119,#163120,
#163121,#163122,#163123,#163124,#163125,#163126,#163127,#163128,#163129,
#163130,#163131,#163132,#163133,#163134,#163135,#163136,#163137,#163138,
#163139,#163140,#163141,#163142,#163143,#163144,#163145,#163146,#163147,
#163148,#163149,#163150,#163151,#163152,#163153,#163154,#163155,#163156,
#163157,#163158,#163159,#163160,#163161,#163162,#163163,#163164,#163165,
#163166,#163167,#163168,#163169,#163170,#163171,#163172,#163173,#163174,
#163175,#163176,#163177,#163178,#163179,#163180,#163181,#163182,#163183,
#163184,#163185,#163186,#163187,#163188,#163189,#163190,#163191,#163192,
#163193,#163194,#163195,#163196,#163197,#163198,#163199,#163200,#163201,
#163202,#163203,#163204,#163205,#163206,#163207,#163208,#163209,#163210,
#163211,#163212,#163213,#163214,#163215,#163216,#163217,#163218,#163219,
#163220,#163221,#163222,#163223,#163224,#163225,#163226,#163227,#163228,
#163229,#163230,#163231,#163232,#163233,#163234,#163235,#163236,#163237,
#163238,#163239,#163240,#163241,#163242,#163243,#163244,#163245,#163246,
#163247,#163248,#163249,#163250,#163251,#163252,#163253,#163254,#163255,
#163256,#163257,#163258,#163259,#163260,#163261,#163262,#163263,#163264,
#163265,#163266,#163267,#163268,#163269,#163270,#163271,#163272,#163273,
#163274,#163275,#163276,#163277,#163278,#163279,#163280,#163281,#163282,
#163283,#163284,#163285,#163286,#163287,#163288,#163289,#163290,#163291,
#163292,#163293,#163294,#163295,#163296,#163297,#163298,#163299,#163300,
#163301,#163302,#163303,#163304,#163305,#163306,#163307,#163308,#163309,
#163310,#163311,#163312,#163313,#163314,#163315,#163316,#163317,#163318,
#163319,#163320,#163321,#163322,#163323,#163324,#163325,#163326,#163327,
#163328,#163329,#163330,#163331,#163332,#163333,#163334,#163335,#163336,
#163337,#163338,#163339,#163340,#163341,#163342,#163343,#163344,#163345,
#163346,#163347,#163348,#163349,#163350,#163351,#163352,#163353,#163354,
#163355,#163356,#163357,#163358,#163359,#163360,#163361,#163362,#163363,
#163364,#163365,#163366,#163367,#163368,#163369,#163370,#163371,#163372,
#163373,#163374,#163375,#163376,#163377,#163378,#163379,#163380,#163381,
#163382,#163383,#163384,#163385,#163386,#163387,#163388,#163389,#163390,
#163391,#163392,#163393,#163394,#163395,#163396,#163397,#163398,#163399,
#163400,#163401,#163402,#163403,#163404,#163405,#163406,#163407,#163408,
#163409,#163410,#163411,#163412,#163413,#163414,#163415,#163416,#163417,
#163418,#163419,#163420,#163421,#163422,#163423,#163424,#163425,#163426,
#163427,#163428,#163429,#163430,#163431,#163432,#163433,#163434,#163435,
#163436,#163437,#163438,#163439,#163440,#163441,#163442,#163443,#163444,
#163445,#163446,#163447,#163448,#163449,#163450,#163451,#163452,#163453,
#163454,#163455,#163456,#163457,#163458,#163459,#163460,#163461,#163462,
#163463,#163464,#163465,#163466,#163467),.UNSPECIFIED.,.F.,.F.,(4,2,2,2,
2,2,2,2,2,2,2,2,2,2,2,2,2,2,2,2,2,2,2,2,2,2,2,2,2,2,2,2,2,2,2,2,2,2,2,2,
2,2,2,2,2,2,2,2,2,2,2,2,2,2,2,2,2,2,2,2,2,2,2,2,2,2,2,2,2,2,2,2,2,2,2,2,
2,2,2,2,2,2,2,2,2,2,2,2,2,2,2,2,2,2,2,2,2,2,2,2,2,2,2,2,2,2,2,2,2,2,2,2,
2,2,2,2,2,2,2,2,2,2,2,2,2,2,2,2,2,2,2,2,2,2,2,2,2,2,2,2,2,2,2,2,2,2,2,2,
2,2,2,2,2,2,2,2,2,2,2,2,2,2,2,2,2,2,2,2,2,2,2,2,2,2,2,2,2,2,2,2,2,2,2,2,
2,2,2,2,2,2,2,2,2,2,2,2,2,2,2,2,2,2,2,2,2,2,2,2,2,2,2,2,2,2,2,2,2,2,2,2,
2,2,2,2,2,2,2,2,2,2,2,2,2,2,2,2,2,2,2,2,2,2,2,2,2,2,2,2,2,2,2,2,2,2,2,2,
2,2,2,2,2,2,2,2,2,4),(0.00102620743934878,0.0700209818904994,0.0806719562036417,
0.0876625602166402,0.0933455982497069,0.0987635694929107,0.10602105163566,
0.118954101730982,0.140940519298676,0.209927368824877,0.268278680050802,
0.290788123848363,0.2919857074657,0.293116341985048,0.29419909489967,0.295251736500306,
0.305095991739884,0.315213759000764,0.328817503760316,0.358985729663482,
0.453055377360456,0.476259475550913,0.487476149288899,0.496530106114982,
0.502362935886591,0.507952479037652,0.514967017977698,0.53441096837326,
0.663378493294355,0.774388809782231,0.808040657082333,0.820068145035925,
0.830549616056012,0.841938577459714,0.856814654914812,0.889668268399421,
1.01781338348057,1.19311357534889,1.25965708118509,1.27850067970099,1.28634410385851,
1.29211690711147,1.2950063661145,1.29718598972696,1.29923650175584,1.30207830880631,
1.30939161247657,1.4341398828131,1.54173678797794,1.71526985075659,1.72379199624076,
1.72767606657096,1.73059608260202,1.73333669055125,1.73712453524325,1.74681126620348,
1.898363775872,1.97547626769385,2.13789994777,2.14630839788965,2.14967966470455,
2.15203770884844,2.15433929067944,2.15710462687996,2.16396246266373,2.23778839586647,
2.48337361210746,2.50425612762181,2.5207052170681,2.52891807390989,2.53551225970664,
2.54167570172066,2.5515628889052,2.57578129448143,2.82408548684629,2.89769158901368,
2.90948589066238,2.9132945898873,2.91573226843855,2.91801364819259,2.92099323901915,
2.92598222351163,2.9596933461137,3.165804822578,3.31929548950605,3.33073917196909,
3.33511641802254,3.33812842403486,3.34107658092285,3.34462635678182,3.35347659320394,
3.43665628113804,3.47789038546963,3.65816755393568,3.75935762839008,3.76648180533531,
3.7695192772212,3.77172386934463,3.77373887638085,3.77644219370254,3.78308977881575,
3.87773376043939,3.99967004399163,4.17758947343506,4.21147312485926,4.22645416308629,
4.23781998571136,4.25020225283901,4.27040312051728,4.34103645665924,4.47438213190967,
4.52334182318996,4.54212774238508,4.55603631215657,4.56266520027506,4.56823060131556,
4.57527433558988,4.58662504521373,4.66167321453443,4.69769899208694,4.73617727699897,
4.75095049247094,4.76168106237837,4.77165913967037,4.78835947139651,4.84062578258731,
4.92440623133414,4.94156425673843,4.96119170028082,4.96876520393286,4.9740885556359,
4.98083171383756,4.99253057159583,5.05847221417962,5.0606767050835,5.11330849752744,
5.15365353057435,5.20049130544304,5.22120477625719,5.23762195018358,5.25708729763257,
5.27917829186422,5.32559172290031,5.35937866830028,5.37268531287157,5.38599123315558,
5.42502051697027,5.48935159506218,5.50848090263054,5.52493354984753,5.54647271440661,
5.60127777609871,5.69860381934907,5.69978175859626,5.75323504073444,5.76473709065591,
5.77143805049514,5.77676619526878,5.78442657528527,5.80469744512164,5.83799372064855,
5.95032276254109,5.97045843955424,5.98224423502657,5.99176770424688,6.00492814241617,
6.03242686949473,6.0714412386122,6.11453656211721,6.16299771366623,6.17319076156436,
6.17874083826709,6.18375076520503,6.1909769334548,6.20828153075202,6.23332523994474,
6.35370862854993,6.47125471359405,6.49319723231978,6.50607591877961,6.51734239045168,
6.53143448628335,6.56022510285602,6.68058966593425,6.8528966158712,6.96245257734062,
6.96914099139685,6.97180617002718,6.97401190368873,6.97625912026927,6.97951427689822,
6.98796906763584,6.99968093921829,7.03286204984243,7.06304267189232,7.2265002485369,
7.39008670450619,7.39998130684094,7.40380293181339,7.40655192432134,7.40946603371027,
7.41331704609155,7.42166713793362,7.55863755388565,7.74705828798871,7.81797439460717,
7.82438517814879,7.827340224763,7.82961719733814,7.8320642948198,7.83552560643319,
7.84588866273015,7.95965297673849,8.03807689306549,8.09222294330772,8.1826611921389,
8.19655832434229,8.2050279646888,8.21165495037634,8.21855984671554,8.22837613678482,
8.23955667813622,8.25950737175954,8.47155694349294,8.58044036235954,8.58744562595582,
8.5902348076198,8.5925423212446,8.59489234334112,8.59796594661942,8.60546728409272,
8.68905625519971,8.776979042251,8.96796635367108,9.0022192860846,9.00838741969961,
9.01213313976895,9.01504124778092,9.0181883553364,9.02318866121053,9.03933031646316,
9.13334434742648,9.2361744062263,9.30498849781451,9.43334371731024,9.44177802167838,
9.44479619338025,9.44689434784662,9.44883783825147,9.4514814362744,9.45655114230102,
9.4879687260255,9.59953843124879,9.69148493559475,9.82745307051558,9.88016251002461,
9.8981974190565,9.90892889271097,9.92035674372422,9.93152864887158,9.94633440437264,
9.97022941381108,10.0186624710519,10.1113075789678,10.1997473077657,10.2233318581722),
 .UNSPECIFIED.);
#3186=B_SPLINE_CURVE_WITH_KNOTS('',3,(#163469,#163470,#163471,#163472,#163473,
#163474,#163475,#163476,#163477,#163478,#163479,#163480,#163481,#163482,
#163483),.UNSPECIFIED.,.F.,.F.,(4,1,1,1,1,1,1,1,1,1,1,1,4),(59.6902604182067,
59.7078879712644,60.206356514572,60.7048250578795,61.2032936011871,61.7017621444946,
62.2002306878022,62.6986992311097,63.6956363177249,64.1941048610324,64.69257340434,
65.6895104909551,65.9734457253863),.UNSPECIFIED.);
#3187=B_SPLINE_CURVE_WITH_KNOTS('',3,(#163485,#163486,#163487,#163488,#163489,
#163490,#163491,#163492,#163493,#163494,#163495,#163496,#163497,#163498,
#163499,#163500,#163501,#163502,#163503,#163504,#163505,#163506,#163507,
#163508,#163509,#163510,#163511,#163512,#163513,#163514,#163515,#163516,
#163517,#163518,#163519,#163520,#163521,#163522,#163523,#163524,#163525,
#163526,#163527,#163528,#163529,#163530,#163531,#163532,#163533,#163534,
#163535,#163536,#163537,#163538,#163539,#163540,#163541,#163542,#163543,
#163544,#163545,#163546,#163547,#163548,#163549,#163550,#163551,#163552,
#163553,#163554,#163555,#163556,#163557,#163558,#163559,#163560,#163561,
#163562,#163563,#163564,#163565,#163566,#163567,#163568,#163569,#163570,
#163571,#163572,#163573,#163574,#163575,#163576,#163577,#163578,#163579,
#163580,#163581,#163582,#163583,#163584,#163585,#163586,#163587,#163588,
#163589,#163590,#163591,#163592,#163593,#163594,#163595,#163596,#163597,
#163598,#163599,#163600,#163601,#163602,#163603,#163604,#163605,#163606,
#163607,#163608,#163609,#163610,#163611,#163612,#163613,#163614,#163615,
#163616,#163617,#163618,#163619,#163620,#163621,#163622,#163623,#163624,
#163625,#163626,#163627,#163628,#163629,#163630,#163631,#163632,#163633,
#163634,#163635,#163636,#163637,#163638,#163639,#163640,#163641,#163642,
#163643,#163644,#163645,#163646,#163647,#163648,#163649,#163650,#163651,
#163652,#163653,#163654,#163655,#163656,#163657,#163658,#163659,#163660,
#163661,#163662,#163663,#163664,#163665,#163666,#163667,#163668,#163669,
#163670,#163671,#163672,#163673,#163674,#163675,#163676,#163677,#163678,
#163679,#163680,#163681,#163682,#163683,#163684,#163685,#163686,#163687,
#163688,#163689,#163690,#163691,#163692,#163693,#163694,#163695,#163696,
#163697,#163698,#163699,#163700,#163701,#163702,#163703,#163704,#163705,
#163706,#163707,#163708,#163709,#163710,#163711,#163712,#163713,#163714,
#163715,#163716,#163717,#163718,#163719,#163720,#163721,#163722,#163723,
#163724,#163725,#163726,#163727,#163728,#163729,#163730,#163731,#163732,
#163733,#163734,#163735,#163736,#163737,#163738,#163739,#163740,#163741,
#163742,#163743),.UNSPECIFIED.,.F.,.F.,(4,3,3,3,3,3,3,3,3,3,3,3,3,3,3,3,
3,3,3,3,3,3,3,3,3,3,3,3,3,3,3,3,3,3,3,3,3,3,3,3,3,3,3,3,3,3,3,3,3,3,3,3,
3,3,3,3,3,3,3,3,3,3,3,3,3,3,3,3,3,3,3,3,3,3,3,3,3,3,3,3,3,3,3,3,3,3,4),
(65.9734457253863,66.0415874873975,66.1097252065017,66.1778850487403,66.1879790342627,
66.2756845236033,66.3638608860217,66.4524652966393,66.541165603522,66.6297618634573,
66.6864475775702,66.7594170220203,66.8323410131141,66.9052325398549,66.9781147387756,
67.0509896568192,67.1238926065293,67.1849161208778,67.2642169048273,67.3435398353038,
67.4228824373142,67.5022555144866,67.581637195484,67.6610339725923,67.6833846641853,
67.7627820588542,67.8421657326823,67.9215331843232,68.0008783681353,68.0802013874019,
68.1594956170233,68.1818532074929,68.2547556077617,68.327635464807,68.4005057342406,
68.4734020786457,68.5463107344307,68.6192790473791,68.6803217508004,68.7688960824135,
68.8575964478861,68.9461632599889,69.0345066735528,69.122276390178,69.178790294108,
69.250113792458,69.3214175426133,69.3927150458857,69.4640475415319,69.5353959002714,
69.6068165552382,69.6772588374156,69.7533623334367,69.8294154795072,69.9054286697423,
69.981412269623,70.0573766229516,70.1344790355865,70.210450763625,70.2864350908839,
70.3624414325567,70.4403800554252,70.5164890948532,70.5953425094419,70.6741959240307,
70.750328796276,70.8263684973471,70.9023245027181,70.9781829452555,71.0539840088092,
71.1297233295435,71.1726644673382,71.248406832161,71.324194952911,71.4000381237537,
71.4759930820135,71.5520095143471,71.6281453098475,71.6711330106458,71.7483084662108,
71.8254087694881,71.902441172545,71.9794128876601,72.0563165758884,72.1331783316029,
72.20999778443,72.2566310325659),.UNSPECIFIED.);
#3188=B_SPLINE_CURVE_WITH_KNOTS('',3,(#163745,#163746,#163747,#163748,#163749,
#163750,#163751,#163752,#163753,#163754,#163755,#163756,#163757,#163758,
#163759,#163760,#163761,#163762,#163763,#163764,#163765,#163766,#163767,
#163768,#163769,#163770,#163771,#163772,#163773,#163774,#163775,#163776,
#163777,#163778,#163779,#163780,#163781,#163782,#163783,#163784,#163785,
#163786,#163787,#163788,#163789,#163790,#163791,#163792,#163793,#163794,
#163795,#163796,#163797,#163798,#163799,#163800,#163801,#163802,#163803,
#163804,#163805,#163806,#163807,#163808,#163809,#163810,#163811,#163812,
#163813,#163814,#163815,#163816,#163817,#163818,#163819,#163820,#163821,
#163822,#163823,#163824,#163825,#163826,#163827,#163828,#163829,#163830,
#163831,#163832,#163833,#163834,#163835,#163836,#163837,#163838,#163839,
#163840,#163841,#163842,#163843,#163844,#163845,#163846,#163847,#163848,
#163849,#163850,#163851,#163852,#163853,#163854,#163855,#163856,#163857,
#163858,#163859,#163860,#163861,#163862,#163863,#163864,#163865,#163866,
#163867,#163868,#163869,#163870,#163871,#163872,#163873,#163874,#163875,
#163876,#163877,#163878,#163879,#163880,#163881,#163882,#163883,#163884,
#163885,#163886,#163887,#163888,#163889,#163890,#163891,#163892,#163893,
#163894,#163895,#163896,#163897,#163898,#163899,#163900,#163901,#163902,
#163903,#163904,#163905,#163906,#163907,#163908,#163909,#163910,#163911,
#163912,#163913,#163914,#163915,#163916,#163917,#163918,#163919,#163920,
#163921,#163922,#163923,#163924,#163925,#163926,#163927,#163928,#163929,
#163930,#163931,#163932,#163933,#163934,#163935,#163936,#163937,#163938,
#163939,#163940,#163941,#163942,#163943,#163944,#163945,#163946,#163947,
#163948,#163949,#163950,#163951,#163952,#163953,#163954,#163955,#163956,
#163957,#163958,#163959,#163960,#163961,#163962,#163963,#163964,#163965,
#163966,#163967,#163968,#163969,#163970,#163971,#163972,#163973,#163974,
#163975,#163976,#163977,#163978,#163979,#163980,#163981,#163982,#163983,
#163984,#163985,#163986,#163987,#163988,#163989,#163990,#163991,#163992,
#163993,#163994,#163995,#163996,#163997,#163998,#163999,#164000),
 .UNSPECIFIED.,.F.,.F.,(4,3,3,3,3,3,3,3,3,3,3,3,3,3,3,3,3,3,3,3,3,3,3,3,
3,3,3,3,3,3,3,3,3,3,3,3,3,3,3,3,3,3,3,3,3,3,3,3,3,3,3,3,3,3,3,3,3,3,3,3,
3,3,3,3,3,3,3,3,3,3,3,3,3,3,3,3,3,3,3,3,3,3,3,3,3,4),(72.2566310326343,
72.341007590014,72.4257777283301,72.510706500726,72.59578785161,72.6680700972609,
72.7394933721108,72.810863499024,72.8821940705451,72.9535074080307,73.024808094853,
73.0961335763454,73.1665386405685,73.2542441299096,73.342420492328,73.4310249029457,
73.5197252098287,73.6083214697641,73.665007183876,73.7379766283261,73.8109006194199,
73.8837921461609,73.9566743450818,74.0295492631251,74.1024522128351,74.1634757271836,
74.242776511133,74.3220994416096,74.4014420436201,74.4808151207924,74.5601968017891,
74.6395935788977,74.6619442704911,74.74134166516,74.8207253389878,74.9000927906292,
74.9794379744413,75.0587609937076,75.1380552233294,75.1604128137987,75.2333152140674,
75.3061950711126,75.3790653405456,75.4519616849508,75.5248703407358,75.5978386536842,
75.6588813571063,75.7474556887191,75.8361560541932,75.924722866296,76.0130662798609,
76.1008359964866,76.1573499004138,76.2286733987638,76.2999771489191,76.371274652191,
76.4426071478373,76.5139555065764,76.5853761615433,76.6558184437214,76.7319219397426,
76.8079750858132,76.8839882760484,76.9599718759296,77.0359362292584,77.1130386418931,
77.1890103699317,77.2649946971906,77.3410010388627,77.4189396617312,77.4950487011589,
77.5739021157477,77.6527555303365,77.7288884025816,77.8049281036525,77.8808841090234,
77.9567425515606,78.0325436151146,78.108282935849,78.151224073644,78.2243297162825,
78.2974563861152,78.3706483030038,78.4438786071505,78.517191606161,78.5398163397455),
 .UNSPECIFIED.);
#3189=B_SPLINE_CURVE_WITH_KNOTS('',3,(#164002,#164003,#164004,#164005,#164006,
#164007,#164008,#164009,#164010,#164011,#164012,#164013,#164014,#164015,
#164016),.UNSPECIFIED.,.F.,.F.,(4,1,1,1,1,1,1,1,1,1,1,1,4),(78.5398163397455,
78.6496926169516,79.6466297035667,80.1450982468743,80.6435667901818,81.1420353334894,
81.6405038767969,82.1389724201045,82.6374409634121,83.1359095067196,83.6343780500272,
84.6313151366423,84.8230016469251),.UNSPECIFIED.);
#3190=B_SPLINE_CURVE_WITH_KNOTS('',3,(#164018,#164019,#164020,#164021,#164022,
#164023,#164024,#164025,#164026,#164027,#164028,#164029,#164030,#164031,
#164032,#164033,#164034,#164035,#164036,#164037,#164038,#164039,#164040,
#164041,#164042,#164043,#164044,#164045,#164046,#164047,#164048,#164049,
#164050,#164051,#164052,#164053,#164054,#164055,#164056,#164057,#164058,
#164059,#164060,#164061,#164062,#164063,#164064,#164065,#164066,#164067,
#164068,#164069,#164070,#164071,#164072,#164073,#164074,#164075,#164076,
#164077,#164078,#164079,#164080,#164081,#164082,#164083,#164084,#164085,
#164086,#164087,#164088,#164089,#164090,#164091,#164092,#164093,#164094,
#164095,#164096,#164097,#164098,#164099,#164100,#164101,#164102,#164103,
#164104,#164105,#164106,#164107,#164108,#164109,#164110,#164111,#164112,
#164113,#164114,#164115,#164116,#164117,#164118,#164119,#164120,#164121,
#164122,#164123,#164124,#164125,#164126,#164127,#164128,#164129,#164130,
#164131,#164132,#164133,#164134,#164135,#164136,#164137,#164138,#164139,
#164140,#164141,#164142,#164143,#164144,#164145,#164146,#164147,#164148,
#164149,#164150,#164151,#164152,#164153,#164154,#164155,#164156,#164157,
#164158,#164159,#164160,#164161,#164162,#164163,#164164,#164165,#164166,
#164167,#164168,#164169,#164170,#164171,#164172,#164173,#164174,#164175,
#164176,#164177,#164178,#164179,#164180,#164181,#164182,#164183,#164184,
#164185,#164186,#164187,#164188,#164189,#164190,#164191,#164192,#164193,
#164194,#164195,#164196,#164197,#164198,#164199,#164200,#164201,#164202,
#164203,#164204,#164205,#164206,#164207,#164208,#164209,#164210,#164211,
#164212,#164213,#164214,#164215,#164216,#164217,#164218,#164219,#164220,
#164221,#164222,#164223,#164224,#164225,#164226,#164227,#164228,#164229,
#164230,#164231,#164232,#164233,#164234,#164235,#164236,#164237,#164238,
#164239,#164240,#164241,#164242,#164243,#164244,#164245,#164246,#164247,
#164248,#164249,#164250,#164251,#164252,#164253,#164254,#164255,#164256,
#164257,#164258,#164259,#164260,#164261,#164262,#164263,#164264,#164265,
#164266,#164267,#164268,#164269,#164270,#164271,#164272,#164273),
 .UNSPECIFIED.,.F.,.F.,(4,3,3,3,3,3,3,3,3,3,3,3,3,3,3,3,3,3,3,3,3,3,3,3,
3,3,3,3,3,3,3,3,3,3,3,3,3,3,3,3,3,3,3,3,3,3,3,3,3,3,3,3,3,3,3,3,3,3,3,3,
3,3,3,3,3,3,3,3,3,3,3,3,3,3,3,3,3,3,3,3,3,3,3,3,3,4),(84.8230016469251,
84.8950329886772,84.9670035295852,85.0389391630576,85.1108531641058,85.1297836799499,
85.2055260447726,85.2813141655222,85.3571573363646,85.4331122946245,85.5091287269584,
85.5852645224588,85.6282522232574,85.7044628037309,85.780605407983,85.8566904943232,
85.9327284805954,86.0087297511505,86.0857871959908,86.1617524581157,86.2377140499803,
86.3136813770418,86.3915583602494,86.467588157682,86.5463887337772,86.6251893098725,
86.6966125847225,86.7679827116359,86.8393132831573,86.9106266206429,86.9819273074649,
87.0532527889575,87.1236578531801,87.2113633425206,87.2995397049393,87.3881441155568,
87.4768444224396,87.5654406823742,87.6221263964876,87.6950958409377,87.7680198320316,
87.8409113587729,87.9137935576939,87.9866684757374,88.0595714254476,88.1205949397952,
88.1998957237444,88.2792186542207,88.3585612562308,88.4379343334031,88.5173160144004,
88.5967127915087,88.6190634831028,88.6984608777717,88.7778445516,88.8572120032418,
88.936557187054,89.0158802063202,89.0951744359419,89.1175320264103,89.190434426679,
89.2633142837243,89.3361845531575,89.4090808975625,89.4819895533475,89.554957866296,
89.6160005697179,89.7045749013317,89.793275266806,89.8818420789087,89.9701854924737,
90.0579552090997,90.1144691130254,90.1857926113755,90.257096361531,90.3283938648039,
90.3997263604502,90.4710747191896,90.5424953741565,90.612937656333,90.6939127385888,
90.7748258176601,90.8576659473002,90.9383778712841,91.0222821037523,91.1061863362205),
 .UNSPECIFIED.);
#3191=B_SPLINE_CURVE_WITH_KNOTS('',3,(#164275,#164276,#164277,#164278,#164279,
#164280,#164281,#164282,#164283,#164284,#164285,#164286,#164287,#164288,
#164289,#164290,#164291,#164292,#164293,#164294,#164295,#164296,#164297,
#164298,#164299,#164300,#164301,#164302,#164303,#164304,#164305,#164306,
#164307,#164308,#164309,#164310,#164311,#164312,#164313,#164314,#164315,
#164316,#164317,#164318,#164319,#164320,#164321,#164322,#164323,#164324,
#164325,#164326,#164327,#164328,#164329,#164330,#164331,#164332,#164333,
#164334,#164335,#164336,#164337,#164338,#164339,#164340,#164341,#164342,
#164343,#164344,#164345,#164346,#164347,#164348,#164349,#164350,#164351,
#164352,#164353,#164354,#164355,#164356,#164357,#164358,#164359,#164360,
#164361,#164362,#164363,#164364,#164365,#164366,#164367,#164368,#164369,
#164370,#164371,#164372,#164373,#164374,#164375,#164376,#164377,#164378,
#164379,#164380,#164381,#164382,#164383,#164384,#164385,#164386,#164387,
#164388,#164389,#164390,#164391,#164392,#164393,#164394,#164395,#164396,
#164397,#164398,#164399,#164400,#164401,#164402,#164403,#164404,#164405,
#164406,#164407,#164408,#164409,#164410,#164411,#164412,#164413,#164414,
#164415,#164416,#164417,#164418,#164419,#164420,#164421,#164422,#164423,
#164424,#164425,#164426,#164427,#164428,#164429,#164430,#164431,#164432,
#164433,#164434,#164435,#164436,#164437,#164438,#164439,#164440,#164441,
#164442,#164443,#164444,#164445,#164446,#164447,#164448,#164449,#164450,
#164451,#164452,#164453,#164454,#164455,#164456,#164457,#164458,#164459,
#164460,#164461,#164462,#164463,#164464,#164465,#164466,#164467,#164468,
#164469,#164470,#164471,#164472,#164473,#164474,#164475,#164476,#164477,
#164478,#164479,#164480,#164481,#164482,#164483,#164484,#164485,#164486,
#164487,#164488,#164489,#164490,#164491,#164492,#164493,#164494,#164495,
#164496,#164497,#164498,#164499,#164500,#164501,#164502,#164503,#164504,
#164505,#164506,#164507,#164508,#164509,#164510,#164511,#164512,#164513,
#164514,#164515,#164516,#164517,#164518,#164519,#164520,#164521,#164522,
#164523,#164524,#164525,#164526,#164527,#164528,#164529,#164530,#164531,
#164532,#164533),.UNSPECIFIED.,.F.,.F.,(4,3,3,3,3,3,3,3,3,3,3,3,3,3,3,3,
3,3,3,3,3,3,3,3,3,3,3,3,3,3,3,3,3,3,3,3,3,3,3,3,3,3,3,3,3,3,3,3,3,3,3,3,
3,3,3,3,3,3,3,3,3,3,3,3,3,3,3,3,3,3,3,3,3,3,3,3,3,3,3,3,3,3,3,3,3,3,4),
(91.1061869541046,91.185072039433,91.2640500284989,91.3431199147297,91.4223307290269,
91.501614799976,91.5810109127831,91.6098747429481,91.6860076151932,91.7620473162646,
91.8380033216353,91.9138617641726,91.9896628277263,92.0654021484602,92.1083432862557,
92.1840856510784,92.2598737718279,92.3357169426699,92.4116719009298,92.487688333264,
92.5638241287644,92.6068118295632,92.6830224100368,92.7591650142889,92.8352501006293,
92.9112880869015,92.9872893574565,93.0643468022967,93.1403120644216,93.2162736562862,
93.2922409833475,93.3701179665552,93.4461477639878,93.5249483400831,93.6037489161783,
93.6751721910282,93.7465423179415,93.8178728894628,93.8891862269484,93.9604869137707,
94.0318123952632,94.1022174594859,94.1899229488263,94.2780993112448,94.3667037218623,
94.455404028745,94.5440002886799,94.6006860027935,94.6736554472436,94.7465794383374,
94.8194709650783,94.8923531639992,94.9652280820427,95.0381310317529,95.099154546101,
95.1784553300503,95.2577782605266,95.3371208625367,95.416493939709,95.495875620706,
95.5752723978145,95.5976230894086,95.6770204840775,95.7564041579055,95.8357716095462,
95.9151167933585,95.9944398126247,96.0737340422464,96.0960916327161,96.1689940329847,
96.24187389003,96.3147441594632,96.3876405038683,96.4605491596532,96.5335174726015,
96.5945601760237,96.6831345076366,96.7718348731101,96.8604016852129,96.9487450987768,
97.0365148154024,97.0930287193312,97.1614881029375,97.229931937027,97.2983663514909,
97.3668185260313,97.3893722612842),.UNSPECIFIED.);
#3192=B_SPLINE_CURVE_WITH_KNOTS('',3,(#164535,#164536,#164537,#164538,#164539,
#164540,#164541,#164542,#164543,#164544,#164545,#164546,#164547,#164548,
#164549,#164550,#164551,#164552,#164553,#164554,#164555,#164556,#164557,
#164558,#164559,#164560,#164561,#164562,#164563,#164564,#164565,#164566,
#164567,#164568,#164569,#164570,#164571,#164572,#164573,#164574,#164575,
#164576,#164577,#164578,#164579,#164580,#164581,#164582,#164583,#164584,
#164585,#164586,#164587,#164588,#164589,#164590,#164591,#164592,#164593,
#164594,#164595,#164596,#164597,#164598,#164599,#164600,#164601,#164602,
#164603,#164604,#164605,#164606,#164607,#164608,#164609,#164610,#164611,
#164612,#164613,#164614,#164615,#164616,#164617,#164618,#164619,#164620,
#164621,#164622,#164623,#164624,#164625,#164626,#164627,#164628,#164629,
#164630,#164631,#164632,#164633,#164634,#164635,#164636,#164637,#164638,
#164639,#164640,#164641,#164642,#164643,#164644,#164645,#164646,#164647,
#164648,#164649,#164650,#164651,#164652,#164653,#164654,#164655,#164656,
#164657,#164658,#164659,#164660,#164661,#164662,#164663,#164664,#164665,
#164666,#164667,#164668,#164669,#164670,#164671,#164672,#164673,#164674,
#164675,#164676,#164677,#164678,#164679,#164680,#164681,#164682,#164683,
#164684,#164685,#164686,#164687,#164688,#164689,#164690,#164691,#164692,
#164693,#164694,#164695,#164696,#164697,#164698,#164699,#164700,#164701,
#164702,#164703,#164704,#164705,#164706,#164707,#164708,#164709,#164710,
#164711,#164712,#164713,#164714,#164715,#164716,#164717,#164718,#164719,
#164720,#164721,#164722,#164723,#164724,#164725,#164726,#164727,#164728,
#164729,#164730,#164731,#164732,#164733,#164734,#164735,#164736,#164737,
#164738,#164739,#164740,#164741,#164742,#164743,#164744,#164745,#164746,
#164747,#164748,#164749,#164750,#164751,#164752,#164753,#164754,#164755,
#164756,#164757,#164758,#164759,#164760,#164761,#164762,#164763,#164764,
#164765,#164766,#164767,#164768,#164769,#164770,#164771,#164772,#164773,
#164774,#164775,#164776,#164777,#164778,#164779,#164780,#164781,#164782,
#164783,#164784,#164785,#164786,#164787,#164788,#164789,#164790,#164791,
#164792,#164793,#164794,#164795,#164796,#164797,#164798,#164799,#164800,
#164801,#164802,#164803,#164804,#164805,#164806,#164807,#164808,#164809,
#164810,#164811,#164812,#164813,#164814,#164815,#164816,#164817,#164818,
#164819,#164820,#164821,#164822,#164823,#164824,#164825,#164826,#164827,
#164828,#164829,#164830,#164831,#164832,#164833,#164834,#164835,#164836,
#164837,#164838,#164839,#164840,#164841,#164842,#164843,#164844,#164845,
#164846,#164847,#164848,#164849,#164850,#164851,#164852,#164853,#164854,
#164855,#164856,#164857,#164858,#164859,#164860,#164861,#164862,#164863,
#164864,#164865,#164866,#164867,#164868,#164869,#164870,#164871,#164872,
#164873,#164874,#164875,#164876,#164877,#164878,#164879,#164880,#164881,
#164882,#164883,#164884,#164885,#164886,#164887,#164888,#164889,#164890,
#164891,#164892,#164893,#164894,#164895,#164896,#164897,#164898,#164899,
#164900,#164901,#164902,#164903,#164904,#164905,#164906,#164907,#164908,
#164909,#164910,#164911,#164912,#164913,#164914,#164915,#164916,#164917,
#164918,#164919,#164920,#164921,#164922,#164923,#164924,#164925,#164926,
#164927,#164928,#164929,#164930,#164931,#164932,#164933,#164934,#164935,
#164936,#164937,#164938,#164939,#164940,#164941,#164942,#164943,#164944,
#164945,#164946,#164947,#164948,#164949,#164950,#164951,#164952,#164953,
#164954,#164955,#164956,#164957,#164958,#164959,#164960,#164961,#164962,
#164963,#164964,#164965,#164966,#164967,#164968,#164969,#164970,#164971,
#164972,#164973,#164974,#164975,#164976,#164977,#164978,#164979,#164980,
#164981,#164982,#164983,#164984,#164985,#164986,#164987,#164988,#164989,
#164990,#164991,#164992,#164993,#164994,#164995,#164996,#164997,#164998,
#164999,#165000,#165001,#165002,#165003,#165004,#165005,#165006,#165007,
#165008,#165009,#165010,#165011,#165012,#165013,#165014,#165015,#165016,
#165017,#165018,#165019,#165020,#165021,#165022,#165023,#165024,#165025,
#165026,#165027,#165028,#165029,#165030,#165031,#165032,#165033,#165034,
#165035,#165036,#165037,#165038,#165039,#165040,#165041,#165042,#165043,
#165044,#165045,#165046,#165047,#165048,#165049,#165050,#165051,#165052,
#165053,#165054,#165055,#165056,#165057,#165058,#165059,#165060,#165061,
#165062,#165063,#165064,#165065,#165066,#165067,#165068,#165069,#165070,
#165071,#165072,#165073,#165074,#165075,#165076,#165077,#165078,#165079,
#165080,#165081,#165082,#165083,#165084,#165085,#165086,#165087,#165088,
#165089,#165090,#165091,#165092,#165093,#165094,#165095,#165096,#165097,
#165098,#165099,#165100,#165101,#165102,#165103,#165104,#165105,#165106,
#165107,#165108,#165109,#165110,#165111,#165112,#165113,#165114,#165115,
#165116,#165117,#165118,#165119,#165120,#165121,#165122,#165123,#165124,
#165125,#165126,#165127,#165128,#165129,#165130,#165131,#165132,#165133,
#165134,#165135,#165136,#165137,#165138,#165139,#165140,#165141,#165142,
#165143,#165144,#165145,#165146,#165147,#165148,#165149,#165150,#165151,
#165152,#165153,#165154,#165155,#165156,#165157,#165158,#165159,#165160,
#165161,#165162,#165163,#165164,#165165,#165166,#165167,#165168,#165169,
#165170,#165171,#165172,#165173,#165174,#165175,#165176,#165177,#165178,
#165179,#165180,#165181,#165182,#165183,#165184,#165185,#165186,#165187,
#165188,#165189,#165190,#165191,#165192,#165193,#165194,#165195,#165196,
#165197,#165198,#165199,#165200,#165201,#165202,#165203,#165204,#165205,
#165206,#165207,#165208,#165209,#165210,#165211,#165212,#165213,#165214,
#165215,#165216,#165217,#165218,#165219,#165220,#165221,#165222,#165223,
#165224,#165225,#165226,#165227,#165228,#165229,#165230,#165231,#165232,
#165233,#165234,#165235,#165236,#165237,#165238,#165239,#165240,#165241,
#165242,#165243,#165244,#165245,#165246,#165247,#165248,#165249,#165250,
#165251,#165252,#165253,#165254,#165255,#165256,#165257,#165258),
 .UNSPECIFIED.,.F.,.F.,(4,2,2,2,2,2,2,2,2,2,2,2,2,2,2,2,2,2,2,2,2,2,2,2,
2,2,2,2,2,2,2,2,2,2,2,2,2,2,2,2,2,2,2,2,2,2,2,2,2,2,2,2,2,2,2,2,2,2,2,2,
2,2,2,2,2,2,2,2,2,2,2,2,2,2,2,2,2,2,2,2,2,2,2,2,2,2,2,2,2,2,2,2,2,2,2,2,
2,2,2,2,2,2,2,2,2,2,2,2,2,2,2,2,2,2,2,2,2,2,2,2,2,2,2,2,2,2,2,2,2,2,2,2,
2,2,2,2,2,2,2,2,2,2,2,2,2,2,2,2,2,2,2,2,2,2,2,2,2,2,2,2,2,2,2,2,2,2,2,2,
2,2,2,2,2,2,2,2,2,2,2,2,2,2,2,2,2,2,2,2,2,2,2,2,2,2,2,2,2,2,2,2,2,2,2,2,
2,2,2,2,2,2,2,2,2,2,2,2,2,2,2,2,2,2,2,2,2,2,2,2,2,2,2,2,2,2,2,2,2,2,2,2,
2,2,2,2,2,2,2,2,2,2,2,2,2,2,2,2,2,2,2,2,2,2,2,2,2,2,2,2,2,2,2,2,2,2,2,2,
2,2,2,2,2,2,2,2,2,2,2,2,2,2,2,2,2,2,2,2,2,2,2,2,2,2,2,2,2,2,2,2,2,2,2,2,
2,2,2,2,2,2,2,2,2,2,2,2,2,2,2,2,2,2,2,2,2,2,2,2,2,2,2,2,2,2,2,2,2,2,2,2,
2,2,2,2,2,2,2,2,2,2,2,2,2,4),(0.00175068145111175,0.134011030493767,0.138634978208069,
0.141510891536465,0.143675177905201,0.145865861977993,0.147898128219227,
0.150670147329979,0.156128791954469,0.218904577978021,0.253373337729684,
0.271399628962356,0.297726024991574,0.334632242767568,0.409083717063428,
0.520385324309226,0.566345440885185,0.573275583049934,0.576845253459886,
0.579699806871459,0.58255545909305,0.587669036857107,0.603126833170253,
0.870804313282468,0.927422269494703,0.970581617958302,0.984891875418743,
0.994813470394621,0.998399463628681,1.00049902275691,1.00276556583873,1.00569105443112,
1.01177742507548,1.05391356569697,1.18009633810029,1.28059991335028,1.33131231686721,
1.36347352356323,1.37424075320674,1.38127739511405,1.38786128432668,1.39614134393183,
1.4090925899202,1.47859786697299,1.49115523764654,1.55871838182118,1.6400507016171,
1.74326408493459,1.75266721674397,1.75746543472939,1.76146386785603,1.76392991606873,
1.76618948797032,1.76905778140773,1.77485609804717,1.8161320534101,1.82162002368309,
2.04722862911486,2.1596758369333,2.17763716594957,2.18283861950859,2.18603146184098,
2.18892818775009,2.19264720187391,2.19859053660356,2.22922431720825,2.44839371798544,
2.60656799284768,2.61498176304512,2.61823132686803,2.62047799114371,2.62268579227223,
2.62535664959904,2.63207631729564,2.73650099359328,2.91260834049862,3.03413896399209,
3.06308463758117,3.07720865049273,3.08848150615735,3.10134686954032,3.12321606461796,
3.23928404073321,3.36047347272984,3.38606706105148,3.40365638652497,3.41093121471606,
3.41647669150467,3.42301926965352,3.43471750094256,3.50662769021987,3.58033457861406,
3.5974510175504,3.60861788776679,3.61933499877933,3.63222294110174,3.66402302370758,
3.71871540548264,3.77935003739452,3.79899838570045,3.81301678758811,3.81975196395409,
3.82569940995075,3.83341569211323,3.8461781803915,3.95715492100013,4.00589566204327,
4.05167656332163,4.07205957561714,4.08830035182536,4.10831338891101,4.15752195595253,
4.19208659720518,4.20272163769428,4.2186851683656,4.23070700122613,4.24812676325788,
4.304461625542,4.32279881912596,4.34879086999873,4.36569829043325,4.38118536310892,
4.408006893285,4.54680592976487,4.58521538376171,4.60130133424854,4.61380268457729,
4.62071771357805,4.62661544059658,4.63413770759333,4.651631668965,4.72859306163979,
4.7794707745708,4.81290323013672,4.82706741833238,4.83771048242841,4.84786367479352,
4.86553244870683,4.96137711464545,4.99648683212428,5.01746876894224,5.02553781623566,
5.03125923032708,5.03651959628616,5.04622401050655,5.07989689879688,5.1142738476073,
5.25314698952696,5.25623071551449,5.32536953398259,5.34544566715934,5.35780433808763,
5.3691832859131,5.38423334506416,5.41851704874251,5.60387741343003,5.73060722271663,
5.81277345713204,5.81945616133057,5.82212094555868,5.82432708718931,5.82657546245093,
5.82983364060598,5.83830374223236,5.87559417485033,5.91338366008016,6.0012139475115,
6.08349114031398,6.240631152834,6.2504149007525,6.25421925360012,6.25696445981735,
6.25988255228077,6.26375238830769,6.27219685741442,6.42713990792728,6.6605772612252,
6.67282472533302,6.67684477474014,6.67908078752245,6.68133302228001,6.68412526920551,
6.68955304243106,6.72623012148463,6.82397060594503,6.89647081849563,7.03199979411896,
7.0482913028952,7.05661375056243,7.06320297248004,7.07022130004281,7.08090257149064,
7.11293058485085,7.35812291436516,7.43204235528481,7.43890392114801,7.44167055307541,
7.44397312791639,7.44633210338918,7.44977302276103,7.45884511930544,7.50066991308049,
7.52835637967532,7.672750589987,7.84764417394031,7.85846618543644,7.86243744503269,
7.86522796872251,7.86783721604346,7.871423425317,7.87843012943556,7.92648394749109,
7.98435140079447,8.17240102025664,8.28706847158256,8.2942807017657,8.29710619189759,
8.29915282949482,8.30133570215935,8.30424206064701,8.31050513071682,8.36196508622292,
8.42013957513948,8.51054999994118,8.61358515036602,8.71226959267471,8.74173865690321,
8.75595991399811,8.76724262799249,8.77777254733366,8.79268411751894,8.83872658224809,
8.91210064491931,8.98107778509443,9.03942084606236,9.07690281967958,9.086896578827,
9.09220420910962,9.09722913784367,9.09724523595471,9.09726129654262,9.09727732001483,
9.09729330669885,9.09730925702172,9.09732517135649,9.09734105008431,9.09735689363703,
9.09737270235281,9.09738847657413,9.09740421675583,9.09741992323606,9.09743559638129,
9.09745123648668,9.09746684401147,9.09748241923962,9.09749796253769,9.09751347432227,
9.09752895492289,9.09754440468476,9.09755982394042,9.09757521304138,9.0975905722994,
9.09760590207696,9.0976212027568,9.09763647458273,9.09765171789646,9.09766693304972,
9.09768212034341,9.09769728004803,9.09771241261139,9.09772751835617,9.0977425975128,
9.09775765037659,9.09777267726359,9.09778767853363,9.09780265453569,9.09781760558654,
9.0978325319059,9.09784743384839,9.09786231166902,9.09787716567843,9.09789199612518,
9.0979068033323,9.0979215876016,9.09793634923074,9.09795108847808,9.09796580564063,
9.09798050103171,9.09799517490246,9.09800982753272,9.09802445926074,9.09803907028262,
9.09805366090144,9.09806823138489,9.09808278196589,9.0980973129296,9.09811182454834,
9.098126317194,9.09814079107453,9.09815524636716,9.09816968342256,9.10376770015621,
9.11170544754015,9.12531173155767,9.15686879604102,9.254550635845,9.27408438484564,
9.28574103015298,9.29592948071053,9.29603839081233,9.29614580743692,9.29625175834067,
9.29635627070302,9.29645937111086,9.29656108559078,9.29666143961484,9.29676045811431,
9.29685816547961,9.29695458558435,9.31092411781765,9.34412631179128,9.39483863365628,
9.47158465277903,9.48944448302903,9.49702740511677,9.50260413151457,9.50891371067642,
9.50895489382347,9.50899621336665,9.50903767187097,9.50907927213511,9.50912101701083,
9.50916290933531,9.50920495196572,9.50924714778553,9.50928949974651,9.50933201081573,
9.50937468394175,9.52063607473001,9.53505424093766,9.56737159552485,9.63207094206619,
9.67801527753326,9.71864187171298,9.74401598578509,9.75928174231616,9.77510754230476,
9.79264076242029,9.80201134648943,9.82507503155774,9.88661125776569,9.89686058377307,
9.90774692212002,9.91994448989332,9.93949531280475,9.99424684689922,10.0246091225099,
10.0403705671353,10.0557025297082,10.0717420470211,10.0934521740875,10.2275071693496),
 .UNSPECIFIED.);
#3193=B_SPLINE_CURVE_WITH_KNOTS('',3,(#165260,#165261,#165262,#165263,#165264,
#165265,#165266,#165267,#165268,#165269,#165270,#165271,#165272,#165273,
#165274,#165275,#165276,#165277,#165278,#165279,#165280,#165281,#165282,
#165283,#165284,#165285,#165286,#165287,#165288,#165289,#165290,#165291,
#165292,#165293,#165294,#165295,#165296,#165297,#165298,#165299,#165300,
#165301,#165302,#165303,#165304,#165305,#165306,#165307,#165308,#165309,
#165310,#165311,#165312,#165313,#165314,#165315,#165316,#165317,#165318,
#165319,#165320,#165321,#165322,#165323,#165324,#165325,#165326,#165327,
#165328,#165329,#165330,#165331,#165332,#165333,#165334,#165335,#165336,
#165337,#165338,#165339,#165340,#165341,#165342,#165343,#165344,#165345,
#165346,#165347,#165348,#165349,#165350,#165351,#165352,#165353,#165354,
#165355,#165356,#165357,#165358,#165359,#165360,#165361,#165362,#165363,
#165364,#165365,#165366,#165367,#165368,#165369,#165370,#165371,#165372,
#165373,#165374,#165375,#165376,#165377,#165378,#165379,#165380,#165381,
#165382,#165383,#165384,#165385,#165386,#165387,#165388,#165389,#165390,
#165391,#165392,#165393,#165394,#165395,#165396,#165397,#165398,#165399,
#165400,#165401,#165402,#165403,#165404,#165405,#165406,#165407,#165408,
#165409,#165410,#165411,#165412,#165413,#165414,#165415,#165416,#165417,
#165418,#165419,#165420,#165421,#165422,#165423,#165424,#165425,#165426,
#165427,#165428,#165429,#165430,#165431,#165432,#165433,#165434,#165435,
#165436,#165437,#165438,#165439,#165440,#165441,#165442,#165443,#165444,
#165445,#165446,#165447,#165448,#165449,#165450,#165451,#165452,#165453,
#165454,#165455,#165456,#165457,#165458,#165459,#165460,#165461,#165462,
#165463,#165464,#165465,#165466,#165467,#165468,#165469,#165470,#165471,
#165472,#165473,#165474,#165475,#165476,#165477,#165478,#165479,#165480,
#165481,#165482,#165483,#165484,#165485,#165486,#165487,#165488,#165489,
#165490,#165491,#165492,#165493,#165494,#165495,#165496,#165497,#165498,
#165499,#165500,#165501,#165502,#165503,#165504,#165505,#165506,#165507,
#165508,#165509,#165510,#165511,#165512,#165513,#165514,#165515,#165516,
#165517,#165518,#165519,#165520,#165521,#165522,#165523,#165524,#165525,
#165526,#165527,#165528,#165529,#165530,#165531,#165532,#165533,#165534,
#165535,#165536,#165537,#165538,#165539,#165540,#165541,#165542,#165543,
#165544,#165545,#165546,#165547,#165548,#165549,#165550,#165551,#165552,
#165553,#165554,#165555,#165556,#165557,#165558,#165559,#165560,#165561,
#165562,#165563,#165564,#165565,#165566,#165567,#165568,#165569,#165570,
#165571,#165572,#165573,#165574,#165575,#165576,#165577,#165578,#165579,
#165580,#165581,#165582,#165583,#165584,#165585,#165586,#165587,#165588,
#165589,#165590,#165591,#165592,#165593,#165594,#165595,#165596,#165597,
#165598,#165599,#165600,#165601,#165602,#165603,#165604,#165605,#165606,
#165607,#165608,#165609,#165610,#165611,#165612,#165613,#165614,#165615,
#165616,#165617,#165618,#165619,#165620,#165621,#165622,#165623,#165624,
#165625,#165626,#165627,#165628,#165629,#165630,#165631,#165632,#165633,
#165634,#165635,#165636,#165637,#165638,#165639,#165640,#165641,#165642,
#165643,#165644,#165645,#165646,#165647,#165648,#165649,#165650,#165651,
#165652,#165653,#165654,#165655,#165656,#165657,#165658,#165659,#165660,
#165661,#165662,#165663,#165664,#165665,#165666,#165667,#165668,#165669,
#165670,#165671,#165672,#165673,#165674,#165675,#165676,#165677,#165678,
#165679,#165680,#165681,#165682,#165683,#165684,#165685,#165686,#165687,
#165688,#165689,#165690,#165691,#165692,#165693,#165694,#165695,#165696,
#165697,#165698,#165699,#165700,#165701,#165702,#165703,#165704,#165705,
#165706,#165707,#165708,#165709,#165710,#165711,#165712,#165713,#165714,
#165715,#165716,#165717,#165718,#165719,#165720,#165721,#165722,#165723,
#165724,#165725,#165726,#165727,#165728,#165729,#165730,#165731,#165732,
#165733,#165734,#165735,#165736,#165737,#165738,#165739,#165740,#165741,
#165742,#165743,#165744,#165745,#165746,#165747,#165748,#165749,#165750,
#165751,#165752,#165753,#165754,#165755,#165756,#165757,#165758,#165759,
#165760,#165761,#165762,#165763,#165764,#165765,#165766,#165767,#165768,
#165769,#165770,#165771,#165772,#165773,#165774,#165775,#165776,#165777,
#165778,#165779,#165780,#165781,#165782,#165783,#165784,#165785,#165786,
#165787,#165788,#165789,#165790,#165791,#165792,#165793,#165794,#165795,
#165796,#165797,#165798,#165799,#165800,#165801),.UNSPECIFIED.,.F.,.F.,
(4,2,2,2,2,2,2,2,2,2,2,2,2,2,2,2,2,2,2,2,2,2,2,2,2,2,2,2,2,2,2,2,2,2,2,
2,2,2,2,2,2,2,2,2,2,2,2,2,2,2,2,2,2,2,2,2,2,2,2,2,2,2,2,2,2,2,2,2,2,2,2,
2,2,2,2,2,2,2,2,2,2,2,2,2,2,2,2,2,2,2,2,2,2,2,2,2,2,2,2,2,2,2,2,2,2,2,2,
2,2,2,2,2,2,2,2,2,2,2,2,2,2,2,2,2,2,2,2,2,2,2,2,2,2,2,2,2,2,2,2,2,2,2,2,
2,2,2,2,2,2,2,2,2,2,2,2,2,2,2,2,2,2,2,2,2,2,2,2,2,2,2,2,2,2,2,2,2,2,2,2,
2,2,2,2,2,2,2,2,2,2,2,2,2,2,2,2,2,2,2,2,2,2,2,2,2,2,2,2,2,2,2,2,2,2,2,2,
2,2,2,2,2,2,2,2,2,2,2,2,2,2,2,2,2,2,2,2,2,2,2,2,2,2,2,2,2,2,2,2,2,2,2,2,
2,2,2,2,2,2,2,2,2,2,2,2,2,2,2,2,2,2,2,4),(0.00186199683268441,0.0535642282285645,
0.0630877328723694,0.0696351131693898,0.0752500213517179,0.0811989772806776,
0.088362912300289,0.10908685004617,0.119623293193971,0.201548095287269,
0.244189440712299,0.269675950580021,0.280137626972409,0.290169430701876,
0.300137816356626,0.31678381431195,0.369057831022039,0.37083408155873,0.431445777403261,
0.455973952503189,0.467595688565333,0.476972384577673,0.482457599612003,
0.487927247505554,0.494527592164464,0.510720097351574,0.617630405419689,
0.65911088494058,0.767015788711514,0.792505078442363,0.803780297652384,
0.81526496408748,0.825913352571771,0.840603391281476,0.880582300677057,
1.00281431820652,1.161471926301,1.23740230070852,1.25803714022971,1.26641154476457,
1.27265338125613,1.27554861976409,1.27772911668787,1.27977789660999,1.28261325563633,
1.28988797049119,1.41277504561787,1.52102929598508,1.69581005597633,1.70433583150545,
1.70822053462579,1.71114060620604,1.71388095931465,1.71766796647744,1.72734995544263,
1.87813929223131,1.95513954672685,2.11856549384494,2.12424496224557,2.12876929239171,
2.13146616057173,2.1334936688928,2.13605295738736,2.14040659402505,2.1554872883031,
2.15745647869779,2.17614527331743,2.21387900683578,2.32340512223105,2.46810413041667,
2.48678589322234,2.50179402274962,2.50962019097846,2.51618420073926,2.52242896408552,
2.53275891623459,2.55971100605392,2.74839199957644,2.8730923394382,2.88868062295377,
2.89289618240161,2.89542468657957,2.89768135341565,2.90052826897125,2.90603885331675,
2.94067875320462,3.14960715613848,3.30358274056309,3.31202051377418,3.31588838086973,
3.31880544491032,3.32155002035642,3.32535403434762,3.33513980875609,3.49314022624314,
3.57604723511976,3.67666450751218,3.69982988544085,3.72793708234981,3.744115649835,
3.74825858110122,3.75070109352932,3.75285471351248,3.75553693169349,3.75967247259297,
3.77851407675741,4.00151591376745,4.09062969189725,4.17487210723701,4.19787459767563,
4.21083142662629,4.22209059252564,4.23607106785952,4.26312676595551,4.45153254464311,
4.50264690832833,4.52196238343777,4.53617166594015,4.54285600582181,4.5484163993348,
4.55540384444795,4.56655767443692,4.6321874210292,4.68495437240109,4.71824348253228,
4.73232118112925,4.74294826238949,4.75456667003629,4.77388306384699,4.87683237556472,
4.93132912088735,4.94439015254172,4.95096941616951,4.95694800077712,4.96476356588773,
4.97817805183452,5.04853713350459,5.11382318120744,5.1757174525467,5.19637450479622,
5.21155273698212,5.22881143792393,5.25754612351168,5.30027725845294,5.33874981194839,
5.35242214148458,5.36540416933083,5.39841500532554,5.47211467157039,5.49055122316089,
5.507139283974,5.52991417199247,5.59700422966766,5.65839282004497,5.72751564801281,
5.74244898033661,5.749950073129,5.7558709698339,5.76277644098215,5.77787389000309,
5.79963225545946,5.87487674202028,5.93619073628499,5.95347487049008,5.96355822923337,
5.97422741436862,5.98860245227584,6.0240060522236,6.09301632905145,6.14320146832196,
6.1534827616281,6.1590500169829,6.16405738516219,6.17124025073293,6.18828403224541,
6.21282485305556,6.3326432396067,6.45153966852532,6.4735396407168,6.48643156207287,
6.49769724050674,6.51177200729218,6.54046636723328,6.66008290580623,6.82994401051037,
6.92489536519698,6.94587361642104,6.95016677254978,6.95289750564723,6.95505564666766,
6.95746704872175,6.96147148843887,6.97609737426708,7.08992812678715,7.23761359847736,
7.37090196039549,7.38047786746523,7.38424648066357,7.38698156305497,7.38990353148128,
7.39380358869357,7.40241497286651,7.52229387398696,7.72419730999893,7.79829781366815,
7.80476052531121,7.8077254300926,7.81000408578516,7.81244719036203,7.81495136837684,
7.82229806306039,7.83263610775129,7.95753542443239,8.14578033661352,8.17281096784043,
8.18314786432988,8.18939302260039,8.19595516725053,8.2033268272341,8.21723703484199,
8.23453167456104,8.35927511476581,8.52759722226799,8.55247731645695,8.56565555726439,
8.56978660265598,8.57204571919405,8.57429402342049,8.57704422684477,8.58163166081751,
8.60599943034831,8.65445800415061,8.75341181582875,8.82966261761597,8.97796569438977,
8.98762867651646,8.99141172282758,8.99415041113987,8.99706982851656,9.00095557332558,
9.00949131344891,9.18872204606232,9.28193523226186,9.41272295691981,9.42190792789857,
9.42538573198735,9.42744977026146,9.42940392715672,9.43212876400306,9.43507507126447,
9.44681506989839,9.47586682520955,9.56539509660465,9.66959759990051,9.67324628813472,
9.69476972276663,9.83257384078495,9.86658710463717,9.88047385728483,9.89196937718491,
9.90248245502818,9.91403223559125,9.92986860774804,10.0393653359466,10.0773539343858,
10.1300511129673,10.2018099159825,10.2132832248525,10.2192571617898,10.2224066646963,
10.2237944604769),.UNSPECIFIED.);
#3194=B_SPLINE_CURVE_WITH_KNOTS('',3,(#165803,#165804,#165805,#165806,#165807,
#165808,#165809,#165810,#165811,#165812,#165813,#165814,#165815,#165816,
#165817,#165818,#165819,#165820,#165821,#165822,#165823,#165824,#165825,
#165826,#165827,#165828,#165829,#165830,#165831,#165832,#165833,#165834,
#165835,#165836,#165837,#165838,#165839,#165840,#165841,#165842,#165843,
#165844,#165845,#165846,#165847,#165848,#165849,#165850,#165851,#165852,
#165853,#165854,#165855,#165856,#165857,#165858,#165859,#165860,#165861,
#165862,#165863,#165864,#165865,#165866,#165867,#165868,#165869,#165870,
#165871,#165872,#165873,#165874,#165875,#165876,#165877,#165878,#165879,
#165880,#165881,#165882,#165883,#165884,#165885,#165886,#165887,#165888,
#165889,#165890,#165891,#165892,#165893,#165894,#165895,#165896,#165897,
#165898,#165899,#165900,#165901,#165902,#165903,#165904,#165905,#165906,
#165907,#165908,#165909,#165910,#165911,#165912,#165913,#165914,#165915,
#165916,#165917,#165918,#165919,#165920,#165921,#165922,#165923,#165924,
#165925,#165926,#165927,#165928,#165929,#165930,#165931,#165932,#165933,
#165934,#165935,#165936,#165937,#165938,#165939,#165940,#165941,#165942,
#165943,#165944,#165945,#165946,#165947,#165948,#165949,#165950,#165951,
#165952,#165953,#165954,#165955,#165956,#165957,#165958,#165959,#165960,
#165961,#165962,#165963,#165964,#165965,#165966,#165967,#165968,#165969,
#165970,#165971,#165972,#165973,#165974,#165975,#165976,#165977,#165978,
#165979,#165980,#165981,#165982,#165983,#165984,#165985,#165986,#165987,
#165988,#165989,#165990,#165991,#165992,#165993,#165994,#165995,#165996,
#165997,#165998,#165999,#166000,#166001,#166002,#166003,#166004,#166005,
#166006,#166007,#166008,#166009,#166010,#166011,#166012,#166013,#166014,
#166015,#166016,#166017,#166018,#166019,#166020,#166021,#166022,#166023,
#166024,#166025,#166026,#166027,#166028,#166029,#166030,#166031,#166032,
#166033,#166034,#166035,#166036,#166037,#166038,#166039,#166040,#166041,
#166042,#166043,#166044,#166045,#166046,#166047,#166048,#166049,#166050,
#166051,#166052,#166053,#166054,#166055,#166056,#166057,#166058,#166059,
#166060,#166061,#166062,#166063,#166064,#166065,#166066,#166067,#166068,
#166069,#166070,#166071,#166072,#166073,#166074,#166075,#166076,#166077,
#166078,#166079,#166080,#166081,#166082,#166083,#166084,#166085,#166086,
#166087,#166088,#166089,#166090,#166091,#166092,#166093,#166094,#166095,
#166096,#166097,#166098,#166099,#166100,#166101,#166102,#166103,#166104,
#166105,#166106,#166107,#166108,#166109,#166110,#166111,#166112,#166113,
#166114,#166115,#166116,#166117,#166118,#166119,#166120,#166121,#166122,
#166123,#166124,#166125,#166126,#166127,#166128,#166129,#166130,#166131,
#166132,#166133,#166134,#166135,#166136,#166137,#166138,#166139,#166140,
#166141,#166142,#166143,#166144,#166145,#166146,#166147,#166148,#166149,
#166150,#166151,#166152,#166153,#166154,#166155,#166156,#166157,#166158,
#166159,#166160,#166161,#166162,#166163,#166164,#166165,#166166,#166167,
#166168,#166169,#166170,#166171,#166172,#166173,#166174,#166175,#166176,
#166177,#166178,#166179,#166180,#166181,#166182,#166183,#166184,#166185,
#166186,#166187,#166188,#166189,#166190,#166191,#166192,#166193,#166194,
#166195,#166196,#166197,#166198,#166199,#166200,#166201,#166202,#166203,
#166204,#166205,#166206,#166207,#166208,#166209,#166210,#166211,#166212,
#166213,#166214,#166215,#166216,#166217,#166218,#166219,#166220,#166221,
#166222,#166223,#166224,#166225,#166226,#166227,#166228,#166229,#166230,
#166231,#166232,#166233,#166234,#166235,#166236,#166237,#166238,#166239,
#166240,#166241,#166242,#166243,#166244,#166245,#166246,#166247,#166248,
#166249,#166250,#166251,#166252,#166253,#166254,#166255,#166256,#166257,
#166258,#166259,#166260,#166261,#166262,#166263,#166264,#166265,#166266,
#166267,#166268,#166269,#166270,#166271,#166272,#166273,#166274,#166275,
#166276,#166277,#166278,#166279,#166280,#166281,#166282,#166283,#166284,
#166285,#166286,#166287,#166288,#166289,#166290,#166291,#166292,#166293,
#166294,#166295,#166296,#166297,#166298,#166299,#166300,#166301,#166302,
#166303,#166304,#166305,#166306,#166307,#166308,#166309,#166310,#166311,
#166312,#166313,#166314,#166315,#166316,#166317,#166318,#166319,#166320,
#166321,#166322,#166323,#166324,#166325,#166326,#166327,#166328,#166329,
#166330,#166331,#166332,#166333,#166334,#166335,#166336,#166337,#166338,
#166339,#166340,#166341,#166342,#166343,#166344,#166345,#166346,#166347,
#166348,#166349,#166350,#166351,#166352,#166353,#166354,#166355,#166356,
#166357,#166358,#166359,#166360,#166361,#166362,#166363,#166364,#166365,
#166366,#166367,#166368,#166369,#166370,#166371,#166372,#166373,#166374,
#166375,#166376,#166377,#166378,#166379,#166380,#166381,#166382,#166383,
#166384,#166385,#166386,#166387,#166388,#166389,#166390,#166391,#166392,
#166393,#166394),.UNSPECIFIED.,.F.,.F.,(4,2,2,2,2,2,2,2,2,2,2,2,2,2,2,2,
2,2,2,2,2,2,2,2,2,2,2,2,2,2,2,2,2,2,2,2,2,2,2,2,2,2,2,2,2,2,2,2,2,2,2,2,
2,2,2,2,2,2,2,2,2,2,2,2,2,2,2,2,2,2,2,2,2,2,2,2,2,2,2,2,2,2,2,2,2,2,2,2,
2,2,2,2,2,2,2,2,2,2,2,2,2,2,2,2,2,2,2,2,2,2,2,2,2,2,2,2,2,2,2,2,2,2,2,2,
2,2,2,2,2,2,2,2,2,2,2,2,2,2,2,2,2,2,2,2,2,2,2,2,2,2,2,2,2,2,2,2,2,2,2,2,
2,2,2,2,2,2,2,2,2,2,2,2,2,2,2,2,2,2,2,2,2,2,2,2,2,2,2,2,2,2,2,2,2,2,2,2,
2,2,2,2,2,2,2,2,2,2,2,2,2,2,2,2,2,2,2,2,2,2,2,2,2,2,2,2,2,2,2,2,2,2,2,2,
2,2,2,2,2,2,2,2,2,2,2,2,2,2,2,2,2,2,2,2,2,2,2,2,2,2,2,2,2,2,2,2,2,2,2,2,
2,2,2,2,2,2,2,2,2,2,2,2,2,2,2,2,2,2,2,2,2,2,2,2,2,2,2,4),(0.00188190208457017,
0.00399627713341498,0.00873346078420522,0.0196781469812297,0.0856369599480584,
0.161869882608815,0.175737014961344,0.186182018023973,0.196303179196513,
0.206344975829605,0.223395483122565,0.280569084600253,0.341429096207342,
0.374922414610643,0.388925204464006,0.396843424988868,0.402465300888644,
0.40817524846264,0.414838693706063,0.42616349746827,0.474906685334838,0.576981540011668,
0.627361376000328,0.630159019113763,0.631722892788452,0.632567972685891,
0.633016321902011,0.634982791062869,0.636534990113496,0.637744550736026,
0.638677280703863,0.639390520969028,0.639932318775882,0.640341765382074,
0.640649963956381,0.641574755610088,0.656940208644136,0.673167247567888,
0.693227522909643,0.738030196848381,0.775390350516043,0.798232859895037,
0.80954310109032,0.821989926849744,0.827826911121362,0.858601163433563,
0.918035570875503,0.935076074699258,0.951101962048288,0.968945151418558,
0.999212564962949,1.14454667873245,1.17469868185873,1.18848310579882,1.19670465538289,
1.20276285105365,1.20844387698576,1.21396960848659,1.22424468494723,1.28766561062729,
1.34152699585792,1.37574915565574,1.40104465114948,1.41148520739628,1.42153158100933,
1.43152337018159,1.44830202563702,1.50589792573087,1.57219325631432,1.59129402420728,
1.60512352989554,1.6107715416142,1.61616820931015,1.62216505797161,1.63264728587892,
1.68087548643409,1.78837934048518,1.86671182185378,1.89944189697937,1.92464929704944,
1.93577431579996,1.9471793023478,1.95796026479062,1.97625411815051,2.0301224455804,
2.24383548879379,2.36171191159315,2.39754176563455,2.40389933322904,2.40684862651801,
2.40903795723456,2.41107214203255,2.41385167968018,2.4193397805965,2.48385531213702,
2.51635324883219,2.70798411436433,2.8270133535038,2.83567077444962,2.83957986274691,
2.84250378776175,2.84523725015434,2.84899822616757,2.85852621101432,2.99096102885002,
3.14520869896789,3.19736879721844,3.24271933681024,3.25679728248856,3.26086488725105,
3.26336042126369,3.26562394671381,3.26852964835857,3.27318066824222,3.29796765457727,
3.33579943223096,3.4113810060932,3.54794764449462,3.62043879645794,3.63425973820241,
3.64195743614027,3.64848779316595,3.65587102728352,3.66823900904374,3.71147090873089,
3.76230070591415,3.92459900760316,3.98989280945017,4.01837214484894,4.0234600944039,
4.02618030125787,4.02820895394901,4.03042741944535,4.03436168120946,4.04597543793212,
4.04691811385669,4.29182271975965,4.39365336085305,4.43747543095095,4.4443233437924,
4.44787568433054,4.45047984560055,4.45368350128684,4.45893505367947,4.47544724711454,
4.7874602434939,4.86468783702226,4.87708779838307,4.88086238931171,4.8832230103228,
4.88539441458556,4.88817814711441,4.89408376138162,4.936766886737,5.114669525566,
5.28650197513703,5.32213065495992,5.3362819177911,5.34784898100086,5.35962994739869,
5.37693645312297,5.426208416691,5.54801068839648,5.59446180885821,5.60142787624911,
5.65902934921753,5.67031119029756,5.67644769639869,5.68211753646609,5.68989507527497,
5.708860805591,5.72499754754483,5.80228082916276,5.81388619575106,5.84916595000714,
5.86238407825231,5.8731785196803,5.88424187843515,5.90080664840088,5.95571664728315,
6.03507302572295,6.07003480130233,6.07948728764132,6.08491457861945,6.09110945593149,
6.10023215772556,6.12608762339023,6.15027767645197,6.28751983695318,6.32130515314122,
6.33977899967134,6.35466082524932,6.37649860877436,6.40297669314087,6.47177880842746,
6.48533865175689,6.49842213323086,6.53292344288207,6.6044893659996,6.62304051502869,
6.63960728147354,6.66216839586275,6.72677357419958,6.79092377531655,6.86064898836049,
6.87415034180332,6.8819914004204,6.88797582782014,6.89454414028451,6.9075268602895,
6.91709340421134,6.9342523150848,7.01800187584957,7.07035517995359,7.0870663139455,
7.09704934855207,7.10778414978548,7.12256113904019,7.16103441391893,7.19703950833263,
7.27199204172726,7.28345682786914,7.29053475450935,7.29610567296989,7.30270846818865,
7.31646627749367,7.32659124670002,7.35893639309173,7.48872860506365,7.51790696745331,
7.58852944976054,7.60873548413547,7.62112236694546,7.63249337448912,7.64748264309209,
7.68139131372957,7.85957857108816,7.98353725714297,8.07611339840757,8.08276340023158,
8.08546781040463,8.08748367171114,8.08968923712917,8.09272812182832,8.09985593466942,
8.20111400639101,8.24558059665294,8.47132399001199,8.50873758336276,8.51508830173201,
8.51888909708128,8.52180683926192,8.52486900330743,8.52960175168872,8.53511851340148,
8.54540669291271,8.63395034576474,8.87508719385648,8.93278321007588,8.93897836069356,
8.94189347840398,8.94416546258657,8.94663301765988,8.95057352872476,8.96348488003056,
9.0503347083963,9.19328516283191,9.29668033899776,9.3123037639036,9.32036894188253,
9.32695700208053,9.33398004758763,9.34468285234216,9.37688562016362,9.42524405614271,
9.45075560818347,9.57144882521517,9.69540937830716,9.70228079273981,9.70504896937153,
9.70735186806826,9.70971019284281,9.71314836479771,9.72220295897674,9.76389393225265,
10.0273273265981,10.0435888611411,10.1149195263784,10.1225790603345,10.1263770390947,
10.1291206067928,10.1318877839019,10.1347204895935,10.1383950572546,10.1441483691459,
10.2281508016451),.UNSPECIFIED.);
#3195=B_SPLINE_CURVE_WITH_KNOTS('',3,(#166396,#166397,#166398,#166399,#166400,
#166401,#166402,#166403,#166404,#166405,#166406,#166407,#166408,#166409,
#166410,#166411,#166412,#166413,#166414,#166415,#166416,#166417,#166418,
#166419,#166420,#166421,#166422,#166423,#166424,#166425,#166426,#166427,
#166428,#166429,#166430,#166431,#166432,#166433,#166434,#166435,#166436,
#166437,#166438,#166439,#166440,#166441,#166442,#166443,#166444,#166445,
#166446,#166447,#166448,#166449,#166450,#166451,#166452,#166453,#166454,
#166455,#166456,#166457,#166458,#166459,#166460,#166461,#166462,#166463,
#166464,#166465,#166466,#166467,#166468,#166469,#166470,#166471,#166472,
#166473,#166474,#166475,#166476,#166477,#166478,#166479,#166480,#166481,
#166482,#166483,#166484,#166485,#166486,#166487,#166488,#166489,#166490,
#166491,#166492,#166493,#166494,#166495,#166496,#166497,#166498,#166499,
#166500,#166501,#166502,#166503,#166504,#166505,#166506,#166507,#166508,
#166509,#166510,#166511,#166512,#166513,#166514,#166515,#166516,#166517,
#166518,#166519,#166520,#166521,#166522,#166523,#166524,#166525,#166526,
#166527,#166528,#166529,#166530,#166531,#166532,#166533,#166534,#166535,
#166536,#166537,#166538,#166539,#166540,#166541,#166542,#166543,#166544,
#166545,#166546,#166547,#166548,#166549,#166550,#166551,#166552,#166553,
#166554,#166555,#166556,#166557,#166558,#166559,#166560,#166561,#166562,
#166563,#166564,#166565,#166566,#166567,#166568,#166569,#166570,#166571,
#166572,#166573,#166574,#166575,#166576,#166577,#166578,#166579,#166580,
#166581,#166582,#166583,#166584,#166585,#166586,#166587,#166588,#166589,
#166590,#166591,#166592,#166593,#166594,#166595,#166596,#166597,#166598,
#166599,#166600,#166601,#166602,#166603,#166604,#166605,#166606,#166607,
#166608,#166609,#166610,#166611,#166612,#166613,#166614,#166615,#166616,
#166617,#166618,#166619,#166620,#166621,#166622,#166623,#166624,#166625,
#166626,#166627,#166628,#166629,#166630,#166631,#166632,#166633,#166634,
#166635,#166636,#166637,#166638,#166639,#166640,#166641,#166642,#166643,
#166644,#166645,#166646,#166647,#166648,#166649,#166650,#166651),
 .UNSPECIFIED.,.F.,.F.,(4,3,3,3,3,3,3,3,3,3,3,3,3,3,3,3,3,3,3,3,3,3,3,3,
3,3,3,3,3,3,3,3,3,3,3,3,3,3,3,3,3,3,3,3,3,3,3,3,3,3,3,3,3,3,3,3,3,3,3,3,
3,3,3,3,3,3,3,3,3,3,3,3,3,3,3,3,3,3,3,3,3,3,3,3,3,4),(135.088484268768,
135.174411881758,135.260833130134,135.347449824148,135.434213236371,135.475106554013,
135.546529828863,135.617899955776,135.689230527297,135.760543864782,135.831844551604,
135.903170033097,135.973575097321,136.061280586662,136.149456949081,136.238061359699,
136.326761666583,136.415357926518,136.472043640628,136.545013085078,136.617937076171,
136.690828602912,136.763710801833,136.836585719876,136.909488669586,136.970512183936,
137.049812967885,137.129135898362,137.208478500372,137.287851577545,137.367233258542,
137.446630035651,137.468980727243,137.548378121912,137.62776179574,137.707129247381,
137.786474431193,137.865797450459,137.945091680081,137.967449270551,138.04035167082,
138.113231527865,138.186101797298,138.258998141703,138.331906797488,138.404875110437,
138.465917813859,138.554492145472,138.643192510946,138.731759323049,138.820102736613,
138.907872453238,138.964386357166,139.035709855516,139.107013605671,139.178311108943,
139.24964360459,139.320991963329,139.392412618296,139.462854900474,139.538958396495,
139.615011542566,139.691024732801,139.767008332682,139.84297268601,139.920075098645,
139.996046826684,140.072031153943,140.148037495615,140.225976118484,140.302085157912,
140.3809385725,140.459791987089,140.535924859334,140.611964560405,140.687920565776,
140.763779008313,140.839580071867,140.915319392601,140.958260530396,141.031847365433,
141.10545872087,141.179143713537,141.252869320595,141.326690169256,141.371669411541),
 .UNSPECIFIED.);
#3196=B_SPLINE_CURVE_WITH_KNOTS('',3,(#166653,#166654,#166655,#166656,#166657,
#166658,#166659,#166660,#166661,#166662,#166663,#166664,#166665,#166666,
#166667),.UNSPECIFIED.,.F.,.F.,(4,1,1,1,1,1,1,1,1,1,1,1,4),(141.371669411541,
141.456729073704,142.453666160319,142.952134703627,143.450603246934,143.949071790242,
144.447540333549,144.946008876857,145.444477420164,145.942945963472,146.441414506779,
147.438351593395,147.654854718721),.UNSPECIFIED.);
#3197=B_SPLINE_CURVE_WITH_KNOTS('',3,(#166669,#166670,#166671,#166672,#166673,
#166674,#166675,#166676,#166677,#166678,#166679,#166680,#166681,#166682,
#166683,#166684,#166685,#166686,#166687,#166688,#166689,#166690,#166691,
#166692,#166693,#166694,#166695,#166696,#166697,#166698,#166699,#166700,
#166701,#166702,#166703,#166704,#166705,#166706,#166707,#166708,#166709,
#166710,#166711,#166712,#166713,#166714,#166715,#166716,#166717,#166718,
#166719,#166720,#166721,#166722,#166723,#166724,#166725,#166726,#166727,
#166728,#166729,#166730,#166731,#166732,#166733,#166734,#166735,#166736,
#166737,#166738,#166739,#166740,#166741,#166742,#166743,#166744,#166745,
#166746,#166747,#166748,#166749,#166750,#166751,#166752,#166753,#166754,
#166755,#166756,#166757,#166758,#166759,#166760,#166761,#166762,#166763,
#166764,#166765,#166766,#166767,#166768,#166769,#166770,#166771,#166772,
#166773,#166774,#166775,#166776,#166777,#166778,#166779,#166780,#166781,
#166782,#166783,#166784,#166785,#166786,#166787,#166788,#166789,#166790,
#166791,#166792,#166793,#166794,#166795,#166796,#166797,#166798,#166799,
#166800,#166801,#166802,#166803,#166804,#166805,#166806,#166807,#166808,
#166809,#166810,#166811,#166812,#166813,#166814,#166815,#166816,#166817,
#166818,#166819,#166820,#166821,#166822,#166823,#166824,#166825,#166826,
#166827,#166828,#166829,#166830,#166831,#166832,#166833,#166834,#166835,
#166836,#166837,#166838,#166839,#166840,#166841,#166842,#166843,#166844,
#166845,#166846,#166847,#166848,#166849,#166850,#166851,#166852,#166853,
#166854,#166855,#166856,#166857,#166858,#166859,#166860,#166861,#166862,
#166863,#166864,#166865,#166866,#166867,#166868,#166869,#166870,#166871,
#166872,#166873,#166874,#166875,#166876,#166877,#166878,#166879,#166880,
#166881,#166882,#166883,#166884,#166885,#166886,#166887,#166888,#166889,
#166890,#166891,#166892,#166893,#166894,#166895,#166896,#166897,#166898,
#166899,#166900,#166901,#166902,#166903,#166904,#166905,#166906,#166907,
#166908,#166909,#166910,#166911,#166912,#166913,#166914,#166915,#166916,
#166917,#166918,#166919,#166920,#166921,#166922,#166923,#166924),
 .UNSPECIFIED.,.F.,.F.,(4,3,3,3,3,3,3,3,3,3,3,3,3,3,3,3,3,3,3,3,3,3,3,3,
3,3,3,3,3,3,3,3,3,3,3,3,3,3,3,3,3,3,3,3,3,3,3,3,3,3,3,3,3,3,3,3,3,3,3,3,
3,3,3,3,3,3,3,3,3,3,3,3,3,3,3,3,3,3,3,3,3,3,3,3,3,4),(147.654854718721,
147.72659930312,147.798301556539,147.869977993175,147.936820136702,148.01256250148,
148.088350622185,148.164193792981,148.240148751194,148.316165183482,148.392300978936,
148.43528868001,148.511499260519,148.587641864807,148.663726951184,148.739764937492,
148.815766208083,148.892823652901,148.968788915062,149.044750506961,149.120717834058,
149.198594817199,149.274624614666,149.353425190645,149.432225766625,149.503649041421,
149.575019168282,149.64634973975,149.717663077184,149.788963763955,149.860289245397,
149.930694309932,150.018399799239,150.106576161617,150.195180572185,150.283880879014,
150.372477138894,150.42916285324,150.502132298068,150.57505628954,150.647947816658,
150.720830015955,150.793704934373,150.866607884455,150.927631396547,151.006932178665,
151.08625510729,151.165597707437,151.244970782754,151.324352461906,151.403749237202,
151.426099939855,151.505497338627,151.584881016578,151.664248472337,151.743593660218,
151.822916683505,151.90221091705,151.924568483163,151.99747087888,152.070350731371,
152.143220996249,152.216117336111,152.289025987356,152.361994295789,152.42303702647,
152.511611372041,152.600311751838,152.688878577832,152.777222004591,152.864991732835,
152.921505569778,152.992829065116,153.064132812262,153.13543031253,153.206762805185,
153.278111160937,153.349531812937,153.419974113085,153.500009163612,153.57998474546,
153.659895229108,153.739703944664,153.819442361188,153.899074932354,153.938038318046),
 .UNSPECIFIED.);
#3198=B_SPLINE_CURVE_WITH_KNOTS('',3,(#166926,#166927,#166928,#166929,#166930,
#166931,#166932,#166933,#166934,#166935,#166936,#166937,#166938,#166939,
#166940,#166941,#166942,#166943,#166944,#166945,#166946,#166947,#166948,
#166949,#166950,#166951,#166952,#166953,#166954,#166955,#166956,#166957,
#166958,#166959,#166960,#166961,#166962,#166963,#166964,#166965,#166966,
#166967,#166968,#166969,#166970,#166971,#166972,#166973,#166974,#166975,
#166976,#166977,#166978,#166979,#166980,#166981,#166982,#166983,#166984,
#166985,#166986,#166987,#166988,#166989,#166990,#166991,#166992,#166993,
#166994,#166995,#166996,#166997,#166998,#166999,#167000,#167001,#167002,
#167003,#167004,#167005,#167006,#167007,#167008,#167009,#167010,#167011,
#167012,#167013,#167014,#167015,#167016,#167017,#167018,#167019,#167020,
#167021,#167022,#167023,#167024,#167025,#167026,#167027,#167028,#167029,
#167030,#167031,#167032,#167033,#167034,#167035,#167036,#167037,#167038,
#167039,#167040,#167041,#167042,#167043,#167044,#167045,#167046,#167047,
#167048,#167049,#167050,#167051,#167052,#167053,#167054,#167055,#167056,
#167057,#167058,#167059,#167060,#167061,#167062,#167063,#167064,#167065,
#167066,#167067,#167068,#167069,#167070,#167071,#167072,#167073,#167074,
#167075,#167076,#167077,#167078,#167079,#167080,#167081,#167082,#167083,
#167084,#167085,#167086,#167087,#167088,#167089,#167090,#167091,#167092,
#167093,#167094,#167095,#167096,#167097,#167098,#167099,#167100,#167101,
#167102,#167103,#167104,#167105,#167106,#167107,#167108,#167109,#167110,
#167111,#167112,#167113,#167114,#167115,#167116,#167117,#167118,#167119,
#167120,#167121,#167122,#167123,#167124,#167125,#167126,#167127,#167128,
#167129,#167130,#167131,#167132,#167133,#167134,#167135,#167136,#167137,
#167138,#167139,#167140,#167141,#167142,#167143,#167144,#167145,#167146,
#167147,#167148,#167149,#167150,#167151,#167152,#167153,#167154,#167155,
#167156,#167157,#167158,#167159,#167160,#167161,#167162,#167163,#167164,
#167165,#167166,#167167,#167168,#167169,#167170,#167171,#167172,#167173,
#167174,#167175,#167176,#167177,#167178,#167179,#167180,#167181),
 .UNSPECIFIED.,.F.,.F.,(4,3,3,3,3,3,3,3,3,3,3,3,3,3,3,3,3,3,3,3,3,3,3,3,
3,3,3,3,3,3,3,3,3,3,3,3,3,3,3,3,3,3,3,3,3,3,3,3,3,3,3,3,3,3,3,3,3,3,3,3,
3,3,3,3,3,3,3,3,3,3,3,3,3,3,3,3,3,3,3,3,3,3,3,3,3,4),(153.9380400259,154.01774156604,
154.097563789192,154.177571946043,154.257667774446,154.337910276897,154.4169111997,
154.493044120776,154.569083870191,154.645039923326,154.720898412545,154.796699522112,
154.872438887665,154.915379743008,154.991122030882,155.066910073592,155.142753165459,
155.218708043807,155.294724395709,155.370860110543,155.413848286316,155.490058890158,
155.566201517879,155.642286627742,155.718324637542,155.79432593158,155.871383361749,
155.947348647013,156.023310261818,156.099277611579,156.177154551917,156.253184371199,
156.331984872065,156.410785372931,156.482208725666,156.553578930457,156.624909579826,
156.696222994972,156.767523759411,156.838849318175,156.909253916238,156.996958497115,
157.085133874579,157.173737247445,157.262436517993,157.351031797816,157.407722459546,
157.480692987845,157.553618060411,157.62651066566,157.699393935898,157.772269921869,
157.845173929934,157.906191002853,157.985488516737,158.064808145032,158.144147430725,
158.223517208898,158.302895613596,158.382289175932,158.404659546161,158.484062011193,
158.563450771727,158.642823298686,158.722173484869,158.801501443599,158.880800482891,
158.903128089468,158.976027192385,159.048903755277,159.121770735486,159.194663807133,
159.267569196936,159.340534269289,159.401596632776,159.49017046845,159.578870172144,
159.667436123138,159.755778593328,159.843547284668,159.900065176084,159.968705563624,
160.03733317896,160.105951360206,160.174594356136,160.220901167348),
 .UNSPECIFIED.);
#3199=B_SPLINE_CURVE_WITH_KNOTS('',3,(#167183,#167184,#167185,#167186,#167187,
#167188,#167189,#167190,#167191,#167192,#167193,#167194,#167195,#167196,
#167197,#167198,#167199,#167200),.UNSPECIFIED.,.F.,.F.,(4,2,2,2,2,2,2,2,
4),(160.221433754171,161.050583109518,161.879940885956,162.709298662394,
163.538656438832,164.36801421527,165.197371991708,166.026729768145,166.504401885182),
 .UNSPECIFIED.);
#3200=B_SPLINE_CURVE_WITH_KNOTS('',3,(#167202,#167203,#167204,#167205,#167206,
#167207,#167208,#167209,#167210,#167211,#167212,#167213),.UNSPECIFIED.,
 .F.,.F.,(4,1,1,1,1,1,1,1,1,4),(166.504733301143,167.377093325697,168.374030412312,
169.370967498927,169.869436042235,170.367904585542,170.86637312885,171.364841672157,
172.361778758772,172.787595947439),.UNSPECIFIED.);
#3201=B_SPLINE_CURVE_WITH_KNOTS('',3,(#167215,#167216,#167217,#167218,#167219,
#167220,#167221,#167222,#167223,#167224,#167225,#167226,#167227,#167228,
#167229,#167230,#167231,#167232),.UNSPECIFIED.,.F.,.F.,(4,2,2,2,2,2,2,2,
4),(172.787595947439,173.616953723877,174.446311500315,175.275669276753,
176.105027053191,176.934384829629,177.763742606067,178.593100382505,179.070781254619),
 .UNSPECIFIED.);
#3202=B_SPLINE_CURVE_WITH_KNOTS('',3,(#167234,#167235,#167236,#167237,#167238,
#167239,#167240,#167241,#167242,#167243,#167244,#167245,#167246,#167247,
#167248,#167249,#167250,#167251,#167252,#167253,#167254,#167255,#167256,
#167257,#167258,#167259,#167260,#167261,#167262,#167263,#167264,#167265,
#167266,#167267,#167268,#167269,#167270,#167271,#167272,#167273,#167274,
#167275,#167276,#167277,#167278,#167279,#167280,#167281,#167282,#167283,
#167284,#167285,#167286,#167287,#167288,#167289,#167290,#167291,#167292,
#167293,#167294,#167295,#167296,#167297,#167298,#167299,#167300,#167301,
#167302,#167303,#167304,#167305,#167306,#167307,#167308,#167309,#167310,
#167311,#167312,#167313,#167314,#167315,#167316,#167317,#167318,#167319,
#167320,#167321,#167322,#167323,#167324,#167325,#167326,#167327,#167328,
#167329,#167330,#167331,#167332,#167333,#167334,#167335,#167336,#167337,
#167338,#167339,#167340,#167341,#167342,#167343,#167344,#167345,#167346,
#167347,#167348,#167349,#167350,#167351,#167352,#167353,#167354,#167355,
#167356,#167357,#167358,#167359,#167360,#167361,#167362,#167363,#167364,
#167365,#167366,#167367,#167368,#167369,#167370,#167371,#167372,#167373,
#167374,#167375,#167376,#167377,#167378,#167379,#167380,#167381,#167382,
#167383,#167384,#167385,#167386,#167387,#167388,#167389,#167390,#167391,
#167392,#167393,#167394,#167395,#167396,#167397,#167398,#167399,#167400,
#167401,#167402,#167403,#167404,#167405,#167406,#167407,#167408,#167409,
#167410,#167411,#167412,#167413,#167414,#167415,#167416,#167417,#167418,
#167419,#167420,#167421,#167422,#167423,#167424,#167425,#167426,#167427,
#167428,#167429,#167430,#167431,#167432,#167433,#167434,#167435,#167436,
#167437,#167438,#167439,#167440,#167441,#167442,#167443,#167444,#167445,
#167446,#167447,#167448,#167449,#167450,#167451,#167452,#167453,#167454,
#167455,#167456,#167457,#167458,#167459,#167460,#167461,#167462,#167463,
#167464,#167465,#167466,#167467,#167468,#167469,#167470,#167471,#167472,
#167473,#167474,#167475,#167476,#167477,#167478,#167479,#167480,#167481,
#167482,#167483,#167484,#167485,#167486,#167487,#167488,#167489,#167490,
#167491,#167492,#167493,#167494,#167495,#167496,#167497,#167498,#167499,
#167500,#167501,#167502,#167503,#167504,#167505,#167506,#167507,#167508,
#167509,#167510,#167511,#167512,#167513,#167514,#167515,#167516,#167517,
#167518,#167519,#167520,#167521,#167522,#167523,#167524,#167525,#167526,
#167527,#167528,#167529,#167530,#167531,#167532,#167533,#167534,#167535,
#167536,#167537,#167538,#167539,#167540,#167541,#167542,#167543,#167544,
#167545,#167546,#167547,#167548,#167549,#167550,#167551,#167552,#167553,
#167554,#167555,#167556,#167557,#167558,#167559,#167560,#167561,#167562,
#167563,#167564,#167565,#167566,#167567,#167568,#167569,#167570,#167571,
#167572,#167573,#167574,#167575,#167576,#167577,#167578,#167579,#167580,
#167581,#167582,#167583,#167584,#167585,#167586,#167587,#167588,#167589,
#167590,#167591,#167592,#167593,#167594,#167595,#167596,#167597,#167598,
#167599,#167600,#167601,#167602,#167603,#167604,#167605,#167606,#167607,
#167608,#167609,#167610,#167611,#167612,#167613,#167614,#167615,#167616,
#167617,#167618,#167619,#167620,#167621,#167622,#167623,#167624,#167625,
#167626,#167627,#167628,#167629,#167630,#167631,#167632,#167633,#167634,
#167635,#167636,#167637,#167638,#167639,#167640,#167641,#167642,#167643,
#167644,#167645,#167646,#167647,#167648,#167649,#167650,#167651,#167652,
#167653,#167654,#167655,#167656,#167657,#167658,#167659,#167660,#167661,
#167662,#167663,#167664,#167665,#167666,#167667,#167668,#167669,#167670,
#167671,#167672,#167673,#167674,#167675,#167676,#167677,#167678,#167679,
#167680,#167681,#167682,#167683,#167684,#167685,#167686,#167687,#167688,
#167689,#167690,#167691,#167692,#167693,#167694,#167695,#167696,#167697,
#167698,#167699,#167700,#167701,#167702,#167703,#167704,#167705,#167706,
#167707,#167708,#167709,#167710,#167711,#167712,#167713,#167714,#167715,
#167716,#167717,#167718,#167719,#167720,#167721,#167722,#167723,#167724,
#167725,#167726,#167727,#167728,#167729,#167730,#167731,#167732,#167733,
#167734,#167735,#167736,#167737,#167738,#167739,#167740,#167741,#167742,
#167743,#167744,#167745,#167746,#167747,#167748,#167749,#167750,#167751,
#167752,#167753,#167754,#167755,#167756,#167757,#167758,#167759,#167760,
#167761,#167762,#167763,#167764,#167765,#167766,#167767,#167768,#167769,
#167770,#167771,#167772,#167773,#167774,#167775,#167776,#167777,#167778,
#167779,#167780,#167781,#167782,#167783,#167784,#167785,#167786,#167787,
#167788,#167789,#167790,#167791,#167792,#167793,#167794,#167795,#167796,
#167797,#167798,#167799,#167800,#167801,#167802,#167803,#167804,#167805,
#167806,#167807,#167808,#167809,#167810,#167811,#167812,#167813),
 .UNSPECIFIED.,.F.,.F.,(4,2,2,2,2,2,2,2,2,2,2,2,2,2,2,2,2,2,2,2,2,2,2,2,
2,2,2,2,2,2,2,2,2,2,2,2,2,2,2,2,2,2,2,2,2,2,2,2,2,2,2,2,2,2,2,2,2,2,2,2,
2,2,2,2,2,2,2,2,2,2,2,2,2,2,2,2,2,2,2,2,2,2,2,2,2,2,2,2,2,2,2,2,2,2,2,2,
2,2,2,2,2,2,2,2,2,2,2,2,2,2,2,2,2,2,2,2,2,2,2,2,2,2,2,2,2,2,2,2,2,2,2,2,
2,2,2,2,2,2,2,2,2,2,2,2,2,2,2,2,2,2,2,2,2,2,2,2,2,2,2,2,2,2,2,2,2,2,2,2,
2,2,2,2,2,2,2,2,2,2,2,2,2,2,2,2,2,2,2,2,2,2,2,2,2,2,2,2,2,2,2,2,2,2,2,2,
2,2,2,2,2,2,2,2,2,2,2,2,2,2,2,2,2,2,2,2,2,2,2,2,2,2,2,2,2,2,2,2,2,2,2,2,
2,2,2,2,2,2,2,2,2,2,2,2,2,2,2,2,2,2,2,2,2,2,2,2,2,2,2,2,2,2,2,2,2,2,2,2,
2,2,2,2,2,2,2,2,2,2,2,2,2,4),(0.00175473219377527,0.0102639915195822,0.0198551234661248,
0.0302624690351261,0.0442639585826937,0.0762429488247187,0.110239649230437,
0.141167562458834,0.199412869610709,0.207414357874238,0.213183952960719,
0.218465970450596,0.223602668039412,0.232650938987427,0.255783539160852,
0.285481548946414,0.289429207702587,0.387495333935431,0.469927022923076,
0.502691690386715,0.520987016661417,0.533502844462343,0.544021574055287,
0.555281059642907,0.569419391193581,0.59850935210662,0.694552126930168,
0.811921268581424,0.880576941442497,0.962237397992056,1.00024304425663,
1.00665281604221,1.0095615408409,1.0117437427584,1.01378796825245,1.01716291012073,
1.02571567642927,1.15936661647529,1.23081736289662,1.33873084442956,1.43058111604604,
1.43852973544966,1.44230426895295,1.44520768326752,1.44798223725234,1.45269045860845,
1.46532649307236,1.66881119872638,1.78561912740571,1.83270908311646,1.85792111085327,
1.86254606258551,1.86530647538949,1.86755602336931,1.86981043098472,1.87391598249238,
1.88688176234183,2.07146869941756,2.20405899312687,2.22191526164143,2.2322523882598,
2.23945424949218,2.24646731437987,2.24648779918434,2.24650846143184,2.24652930160323,
2.24655032020409,2.24657151770201,2.2465928944687,2.24661445089594,2.24663617867777,
2.24665806969917,2.24668014241987,2.24670240458843,2.24672878287883,2.2467560505632,
2.24678422992943,2.2468133433831,2.24684341329753,2.24687446205743,2.24690651202037,
2.24693958543641,2.24697370441048,2.2470088909034,2.24704516665339,2.25363205660697,
2.26196122984078,2.27829941173527,2.42277900501808,2.50239711969813,2.60865122694243,
2.62302258262459,2.62711867329848,2.62962041614353,2.63188228856662,2.63477573781953,
2.63937301690103,2.66372676850353,2.83675971454541,2.95093174102913,3.02940881452137,
3.04380590509473,3.04859521224104,3.05169582858694,3.05462253382368,3.05848104175936,
3.06709423594561,3.14172326738905,3.31349454649346,3.47163136632539,3.48003623722723,
3.48328387300885,3.4855296942585,3.48773705371138,3.49040784876959,3.49712988682739,
3.60041100660568,3.77728778908965,3.89902308387369,3.92798960650723,3.94211463379963,
3.95338430996426,3.96624174476683,3.98808691089097,4.10360942433689,4.22502169338295,
4.25077288853278,4.26844156627594,4.27572797744257,4.28074259414517,4.28627095258433,
4.29634956798692,4.33861879763701,4.41080859296117,4.43757189899509,4.45864029675713,
4.47060258147791,4.48115569481206,4.49458495611188,4.52343382075178,4.58024363676307,
4.64333646649951,4.67285838548971,4.68155635514232,4.68751173879338,4.69321943481464,
4.7013640159026,4.72475739058829,4.85117107257798,4.91158601336947,4.93373620098741,
4.95024994073748,4.96900584347225,5.01033944071091,5.04715643646294,5.06749076981571,
5.08336672650831,5.09540066083849,5.11293414767461,5.16450425872884,5.20523099201403,
5.22388156243171,5.24041785976391,5.26276410868403,5.32515061251997,5.39082874106249,
5.39833906223304,5.40214996477169,5.46712424776639,5.47882920950683,5.48557401439953,
5.49089767759533,5.49846957464732,5.51808263661487,5.53522140029342,5.61878935055442,
5.67127506498819,5.68799340436212,5.69797518539345,5.70870451942961,5.72346636505519,
5.76184645233346,5.79770679465068,5.8721853988259,5.88402367110536,5.89120586463471,
5.89678650209857,5.90329424901015,5.91654913550917,5.93419862424077,6.06223755129916,
6.18529951441336,6.20739172807289,6.2203043684978,6.23156810301128,6.24561405996954,
6.27415203952366,6.39257553874006,6.48898460078045,6.65681224782744,6.67958074887322,
6.68399482209428,6.68676263693873,6.6889251373689,6.69131580485672,6.69522722337943,
6.70890884844539,6.80389264846716,6.97328335917045,7.10492468536199,7.11448183264075,
7.11824741278404,7.12098181151917,7.12390447185036,7.12780790026219,7.13643667647576,
7.25628636913056,7.45913210414344,7.53235043294122,7.53879543894682,7.54175713943717,
7.54403540023546,7.54648011053504,7.55032142064125,7.56238820330349,7.63912570255235,
7.88504274321496,7.90841725196076,7.91717885079275,7.92346022498246,7.92935939418366,
7.93695347219224,7.95044890555484,7.96685431206167,8.0796301237949,8.28267026853171,
8.28719827583329,8.300086867302,8.30418217661532,8.30643417327188,8.30868338328819,
8.31144642315177,8.31649931281682,8.34749806235849,8.37808690709208,8.50176356742623,
8.70798840858865,8.72096628124147,8.72572628919026,8.72851063790588,8.7311195772564,
8.73471389008161,8.74176641706399,8.7912658949537,8.88288436049876,9.00857158721545,
9.14724117327041,9.15640766933732,9.15988259505161,9.16194610852591,9.16390054970121,
9.16662703393643,9.17209866878485,9.21035819211417,9.29338820192485,9.44452207735449,
9.56902893193325,9.60247371703836,9.61722186940431,9.62858925684194,9.63906982278748,
9.65114910945188,9.68554096969399,9.73451548259927,9.9019120522969,9.93949848342984,
9.94948066519615,9.95478401210923,9.96016128914257,9.96583709243551,9.9687285708481,
9.98881023100644,10.0306775926922,10.1157874817235,10.1359746972935,10.1477584569336,
10.1580074895441,10.1682341579043,10.1814573680671,10.2240413365649),
 .UNSPECIFIED.);
#3203=B_SPLINE_CURVE_WITH_KNOTS('',3,(#167815,#167816,#167817,#167818,#167819,
#167820,#167821,#167822,#167823,#167824,#167825,#167826,#167827,#167828,
#167829,#167830,#167831,#167832),.UNSPECIFIED.,.F.,.F.,(4,2,2,2,2,2,2,2,
4),(191.637151868978,192.466509645416,193.295867421854,194.125225198292,
194.95458297473,195.783940751168,196.613298527606,197.442656304043,197.920337176157),
 .UNSPECIFIED.);
#3204=B_SPLINE_CURVE_WITH_KNOTS('',3,(#167834,#167835,#167836,#167837,#167838,
#167839,#167840,#167841,#167842,#167843,#167844,#167845,#167846,#167847,
#167848,#167849,#167850,#167851,#167852,#167853,#167854,#167855,#167856,
#167857,#167858,#167859,#167860,#167861,#167862,#167863,#167864,#167865,
#167866,#167867,#167868,#167869,#167870,#167871,#167872,#167873,#167874,
#167875,#167876,#167877,#167878,#167879,#167880,#167881,#167882,#167883,
#167884,#167885,#167886,#167887,#167888,#167889,#167890,#167891,#167892,
#167893,#167894,#167895,#167896,#167897,#167898,#167899,#167900,#167901,
#167902,#167903,#167904,#167905,#167906,#167907,#167908,#167909,#167910,
#167911,#167912,#167913,#167914,#167915,#167916,#167917,#167918,#167919,
#167920,#167921,#167922,#167923,#167924,#167925,#167926,#167927,#167928,
#167929,#167930,#167931,#167932,#167933,#167934,#167935,#167936,#167937,
#167938,#167939,#167940,#167941,#167942,#167943,#167944,#167945,#167946,
#167947,#167948,#167949,#167950,#167951,#167952,#167953,#167954,#167955,
#167956,#167957,#167958,#167959,#167960,#167961,#167962,#167963,#167964,
#167965,#167966,#167967,#167968,#167969,#167970,#167971,#167972,#167973,
#167974,#167975,#167976,#167977,#167978,#167979,#167980,#167981,#167982,
#167983,#167984,#167985,#167986,#167987,#167988,#167989,#167990,#167991,
#167992,#167993,#167994,#167995,#167996,#167997,#167998,#167999,#168000,
#168001,#168002,#168003,#168004,#168005,#168006,#168007,#168008,#168009,
#168010,#168011,#168012,#168013,#168014,#168015,#168016,#168017,#168018,
#168019,#168020,#168021,#168022,#168023,#168024,#168025,#168026,#168027,
#168028,#168029,#168030,#168031,#168032,#168033,#168034,#168035,#168036,
#168037,#168038,#168039,#168040,#168041,#168042,#168043,#168044,#168045,
#168046,#168047,#168048,#168049,#168050,#168051,#168052,#168053,#168054,
#168055,#168056,#168057,#168058,#168059,#168060,#168061,#168062,#168063,
#168064,#168065,#168066,#168067,#168068,#168069,#168070,#168071,#168072,
#168073,#168074,#168075,#168076,#168077,#168078,#168079,#168080,#168081,
#168082,#168083,#168084,#168085,#168086,#168087,#168088,#168089,#168090,
#168091,#168092,#168093,#168094,#168095,#168096,#168097,#168098,#168099,
#168100,#168101,#168102,#168103,#168104,#168105,#168106,#168107,#168108,
#168109,#168110,#168111,#168112,#168113,#168114,#168115,#168116,#168117,
#168118,#168119,#168120,#168121,#168122,#168123,#168124,#168125,#168126,
#168127,#168128,#168129,#168130,#168131,#168132,#168133,#168134,#168135,
#168136,#168137,#168138,#168139,#168140,#168141,#168142,#168143,#168144,
#168145,#168146,#168147,#168148,#168149,#168150,#168151,#168152,#168153,
#168154,#168155,#168156,#168157,#168158,#168159,#168160,#168161,#168162,
#168163,#168164,#168165,#168166,#168167,#168168,#168169,#168170,#168171,
#168172,#168173,#168174,#168175,#168176,#168177,#168178,#168179,#168180,
#168181,#168182,#168183,#168184,#168185,#168186,#168187,#168188,#168189,
#168190,#168191,#168192,#168193,#168194,#168195,#168196,#168197,#168198,
#168199,#168200,#168201,#168202,#168203,#168204,#168205,#168206,#168207,
#168208,#168209,#168210,#168211,#168212,#168213,#168214,#168215,#168216,
#168217,#168218,#168219,#168220,#168221,#168222,#168223,#168224,#168225,
#168226,#168227,#168228,#168229,#168230,#168231,#168232,#168233,#168234,
#168235,#168236,#168237,#168238,#168239,#168240,#168241,#168242,#168243,
#168244,#168245,#168246,#168247,#168248,#168249,#168250,#168251,#168252,
#168253,#168254,#168255,#168256,#168257,#168258,#168259,#168260,#168261,
#168262,#168263,#168264,#168265,#168266,#168267,#168268,#168269,#168270,
#168271,#168272,#168273,#168274,#168275,#168276,#168277,#168278,#168279,
#168280,#168281,#168282,#168283,#168284,#168285,#168286,#168287,#168288,
#168289,#168290,#168291,#168292,#168293,#168294,#168295,#168296,#168297,
#168298,#168299,#168300,#168301,#168302,#168303,#168304,#168305,#168306,
#168307,#168308,#168309,#168310,#168311,#168312,#168313,#168314,#168315,
#168316,#168317,#168318,#168319,#168320,#168321,#168322,#168323,#168324,
#168325,#168326,#168327,#168328,#168329,#168330,#168331,#168332,#168333,
#168334,#168335,#168336,#168337,#168338,#168339,#168340,#168341,#168342,
#168343,#168344,#168345,#168346,#168347,#168348,#168349,#168350,#168351,
#168352,#168353,#168354,#168355,#168356,#168357,#168358,#168359,#168360,
#168361,#168362,#168363,#168364,#168365,#168366,#168367,#168368,#168369,
#168370,#168371,#168372,#168373,#168374,#168375,#168376,#168377,#168378,
#168379,#168380,#168381,#168382,#168383,#168384,#168385,#168386,#168387,
#168388,#168389,#168390,#168391,#168392,#168393,#168394,#168395,#168396,
#168397,#168398,#168399,#168400,#168401,#168402,#168403,#168404,#168405,
#168406,#168407,#168408,#168409,#168410,#168411,#168412,#168413,#168414,
#168415,#168416,#168417,#168418,#168419,#168420,#168421,#168422,#168423,
#168424,#168425,#168426,#168427,#168428,#168429,#168430,#168431,#168432,
#168433,#168434,#168435),.UNSPECIFIED.,.F.,.F.,(4,2,2,2,2,2,2,2,2,2,2,2,
2,2,2,2,2,2,2,2,2,2,2,2,2,2,2,2,2,2,2,2,2,2,2,2,2,2,2,2,2,2,2,2,2,2,2,2,
2,2,2,2,2,2,2,2,2,2,2,2,2,2,2,2,2,2,2,2,2,2,2,2,2,2,2,2,2,2,2,2,2,2,2,2,
2,2,2,2,2,2,2,2,2,2,2,2,2,2,2,2,2,2,2,2,2,2,2,2,2,2,2,2,2,2,2,2,2,2,2,2,
2,2,2,2,2,2,2,2,2,2,2,2,2,2,2,2,2,2,2,2,2,2,2,2,2,2,2,2,2,2,2,2,2,2,2,2,
2,2,2,2,2,2,2,2,2,2,2,2,2,2,2,2,2,2,2,2,2,2,2,2,2,2,2,2,2,2,2,2,2,2,2,2,
2,2,2,2,2,2,2,2,2,2,2,2,2,2,2,2,2,2,2,2,2,2,2,2,2,2,2,2,2,2,2,2,2,2,2,2,
2,2,2,2,2,2,2,2,2,2,2,2,2,2,2,2,2,2,2,2,2,2,2,2,2,2,2,2,2,2,2,2,2,2,2,2,
2,2,2,2,2,2,2,2,2,2,2,2,2,2,2,2,2,2,2,2,2,2,2,2,2,2,2,2,2,2,2,2,2,2,2,2,
4),(0.00175495097563408,0.0352625399406719,0.197360108617795,0.253608699459729,
0.274137831421876,0.284540307816254,0.291090370885871,0.296216182098079,
0.301785480521977,0.308860599834827,0.320319216837973,0.371350304294198,
0.436674209203219,0.471058084799032,0.485293161062722,0.495397622816899,
0.506513777457236,0.523788811408338,0.593857050788224,0.645243823011645,
0.675776901551024,0.688989513769135,0.696610806006971,0.702172600756485,
0.707502347824358,0.714198211852011,0.725673491290616,0.778350542453821,
0.782644126998547,0.882418987187402,0.933655256832732,0.954764872212928,
0.970598314027118,0.988147877967994,1.02602581308313,1.0712697490232,1.08942473941662,
1.08982884048817,1.09023277301792,1.09063663129866,1.09104051294525,1.09144451882367,
1.09157517239452,1.09171715794843,1.09187136545249,1.09203874037196,1.09222028517601,
1.09241706072286,1.09263018747407,1.09286084657252,1.09311028083545,1.09337979568197,
1.09367076006785,1.09398460752515,1.09432283737211,1.09468701623391,1.09507877994561,
1.09549983595649,1.09595196631501,1.09643703122404,1.0969569731285,1.10801517055347,
1.1223962736298,1.20753471703579,1.23311876062243,1.24910045041635,1.25707286181742,
1.25968093241407,1.28124030461214,1.33602465638445,1.44760942221458,1.47544015371053,
1.48852304799468,1.49647212012827,1.50243551124633,1.50842090095045,1.51497755266692,
1.52789598185376,1.5839778386596,1.63204744207204,1.67109965763502,1.69912000847182,
1.71240757755335,1.7225174825199,1.73410848898233,1.75361627552157,1.8181894524433,
1.8725488350463,1.89102387475517,1.90070279013383,1.9081864858002,1.91408237897576,
1.91917605973781,1.92628729049803,1.94633080341079,1.95083214455481,2.07858476422359,
2.20518474348015,2.22116889423628,2.23277651738855,2.24425943024408,2.25553366701155,
2.26970958505557,2.30551636427595,2.49938912017426,2.65901711994682,2.69853463434638,
2.70386637554691,2.70656479820441,2.70851570434621,2.71059091729695,2.71352458133718,
2.72140834618246,2.83658764567174,3.00040939141186,3.1246582500748,3.13440830470489,
3.13851197617747,3.14147020754299,3.14415895465361,3.14774327053315,3.15680295804168,
3.24890927194457,3.43790246844447,3.49385049845787,3.5232874633109,3.55416366803585,
3.55929913921458,3.5620297101123,3.56406071201076,3.56659589152047,3.57084018130091,
3.5849646110978,3.60917850321082,3.62918076345487,3.75799623904513,3.84812567182715,
3.91983489106167,3.93361836881346,3.9413085110774,3.94783915022913,3.95522986102456,
3.967630035295,4.01118304502898,4.05140509298979,4.12020746605273,4.20109216079533,
4.28369738842697,4.31726063527399,4.32257183516267,4.32533945489747,4.327589568565,
4.32983820038647,4.33392208256509,4.3466634704121,4.58536769347246,4.69172273248207,
4.73666401108837,4.7435554222001,4.74711699813715,4.7499972939198,4.75286392617472,
4.75803223062875,4.77390391493287,5.05627709492252,5.11325855885042,5.17229405399529,
5.17769174262378,5.18044835212201,5.18247690613933,5.18467086704538,5.1876452745471,
5.19441022531098,5.30168709418233,5.4964913320072,5.59555220571743,5.62506448040751,
5.6392917567656,5.65057292509323,5.66336876815058,5.68549874640199,5.81110591610013,
5.94204548835099,5.96390036591449,5.97126094232207,5.97640205841875,5.98223293598735,
5.99086700088689,6.01638172990783,6.04212509726058,6.12901010287418,6.1534241991619,
6.1661829252739,6.17669678700075,6.18917163010758,6.21275339876847,6.22944691034306,
6.28371868699829,6.36456173047886,6.3765056194844,6.38290610846679,6.38894542841228,
6.39725734210314,6.4173641758281,6.43402967186209,6.50292904282763,6.55352949228307,
6.60928860884352,6.62917724565551,6.64573248053629,6.6637233983993,6.69868752994647,
6.76567353545787,6.78130164492111,6.79215629301713,6.8127917352042,6.86091174150864,
6.90239216188215,6.92119599242194,6.93770625900967,6.95978757369098,7.01948714791512,
7.14094312901029,7.16892247457594,7.17856865200984,7.18424866420476,7.19021870124338,
7.19906483130723,7.23023236254152,7.30076375127872,7.36746137937351,7.38497608701334,
7.39510334423278,7.40575546678763,7.41999617638211,7.45440835533803,7.51473037295328,
7.57087991766468,7.58227458628751,7.58933212802182,7.59490048906351,7.60152077370934,
7.61537544191856,7.63406479057055,7.68262778203271,7.82251934479748,7.88815860391264,
7.90751965824174,7.91964916324831,7.9307745069614,7.94549359367843,7.97779488883906,
8.13216671623121,8.36358374414034,8.37904091615512,8.3832642057436,8.38574952740638,
8.38789972132987,8.39052529235364,8.395505046581,8.42752811672482,8.48146159713842,
8.64367310446665,8.80311868340908,8.81291476662083,8.81672126626415,8.81946711462304,
8.82238504936972,8.82625324933647,8.83468849200978,8.91758419458684,9.04022973465267,
9.22489764793346,9.23554697745061,9.23934449189476,9.2415358536265,9.24357090924747,
9.24634704820871,9.25169818356904,9.28628376534383,9.36875076707217,9.47836524403668,
9.50485501420989,9.59589938945606,9.61104968965221,9.61902732485961,9.62546043080808,
9.63157929807612,9.64155373233103,9.66824360650781,9.79991339906604,9.98219948507729,
9.99796931467612,10.0023460116868,10.0049361715052,10.0071860348159,10.0099446596262,
10.0152113752771,10.0498221746028,10.0797479890141,10.2255100735221),
 .UNSPECIFIED.);
#3205=B_SPLINE_CURVE_WITH_KNOTS('',3,(#168437,#168438,#168439,#168440,#168441,
#168442,#168443,#168444,#168445,#168446,#168447,#168448,#168449,#168450,
#168451),.UNSPECIFIED.,.F.,.F.,(4,1,1,1,1,1,1,1,1,1,1,1,4),(210.486707790517,
211.242325136762,211.74079368007,212.239262223377,212.737730766685,213.236199309992,
213.7346678533,214.233136396607,214.731604939915,215.230073483222,216.227010569838,
216.725479113145,216.769893097696),.UNSPECIFIED.);
#3206=B_SPLINE_CURVE_WITH_KNOTS('',3,(#168453,#168454,#168455,#168456,#168457,
#168458,#168459,#168460,#168461,#168462,#168463,#168464,#168465,#168466,
#168467,#168468,#168469,#168470,#168471,#168472,#168473,#168474,#168475,
#168476,#168477,#168478,#168479,#168480,#168481,#168482,#168483,#168484,
#168485,#168486,#168487,#168488,#168489,#168490,#168491,#168492,#168493,
#168494,#168495,#168496,#168497,#168498,#168499,#168500,#168501,#168502,
#168503,#168504,#168505,#168506,#168507,#168508,#168509,#168510,#168511,
#168512,#168513,#168514,#168515,#168516,#168517,#168518,#168519,#168520,
#168521,#168522,#168523,#168524,#168525,#168526,#168527,#168528,#168529,
#168530,#168531,#168532,#168533,#168534,#168535,#168536,#168537,#168538,
#168539,#168540,#168541,#168542,#168543,#168544,#168545,#168546,#168547,
#168548,#168549,#168550,#168551,#168552,#168553,#168554,#168555,#168556,
#168557,#168558,#168559,#168560,#168561,#168562,#168563,#168564,#168565,
#168566,#168567,#168568,#168569,#168570,#168571,#168572,#168573,#168574,
#168575,#168576,#168577,#168578,#168579,#168580,#168581,#168582,#168583,
#168584,#168585,#168586,#168587,#168588,#168589,#168590,#168591,#168592,
#168593,#168594,#168595,#168596,#168597,#168598,#168599,#168600,#168601,
#168602,#168603,#168604,#168605,#168606,#168607,#168608,#168609,#168610,
#168611,#168612,#168613,#168614,#168615,#168616,#168617,#168618,#168619,
#168620,#168621,#168622,#168623,#168624,#168625,#168626,#168627,#168628,
#168629,#168630,#168631,#168632,#168633,#168634,#168635,#168636,#168637,
#168638,#168639,#168640,#168641,#168642,#168643,#168644,#168645,#168646,
#168647,#168648,#168649,#168650,#168651,#168652,#168653,#168654,#168655,
#168656,#168657,#168658,#168659,#168660,#168661,#168662,#168663,#168664,
#168665,#168666,#168667,#168668,#168669,#168670,#168671,#168672,#168673,
#168674,#168675,#168676,#168677,#168678,#168679,#168680,#168681,#168682,
#168683,#168684,#168685,#168686,#168687,#168688,#168689,#168690,#168691,
#168692,#168693,#168694,#168695,#168696,#168697,#168698,#168699,#168700,
#168701,#168702,#168703,#168704,#168705,#168706,#168707,#168708),
 .UNSPECIFIED.,.F.,.F.,(4,3,3,3,3,3,3,3,3,3,3,3,3,3,3,3,3,3,3,3,3,3,3,3,
3,3,3,3,3,3,3,3,3,3,3,3,3,3,3,3,3,3,3,3,3,3,3,3,3,3,3,3,3,3,3,3,3,3,3,3,
3,3,3,3,3,3,3,3,3,3,3,3,3,3,3,3,3,3,3,3,3,3,3,3,3,4),(216.769893133811,
216.846463313756,216.923103012482,216.999878057372,217.076723021884,217.153710500839,
217.223947656453,217.300158236927,217.376300841179,217.452385927519,217.528423913791,
217.604425184346,217.681482629186,217.757447891311,217.833409483176,217.909376810237,
217.987253793445,218.063283590877,218.142084166973,218.220884743068,218.292308017918,
218.363678144831,218.435008716353,218.506322053838,218.577622740661,218.648948222153,
218.719353286375,218.807058775715,218.895235138133,218.98383954875,219.072539855632,
219.161136115566,219.217821829683,219.290791274133,219.363715265227,219.436606791968,
219.509488990889,219.582363908933,219.655266858643,219.71629037299,219.795591156939,
219.874914087416,219.954256689426,220.033629766598,220.113011447596,220.192408224704,
220.214758916298,220.294156310967,220.373539984795,220.452907436436,220.532252620248,
220.611575639514,220.690869869136,220.713227459606,220.786129859875,220.85900971692,
220.931879986353,221.004776330759,221.077684986544,221.150653299492,221.211696002913,
221.300270334525,221.388970699998,221.477537512099,221.565880925662,221.653650642287,
221.710164546221,221.781488044571,221.852791794727,221.924089297999,221.995421793646,
222.066770152385,222.138190807352,222.208633089528,222.283749424407,222.358810363004,
222.43382811189,222.511234398514,222.586208928398,222.661179643841,222.736157562242,
222.811153703102,222.886205945411,222.96129135231,223.036446415907,223.053078404876),
 .UNSPECIFIED.);
#3207=B_SPLINE_CURVE_WITH_KNOTS('',3,(#168710,#168711,#168712,#168713,#168714,
#168715,#168716,#168717,#168718,#168719,#168720,#168721,#168722,#168723,
#168724,#168725),.UNSPECIFIED.,.F.,.F.,(4,1,1,1,1,1,1,1,1,1,1,1,1,4),(223.053078404876,
223.205570176143,223.704038719451,224.202507262759,225.199444349374,225.697912892681,
226.196381435989,226.694849979296,227.193318522604,227.691787065911,228.190255609219,
228.688724152527,229.187192695834,229.336263712055),.UNSPECIFIED.);
#3208=B_SPLINE_CURVE_WITH_KNOTS('',3,(#168727,#168728,#168729,#168730,#168731,
#168732,#168733,#168734,#168735,#168736,#168737,#168738,#168739,#168740,
#168741,#168742,#168743,#168744,#168745,#168746,#168747,#168748,#168749,
#168750,#168751,#168752,#168753,#168754,#168755,#168756,#168757,#168758,
#168759,#168760,#168761,#168762,#168763,#168764,#168765,#168766,#168767,
#168768,#168769,#168770,#168771,#168772,#168773,#168774,#168775,#168776,
#168777,#168778,#168779,#168780,#168781,#168782,#168783,#168784,#168785,
#168786,#168787,#168788,#168789,#168790,#168791,#168792,#168793,#168794,
#168795,#168796,#168797,#168798,#168799,#168800,#168801,#168802,#168803,
#168804,#168805,#168806,#168807,#168808,#168809,#168810,#168811,#168812,
#168813,#168814,#168815,#168816,#168817,#168818,#168819,#168820,#168821,
#168822,#168823,#168824,#168825,#168826,#168827,#168828,#168829,#168830,
#168831,#168832,#168833,#168834,#168835,#168836,#168837,#168838,#168839,
#168840,#168841,#168842,#168843,#168844,#168845,#168846,#168847,#168848,
#168849,#168850,#168851,#168852,#168853,#168854,#168855,#168856,#168857,
#168858,#168859,#168860,#168861,#168862,#168863,#168864,#168865,#168866,
#168867,#168868,#168869,#168870,#168871,#168872,#168873,#168874,#168875,
#168876,#168877,#168878,#168879,#168880,#168881,#168882,#168883,#168884,
#168885,#168886,#168887,#168888,#168889,#168890,#168891,#168892,#168893,
#168894,#168895,#168896,#168897,#168898,#168899,#168900,#168901,#168902,
#168903,#168904,#168905,#168906,#168907,#168908,#168909,#168910,#168911,
#168912,#168913,#168914,#168915,#168916,#168917,#168918,#168919,#168920,
#168921,#168922,#168923,#168924,#168925,#168926,#168927,#168928,#168929,
#168930,#168931,#168932,#168933,#168934,#168935,#168936,#168937,#168938,
#168939,#168940,#168941,#168942,#168943,#168944,#168945,#168946,#168947,
#168948,#168949,#168950,#168951,#168952,#168953,#168954,#168955,#168956,
#168957,#168958,#168959,#168960,#168961,#168962,#168963,#168964,#168965,
#168966,#168967,#168968,#168969,#168970,#168971,#168972,#168973,#168974,
#168975,#168976,#168977,#168978,#168979,#168980,#168981,#168982),
 .UNSPECIFIED.,.F.,.F.,(4,3,3,3,3,3,3,3,3,3,3,3,3,3,3,3,3,3,3,3,3,3,3,3,
3,3,3,3,3,3,3,3,3,3,3,3,3,3,3,3,3,3,3,3,3,3,3,3,3,3,3,3,3,3,3,3,3,3,3,3,
3,3,3,3,3,3,3,3,3,3,3,3,3,3,3,3,3,3,3,3,3,3,3,3,3,4),(229.336263712055,
229.411092925826,229.485870339396,229.560608562626,229.638548715104,229.713256024592,
229.787964681614,229.862686074969,229.937431598213,230.012243669549,230.087094611738,
230.162026109137,230.184129782449,230.260262654694,230.336302355765,230.412258361136,
230.488116803673,230.563917867227,230.639657187961,230.682598325757,230.75834069058,
230.834128811329,230.909971982171,230.985926940431,231.061943372765,231.138079168265,
231.181066869064,231.257277449538,231.33342005379,231.40950514013,231.485543126402,
231.561544396957,231.638601841798,231.714567103922,231.790528695787,231.866496022848,
231.944373006056,232.020402803488,232.099203379584,232.178003955679,232.249427230529,
232.320797357442,232.392127928964,232.46344126645,232.534741953272,232.606067434765,
232.676472498987,232.764177988327,232.852354350746,232.940958761363,233.029659068245,
233.11825532818,233.174941042295,233.247910486745,233.320834477839,233.393726004581,
233.466608203502,233.539483121546,233.612386071256,233.673409585602,233.752710369551,
233.832033300026,233.911375902035,233.990748979207,234.070130660204,234.149527437312,
234.17187812891,234.251275523579,234.330659197407,234.410026649048,234.489371832861,
234.568694852128,234.647989081749,234.670346672217,234.743249072485,234.816128929531,
234.888999198964,234.961895543369,235.034804199154,235.107772512102,235.168815215525,
235.257873628456,235.34826747615,235.437366543456,235.528407781346,235.619449019235),
 .UNSPECIFIED.);
#3209=B_SPLINE_CURVE_WITH_KNOTS('',3,(#168984,#168985,#168986,#168987,#168988,
#168989,#168990,#168991,#168992,#168993,#168994,#168995,#168996,#168997,
#168998,#168999,#169000,#169001),.UNSPECIFIED.,.F.,.F.,(4,2,2,2,2,2,2,2,
4),(235.619449019235,236.448806795673,237.278164572111,238.107522348549,
238.936880124987,239.766237901425,240.595595677862,241.4249534543,241.902634326414),
 .UNSPECIFIED.);
#3210=B_SPLINE_CURVE_WITH_KNOTS('',3,(#169003,#169004,#169005,#169006,#169007,
#169008,#169009,#169010,#169011,#169012,#169013,#169014,#169015,#169016,
#169017),.UNSPECIFIED.,.F.,.F.,(4,1,1,1,1,1,1,1,1,1,1,1,4),(241.902634326414,
242.147374821831,242.645843365138,243.144311908446,244.141248995061,244.639717538368,
245.138186081676,246.135123168291,246.633591711599,247.132060254906,247.630528798214,
248.128997341521,248.1858196054),.UNSPECIFIED.);
#3211=B_SPLINE_CURVE_WITH_KNOTS('',3,(#169019,#169020,#169021,#169022,#169023,
#169024,#169025,#169026,#169027,#169028,#169029,#169030,#169031,#169032,
#169033,#169034,#169035,#169036,#169037,#169038,#169039,#169040,#169041,
#169042,#169043,#169044,#169045,#169046,#169047,#169048,#169049,#169050,
#169051,#169052,#169053,#169054,#169055,#169056,#169057,#169058,#169059,
#169060,#169061,#169062,#169063,#169064,#169065,#169066,#169067,#169068,
#169069,#169070,#169071,#169072,#169073,#169074,#169075,#169076,#169077,
#169078,#169079,#169080,#169081,#169082,#169083,#169084,#169085,#169086,
#169087,#169088,#169089,#169090,#169091,#169092,#169093,#169094,#169095,
#169096,#169097,#169098,#169099,#169100,#169101,#169102,#169103,#169104,
#169105,#169106,#169107,#169108,#169109,#169110,#169111,#169112,#169113,
#169114,#169115,#169116,#169117,#169118,#169119,#169120,#169121,#169122,
#169123,#169124,#169125,#169126,#169127,#169128,#169129,#169130,#169131,
#169132,#169133,#169134,#169135,#169136,#169137,#169138,#169139,#169140,
#169141,#169142,#169143,#169144,#169145,#169146,#169147,#169148,#169149,
#169150,#169151,#169152,#169153,#169154,#169155,#169156,#169157,#169158,
#169159,#169160,#169161,#169162,#169163,#169164,#169165,#169166,#169167,
#169168,#169169,#169170,#169171,#169172,#169173,#169174,#169175,#169176,
#169177,#169178,#169179,#169180,#169181,#169182,#169183,#169184,#169185,
#169186,#169187,#169188,#169189,#169190,#169191,#169192,#169193,#169194,
#169195,#169196,#169197,#169198,#169199,#169200,#169201,#169202,#169203,
#169204,#169205,#169206,#169207,#169208,#169209,#169210,#169211,#169212,
#169213,#169214,#169215,#169216,#169217,#169218,#169219,#169220,#169221,
#169222,#169223,#169224,#169225,#169226,#169227,#169228,#169229,#169230,
#169231,#169232,#169233,#169234,#169235,#169236,#169237,#169238,#169239,
#169240,#169241,#169242,#169243,#169244,#169245,#169246,#169247,#169248,
#169249,#169250,#169251,#169252,#169253,#169254,#169255,#169256,#169257,
#169258,#169259,#169260,#169261,#169262,#169263,#169264,#169265,#169266,
#169267,#169268,#169269,#169270,#169271),.UNSPECIFIED.,.F.,.F.,(4,3,3,3,
3,3,3,3,3,3,3,3,3,3,3,3,3,3,3,3,3,3,3,3,3,3,3,3,3,3,3,3,3,3,3,3,3,3,3,3,
3,3,3,3,3,3,3,3,3,3,3,3,3,3,3,3,3,3,3,3,3,3,3,3,3,3,3,3,3,3,3,3,3,3,3,3,
3,3,3,3,3,3,3,3,4),(248.185819633594,248.265215616196,248.34459622705,248.423955987765,
248.503293808868,248.582602862825,248.627465884829,248.700368285098,248.773248142143,
248.846118411576,248.919014755981,248.991923411766,249.064891724714,249.125934428136,
249.214508759749,249.303209125222,249.391775937325,249.48011935089,249.567889067515,
249.624402971444,249.695726469794,249.76703021995,249.838327723222,249.909660218868,
249.981008577608,250.052429232575,250.122871514752,250.198975010773,250.275028156844,
250.351041347079,250.427024946959,250.502989300287,250.580091712922,250.656063440961,
250.73204776822,250.808054109892,250.885992732761,250.962101772189,251.040955186778,
251.119808601367,251.195941473612,251.271981174683,251.347937180054,251.423795622591,
251.499596686144,251.575336006878,251.618277144674,251.694019509497,251.769807630246,
251.845650801089,251.921605759348,251.997622191683,252.073757987183,252.116745687982,
252.192956268456,252.269098872708,252.345183959048,252.42122194532,252.497223215875,
252.574280660715,252.65024592284,252.726207514705,252.802174841766,252.880051824974,
252.956081622406,253.034882198502,253.113682774597,253.185106049447,253.25647617636,
253.327806747881,253.399120085367,253.470420772189,253.541746253681,253.612151317904,
253.699856807244,253.788033169662,253.876637580279,253.965337887162,254.053934147096,
254.110619861212,254.183367085814,254.256062969947,254.328728085723,254.401385195274,
254.469004940773),.UNSPECIFIED.);
#3212=B_SPLINE_CURVE_WITH_KNOTS('',3,(#169273,#169274,#169275,#169276,#169277,
#169278,#169279,#169280,#169281,#169282,#169283,#169284,#169285,#169286,
#169287,#169288,#169289,#169290),.UNSPECIFIED.,.F.,.F.,(4,2,2,2,2,2,2,2,
4),(254.469004940773,255.298362717211,256.127720493649,256.957078270087,
257.786436046525,258.615793822963,259.445151599401,260.274509375839,260.752190247953),
 .UNSPECIFIED.);
#3213=B_SPLINE_CURVE_WITH_KNOTS('',3,(#169292,#169293,#169294,#169295,#169296,
#169297,#169298,#169299,#169300,#169301,#169302,#169303,#169304,#169305,
#169306,#169307,#169308,#169309,#169310,#169311,#169312,#169313,#169314,
#169315,#169316,#169317,#169318,#169319,#169320,#169321,#169322,#169323,
#169324,#169325,#169326,#169327,#169328,#169329,#169330,#169331,#169332,
#169333,#169334,#169335,#169336,#169337,#169338,#169339,#169340,#169341,
#169342,#169343,#169344,#169345,#169346,#169347,#169348,#169349,#169350,
#169351,#169352,#169353,#169354,#169355,#169356,#169357,#169358,#169359,
#169360,#169361,#169362,#169363,#169364,#169365,#169366,#169367,#169368,
#169369,#169370,#169371,#169372,#169373,#169374,#169375,#169376,#169377,
#169378,#169379,#169380,#169381,#169382,#169383,#169384,#169385,#169386,
#169387,#169388,#169389,#169390,#169391,#169392,#169393,#169394,#169395,
#169396,#169397,#169398,#169399,#169400,#169401,#169402,#169403,#169404,
#169405,#169406,#169407,#169408,#169409,#169410,#169411,#169412,#169413,
#169414,#169415,#169416,#169417,#169418,#169419,#169420,#169421,#169422,
#169423,#169424,#169425,#169426,#169427,#169428,#169429,#169430,#169431,
#169432,#169433,#169434,#169435,#169436,#169437,#169438,#169439,#169440,
#169441,#169442,#169443,#169444,#169445,#169446,#169447,#169448,#169449,
#169450,#169451,#169452,#169453,#169454,#169455,#169456,#169457,#169458,
#169459,#169460,#169461,#169462,#169463,#169464,#169465,#169466,#169467,
#169468,#169469,#169470,#169471,#169472,#169473,#169474,#169475,#169476,
#169477,#169478,#169479,#169480,#169481,#169482,#169483,#169484,#169485,
#169486,#169487,#169488,#169489,#169490,#169491,#169492,#169493,#169494,
#169495,#169496,#169497,#169498,#169499,#169500,#169501,#169502,#169503,
#169504,#169505,#169506,#169507,#169508,#169509,#169510,#169511,#169512,
#169513,#169514,#169515,#169516,#169517,#169518,#169519,#169520,#169521,
#169522,#169523,#169524,#169525,#169526,#169527,#169528,#169529,#169530,
#169531,#169532,#169533,#169534,#169535,#169536,#169537,#169538,#169539,
#169540,#169541,#169542,#169543,#169544,#169545,#169546,#169547,#169548,
#169549,#169550,#169551,#169552,#169553,#169554,#169555,#169556,#169557,
#169558,#169559,#169560,#169561,#169562,#169563,#169564,#169565,#169566,
#169567,#169568,#169569,#169570,#169571,#169572,#169573,#169574,#169575,
#169576,#169577,#169578,#169579,#169580,#169581,#169582,#169583,#169584,
#169585,#169586,#169587,#169588,#169589,#169590,#169591,#169592,#169593,
#169594,#169595,#169596,#169597,#169598,#169599,#169600,#169601,#169602,
#169603,#169604,#169605,#169606,#169607,#169608,#169609,#169610,#169611,
#169612,#169613,#169614,#169615,#169616,#169617,#169618,#169619,#169620,
#169621,#169622,#169623,#169624,#169625,#169626,#169627,#169628,#169629,
#169630,#169631,#169632,#169633,#169634,#169635,#169636,#169637,#169638,
#169639,#169640,#169641,#169642,#169643,#169644,#169645,#169646,#169647,
#169648,#169649,#169650,#169651,#169652,#169653,#169654,#169655,#169656,
#169657,#169658,#169659,#169660,#169661,#169662,#169663,#169664,#169665,
#169666,#169667,#169668,#169669,#169670,#169671,#169672,#169673,#169674,
#169675,#169676,#169677,#169678,#169679,#169680,#169681,#169682,#169683,
#169684,#169685,#169686,#169687,#169688,#169689,#169690,#169691,#169692,
#169693,#169694,#169695,#169696,#169697,#169698,#169699,#169700,#169701,
#169702,#169703,#169704,#169705,#169706,#169707,#169708,#169709,#169710,
#169711,#169712,#169713,#169714,#169715,#169716,#169717,#169718,#169719,
#169720,#169721,#169722,#169723,#169724,#169725,#169726,#169727,#169728,
#169729,#169730,#169731,#169732,#169733,#169734,#169735,#169736,#169737,
#169738,#169739,#169740,#169741,#169742,#169743,#169744,#169745,#169746,
#169747,#169748,#169749,#169750,#169751,#169752,#169753,#169754,#169755,
#169756,#169757,#169758,#169759,#169760,#169761,#169762,#169763,#169764,
#169765,#169766,#169767,#169768,#169769,#169770,#169771,#169772,#169773,
#169774,#169775,#169776,#169777,#169778,#169779,#169780,#169781,#169782,
#169783,#169784,#169785,#169786,#169787,#169788,#169789,#169790,#169791,
#169792,#169793,#169794,#169795,#169796,#169797,#169798,#169799,#169800,
#169801,#169802,#169803,#169804,#169805,#169806,#169807,#169808,#169809,
#169810,#169811,#169812,#169813,#169814,#169815,#169816,#169817,#169818,
#169819,#169820,#169821,#169822,#169823,#169824,#169825,#169826,#169827,
#169828,#169829,#169830,#169831,#169832,#169833,#169834,#169835,#169836,
#169837,#169838,#169839,#169840,#169841,#169842,#169843,#169844,#169845,
#169846,#169847,#169848,#169849,#169850,#169851,#169852,#169853,#169854,
#169855,#169856,#169857,#169858,#169859,#169860,#169861,#169862,#169863,
#169864,#169865,#169866,#169867,#169868,#169869,#169870,#169871,#169872,
#169873,#169874,#169875,#169876,#169877,#169878,#169879,#169880,#169881,
#169882,#169883,#169884,#169885,#169886,#169887,#169888,#169889,#169890,
#169891,#169892,#169893,#169894,#169895,#169896,#169897,#169898,#169899,
#169900,#169901,#169902,#169903,#169904,#169905,#169906,#169907,#169908,
#169909,#169910,#169911,#169912,#169913,#169914,#169915,#169916,#169917,
#169918,#169919,#169920,#169921,#169922,#169923,#169924,#169925,#169926,
#169927,#169928,#169929,#169930,#169931,#169932,#169933,#169934,#169935,
#169936,#169937,#169938,#169939,#169940,#169941,#169942,#169943,#169944,
#169945,#169946,#169947,#169948,#169949,#169950,#169951,#169952,#169953,
#169954,#169955,#169956,#169957,#169958,#169959,#169960,#169961,#169962,
#169963,#169964,#169965,#169966,#169967,#169968,#169969,#169970,#169971,
#169972,#169973,#169974,#169975,#169976,#169977,#169978,#169979,#169980,
#169981,#169982,#169983,#169984,#169985,#169986,#169987,#169988,#169989,
#169990,#169991,#169992,#169993,#169994,#169995,#169996,#169997,#169998,
#169999,#170000,#170001,#170002,#170003,#170004,#170005,#170006,#170007,
#170008,#170009,#170010,#170011,#170012,#170013,#170014,#170015,#170016,
#170017,#170018,#170019,#170020,#170021,#170022,#170023,#170024,#170025,
#170026,#170027,#170028,#170029,#170030,#170031,#170032,#170033,#170034,
#170035,#170036,#170037,#170038,#170039,#170040,#170041,#170042,#170043,
#170044,#170045,#170046,#170047,#170048,#170049,#170050,#170051,#170052,
#170053,#170054,#170055,#170056,#170057),.UNSPECIFIED.,.F.,.F.,(4,2,2,2,
2,2,2,2,2,2,2,2,2,2,2,2,2,2,2,2,2,2,2,2,2,2,2,2,2,2,2,2,2,2,2,2,2,2,2,2,
2,2,2,2,2,2,2,2,2,2,2,2,2,2,2,2,2,2,2,2,2,2,2,2,2,2,2,2,2,2,2,2,2,2,2,2,
2,2,2,2,2,2,2,2,2,2,2,2,2,2,2,2,2,2,2,2,2,2,2,2,2,2,2,2,2,2,2,2,2,2,2,2,
2,2,2,2,2,2,2,2,2,2,2,2,2,2,2,2,2,2,2,2,2,2,2,2,2,2,2,2,2,2,2,2,2,2,2,2,
2,2,2,2,2,2,2,2,2,2,2,2,2,2,2,2,2,2,2,2,2,2,2,2,2,2,2,2,2,2,2,2,2,2,2,2,
2,2,2,2,2,2,2,2,2,2,2,2,2,2,2,2,2,2,2,2,2,2,2,2,2,2,2,2,2,2,2,2,2,2,2,2,
2,2,2,2,2,2,2,2,2,2,2,2,2,2,2,2,2,2,2,2,2,2,2,2,2,2,2,2,2,2,2,2,2,2,2,2,
2,2,2,2,2,2,2,2,2,2,2,2,2,2,2,2,2,2,2,2,2,2,2,2,2,2,2,2,2,2,2,2,2,2,2,2,
2,2,2,2,2,2,2,2,2,2,2,2,2,2,2,2,2,2,2,2,2,2,2,2,2,2,2,2,2,2,2,2,2,2,2,2,
2,2,2,2,2,2,2,2,2,2,2,2,2,2,2,2,2,2,2,2,2,2,2,2,2,2,2,2,2,2,2,2,2,2,2,2,
2,2,2,2,2,2,2,2,2,2,2,2,2,2,2,2,2,2,4),(0.00175515510389137,0.233477217887913,
0.25413703343595,0.26458559800326,0.271154459994723,0.276282396962432,0.281849533512794,
0.288901966614316,0.300280715426606,0.357262708118248,0.415603903548912,
0.45085908282636,0.465215104594165,0.475293962475098,0.486357255560859,
0.503385792319506,0.564701835533945,0.6398356464392,0.661581926413047,0.672185324833179,
0.678797981477316,0.684240763060695,0.690212940547745,0.697982880634005,
0.71123025721564,0.791283504926808,0.866715769811109,0.914874922190495,
0.935584029401951,0.951600003526206,0.968969172068741,1.00932986584437,
1.06420270912661,1.06459270061813,1.06497063122061,1.06533745121251,1.06569402661649,
1.06604114927938,1.0663795455561,1.06670988380967,1.0670327809382,1.06734880806243,
1.0676584955139,1.06796233720735,1.06826079452005,1.06855429971448,1.06884325898597,
1.06912805519464,1.06940905029064,1.06968658751496,1.06996099338418,1.07023257948723,
1.07050164412487,1.07076847380039,1.07103334460418,1.07129652347151,1.07155826937261,
1.07181883440759,1.0720784648375,1.072337402053,1.0725958834945,1.07285414354116,
1.07311241434677,1.07337092666556,1.07362991063493,1.07388959655672,1.07415021567128,
1.07441200091583,1.07467518767515,1.07494001454384,1.07520672410221,1.07547556369038,
1.07574678619495,1.07602065087022,1.07629742416933,1.07657738060112,1.07686080361825,
1.08781962073341,1.10197716490331,1.15002880852661,1.18625581917963,1.21257682033107,
1.22824407953828,1.2449993049137,1.27056306991027,1.39867339113269,1.44524476935404,
1.46333843076665,1.47584638964651,1.47585815312406,1.47586991439948,1.47588167353886,
1.47589343053064,1.47590518543313,1.47591693828364,1.47592868900168,1.47594043759191,
1.47595218416309,1.4759639286548,1.47597567104591,1.47598741141739,1.47599914969255,
1.47601088592738,1.47602262012269,1.4760343523083,1.47604608250151,1.47605781074983,
1.4760695369906,1.47608126127869,1.47609298362109,1.47610470397389,1.47611642236231,
1.47612813880026,1.47613985331399,1.47615156591528,1.47616327665493,1.47617498546208,
1.47618669242915,1.4761983974872,1.47621010062884,1.47622180192393,1.47623350133894,
1.47624519889774,1.47625689464955,1.4762685885908,1.47628028073621,1.47629197106438,
1.47630365961983,1.47631534644594,1.4763270314473,1.47633871472641,1.47635039624674,
1.4763620760455,1.4763737541165,1.47638543049538,1.47639710516244,1.47640877814654,
1.47642044938156,1.47643211898983,1.47644378683111,1.47645545303301,1.47646711759522,
1.47647878053287,1.47649044188986,1.47650210161836,1.47651375972637,1.47652541618465,
1.47653707105855,1.47654872438652,1.4765603761387,1.47657202634678,1.47658367504197,
1.47659532223396,1.47660696788615,1.48257240671224,1.48855891242022,1.49511239671956,
1.50801037252183,1.5634835740125,1.61004197639941,1.63133733756868,1.67389501185857,
1.6892645502926,1.69922365512451,1.70935745468947,1.72436020873488,1.76382280958394,
1.84609078677853,1.86825711214699,1.8791488358587,1.88678270785041,1.89214181958446,
1.89712855586481,1.90401414228836,1.91933549196333,2.05051976628145,2.14045537791271,
2.17604001437676,2.19540302882133,2.20835915391724,2.22074635752232,2.22078260957332,
2.22081900314508,2.2208555396054,2.23176488230404,2.24609451722107,2.2761792622228,
2.37728760371622,2.58709277620618,2.67603376760491,2.68311216447253,2.68614184150776,
2.68834541786443,2.69036122329734,2.69306796494391,2.69959586351883,2.8055016929206,
2.95583583270476,3.10677991989484,3.11521508027641,3.11908303531526,3.12200068954504,
3.12474623967715,3.12855228198413,3.13624469868799,3.2088398194217,3.25521222803167,
3.45867078089983,3.48681670119209,3.5286285783174,3.5376978331576,3.54113789529451,
3.54349635396022,3.54579847973153,3.54856463728212,3.55542538286991,3.62938312966554,
3.87440341521721,3.90644803481321,3.91712992632398,3.92414739352503,3.93073506575537,
3.93905435529049,3.95533569309754,4.12316938130341,4.16704554026442,4.28491574368914,
4.30007338439049,4.30424803637416,4.3067675632827,4.30902613948356,4.31188890947859,
4.31766152280319,4.35811393803448,4.37097403415593,4.39865388396153,4.62303097563096,
4.71566436585532,4.72362076631482,4.72739693827814,4.73030072319465,4.73307492052381,
4.73778090938272,4.75040116928648,4.9593422547546,5.07893771558406,5.11367129404802,
5.15331585190229,5.15884497898514,5.16158380561712,5.16374311567003,5.16615037184357,
5.17013544370944,5.18456712682551,5.29649760092421,5.4431241269617,5.56966840778963,
5.60322224863298,5.61799147295701,5.6293651187069,5.64173231640786,5.661854789329,
5.74119636823205,5.83015418058168,5.93016731041987,5.94650556636355,5.95349327340243,
5.95903657991471,5.96567826631202,5.97819338784467,6.02544957701399,6.11361693750067,
6.13528811288873,6.14749318726828,6.15801978640242,6.17109926704762,6.19793600523263,
6.21794073482931,6.29117843336744,6.34759750657495,6.35777166329348,6.36328461872042,
6.36938176163861,6.37801321498269,6.40023911392053,6.48552621733961,6.53204991383895,
6.58885642938433,6.60888601772983,6.62546853419877,6.64338734369971,6.67767451557907,
6.73366769184109,6.75393387992771,6.76519738058678,6.77890519915598,6.82326897067486,
6.87933026136105,6.89906914405145,6.91385486732147,6.93375865598872,6.97628364780968,
7.00961022733493,7.07042720479597,7.07740954194317,7.0969449960031,7.1454868082527,
7.15679494648413,7.16345505888059,7.16937602255614,7.17759268574359,7.20239410292237,
7.24833049987884,7.34187808713147,7.3622144920666,7.37404282418338,7.38356079744233,
7.39665914385762,7.4237882756603,7.46202336420416,7.53433530408394,7.55809713228422,
7.56590552075492,7.57130756773959,7.57691744331908,7.58506318876277,7.60862790139616,
7.62979070396718,7.72361099869899,7.79631111824225,7.86697847717529,7.88678330214175,
7.89901298487519,7.91010975546727,7.92461905636662,7.95571488185342,8.09650862064676,
8.33256820221607,8.3573507268996,8.36189061219046,8.36469692759916,8.36686475342219,
8.36923646362575,8.37306162192178,8.3859218083503,8.46890109816707,8.64294715347879,
8.78291563982107,8.79256563867432,8.79634738452495,8.79908644324316,8.80200747254907,
8.80589738368821,8.81420847091793,8.88890657519997,9.00435405993594,9.20295840426713,
9.21477221130106,9.21873385251936,9.22095787865279,9.22319013651098,9.2259944467728,
9.23148175640772,9.26993303922492,9.33011201574586,9.46706674441134,9.57459592702731,
9.59026327815184,9.59843681238614,9.6047593279856,9.61172843283533,9.62218051806888,
9.65239298224312,9.86570930835225,9.97338547415581,9.98039934692653,9.98319056743156,
9.98549922691861,9.9878498695486,9.99125223818228,10.0000748706393,10.0399943403384,
10.2253631395449),.UNSPECIFIED.);
#3214=B_SPLINE_CURVE_WITH_KNOTS('',3,(#170059,#170060,#170061,#170062,#170063,
#170064,#170065,#170066,#170067,#170068,#170069,#170070,#170071,#170072,
#170073),.UNSPECIFIED.,.F.,.F.,(4,1,1,1,1,1,1,1,1,1,1,1,4),(273.318560862312,
274.049361593514,274.547830136822,275.046298680129,275.544767223437,276.043235766745,
276.541704310052,277.04017285336,277.538641396667,278.037109939975,279.03404702659,
279.532515569897,279.601746169492),.UNSPECIFIED.);
#3215=B_SPLINE_CURVE_WITH_KNOTS('',3,(#170075,#170076,#170077,#170078,#170079,
#170080,#170081,#170082,#170083,#170084,#170085,#170086,#170087,#170088),
 .UNSPECIFIED.,.F.,.F.,(4,1,1,1,1,1,1,1,1,1,1,4),(279.601746169492,280.030984113205,
281.02792119982,281.526389743128,282.024858286435,282.523326829743,283.02179537305,
283.520263916358,284.018732459666,284.517201002973,285.015669546281,285.884931476671),
 .UNSPECIFIED.);
#3216=B_SPLINE_CURVE_WITH_KNOTS('',3,(#170090,#170091,#170092,#170093,#170094,
#170095,#170096,#170097,#170098,#170099,#170100,#170101,#170102,#170103,
#170104,#170105),.UNSPECIFIED.,.F.,.F.,(4,1,1,1,1,1,1,1,1,1,1,1,1,4),(285.884931476671,
286.012606632896,286.511075176203,287.009543719511,288.006480806126,288.504949349434,
289.003417892741,289.501886436049,290.000354979356,290.498823522664,290.997292065971,
291.495760609279,291.994229152586,292.168116783851),.UNSPECIFIED.);
#3217=B_SPLINE_CURVE_WITH_KNOTS('',3,(#170107,#170108,#170109,#170110,#170111,
#170112,#170113,#170114,#170115,#170116,#170117,#170118,#170119,#170120,
#170121,#170122,#170123,#170124,#170125,#170126,#170127,#170128,#170129,
#170130,#170131,#170132,#170133,#170134,#170135,#170136,#170137,#170138,
#170139,#170140,#170141,#170142,#170143,#170144,#170145,#170146,#170147,
#170148,#170149,#170150,#170151,#170152,#170153,#170154,#170155,#170156,
#170157,#170158,#170159,#170160,#170161,#170162,#170163,#170164,#170165,
#170166,#170167,#170168,#170169,#170170,#170171,#170172,#170173,#170174,
#170175,#170176,#170177,#170178,#170179,#170180,#170181,#170182,#170183,
#170184,#170185,#170186,#170187,#170188,#170189,#170190,#170191,#170192,
#170193,#170194,#170195,#170196,#170197,#170198,#170199,#170200,#170201,
#170202,#170203,#170204,#170205,#170206,#170207,#170208,#170209,#170210,
#170211,#170212,#170213,#170214,#170215,#170216,#170217,#170218,#170219,
#170220,#170221,#170222,#170223,#170224,#170225,#170226,#170227,#170228,
#170229,#170230,#170231,#170232,#170233,#170234,#170235,#170236,#170237,
#170238,#170239,#170240,#170241,#170242,#170243,#170244,#170245,#170246,
#170247,#170248,#170249,#170250,#170251,#170252,#170253,#170254,#170255,
#170256,#170257,#170258,#170259,#170260,#170261,#170262,#170263,#170264,
#170265,#170266,#170267,#170268,#170269,#170270,#170271,#170272,#170273,
#170274,#170275,#170276,#170277,#170278,#170279,#170280,#170281,#170282,
#170283,#170284,#170285,#170286,#170287,#170288,#170289,#170290,#170291,
#170292,#170293,#170294,#170295,#170296,#170297,#170298,#170299,#170300,
#170301,#170302,#170303,#170304,#170305,#170306,#170307,#170308,#170309,
#170310,#170311,#170312,#170313,#170314,#170315,#170316,#170317,#170318,
#170319,#170320,#170321,#170322,#170323,#170324,#170325,#170326,#170327,
#170328,#170329,#170330,#170331,#170332,#170333,#170334,#170335,#170336,
#170337,#170338,#170339,#170340,#170341,#170342,#170343,#170344,#170345,
#170346,#170347,#170348,#170349,#170350,#170351,#170352,#170353,#170354,
#170355,#170356,#170357,#170358,#170359,#170360,#170361,#170362),
 .UNSPECIFIED.,.F.,.F.,(4,3,3,3,3,3,3,3,3,3,3,3,3,3,3,3,3,3,3,3,3,3,3,3,
3,3,3,3,3,3,3,3,3,3,3,3,3,3,3,3,3,3,3,3,3,3,3,3,3,3,3,3,3,3,3,3,3,3,3,3,
3,3,3,3,3,3,3,3,3,3,3,3,3,3,3,3,3,3,3,3,3,3,3,3,3,4),(292.168116783851,
292.242892619617,292.317620259225,292.392312354933,292.467169090467,292.541838664995,
292.616512565346,292.691202226417,292.766193229613,292.840977674388,292.916071956795,
292.991166239202,293.067299111447,293.143338812519,293.21929481789,293.295153260427,
293.370954323981,293.446693644715,293.489634782509,293.565377147332,293.641165268081,
293.717008438923,293.792963397183,293.868979829517,293.945115625018,293.988103325817,
294.064313906291,294.140456510543,294.216541596883,294.292579583156,294.368580853711,
294.445638298551,294.521603560676,294.59756515254,294.673532479602,294.751409462809,
294.827439260242,294.906239836337,294.985040412432,295.056463687282,295.127833814195,
295.199164385717,295.270477723203,295.341778410025,295.413103891517,295.483508955739,
295.571214445079,295.659390807497,295.747995218113,295.836695524995,295.92529178493,
295.981977499047,296.054946943497,296.127870934591,296.200762461333,296.273644660254,
296.346519578297,296.419422528008,296.480446042354,296.559746826303,296.63906975678,
296.71841235879,296.797785435963,296.87716711696,296.956563894069,296.978914585662,
297.058311980331,297.13769565416,297.217063105802,297.296408289614,297.37573130888,
297.455025538502,297.47738312897,297.550285529238,297.623165386283,297.696035655715,
297.76893200012,297.841840655905,297.914808968853,297.975851672277,298.064621143056,
298.153528187369,298.242313953431,298.330875461396,298.418895475305,298.45130209103),
 .UNSPECIFIED.);
#3218=B_SPLINE_CURVE_WITH_KNOTS('',3,(#170364,#170365,#170366,#170367,#170368,
#170369,#170370,#170371,#170372,#170373,#170374,#170375,#170376,#170377,
#170378,#170379,#170380,#170381,#170382,#170383,#170384,#170385,#170386,
#170387,#170388,#170389,#170390,#170391,#170392,#170393,#170394,#170395,
#170396,#170397,#170398,#170399,#170400,#170401,#170402,#170403,#170404,
#170405,#170406,#170407,#170408,#170409,#170410,#170411,#170412,#170413,
#170414,#170415,#170416,#170417,#170418,#170419,#170420,#170421,#170422,
#170423,#170424,#170425,#170426,#170427,#170428,#170429,#170430,#170431,
#170432,#170433,#170434,#170435,#170436,#170437,#170438,#170439,#170440,
#170441,#170442,#170443,#170444,#170445,#170446,#170447,#170448,#170449,
#170450,#170451,#170452,#170453,#170454,#170455,#170456,#170457,#170458,
#170459,#170460,#170461,#170462,#170463,#170464,#170465,#170466,#170467,
#170468,#170469,#170470,#170471,#170472,#170473,#170474,#170475,#170476,
#170477,#170478,#170479,#170480,#170481,#170482,#170483,#170484,#170485,
#170486,#170487,#170488,#170489,#170490,#170491,#170492,#170493,#170494,
#170495,#170496,#170497,#170498,#170499,#170500,#170501,#170502,#170503,
#170504,#170505,#170506,#170507,#170508,#170509,#170510,#170511,#170512,
#170513,#170514,#170515,#170516,#170517,#170518,#170519,#170520,#170521,
#170522,#170523,#170524,#170525,#170526,#170527,#170528,#170529,#170530,
#170531,#170532,#170533,#170534,#170535,#170536,#170537,#170538,#170539,
#170540,#170541,#170542,#170543,#170544,#170545,#170546,#170547,#170548,
#170549,#170550,#170551,#170552,#170553,#170554,#170555,#170556,#170557,
#170558,#170559,#170560,#170561,#170562,#170563,#170564,#170565,#170566,
#170567,#170568,#170569,#170570,#170571,#170572,#170573,#170574,#170575,
#170576,#170577,#170578,#170579,#170580,#170581,#170582,#170583,#170584,
#170585,#170586,#170587,#170588,#170589,#170590,#170591,#170592,#170593,
#170594,#170595,#170596,#170597,#170598,#170599,#170600,#170601,#170602,
#170603,#170604,#170605,#170606,#170607,#170608,#170609,#170610,#170611,
#170612,#170613,#170614,#170615,#170616,#170617,#170618,#170619,#170620,
#170621,#170622,#170623,#170624,#170625,#170626,#170627,#170628,#170629,
#170630,#170631,#170632,#170633,#170634,#170635,#170636,#170637,#170638,
#170639,#170640,#170641,#170642,#170643,#170644,#170645,#170646,#170647,
#170648,#170649,#170650,#170651,#170652,#170653,#170654,#170655,#170656,
#170657,#170658,#170659,#170660,#170661,#170662,#170663,#170664,#170665,
#170666,#170667,#170668,#170669,#170670,#170671,#170672,#170673,#170674,
#170675,#170676,#170677,#170678,#170679,#170680,#170681,#170682,#170683,
#170684,#170685,#170686,#170687,#170688,#170689,#170690,#170691,#170692,
#170693,#170694,#170695,#170696,#170697,#170698,#170699,#170700,#170701,
#170702,#170703,#170704,#170705,#170706,#170707,#170708,#170709,#170710,
#170711,#170712,#170713,#170714,#170715,#170716,#170717,#170718,#170719,
#170720,#170721,#170722,#170723,#170724,#170725,#170726,#170727,#170728,
#170729,#170730,#170731,#170732,#170733,#170734,#170735,#170736,#170737,
#170738,#170739,#170740,#170741,#170742,#170743,#170744,#170745,#170746,
#170747,#170748,#170749,#170750,#170751,#170752,#170753,#170754,#170755,
#170756,#170757,#170758,#170759,#170760,#170761,#170762,#170763,#170764,
#170765,#170766,#170767,#170768,#170769,#170770,#170771,#170772,#170773,
#170774,#170775,#170776,#170777,#170778,#170779,#170780,#170781,#170782,
#170783,#170784,#170785,#170786,#170787,#170788,#170789,#170790,#170791,
#170792,#170793,#170794,#170795,#170796,#170797,#170798,#170799,#170800,
#170801,#170802,#170803,#170804,#170805,#170806,#170807,#170808,#170809,
#170810,#170811,#170812,#170813,#170814,#170815,#170816,#170817,#170818,
#170819,#170820,#170821,#170822,#170823,#170824,#170825,#170826,#170827,
#170828,#170829,#170830,#170831,#170832,#170833,#170834,#170835,#170836,
#170837,#170838,#170839,#170840,#170841,#170842,#170843,#170844,#170845,
#170846,#170847,#170848,#170849,#170850,#170851,#170852,#170853,#170854,
#170855,#170856,#170857,#170858,#170859,#170860,#170861,#170862,#170863,
#170864,#170865,#170866,#170867,#170868,#170869,#170870,#170871,#170872,
#170873,#170874,#170875,#170876,#170877,#170878,#170879,#170880,#170881,
#170882,#170883,#170884,#170885,#170886,#170887,#170888,#170889,#170890,
#170891,#170892,#170893,#170894,#170895,#170896,#170897),.UNSPECIFIED.,
 .F.,.F.,(4,2,2,2,2,2,2,2,2,2,2,2,2,2,2,2,2,2,2,2,2,2,2,2,2,2,2,2,2,2,2,
2,2,2,2,2,2,2,2,2,2,2,2,2,2,2,2,2,2,2,2,2,2,2,2,2,2,2,2,2,2,2,2,2,2,2,2,
2,2,2,2,2,2,2,2,2,2,2,2,2,2,2,2,2,2,2,2,2,2,2,2,2,2,2,2,2,2,2,2,2,2,2,2,
2,2,2,2,2,2,2,2,2,2,2,2,2,2,2,2,2,2,2,2,2,2,2,2,2,2,2,2,2,2,2,2,2,2,2,2,
2,2,2,2,2,2,2,2,2,2,2,2,2,2,2,2,2,2,2,2,2,2,2,2,2,2,2,2,2,2,2,2,2,2,2,2,
2,2,2,2,2,2,2,2,2,2,2,2,2,2,2,2,2,2,2,2,2,2,2,2,2,2,2,2,2,2,2,2,2,2,2,2,
2,2,2,2,2,2,2,2,2,2,2,2,2,2,2,2,2,2,2,2,2,2,2,2,2,2,2,2,2,2,2,2,2,2,2,2,
2,2,2,2,2,2,2,2,2,2,2,2,2,2,2,2,2,2,2,4),(0.00122791027254725,0.0770820827091792,
0.249473293479002,0.35938565459511,0.396222145161444,0.401470223157442,
0.404151400110561,0.406285224019235,0.408410814910348,0.412196213564084,
0.423475551746603,0.602149485012172,0.659425583079787,0.677777713760731,
0.704614520043833,0.823643580796911,0.832382970895941,0.836307131751904,
0.83923348903228,0.841962843712299,0.845708201067346,0.855144521174502,
0.979824151879159,1.05588477287752,1.17520667966232,1.24210984092913,1.25397834072015,
1.25779707324021,1.26023699649726,1.2625174720715,1.26549224401887,1.27048069588069,
1.30077755015236,1.42946571425106,1.53656613983677,1.58858242833206,1.610956029209,
1.62309297067942,1.63366928033205,1.64056720086361,1.64673459641745,1.65473566225044,
1.66678353740102,1.72157774112728,1.76395016251119,1.91948843800925,2.0043737721778,
2.0171235096307,2.02104482676514,2.02350753158127,2.0257799452495,2.02870241098462,
2.03493914970703,2.09505126887309,2.14929829547459,2.27094440408111,2.43123907130445,
2.43970363795816,2.44357682189537,2.44649501217603,2.4492385319426,2.4530377241848,
2.46279293163981,2.61559574606392,2.79152728449851,2.86112861009212,2.87285807117308,
2.87655489027948,2.87889784844497,2.88107441616306,2.88389483183564,2.88858367266565,
2.91600477782473,3.07519780857927,3.2838046531056,3.31901744763817,3.33421568568152,
3.34561465457157,3.35790744572186,3.37768042746172,3.44354325987826,3.58315168023071,
3.63171911978052,3.65040882157333,3.66426321037291,3.67088300815463,3.67645076278207,
3.68350732620053,3.69489996863144,3.7510813816026,3.80996282193589,3.84539816707146,
3.85977915942087,3.87045071776729,3.88053485765473,3.89781657101398,3.95876325979922,
4.03434661989895,4.0665096349813,4.07543900336064,4.081416536214,4.08708021207258,
4.09505547764317,4.11715568455006,4.24506756066764,4.30569274491526,4.32786694565951,
4.34438577868516,4.36313385068249,4.42998159343901,4.46793891923492,4.48120285085966,
4.49455810178358,4.55445365760738,4.58542587726186,4.60946657218916,4.62613071232053,
4.64427836545532,4.67623618368438,4.70663472748092,4.7373624594192,4.81561241655197,
4.84025709922769,4.86642423927287,4.87558460205099,4.88178618611138,4.88720679323757,
4.89660711334873,4.93103608333354,5.02615194728681,5.05482932556069,5.07725386175143,
5.08950182858655,5.10002505632894,5.11305050546241,5.13976166004577,5.1771318085889,
5.22058818729292,5.27139924944099,5.28168312523945,5.28725146017345,5.2922596135758,
5.29944319754572,5.31648707991604,5.34102676807479,5.46085939185313,5.57978880817953,
5.60179261053654,5.61468668116615,5.62595418018708,5.64003114539705,5.66872970313352,
5.788362176433,5.95823962779432,6.05306548968299,6.0741849720216,6.07848847249037,
6.08122261170812,6.0833814236841,6.08579146829691,6.0897887433754,6.10433480837078,
6.21618231086416,6.42404036705696,6.5010029633691,6.50968361712007,6.51320547988452,
6.51614647868682,6.51916762023086,6.52358833811566,6.53531831464861,6.59141922782749,
6.71389724819145,6.91950030055133,6.93115959405315,6.93510073760973,6.93732040167437,
6.93955303450742,6.94236501532933,6.94789084758862,6.98756279271893,7.05058094010175,
7.2790725721291,7.30276588050363,7.31157743500253,7.31787243245515,7.32376954551401,
7.3314900735133,7.34542178253661,7.42027116082209,7.51692417093367,7.67635742431983,
7.69356773735894,7.69808839982265,7.70071146794937,7.70295843532122,7.70567442477478,
7.70853673660549,7.71300050279924,7.72136320684039,7.79747418562558,7.93128789258829,
8.10604481814092,8.11631022754147,8.1201927066759,8.12295826933843,8.12586521562977,
8.12966567965862,8.13774893473,8.24094238431121,8.40820621626666,8.54261131083952,
8.55114852540975,8.55452114093056,8.55656512754395,8.55874796400886,8.56165906580973,
8.5680802936016,8.5767049402225,8.6679032131965,8.76219829244233,8.95939214377268,
8.99508448427386,9.00924348783601,9.02080950713053,9.03134619390067,9.04662060841632,
9.08202327295041,9.13336157038587,9.22333375485016,9.32338677381066,9.33966071708891,
9.34627494337092,9.35185710994299,9.35716155295603,9.36486048767306,9.3751531169544,
9.39546283920925,9.46184059702045,9.51748793901424,9.53378365225853,9.544685548757,
9.55456395319087,9.56512369349176,9.59237362292246,9.61281862834854,9.70805983410475,
9.742769081438,9.7521998228333,9.7576230284564,9.7632589780941,9.76944815665706,
9.77803153874953,9.79275870214336,9.82617109120628,9.90426362675867,9.97874077013341,
10.0026568325412,10.019234100866,10.0339356097584,10.0621071748144,10.1037487198327,
10.1424488115996,10.1567160209096,10.1677229097695,10.1830828621877,10.2246332076101),
 .UNSPECIFIED.);
#3219=B_SPLINE_CURVE_WITH_KNOTS('',3,(#170899,#170900,#170901,#170902,#170903,
#170904,#170905,#170906,#170907,#170908,#170909,#170910,#170911,#170912),
 .UNSPECIFIED.,.F.,.F.,(4,1,1,1,1,1,1,1,1,1,1,4),(311.017745311523,311.434502341581,
311.932970884889,312.431439428196,312.929907971504,313.926845058119,314.425313601427,
314.923782144734,315.920719231349,316.419187774657,316.917656317964,317.300850558385),
 .UNSPECIFIED.);
#3220=B_SPLINE_CURVE_WITH_KNOTS('',3,(#170914,#170915,#170916,#170917,#170918,
#170919,#170920,#170921,#170922,#170923,#170924,#170925,#170926,#170927,
#170928,#170929,#170930,#170931),.UNSPECIFIED.,.F.,.F.,(4,2,2,2,2,2,2,2,
4),(317.300858012569,318.130215789007,318.959573565445,319.788931341883,
320.618289118321,321.447646894759,322.277004671197,323.106362447635,323.584043319749),
 .UNSPECIFIED.);
#3221=B_SPLINE_CURVE_WITH_KNOTS('',3,(#170933,#170934,#170935,#170936,#170937,
#170938,#170939,#170940,#170941,#170942,#170943,#170944,#170945,#170946,
#170947,#170948,#170949,#170950,#170951,#170952,#170953,#170954,#170955,
#170956,#170957,#170958,#170959,#170960,#170961,#170962,#170963,#170964,
#170965,#170966,#170967,#170968,#170969,#170970,#170971,#170972,#170973,
#170974,#170975,#170976,#170977,#170978,#170979,#170980,#170981,#170982,
#170983,#170984,#170985,#170986,#170987),.UNSPECIFIED.,.F.,.F.,(4,3,3,3,
3,3,3,3,3,3,3,3,3,3,3,3,3,3,4),(323.584043319749,323.665206603477,323.746378549093,
323.82754791565,323.89621592427,323.972076794865,324.047910661161,324.12372725779,
324.199547384246,324.275367646974,324.351214673505,324.394684467578,324.473160269805,
324.551626766589,324.630085813129,324.708544612275,324.786997107681,324.865450438762,
324.893153010885),.UNSPECIFIED.);
#3222=B_SPLINE_CURVE_WITH_KNOTS('',3,(#170991,#170992,#170993,#170994,#170995,
#170996,#170997,#170998),.UNSPECIFIED.,.F.,.F.,(4,2,2,4),(323.584043319749,
324.413401096187,325.242758872624,325.416526282203),.UNSPECIFIED.);
#3223=B_SPLINE_CURVE_WITH_KNOTS('',3,(#171000,#171001,#171002,#171003,#171004,
#171005,#171006,#171007,#171008,#171009,#171010,#171011,#171012,#171013,
#171014),.UNSPECIFIED.,.F.,.F.,(4,1,1,1,1,1,1,1,1,1,1,1,4),(317.300858012569,
317.467727907809,318.464664994424,318.963133537731,319.461602081039,319.960070624347,
320.458539167654,320.957007710962,321.455476254269,321.953944797577,322.452413340884,
323.449350427499,323.584043319749),.UNSPECIFIED.);
#3224=B_SPLINE_CURVE_WITH_KNOTS('',3,(#171016,#171017,#171018,#171019,#171020,
#171021,#171022,#171023,#171024,#171025,#171026,#171027,#171028,#171029,
#171030,#171031,#171032,#171033,#171034,#171035,#171036,#171037,#171038,
#171039,#171040,#171041,#171042,#171043,#171044,#171045,#171046,#171047,
#171048,#171049,#171050,#171051,#171052,#171053,#171054,#171055,#171056,
#171057,#171058,#171059,#171060,#171061,#171062,#171063,#171064,#171065,
#171066,#171067,#171068,#171069,#171070,#171071,#171072,#171073,#171074,
#171075,#171076,#171077,#171078,#171079,#171080,#171081,#171082,#171083,
#171084,#171085,#171086,#171087,#171088,#171089,#171090,#171091,#171092,
#171093,#171094,#171095,#171096,#171097,#171098,#171099,#171100,#171101,
#171102,#171103,#171104,#171105,#171106,#171107,#171108,#171109,#171110,
#171111,#171112,#171113,#171114,#171115,#171116,#171117,#171118,#171119,
#171120,#171121,#171122,#171123,#171124,#171125,#171126,#171127,#171128,
#171129,#171130,#171131,#171132,#171133,#171134,#171135,#171136,#171137,
#171138,#171139,#171140,#171141,#171142,#171143,#171144,#171145,#171146,
#171147,#171148,#171149,#171150,#171151,#171152,#171153,#171154,#171155,
#171156,#171157,#171158,#171159,#171160,#171161,#171162,#171163,#171164,
#171165,#171166,#171167,#171168,#171169,#171170,#171171,#171172,#171173,
#171174,#171175,#171176,#171177,#171178,#171179,#171180,#171181,#171182,
#171183,#171184,#171185,#171186,#171187,#171188,#171189,#171190,#171191,
#171192,#171193,#171194,#171195,#171196,#171197,#171198,#171199,#171200,
#171201,#171202,#171203,#171204,#171205,#171206,#171207,#171208,#171209,
#171210,#171211,#171212,#171213,#171214,#171215,#171216,#171217,#171218,
#171219,#171220,#171221,#171222,#171223,#171224,#171225,#171226,#171227,
#171228,#171229,#171230,#171231,#171232,#171233,#171234,#171235,#171236,
#171237,#171238,#171239,#171240,#171241,#171242,#171243,#171244,#171245,
#171246,#171247,#171248,#171249,#171250,#171251,#171252,#171253,#171254,
#171255,#171256,#171257,#171258,#171259,#171260,#171261,#171262,#171263,
#171264,#171265,#171266,#171267,#171268,#171269,#171270,#171271,#171272,
#171273,#171274,#171275,#171276,#171277,#171278,#171279,#171280,#171281,
#171282,#171283,#171284,#171285,#171286,#171287,#171288,#171289,#171290,
#171291,#171292,#171293,#171294,#171295,#171296,#171297,#171298,#171299,
#171300,#171301,#171302,#171303,#171304,#171305,#171306,#171307,#171308,
#171309,#171310,#171311,#171312,#171313,#171314,#171315,#171316,#171317,
#171318,#171319,#171320,#171321,#171322,#171323,#171324,#171325,#171326,
#171327,#171328,#171329,#171330,#171331,#171332,#171333,#171334,#171335,
#171336,#171337,#171338,#171339,#171340,#171341,#171342,#171343,#171344,
#171345,#171346,#171347,#171348,#171349,#171350,#171351,#171352,#171353,
#171354,#171355,#171356,#171357,#171358,#171359,#171360,#171361,#171362,
#171363,#171364,#171365,#171366,#171367,#171368,#171369,#171370,#171371,
#171372,#171373,#171374,#171375,#171376,#171377,#171378,#171379,#171380,
#171381,#171382,#171383,#171384,#171385,#171386,#171387,#171388,#171389,
#171390,#171391,#171392,#171393,#171394,#171395,#171396,#171397,#171398,
#171399,#171400,#171401,#171402,#171403,#171404,#171405,#171406,#171407,
#171408,#171409,#171410,#171411,#171412,#171413,#171414,#171415,#171416,
#171417,#171418,#171419,#171420,#171421,#171422,#171423,#171424,#171425,
#171426,#171427,#171428,#171429,#171430,#171431,#171432,#171433,#171434,
#171435,#171436,#171437,#171438,#171439,#171440,#171441,#171442,#171443,
#171444,#171445,#171446,#171447,#171448,#171449,#171450,#171451,#171452,
#171453,#171454,#171455,#171456,#171457,#171458,#171459,#171460,#171461,
#171462,#171463,#171464,#171465,#171466,#171467,#171468,#171469,#171470,
#171471,#171472,#171473,#171474,#171475,#171476,#171477,#171478,#171479,
#171480,#171481,#171482,#171483,#171484,#171485,#171486,#171487,#171488,
#171489,#171490,#171491,#171492,#171493,#171494,#171495,#171496,#171497,
#171498,#171499,#171500,#171501,#171502,#171503,#171504,#171505,#171506,
#171507,#171508,#171509,#171510,#171511,#171512,#171513,#171514,#171515,
#171516,#171517,#171518,#171519,#171520,#171521,#171522,#171523,#171524,
#171525,#171526,#171527,#171528,#171529,#171530,#171531,#171532,#171533,
#171534,#171535,#171536,#171537,#171538,#171539,#171540,#171541,#171542,
#171543,#171544,#171545,#171546,#171547,#171548,#171549,#171550,#171551,
#171552,#171553,#171554,#171555,#171556,#171557,#171558,#171559,#171560,
#171561,#171562,#171563,#171564,#171565,#171566,#171567,#171568,#171569,
#171570,#171571,#171572,#171573,#171574,#171575,#171576,#171577,#171578,
#171579,#171580,#171581,#171582,#171583,#171584,#171585,#171586,#171587,
#171588,#171589,#171590,#171591,#171592,#171593,#171594,#171595,#171596,
#171597,#171598,#171599,#171600,#171601,#171602,#171603,#171604,#171605,
#171606,#171607,#171608,#171609,#171610,#171611,#171612,#171613,#171614,
#171615,#171616,#171617,#171618,#171619,#171620,#171621,#171622,#171623,
#171624,#171625,#171626,#171627,#171628,#171629,#171630,#171631,#171632,
#171633,#171634,#171635,#171636,#171637,#171638,#171639,#171640,#171641,
#171642,#171643,#171644,#171645,#171646,#171647,#171648,#171649,#171650,
#171651,#171652,#171653,#171654,#171655,#171656,#171657,#171658,#171659,
#171660,#171661,#171662,#171663,#171664,#171665,#171666,#171667,#171668,
#171669,#171670,#171671,#171672,#171673,#171674,#171675,#171676,#171677,
#171678,#171679,#171680,#171681,#171682,#171683,#171684,#171685,#171686,
#171687,#171688,#171689,#171690,#171691,#171692,#171693,#171694,#171695,
#171696,#171697,#171698,#171699,#171700,#171701,#171702,#171703,#171704,
#171705,#171706,#171707,#171708,#171709,#171710,#171711,#171712,#171713,
#171714,#171715,#171716,#171717,#171718,#171719,#171720,#171721,#171722,
#171723,#171724,#171725,#171726,#171727,#171728,#171729,#171730,#171731,
#171732,#171733,#171734,#171735,#171736,#171737,#171738,#171739,#171740,
#171741,#171742,#171743,#171744,#171745,#171746,#171747,#171748,#171749,
#171750,#171751,#171752,#171753,#171754,#171755,#171756,#171757,#171758,
#171759,#171760,#171761,#171762,#171763,#171764,#171765,#171766,#171767,
#171768,#171769,#171770,#171771,#171772,#171773,#171774,#171775,#171776,
#171777,#171778,#171779,#171780,#171781,#171782,#171783,#171784,#171785,
#171786,#171787,#171788,#171789,#171790,#171791,#171792,#171793,#171794,
#171795,#171796,#171797,#171798,#171799,#171800,#171801),.UNSPECIFIED.,
 .F.,.F.,(4,2,2,2,2,2,2,2,2,2,2,2,2,2,2,2,2,2,2,2,2,2,2,2,2,2,2,2,2,2,2,
2,2,2,2,2,2,2,2,2,2,2,2,2,2,2,2,2,2,2,2,2,2,2,2,2,2,2,2,2,2,2,2,2,2,2,2,
2,2,2,2,2,2,2,2,2,2,2,2,2,2,2,2,2,2,2,2,2,2,2,2,2,2,2,2,2,2,2,2,2,2,2,2,
2,2,2,2,2,2,2,2,2,2,2,2,2,2,2,2,2,2,2,2,2,2,2,2,2,2,2,2,2,2,2,2,2,2,2,2,
2,2,2,2,2,2,2,2,2,2,2,2,2,2,2,2,2,2,2,2,2,2,2,2,2,2,2,2,2,2,2,2,2,2,2,2,
2,2,2,2,2,2,2,2,2,2,2,2,2,2,2,2,2,2,2,2,2,2,2,2,2,2,2,2,2,2,2,2,2,2,2,2,
2,2,2,2,2,2,2,2,2,2,2,2,2,2,2,2,2,2,2,2,2,2,2,2,2,2,2,2,2,2,2,2,2,2,2,2,
2,2,2,2,2,2,2,2,2,2,2,2,2,2,2,2,2,2,2,2,2,2,2,2,2,2,2,2,2,2,2,2,2,2,2,2,
2,2,2,2,2,2,2,2,2,2,2,2,2,2,2,2,2,2,2,2,2,2,2,2,2,2,2,2,2,2,2,2,2,2,2,2,
2,2,2,2,2,2,2,2,2,2,2,2,2,2,2,2,2,2,2,2,2,2,2,2,2,2,2,2,2,2,2,2,2,2,2,2,
2,2,2,2,2,2,2,2,2,2,2,2,2,2,2,2,2,2,2,2,2,2,2,2,2,2,2,2,2,2,2,2,2,2,2,2,
2,4),(0.00175773553931062,0.219103254936723,0.24130675056173,0.253373369810396,
0.26400885429678,0.271010046070725,0.277588550997247,0.285910960050424,
0.302249272794649,0.441652005642513,0.517334035163842,0.573661124162176,
0.642628906649389,0.649141964325655,0.651548363312784,0.653662174922928,
0.655941397471844,0.658910732938449,0.665158306217353,0.730535299668664,
0.821431482018592,0.897670017795671,1.06124648248905,1.06972199635467,1.07359686257024,
1.07651494469592,1.07925735443216,1.08305340993945,1.09070766589037,1.16168760892158,
1.35647748551397,1.44920633297773,1.48326282640086,1.49517679124251,1.50361653908362,
1.50691092124709,1.50891569300446,1.51109605320493,1.51394152432146,1.52017635765003,
1.57374086012011,1.77004040456218,1.85380542168094,1.9323194264709,1.95550614639026,
1.9684984695291,1.97975037107685,1.99367251838452,2.02045895169309,2.18177440747651,
2.27676677816675,2.29298497237854,2.300026587392,2.30546542550424,2.3119241945082,
2.32361280667504,2.39430370226642,2.44426104636348,2.47638132625004,2.49001048845845,
2.49002447912599,2.49003848384626,2.4900525027195,2.49006653573498,2.49008058294009,
2.49009464438562,2.49010872016212,2.49012281031995,2.49013691483824,2.49015103381578,
2.49016516733543,2.49017931535028,2.49019347789304,2.49020765510122,2.49022184709889,
2.49023605378203,2.4902502752544,2.49026451164043,2.49027876290929,2.49029302907541,
2.49030731024939,2.49032160654275,2.49033591798422,2.50094928211647,2.51262434213112,
2.53221097121147,2.64706595965801,2.67939037980069,2.69926914385526,2.706878152016,
2.71220448103205,2.71807930181039,2.72873337570024,2.76686250023774,2.87828861367725,
2.93623224914979,2.95812530346132,2.97461351130785,2.99352213844178,3.03836168476794,
3.0879662388034,3.10562500164156,3.11747068542495,3.13304124034964,3.16671683525354,
3.19802874601558,3.23215616702389,3.25005725735955,3.26664612597028,3.28670977963142,
3.34368868867307,3.45264000311483,3.48023195286248,3.4988624845606,3.50693398937084,
3.51293219071194,3.51944501984934,3.53209183362207,3.60222639506482,3.68263921607325,
3.70627320395919,3.71875708277615,3.72926934321183,3.74201478281325,3.76636627514229,
3.85326945144904,3.8860865292963,3.90618166566052,3.91412477598333,3.91982250854305,
3.92511658531051,3.93503465805392,3.971631087357,4.04353339413235,4.12914377562721,
4.21300180379531,4.23342185086128,4.24585236336118,4.25720668401509,4.27184147911976,
4.30458249145143,4.42621249308663,4.60599934339915,4.67471734931112,4.70367241661355,
4.7086174106494,4.71123509451903,4.713176138818,4.71559382117842,4.7196254021198,
4.73283657596282,4.98808542030521,5.0771886966021,5.1143485646209,5.13565526533211,
5.14138094821278,5.144724154391,5.14759961151006,5.15108920504921,5.15764163483308,
5.19469059275185,5.2665560182974,5.54043555121987,5.559890466168,5.56419146418071,
5.56699335906224,5.56924618975467,5.57180457526152,5.57615245472894,5.59319977208206,
5.62393500696221,5.70261396549574,5.77935373268335,5.84915966813338,5.92339501433832,
5.93658395048812,5.9449358131758,5.95152838298344,5.9585335786119,5.96915481581509,
6.00070014138159,6.24784710410159,6.31422215349762,6.32543161127122,6.32930608349613,
6.33151434571518,6.3335472115256,6.33629285799145,6.34149805304394,6.37427083004007,
6.42221888210893,6.61240639593722,6.73790331560348,6.74735376784438,6.75110200563635,
6.75383249807268,6.7567591688638,6.7606821759407,6.769412506671,6.88848865610534,
7.14796800782987,7.1788927888432,7.18359207325653,7.18642040719891,7.18859886790867,
7.19093923000229,7.19462234215071,7.20623859633274,7.22478654868713,7.28975036595375,
7.50311638502679,7.60123389903768,7.63062995911758,7.64483776206688,7.65611911412314,
7.66893180015192,7.69113395071036,7.80677850944997,7.91149078331142,7.92724116144502,
7.93040424426407,7.95674358126864,7.97187318474109,7.97881485293055,7.98422898749944,
7.98423449530929,7.9842399911831,7.98424548058366,7.98425096343306,7.98425643994694,
7.98426190998369,7.98426737340359,7.98427283034096,7.98427828094693,7.98428372516629,
7.98428916298115,7.98429459438308,7.98430001941677,7.98430543803675,7.98431085028059,
7.98431625629666,7.98432165597753,7.98432704948173,7.9843324366821,7.98433781760566,
7.98434319220649,7.98434856053036,7.9843539226696,7.98435927860954,7.98436462821854,
7.98436997161479,7.98437530864554,7.98438063968183,7.98438596461978,7.98439128334387,
7.98439659583971,7.98440190224997,7.98440720262674,7.98976232166622,8.0003894723859,
8.06228631435481,8.14324823959832,8.16265105506578,8.1742638683533,8.18486821820486,
8.18488608151234,8.18490394305623,8.18492179598146,8.18493964028774,8.18495747603514,
8.18497530328501,8.18499312210091,8.18501093255323,8.18502873465068,8.18504652844231,
8.18506431401927,8.18508209143511,8.18509986069162,8.185117621884,8.18513537511171,
8.18515312033165,8.1851708576113,8.18518858705245,8.18520630868814,8.18522402254627,
8.18524172866618,8.18525942709194,8.18527711792504,8.18529480122889,8.18531247704046,
8.18533014539189,8.18534780632293,8.18536545987528,8.18538310613759,8.18540074518451,
8.18541837704094,8.18543600174093,8.19926806755702,8.23235884162917,8.28275511167052,
8.35854144903252,8.3772875446188,8.38486286081928,8.39032494313797,8.39036375199302,
8.39040046422107,8.39042357730001,8.39044638217812,8.39046888768473,8.3904910984323,
8.39051301885942,8.3905346533365,8.39055600620307,8.39057708163389,8.39059788382034,
8.39061841680037,8.39063868452902,8.39065869099236,8.3906784400369,8.39069793540036,
8.39071718075312,8.39073617983866,8.39075493622398,8.39077345341528,8.39079173484714,
8.39080978396012,8.39082760410349,8.39084519854574,8.39086257046582,8.39087414482491,
8.39088572026534,8.39089726116498,8.39090876770239,8.39092024008883,8.39093167839267,
8.39659483682501,8.40729864480983,8.45002625920061,8.57499910953089,8.61849057401589,
8.63893061114731,8.65536095720363,8.67513341979719,8.67539319551005,8.67565556400815,
8.67592064609455,8.67618856667261,8.67645945499847,8.67673344495327,8.73466225979669,
8.77601763080902,8.78803432447916,8.79924360381503,8.82258803183516,8.86148297575841,
8.90767426342444,8.92664310148138,8.94315597067937,8.96307983800104,9.01380549014799,
9.09709794554847,9.11800517335987,9.17141096545959,9.18270125807024,9.18894189376735,
9.19482167955657,9.20238899876156,9.22190300163407,9.23889919255774,9.32076450653238,
9.37527822464089,9.39215945163949,9.40218321154727,9.41291704052995,9.42353223026847,
9.44839252377286,9.53305464133504,9.58186561512102,9.58871930503183,9.5956740002792,
9.60101753776024,9.60732353642894,9.61946888376378,9.63523148033024,9.77791606178537,
9.89069508729099,9.91274824832863,9.92566695546978,9.93695339681467,9.95105061597933,
9.96638042027543,9.99188617045719,10.2304410678172),.UNSPECIFIED.);
#3225=B_SPLINE_CURVE_WITH_KNOTS('',3,(#171803,#171804,#171805,#171806,#171807,
#171808,#171809,#171810,#171811,#171812,#171813,#171814,#171815,#171816,
#171817,#171818,#171819,#171820,#171821,#171822,#171823,#171824,#171825,
#171826,#171827,#171828,#171829,#171830,#171831,#171832,#171833,#171834,
#171835,#171836,#171837,#171838,#171839,#171840,#171841,#171842,#171843,
#171844,#171845,#171846,#171847,#171848,#171849,#171850,#171851,#171852,
#171853,#171854,#171855,#171856,#171857,#171858,#171859,#171860,#171861,
#171862,#171863,#171864,#171865,#171866,#171867,#171868,#171869,#171870,
#171871,#171872,#171873,#171874,#171875,#171876,#171877,#171878,#171879,
#171880,#171881,#171882,#171883,#171884,#171885,#171886,#171887,#171888,
#171889,#171890,#171891,#171892,#171893,#171894,#171895,#171896,#171897,
#171898,#171899,#171900,#171901,#171902,#171903,#171904,#171905,#171906,
#171907,#171908,#171909,#171910,#171911,#171912,#171913,#171914,#171915,
#171916,#171917,#171918,#171919,#171920,#171921,#171922,#171923,#171924,
#171925,#171926,#171927,#171928,#171929,#171930,#171931,#171932,#171933,
#171934,#171935,#171936,#171937,#171938,#171939,#171940,#171941,#171942,
#171943,#171944,#171945,#171946,#171947,#171948,#171949,#171950,#171951,
#171952,#171953,#171954,#171955,#171956,#171957,#171958,#171959,#171960,
#171961,#171962,#171963,#171964,#171965,#171966,#171967,#171968,#171969,
#171970,#171971,#171972,#171973,#171974,#171975,#171976,#171977,#171978,
#171979,#171980,#171981,#171982,#171983,#171984,#171985,#171986,#171987,
#171988,#171989,#171990,#171991,#171992,#171993,#171994,#171995,#171996,
#171997,#171998,#171999,#172000,#172001,#172002,#172003,#172004,#172005,
#172006,#172007,#172008,#172009,#172010,#172011,#172012,#172013,#172014,
#172015,#172016,#172017,#172018,#172019,#172020,#172021,#172022,#172023,
#172024,#172025,#172026,#172027,#172028,#172029,#172030,#172031,#172032,
#172033,#172034,#172035,#172036,#172037,#172038,#172039,#172040,#172041,
#172042,#172043,#172044,#172045,#172046,#172047,#172048,#172049,#172050,
#172051,#172052,#172053,#172054,#172055,#172056,#172057,#172058,#172059,
#172060,#172061,#172062,#172063,#172064,#172065,#172066,#172067,#172068,
#172069,#172070,#172071,#172072,#172073,#172074,#172075,#172076,#172077,
#172078,#172079,#172080,#172081,#172082,#172083,#172084,#172085,#172086,
#172087,#172088,#172089,#172090,#172091,#172092,#172093,#172094,#172095,
#172096,#172097,#172098,#172099,#172100,#172101,#172102,#172103,#172104,
#172105,#172106,#172107,#172108,#172109,#172110,#172111,#172112,#172113,
#172114,#172115,#172116,#172117,#172118,#172119,#172120,#172121,#172122,
#172123,#172124,#172125,#172126,#172127,#172128,#172129,#172130,#172131,
#172132,#172133,#172134,#172135,#172136,#172137,#172138,#172139,#172140,
#172141,#172142,#172143,#172144,#172145,#172146,#172147,#172148,#172149,
#172150,#172151,#172152,#172153,#172154,#172155,#172156,#172157,#172158,
#172159,#172160,#172161,#172162,#172163,#172164,#172165,#172166,#172167,
#172168,#172169,#172170,#172171,#172172,#172173,#172174,#172175,#172176,
#172177,#172178,#172179,#172180,#172181,#172182,#172183,#172184,#172185,
#172186,#172187,#172188,#172189,#172190,#172191,#172192,#172193,#172194,
#172195,#172196,#172197,#172198,#172199,#172200,#172201,#172202,#172203,
#172204,#172205,#172206,#172207,#172208,#172209,#172210,#172211,#172212,
#172213,#172214,#172215,#172216,#172217,#172218,#172219,#172220,#172221,
#172222,#172223,#172224,#172225,#172226,#172227,#172228,#172229,#172230,
#172231,#172232,#172233,#172234,#172235,#172236,#172237,#172238,#172239,
#172240,#172241,#172242,#172243,#172244,#172245,#172246,#172247,#172248,
#172249,#172250,#172251,#172252,#172253,#172254,#172255,#172256,#172257,
#172258,#172259,#172260,#172261,#172262,#172263,#172264,#172265,#172266,
#172267,#172268,#172269,#172270,#172271,#172272,#172273,#172274,#172275,
#172276,#172277,#172278,#172279,#172280,#172281,#172282,#172283,#172284,
#172285,#172286,#172287,#172288,#172289,#172290,#172291,#172292,#172293,
#172294,#172295,#172296,#172297,#172298,#172299,#172300,#172301,#172302,
#172303,#172304,#172305,#172306,#172307,#172308,#172309,#172310,#172311,
#172312,#172313,#172314,#172315,#172316,#172317,#172318,#172319,#172320,
#172321,#172322,#172323,#172324,#172325,#172326,#172327,#172328,#172329,
#172330,#172331,#172332,#172333,#172334,#172335,#172336,#172337,#172338,
#172339,#172340,#172341,#172342,#172343,#172344,#172345,#172346,#172347,
#172348,#172349,#172350,#172351,#172352,#172353,#172354,#172355,#172356,
#172357,#172358,#172359,#172360,#172361,#172362,#172363,#172364,#172365,
#172366,#172367,#172368,#172369,#172370,#172371,#172372,#172373,#172374,
#172375,#172376,#172377,#172378,#172379,#172380,#172381,#172382,#172383,
#172384,#172385,#172386,#172387,#172388,#172389,#172390,#172391,#172392,
#172393,#172394,#172395,#172396,#172397,#172398,#172399,#172400,#172401,
#172402,#172403,#172404,#172405,#172406,#172407,#172408,#172409,#172410,
#172411,#172412,#172413,#172414,#172415,#172416,#172417,#172418,#172419,
#172420,#172421,#172422,#172423,#172424,#172425,#172426,#172427,#172428,
#172429,#172430,#172431,#172432,#172433,#172434,#172435,#172436,#172437,
#172438,#172439,#172440,#172441,#172442,#172443,#172444,#172445,#172446,
#172447,#172448,#172449,#172450,#172451,#172452,#172453,#172454,#172455,
#172456,#172457,#172458,#172459,#172460,#172461,#172462,#172463,#172464,
#172465,#172466,#172467,#172468,#172469,#172470,#172471,#172472,#172473,
#172474,#172475,#172476,#172477,#172478,#172479,#172480,#172481,#172482,
#172483,#172484,#172485,#172486,#172487,#172488,#172489,#172490,#172491,
#172492,#172493,#172494,#172495,#172496,#172497,#172498,#172499,#172500,
#172501,#172502,#172503,#172504,#172505,#172506),.UNSPECIFIED.,.F.,.F.,
(4,2,2,2,2,2,2,2,2,2,2,2,2,2,2,2,2,2,2,2,2,2,2,2,2,2,2,2,2,2,2,2,2,2,2,
2,2,2,2,2,2,2,2,2,2,2,2,2,2,2,2,2,2,2,2,2,2,2,2,2,2,2,2,2,2,2,2,2,2,2,2,
2,2,2,2,2,2,2,2,2,2,2,2,2,2,2,2,2,2,2,2,2,2,2,2,2,2,2,2,2,2,2,2,2,2,2,2,
2,2,2,2,2,2,2,2,2,2,2,2,2,2,2,2,2,2,2,2,2,2,2,2,2,2,2,2,2,2,2,2,2,2,2,2,
2,2,2,2,2,2,2,2,2,2,2,2,2,2,2,2,2,2,2,2,2,2,2,2,2,2,2,2,2,2,2,2,2,2,2,2,
2,2,2,2,2,2,2,2,2,2,2,2,2,2,2,2,2,2,2,2,2,2,2,2,2,2,2,2,2,2,2,2,2,2,2,2,
2,2,2,2,2,2,2,2,2,2,2,2,2,2,2,2,2,2,2,2,2,2,2,2,2,2,2,2,2,2,2,2,2,2,2,2,
2,2,2,2,2,2,2,2,2,2,2,2,2,2,2,2,2,2,2,2,2,2,2,2,2,2,2,2,2,2,2,2,2,2,2,2,
2,2,2,2,2,2,2,2,2,2,2,2,2,2,2,2,2,2,2,2,2,2,2,2,2,2,2,2,2,2,2,2,2,2,2,2,
2,2,2,2,2,2,2,2,2,2,2,2,2,2,2,2,2,2,2,2,2,2,2,2,2,2,2,2,4),(0.00222864392066332,
0.145752713813109,0.154791928451702,0.159396326581129,0.162264130794258,
0.164425517493528,0.166614639667749,0.168649290422639,0.171430485007103,
0.178384690789793,0.293562036677726,0.334592796162703,0.375675830641575,
0.465288439484411,0.584332488052246,0.593073292281324,0.59699800374325,
0.599924737670028,0.602654419157341,0.606400186788489,0.61385331218668,
0.678208354816265,0.873987252073665,0.922852180608173,0.979251475758716,
1.00070058020002,1.01434587787992,1.01837491691129,1.02049685833035,1.02252096157089,
1.02512984125736,1.02958757197051,1.0461410535428,1.1666078661986,1.30957250923845,
1.36136959646054,1.38605540093741,1.39585889250909,1.40269625282933,1.40936447496336,
1.41807350376215,1.43278605609214,1.55778909834871,1.71832385764177,1.76945439376248,
1.77903896584968,1.78254831562554,1.78466332692828,1.78693861525808,1.78987733445077,
1.79619734647444,1.86085768472907,2.08004265511586,2.19307531945937,2.20125313871922,
2.20507240359412,2.20798277593868,2.21074336851788,2.21537819555806,2.22754200321335,
2.43134625567394,2.56529135977613,2.62398890534212,2.63466156520055,2.63822881060265,
2.64054335950563,2.64273205632357,2.645624170723,2.65055742981425,2.68296170204597,
2.71882011910063,2.71982889577092,2.84973315290992,3.04593951658693,3.08071161858082,
3.09584105917549,3.10723166525579,3.11955668343999,3.13947380995051,3.20684683879622,
3.39454293907706,3.41263260619009,3.42614325388338,3.43270012242929,3.43827643518663,
3.44540570134363,3.45705148776271,3.54516724342479,3.57401033941666,3.60774680608874,
3.62189249785948,3.63253209545195,3.64269043738467,3.6603718965382,3.72983649015465,
3.78013601586695,3.80485432996246,3.82974349605703,3.83797114468403,3.84389394217918,
3.85055200107205,3.86184645097685,3.91004441181189,3.91238676080507,3.91371674091713,
3.91798156111839,4.01452135062403,4.06913856121101,4.09066209709999,4.10711943595327,
4.12627322391632,4.19048740211883,4.2296160630797,4.24293079069542,4.25623972954272,
4.29002536606598,4.33647312532537,4.35857595535477,4.37805095417511,4.3944748981709,
4.41519528751392,4.46215696094581,4.48714231091662,4.58634661497921,4.61296853788919,
4.63113087895284,4.63912460249245,4.64511174704584,4.65166953203201,4.66458763746315,
4.72058719053112,4.79078718389885,4.81032924055283,4.83672779543976,4.8497302190135,
4.86025446558893,4.87252386886401,4.89449856271038,4.9825450664432,5.0172538813494,
5.03808423035349,5.04613248111265,5.05185023962814,5.05787026577873,5.06853148641755,
5.1147251600168,5.23689491567324,5.27769883775891,5.3460594407408,5.36606667969574,
5.37841100607796,5.38979530389436,5.40488017087536,5.43937554834491,5.62916506115224,
5.75641739225734,5.83341941371237,5.83940444222344,5.84230436713257,5.84437090824065,
5.84654426827029,5.84938938459321,5.85545670814646,5.95726587322646,6.02248734172103,
6.10456251384157,6.26128579029209,6.27106833757507,6.2748727718778,6.27761822474729,
6.28053675355615,6.28440746415585,6.29285501588599,6.44828668234007,6.68131890665693,
6.6935382803584,6.69755492512495,6.69979043630343,6.70204308107137,6.70483720911909,
6.71027300180708,6.74716427713634,6.84800337643436,7.0381354625443,7.06439164361406,
7.0746092049952,7.08083496991808,7.08740878186555,7.09560116775854,7.11180070221573,
7.29162721837968,7.32321026075574,7.42781077739799,7.45503999791139,7.4598666418968,
7.46279433077781,7.46506821205946,7.46753039808207,7.47144620864666,7.48412805875149,
7.55963608588631,7.6984497095742,7.80839021325637,7.8721658441708,7.87960238993289,
7.88334450371148,7.88607375087583,7.88900212370012,7.89293268505709,7.90170162012449,
8.02080993220388,8.19202724149539,8.30772092336658,8.31485996978492,8.3176731951105,
8.31971663695966,8.32190143486072,8.32481953081665,8.33114439338697,8.3833592251149,
8.44224454137476,8.53318766649393,8.7228258852945,8.75844365625477,8.77259399323171,
8.78416173982891,8.79470232994797,8.80998127479262,8.84831254640901,8.90377103333723,
8.98929993120174,9.02087970194307,9.06920266201967,9.09891662976408,9.10822406193392,
9.11342323407321,9.11810506104238,9.1181206857969,9.11813627721229,9.11815183436659,
9.11816735763323,9.11818284736614,9.1181983038891,9.11821372750712,9.11822911861957,
9.11824447757168,9.11825980476813,9.11827510051404,9.11829036505129,9.11830559881839,
9.11832080219563,9.1183359754508,9.11835111896383,9.11836623296018,9.11838131780409,
9.11839637385397,9.11841140145639,9.11842640087208,9.1184413723903,9.11845631639496,
9.11847123315721,9.118486123009,9.11850098624138,9.11851582319342,9.11853063412191,
9.11854541930116,9.11856017903026,9.11857491367371,9.11858962350373,9.11860430874351,
9.11861896976863,9.1186336068464,9.11864822025547,9.1186628102186,9.1186773771369,
9.11869192132261,9.11870644293731,9.11872094228361,9.11873541958983,9.11874987514441,
9.11876430926325,9.11877872223553,9.11879311423609,9.11880748557093,9.11882183652364,
9.11883616734598,9.11885047827484,9.11886476965527,9.11887904169879,9.12447633339158,
9.13240972233585,9.14600325565374,9.17750894663704,9.26362320253015,9.2901178103735,
9.30310897002314,9.31292058209694,9.3131613658508,9.31338600044482,9.31359556748995,
9.31379107967034,9.31397348401925,9.31414366534419,9.31430244967537,9.31445060771165,
9.31458885819979,9.31471787119976,9.3148382712068,9.31495064015506,9.31505552022617,
9.31515341656896,9.31524479977996,9.31533010827759,9.31540975052063,9.31548410706331,
9.31560936332118,9.31573283957854,9.31585456886046,9.31597458659128,9.31609292622285,
9.327766496573,9.35284995356795,9.38655198407043,9.44127074805844,9.44967862585153,
9.50509500327044,9.51526810100552,9.52078290411029,9.52638001347458,9.53411889183065,
9.55219993613889,9.57898607067872,9.67970075853278,9.74551653714096,9.76590818147345,
9.7810397483565,9.79680409738449,9.81460486887346,9.82302515137781,9.84575828938478,
9.90731600452193,9.91744145069483,9.92843559728806,9.94057770605154,9.95994393761197,
10.0132912485553,10.0448031802273,10.0606934176668,10.0760958206565,10.0920438422306,
10.1134746853582,10.2281817080754),.UNSPECIFIED.);
#3226=B_SPLINE_CURVE_WITH_KNOTS('',3,(#172508,#172509,#172510,#172511,#172512,
#172513,#172514,#172515,#172516,#172517,#172518,#172519,#172520,#172521,
#172522,#172523,#172524,#172525,#172526,#172527,#172528,#172529,#172530,
#172531,#172532,#172533,#172534,#172535,#172536,#172537,#172538,#172539,
#172540,#172541,#172542,#172543,#172544,#172545,#172546,#172547,#172548,
#172549,#172550,#172551,#172552,#172553,#172554,#172555,#172556,#172557,
#172558,#172559,#172560,#172561,#172562,#172563,#172564,#172565,#172566,
#172567,#172568,#172569,#172570,#172571,#172572,#172573,#172574,#172575,
#172576,#172577,#172578,#172579,#172580,#172581,#172582,#172583,#172584,
#172585,#172586,#172587,#172588,#172589,#172590,#172591,#172592,#172593,
#172594,#172595,#172596,#172597,#172598,#172599,#172600,#172601,#172602,
#172603,#172604,#172605,#172606,#172607,#172608,#172609,#172610,#172611,
#172612,#172613,#172614,#172615,#172616,#172617,#172618,#172619,#172620,
#172621,#172622,#172623,#172624,#172625,#172626,#172627,#172628,#172629,
#172630,#172631,#172632,#172633,#172634,#172635,#172636,#172637,#172638,
#172639,#172640,#172641,#172642,#172643,#172644,#172645,#172646,#172647,
#172648,#172649,#172650,#172651,#172652,#172653,#172654,#172655,#172656,
#172657,#172658,#172659,#172660,#172661,#172662,#172663,#172664,#172665,
#172666,#172667,#172668,#172669,#172670,#172671,#172672,#172673,#172674,
#172675,#172676,#172677,#172678,#172679,#172680,#172681,#172682,#172683,
#172684,#172685,#172686,#172687,#172688,#172689,#172690,#172691,#172692,
#172693,#172694,#172695,#172696,#172697,#172698,#172699,#172700,#172701,
#172702,#172703,#172704,#172705,#172706,#172707,#172708,#172709,#172710,
#172711,#172712,#172713,#172714,#172715,#172716,#172717,#172718,#172719,
#172720,#172721,#172722,#172723,#172724,#172725,#172726,#172727,#172728,
#172729,#172730,#172731,#172732,#172733,#172734,#172735,#172736,#172737,
#172738,#172739,#172740,#172741,#172742,#172743,#172744,#172745,#172746,
#172747,#172748,#172749,#172750,#172751,#172752,#172753,#172754,#172755,
#172756,#172757,#172758,#172759,#172760,#172761,#172762,#172763,#172764,
#172765,#172766,#172767,#172768,#172769,#172770,#172771,#172772,#172773,
#172774,#172775,#172776,#172777,#172778,#172779,#172780,#172781,#172782,
#172783,#172784,#172785,#172786,#172787,#172788,#172789,#172790,#172791,
#172792,#172793,#172794,#172795,#172796,#172797,#172798,#172799,#172800,
#172801,#172802,#172803,#172804,#172805,#172806,#172807,#172808,#172809,
#172810,#172811,#172812,#172813,#172814,#172815,#172816,#172817,#172818,
#172819,#172820,#172821,#172822,#172823,#172824,#172825,#172826,#172827,
#172828,#172829,#172830,#172831,#172832,#172833,#172834,#172835,#172836,
#172837,#172838,#172839,#172840,#172841,#172842,#172843,#172844,#172845,
#172846,#172847,#172848,#172849,#172850,#172851,#172852,#172853,#172854,
#172855,#172856,#172857,#172858,#172859,#172860,#172861,#172862,#172863,
#172864,#172865,#172866,#172867,#172868,#172869,#172870,#172871,#172872,
#172873,#172874,#172875,#172876,#172877,#172878,#172879,#172880,#172881,
#172882,#172883,#172884,#172885,#172886,#172887,#172888,#172889,#172890,
#172891,#172892,#172893,#172894,#172895,#172896,#172897,#172898,#172899,
#172900,#172901,#172902,#172903,#172904,#172905,#172906,#172907,#172908,
#172909,#172910,#172911,#172912,#172913,#172914,#172915,#172916,#172917,
#172918,#172919,#172920,#172921,#172922,#172923,#172924,#172925,#172926,
#172927,#172928,#172929,#172930,#172931,#172932,#172933,#172934,#172935,
#172936,#172937,#172938,#172939,#172940,#172941,#172942,#172943,#172944,
#172945,#172946,#172947,#172948,#172949,#172950,#172951,#172952,#172953,
#172954,#172955,#172956,#172957,#172958,#172959,#172960,#172961,#172962,
#172963,#172964,#172965,#172966,#172967,#172968,#172969,#172970,#172971,
#172972,#172973,#172974,#172975,#172976,#172977,#172978,#172979,#172980,
#172981,#172982,#172983,#172984,#172985,#172986,#172987,#172988,#172989,
#172990,#172991,#172992,#172993,#172994,#172995,#172996,#172997,#172998,
#172999,#173000,#173001,#173002,#173003,#173004,#173005,#173006,#173007,
#173008,#173009,#173010,#173011,#173012,#173013,#173014,#173015,#173016,
#173017,#173018,#173019,#173020,#173021,#173022,#173023,#173024,#173025,
#173026,#173027,#173028,#173029,#173030,#173031,#173032,#173033,#173034,
#173035,#173036,#173037,#173038,#173039,#173040,#173041,#173042,#173043,
#173044,#173045,#173046,#173047,#173048,#173049),.UNSPECIFIED.,.F.,.F.,
(4,2,2,2,2,2,2,2,2,2,2,2,2,2,2,2,2,2,2,2,2,2,2,2,2,2,2,2,2,2,2,2,2,2,2,
2,2,2,2,2,2,2,2,2,2,2,2,2,2,2,2,2,2,2,2,2,2,2,2,2,2,2,2,2,2,2,2,2,2,2,2,
2,2,2,2,2,2,2,2,2,2,2,2,2,2,2,2,2,2,2,2,2,2,2,2,2,2,2,2,2,2,2,2,2,2,2,2,
2,2,2,2,2,2,2,2,2,2,2,2,2,2,2,2,2,2,2,2,2,2,2,2,2,2,2,2,2,2,2,2,2,2,2,2,
2,2,2,2,2,2,2,2,2,2,2,2,2,2,2,2,2,2,2,2,2,2,2,2,2,2,2,2,2,2,2,2,2,2,2,2,
2,2,2,2,2,2,2,2,2,2,2,2,2,2,2,2,2,2,2,2,2,2,2,2,2,2,2,2,2,2,2,2,2,2,2,2,
2,2,2,2,2,2,2,2,2,2,2,2,2,2,2,2,2,2,2,2,2,2,2,2,2,2,2,2,2,2,2,2,2,2,2,2,
2,2,2,2,2,2,2,2,2,2,2,2,2,2,2,2,2,2,2,4),(0.00102620614831673,0.0568395121519397,
0.0781476365882496,0.0858676499435164,0.0917549942783009,0.0975572177948521,
0.104209418963546,0.117718867000098,0.140873799900062,0.209787996764556,
0.26788818954445,0.290631847902776,0.291838944442536,0.292976648736238,
0.294064243783625,0.303958307270033,0.313682779774412,0.326502687937221,
0.35206394367747,0.452291696904518,0.475942494000112,0.487297021785289,
0.496439627916323,0.502253254910401,0.507828595969424,0.514762713683678,
0.533565358816321,0.663095578600488,0.773113263412681,0.807680316258092,
0.819786924111683,0.83027169013811,0.841634979043136,0.856335739853958,
0.889475990545155,1.0131264482929,1.17708042018566,1.25584166138584,1.27710490670949,
1.28566214189708,1.29008815764266,1.29385144559114,1.29620902902076,1.29838044441402,
1.30116747301061,1.30709407909758,1.3624960905748,1.40713069174675,1.47985115846917,
1.62910456283263,1.70712778795053,1.72150504741987,1.72629207696349,1.72939233653898,
1.73231950809825,1.73617982125951,1.74480201657441,1.81999982901002,1.94156121740033,
2.04967966638447,2.09256965895016,2.13649170847692,2.14273173807503,2.14778281122737,
2.15051958331156,2.15276763605195,2.15503559523524,2.15920895211213,2.17273127648019,
2.19737282608329,2.33787485357274,2.48276778677318,2.50365514423809,2.52010767786161,
2.52832174848353,2.5349166870894,2.54108069464312,2.55096840605079,2.57518623818831,
2.82351302936569,2.89713462538576,2.9089308613311,2.9127400507745,2.91517800892091,
2.91745962621654,2.9204394926797,2.92542886341437,2.95913901053721,3.16527192909523,
3.31878458652489,3.33022950419429,3.33460722095287,3.33761955029446,3.3405680232154,
3.344118179065,3.35296936006526,3.43615778853247,3.47739647774249,3.65769297450708,
3.75889393773878,3.76601887945577,3.76905667726209,3.77126150588284,3.77327672903998,
3.77598033625042,3.78262863393014,3.87729116904309,3.9992328027486,4.17717068951971,
4.21105794054042,4.22604057998807,4.23740762100006,4.24979121894257,4.26999426569961,
4.34063532123631,4.47399507575917,4.52296005770062,4.54174800167084,4.55565806888299,
4.56228766908029,4.5678536670028,4.57489815576959,4.58625007921004,4.66130630310504,
4.69733594625616,4.73581835933664,4.7505931595773,4.76132488053928,4.77130402813517,
4.78800615115649,4.84027806722212,4.92406750407647,4.94122737007191,4.96085691906785,
4.96843123511866,4.97375515784402,4.98049903936461,4.99219915201916,5.05814786787396,
5.06035259520831,5.11299003324026,5.15333939368309,5.20018219283488,5.22089788552376,
5.23731682048131,5.25678425594725,5.27887761985863,5.32529602977783,5.35908659909043,
5.37239467096206,5.38570201862689,5.42473549139449,5.48907346569522,5.50820482570642,
5.52465923770158,5.54620071201092,5.60101164646442,5.69834810586112,5.69952624098705,
5.75298522091397,5.76448850334058,5.77119018169888,5.77651889804539,5.78418010036951,
5.80445314908984,5.83775300740412,5.95009407008174,5.97023191300291,5.98201897393524,
5.99154346447942,6.00470531232457,6.03220697741315,6.07122550678907,6.1143254579551,
6.16279184324237,6.17298598539828,6.17853665761317,6.18354712192532,6.19077406487219,
6.20808051575612,6.23312690623326,6.35352320174268,6.47108190878521,6.49302678200077,
6.50590685009901,6.5171745302817,6.53126813749671,6.56006184105458,6.68043930490046,
6.85276470404648,6.96233246301301,6.96902159425894,6.97168705873444,6.97389302898849,
6.97614048663521,6.97939599249955,6.98785169056937,6.99956481915813,7.03274949209682,
7.06293335360849,7.2264084602597,7.39001246041463,7.39990812393551,7.40373015881433,
7.4064794461922,7.40939386817519,7.41324529367254,7.42159628135234,7.55858141389394,
7.74702234239047,7.81794604807203,7.82435751917478,7.82731288274965,7.82959009956768,
7.83203745955296,7.83549914248941,7.8458633106777,7.95964018618104,8.03807234203696,
8.09222144809225,8.18267184424082,8.19657053303832,8.20504110127206,8.21166880083292,
8.21857443138875,8.22839176053112,8.23957346880838,8.25952622133303,8.4715944205025,
8.58049382172193,8.58749981543922,8.59028929281688,8.59259705304038,8.59494732825187,
8.59802126450257,8.6055234310155,8.68912148674426,8.7770536055165,8.96806131025238,
9.00231795104721,9.00848674831538,9.01223287077243,9.01514129081237,9.01828873566096,
9.02328957663687,9.03943295244869,9.13345696586996,9.23629817586924,9.305119643732,
9.43348863068548,9.44192383883372,9.44494233413934,9.44704071362441,9.44898441250636,
9.45162829417569,9.4566985443934,9.48811950804353,9.59970117365182,9.69165753739034,
9.82764257374894,9.88035604089167,9.89839256157906,9.90912512694945,9.92055423769859,
9.9317274060158,9.94653493357267,9.97043295938086,10.018872567841,10.1115261152096,
10.1999744616998,10.2235615089747),.UNSPECIFIED.);
#3227=B_SPLINE_CURVE_WITH_KNOTS('',3,(#173051,#173052,#173053,#173054,#173055,
#173056,#173057,#173058,#173059,#173060,#173061,#173062,#173063,#173064,
#173065),.UNSPECIFIED.,.F.,.F.,(4,1,1,1,1,1,1,1,1,1,1,1,4),(273.318560862312,
273.602496096744,274.599433183359,275.097901726666,275.596370269974,276.593307356589,
277.091775899897,277.590244443204,278.088712986512,278.587181529819,279.085650073127,
279.584118616434,279.601746169492),.UNSPECIFIED.);
#3228=B_SPLINE_CURVE_WITH_KNOTS('',3,(#173067,#173068,#173069,#173070,#173071,
#173072,#173073,#173074,#173075,#173076,#173077,#173078,#173079,#173080,
#173081,#173082,#173083,#173084,#173085,#173086,#173087,#173088,#173089,
#173090,#173091,#173092,#173093,#173094,#173095,#173096,#173097,#173098,
#173099,#173100,#173101,#173102,#173103,#173104,#173105,#173106,#173107,
#173108,#173109,#173110,#173111,#173112,#173113,#173114,#173115,#173116,
#173117,#173118,#173119,#173120,#173121,#173122,#173123,#173124,#173125,
#173126,#173127,#173128,#173129,#173130,#173131,#173132,#173133,#173134,
#173135,#173136,#173137,#173138,#173139,#173140,#173141,#173142,#173143,
#173144,#173145,#173146,#173147,#173148,#173149,#173150,#173151,#173152,
#173153,#173154,#173155,#173156,#173157,#173158,#173159,#173160,#173161,
#173162,#173163,#173164,#173165,#173166,#173167,#173168,#173169,#173170,
#173171,#173172,#173173,#173174,#173175,#173176,#173177,#173178,#173179,
#173180,#173181,#173182,#173183,#173184,#173185,#173186,#173187,#173188,
#173189,#173190,#173191,#173192,#173193,#173194,#173195,#173196,#173197,
#173198,#173199,#173200,#173201,#173202,#173203,#173204,#173205,#173206,
#173207,#173208,#173209,#173210,#173211,#173212,#173213,#173214,#173215,
#173216,#173217,#173218,#173219,#173220,#173221,#173222,#173223,#173224,
#173225,#173226,#173227,#173228,#173229,#173230,#173231,#173232,#173233,
#173234,#173235,#173236,#173237,#173238,#173239,#173240,#173241,#173242,
#173243,#173244,#173245,#173246,#173247,#173248,#173249,#173250,#173251,
#173252,#173253,#173254,#173255,#173256,#173257,#173258,#173259,#173260,
#173261,#173262,#173263,#173264,#173265,#173266,#173267,#173268,#173269,
#173270,#173271,#173272,#173273,#173274,#173275,#173276,#173277,#173278,
#173279,#173280,#173281,#173282,#173283,#173284,#173285,#173286,#173287,
#173288,#173289,#173290,#173291,#173292,#173293,#173294,#173295,#173296,
#173297,#173298,#173299,#173300,#173301,#173302,#173303,#173304,#173305,
#173306,#173307,#173308,#173309,#173310,#173311,#173312,#173313,#173314,
#173315,#173316,#173317,#173318,#173319,#173320,#173321,#173322,#173323,
#173324,#173325),.UNSPECIFIED.,.F.,.F.,(4,3,3,3,3,3,3,3,3,3,3,3,3,3,3,3,
3,3,3,3,3,3,3,3,3,3,3,3,3,3,3,3,3,3,3,3,3,3,3,3,3,3,3,3,3,3,3,3,3,3,3,3,
3,3,3,3,3,3,3,3,3,3,3,3,3,3,3,3,3,3,3,3,3,3,3,3,3,3,3,3,3,3,3,3,3,3,4),
(267.035375555133,267.112204324455,267.189064455074,267.26596304077,267.342907197631,
267.419944352232,267.497030673745,267.574214775759,267.620873577053,267.697006449298,
267.77304615037,267.849002155741,267.924860598278,268.000661661832,268.076400982566,
268.11934212036,268.195084485183,268.270872605932,268.346715776774,268.422670735034,
268.498687167368,268.574822962869,268.617810663668,268.694021244142,268.770163848394,
268.846248934735,268.922286921007,268.998288191562,269.075345636402,269.151310898527,
269.227272490392,269.303239817453,269.381116800661,269.457146598094,269.535947174188,
269.614747750283,269.686171025133,269.757541152046,269.828871723567,269.900185061053,
269.971485747875,270.042811229367,270.113216293591,270.200921782932,270.289098145351,
270.377702555969,270.466402862852,270.554999122788,270.611684836898,270.684654281348,
270.757578272441,270.830469799182,270.903351998102,270.976226916146,271.049129865855,
271.110153380206,271.189454164155,271.268777094632,271.348119696642,271.427492773815,
271.506874454812,271.586271231921,271.608621923513,271.688019318182,271.76740299201,
271.846770443651,271.926115627463,272.00543864673,272.084732876351,272.107090466821,
272.17999286709,272.252872724135,272.325742993569,272.398639337974,272.471547993759,
272.544516306707,272.605559010129,272.694133341742,272.782833707216,272.871400519319,
272.959743932883,273.047513649509,273.104027553436,273.172188286623,273.240326894936,
273.308462615678,273.318560862312),.UNSPECIFIED.);
#3229=B_SPLINE_CURVE_WITH_KNOTS('',3,(#173327,#173328,#173329,#173330,#173331,
#173332,#173333,#173334,#173335,#173336,#173337,#173338,#173339,#173340,
#173341,#173342,#173343,#173344,#173345,#173346,#173347,#173348,#173349,
#173350,#173351,#173352,#173353,#173354,#173355,#173356,#173357,#173358,
#173359,#173360,#173361,#173362,#173363,#173364,#173365,#173366,#173367,
#173368,#173369,#173370,#173371,#173372,#173373,#173374,#173375,#173376,
#173377,#173378,#173379,#173380,#173381,#173382,#173383,#173384,#173385,
#173386,#173387,#173388,#173389,#173390,#173391,#173392,#173393,#173394,
#173395,#173396,#173397,#173398,#173399,#173400,#173401,#173402,#173403,
#173404,#173405,#173406,#173407,#173408,#173409,#173410,#173411,#173412,
#173413,#173414,#173415,#173416,#173417,#173418,#173419,#173420,#173421,
#173422,#173423,#173424,#173425,#173426,#173427,#173428,#173429,#173430,
#173431,#173432,#173433,#173434,#173435,#173436,#173437,#173438,#173439,
#173440,#173441,#173442,#173443,#173444,#173445,#173446,#173447,#173448,
#173449,#173450,#173451,#173452,#173453,#173454,#173455,#173456,#173457,
#173458,#173459,#173460,#173461,#173462,#173463,#173464,#173465,#173466,
#173467,#173468,#173469,#173470,#173471,#173472,#173473,#173474,#173475,
#173476,#173477,#173478,#173479,#173480,#173481,#173482,#173483,#173484,
#173485,#173486,#173487,#173488,#173489,#173490,#173491,#173492,#173493,
#173494,#173495,#173496,#173497,#173498,#173499,#173500,#173501,#173502,
#173503,#173504,#173505,#173506,#173507,#173508,#173509,#173510,#173511,
#173512,#173513,#173514,#173515,#173516,#173517,#173518,#173519,#173520,
#173521,#173522,#173523,#173524,#173525,#173526,#173527,#173528,#173529,
#173530,#173531,#173532,#173533,#173534,#173535,#173536,#173537,#173538,
#173539,#173540,#173541,#173542,#173543,#173544,#173545,#173546,#173547,
#173548,#173549,#173550,#173551,#173552,#173553,#173554,#173555,#173556,
#173557,#173558,#173559,#173560,#173561,#173562,#173563,#173564,#173565,
#173566,#173567,#173568,#173569,#173570,#173571,#173572,#173573,#173574,
#173575,#173576,#173577,#173578,#173579,#173580,#173581,#173582),
 .UNSPECIFIED.,.F.,.F.,(4,3,3,3,3,3,3,3,3,3,3,3,3,3,3,3,3,3,3,3,3,3,3,3,
3,3,3,3,3,3,3,3,3,3,3,3,3,3,3,3,3,3,3,3,3,3,3,3,3,3,3,3,3,3,3,3,3,3,3,3,
3,3,3,3,3,3,3,3,3,3,3,3,3,3,3,3,3,3,3,3,3,3,3,3,3,4),(260.752190247953,
260.825502775604,260.89874534631,260.971919280042,261.045053716347,261.118158903979,
261.140782514055,261.216524878878,261.292312999627,261.368156170469,261.444111128729,
261.520127561063,261.596263356563,261.639251057362,261.715461637835,261.791604242088,
261.867689328428,261.943727314701,262.019728585256,262.096786030096,262.172751292221,
262.248712884085,262.324680211146,262.402557194354,262.478586991787,262.557387567882,
262.636188143977,262.707611418827,262.77898154574,262.850312117261,262.921625454747,
262.992926141569,263.064251623061,263.134656687285,263.222362176625,263.310538539043,
263.399142949661,263.487843256543,263.576439516478,263.633125230592,263.706094675042,
263.779018666136,263.851910192877,263.924792391797,263.997667309841,264.070570259551,
264.1315937739,264.210894557849,264.290217488325,264.369560090336,264.448933167509,
264.528314848507,264.607711625615,264.630062317208,264.709459711877,264.788843385705,
264.868210837346,264.947556021158,265.026879040424,265.106173270045,265.128530860515,
265.201433260783,265.274313117828,265.347183387261,265.420079731666,265.492988387451,
265.565956700399,265.626999403823,265.715573735436,265.80427410091,265.892840913013,
265.981184326577,266.068954043202,266.12546794713,266.19679144548,266.268095195635,
266.339392698906,266.410725194553,266.482073553292,266.553494208259,266.623936490438,
266.709040194389,266.793997180456,266.878810120939,266.963290026646,267.035375555065),
 .UNSPECIFIED.);
#3230=B_SPLINE_CURVE_WITH_KNOTS('',3,(#173584,#173585,#173586,#173587,#173588,
#173589,#173590,#173591,#173592,#173593,#173594,#173595,#173596,#173597,
#173598),.UNSPECIFIED.,.F.,.F.,(4,1,1,1,1,1,1,1,1,1,1,1,4),(254.469004940773,
254.660691451056,255.657628537672,256.156097080979,256.654565624287,257.153034167594,
257.651502710902,258.149971254209,258.648439797517,259.146908340824,259.645376884132,
260.642313970747,260.752190247953),.UNSPECIFIED.);
#3231=B_SPLINE_CURVE_WITH_KNOTS('',3,(#173600,#173601,#173602,#173603,#173604,
#173605,#173606,#173607,#173608,#173609,#173610,#173611,#173612,#173613,
#173614,#173615,#173616,#173617,#173618,#173619,#173620,#173621,#173622,
#173623,#173624,#173625,#173626,#173627,#173628,#173629,#173630,#173631,
#173632,#173633,#173634,#173635,#173636,#173637,#173638,#173639,#173640,
#173641,#173642,#173643,#173644,#173645,#173646,#173647,#173648,#173649,
#173650,#173651,#173652,#173653,#173654,#173655,#173656,#173657,#173658,
#173659,#173660,#173661,#173662,#173663,#173664,#173665,#173666,#173667,
#173668,#173669,#173670,#173671,#173672,#173673,#173674,#173675,#173676,
#173677,#173678,#173679,#173680,#173681,#173682,#173683,#173684,#173685,
#173686,#173687,#173688,#173689,#173690,#173691,#173692,#173693,#173694,
#173695,#173696,#173697,#173698,#173699,#173700,#173701,#173702,#173703,
#173704,#173705,#173706,#173707,#173708,#173709,#173710,#173711,#173712,
#173713,#173714,#173715,#173716,#173717,#173718,#173719,#173720,#173721,
#173722,#173723,#173724,#173725,#173726,#173727,#173728,#173729,#173730,
#173731,#173732,#173733,#173734,#173735,#173736,#173737,#173738,#173739,
#173740,#173741,#173742,#173743,#173744,#173745,#173746,#173747,#173748,
#173749,#173750,#173751,#173752,#173753,#173754,#173755,#173756,#173757,
#173758,#173759,#173760,#173761,#173762,#173763,#173764,#173765,#173766,
#173767,#173768,#173769,#173770,#173771,#173772,#173773,#173774,#173775,
#173776,#173777,#173778,#173779,#173780,#173781,#173782,#173783,#173784,
#173785,#173786,#173787,#173788,#173789,#173790,#173791,#173792,#173793,
#173794,#173795,#173796,#173797,#173798,#173799,#173800,#173801,#173802,
#173803,#173804,#173805,#173806,#173807,#173808,#173809,#173810,#173811,
#173812,#173813,#173814,#173815,#173816,#173817,#173818,#173819,#173820,
#173821,#173822,#173823,#173824,#173825,#173826,#173827,#173828,#173829,
#173830,#173831,#173832,#173833,#173834,#173835,#173836,#173837,#173838,
#173839,#173840,#173841,#173842,#173843,#173844,#173845,#173846,#173847,
#173848,#173849,#173850,#173851,#173852,#173853,#173854,#173855),
 .UNSPECIFIED.,.F.,.F.,(4,3,3,3,3,3,3,3,3,3,3,3,3,3,3,3,3,3,3,3,3,3,3,3,
3,3,3,3,3,3,3,3,3,3,3,3,3,3,3,3,3,3,3,3,3,3,3,3,3,3,3,3,3,3,3,3,3,3,3,3,
3,3,3,3,3,3,3,3,3,3,3,3,3,3,3,3,3,3,3,3,3,3,3,3,3,4),(248.185820251478,
248.266341504436,248.346973689163,248.429997499714,248.510857010287,248.594962970826,
248.679068931366,248.750492206216,248.821862333129,248.893192904651,248.964506242137,
249.035806928959,249.107132410451,249.177537474673,249.265242964013,249.353419326431,
249.442023737048,249.53072404393,249.619320303864,249.676006017981,249.748975462431,
249.821899453525,249.894790980266,249.967673179187,250.040548097231,250.113451046941,
250.174474561288,250.253775345237,250.333098275714,250.412440877725,250.491813954897,
250.571195635894,250.650592413002,250.672943104596,250.752340499265,250.831724173093,
250.911091624734,250.990436808546,251.069759827812,251.149054057433,251.171411647904,
251.244314048173,251.317193905218,251.390064174651,251.462960519057,251.535869174842,
251.60883748779,251.669880191211,251.758454522823,251.847154888296,251.935721700398,
252.024065113961,252.111834830586,252.168348734519,252.239672232869,252.310975983024,
252.382273486296,252.453605981943,252.524954340682,252.596374995649,252.666817277826,
252.742920773847,252.818973919918,252.894987110153,252.970970710034,253.046935063362,
253.124037475997,253.200009204035,253.275993531294,253.351999872967,253.429938495836,
253.506047535264,253.584900949852,253.663754364441,253.739887236686,253.815926937757,
253.891882943129,253.967741385666,254.043542449219,254.119281769953,254.162222907749,
254.234133288965,254.306079971583,254.378048461525,254.450075949408,254.469004940773),
 .UNSPECIFIED.);
#3232=B_SPLINE_CURVE_WITH_KNOTS('',3,(#173857,#173858,#173859,#173860,#173861,
#173862,#173863,#173864,#173865,#173866,#173867,#173868,#173869,#173870,
#173871,#173872,#173873,#173874,#173875,#173876,#173877,#173878,#173879,
#173880,#173881,#173882,#173883,#173884,#173885,#173886,#173887,#173888,
#173889,#173890,#173891,#173892,#173893,#173894,#173895,#173896,#173897,
#173898,#173899,#173900,#173901,#173902,#173903,#173904,#173905,#173906,
#173907,#173908,#173909,#173910,#173911,#173912,#173913,#173914,#173915,
#173916,#173917,#173918,#173919,#173920,#173921,#173922,#173923,#173924,
#173925,#173926,#173927,#173928,#173929,#173930,#173931,#173932,#173933,
#173934,#173935,#173936,#173937,#173938,#173939,#173940,#173941,#173942,
#173943,#173944,#173945,#173946,#173947,#173948,#173949,#173950,#173951,
#173952,#173953,#173954,#173955,#173956,#173957,#173958,#173959,#173960,
#173961,#173962,#173963,#173964,#173965,#173966,#173967,#173968,#173969,
#173970,#173971,#173972,#173973,#173974,#173975,#173976,#173977,#173978,
#173979,#173980,#173981,#173982,#173983,#173984,#173985,#173986,#173987,
#173988,#173989,#173990,#173991,#173992,#173993,#173994,#173995,#173996,
#173997,#173998,#173999,#174000,#174001,#174002,#174003,#174004,#174005,
#174006,#174007,#174008,#174009,#174010,#174011,#174012,#174013,#174014,
#174015,#174016,#174017,#174018,#174019,#174020,#174021,#174022,#174023,
#174024,#174025,#174026,#174027,#174028,#174029,#174030,#174031,#174032,
#174033,#174034,#174035,#174036,#174037,#174038,#174039,#174040,#174041,
#174042,#174043,#174044,#174045,#174046,#174047,#174048,#174049,#174050,
#174051,#174052,#174053,#174054,#174055,#174056,#174057,#174058,#174059,
#174060,#174061,#174062,#174063,#174064,#174065,#174066,#174067,#174068,
#174069,#174070,#174071,#174072,#174073,#174074,#174075,#174076,#174077,
#174078,#174079,#174080,#174081,#174082,#174083,#174084,#174085,#174086,
#174087,#174088,#174089,#174090,#174091,#174092,#174093,#174094,#174095,
#174096,#174097,#174098,#174099,#174100,#174101,#174102,#174103,#174104,
#174105,#174106,#174107,#174108,#174109,#174110,#174111,#174112,#174113,
#174114,#174115),.UNSPECIFIED.,.F.,.F.,(4,3,3,3,3,3,3,3,3,3,3,3,3,3,3,3,
3,3,3,3,3,3,3,3,3,3,3,3,3,3,3,3,3,3,3,3,3,3,3,3,3,3,3,3,3,3,3,3,3,3,3,3,
3,3,3,3,3,3,3,3,3,3,3,3,3,3,3,3,3,3,3,3,3,3,3,3,3,3,3,3,3,3,3,3,3,3,4),
(241.902634326414,241.971086085413,242.039528364561,242.107964736407,242.176423951892,
242.198977868367,242.286683357707,242.374859720126,242.463464130744,242.552164437627,
242.640760697563,242.697446411675,242.770415856125,242.843339847219,242.91623137396,
242.989113572881,243.061988490924,243.134891440634,243.195914954983,243.275215738932,
243.354538669409,243.43388127142,243.513254348593,243.59263602959,243.672032806699,
243.69438349829,243.773780892958,243.853164566786,243.932532018426,244.011877202238,
244.091200221503,244.170494451125,244.192852041598,244.265754441867,244.338634298912,
244.411504568346,244.484400912751,244.557309568536,244.630277881485,244.691320584905,
244.779894916517,244.86859528199,244.957162094092,245.045505507656,245.133275224281,
245.189789128213,245.261112626563,245.332416376718,245.403713879991,245.475046375638,
245.546394734377,245.617815389344,245.68825767152,245.764361167541,245.840414313611,
245.916427503847,245.992411103727,246.068375457055,246.14547786969,246.221449597729,
246.297433924988,246.37344026666,246.451378889529,246.527487928957,246.606341343547,
246.685194758136,246.761327630381,246.837367331453,246.913323336824,246.989181779361,
247.064982842916,247.14072216365,247.183663301443,247.259405666265,247.335193787014,
247.411036957855,247.486991916115,247.563008348449,247.639144143949,247.682131844751,
247.761518664415,247.840814500136,247.92001827371,247.999090510025,248.078078319358,
248.156948820267,248.185819633594),.UNSPECIFIED.);
#3233=B_SPLINE_CURVE_WITH_KNOTS('',3,(#174117,#174118,#174119,#174120,#174121,
#174122,#174123,#174124,#174125,#174126,#174127,#174128,#174129,#174130,
#174131,#174132,#174133,#174134,#174135,#174136,#174137,#174138,#174139,
#174140,#174141,#174142,#174143,#174144,#174145,#174146,#174147,#174148,
#174149,#174150,#174151,#174152,#174153,#174154,#174155,#174156,#174157,
#174158,#174159,#174160,#174161,#174162,#174163,#174164,#174165,#174166,
#174167,#174168,#174169,#174170,#174171,#174172,#174173,#174174,#174175,
#174176,#174177,#174178,#174179,#174180,#174181,#174182,#174183,#174184,
#174185,#174186,#174187,#174188,#174189,#174190,#174191,#174192,#174193,
#174194,#174195,#174196,#174197,#174198,#174199,#174200,#174201,#174202,
#174203,#174204,#174205,#174206,#174207,#174208,#174209,#174210,#174211,
#174212,#174213,#174214,#174215,#174216,#174217,#174218,#174219,#174220,
#174221,#174222,#174223,#174224,#174225,#174226,#174227,#174228,#174229,
#174230,#174231,#174232,#174233,#174234,#174235,#174236,#174237,#174238,
#174239,#174240,#174241,#174242,#174243,#174244,#174245,#174246,#174247,
#174248,#174249,#174250,#174251,#174252,#174253,#174254,#174255,#174256,
#174257,#174258,#174259,#174260,#174261,#174262,#174263,#174264,#174265,
#174266,#174267,#174268,#174269,#174270,#174271,#174272,#174273,#174274,
#174275,#174276,#174277,#174278,#174279,#174280,#174281,#174282,#174283,
#174284,#174285,#174286,#174287,#174288,#174289,#174290,#174291,#174292,
#174293,#174294,#174295,#174296,#174297,#174298,#174299,#174300,#174301,
#174302,#174303,#174304,#174305,#174306,#174307,#174308,#174309,#174310,
#174311,#174312,#174313,#174314,#174315,#174316,#174317,#174318,#174319,
#174320,#174321,#174322,#174323,#174324,#174325,#174326,#174327,#174328,
#174329,#174330,#174331,#174332,#174333,#174334,#174335,#174336,#174337,
#174338,#174339,#174340,#174341,#174342,#174343,#174344,#174345,#174346,
#174347,#174348,#174349,#174350,#174351,#174352,#174353,#174354,#174355,
#174356,#174357,#174358,#174359,#174360,#174361,#174362,#174363,#174364,
#174365,#174366,#174367,#174368,#174369,#174370,#174371,#174372,#174373,
#174374,#174375,#174376,#174377,#174378,#174379,#174380,#174381,#174382,
#174383,#174384,#174385,#174386,#174387,#174388,#174389,#174390,#174391,
#174392,#174393,#174394,#174395,#174396,#174397,#174398,#174399,#174400,
#174401,#174402,#174403,#174404,#174405,#174406,#174407,#174408,#174409,
#174410,#174411,#174412,#174413,#174414,#174415,#174416,#174417,#174418,
#174419,#174420,#174421,#174422,#174423,#174424,#174425,#174426,#174427,
#174428,#174429,#174430,#174431,#174432,#174433,#174434,#174435,#174436,
#174437,#174438,#174439,#174440,#174441,#174442,#174443,#174444,#174445,
#174446,#174447,#174448,#174449,#174450,#174451,#174452,#174453,#174454,
#174455,#174456,#174457,#174458,#174459,#174460,#174461,#174462,#174463,
#174464,#174465,#174466,#174467,#174468,#174469,#174470,#174471,#174472,
#174473,#174474,#174475,#174476,#174477,#174478,#174479,#174480,#174481,
#174482,#174483,#174484,#174485,#174486,#174487,#174488,#174489,#174490,
#174491,#174492,#174493,#174494,#174495,#174496,#174497,#174498,#174499,
#174500,#174501,#174502,#174503,#174504,#174505,#174506,#174507,#174508,
#174509,#174510,#174511,#174512,#174513,#174514,#174515,#174516,#174517,
#174518,#174519,#174520,#174521,#174522,#174523,#174524,#174525,#174526,
#174527,#174528,#174529,#174530,#174531,#174532,#174533,#174534,#174535,
#174536,#174537,#174538,#174539,#174540,#174541,#174542,#174543,#174544,
#174545,#174546,#174547,#174548,#174549,#174550,#174551,#174552,#174553,
#174554,#174555,#174556,#174557,#174558,#174559,#174560,#174561,#174562,
#174563,#174564,#174565,#174566,#174567,#174568,#174569,#174570,#174571,
#174572,#174573,#174574,#174575,#174576,#174577,#174578,#174579,#174580,
#174581,#174582,#174583,#174584,#174585,#174586,#174587,#174588,#174589,
#174590,#174591,#174592,#174593,#174594,#174595,#174596,#174597,#174598,
#174599,#174600,#174601,#174602,#174603,#174604,#174605,#174606,#174607,
#174608,#174609,#174610,#174611,#174612,#174613,#174614,#174615,#174616,
#174617,#174618,#174619,#174620,#174621,#174622,#174623,#174624,#174625,
#174626,#174627,#174628,#174629,#174630,#174631,#174632,#174633,#174634,
#174635,#174636,#174637,#174638,#174639,#174640,#174641,#174642,#174643,
#174644,#174645,#174646,#174647,#174648,#174649,#174650,#174651,#174652,
#174653,#174654,#174655,#174656,#174657,#174658,#174659,#174660,#174661,
#174662,#174663,#174664,#174665,#174666,#174667,#174668,#174669,#174670,
#174671,#174672,#174673,#174674,#174675,#174676,#174677,#174678,#174679,
#174680,#174681,#174682,#174683,#174684,#174685,#174686,#174687,#174688,
#174689,#174690,#174691,#174692,#174693,#174694,#174695,#174696,#174697,
#174698,#174699,#174700,#174701,#174702,#174703,#174704,#174705,#174706,
#174707,#174708,#174709,#174710,#174711,#174712,#174713,#174714,#174715,
#174716,#174717,#174718,#174719,#174720,#174721,#174722,#174723,#174724,
#174725,#174726,#174727,#174728,#174729,#174730,#174731,#174732,#174733,
#174734,#174735,#174736,#174737,#174738,#174739,#174740,#174741,#174742,
#174743,#174744,#174745,#174746,#174747,#174748,#174749,#174750,#174751,
#174752,#174753,#174754,#174755,#174756,#174757,#174758,#174759,#174760,
#174761,#174762,#174763,#174764,#174765,#174766,#174767,#174768,#174769,
#174770,#174771,#174772,#174773,#174774,#174775,#174776,#174777,#174778,
#174779,#174780,#174781,#174782,#174783,#174784,#174785,#174786,#174787,
#174788,#174789,#174790,#174791,#174792,#174793,#174794,#174795,#174796,
#174797,#174798,#174799,#174800,#174801,#174802,#174803,#174804,#174805,
#174806,#174807,#174808,#174809,#174810,#174811,#174812,#174813,#174814,
#174815,#174816,#174817,#174818,#174819,#174820,#174821,#174822,#174823,
#174824,#174825,#174826,#174827,#174828,#174829,#174830,#174831,#174832,
#174833,#174834,#174835,#174836,#174837,#174838,#174839,#174840),
 .UNSPECIFIED.,.F.,.F.,(4,2,2,2,2,2,2,2,2,2,2,2,2,2,2,2,2,2,2,2,2,2,2,2,
2,2,2,2,2,2,2,2,2,2,2,2,2,2,2,2,2,2,2,2,2,2,2,2,2,2,2,2,2,2,2,2,2,2,2,2,
2,2,2,2,2,2,2,2,2,2,2,2,2,2,2,2,2,2,2,2,2,2,2,2,2,2,2,2,2,2,2,2,2,2,2,2,
2,2,2,2,2,2,2,2,2,2,2,2,2,2,2,2,2,2,2,2,2,2,2,2,2,2,2,2,2,2,2,2,2,2,2,2,
2,2,2,2,2,2,2,2,2,2,2,2,2,2,2,2,2,2,2,2,2,2,2,2,2,2,2,2,2,2,2,2,2,2,2,2,
2,2,2,2,2,2,2,2,2,2,2,2,2,2,2,2,2,2,2,2,2,2,2,2,2,2,2,2,2,2,2,2,2,2,2,2,
2,2,2,2,2,2,2,2,2,2,2,2,2,2,2,2,2,2,2,2,2,2,2,2,2,2,2,2,2,2,2,2,2,2,2,2,
2,2,2,2,2,2,2,2,2,2,2,2,2,2,2,2,2,2,2,2,2,2,2,2,2,2,2,2,2,2,2,2,2,2,2,2,
2,2,2,2,2,2,2,2,2,2,2,2,2,2,2,2,2,2,2,2,2,2,2,2,2,2,2,2,2,2,2,2,2,2,2,2,
2,2,2,2,2,2,2,2,2,2,2,2,2,2,2,2,2,2,2,2,2,2,2,2,2,2,2,2,2,2,2,2,2,2,2,2,
2,2,2,2,2,2,2,2,2,2,2,2,2,4),(0.0017506814511106,0.134011037079277,0.13863498196845,
0.141510894125579,0.143675180075276,0.145865863922226,0.147898130505966,
0.150670150933493,0.156128800685242,0.218904837886574,0.253373309699606,
0.2713995518874,0.297725977712415,0.334632156279759,0.409083522008049,0.520385300887421,
0.566345439752942,0.573275582751303,0.576845253339605,0.579699806771832,
0.582555458912094,0.587669036252463,0.603126829471007,0.870804288318988,
0.927422212127102,0.970581601793251,0.9848918686534,0.994813468929493,0.998399462885633,
1.0004990220348,1.0027655650585,1.00569105317595,1.01177742138225,1.05391349914012,
1.18009622661855,1.28059987564952,1.33131222945727,1.36347350583833,1.3742407439205,
1.38127738763749,1.38786127635502,1.39614133189458,1.40909256450011,1.47859758061937,
1.49115531215296,1.5587183989163,1.64005073066659,1.74326408723159,1.75266721780301,
1.75746543533536,1.76146386815625,1.76392991630215,1.76618948822263,1.76905778179412,
1.77485609908085,1.81613207590194,1.82162002063461,2.04722861024931,2.15967583498945,
2.17763716563563,2.18283861937298,2.18603146174995,2.18892818765682,2.19264720171819,
2.19859053623103,2.22922431341702,2.44839372180056,2.60656808930926,2.61498178858879,
2.61823134145179,2.62047800348131,2.62268580660917,2.62535667148648,2.63207638564006,
2.73649002110687,2.91260549609256,3.03413850890854,3.06308448618106,3.07720855502232,
3.08848141520548,3.10134674053766,3.12321576501316,3.23927938517667,3.3604710191477,
3.38606604048794,3.40365610122618,3.41093105008172,3.41647652943451,3.42301903706092,
3.43471694238046,3.50662666864935,3.58033455075747,3.59745100796469,3.60861788178852,
3.61933499038916,3.63222292267813,3.66402294061125,3.71871535749359,3.77935003360823,
3.79899838911008,3.81301679475049,3.81975197170663,3.82569941757997,3.83341569888974,
3.84617818421831,3.95715494259211,4.00589568999809,4.05167657705705,4.07205958729372,
4.08830036339894,4.10831340240641,4.15752203024455,4.19208662808957,4.2027216608629,
4.21868518394084,4.23070701819041,4.24812679100687,4.30446165678307,4.32279884076342,
4.3487908836774,4.36569830305274,4.38118537683877,4.40800691424252,4.54680591499908,
4.58521538211865,4.60130133601558,4.61380268835446,4.62071771776603,4.62661544475266,
4.63413771099004,4.65163166787588,4.72859306170826,4.7794707773513,4.81290323400089,
4.82706742233238,4.83771048642375,4.84786367870627,4.86553245227002,4.96137712836724,
4.99648683897189,5.01746877316622,5.02553782008216,5.03125923409228,5.03651960013234,
5.04622401492361,5.07989691039116,5.11427385054093,5.25314699160246,5.25623071765815,
5.3253695358523,5.34544566896279,5.35780433985531,5.36918328765182,5.38423334677144,
5.4185170504197,5.60387741534106,5.73060731515254,5.81277345777961,5.81945616126802,
5.82212094537614,5.82432708697088,5.82657546225993,5.82983364057102,5.83830374325064,
5.87559419445762,5.91338371254504,6.00121395149035,6.08349114182264,6.24063115025451,
6.25041489811844,6.25421925095062,6.25696445715838,6.25988254961366,6.2637523856324,
6.27219685473291,6.42713990977992,6.66057725614571,6.67282472039797,6.67684476981671,
6.67908078259702,6.68133301734677,6.6841252642536,6.68955303741645,6.72623011507484,
6.82397057895111,6.89647080034816,7.03199978699402,7.04829129586106,7.05661374353084,
7.06320296543036,7.07022129295673,7.0809025643062,7.11293057704927,7.3581229076199,
7.43204234632018,7.4389039121332,7.44167054404701,7.44397311887888,7.44633209434472,
7.44977301371144,7.4588451102699,7.50066990425859,7.52835637073232,7.67275058015654,
7.84764416310736,7.85846617419166,7.86243743371532,7.8652279573796,7.86783720469648,
7.87142341399599,7.87843011827409,7.92648394143464,7.98435147450019,8.17240101845266,
8.28706843464876,8.29428068063963,8.29710617341732,8.29915281170705,8.30133568396748,
8.30424203996012,8.31050509690418,8.36196506764097,8.42013955385869,8.51054997994833,
8.61358512606202,8.71226957498,8.74173864000045,8.75595989721054,8.76724261118356,
8.77777253047674,8.79268410061458,8.83872656420922,8.91210062435603,8.98107783247322,
9.03942036151044,9.07690273371647,9.0868965295736,9.09220416584354,9.09722909586111,
9.09724519404607,9.09726125470968,9.09727727820422,9.09729326492776,9.09730921524664,
9.09732512954939,9.09734100822504,9.09735685168681,9.09737266033171,9.09738843450381,
9.09740417465555,9.09741988105226,9.09743555410995,9.09745119426574,9.0974668018405,
9.09748237710095,9.09749792042229,9.09751343221599,9.09752891280702,9.09754436252808,
9.09755978170931,9.09757517077558,9.09759053003072,9.0976058597598,9.09762116025292,
9.09763643191778,9.09765167518182,9.09766689031797,9.09768207759256,9.09769723736394,
9.09771236991245,9.09772747555218,9.09774255465622,9.09775760754086,9.09777263449457,
9.09778763578268,9.0978026117394,9.09781756268493,9.09783248889226,9.09784739071474,
9.09786226846576,9.0978771224258,9.09789195287733,9.09790676006307,9.09792154429873,
9.09793630585734,9.0979510450589,9.09796576219781,9.09798045756381,9.09799513138782,
9.09800978391952,9.09802441549316,9.09803902644034,9.09805361694611,9.09806818736886,
9.09808273795104,9.09809726888821,9.09811178050891,9.09812627306761,9.09814074681622,
9.09815520201693,9.09816963896134,9.10376758873861,9.111705228767,9.12531131906822,
9.15686789419644,9.25454872956124,9.27408222205404,9.28573872111132,9.29592704517915,
9.29603595381324,9.29614336899312,9.29624931848151,9.29635382943915,9.2964569284654,
9.29655864159056,9.29665899427572,9.29675801144607,9.29685571750476,9.29695213632015,
9.31092150276583,9.34412332454436,9.3948351083356,9.47158009032108,9.4894396755397,
9.49702250064662,9.50259915727206,9.50890866066505,9.5089498433501,9.50899116245939,
9.50903262050805,9.50907422032181,9.50911596471042,9.50915785653998,9.50919989870679,
9.50924209410722,9.50928444563142,9.50932695623728,9.50936962886592,9.52063089822793,
9.53504891151008,9.56736593875558,9.63206451171904,9.67800823402137,9.71867947861838,
9.74403185537591,9.75929422515171,9.77511822310509,9.79265678210112,9.80203837035258,
9.82518662032188,9.8865267092225,9.89677661176384,9.90769244598511,9.91987359611358,
9.93937083100793,9.99371491344264,10.0244018205133,10.0401994715322,10.0555506604875,
10.0715617790068,10.0931872119106,10.2274941457884),.UNSPECIFIED.);
#3234=B_SPLINE_CURVE_WITH_KNOTS('',3,(#174842,#174843,#174844,#174845,#174846,
#174847,#174848,#174849,#174850,#174851,#174852,#174853,#174854,#174855,
#174856,#174857,#174858,#174859,#174860,#174861,#174862,#174863,#174864,
#174865,#174866,#174867,#174868,#174869,#174870,#174871,#174872,#174873,
#174874,#174875,#174876,#174877,#174878,#174879,#174880,#174881,#174882,
#174883,#174884,#174885,#174886,#174887,#174888,#174889,#174890,#174891,
#174892,#174893,#174894,#174895,#174896,#174897,#174898,#174899,#174900,
#174901,#174902,#174903,#174904,#174905,#174906,#174907,#174908,#174909,
#174910,#174911,#174912,#174913,#174914,#174915,#174916,#174917,#174918,
#174919,#174920,#174921,#174922,#174923,#174924,#174925,#174926,#174927,
#174928,#174929,#174930,#174931,#174932,#174933,#174934,#174935,#174936,
#174937,#174938,#174939,#174940,#174941,#174942,#174943,#174944,#174945,
#174946,#174947,#174948,#174949,#174950,#174951,#174952,#174953,#174954,
#174955,#174956,#174957,#174958,#174959,#174960,#174961,#174962,#174963,
#174964,#174965,#174966,#174967,#174968,#174969,#174970,#174971,#174972,
#174973,#174974,#174975,#174976,#174977,#174978,#174979,#174980,#174981,
#174982,#174983,#174984,#174985,#174986,#174987,#174988,#174989,#174990,
#174991,#174992,#174993,#174994,#174995,#174996,#174997,#174998,#174999,
#175000,#175001,#175002,#175003,#175004,#175005,#175006,#175007,#175008,
#175009,#175010,#175011,#175012,#175013,#175014,#175015,#175016,#175017,
#175018,#175019,#175020,#175021,#175022,#175023,#175024,#175025,#175026,
#175027,#175028,#175029,#175030,#175031,#175032,#175033,#175034,#175035,
#175036,#175037,#175038,#175039,#175040,#175041,#175042,#175043,#175044,
#175045,#175046,#175047,#175048,#175049,#175050,#175051,#175052,#175053,
#175054,#175055,#175056,#175057,#175058,#175059,#175060,#175061,#175062,
#175063,#175064,#175065,#175066,#175067,#175068,#175069,#175070,#175071,
#175072,#175073,#175074,#175075,#175076,#175077,#175078,#175079,#175080,
#175081,#175082,#175083,#175084,#175085,#175086,#175087,#175088,#175089,
#175090,#175091,#175092,#175093,#175094,#175095,#175096,#175097,#175098,
#175099,#175100,#175101,#175102,#175103,#175104,#175105,#175106,#175107,
#175108,#175109,#175110,#175111,#175112,#175113,#175114,#175115,#175116,
#175117,#175118,#175119,#175120,#175121,#175122,#175123,#175124,#175125,
#175126,#175127,#175128,#175129,#175130,#175131,#175132,#175133,#175134,
#175135,#175136,#175137,#175138,#175139,#175140,#175141,#175142,#175143,
#175144,#175145,#175146,#175147,#175148,#175149,#175150,#175151,#175152,
#175153,#175154,#175155,#175156,#175157,#175158,#175159,#175160,#175161,
#175162,#175163,#175164,#175165,#175166,#175167,#175168,#175169,#175170,
#175171,#175172,#175173,#175174,#175175,#175176,#175177,#175178,#175179,
#175180,#175181,#175182,#175183,#175184,#175185,#175186,#175187,#175188,
#175189,#175190,#175191,#175192,#175193,#175194,#175195,#175196,#175197,
#175198,#175199,#175200,#175201,#175202,#175203,#175204,#175205,#175206,
#175207,#175208,#175209,#175210,#175211,#175212,#175213,#175214,#175215,
#175216,#175217,#175218,#175219,#175220,#175221,#175222,#175223,#175224,
#175225,#175226,#175227,#175228,#175229,#175230,#175231,#175232,#175233,
#175234,#175235,#175236,#175237,#175238,#175239,#175240,#175241,#175242,
#175243,#175244,#175245,#175246,#175247,#175248,#175249,#175250,#175251,
#175252,#175253,#175254,#175255,#175256,#175257,#175258,#175259,#175260,
#175261,#175262,#175263,#175264,#175265,#175266,#175267,#175268,#175269,
#175270,#175271,#175272,#175273,#175274,#175275,#175276,#175277,#175278,
#175279,#175280,#175281,#175282,#175283,#175284,#175285,#175286,#175287,
#175288,#175289,#175290,#175291,#175292,#175293,#175294,#175295,#175296,
#175297,#175298,#175299,#175300,#175301,#175302,#175303,#175304,#175305,
#175306,#175307,#175308,#175309,#175310,#175311,#175312,#175313,#175314,
#175315,#175316,#175317,#175318,#175319,#175320,#175321,#175322,#175323,
#175324,#175325,#175326,#175327,#175328,#175329,#175330,#175331,#175332,
#175333,#175334,#175335,#175336,#175337,#175338,#175339,#175340,#175341,
#175342,#175343,#175344,#175345,#175346,#175347,#175348,#175349,#175350,
#175351,#175352,#175353,#175354,#175355,#175356,#175357,#175358,#175359,
#175360,#175361,#175362,#175363,#175364,#175365,#175366,#175367,#175368,
#175369,#175370,#175371,#175372,#175373,#175374,#175375,#175376,#175377),
 .UNSPECIFIED.,.F.,.F.,(4,2,2,2,2,2,2,2,2,2,2,2,2,2,2,2,2,2,2,2,2,2,2,2,
2,2,2,2,2,2,2,2,2,2,2,2,2,2,2,2,2,2,2,2,2,2,2,2,2,2,2,2,2,2,2,2,2,2,2,2,
2,2,2,2,2,2,2,2,2,2,2,2,2,2,2,2,2,2,2,2,2,2,2,2,2,2,2,2,2,2,2,2,2,2,2,2,
2,2,2,2,2,2,2,2,2,2,2,2,2,2,2,2,2,2,2,2,2,2,2,2,2,2,2,2,2,2,2,2,2,2,2,2,
2,2,2,2,2,2,2,2,2,2,2,2,2,2,2,2,2,2,2,2,2,2,2,2,2,2,2,2,2,2,2,2,2,2,2,2,
2,2,2,2,2,2,2,2,2,2,2,2,2,2,2,2,2,2,2,2,2,2,2,2,2,2,2,2,2,2,2,2,2,2,2,2,
2,2,2,2,2,2,2,2,2,2,2,2,2,2,2,2,2,2,2,2,2,2,2,2,2,2,2,2,2,2,2,2,2,2,2,2,
2,2,2,2,2,2,2,2,2,2,2,2,2,2,2,2,2,2,2,2,2,2,2,2,2,2,2,4),(0.00186199678217356,
0.0534072979824111,0.0629898090321268,0.0695601494279824,0.0751767148818409,
0.081119914342048,0.0882323224250048,0.108582833537339,0.120014112296188,
0.203904176637935,0.250671400770191,0.272139577502702,0.273284294429323,
0.274372228732696,0.275421424796998,0.28528162156847,0.295223186251498,
0.308477269692847,0.33651753295084,0.431316100633483,0.455932033728342,
0.467580263714209,0.476973769804133,0.482500531018475,0.487972346737579,
0.4945887990737,0.510873655122722,0.610289448462213,0.660207728472387,0.766253107149157,
0.792238054434032,0.803560964927062,0.815072251199551,0.825684800096252,
0.840229596362484,0.879090724950023,1.00301836409177,1.16210646173142,1.23756629235987,
1.25810633829328,1.26645302392921,1.27268951732162,1.27557748692769,1.27775685346682,
1.27980775996973,1.28265112476593,1.28997396512792,1.41279317645232,1.52105185422502,
1.69582821530593,1.70435400707048,1.70823872164865,1.71115880351145,1.71389916748984,
1.71768619160247,1.72736823423339,1.87816109685742,1.95516211163061,2.11858483014467,
2.12426447842029,2.12878884687946,2.13148577607152,2.13351329618611,2.13607255430391,
2.1404260284835,2.15550520917435,2.15747627858046,2.17616517692931,2.21389904244859,
2.32342555704627,2.46812510259257,2.48680693445919,2.50181511942128,2.50964131649009,
2.51620535040733,2.52245013671291,2.53278012677793,2.55973231510332,2.74841402331646,
2.873114803034,2.88870314273191,2.89291871757978,2.89544723103635,2.89770390617979,
2.90055083225084,2.90606143705936,2.94070146978887,3.14963064321459,3.30360678583918,
3.31204459005846,3.31591247137814,3.3188295461504,3.32157413169692,3.32537815969253,
3.33516397015224,3.49316497869749,3.57607230090745,3.67668993474441,3.69985539312709,
3.72796268969078,3.74414131525996,3.74828426164853,3.75072678303652,3.75288041094717,
3.75556263903683,3.75969819528162,3.77853987043052,4.00154252461507,4.09065663081161,
4.17489935622442,4.19790193134568,4.21085880797874,4.22211801530399,4.23609854206547,
4.2631543396556,4.45156081044648,4.50267536253318,4.52199090878683,4.53620024361153,
4.54288460809449,4.54844502206459,4.55543249288046,4.56658636389042,4.63221635151138,
4.68498349709671,4.71827272971454,4.73235048010506,4.74297760046393,4.7545960508579,
4.77391251574424,4.87686220568772,4.93135915160501,4.94442023131774,4.95099951915212,
4.95697812575695,4.96479371962575,4.97820825493997,5.04856759527427,5.11385388301294,
5.17705707378499,5.19722334136655,5.21383241490362,5.23168332090402,5.26535862352199,
5.29572252496139,5.33867414986147,5.35238743352054,5.36533766955413,5.39789401081938,
5.45766394357715,5.48155591903656,5.49820056457008,5.5163916527567,5.54860467717707,
5.58925602725705,5.71820743358845,5.73942154051105,5.74726212401161,5.75289030180623,
5.75888748102626,5.76801484153087,5.80272905916415,5.89390196145271,5.93893469869855,
5.95497420334539,5.96483716868131,5.97566020513873,5.99097636918636,6.03419831920534,
6.12597397133509,6.14732351179798,6.15483762352221,6.16016213165038,6.16581649880847,
6.17431904181378,6.2007947281686,6.35067156021419,6.38480538282014,6.45549630701774,
6.47570277153914,6.48808666366836,6.49945279733003,6.51443249269318,6.54830479557834,
6.72600471931166,6.82483162071745,6.9430956073783,6.94961596574745,6.95229720944739,
6.95450724002338,6.95674978735377,6.95998194976302,6.96828806985215,7.1265360373614,
7.21853174650482,7.37086070386074,7.38061188920959,7.38441023446956,7.38715339001454,
7.39007142252451,7.3939447849756,7.40241128529133,7.56334721790338,7.73852412333251,
7.79888961203032,7.80513076217893,7.80805399045748,7.81032643284637,7.81278860423803,
7.81532062805158,7.82296003664465,7.83380438231452,7.97204126044276,8.14589521011125,
8.17305740099466,8.18341283674055,8.18966211179188,8.19557021959188,8.20267129028787,
8.21529299392772,8.23072956420941,8.36777838079023,8.53969866739713,8.55793286765043,
8.56716912042244,8.57074506539148,8.5728938704501,8.57517246422569,8.57818675319267,
8.58460735667885,8.63391710960613,8.74802283071234,8.82531502385275,8.97843621313215,
8.98813079430965,8.99191974870661,8.99466048371041,8.99758000590887,9.00146234191693,
9.00997636464759,9.18113179060977,9.28168368875777,9.41381921510857,9.42265232114481,
9.4260740300293,9.4281275422882,9.43030537944654,9.43318405168816,9.43634545633717,
9.45187636663706,9.5049671831726,9.63864459027471,9.70180423477838,9.83478022474929,
9.86854322981692,9.88334565242782,9.8947232432244,9.90520541755825,9.91726476300876,
9.93440758216976,10.0757893204251,10.0782104616455,10.130921252948,10.2026985925259,
10.2141748651263,10.2201503452187,10.2233006616878,10.2246888159593),
 .UNSPECIFIED.);
#3235=B_SPLINE_CURVE_WITH_KNOTS('',3,(#175379,#175380,#175381,#175382,#175383,
#175384,#175385,#175386,#175387,#175388,#175389,#175390,#175391,#175392,
#175393,#175394,#175395,#175396,#175397,#175398,#175399,#175400,#175401,
#175402,#175403,#175404,#175405,#175406,#175407,#175408,#175409,#175410,
#175411,#175412,#175413,#175414,#175415,#175416,#175417,#175418,#175419,
#175420,#175421,#175422,#175423,#175424,#175425,#175426,#175427,#175428,
#175429,#175430,#175431,#175432,#175433,#175434,#175435,#175436,#175437,
#175438,#175439,#175440,#175441,#175442,#175443,#175444,#175445,#175446,
#175447,#175448,#175449,#175450,#175451,#175452,#175453,#175454,#175455,
#175456,#175457,#175458,#175459,#175460,#175461,#175462,#175463,#175464,
#175465,#175466,#175467,#175468,#175469,#175470,#175471,#175472,#175473,
#175474,#175475,#175476,#175477,#175478,#175479,#175480,#175481,#175482,
#175483,#175484,#175485,#175486,#175487,#175488,#175489,#175490,#175491,
#175492,#175493,#175494,#175495,#175496,#175497,#175498,#175499,#175500,
#175501,#175502,#175503,#175504,#175505,#175506,#175507,#175508,#175509,
#175510,#175511,#175512,#175513,#175514,#175515,#175516,#175517,#175518,
#175519,#175520,#175521,#175522,#175523,#175524,#175525,#175526,#175527,
#175528,#175529,#175530,#175531,#175532,#175533,#175534,#175535,#175536,
#175537,#175538,#175539,#175540,#175541,#175542,#175543,#175544,#175545,
#175546,#175547,#175548,#175549,#175550,#175551,#175552,#175553,#175554,
#175555,#175556,#175557,#175558,#175559,#175560,#175561,#175562,#175563,
#175564,#175565,#175566,#175567,#175568,#175569,#175570,#175571,#175572,
#175573,#175574,#175575,#175576,#175577,#175578,#175579,#175580,#175581,
#175582,#175583,#175584,#175585,#175586,#175587,#175588,#175589,#175590,
#175591,#175592,#175593,#175594,#175595,#175596,#175597,#175598,#175599,
#175600,#175601,#175602,#175603,#175604,#175605,#175606,#175607,#175608,
#175609,#175610,#175611,#175612,#175613,#175614,#175615,#175616,#175617,
#175618,#175619,#175620,#175621,#175622,#175623,#175624,#175625,#175626,
#175627,#175628,#175629,#175630,#175631,#175632,#175633,#175634,#175635,
#175636,#175637,#175638,#175639,#175640,#175641,#175642,#175643,#175644,
#175645,#175646,#175647,#175648,#175649,#175650,#175651,#175652,#175653,
#175654,#175655,#175656,#175657,#175658,#175659,#175660,#175661,#175662,
#175663,#175664,#175665,#175666,#175667,#175668,#175669,#175670,#175671,
#175672,#175673,#175674,#175675,#175676,#175677,#175678,#175679,#175680,
#175681,#175682,#175683,#175684,#175685,#175686,#175687,#175688,#175689,
#175690,#175691,#175692,#175693,#175694,#175695,#175696,#175697,#175698,
#175699,#175700,#175701,#175702,#175703,#175704,#175705,#175706,#175707,
#175708,#175709,#175710,#175711,#175712,#175713,#175714,#175715,#175716,
#175717,#175718,#175719,#175720,#175721,#175722,#175723,#175724,#175725,
#175726,#175727,#175728,#175729,#175730,#175731,#175732,#175733,#175734,
#175735,#175736,#175737,#175738,#175739,#175740,#175741,#175742,#175743,
#175744,#175745,#175746,#175747,#175748,#175749,#175750,#175751,#175752,
#175753,#175754,#175755,#175756,#175757,#175758,#175759,#175760,#175761,
#175762,#175763,#175764,#175765,#175766,#175767,#175768,#175769,#175770,
#175771,#175772,#175773,#175774,#175775,#175776,#175777,#175778,#175779,
#175780,#175781,#175782,#175783,#175784,#175785,#175786,#175787,#175788,
#175789,#175790,#175791,#175792,#175793,#175794,#175795,#175796,#175797,
#175798,#175799,#175800,#175801,#175802,#175803,#175804,#175805,#175806,
#175807,#175808,#175809,#175810,#175811,#175812,#175813,#175814,#175815,
#175816,#175817,#175818,#175819,#175820,#175821,#175822,#175823,#175824,
#175825,#175826,#175827,#175828,#175829,#175830,#175831,#175832,#175833,
#175834,#175835,#175836,#175837,#175838,#175839,#175840,#175841,#175842,
#175843,#175844,#175845,#175846,#175847,#175848,#175849,#175850,#175851,
#175852,#175853,#175854,#175855,#175856,#175857,#175858,#175859,#175860,
#175861,#175862,#175863,#175864,#175865,#175866,#175867,#175868,#175869,
#175870,#175871,#175872,#175873,#175874,#175875,#175876,#175877,#175878,
#175879,#175880,#175881,#175882,#175883,#175884,#175885,#175886,#175887,
#175888,#175889,#175890,#175891,#175892,#175893,#175894,#175895,#175896,
#175897,#175898,#175899,#175900,#175901,#175902,#175903,#175904,#175905,
#175906,#175907,#175908,#175909,#175910,#175911,#175912,#175913,#175914,
#175915,#175916,#175917,#175918,#175919,#175920,#175921,#175922,#175923,
#175924,#175925,#175926,#175927,#175928,#175929,#175930,#175931,#175932,
#175933,#175934,#175935,#175936,#175937,#175938,#175939,#175940,#175941,
#175942,#175943,#175944,#175945,#175946),.UNSPECIFIED.,.F.,.F.,(4,2,2,2,
2,2,2,2,2,2,2,2,2,2,2,2,2,2,2,2,2,2,2,2,2,2,2,2,2,2,2,2,2,2,2,2,2,2,2,2,
2,2,2,2,2,2,2,2,2,2,2,2,2,2,2,2,2,2,2,2,2,2,2,2,2,2,2,2,2,2,2,2,2,2,2,2,
2,2,2,2,2,2,2,2,2,2,2,2,2,2,2,2,2,2,2,2,2,2,2,2,2,2,2,2,2,2,2,2,2,2,2,2,
2,2,2,2,2,2,2,2,2,2,2,2,2,2,2,2,2,2,2,2,2,2,2,2,2,2,2,2,2,2,2,2,2,2,2,2,
2,2,2,2,2,2,2,2,2,2,2,2,2,2,2,2,2,2,2,2,2,2,2,2,2,2,2,2,2,2,2,2,2,2,2,2,
2,2,2,2,2,2,2,2,2,2,2,2,2,2,2,2,2,2,2,2,2,2,2,2,2,2,2,2,2,2,2,2,2,2,2,2,
2,2,2,2,2,2,2,2,2,2,2,2,2,2,2,2,2,2,2,2,2,2,2,2,2,2,2,2,2,2,2,2,2,2,2,2,
2,2,2,2,2,2,2,2,2,2,2,2,2,2,2,2,2,2,2,2,2,2,2,2,2,2,2,4),(0.00188190206533328,
0.00394021362682194,0.00859255636028643,0.0192593108961252,0.0763073776529958,
0.13039204283185,0.169294902247269,0.181048040623909,0.190948316303338,
0.201514682354913,0.215072105645199,0.24468029956132,0.33646633764414,0.37325433031622,
0.388089829256446,0.396316335471121,0.402008134682251,0.407631898860544,
0.41333215793546,0.421447689260994,0.444585169692429,0.571292694284215,
0.611756096805257,0.621064326911909,0.626383090426756,0.629608099546713,
0.631433580688767,0.633723600211907,0.635549775856493,0.636984939885039,
0.638099289844188,0.638956115619663,0.639609811136581,0.655217908181767,
0.670970293096031,0.689956399348377,0.736273085148862,0.774843265168787,
0.798067317351602,0.809276671969745,0.823393418882983,0.867810357299684,
0.924145869669683,0.940207667926138,0.954967542592683,0.97419169732368,
1.01241387708126,1.12796747826932,1.16867623363583,1.18535156836009,1.19466719712562,
1.20113402152816,1.20674535197142,1.21271936258327,1.22008102801901,1.24238664980676,
1.31661522242514,1.36534685560889,1.38771851572256,1.40579596117075,1.41569901214977,
1.42538064937492,1.43811426835037,1.4624073585641,1.54933480888982,1.59755983691416,
1.60774331583143,1.61307769051002,1.61829702453316,1.6253205419314,1.64061451933967,
1.76875418237282,1.86032773109508,1.8962906893597,1.92355280407125,1.93486202201446,
1.94636558129077,1.95698804989473,1.97157338927446,2.00176953722281,2.12630672902658,
2.23993389259797,2.36123028584463,2.39766834475812,2.40382249096465,2.40673334814975,
2.40891631772271,2.4109606576616,2.41377921658978,2.41942082491633,2.49461972866057,
2.64569242208153,2.82703154397473,2.835575305209,2.83946328527691,2.8423838006839,
2.84512309637037,2.84890631420152,2.85856616420846,3.00596244379951,3.16599919944367,
3.24404448987258,3.25694787007714,3.26088798024286,3.26335499830134,3.26562622589582,
3.26854062568793,3.27332438101888,3.29982333355065,3.46299596640571,3.55027865537353,
3.6205775003343,3.6342887330012,3.64196274858779,3.64849189093521,3.65589402960894,
3.66834956363616,3.71248765073057,3.75167699345357,3.82050701850602,3.90111983843628,
4.00577542185636,4.01524398632385,4.02222494379172,4.02531871996827,4.02761033249559,
4.02973602398435,4.03263515997484,4.0383433526799,4.10475750941039,4.25406004791312,
4.4239570695574,4.4403738408984,4.44540624053903,4.44856092631052,4.45146742589732,
4.45519910434056,4.46131853482933,4.49473268794736,4.78254012027149,4.86371722699902,
4.87643753794344,4.88024766622227,4.88261618216237,4.88478520008413,4.88759891162846,
4.89350437599001,4.93618641792744,5.11408454039127,5.28591262776393,5.32154040317637,
5.3356913067907,5.34725807638374,5.35903874373822,5.37634481016825,5.42561552312411,
5.54737889030724,5.59345699241652,5.64874871993721,5.66584711736607,5.67260176558865,
5.67820532253348,5.68438899738462,5.69469923302105,5.74710161830624,5.84130773624172,
5.85929414249924,5.86950537565795,5.88012537562142,5.89411664934785,5.92641219551067,
5.97461979844949,6.04585903950909,6.07122786329442,6.07894089839188,6.08436165927916,
6.09056584153224,6.09973477018372,6.1259617990716,6.15069112060431,6.22838161100326,
6.3058878893645,6.32965232916615,6.34621240367765,6.36419669778839,6.39908343992429,
6.47025454937043,6.48414476414463,6.49697452545205,6.52787592629551,6.58747888407595,
6.61248395614754,6.62926707273742,6.64714617489393,6.67759380475321,6.78292088530635,
6.86035494872068,6.87365418039129,6.88143944712878,6.88741509808642,6.89401725735288,
6.90720959851432,6.92530419994896,6.9771355598698,7.06132736608888,7.08213927786219,
7.09418175483623,7.10462687852032,7.11789222589014,7.14598535119953,7.18626007253536,
7.22913279705064,7.27579414277792,7.28596129674123,7.2915079086961,7.29652101487956,
7.3037656569116,7.32117059646132,7.3464049971747,7.46707325528123,7.5841775558822,
7.60610010136548,7.61897772187771,7.63024971760534,7.64435727239795,7.67321145775631,
7.79402629132358,7.96772044760927,8.07551532636859,8.08221781876246,8.08488595778167,
8.08709310913079,8.08934072673616,8.0925945809095,8.10103555068788,8.25914363427256,
8.47633848470989,8.50868295190553,8.51473707560164,8.51844966251296,8.5213539394339,
8.52445540843903,8.52936040052161,8.53512389444153,8.54605109495126,8.6440613137291,
8.76895956265577,8.92724585772357,8.93653949457682,8.94012794504473,8.9422781867819,
8.94455608695947,8.94756279957616,8.95407144357245,9.09339671263441,9.21559569567429,
9.29718064547672,9.31196046140954,9.31984406107301,9.32640851503893,9.33352024462134,
9.34463967878358,9.38044694322873,9.43611586327997,9.57602308524526,9.69437094429324,
9.70062017611394,9.70365083835392,9.70581172726951,9.70808537828086,9.71106351264648,
9.71742103396116,9.81172048805468,10.0261267527293,10.0423886006616,10.1137206403557,
10.1213803219175,10.1251783738698,10.1279219944405,10.1306892248764,10.1335219851595,
10.1371966236365,10.1429500464066,10.2269540975582),.UNSPECIFIED.);
#3236=B_SPLINE_CURVE_WITH_KNOTS('',3,(#175948,#175949,#175950,#175951,#175952,
#175953,#175954,#175955,#175956,#175957,#175958,#175959,#175960,#175961,
#175962,#175963,#175964,#175965,#175966,#175967,#175968,#175969,#175970,
#175971,#175972,#175973,#175974,#175975,#175976,#175977,#175978,#175979,
#175980,#175981,#175982,#175983,#175984,#175985,#175986,#175987,#175988,
#175989,#175990,#175991,#175992,#175993,#175994,#175995,#175996,#175997,
#175998,#175999,#176000,#176001,#176002,#176003,#176004,#176005,#176006,
#176007,#176008,#176009,#176010,#176011,#176012,#176013,#176014,#176015,
#176016,#176017,#176018,#176019,#176020,#176021,#176022,#176023,#176024,
#176025,#176026,#176027,#176028,#176029,#176030,#176031,#176032,#176033,
#176034,#176035,#176036,#176037,#176038,#176039,#176040,#176041,#176042,
#176043,#176044,#176045,#176046,#176047,#176048,#176049,#176050,#176051,
#176052,#176053,#176054,#176055,#176056,#176057,#176058,#176059,#176060,
#176061,#176062,#176063,#176064,#176065,#176066,#176067,#176068,#176069,
#176070,#176071,#176072,#176073,#176074,#176075,#176076,#176077,#176078,
#176079,#176080,#176081,#176082,#176083,#176084,#176085,#176086,#176087,
#176088,#176089,#176090,#176091,#176092,#176093,#176094,#176095,#176096,
#176097,#176098,#176099,#176100,#176101,#176102,#176103,#176104,#176105,
#176106,#176107,#176108,#176109,#176110,#176111,#176112,#176113,#176114,
#176115,#176116,#176117,#176118,#176119,#176120,#176121,#176122,#176123,
#176124,#176125,#176126,#176127,#176128,#176129,#176130,#176131,#176132,
#176133,#176134,#176135,#176136,#176137,#176138,#176139,#176140,#176141,
#176142,#176143,#176144,#176145,#176146,#176147,#176148,#176149,#176150,
#176151,#176152,#176153,#176154,#176155,#176156,#176157,#176158,#176159,
#176160,#176161,#176162,#176163,#176164,#176165,#176166,#176167,#176168,
#176169,#176170,#176171,#176172,#176173,#176174,#176175,#176176,#176177,
#176178,#176179,#176180,#176181,#176182,#176183,#176184,#176185,#176186,
#176187,#176188,#176189,#176190,#176191,#176192,#176193,#176194,#176195,
#176196,#176197,#176198,#176199,#176200,#176201,#176202,#176203),
 .UNSPECIFIED.,.F.,.F.,(4,3,3,3,3,3,3,3,3,3,3,3,3,3,3,3,3,3,3,3,3,3,3,3,
3,3,3,3,3,3,3,3,3,3,3,3,3,3,3,3,3,3,3,3,3,3,3,3,3,3,3,3,3,3,3,3,3,3,3,3,
3,3,3,3,3,3,3,3,3,3,3,3,3,3,3,3,3,3,3,3,3,3,3,3,3,4),(197.920337176157,
197.994164212812,198.067915796059,198.141589609895,198.21521846511,198.288810978896,
198.333746057302,198.409488422125,198.485276542875,198.561119713718,198.637074671978,
198.713091104313,198.789226899813,198.83221460061,198.908425181084,198.984567785336,
199.060652871676,199.136690857949,199.212692128503,199.289749573344,199.365714835468,
199.441676427333,199.517643754394,199.595520737602,199.671550535035,199.75035111113,
199.829151687225,199.900574962075,199.971945088988,200.043275660509,200.114588997995,
200.185889684817,200.257215166309,200.327620230533,200.415325719874,200.503502082292,
200.59210649291,200.680806799793,200.769403059729,200.82608877384,200.89905821829,
200.971982209383,201.044873736124,201.117755935044,201.190630853087,201.263533802797,
201.324557317148,201.403858101098,201.483181031574,201.562523633586,201.641896710759,
201.721278391757,201.800675168866,201.823025860455,201.902423255123,201.981806928951,
202.061174380592,202.140519564404,202.21984258367,202.299136813291,202.321494403763,
202.394396804032,202.467276661077,202.54014693051,202.613043274915,202.6859519307,
202.758920243649,202.81996294707,202.908537278682,202.997237644155,203.085804456258,
203.174147869823,203.261917586448,203.318431490378,203.389754988728,203.461058738883,
203.532356242156,203.603688737803,203.675037096542,203.746457751509,203.816900033686,
203.903674402841,203.990284356058,204.076705714213,204.162709280465,204.203522318931),
 .UNSPECIFIED.);
#3237=B_SPLINE_CURVE_WITH_KNOTS('',3,(#176205,#176206,#176207,#176208,#176209,
#176210,#176211,#176212,#176213,#176214,#176215,#176216,#176217,#176218,
#176219),.UNSPECIFIED.,.F.,.F.,(4,1,1,1,1,1,1,1,1,1,1,1,4),(191.637151868978,
191.853654994304,192.850592080919,193.349060624227,193.847529167534,194.345997710842,
194.844466254149,195.342934797457,195.841403340765,196.339871884072,196.83834042738,
197.835277513995,197.920337176157),.UNSPECIFIED.);
#3238=B_SPLINE_CURVE_WITH_KNOTS('',3,(#176221,#176222,#176223,#176224,#176225,
#176226,#176227,#176228,#176229,#176230,#176231,#176232,#176233,#176234,
#176235,#176236,#176237,#176238,#176239,#176240,#176241,#176242,#176243,
#176244,#176245,#176246,#176247,#176248,#176249,#176250,#176251,#176252,
#176253,#176254,#176255,#176256,#176257,#176258,#176259,#176260,#176261,
#176262,#176263,#176264,#176265,#176266,#176267,#176268,#176269,#176270,
#176271,#176272,#176273,#176274,#176275,#176276,#176277,#176278,#176279,
#176280,#176281,#176282,#176283,#176284,#176285,#176286,#176287,#176288,
#176289,#176290,#176291,#176292,#176293,#176294,#176295,#176296,#176297,
#176298,#176299,#176300,#176301,#176302,#176303,#176304,#176305,#176306,
#176307,#176308,#176309,#176310,#176311,#176312,#176313,#176314,#176315,
#176316,#176317,#176318,#176319,#176320,#176321,#176322,#176323,#176324,
#176325,#176326,#176327,#176328,#176329,#176330,#176331,#176332,#176333,
#176334,#176335,#176336,#176337,#176338,#176339,#176340,#176341,#176342,
#176343,#176344,#176345,#176346,#176347,#176348,#176349,#176350,#176351,
#176352,#176353,#176354,#176355,#176356,#176357,#176358,#176359,#176360,
#176361,#176362,#176363,#176364,#176365,#176366,#176367,#176368,#176369,
#176370,#176371,#176372,#176373,#176374,#176375,#176376,#176377,#176378,
#176379,#176380,#176381,#176382,#176383,#176384,#176385,#176386,#176387,
#176388,#176389,#176390,#176391,#176392,#176393,#176394,#176395,#176396,
#176397,#176398,#176399,#176400,#176401,#176402,#176403,#176404,#176405,
#176406,#176407,#176408,#176409,#176410,#176411,#176412,#176413,#176414,
#176415,#176416,#176417,#176418,#176419,#176420,#176421,#176422,#176423,
#176424,#176425,#176426,#176427,#176428,#176429,#176430,#176431,#176432,
#176433,#176434,#176435,#176436,#176437,#176438,#176439,#176440,#176441,
#176442,#176443,#176444,#176445,#176446,#176447,#176448,#176449,#176450,
#176451,#176452,#176453,#176454,#176455,#176456,#176457,#176458,#176459,
#176460,#176461,#176462,#176463,#176464,#176465,#176466,#176467,#176468,
#176469,#176470,#176471,#176472,#176473,#176474,#176475,#176476),
 .UNSPECIFIED.,.F.,.F.,(4,3,3,3,3,3,3,3,3,3,3,3,3,3,3,3,3,3,3,3,3,3,3,3,
3,3,3,3,3,3,3,3,3,3,3,3,3,3,3,3,3,3,3,3,3,3,3,3,3,3,3,3,3,3,3,3,3,3,3,3,
3,3,3,3,3,3,3,3,3,3,3,3,3,3,3,3,3,3,3,3,3,3,3,3,3,4),(185.353968266458,
185.433608279155,185.513330531198,185.593129643172,185.673039876824,185.753001540758,
185.833039193569,185.872032474613,185.943456083504,186.014826544482,186.086157450001,
186.157471120795,186.228772140797,186.300097954107,186.370501017921,186.458205923838,
186.546381642246,186.634985357635,186.723684960917,186.812280540737,186.868969561229,
186.941939130312,187.014863246311,187.08775489816,187.1606372222,187.233512265437,
187.306415339985,187.367438104536,187.446738835565,187.526061712239,187.605404259861,
187.684777282415,187.764158908868,187.843555632021,187.865906647844,187.94530403915,
188.024687709446,188.104055157406,188.183400337357,188.262723352672,188.342017578244,
188.364375191151,188.437277603237,188.510157472198,188.583027753639,188.655924110162,
188.728832778134,188.801801103328,188.862843734459,188.951418041443,189.040118380849,
189.12868516653,189.217028554337,189.304798247261,189.361312277766,189.432635780675,
189.503939535424,189.575237043324,189.646569543641,189.717917907078,189.78933856677,
189.859780821074,189.935884316139,190.011937461231,190.087950650469,190.163934249335,
190.239898601634,190.317001014891,190.392972741875,190.468957068073,190.54496340868,
190.622902033432,190.699011071797,190.777864489743,190.856717907689,190.932850779911,
191.008890480957,191.084846486298,191.160704928803,191.236505992322,191.312245313017,
191.355186450997,191.426863904643,191.498550254089,191.570294990333,191.637151868978),
 .UNSPECIFIED.);
#3239=B_SPLINE_CURVE_WITH_KNOTS('',3,(#176478,#176479,#176480,#176481,#176482,
#176483,#176484,#176485,#176486,#176487,#176488,#176489,#176490,#176491,
#176492,#176493,#176494,#176495,#176496,#176497,#176498,#176499,#176500,
#176501,#176502,#176503,#176504,#176505,#176506,#176507,#176508,#176509,
#176510,#176511,#176512,#176513,#176514,#176515,#176516,#176517,#176518,
#176519,#176520,#176521,#176522,#176523,#176524,#176525,#176526,#176527,
#176528,#176529,#176530,#176531,#176532,#176533,#176534,#176535,#176536,
#176537,#176538,#176539,#176540,#176541,#176542,#176543,#176544,#176545,
#176546,#176547,#176548,#176549,#176550,#176551,#176552,#176553,#176554,
#176555,#176556,#176557,#176558,#176559,#176560,#176561,#176562,#176563,
#176564,#176565,#176566,#176567,#176568,#176569,#176570,#176571,#176572,
#176573,#176574,#176575,#176576,#176577,#176578,#176579,#176580,#176581,
#176582,#176583,#176584,#176585,#176586,#176587,#176588,#176589,#176590,
#176591,#176592,#176593,#176594,#176595,#176596,#176597,#176598,#176599,
#176600,#176601,#176602,#176603,#176604,#176605,#176606,#176607,#176608,
#176609,#176610,#176611,#176612,#176613,#176614,#176615,#176616,#176617,
#176618,#176619,#176620,#176621,#176622,#176623,#176624,#176625,#176626,
#176627,#176628,#176629,#176630,#176631,#176632,#176633,#176634,#176635,
#176636,#176637,#176638,#176639,#176640,#176641,#176642,#176643,#176644,
#176645,#176646,#176647,#176648,#176649,#176650,#176651,#176652,#176653,
#176654,#176655,#176656,#176657,#176658,#176659,#176660,#176661,#176662,
#176663,#176664,#176665,#176666,#176667,#176668,#176669,#176670,#176671,
#176672,#176673,#176674,#176675,#176676,#176677,#176678,#176679,#176680,
#176681,#176682,#176683,#176684,#176685,#176686,#176687,#176688,#176689,
#176690,#176691,#176692,#176693,#176694,#176695,#176696,#176697,#176698,
#176699,#176700,#176701,#176702,#176703,#176704,#176705,#176706,#176707,
#176708,#176709,#176710,#176711,#176712,#176713,#176714,#176715,#176716,
#176717,#176718,#176719,#176720,#176721,#176722,#176723,#176724,#176725,
#176726,#176727,#176728,#176729,#176730,#176731,#176732,#176733),
 .UNSPECIFIED.,.F.,.F.,(4,3,3,3,3,3,3,3,3,3,3,3,3,3,3,3,3,3,3,3,3,3,3,3,
3,3,3,3,3,3,3,3,3,3,3,3,3,3,3,3,3,3,3,3,3,3,3,3,3,3,3,3,3,3,3,3,3,3,3,3,
3,3,3,3,3,3,3,3,3,3,3,3,3,3,3,3,3,3,3,3,3,3,3,3,3,4),(179.071060446364,
179.140082435305,179.209090416259,179.278088452461,179.347109745067,179.391941411615,
179.478877889249,179.566207692725,179.653898138385,179.74167150702,179.829365837672,
179.890409954923,179.963618397179,180.03678211922,180.109913970165,180.183036814402,
180.256152680139,180.329296142636,180.38887849823,180.468009009373,180.547158375392,
180.626325060468,180.705520759866,180.784724865077,180.863945321648,180.887347041538,
180.966805552748,181.04625110072,181.125680838219,181.205088211607,181.284473109547,
181.363828276015,181.385815584845,181.458712668952,181.53158721015,181.604452166954,
181.677343218298,181.750246588051,181.823209649975,181.884284128153,181.972844519505,
182.061529962692,182.150081408985,182.238409708929,182.326165309575,182.382752671461,
182.454080858286,182.525389340606,182.59669161852,182.66802894482,182.739382169653,
182.810807728317,182.881221214768,182.957322968518,183.033374332627,183.109385705406,
183.185367456511,183.261329933897,183.338433479833,183.414403285331,183.490385678004,
183.566390076668,183.644332132847,183.720439231401,183.799298766392,183.878158301383,
183.954292780035,184.030334077574,184.106291666431,184.182151666093,184.257954270009,
184.333695099835,184.376626844691,184.452368681572,184.528156266499,184.603998894723,
184.679953303427,184.755969182361,184.832104422473,184.875095387998,184.955360700984,
185.035527324997,185.115534876663,185.195441645898,185.275182204737,185.353966561798),
 .UNSPECIFIED.);
#3240=B_SPLINE_CURVE_WITH_KNOTS('',3,(#176735,#176736,#176737,#176738,#176739,
#176740,#176741,#176742,#176743,#176744,#176745,#176746,#176747,#176748,
#176749,#176750,#176751,#176752),.UNSPECIFIED.,.F.,.F.,(4,2,2,2,2,2,2,2,
4),(172.787615115558,173.616953723877,174.446311500315,175.275669276753,
176.105027053191,176.934384829629,177.763742606067,178.593100382505,179.070559707459),
 .UNSPECIFIED.);
#3241=B_SPLINE_CURVE_WITH_KNOTS('',3,(#176754,#176755,#176756,#176757,#176758,
#176759,#176760,#176761,#176762,#176763,#176764,#176765,#176766,#176767,
#176768,#176769,#176770,#176771,#176772,#176773,#176774,#176775,#176776,
#176777,#176778,#176779,#176780,#176781,#176782,#176783,#176784,#176785,
#176786,#176787,#176788,#176789,#176790,#176791,#176792,#176793,#176794,
#176795,#176796,#176797,#176798,#176799,#176800,#176801,#176802,#176803,
#176804,#176805,#176806,#176807,#176808,#176809,#176810,#176811,#176812,
#176813,#176814,#176815,#176816,#176817,#176818,#176819,#176820,#176821,
#176822,#176823,#176824,#176825,#176826,#176827,#176828,#176829,#176830,
#176831,#176832,#176833,#176834,#176835,#176836,#176837,#176838,#176839,
#176840,#176841,#176842,#176843,#176844,#176845,#176846,#176847,#176848,
#176849,#176850,#176851,#176852,#176853,#176854,#176855,#176856,#176857,
#176858,#176859,#176860,#176861,#176862,#176863,#176864,#176865,#176866,
#176867,#176868,#176869,#176870,#176871,#176872,#176873,#176874,#176875,
#176876,#176877,#176878,#176879,#176880,#176881,#176882,#176883,#176884,
#176885,#176886,#176887,#176888,#176889,#176890,#176891,#176892,#176893,
#176894,#176895,#176896,#176897,#176898,#176899,#176900,#176901,#176902,
#176903,#176904,#176905,#176906,#176907,#176908,#176909,#176910,#176911,
#176912,#176913,#176914,#176915,#176916,#176917,#176918,#176919,#176920,
#176921,#176922,#176923,#176924,#176925,#176926,#176927,#176928,#176929,
#176930,#176931,#176932,#176933,#176934,#176935,#176936,#176937,#176938,
#176939,#176940,#176941,#176942,#176943,#176944,#176945,#176946,#176947,
#176948,#176949,#176950,#176951,#176952,#176953,#176954,#176955,#176956,
#176957,#176958,#176959,#176960,#176961,#176962,#176963,#176964,#176965,
#176966,#176967,#176968,#176969,#176970,#176971,#176972,#176973,#176974,
#176975,#176976,#176977,#176978,#176979,#176980,#176981,#176982,#176983,
#176984,#176985,#176986,#176987,#176988,#176989,#176990,#176991,#176992,
#176993,#176994,#176995,#176996,#176997,#176998,#176999,#177000,#177001,
#177002,#177003,#177004,#177005,#177006,#177007,#177008,#177009,#177010,
#177011,#177012),.UNSPECIFIED.,.F.,.F.,(4,3,3,3,3,3,3,3,3,3,3,3,3,3,3,3,
3,3,3,3,3,3,3,3,3,3,3,3,3,3,3,3,3,3,3,3,3,3,3,3,3,3,3,3,3,3,3,3,3,3,3,3,
3,3,3,3,3,3,3,3,3,3,3,3,3,3,3,3,3,3,3,3,3,3,3,3,3,3,3,3,3,3,3,3,3,3,4),
(166.50441064026,166.591077657514,166.678165952141,166.765382727969,166.852612902676,
166.930227828926,167.004952485645,167.07962597182,167.154259832905,167.228868307067,
167.303460981558,167.3780613422,167.428696372234,167.504955810607,167.581218455649,
167.657492989338,167.733812277222,167.810154807913,167.886556388693,167.927164915541,
168.009045625696,168.090907992134,168.174589358813,168.256321060986,168.340977259917,
168.425633458849,168.500342464523,168.575047121226,168.649758778482,168.724515678092,
168.799296472705,168.874146305281,168.924102002156,168.999080317636,169.074001238328,
169.148877146241,169.223720393406,169.298543309392,169.376355281814,169.451193529657,
169.526049886415,169.600935534566,169.67586167053,169.750877546777,169.825946010883,
169.901113334991,169.921039088772,169.993549286924,170.065971833029,170.138321444504,
170.210612766232,170.282860386779,170.35507885297,170.42729625324,170.499516401872,
170.571752443362,170.644017533473,170.716368450606,170.788765235898,170.861274470341,
170.917976175387,170.992828246169,171.067594179148,171.142286845693,171.216919070322,
171.291503638633,171.369429841554,171.44396293689,171.518490023338,171.593022627302,
171.66757227602,171.74217856016,171.816817859411,171.891530059673,171.914913262002,
171.991308989042,172.067640616653,172.143917021567,172.220137494927,172.296323925243,
172.37248297344,172.413381805309,172.489576062331,172.565831662664,172.642117280169,
172.718482558834,172.787248854564),.UNSPECIFIED.);
#3242=B_SPLINE_CURVE_WITH_KNOTS('',3,(#177014,#177015,#177016,#177017,#177018,
#177019,#177020,#177021,#177022,#177023,#177024,#177025,#177026,#177027,
#177028,#177029,#177030,#177031),.UNSPECIFIED.,.F.,.F.,(4,2,2,2,2,2,2,2,
4),(160.22122533308,161.050583109518,161.879940885956,162.709298662394,
163.538656438832,164.36801421527,165.197371991708,166.026729768145,166.50441064026),
 .UNSPECIFIED.);
#3243=B_SPLINE_CURVE_WITH_KNOTS('',3,(#177033,#177034,#177035,#177036,#177037,
#177038,#177039,#177040,#177041,#177042,#177043,#177044,#177045,#177046,
#177047,#177048,#177049,#177050,#177051,#177052,#177053,#177054,#177055,
#177056,#177057,#177058,#177059,#177060,#177061,#177062,#177063,#177064,
#177065,#177066,#177067,#177068,#177069,#177070,#177071,#177072,#177073,
#177074,#177075,#177076,#177077,#177078,#177079,#177080,#177081,#177082,
#177083,#177084,#177085,#177086,#177087,#177088,#177089,#177090,#177091,
#177092,#177093,#177094,#177095,#177096,#177097,#177098,#177099,#177100,
#177101,#177102,#177103,#177104,#177105,#177106,#177107,#177108,#177109,
#177110,#177111,#177112,#177113,#177114,#177115,#177116,#177117,#177118,
#177119,#177120,#177121,#177122,#177123,#177124,#177125,#177126,#177127,
#177128,#177129,#177130,#177131,#177132,#177133,#177134,#177135,#177136,
#177137,#177138,#177139,#177140,#177141,#177142,#177143,#177144,#177145,
#177146,#177147,#177148,#177149,#177150,#177151,#177152,#177153,#177154,
#177155,#177156,#177157,#177158,#177159,#177160,#177161,#177162,#177163,
#177164,#177165,#177166,#177167,#177168,#177169,#177170,#177171,#177172,
#177173,#177174,#177175,#177176,#177177,#177178,#177179,#177180,#177181,
#177182,#177183,#177184,#177185,#177186,#177187,#177188,#177189,#177190,
#177191,#177192,#177193,#177194,#177195,#177196,#177197,#177198,#177199,
#177200,#177201,#177202,#177203,#177204,#177205,#177206,#177207,#177208,
#177209,#177210,#177211,#177212,#177213,#177214,#177215,#177216,#177217,
#177218,#177219,#177220,#177221,#177222,#177223,#177224,#177225,#177226,
#177227,#177228,#177229,#177230,#177231,#177232,#177233,#177234,#177235,
#177236,#177237,#177238,#177239,#177240,#177241,#177242,#177243,#177244,
#177245,#177246,#177247,#177248,#177249,#177250,#177251,#177252,#177253,
#177254,#177255,#177256,#177257,#177258,#177259,#177260,#177261,#177262,
#177263,#177264,#177265,#177266,#177267,#177268,#177269,#177270,#177271,
#177272,#177273,#177274,#177275,#177276,#177277,#177278,#177279,#177280,
#177281,#177282,#177283,#177284,#177285,#177286,#177287,#177288,#177289,
#177290,#177291,#177292,#177293,#177294,#177295,#177296,#177297,#177298,
#177299,#177300,#177301,#177302,#177303,#177304,#177305,#177306,#177307,
#177308,#177309,#177310,#177311,#177312,#177313,#177314,#177315,#177316,
#177317,#177318,#177319,#177320,#177321,#177322,#177323,#177324,#177325,
#177326,#177327,#177328,#177329,#177330,#177331,#177332,#177333,#177334,
#177335,#177336,#177337,#177338,#177339,#177340,#177341,#177342,#177343,
#177344,#177345,#177346,#177347,#177348,#177349,#177350,#177351,#177352,
#177353,#177354,#177355,#177356,#177357,#177358,#177359,#177360,#177361,
#177362,#177363,#177364,#177365,#177366,#177367,#177368,#177369,#177370,
#177371,#177372,#177373,#177374,#177375,#177376,#177377,#177378,#177379,
#177380,#177381,#177382,#177383,#177384,#177385,#177386,#177387,#177388,
#177389,#177390,#177391,#177392,#177393,#177394,#177395,#177396,#177397,
#177398,#177399,#177400,#177401,#177402,#177403,#177404,#177405,#177406,
#177407,#177408,#177409,#177410,#177411,#177412,#177413,#177414,#177415,
#177416,#177417,#177418,#177419,#177420,#177421,#177422,#177423,#177424,
#177425,#177426,#177427,#177428,#177429,#177430,#177431,#177432,#177433,
#177434,#177435,#177436,#177437,#177438,#177439,#177440,#177441,#177442,
#177443,#177444,#177445,#177446,#177447,#177448,#177449,#177450,#177451,
#177452,#177453,#177454,#177455,#177456,#177457,#177458,#177459,#177460,
#177461,#177462,#177463,#177464,#177465,#177466,#177467,#177468,#177469,
#177470,#177471,#177472,#177473,#177474,#177475,#177476,#177477,#177478,
#177479,#177480,#177481,#177482,#177483,#177484,#177485,#177486,#177487,
#177488,#177489,#177490,#177491,#177492,#177493,#177494,#177495,#177496,
#177497,#177498,#177499,#177500,#177501,#177502,#177503,#177504,#177505,
#177506,#177507,#177508,#177509,#177510,#177511,#177512,#177513,#177514,
#177515,#177516,#177517,#177518,#177519,#177520,#177521,#177522,#177523,
#177524,#177525,#177526,#177527,#177528,#177529,#177530,#177531,#177532,
#177533,#177534,#177535,#177536,#177537,#177538,#177539,#177540,#177541,
#177542,#177543,#177544,#177545,#177546,#177547,#177548,#177549,#177550,
#177551,#177552,#177553,#177554,#177555,#177556,#177557,#177558,#177559,
#177560,#177561,#177562,#177563,#177564,#177565,#177566,#177567,#177568,
#177569,#177570,#177571,#177572,#177573,#177574,#177575,#177576,#177577,
#177578,#177579,#177580,#177581,#177582,#177583,#177584,#177585,#177586,
#177587,#177588,#177589,#177590,#177591,#177592,#177593,#177594,#177595,
#177596,#177597,#177598,#177599,#177600,#177601,#177602,#177603,#177604,
#177605,#177606,#177607,#177608,#177609,#177610,#177611,#177612,#177613,
#177614,#177615,#177616,#177617,#177618,#177619,#177620,#177621,#177622,
#177623,#177624,#177625,#177626,#177627,#177628,#177629,#177630,#177631,
#177632,#177633,#177634,#177635,#177636,#177637,#177638,#177639,#177640,
#177641,#177642,#177643,#177644,#177645,#177646,#177647,#177648,#177649,
#177650,#177651,#177652,#177653,#177654,#177655,#177656,#177657,#177658,
#177659,#177660,#177661,#177662,#177663,#177664,#177665,#177666,#177667,
#177668,#177669,#177670,#177671,#177672,#177673,#177674,#177675,#177676,
#177677,#177678,#177679,#177680,#177681,#177682,#177683,#177684,#177685,
#177686,#177687,#177688,#177689,#177690,#177691,#177692,#177693,#177694,
#177695,#177696,#177697,#177698,#177699,#177700,#177701,#177702,#177703,
#177704,#177705,#177706,#177707,#177708,#177709,#177710,#177711,#177712,
#177713,#177714,#177715,#177716,#177717,#177718,#177719,#177720,#177721,
#177722,#177723,#177724,#177725,#177726,#177727,#177728,#177729,#177730,
#177731,#177732,#177733,#177734,#177735,#177736,#177737,#177738),
 .UNSPECIFIED.,.F.,.F.,(4,2,2,2,2,2,2,2,2,2,2,2,2,2,2,2,2,2,2,2,2,2,2,2,
2,2,2,2,2,2,2,2,2,2,2,2,2,2,2,2,2,2,2,2,2,2,2,2,2,2,2,2,2,2,2,2,2,2,2,2,
2,2,2,2,2,2,2,2,2,2,2,2,2,2,2,2,2,2,2,2,2,2,2,2,2,2,2,2,2,2,2,2,2,2,2,2,
2,2,2,2,2,2,2,2,2,2,2,2,2,2,2,2,2,2,2,2,2,2,2,2,2,2,2,2,2,2,2,2,2,2,2,2,
2,2,2,2,2,2,2,2,2,2,2,2,2,2,2,2,2,2,2,2,2,2,2,2,2,2,2,2,2,2,2,2,2,2,2,2,
2,2,2,2,2,2,2,2,2,2,2,2,2,2,2,2,2,2,2,2,2,2,2,2,2,2,2,2,2,2,2,2,2,2,2,2,
2,2,2,2,2,2,2,2,2,2,2,2,2,2,2,2,2,2,2,2,2,2,2,2,2,2,2,2,2,2,2,2,2,2,2,2,
2,2,2,2,2,2,2,2,2,2,2,2,2,2,2,2,2,2,2,2,2,2,2,2,2,2,2,2,2,2,2,2,2,2,2,2,
2,2,2,2,2,2,2,2,2,2,2,2,2,2,2,2,2,2,2,2,2,2,2,2,2,2,2,2,2,2,2,2,2,2,2,2,
2,2,2,2,2,2,2,2,2,2,2,2,2,2,2,2,2,2,2,2,2,2,2,2,2,2,2,2,2,2,2,2,2,2,2,2,
2,2,2,2,4),(0.00175465339390005,0.0106630426745053,0.0205737566905323,0.0309773363492851,
0.0449011586812518,0.0761970396275529,0.110081740051457,0.154906126710259,
0.200342621344964,0.207965395092099,0.213623201483809,0.219015379887419,
0.224348799802594,0.234505119131874,0.27387986478419,0.288553455097379,
0.388871765465751,0.469520721251558,0.502286847933687,0.520588609152811,
0.533113087069208,0.543643727004756,0.554918022868189,0.569085328398199,
0.598276863271334,0.694955163729441,0.811946713382373,0.880397741089542,
0.96229181838556,1.00023598821217,1.00664366631311,1.00955245326006,1.01173511729369,
1.01378007837786,1.01715694034604,1.02571813211193,1.15960646309933,1.231986951194,
1.34743429563182,1.38505278697767,1.4321260925016,1.43909640371432,1.4426743327216,
1.44528177472768,1.44807436584836,1.45287312965519,1.4661022137583,1.67529778998201,
1.8024443972039,1.83881086531281,1.85851956117606,1.86282671355505,1.86550927311032,
1.86773473192657,1.87038114418582,1.87500070315741,1.89326354117798,2.0727824063289,
2.20422558955622,2.22200261636897,2.23230807818747,2.23949750633857,2.24650235364747,
2.24652257494582,2.24654297632481,2.24656355833462,2.24658432149997,2.24660526645583,
2.24662639375394,2.24664769464303,2.24666916054298,2.2466908111234,2.24671264688734,
2.2467346682356,2.24675687559219,2.24677927627373,2.24680627064681,2.24683419169507,
2.24686306339174,2.24689290983735,2.24692375523848,2.24695562378715,2.24698853961937,
2.24702252685742,2.25361008826048,2.26193037459867,2.27821743186043,2.41520024762271,
2.48881652761243,2.6076408893715,2.62285978351591,2.62704023172776,2.62956097730095,
2.63181919109457,2.63467952694543,2.64025152628893,2.67667100073445,2.6801632819919,
2.69056279498917,2.72056249537698,2.91564057921407,3.03335529309531,3.04479184239345,
3.04916827364992,3.05218033215583,3.05512902020671,3.05868001523823,3.0675363391675,
3.1509224182157,3.18722207954488,3.35078207476329,3.46387140953021,3.47846893056943,
3.48247117967666,3.48488238195192,3.48704105782159,3.48977343510445,3.49407105574737,
3.51510532041173,3.7344276894245,3.82416355405774,3.88343516625509,3.92336487043767,
3.93927255370562,3.95078478007927,3.96138522400681,3.97870994025716,4.02418286121904,
4.1737049466551,4.18252609574143,4.23574345235269,4.25556443317704,4.27005853099795,
4.27679522408149,4.28235194516456,4.28928991730693,4.30027104546849,4.36774209505622,
4.43681407794521,4.45843073202738,4.47050223284609,4.48104127754417,4.49430469426287,
4.52218683432077,4.57961413039601,4.64336742114334,4.67304495397062,4.68175748704295,
4.6877144503396,4.69341952019469,4.70155340097515,4.72485052229376,4.85138041973883,
4.9118145690509,4.93396798052398,4.95048327675692,4.96924017146467,5.01057576283585,
5.04739173511335,5.06772829715546,5.08360580623047,5.09564070909482,5.11317589063816,
5.16474993950931,5.20547379823957,5.22412641548529,5.24066341876892,5.26300899796339,
5.32537880021096,5.39101363735221,5.39906571605438,5.40035361936073,5.46211468215961,
5.47550908975743,5.48331945846958,5.48929762005054,5.49588098440515,5.50896510218919,
5.56368369698623,5.66631926184257,5.68567031924147,5.69729647557725,5.70792244553632,
5.72198641865309,5.75517563499079,5.80767104934377,5.8737097394826,5.88487605179403,
5.8918673988831,5.89742854249273,5.90411011167432,5.91830238739391,5.92885619821949,
5.96300869569586,6.11185166782372,6.11929222299259,6.18967837912216,6.20985978979228,
6.22223892173322,6.23360762312449,6.24860097277379,6.28255221263302,6.46164481129914,
6.59247447434857,6.67713295465579,6.68383452192659,6.68650199132543,6.68870847137145,
6.69095528677782,6.69420776563978,6.70264398301759,6.71932666896524,6.76469003875785,
6.86356758228398,6.94667238445084,7.10489559386326,7.11468240686054,7.11848659865712,
7.12123122538557,7.12414827255336,7.128015993173,7.13645295447768,7.29021169177013,
7.47340440680141,7.53298727518265,7.53921394630333,7.54213434162317,7.54440629322068,
7.54686964948646,7.55079448358226,7.56357697402388,7.64886521123102,7.80119831084339,
7.89725186175797,7.91129831311978,7.91981244548549,7.92644721782896,7.92646983873642,
7.92649212757603,7.92651409368743,7.92653574125443,7.9265570742788,7.92657809683473,
7.9265988129232,7.92661922649932,7.92663934148035,7.92665916174584,7.92667869115172,
7.92669793348641,7.92671059496794,7.92672322682934,7.92673581245944,7.92674835200075,
7.92676084553945,7.926773293208,7.92678569521957,7.92679805172078,7.92681036282717,
7.92682262863064,7.92683484930343,7.92684702499527,7.9268591558101,7.92687124181451,
7.92688328314052,7.92689527996041,7.92690723240912,7.92691914063808,7.9269310047965,
7.9269428249828,7.92695460131494,7.92696633396561,7.92697802308025,7.92698966874453,
7.92700127104353,7.92701283020738,7.92702434638551,7.92703581957529,7.92704724996283,
7.92705863769546,7.92706998285827,7.9270812856316,7.92709254620274,7.92710376466872,
7.92711494110861,7.92712607559759,7.92713716830416,7.92714821942435,7.9271592289824,
7.92717019719085,7.92718112429855,7.93409296492652,7.94449066890801,7.95646001647683,
7.97840188989325,8.02902241025803,8.13194487355008,8.2315272125584,8.26283442960562,
8.2869942785653,8.30001614832129,8.30412917955994,8.30638538712158,8.30863524778826,
8.31139387138297,8.31645258709696,8.34724690705752,8.37395317190365,8.50062970178918,
8.70800855314985,8.72109115279372,8.72586826469461,8.72865681581129,8.73126596948673,
8.73485477498857,8.74187610203238,8.79038432614299,8.85345721372875,8.93561109011806,
9.01725103177075,9.14674864326658,9.1565051177784,9.16007193310238,9.16215410963622,
9.16410306830219,9.16678551338433,9.17203869378283,9.20662789031212,9.28874525756097,
9.44383117227937,9.56948340111591,9.60296114310369,9.61771876351963,9.62909157337525,
9.63957667520273,9.65165989305312,9.68605312085834,9.73502300585954,9.90252745862155,
9.94013907325383,9.95012727135301,9.95543321301889,9.96081296631798,9.96649105514681,
9.96938421486085,9.98947207774057,10.0313602480716,10.1165080946907,10.1367043676512,
10.1484933387437,10.1587468895274,10.1689780306746,10.1822069942301,10.2248098208976),
 .UNSPECIFIED.);
#3244=B_SPLINE_CURVE_WITH_KNOTS('',3,(#177740,#177741,#177742,#177743,#177744,
#177745,#177746,#177747,#177748,#177749,#177750,#177751,#177752,#177753,
#177754,#177755,#177756,#177757),.UNSPECIFIED.,.F.,.F.,(4,2,2,2,2,2,2,2,
4),(141.371669411541,142.201027187979,143.030384964417,143.859742740855,
144.689100517293,145.518458293731,146.347816070169,147.177173846607,147.654854718721),
 .UNSPECIFIED.);
#3245=B_SPLINE_CURVE_WITH_KNOTS('',3,(#177759,#177760,#177761,#177762,#177763,
#177764,#177765,#177766,#177767,#177768,#177769,#177770,#177771,#177772,
#177773,#177774,#177775,#177776,#177777,#177778,#177779,#177780,#177781,
#177782,#177783,#177784,#177785,#177786,#177787,#177788,#177789,#177790,
#177791,#177792,#177793,#177794,#177795,#177796,#177797,#177798,#177799,
#177800,#177801,#177802,#177803,#177804,#177805,#177806,#177807,#177808,
#177809,#177810,#177811,#177812,#177813,#177814,#177815,#177816,#177817,
#177818,#177819,#177820,#177821,#177822,#177823,#177824,#177825,#177826,
#177827,#177828,#177829,#177830,#177831,#177832,#177833,#177834,#177835,
#177836,#177837,#177838,#177839,#177840,#177841,#177842,#177843,#177844,
#177845,#177846,#177847,#177848,#177849,#177850,#177851,#177852,#177853,
#177854,#177855,#177856,#177857,#177858,#177859,#177860,#177861,#177862,
#177863,#177864,#177865,#177866,#177867,#177868,#177869,#177870,#177871,
#177872,#177873,#177874,#177875,#177876,#177877,#177878,#177879,#177880,
#177881,#177882,#177883,#177884,#177885,#177886,#177887,#177888,#177889,
#177890,#177891,#177892,#177893,#177894,#177895,#177896,#177897,#177898,
#177899,#177900,#177901,#177902,#177903,#177904,#177905,#177906,#177907,
#177908,#177909,#177910,#177911,#177912,#177913,#177914,#177915,#177916,
#177917,#177918,#177919,#177920,#177921,#177922,#177923,#177924,#177925,
#177926,#177927,#177928,#177929,#177930,#177931,#177932,#177933,#177934,
#177935,#177936,#177937,#177938,#177939,#177940,#177941,#177942,#177943,
#177944,#177945,#177946,#177947,#177948,#177949,#177950,#177951,#177952,
#177953,#177954,#177955,#177956,#177957,#177958,#177959,#177960,#177961,
#177962,#177963,#177964,#177965,#177966,#177967,#177968,#177969,#177970,
#177971,#177972,#177973,#177974,#177975,#177976,#177977,#177978,#177979,
#177980,#177981,#177982,#177983,#177984,#177985,#177986,#177987,#177988,
#177989,#177990,#177991,#177992,#177993,#177994,#177995,#177996,#177997,
#177998,#177999,#178000,#178001,#178002,#178003,#178004,#178005,#178006,
#178007,#178008,#178009,#178010,#178011,#178012,#178013,#178014,#178015,
#178016,#178017,#178018,#178019,#178020,#178021,#178022,#178023,#178024,
#178025,#178026,#178027,#178028,#178029,#178030,#178031,#178032,#178033,
#178034,#178035,#178036,#178037,#178038,#178039,#178040,#178041,#178042,
#178043,#178044,#178045,#178046,#178047,#178048,#178049,#178050,#178051,
#178052,#178053,#178054,#178055,#178056,#178057,#178058,#178059,#178060,
#178061,#178062,#178063,#178064,#178065,#178066,#178067,#178068,#178069,
#178070,#178071,#178072,#178073,#178074,#178075,#178076,#178077,#178078,
#178079,#178080,#178081,#178082,#178083,#178084,#178085,#178086,#178087,
#178088,#178089,#178090,#178091,#178092,#178093,#178094,#178095,#178096,
#178097,#178098,#178099,#178100,#178101,#178102,#178103,#178104,#178105,
#178106,#178107,#178108,#178109,#178110,#178111,#178112,#178113,#178114,
#178115,#178116,#178117,#178118,#178119,#178120,#178121,#178122,#178123,
#178124,#178125,#178126,#178127,#178128,#178129,#178130,#178131,#178132,
#178133,#178134,#178135,#178136,#178137,#178138,#178139,#178140,#178141,
#178142,#178143,#178144,#178145,#178146,#178147,#178148,#178149,#178150,
#178151,#178152,#178153,#178154,#178155,#178156,#178157,#178158,#178159,
#178160,#178161,#178162,#178163,#178164,#178165,#178166,#178167,#178168,
#178169,#178170,#178171,#178172,#178173,#178174,#178175,#178176,#178177,
#178178,#178179,#178180,#178181,#178182,#178183,#178184,#178185,#178186,
#178187,#178188,#178189,#178190,#178191,#178192,#178193,#178194,#178195,
#178196,#178197,#178198,#178199,#178200,#178201,#178202,#178203,#178204,
#178205,#178206,#178207,#178208,#178209,#178210,#178211,#178212,#178213,
#178214,#178215,#178216,#178217,#178218,#178219,#178220,#178221,#178222,
#178223,#178224,#178225,#178226,#178227,#178228,#178229,#178230,#178231,
#178232,#178233,#178234,#178235,#178236,#178237,#178238,#178239,#178240,
#178241,#178242,#178243,#178244,#178245,#178246,#178247,#178248,#178249,
#178250,#178251,#178252,#178253,#178254,#178255,#178256,#178257,#178258,
#178259,#178260,#178261,#178262,#178263,#178264,#178265,#178266,#178267,
#178268,#178269,#178270,#178271,#178272,#178273,#178274,#178275,#178276,
#178277,#178278,#178279,#178280,#178281,#178282,#178283,#178284,#178285,
#178286,#178287,#178288,#178289,#178290,#178291,#178292,#178293,#178294,
#178295,#178296,#178297,#178298,#178299,#178300,#178301,#178302,#178303,
#178304,#178305,#178306,#178307,#178308,#178309,#178310,#178311,#178312,
#178313,#178314,#178315,#178316,#178317,#178318,#178319,#178320,#178321,
#178322,#178323,#178324,#178325,#178326,#178327,#178328,#178329,#178330,
#178331,#178332,#178333,#178334,#178335,#178336,#178337,#178338,#178339,
#178340,#178341,#178342,#178343,#178344,#178345,#178346,#178347,#178348,
#178349,#178350,#178351,#178352,#178353,#178354,#178355,#178356,#178357,
#178358,#178359,#178360,#178361,#178362,#178363,#178364,#178365,#178366,
#178367,#178368,#178369,#178370,#178371,#178372,#178373,#178374,#178375,
#178376,#178377,#178378,#178379,#178380,#178381,#178382,#178383,#178384,
#178385,#178386,#178387,#178388,#178389,#178390,#178391,#178392,#178393,
#178394,#178395,#178396,#178397,#178398,#178399,#178400,#178401,#178402,
#178403,#178404,#178405,#178406,#178407,#178408,#178409,#178410,#178411,
#178412,#178413,#178414,#178415,#178416,#178417,#178418,#178419,#178420,
#178421,#178422,#178423,#178424,#178425,#178426,#178427,#178428,#178429,
#178430,#178431,#178432,#178433,#178434,#178435,#178436,#178437,#178438,
#178439,#178440,#178441,#178442,#178443,#178444,#178445,#178446,#178447,
#178448,#178449,#178450,#178451,#178452,#178453,#178454,#178455,#178456,
#178457,#178458,#178459,#178460,#178461,#178462,#178463,#178464,#178465,
#178466,#178467,#178468,#178469,#178470,#178471,#178472,#178473,#178474,
#178475,#178476,#178477,#178478,#178479,#178480,#178481,#178482,#178483,
#178484,#178485,#178486,#178487,#178488,#178489,#178490,#178491,#178492,
#178493,#178494,#178495,#178496,#178497,#178498,#178499,#178500,#178501,
#178502,#178503,#178504,#178505,#178506,#178507,#178508,#178509,#178510,
#178511,#178512,#178513,#178514,#178515,#178516,#178517,#178518,#178519,
#178520,#178521,#178522,#178523,#178524,#178525,#178526,#178527,#178528,
#178529,#178530,#178531,#178532,#178533,#178534,#178535,#178536,#178537,
#178538,#178539,#178540,#178541,#178542,#178543,#178544,#178545,#178546,
#178547,#178548,#178549,#178550,#178551,#178552,#178553,#178554,#178555,
#178556,#178557,#178558,#178559,#178560,#178561,#178562,#178563,#178564,
#178565,#178566,#178567,#178568,#178569,#178570,#178571,#178572,#178573,
#178574,#178575,#178576,#178577,#178578,#178579,#178580,#178581,#178582,
#178583,#178584,#178585,#178586,#178587,#178588),.UNSPECIFIED.,.F.,.F.,
(4,2,2,2,2,2,2,2,2,2,2,2,2,2,2,2,2,2,2,2,2,2,2,2,2,2,2,2,2,2,2,2,2,2,2,
2,2,2,2,2,2,2,2,2,2,2,2,2,2,2,2,2,2,2,2,2,2,2,2,2,2,2,2,2,2,2,2,2,2,2,2,
2,2,2,2,2,2,2,2,2,2,2,2,2,2,2,2,2,2,2,2,2,2,2,2,2,2,2,2,2,2,2,2,2,2,2,2,
2,2,2,2,2,2,2,2,2,2,2,2,2,2,2,2,2,2,2,2,2,2,2,2,2,2,2,2,2,2,2,2,2,2,2,2,
2,2,2,2,2,2,2,2,2,2,2,2,2,2,2,2,2,2,2,2,2,2,2,2,2,2,2,2,2,2,2,2,2,2,2,2,
2,2,2,2,2,2,2,2,2,2,2,2,2,2,2,2,2,2,2,2,2,2,2,2,2,2,2,2,2,2,2,2,2,2,2,2,
2,2,2,2,2,2,2,2,2,2,2,2,2,2,2,2,2,2,2,2,2,2,2,2,2,2,2,2,2,2,2,2,2,2,2,2,
2,2,2,2,2,2,2,2,2,2,2,2,2,2,2,2,2,2,2,2,2,2,2,2,2,2,2,2,2,2,2,2,2,2,2,2,
2,2,2,2,2,2,2,2,2,2,2,2,2,2,2,2,2,2,2,2,2,2,2,2,2,2,2,2,2,2,2,2,2,2,2,2,
2,2,2,2,2,2,2,2,2,2,2,2,2,2,2,2,2,2,2,2,2,2,2,2,2,2,2,2,2,2,2,2,2,2,2,2,
2,2,2,2,2,2,2,2,2,2,2,2,2,2,2,2,2,2,2,2,2,2,2,2,2,2,2,2,2,2,2,2,2,2,2,2,
2,2,2,2,2,2,2,2,2,2,2,2,2,2,2,2,2,2,2,4),(0.00176456259827877,0.0354791527871678,
0.196790374928931,0.253475429305457,0.274104640931416,0.284542362063342,
0.291106759236629,0.296234103287553,0.301801626125252,0.308859133551379,
0.320255975232913,0.375844817145895,0.436723782681839,0.471107303508008,
0.485342329110856,0.495446801019947,0.506562977151543,0.52383811378267,
0.593911156180744,0.645311576428964,0.675832753848066,0.68904210448208,
0.696662161924079,0.70222372346386,0.707553383937515,0.714249923353767,
0.725728347426913,0.778491074454082,0.781901393209374,0.789453164869791,
0.795349999311394,0.881736644163965,0.933512344967916,0.954689503265999,
0.970495528921234,0.98801843038599,1.02550304076582,1.07115699475392,1.08937890788177,
1.08978372106954,1.09018835678865,1.09059290617634,1.09099746387978,1.09140212797604,
1.09152900457176,1.09166693085191,1.09181677872865,1.09197947475155,1.09215600158882,
1.09234739933733,1.09255476669435,1.09277926193263,1.0930221037706,1.09328457217315,
1.09356800910783,1.09387381935848,1.09420347150509,1.09455849913191,1.09494050241539,
1.09535115018395,1.09579218253321,1.09626541404477,1.09677273757903,1.10773187688626,
1.12189044429227,1.1722941283807,1.21992713444815,1.23648429998304,1.24858918538963,
1.25693154003857,1.25966051052207,1.28119014990021,1.33576359763709,1.38291416136558,
1.39212273810709,1.45783968648324,1.47980349801168,1.49099185023654,1.49819518039571,
1.49821670782662,1.49823828167337,1.4982599017126,1.49828156774536,1.49830327944473,
1.49832503654937,1.49834683880696,1.49836868594379,1.49839057774008,1.49841251393612,
1.49843449429614,1.49845651855282,1.49847858645597,1.49850069771643,1.49852285209534,
1.49854504937112,1.49856728930827,1.49858957164872,1.49861189613101,1.49863426252369,
1.49865667055174,1.49867912003272,1.49870161072068,1.49872414235811,1.49874671470344,
1.49876932749285,1.49879198051203,1.49881467353265,1.49883740633635,1.49886017868396,
1.49888299034453,1.49890584110256,1.49892873070505,1.49895165892418,1.4989746255198,
1.49899763026166,1.49902067297547,1.49903716916745,1.49905385501501,1.49907073186526,
1.49908780110115,1.49910506406012,1.49912252210605,1.49914017662258,1.49915802890491,
1.49917608029301,1.49919433208919,1.49921278560538,1.49923144215337,1.49925030306319,
1.49926936957892,1.49928864295883,1.49930812451787,1.49932781547836,1.49934771704632,
1.49936783047152,1.49938815696596,1.49940869777694,1.49942945408252,1.49945042703776,
1.49947161784768,1.49949302765423,1.49951465758479,1.49953650877522,1.4995585823223,
1.4995808793697,1.49960340099519,1.49962614825878,1.49964912220659,1.49967232393198,
1.4996957544459,1.49971941473267,1.4997433058091,1.4997674286692,1.49979178422447,
1.4998163734471,1.49984119728414,1.4998662566769,1.49989155253477,1.49991708572863,
1.49994285712852,1.49996886757687,1.49999511791439,1.50002160896151,1.50004834149911,
1.50007531638276,1.50010253434762,1.50012999613522,1.50015770247099,1.50018565407055,
1.50021385165837,1.50024229590577,1.50027098748616,1.50029992705122,1.50032911523616,
1.50035855264421,1.50038823987576,1.50041817752817,1.50044836614614,1.50047880626074,
1.50050949842875,1.50054044318518,1.50057164101083,1.50060309237956,1.50063479773321,
1.50066675752057,1.50069897218229,1.5007314421186,1.50076416778191,1.50079714952683,
1.50083038769501,1.50702540507998,1.51244979352563,1.52188748072014,1.55668088106553,
1.65196236997401,1.68033067283415,1.70257492163237,1.71478668718972,1.72465178687218,
1.73704873894653,1.76036066872376,1.80004982262211,1.86867673800575,1.88928675816551,
1.89967799802112,1.90748492114413,1.91352229794141,1.91912163103238,1.92763418465396,
1.95196850978629,2.07782744874913,2.20516308820483,2.22115638308586,2.23276745579396,
2.24425164814534,2.25552369799069,2.26969075125086,2.30544133276245,2.49260908038558,
2.64617741777159,2.6931855037452,2.70219623701958,2.70553466718051,2.70779941017734,
2.70999145348589,2.71260036041286,2.71895972417339,2.80100785950158,2.94292982500032,
3.12643034188675,3.13497963351553,3.13886867330947,3.14178938695999,3.14452843248949,
3.14831061641904,3.15796414989909,3.30442510247435,3.35061035880158,3.37813430684796,
3.4834989510071,3.54528322898499,3.55663737668665,3.56039246600406,3.56281836588369,
3.56510478343668,3.56811494310066,3.57456969955984,3.63143821143155,3.7577848189724,
3.8479580806371,3.91968438709121,3.93346707829773,3.94115629558767,3.94768590481128,
3.95507518827764,3.96747224807948,4.01100664604917,4.05124291903256,4.12003136034331,
4.20090663395229,4.28349379219818,4.3170493522518,4.32235961251955,4.32512677127682,
4.32737652459947,4.32962480832831,4.33370809211677,4.34644786312021,4.58511203099722,
4.6914512353215,4.73638562037628,4.74327594231664,4.74683695210505,4.74971678841823,
4.75258296204812,4.75775043593847,4.77361954292603,5.0559477177722,5.1129200885104,
5.17194616267539,5.17734298994204,5.18009915954189,5.18212738984376,5.18432100063871,
5.18729493348649,5.19405880470557,5.30131858674226,5.49609129412834,5.59513670410783,
5.62464431153861,5.63886932521267,5.65014869399534,5.66294249014855,5.68506891353167,
5.81065496176032,5.94157457944028,5.96342611523451,5.97078553059454,5.97592582894265,
5.98175577276171,5.99038844365837,6.01589895685601,6.04163797059443,6.12850894084205,
6.15291950848832,6.16567627040948,6.17618845590054,6.18866124285288,6.21223890940093,
6.22892942538726,6.28319089459611,6.3640231741719,6.37596540008591,6.38236490647448,
6.38840324677182,6.39671374320434,6.41681679171683,6.54571678983377,6.60690032467193,
6.62747657931358,6.64263950993826,6.65992693290219,6.68887409008805,6.73223134724458,
6.76978566477348,6.78343913038217,6.79643871098364,6.82968938781901,6.90304451460922,
6.92150115273641,6.93808613749624,6.96082506224678,7.02747689065037,7.08936670584393,
7.15853563616157,7.17347324265738,7.18097568687398,7.1868972796558,7.19380301320175,
7.20889901403962,7.23065358138959,7.30585780195192,7.36723562955551,7.3845225652254,
7.39460718468134,7.40527743858945,7.41965344658761,7.45505656801025,7.4862749203777,
7.52899705512248,7.57450461618095,7.58465981227175,7.5902031813613,7.5952153072515,
7.602462828953,7.61989211721044,7.64517597551845,7.76588879668253,7.88280610038466,
7.90453091707306,7.91719498257534,7.92822552206921,7.94202474915843,7.96925057697626,
8.07833510960258,8.1598204084289,8.29367565917721,8.34876412057702,8.37618687653631,
8.3808755109823,8.383695728477,8.38587210186303,8.3882148097889,8.39191114634577,
8.40363834136371,8.47321284704257,8.64167553943684,8.80176361182149,8.81156010263576,
8.81536589195685,8.81811101313506,8.82102797618225,8.82489455028041,8.83332490961036,
8.91619784478626,9.03880575830107,9.22341643153359,9.2340624577903,9.23785879425779,
9.2400494762243,9.24208390055859,9.24485917833223,9.25020865367425,9.28478350506138,
9.36722493322371,9.476805404586,9.5032869716063,9.59430308675518,9.60944868662987,
9.61742384699808,9.62385495733904,9.62997192649443,9.63994326682273,9.66662486304035,
9.79825382322865,9.98048350089048,9.99624831128481,10.0006236372703,10.0032129904916,
10.0054621561332,10.0082199292609,10.0134850303902,10.0480856911902,10.0780029776344,
10.2237184582249),.UNSPECIFIED.);
#3246=B_SPLINE_CURVE_WITH_KNOTS('',3,(#178590,#178591,#178592,#178593,#178594,
#178595,#178596,#178597,#178598,#178599,#178600,#178601,#178602,#178603,
#178604),.UNSPECIFIED.,.F.,.F.,(4,1,1,1,1,1,1,1,1,1,1,1,4),(122.522113490003,
122.566527474554,123.064996017861,124.061933104476,124.560401647784,125.058870191091,
125.557338734399,126.055807277706,126.554275821014,127.052744364322,127.551212907629,
128.049681450937,128.805298797182),.UNSPECIFIED.);
#3247=B_SPLINE_CURVE_WITH_KNOTS('',3,(#178606,#178607,#178608,#178609,#178610,
#178611,#178612,#178613,#178614,#178615,#178616,#178617,#178618,#178619,
#178620,#178621,#178622,#178623,#178624,#178625,#178626,#178627,#178628,
#178629,#178630,#178631,#178632,#178633,#178634,#178635,#178636,#178637,
#178638,#178639,#178640,#178641,#178642,#178643,#178644,#178645,#178646,
#178647,#178648,#178649,#178650,#178651,#178652,#178653,#178654,#178655,
#178656,#178657,#178658,#178659,#178660,#178661,#178662,#178663,#178664,
#178665,#178666,#178667,#178668,#178669,#178670,#178671,#178672,#178673,
#178674,#178675,#178676,#178677,#178678,#178679,#178680,#178681,#178682,
#178683,#178684,#178685,#178686,#178687,#178688,#178689,#178690,#178691,
#178692,#178693,#178694,#178695,#178696,#178697,#178698,#178699,#178700,
#178701,#178702,#178703,#178704,#178705,#178706,#178707,#178708,#178709,
#178710,#178711,#178712,#178713,#178714,#178715,#178716,#178717,#178718,
#178719,#178720,#178721,#178722,#178723,#178724,#178725,#178726,#178727,
#178728,#178729,#178730,#178731,#178732,#178733,#178734,#178735,#178736,
#178737,#178738,#178739,#178740,#178741,#178742,#178743,#178744,#178745,
#178746,#178747,#178748,#178749,#178750,#178751,#178752,#178753,#178754,
#178755,#178756,#178757,#178758,#178759,#178760,#178761,#178762,#178763,
#178764,#178765,#178766,#178767,#178768,#178769,#178770,#178771,#178772,
#178773,#178774,#178775,#178776,#178777,#178778,#178779,#178780,#178781,
#178782,#178783,#178784,#178785,#178786,#178787,#178788,#178789,#178790,
#178791,#178792,#178793,#178794,#178795,#178796,#178797,#178798,#178799,
#178800,#178801,#178802,#178803,#178804,#178805,#178806,#178807,#178808,
#178809,#178810,#178811,#178812,#178813,#178814,#178815,#178816,#178817,
#178818,#178819,#178820,#178821,#178822,#178823,#178824,#178825,#178826,
#178827,#178828,#178829,#178830,#178831,#178832,#178833,#178834,#178835,
#178836,#178837,#178838,#178839,#178840,#178841,#178842,#178843,#178844,
#178845,#178846,#178847,#178848,#178849,#178850,#178851,#178852,#178853,
#178854,#178855,#178856,#178857,#178858,#178859,#178860,#178861),
 .UNSPECIFIED.,.F.,.F.,(4,3,3,3,3,3,3,3,3,3,3,3,3,3,3,3,3,3,3,3,3,3,3,3,
3,3,3,3,3,3,3,3,3,3,3,3,3,3,3,3,3,3,3,3,3,3,3,3,3,3,3,3,3,3,3,3,3,3,3,3,
3,3,3,3,3,3,3,3,3,3,3,3,3,3,3,3,3,3,3,3,3,3,3,3,3,4),(116.238928182823,
116.314078890482,116.389167626035,116.46420661482,116.541602475239,116.616581818432,
116.691551253406,116.766521798447,116.841504470604,116.916534326775,116.991592107213,
117.066712158694,117.08337349817,117.15479677302,117.226166899934,117.297497471455,
117.36881080894,117.440111495763,117.511436977255,117.581842041478,117.669547530819,
117.757723893237,117.846328303855,117.935028610738,118.023624870673,118.080310584786,
118.153280029236,118.22620402033,118.299095547071,118.371977745992,118.444852664036,
118.517755613746,118.578779128093,118.658079912042,118.737402842518,118.816745444527,
118.896118521699,118.975500202695,119.054896979803,119.077247671401,119.15664506607,
119.236028739899,119.315396191541,119.394741375354,119.474064394621,119.553358624243,
119.575716214708,119.648618614976,119.721498472021,119.794368741454,119.867265085859,
119.940173741644,120.013142054592,120.074184758016,120.162759089629,120.251459455103,
120.340026267206,120.42836968077,120.516139397397,120.572653301323,120.643976799673,
120.715280549828,120.7865780531,120.857910548747,120.929258907486,121.000679562453,
121.071121844631,121.147225340652,121.223278486723,121.299291676958,121.375275276839,
121.451239630168,121.528342042803,121.604313770841,121.6802980981,121.756304439773,
121.834243062641,121.910352102069,121.989205516658,122.068058931246,122.145066413229,
122.221970743137,122.298741465248,122.375434319171,122.452027422789,122.522113453888),
 .UNSPECIFIED.);
#3248=B_SPLINE_CURVE_WITH_KNOTS('',3,(#178863,#178864,#178865,#178866,#178867,
#178868,#178869,#178870,#178871,#178872,#178873,#178874,#178875,#178876,
#178877,#178878),.UNSPECIFIED.,.F.,.F.,(4,1,1,1,1,1,1,1,1,1,1,1,1,4),(109.955742875643,
110.104813891865,110.603282435172,111.10175097848,111.600219521787,112.098688065095,
112.597156608402,113.09562515171,113.594093695018,114.092562238325,115.08949932494,
115.587967868248,116.086436411555,116.238928182823),.UNSPECIFIED.);
#3249=B_SPLINE_CURVE_WITH_KNOTS('',3,(#178880,#178881,#178882,#178883,#178884,
#178885,#178886,#178887,#178888,#178889,#178890,#178891,#178892,#178893,
#178894,#178895,#178896,#178897,#178898,#178899,#178900,#178901,#178902,
#178903,#178904,#178905,#178906,#178907,#178908,#178909,#178910,#178911,
#178912,#178913,#178914,#178915,#178916,#178917,#178918,#178919,#178920,
#178921,#178922,#178923,#178924,#178925,#178926,#178927,#178928,#178929,
#178930,#178931,#178932,#178933,#178934,#178935,#178936,#178937,#178938,
#178939,#178940,#178941,#178942,#178943,#178944,#178945,#178946,#178947,
#178948,#178949,#178950,#178951,#178952,#178953,#178954,#178955,#178956,
#178957,#178958,#178959,#178960,#178961,#178962,#178963,#178964,#178965,
#178966,#178967,#178968,#178969,#178970,#178971,#178972,#178973,#178974,
#178975,#178976,#178977,#178978,#178979,#178980,#178981,#178982,#178983,
#178984,#178985,#178986,#178987,#178988,#178989,#178990,#178991,#178992,
#178993,#178994,#178995,#178996,#178997,#178998,#178999,#179000,#179001,
#179002,#179003,#179004,#179005,#179006,#179007,#179008,#179009,#179010,
#179011,#179012,#179013,#179014,#179015,#179016,#179017,#179018,#179019,
#179020,#179021,#179022,#179023,#179024,#179025,#179026,#179027,#179028,
#179029,#179030,#179031,#179032,#179033,#179034,#179035,#179036,#179037,
#179038,#179039,#179040,#179041,#179042,#179043,#179044,#179045,#179046,
#179047,#179048,#179049,#179050,#179051,#179052,#179053,#179054,#179055,
#179056,#179057,#179058,#179059,#179060,#179061,#179062,#179063,#179064,
#179065,#179066,#179067,#179068,#179069,#179070,#179071,#179072,#179073,
#179074,#179075,#179076,#179077,#179078,#179079,#179080,#179081,#179082,
#179083,#179084,#179085,#179086,#179087,#179088,#179089,#179090,#179091,
#179092,#179093,#179094,#179095,#179096,#179097,#179098,#179099,#179100,
#179101,#179102,#179103,#179104,#179105,#179106,#179107,#179108,#179109,
#179110,#179111,#179112,#179113,#179114,#179115,#179116,#179117,#179118,
#179119,#179120,#179121,#179122,#179123,#179124,#179125,#179126,#179127,
#179128,#179129,#179130,#179131,#179132,#179133,#179134,#179135),
 .UNSPECIFIED.,.F.,.F.,(4,3,3,3,3,3,3,3,3,3,3,3,3,3,3,3,3,3,3,3,3,3,3,3,
3,3,3,3,3,3,3,3,3,3,3,3,3,3,3,3,3,3,3,3,3,3,3,3,3,3,3,3,3,3,3,3,3,3,3,3,
3,3,3,3,3,3,3,3,3,3,3,3,3,3,3,3,3,3,3,3,3,3,3,3,3,4),(103.672557568464,
103.760974723913,103.851528885978,103.940713177353,104.031952274763,104.123191372174,
104.196160816624,104.269084807718,104.341976334459,104.41485853338,104.487733451423,
104.560636401133,104.621659915481,104.70096069943,104.780283629907,104.859626231917,
104.93899930909,105.018380990087,105.097777767196,105.120128458789,105.199525853458,
105.278909527286,105.358276978927,105.437622162739,105.516945182005,105.596239411627,
105.618597002097,105.691499402366,105.764379259411,105.837249528844,105.91014587325,
105.983054529035,106.056022841983,106.117065545404,106.205639877016,106.294340242489,
106.382907054591,106.471250468154,106.559020184779,106.615534088712,106.686857587062,
106.758161337217,106.82945884049,106.900791336136,106.972139694875,107.043560349842,
107.114002632019,107.19010612804,107.266159274111,107.342172464346,107.418156064227,
107.494120417555,107.57122283019,107.647194558229,107.723178885488,107.79918522716,
107.877123850028,107.953232889457,108.032086304045,108.110939718634,108.187072590879,
108.26311229195,108.339068297321,108.414926739859,108.490727803412,108.566467124146,
108.609408261942,108.685150626765,108.760938747515,108.836781918357,108.912736876617,
108.988753308951,109.064889104452,109.107876805249,109.182804990125,109.257662582641,
109.332462245684,109.410372324429,109.485093837599,109.559799282389,109.634500050476,
109.709207529054,109.783955887192,109.858728142048,109.933559479095,109.955742875643),
 .UNSPECIFIED.);
#3250=B_SPLINE_CURVE_WITH_KNOTS('',3,(#179137,#179138,#179139,#179140,#179141,
#179142,#179143,#179144,#179145,#179146,#179147,#179148,#179149,#179150,
#179151,#179152,#179153,#179154),.UNSPECIFIED.,.F.,.F.,(4,2,2,2,2,2,2,2,
4),(97.3893722612842,98.2187300377222,99.0480878141601,99.877445590598,
100.706803367036,101.536161143474,102.365518919912,103.19487669635,103.672557568464),
 .UNSPECIFIED.);
#3251=B_SPLINE_CURVE_WITH_KNOTS('',3,(#179156,#179157,#179158,#179159,#179160,
#179161,#179162,#179163,#179164,#179165,#179166,#179167,#179168,#179169,
#179170),.UNSPECIFIED.,.F.,.F.,(4,1,1,1,1,1,1,1,1,1,1,1,4),(91.106186982299,
91.1630092461774,91.661477789485,92.1599463327925,92.6584148761001,93.1568834194076,
94.1538205060227,94.6522890493303,95.1507575926379,96.147694679253,96.6461632225605,
97.1446317658681,97.3893722612842),.UNSPECIFIED.);
#3252=B_SPLINE_CURVE_WITH_KNOTS('',3,(#179172,#179173,#179174,#179175,#179176,
#179177,#179178,#179179,#179180,#179181,#179182,#179183,#179184,#179185,
#179186,#179187,#179188,#179189,#179190,#179191,#179192,#179193,#179194,
#179195,#179196,#179197,#179198,#179199,#179200,#179201,#179202,#179203,
#179204,#179205,#179206,#179207,#179208,#179209,#179210,#179211,#179212,
#179213,#179214,#179215,#179216,#179217,#179218,#179219,#179220,#179221,
#179222,#179223,#179224,#179225,#179226,#179227,#179228,#179229,#179230,
#179231,#179232,#179233,#179234,#179235,#179236,#179237,#179238,#179239,
#179240,#179241,#179242,#179243,#179244,#179245,#179246,#179247,#179248,
#179249,#179250,#179251,#179252,#179253,#179254,#179255,#179256,#179257,
#179258,#179259,#179260,#179261,#179262,#179263,#179264,#179265,#179266,
#179267,#179268,#179269,#179270,#179271,#179272,#179273,#179274,#179275,
#179276,#179277,#179278,#179279,#179280,#179281,#179282,#179283,#179284,
#179285,#179286,#179287,#179288,#179289,#179290,#179291,#179292,#179293,
#179294,#179295,#179296,#179297,#179298,#179299,#179300,#179301,#179302,
#179303,#179304,#179305,#179306,#179307,#179308,#179309,#179310,#179311,
#179312,#179313,#179314,#179315,#179316,#179317,#179318,#179319,#179320,
#179321,#179322,#179323,#179324,#179325,#179326,#179327,#179328,#179329,
#179330,#179331,#179332,#179333,#179334,#179335,#179336,#179337,#179338,
#179339,#179340,#179341,#179342,#179343,#179344,#179345,#179346,#179347,
#179348,#179349,#179350,#179351,#179352,#179353,#179354,#179355,#179356,
#179357,#179358,#179359,#179360,#179361,#179362,#179363,#179364,#179365,
#179366,#179367,#179368,#179369,#179370,#179371,#179372,#179373,#179374,
#179375,#179376,#179377,#179378,#179379,#179380,#179381,#179382,#179383,
#179384,#179385,#179386,#179387,#179388,#179389,#179390,#179391,#179392,
#179393,#179394,#179395,#179396,#179397,#179398,#179399,#179400,#179401,
#179402,#179403,#179404,#179405,#179406,#179407,#179408,#179409,#179410,
#179411,#179412,#179413,#179414,#179415,#179416,#179417,#179418,#179419,
#179420,#179421,#179422,#179423,#179424),.UNSPECIFIED.,.F.,.F.,(4,3,3,3,
3,3,3,3,3,3,3,3,3,3,3,3,3,3,3,3,3,3,3,3,3,3,3,3,3,3,3,3,3,3,3,3,3,3,3,3,
3,3,3,3,3,3,3,3,3,3,3,3,3,3,3,3,3,3,3,3,3,3,3,3,3,3,3,3,3,3,3,3,3,3,3,3,
3,3,3,3,3,3,3,3,4),(84.8230016469251,84.8956472635889,84.9683166584872,
85.0409964770063,85.113736009744,85.1813867264867,85.2699610580999,85.3586614235737,
85.4472282356765,85.5355716492405,85.6233413658659,85.6798552697942,85.7511787681441,
85.8224825182994,85.8937800215718,85.9651125172181,86.0364608759574,86.1078815309242,
86.1783238131018,86.2544273091229,86.3304804551935,86.4064936454288,86.4824772453094,
86.5584415986381,86.6355440112729,86.7115157393116,86.7875000665704,86.8635064082429,
86.9414450311114,87.0175540705395,87.0964074851282,87.1752608997169,87.251393771962,
87.3274334730333,87.403389478404,87.4792479209413,87.555048984495,87.630788305229,
87.6737294430245,87.7494718078472,87.8252599285969,87.9011030994388,87.9770580576987,
88.0530744900329,88.1292102855333,88.1721979863321,88.2484085668057,88.3245511710578,
88.4006362573982,88.4766742436705,88.5526755142256,88.6297329590658,88.7056982211906,
88.7816598130553,88.8576271401166,88.9355041233242,89.0115339207569,89.0903344968521,
89.1691350729472,89.2405583477971,89.3119284747104,89.3832590462316,89.4545723837173,
89.5258730705395,89.597198552032,89.6676036162547,89.7553091055951,89.8434854680136,
89.932089878631,90.0207901855136,90.1093864454484,90.1660721595623,90.2390416040124,
90.3119655951063,90.3848571218472,90.4577393207681,90.5306142388117,90.6035171885217,
90.6645407028698,90.7438457847053,90.8231735900791,90.902538090652,90.9819133289185,
91.0613095087734,91.1061869541046),.UNSPECIFIED.);
#3253=B_SPLINE_CURVE_WITH_KNOTS('',3,(#179426,#179427,#179428,#179429,#179430,
#179431,#179432,#179433,#179434,#179435,#179436,#179437,#179438,#179439,
#179440,#179441,#179442,#179443),.UNSPECIFIED.,.F.,.F.,(4,2,2,2,2,2,2,2,
4),(78.5398163397455,79.3691741161834,80.1985318926214,81.0278896690593,
81.8572474454973,82.6866052219353,83.5159629983732,84.3453207748112,84.8230016469251),
 .UNSPECIFIED.);
#3254=B_SPLINE_CURVE_WITH_KNOTS('',3,(#179445,#179446,#179447,#179448,#179449,
#179450,#179451,#179452,#179453,#179454,#179455,#179456,#179457,#179458),
 .UNSPECIFIED.,.F.,.F.,(4,1,1,1,1,1,1,1,1,1,1,4),(72.2566310325659,73.2181416871053,
73.7166102304129,74.2150787737204,75.2120158603355,75.7104844036431,76.2089529469506,
76.7074214902582,77.2058900335658,77.7043585768733,78.2028271201809,78.5398163397455),
 .UNSPECIFIED.);
#3255=B_SPLINE_CURVE_WITH_KNOTS('',3,(#179460,#179461,#179462,#179463,#179464,
#179465,#179466,#179467,#179468,#179469,#179470,#179471,#179472,#179473,
#179474,#179475),.UNSPECIFIED.,.F.,.F.,(4,1,1,1,1,1,1,1,1,1,1,1,1,4),(65.9734457253863,
66.2395820807995,66.738050624107,67.2365191674146,68.2334562540297,68.7319247973373,
69.2303933406448,69.7288618839524,70.22733042726,70.7257989705675,71.2242675138751,
71.7227360571826,72.2212046004902,72.2566310325659),.UNSPECIFIED.);
#3256=B_SPLINE_CURVE_WITH_KNOTS('',3,(#179477,#179478,#179479,#179480,#179481,
#179482,#179483,#179484,#179485,#179486,#179487,#179488,#179489,#179490,
#179491),.UNSPECIFIED.,.F.,.F.,(4,1,1,1,1,1,1,1,1,1,1,1,4),(59.6902604182067,
59.7594910178012,60.2579595611088,61.2548966477239,61.7533651910315,62.251833734339,
62.7503022776466,63.2487708209541,63.7472393642617,64.2457079075693,64.7441764508768,
65.2426449941844,65.9734457253863),.UNSPECIFIED.);
#3257=B_SPLINE_CURVE_WITH_KNOTS('',3,(#179493,#179494,#179495,#179496,#179497,
#179498,#179499,#179500,#179501,#179502,#179503,#179504,#179505,#179506),
 .UNSPECIFIED.,.F.,.F.,(4,1,1,1,1,1,1,1,1,1,1,4),(53.4070751110271,54.2763370414181,
54.7748055847256,55.2732741280332,55.7717426713408,56.2702112146483,56.7686797579559,
57.2671483012634,57.765616844571,58.2640853878786,59.2610224744937,59.6902604182067),
 .UNSPECIFIED.);
#3258=B_SPLINE_CURVE_WITH_KNOTS('',3,(#179508,#179509,#179510,#179511,#179512,
#179513,#179514,#179515,#179516,#179517,#179518,#179519,#179520,#179521,
#179522,#179523),.UNSPECIFIED.,.F.,.F.,(4,1,1,1,1,1,1,1,1,1,1,1,1,4),(47.1238898038475,
47.2977774351123,47.7962459784198,48.2947145217274,48.793183065035,49.2916516083425,
49.7901201516501,50.2885886949576,50.7870572382652,51.2855257815727,52.2824628681879,
52.7809314114954,53.279399954803,53.4070751110271),.UNSPECIFIED.);
#3259=B_SPLINE_CURVE_WITH_KNOTS('',3,(#179525,#179526,#179527,#179528,#179529,
#179530,#179531,#179532,#179533,#179534,#179535,#179536,#179537,#179538,
#179539,#179540,#179541,#179542,#179543,#179544,#179545,#179546,#179547,
#179548,#179549,#179550,#179551,#179552,#179553,#179554,#179555,#179556,
#179557,#179558,#179559,#179560,#179561,#179562,#179563,#179564,#179565,
#179566,#179567,#179568,#179569,#179570,#179571,#179572,#179573,#179574,
#179575,#179576,#179577,#179578,#179579,#179580,#179581,#179582,#179583,
#179584,#179585,#179586,#179587,#179588,#179589,#179590,#179591,#179592,
#179593,#179594,#179595,#179596,#179597,#179598,#179599,#179600,#179601,
#179602,#179603,#179604,#179605,#179606,#179607,#179608,#179609,#179610,
#179611,#179612,#179613,#179614,#179615,#179616,#179617,#179618,#179619,
#179620,#179621,#179622,#179623,#179624,#179625,#179626,#179627,#179628,
#179629,#179630,#179631,#179632,#179633,#179634,#179635,#179636,#179637,
#179638,#179639,#179640,#179641,#179642,#179643,#179644,#179645,#179646,
#179647,#179648,#179649,#179650,#179651,#179652,#179653,#179654,#179655,
#179656,#179657,#179658,#179659,#179660,#179661,#179662,#179663,#179664,
#179665,#179666,#179667,#179668,#179669,#179670,#179671,#179672,#179673,
#179674,#179675,#179676,#179677,#179678,#179679,#179680,#179681,#179682,
#179683,#179684,#179685,#179686,#179687,#179688,#179689,#179690,#179691,
#179692,#179693,#179694,#179695,#179696,#179697,#179698,#179699,#179700,
#179701,#179702,#179703,#179704,#179705,#179706,#179707,#179708,#179709,
#179710,#179711,#179712,#179713,#179714,#179715,#179716,#179717,#179718,
#179719,#179720,#179721,#179722,#179723,#179724,#179725,#179726,#179727,
#179728,#179729,#179730,#179731,#179732,#179733,#179734,#179735,#179736,
#179737,#179738,#179739,#179740,#179741,#179742,#179743,#179744,#179745,
#179746,#179747,#179748,#179749,#179750,#179751,#179752,#179753,#179754,
#179755,#179756,#179757,#179758,#179759,#179760,#179761,#179762,#179763,
#179764,#179765,#179766,#179767,#179768,#179769,#179770,#179771,#179772,
#179773,#179774,#179775,#179776,#179777,#179778,#179779,#179780),
 .UNSPECIFIED.,.F.,.F.,(4,3,3,3,3,3,3,3,3,3,3,3,3,3,3,3,3,3,3,3,3,3,3,3,
3,3,3,3,3,3,3,3,3,3,3,3,3,3,3,3,3,3,3,3,3,3,3,3,3,3,3,3,3,3,3,3,3,3,3,3,
3,3,3,3,3,3,3,3,3,3,3,3,3,3,3,3,3,3,3,3,3,3,3,3,3,4),(40.8407044966679,
40.9287194581187,41.0171879336625,41.1060348097448,41.1949478868379,41.2837202383404,
41.3161549154216,41.3891243598713,41.4620483509647,41.5349398777054,41.6078220766259,
41.680696994669,41.7535999443787,41.8146234587291,41.8939242426787,41.9732471731551,
42.0525897751658,42.1319628523385,42.2113445333359,42.2907413104448,42.3130920020367,
42.3924893967055,42.4718730705334,42.5512405221744,42.6305857059864,42.7099087252525,
42.7892029548742,42.8115605453443,42.884462945613,42.9573428026582,43.0302130720914,
43.1031094164965,43.1760180722814,43.2489863852298,43.3100290886518,43.3986034202646,
43.4873037857379,43.5758705978406,43.6642140114044,43.7519837280299,43.8084976319594,
43.8798211303094,43.9511248804646,44.0224223837369,44.0937548793832,44.1651032381225,
44.2365238930893,44.3069661752669,44.383069671288,44.4591228173586,44.5351360075938,
44.6111196074745,44.6870839608031,44.764186373438,44.8401581014766,44.9161424287355,
44.9921487704079,45.0700873932764,45.1461964327046,45.2250498472933,45.303903261882,
45.3800361341271,45.4560758351984,45.5320318405693,45.6078902831066,45.6836913466604,
45.7594306673943,45.8023718051896,45.8781141700123,45.953902290762,46.0297454616037,
46.1057004198636,46.181716852198,46.2578526476984,46.3008403484972,46.3757317456465,
46.4505523614497,46.5253149096933,46.6001367714626,46.6748213521227,46.7494893194585,
46.8241521107267,46.8990865340069,46.9737930881712,47.0488414460093,47.1238898038475),
 .UNSPECIFIED.);
#3260=B_SPLINE_CURVE_WITH_KNOTS('',3,(#179782,#179783,#179784,#179785,#179786,
#179787,#179788,#179789,#179790,#179791,#179792,#179793,#179794,#179795,
#179796,#179797,#179798,#179799,#179800,#179801,#179802,#179803,#179804,
#179805,#179806,#179807,#179808,#179809,#179810,#179811,#179812,#179813,
#179814,#179815,#179816,#179817,#179818,#179819,#179820,#179821,#179822,
#179823,#179824,#179825,#179826,#179827,#179828,#179829,#179830,#179831,
#179832,#179833,#179834,#179835,#179836,#179837,#179838,#179839,#179840,
#179841,#179842,#179843,#179844,#179845,#179846,#179847,#179848,#179849,
#179850,#179851,#179852,#179853,#179854,#179855,#179856,#179857,#179858,
#179859,#179860,#179861,#179862,#179863,#179864,#179865,#179866,#179867,
#179868,#179869,#179870,#179871,#179872,#179873,#179874,#179875,#179876,
#179877,#179878,#179879,#179880,#179881,#179882,#179883,#179884,#179885,
#179886,#179887,#179888,#179889,#179890,#179891,#179892,#179893,#179894,
#179895,#179896,#179897,#179898,#179899,#179900,#179901,#179902,#179903,
#179904,#179905,#179906,#179907,#179908,#179909,#179910,#179911,#179912,
#179913,#179914,#179915,#179916,#179917,#179918,#179919,#179920,#179921,
#179922,#179923,#179924,#179925,#179926,#179927,#179928,#179929,#179930,
#179931,#179932,#179933,#179934,#179935,#179936,#179937,#179938,#179939,
#179940,#179941,#179942,#179943,#179944,#179945,#179946,#179947,#179948,
#179949,#179950,#179951,#179952,#179953,#179954,#179955,#179956,#179957,
#179958,#179959,#179960,#179961,#179962,#179963,#179964,#179965,#179966,
#179967,#179968,#179969,#179970,#179971,#179972,#179973,#179974,#179975,
#179976,#179977,#179978,#179979,#179980,#179981,#179982,#179983,#179984,
#179985,#179986,#179987,#179988,#179989,#179990,#179991,#179992,#179993,
#179994,#179995,#179996,#179997,#179998,#179999,#180000,#180001,#180002,
#180003,#180004,#180005,#180006,#180007,#180008,#180009,#180010,#180011,
#180012,#180013,#180014,#180015,#180016,#180017,#180018,#180019,#180020,
#180021,#180022,#180023,#180024,#180025,#180026,#180027,#180028,#180029,
#180030,#180031,#180032,#180033,#180034,#180035,#180036,#180037,#180038,
#180039,#180040,#180041,#180042,#180043,#180044,#180045,#180046,#180047,
#180048,#180049,#180050,#180051,#180052,#180053,#180054,#180055,#180056,
#180057,#180058,#180059,#180060,#180061,#180062,#180063,#180064,#180065,
#180066,#180067,#180068,#180069,#180070,#180071,#180072,#180073,#180074,
#180075,#180076,#180077,#180078,#180079,#180080,#180081,#180082,#180083,
#180084,#180085,#180086,#180087,#180088,#180089,#180090,#180091,#180092,
#180093,#180094,#180095,#180096,#180097,#180098,#180099,#180100,#180101,
#180102,#180103,#180104,#180105,#180106,#180107,#180108,#180109,#180110,
#180111,#180112,#180113,#180114,#180115,#180116,#180117,#180118,#180119,
#180120,#180121,#180122,#180123,#180124,#180125,#180126,#180127,#180128,
#180129,#180130,#180131,#180132,#180133,#180134,#180135,#180136,#180137,
#180138,#180139,#180140,#180141,#180142,#180143,#180144,#180145,#180146,
#180147,#180148,#180149,#180150,#180151,#180152,#180153,#180154,#180155,
#180156,#180157,#180158,#180159,#180160,#180161,#180162,#180163,#180164,
#180165,#180166,#180167,#180168,#180169,#180170,#180171,#180172,#180173,
#180174,#180175,#180176,#180177,#180178,#180179,#180180,#180181,#180182,
#180183,#180184,#180185,#180186,#180187,#180188,#180189,#180190,#180191,
#180192,#180193,#180194,#180195,#180196,#180197,#180198,#180199,#180200,
#180201,#180202,#180203,#180204,#180205,#180206,#180207,#180208,#180209,
#180210,#180211,#180212,#180213,#180214,#180215,#180216,#180217,#180218,
#180219,#180220,#180221,#180222,#180223,#180224,#180225,#180226,#180227,
#180228,#180229,#180230,#180231,#180232,#180233,#180234,#180235,#180236,
#180237,#180238,#180239,#180240,#180241,#180242,#180243,#180244,#180245,
#180246,#180247,#180248,#180249,#180250,#180251,#180252,#180253,#180254,
#180255,#180256,#180257,#180258,#180259,#180260,#180261,#180262,#180263,
#180264,#180265,#180266,#180267,#180268,#180269,#180270,#180271,#180272,
#180273,#180274,#180275,#180276,#180277,#180278,#180279,#180280,#180281,
#180282,#180283,#180284,#180285,#180286,#180287,#180288,#180289,#180290,
#180291,#180292,#180293,#180294,#180295,#180296,#180297,#180298,#180299,
#180300,#180301,#180302,#180303,#180304,#180305,#180306,#180307,#180308,
#180309,#180310,#180311,#180312,#180313,#180314,#180315,#180316,#180317,
#180318,#180319),.UNSPECIFIED.,.F.,.F.,(4,2,2,2,2,2,2,2,2,2,2,2,2,2,2,2,
2,2,2,2,2,2,2,2,2,2,2,2,2,2,2,2,2,2,2,2,2,2,2,2,2,2,2,2,2,2,2,2,2,2,2,2,
2,2,2,2,2,2,2,2,2,2,2,2,2,2,2,2,2,2,2,2,2,2,2,2,2,2,2,2,2,2,2,2,2,2,2,2,
2,2,2,2,2,2,2,2,2,2,2,2,2,2,2,2,2,2,2,2,2,2,2,2,2,2,2,2,2,2,2,2,2,2,2,2,
2,2,2,2,2,2,2,2,2,2,2,2,2,2,2,2,2,2,2,2,2,2,2,2,2,2,2,2,2,2,2,2,2,2,2,2,
2,2,2,2,2,2,2,2,2,2,2,2,2,2,2,2,2,2,2,2,2,2,2,2,2,2,2,2,2,2,2,2,2,2,2,2,
2,2,2,2,2,2,2,2,2,2,2,2,2,2,2,2,2,2,2,2,2,2,2,2,2,2,2,2,2,2,2,2,2,2,2,2,
2,2,2,2,2,2,2,2,2,2,2,2,2,2,2,2,2,2,2,2,2,2,2,2,2,2,2,2,2,2,2,2,2,2,2,2,
4),(0.00125752731703474,0.0770073154476629,0.2473678712053,0.359216152094507,
0.396265044239058,0.401520059173252,0.404202671083985,0.40633662724841,
0.40846151340549,0.412243402032006,0.423499164554404,0.602221708117882,
0.659613308106922,0.678019555852865,0.824234587801754,0.832645120334795,
0.836508081954302,0.839424590093864,0.842170989525301,0.846734519621614,
0.858458669930312,1.0574495708609,1.19049216789867,1.22517431510643,1.25212306331559,
1.25709375790634,1.25978895949415,1.26201454534388,1.26464883530674,1.2692165403338,
1.28692165845471,1.3320047190122,1.57970137127534,1.60706411844689,1.621101524216,
1.62985766206543,1.63798949437402,1.6444108018159,1.65057324303309,1.66045160573835,
1.68461343508822,1.9097790368194,1.9717667989585,2.01504389710494,2.02067686614194,
2.02351104993524,2.02555350002419,2.0277199385567,2.03077249380004,2.03891591081125,
2.16432114872236,2.30947209752093,2.43049437670148,2.44016938379904,2.4442604069529,
2.44721651275976,2.44990808177577,2.45350318561752,2.46226321896282,2.54636941134557,
2.57278292334523,2.70862982716858,2.80635390048645,2.84736612524927,2.8662928686644,
2.87473060032628,2.87798378089784,2.88023112023578,2.88243814596076,2.88510631155454,
2.89180983983446,2.97658473540921,3.10732956764125,3.2864238980362,3.32038130446213,
3.33537788547056,3.34674924321235,3.35913147235969,3.37931839964686,3.44972880413065,
3.45736116975926,3.6060804967098,3.64022881803426,3.65078217030559,3.66497474572718,
3.67165734304444,3.6772198761296,3.68421346999125,3.6953844345894,3.76147536757163,
3.81395235498242,3.84713795423668,3.86120358132372,3.871831864406,3.88346158649701,
3.90282107936014,4.00545389148317,4.06020985544135,4.07329957436829,4.07988492004892,
4.08586441651803,4.0936759947102,4.10707119856584,4.1687391476082,4.17010235673242,
4.19321050138007,4.26446602536726,4.28658885519433,4.31876022490759,4.33694782439542,
4.35360098806555,4.37752879739541,4.43731636404158,4.46983736229162,4.48278848797526,
4.49455750606592,4.52136498319555,4.57317616923912,4.59619998024701,4.61618720411073,
4.63258225492629,4.6530743427674,4.69559315704525,4.73557735688723,4.82700483158738,
4.84636140789915,4.86865313957536,4.87729501266872,4.88339485579818,4.8889067259845,
4.8990671487418,4.95161815332911,5.02710307701641,5.05583577825819,5.07829332758265,
5.09054902454767,5.10107347109147,5.11409344527995,5.14076609356116,5.1780545075291,
5.22153728595093,5.2724906679816,5.28277547964281,5.28834455049688,5.29335349931155,
5.30053851711047,5.31758695377241,5.34213411718773,5.4619890317345,5.58092706752411,
5.60293409166045,5.61583011758335,5.62709936589149,5.64117857020607,5.66988189226538,
5.78953534958973,5.95944705606483,6.05438733500089,6.07541254432156,6.07970988967138,
6.08244235744867,6.08460127660217,6.08701292940233,6.09101634202681,6.1056226459851,
6.21888960861495,6.42711593918513,6.50235988325432,6.51099187121482,6.51485406205035,
6.51778164529541,6.52088136303134,6.5256655856898,6.54002028993751,6.61812562599479,
6.73212454043503,6.86014688614911,6.9281568542819,6.93388575899285,6.93679019599724,
6.93891725431871,6.94120793924899,6.94429625266686,6.95124710861183,6.96066391199125,
7.06419576110389,7.14517730308026,7.29115987226083,7.30750948719825,7.31584271110859,
7.32243169581325,7.32944239977542,7.34009436004049,7.37189978384187,7.61804813286514,
7.67657730672564,7.69462222939699,7.69886979261845,7.7016513016184,7.7039023121736,
7.70647454335507,7.71088503758533,7.71611488781535,7.83936747883278,7.95529740506117,
8.10824053927392,8.11793614343996,8.12172575261313,8.12446704921031,8.12738725152405,
8.13127063177518,8.1397875047071,8.311275372298,8.42328494910654,8.54474739630907,
8.5528327931149,8.55579824978388,8.55788234428144,8.55983073363021,8.56250871438552,
8.5677402442379,8.60406009269718,8.70936993451049,8.9427573652302,8.99242929539948,
9.01005736126804,9.02071721814504,9.03141607675681,9.04558410355352,9.07388479213853,
9.11297774009509,9.21915080595416,9.32533433501506,9.34155791825231,9.34816423732876,
9.3537464576593,9.35905271635354,9.36675785568267,9.37706681138417,9.39742373908967,
9.46413102200946,9.51940157069119,9.53570044500064,9.54660471173925,9.55648523811236,
9.5670474691921,9.59430454729861,9.61475521428189,9.71001743759616,9.74473307909,
9.75416585364841,9.75959028267143,9.7652275119229,9.77141812278283,9.78000351965131,
9.7947341927376,9.82815473955098,9.90626691052985,9.98075854684207,10.0046799645723,
10.0212609973963,10.0359669130552,10.0641470934526,10.1058036993865,10.1445205585375,
10.1587841267585,10.1697904557197,10.1851584547576,10.2266614198589),
 .UNSPECIFIED.);
#3261=B_SPLINE_CURVE_WITH_KNOTS('',3,(#180321,#180322,#180323,#180324,#180325,
#180326,#180327,#180328,#180329,#180330,#180331,#180332,#180333,#180334),
 .UNSPECIFIED.,.F.,.F.,(4,1,1,1,1,1,1,1,1,1,1,4),(21.991148636497,22.3743502697344,
22.8728188130419,23.3712873563495,24.3682244429646,24.8666929862722,25.3651615295797,
26.3620986161948,26.8605671595024,27.35903570281,27.8575042461175,28.2743171305593),
 .UNSPECIFIED.);
#3262=B_SPLINE_CURVE_WITH_KNOTS('',3,(#180335,#180336,#180337,#180338,#180339,
#180340,#180341,#180342,#180343,#180344,#180345,#180346,#180347,#180348,
#180349,#180350,#180351,#180352),.UNSPECIFIED.,.F.,.F.,(4,2,2,2,2,2,2,2,
4),(15.7079632679496,16.5373210443875,17.3666788208254,18.1960365972634,
19.0253943737013,19.8547521501392,20.6841099265772,21.5134677030151,21.9911411882542),
 .UNSPECIFIED.);
#3263=B_SPLINE_CURVE_WITH_KNOTS('',3,(#180386,#180387,#180388,#180389,#180390,
#180391,#180392,#180393,#180394,#180395,#180396,#180397,#180398,#180399,
#180400,#180401,#180402,#180403,#180404,#180405,#180406,#180407,#180408,
#180409,#180410,#180411,#180412,#180413,#180414,#180415,#180416,#180417,
#180418,#180419,#180420,#180421,#180422,#180423,#180424,#180425,#180426,
#180427,#180428,#180429,#180430,#180431,#180432,#180433,#180434,#180435,
#180436,#180437,#180438,#180439,#180440,#180441,#180442,#180443,#180444,
#180445,#180446,#180447,#180448,#180449,#180450,#180451,#180452,#180453,
#180454,#180455,#180456,#180457,#180458,#180459,#180460,#180461,#180462,
#180463,#180464,#180465,#180466,#180467,#180468,#180469,#180470,#180471,
#180472,#180473,#180474,#180475,#180476,#180477,#180478,#180479,#180480,
#180481,#180482,#180483,#180484,#180485,#180486,#180487,#180488,#180489,
#180490,#180491),.UNSPECIFIED.,.F.,.F.,(4,3,3,3,3,3,3,3,3,3,3,3,3,3,3,3,
3,3,3,3,3,3,3,3,3,3,3,3,3,3,3,3,3,3,3,4),(-1.53973642054047,-1.48309553350524,
-1.42555125559393,-1.37417990184393,-1.36553101890543,-1.30722914366635,
-1.24872710196501,-1.21482678019219,-1.20381532475203,-1.19606511894002,
-1.18103104109073,-1.12346211407032,-1.06450347487904,-1.00508210571978,
-0.945643635900972,-0.91883932096823,-0.908401830512179,-0.847848726025719,
-0.808078428123881,-0.747890453958617,-0.687155807913238,-0.626486811594127,
-0.618542269912916,-0.612188487123754,-0.550651591095428,-0.486102847768932,
-0.421554104442437,-0.359682371036917,-0.317439297897168,-0.306618832338073,
-0.244672610384753,-0.181521847273755,-0.118198336282773,-0.0554614676464781,
-0.0217377859189241,-0.0002294502900981),.UNSPECIFIED.);
#3264=B_SPLINE_CURVE_WITH_KNOTS('',3,(#180492,#180493,#180494,#180495,#180496,
#180497,#180498,#180499,#180500,#180501,#180502,#180503,#180504,#180505,
#180506,#180507,#180508,#180509,#180510,#180511,#180512,#180513,#180514,
#180515,#180516,#180517,#180518,#180519,#180520,#180521,#180522,#180523,
#180524,#180525,#180526,#180527,#180528,#180529,#180530,#180531,#180532,
#180533,#180534,#180535,#180536,#180537,#180538,#180539,#180540,#180541,
#180542,#180543,#180544,#180545,#180546,#180547,#180548,#180549,#180550,
#180551,#180552,#180553,#180554,#180555,#180556,#180557,#180558,#180559,
#180560,#180561,#180562,#180563,#180564,#180565,#180566,#180567,#180568,
#180569,#180570,#180571,#180572,#180573,#180574,#180575,#180576,#180577,
#180578,#180579,#180580,#180581,#180582,#180583,#180584,#180585,#180586,
#180587,#180588,#180589,#180590,#180591,#180592,#180593,#180594,#180595,
#180596,#180597,#180598,#180599,#180600,#180601,#180602,#180603,#180604,
#180605,#180606,#180607,#180608,#180609,#180610,#180611,#180612),
 .UNSPECIFIED.,.F.,.F.,(4,3,3,3,3,3,3,3,3,3,3,3,3,3,3,3,3,3,3,3,3,3,3,3,
3,3,3,3,3,3,3,3,3,3,3,3,3,3,3,3,4),(-1.53496049794141,-1.47178129893344,
-1.40843691381202,-1.37435034446066,-1.3580964238932,-1.34490295184081,
-1.33579830849837,-1.27329007086333,-1.21151125381654,-1.17388303799248,
-1.16095961939653,-1.15226699516528,-1.13641946967192,-1.07545420701605,
-1.01382479674967,-0.95236079989948,-0.891797849505327,-0.863940613600807,
-0.856360761628214,-0.849031173886624,-0.788858717844872,-0.750528920592363,
-0.690182939490677,-0.630180622346739,-0.570395005112455,-0.562781680266923,
-0.555685406180827,-0.496667854192665,-0.437284384333118,-0.377900914473571,
-0.325131736658691,-0.298747147751252,-0.285554853297532,-0.276802264147644,
-0.272362558843812,-0.214747246406761,-0.157173822782883,-0.100144168788378,
-0.0443751750866251,-0.0188072533466611,0.),.UNSPECIFIED.);
#3265=B_SPLINE_CURVE_WITH_KNOTS('',3,(#182765,#182766,#182767,#182768,#182769,
#182770,#182771,#182772,#182773,#182774,#182775,#182776,#182777,#182778,
#182779,#182780,#182781,#182782,#182783,#182784,#182785,#182786,#182787,
#182788,#182789,#182790,#182791,#182792,#182793,#182794,#182795,#182796,
#182797,#182798,#182799,#182800,#182801,#182802,#182803,#182804,#182805,
#182806,#182807,#182808,#182809,#182810,#182811,#182812,#182813,#182814,
#182815,#182816,#182817,#182818,#182819,#182820,#182821,#182822,#182823,
#182824,#182825,#182826,#182827,#182828,#182829,#182830,#182831,#182832,
#182833,#182834,#182835,#182836,#182837,#182838,#182839,#182840,#182841,
#182842,#182843,#182844,#182845,#182846,#182847,#182848,#182849,#182850,
#182851,#182852,#182853,#182854,#182855,#182856,#182857,#182858,#182859,
#182860,#182861,#182862,#182863,#182864,#182865,#182866,#182867,#182868,
#182869,#182870,#182871,#182872,#182873,#182874,#182875,#182876),
 .UNSPECIFIED.,.F.,.F.,(4,3,3,3,3,3,3,3,3,3,3,3,3,3,3,3,3,3,3,3,3,3,3,3,
3,3,3,3,3,3,3,3,3,3,3,3,3,4),(0.,0.0561488103666945,0.113191923654328,0.170826554765673,
0.228516319046485,0.260964459841906,0.274244127071257,0.283126614449263,
0.341981702386085,0.358308882228168,0.416517661403603,0.475296887246886,
0.534320856699363,0.562024956257231,0.56908591189923,0.628813329120672,
0.689174298961302,0.730209481738314,0.790378517014038,0.849791355046748,
0.85680142973422,0.917257569468678,0.978700057224852,1.04030706425093,1.10152839748546,
1.11544043113767,1.14030590548036,1.15393052993428,1.16506174221691,1.22673611738623,
1.28912202595642,1.32139879568865,1.33812146091464,1.35285285612202,1.41610495574213,
1.4793560028455,1.51328802062074,1.53473167268384),.UNSPECIFIED.);
#3266=B_SPLINE_CURVE_WITH_KNOTS('',3,(#185029,#185030,#185031,#185032,#185033,
#185034,#185035,#185036,#185037,#185038,#185039,#185040,#185041,#185042,
#185043,#185044,#185045,#185046,#185047,#185048,#185049,#185050,#185051,
#185052,#185053,#185054,#185055,#185056,#185057,#185058,#185059,#185060,
#185061,#185062,#185063,#185064,#185065,#185066,#185067,#185068,#185069,
#185070,#185071,#185072,#185073,#185074,#185075,#185076,#185077,#185078,
#185079,#185080,#185081,#185082,#185083,#185084,#185085,#185086,#185087,
#185088,#185089,#185090,#185091,#185092,#185093,#185094,#185095,#185096,
#185097,#185098,#185099,#185100,#185101,#185102,#185103,#185104,#185105,
#185106,#185107,#185108,#185109,#185110,#185111,#185112,#185113,#185114,
#185115,#185116,#185117,#185118,#185119,#185120,#185121,#185122,#185123,
#185124,#185125,#185126,#185127,#185128,#185129,#185130,#185131,#185132,
#185133,#185134,#185135,#185136,#185137),.UNSPECIFIED.,.F.,.F.,(4,3,3,3,
3,3,3,3,3,3,3,3,3,3,3,3,3,3,3,3,3,3,3,3,3,3,3,3,3,3,3,3,3,3,3,3,4),(1.15016411802618E-14,
0.0626309539614373,0.126866904460898,0.190025003289835,0.254799879624557,
0.287187317791918,0.303381036875598,0.311555684298871,0.319574755959279,
0.381410337605684,0.400458029617128,0.462480297335892,0.524510838006131,
0.586011000797039,0.61188656071836,0.622914402619484,0.683664933035846,
0.744030234243724,0.787695734468564,0.850206746232349,0.912717757996134,
0.924462553129624,0.983970936762615,1.04337412846815,1.10239878786916,1.16142344727016,
1.1874531784305,1.20024516939136,1.21053455692135,1.2690351269772,1.32713644117412,
1.3696612965529,1.37838125041023,1.43578931046434,1.49222119376588,1.52088321921702,
1.53973642054052),.UNSPECIFIED.);
#3267=B_SPLINE_CURVE_WITH_KNOTS('',3,(#185306,#185307,#185308,#185309,#185310,
#185311,#185312,#185313,#185314,#185315,#185316,#185317,#185318,#185319,
#185320,#185321,#185322,#185323,#185324,#185325,#185326,#185327,#185328,
#185329,#185330,#185331,#185332,#185333,#185334,#185335,#185336,#185337,
#185338,#185339,#185340,#185341,#185342,#185343,#185344,#185345,#185346,
#185347,#185348,#185349,#185350,#185351,#185352,#185353,#185354,#185355,
#185356,#185357,#185358,#185359,#185360,#185361,#185362,#185363,#185364,
#185365,#185366,#185367,#185368,#185369,#185370,#185371,#185372,#185373,
#185374,#185375,#185376,#185377,#185378,#185379,#185380,#185381,#185382,
#185383,#185384,#185385,#185386,#185387,#185388,#185389,#185390,#185391,
#185392,#185393,#185394,#185395,#185396,#185397,#185398,#185399,#185400,
#185401,#185402,#185403,#185404,#185405,#185406,#185407,#185408,#185409,
#185410,#185411,#185412,#185413,#185414,#185415,#185416,#185417,#185418,
#185419,#185420,#185421,#185422,#185423,#185424,#185425,#185426,#185427,
#185428,#185429,#185430,#185431,#185432,#185433,#185434,#185435,#185436,
#185437,#185438),.UNSPECIFIED.,.F.,.F.,(4,3,3,3,3,3,3,3,3,3,3,3,3,3,3,3,
3,3,3,3,3,3,3,3,3,3,3,3,3,3,3,3,3,3,3,3,3,3,3,3,3,3,3,3,4),(10.3763777524407,
10.4542232522646,10.53200845239,10.6097484354634,10.6874582514084,10.7651674175212,
10.8428794104451,10.9206078434063,10.9983663362618,11.0762147773958,11.1541105300842,
11.2321249227821,11.2973484622136,11.3732369885882,11.4490299366276,11.5247441915214,
11.6003965522182,11.6760037517047,11.7535143075011,11.8290965955637,11.904686794747,
11.9802999913294,12.059247043016,12.134995161763,12.2108009921308,12.2867151833181,
12.2960881980758,12.374419020755,12.4526550318628,12.5308110341746,12.6089017742511,
12.6869419524188,12.764949288339,12.842939589717,12.9209261159944,12.9989221219091,
13.076974473593,13.1550558360197,13.233223596569,13.2948279339379,13.3750325299376,
13.4551442153435,13.5352002283623,13.6151987913663,13.6615588095422),
 .UNSPECIFIED.);
#3268=B_SPLINE_CURVE_WITH_KNOTS('',3,(#185441,#185442,#185443,#185444,#185445,
#185446,#185447,#185448,#185449,#185450,#185451,#185452,#185453,#185454,
#185455,#185456,#185457,#185458,#185459,#185460,#185461,#185462,#185463,
#185464,#185465,#185466,#185467,#185468,#185469,#185470,#185471,#185472,
#185473,#185474,#185475,#185476,#185477,#185478,#185479,#185480,#185481,
#185482,#185483,#185484,#185485,#185486,#185487,#185488,#185489,#185490,
#185491,#185492,#185493,#185494,#185495,#185496,#185497,#185498,#185499,
#185500,#185501,#185502,#185503,#185504,#185505,#185506,#185507,#185508,
#185509,#185510,#185511,#185512,#185513,#185514,#185515,#185516,#185517,
#185518,#185519,#185520,#185521,#185522),.UNSPECIFIED.,.F.,.F.,(4,3,3,3,
3,3,3,3,3,3,3,3,3,3,3,3,3,3,3,3,3,3,3,3,3,3,3,4),(11.6150328478192,11.6997947966607,
11.7845824496215,11.8693850422671,11.9541730765905,12.0389208866034,12.1144027157503,
12.1914322579443,12.2684369525882,12.3454311630728,12.4224505903829,12.4994839724856,
12.5765733135033,12.6137725836814,12.7012857649444,12.7888168916037,12.8762822893983,
12.9636620303614,13.0508381795771,13.1131424516125,13.1910545333156,13.2689596642437,
13.3468712530953,13.4248300535109,13.5028157561103,13.5808723881572,13.6125123195436,
13.6615967360777),.UNSPECIFIED.);
#3269=B_SPLINE_CURVE_WITH_KNOTS('',3,(#185528,#185529,#185530,#185531,#185532,
#185533,#185534,#185535,#185536,#185537,#185538,#185539,#185540,#185541,
#185542,#185543,#185544,#185545,#185546,#185547,#185548,#185549,#185550,
#185551,#185552,#185553,#185554,#185555,#185556,#185557,#185558,#185559,
#185560,#185561,#185562,#185563,#185564,#185565,#185566,#185567,#185568,
#185569,#185570,#185571,#185572,#185573,#185574,#185575,#185576,#185577,
#185578,#185579,#185580,#185581,#185582,#185583,#185584,#185585,#185586,
#185587,#185588,#185589,#185590,#185591,#185592,#185593,#185594,#185595,
#185596,#185597,#185598,#185599,#185600,#185601,#185602,#185603,#185604,
#185605,#185606,#185607,#185608,#185609,#185610,#185611,#185612,#185613,
#185614,#185615,#185616,#185617,#185618,#185619,#185620,#185621,#185622,
#185623,#185624,#185625,#185626,#185627,#185628,#185629,#185630,#185631,
#185632,#185633,#185634,#185635,#185636,#185637,#185638,#185639,#185640,
#185641,#185642,#185643,#185644,#185645,#185646,#185647,#185648,#185649,
#185650,#185651,#185652,#185653,#185654,#185655,#185656,#185657,#185658,
#185659,#185660,#185661,#185662,#185663,#185664,#185665,#185666,#185667,
#185668,#185669,#185670,#185671,#185672,#185673,#185674,#185675,#185676,
#185677,#185678,#185679,#185680,#185681,#185682,#185683,#185684),
 .UNSPECIFIED.,.F.,.F.,(4,3,3,3,3,3,3,3,3,3,3,3,3,3,3,3,3,3,3,3,3,3,3,3,
3,3,3,3,3,3,3,3,3,3,3,3,3,3,3,3,3,3,3,3,3,3,3,3,3,3,3,3,4),(15.7079632679498,
15.7904254740354,15.8728873318234,15.9553488481645,16.0378100299085,16.1202708839052,
16.202731417004,16.2851916360542,16.3676515479046,16.4501111594039,16.5325704774007,
16.6150295087427,16.697488260278,16.7799467388542,16.8624049513188,16.944862904519,
17.0273206053015,17.1097780605135,17.1922352770009,17.2782478647903,17.3615725592112,
17.4440391647695,17.5265049261203,17.6089698706785,17.6914340258564,17.7738974190637,
17.8563600777072,17.9388220291911,18.0212833009174,18.1037439202856,18.1862039146928,
18.268663311534,18.3511221382023,18.4335804220887,18.5160381905821,18.5984954710698,
18.6826293845192,18.7650953828176,18.8475597593663,18.9300226238083,19.0124840857651,
19.094944254839,19.1774032406137,19.2598611526566,19.3454582693571,19.4279230063008,
19.5103847785989,19.5928440246899,19.6753011828687,19.7577637017675,19.8402213730509,
19.9226801639591,19.9446380862602),.UNSPECIFIED.);
#3270=B_SPLINE_CURVE_WITH_KNOTS('',3,(#185685,#185686,#185687,#185688,#185689,
#185690,#185691,#185692,#185693,#185694,#185695,#185696,#185697,#185698,
#185699,#185700,#185701,#185702,#185703,#185704,#185705,#185706,#185707,
#185708,#185709,#185710,#185711,#185712,#185713,#185714,#185715,#185716,
#185717,#185718,#185719,#185720,#185721,#185722,#185723,#185724,#185725,
#185726,#185727,#185728,#185729,#185730,#185731,#185732,#185733,#185734,
#185735,#185736,#185737,#185738,#185739,#185740,#185741,#185742,#185743,
#185744,#185745,#185746,#185747,#185748,#185749,#185750,#185751,#185752,
#185753,#185754,#185755,#185756,#185757,#185758,#185759,#185760,#185761,
#185762,#185763,#185764,#185765,#185766),.UNSPECIFIED.,.F.,.F.,(4,3,3,3,
3,3,3,3,3,3,3,3,3,3,3,3,3,3,3,3,3,3,3,3,3,3,3,4),(13.6615588095422,13.7414980263516,
13.794197801869,13.8750436869468,13.955930516902,14.0403398051265,14.1213664543982,
14.2024435631694,14.2836058572761,14.2935676698001,14.3790087171045,14.4643727588897,
14.5495839125019,14.6346852202888,14.719586329486,14.7929375377312,14.8694577764537,
14.9459724650645,15.0224962268134,15.0990757955442,15.1756865300405,15.252380955568,
15.2923074056623,15.379635702775,15.4667829706427,15.5537849884522,15.6404952190153,
15.7079632679498),.UNSPECIFIED.);
#3271=B_SPLINE_CURVE_WITH_KNOTS('',3,(#185768,#185769,#185770,#185771,#185772,
#185773,#185774,#185775,#185776,#185777,#185778,#185779,#185780,#185781,
#185782,#185783,#185784,#185785,#185786,#185787,#185788,#185789,#185790,
#185791,#185792,#185793,#185794,#185795,#185796,#185797,#185798,#185799,
#185800,#185801,#185802,#185803,#185804,#185805,#185806,#185807,#185808,
#185809,#185810,#185811,#185812,#185813,#185814,#185815,#185816,#185817,
#185818,#185819,#185820,#185821,#185822,#185823,#185824,#185825,#185826,
#185827,#185828,#185829,#185830,#185831,#185832,#185833,#185834,#185835,
#185836,#185837,#185838,#185839,#185840,#185841,#185842,#185843,#185844,
#185845,#185846,#185847,#185848,#185849),.UNSPECIFIED.,.F.,.F.,(4,3,3,3,
3,3,3,3,3,3,3,3,3,3,3,3,3,3,3,3,3,3,3,3,3,3,3,4),(13.6615967360777,13.7400356036608,
13.8184202198503,13.8967647778476,13.9750834408796,14.0546045176954,14.1329331115179,
14.2112797336207,14.2896572211474,14.370055929712,14.4485745617826,14.5299133085942,
14.6112520554058,14.6871405817804,14.7629335298198,14.8386477847136,14.9143001454103,
14.9899073448968,15.0674179006932,15.1430001887558,15.2185903879391,15.2942035845215,
15.3731506362081,15.4488987549552,15.5247045853228,15.6006187765102,15.6099917912679,
15.7079632679497),.UNSPECIFIED.);
#3272=B_SPLINE_CURVE_WITH_KNOTS('',3,(#185850,#185851,#185852,#185853,#185854,
#185855,#185856,#185857,#185858,#185859,#185860,#185861,#185862,#185863,
#185864,#185865,#185866,#185867,#185868,#185869,#185870,#185871,#185872,
#185873,#185874,#185875,#185876,#185877,#185878,#185879,#185880,#185881,
#185882,#185883,#185884,#185885,#185886,#185887,#185888,#185889,#185890,
#185891,#185892,#185893,#185894,#185895,#185896,#185897,#185898,#185899,
#185900,#185901,#185902,#185903,#185904,#185905,#185906,#185907,#185908,
#185909,#185910,#185911,#185912,#185913,#185914,#185915,#185916,#185917,
#185918,#185919,#185920,#185921,#185922,#185923,#185924,#185925,#185926,
#185927,#185928,#185929,#185930,#185931,#185932,#185933,#185934,#185935,
#185936,#185937,#185938,#185939,#185940,#185941,#185942,#185943,#185944,
#185945,#185946,#185947,#185948,#185949,#185950,#185951,#185952,#185953,
#185954,#185955,#185956,#185957,#185958,#185959,#185960,#185961,#185962,
#185963,#185964,#185965,#185966,#185967,#185968,#185969,#185970,#185971,
#185972,#185973,#185974,#185975,#185976,#185977,#185978,#185979,#185980,
#185981,#185982,#185983,#185984,#185985,#185986,#185987,#185988,#185989,
#185990,#185991,#185992,#185993,#185994,#185995,#185996,#185997,#185998,
#185999,#186000,#186001,#186002,#186003,#186004,#186005,#186006,#186007,
#186008,#186009,#186010,#186011,#186012,#186013,#186014,#186015,#186016,
#186017,#186018,#186019,#186020,#186021),.UNSPECIFIED.,.F.,.F.,(4,3,3,3,
3,3,3,3,3,3,3,3,3,3,3,3,3,3,3,3,3,3,3,3,3,3,3,3,3,3,3,3,3,3,3,3,3,3,3,3,
3,3,3,3,3,3,3,3,3,3,3,3,3,3,3,3,3,4),(15.7079632680314,15.7849793680378,
15.8619042262796,15.9387539940356,16.0155447640273,16.092293415879,16.1690200754061,
16.2457392290518,16.322465356366,16.3992465261494,16.4760567060718,16.5529541571788,
16.6087315271301,16.6889240591598,16.7690457679708,16.8491062886745,16.9291045159356,
17.0090647219482,17.0889926797773,17.1081013950612,17.1889472801389,17.2698341100947,
17.3542433983191,17.4352700475907,17.5163471563621,17.5975094504688,17.6074712629923,
17.6929123102967,17.7782763520816,17.8634875056938,17.948588813481,18.033489922678,
18.1068411309234,18.1833613696459,18.2598760582566,18.336399820006,18.4129793887368,
18.4895901232335,18.5662845487608,18.6062109988545,18.6857500135597,18.7652285718676,
18.8446589586676,18.9240534212649,19.0034241783015,19.0827960418154,19.1621705106544,
19.2415586849842,19.3209716725316,19.4004560674958,19.4799788538006,19.5595906113493,
19.6049507347167,19.6826484633713,19.760232488877,19.8377508195051,19.9152048727785,
19.9450452040236),.UNSPECIFIED.);
#3273=B_SPLINE_CURVE_WITH_KNOTS('',3,(#186027,#186028,#186029,#186030,#186031,
#186032,#186033,#186034,#186035,#186036,#186037,#186038,#186039,#186040,
#186041,#186042,#186043,#186044,#186045,#186046,#186047,#186048,#186049,
#186050,#186051,#186052,#186053,#186054,#186055,#186056,#186057,#186058,
#186059,#186060,#186061,#186062,#186063,#186064,#186065,#186066,#186067,
#186068,#186069,#186070,#186071,#186072,#186073,#186074,#186075,#186076,
#186077,#186078,#186079,#186080,#186081,#186082,#186083,#186084,#186085,
#186086,#186087,#186088,#186089,#186090,#186091,#186092,#186093,#186094,
#186095,#186096,#186097,#186098,#186099,#186100,#186101,#186102,#186103,
#186104,#186105,#186106,#186107,#186108,#186109,#186110,#186111,#186112,
#186113,#186114,#186115,#186116,#186117,#186118,#186119,#186120,#186121,
#186122,#186123,#186124,#186125,#186126,#186127,#186128,#186129,#186130,
#186131,#186132,#186133,#186134,#186135,#186136,#186137,#186138,#186139,
#186140,#186141,#186142,#186143,#186144,#186145,#186146,#186147,#186148,
#186149,#186150,#186151,#186152,#186153,#186154,#186155,#186156,#186157,
#186158,#186159,#186160,#186161,#186162,#186163,#186164,#186165,#186166,
#186167,#186168,#186169,#186170,#186171,#186172,#186173,#186174,#186175,
#186176,#186177,#186178,#186179,#186180,#186181,#186182,#186183,#186184,
#186185,#186186,#186187,#186188,#186189,#186190,#186191,#186192,#186193,
#186194,#186195),.UNSPECIFIED.,.F.,.F.,(4,3,3,3,3,3,3,3,3,3,3,3,3,3,3,3,
3,3,3,3,3,3,3,3,3,3,3,3,3,3,3,3,3,3,3,3,3,3,3,3,3,3,3,3,3,3,3,3,3,3,3,3,
3,3,3,3,4),(21.9911485751294,22.0726737883961,22.154293407887,22.2360745796861,
22.2834855566976,22.3630326170872,22.4425194078618,22.5219581940468,22.6013612031951,
22.6807406342982,22.7601213131529,22.839504673154,22.918901797279,22.99832377612,
23.0778171653712,23.1573489506337,23.236969634884,23.2822252925598,23.3598810959616,
23.4374507067199,23.5149480581544,23.5923767409349,23.6697656311381,23.7471285688627,
23.7815951604909,23.8650899412174,23.9487415907991,24.0326319574194,24.1166363736405,
24.2008273023064,24.280965028422,24.3584623761376,24.4358776955364,24.5132266162488,
24.5905247202617,24.6677875526241,24.7450435667727,24.8222987213559,24.8995670637133,
24.9768626459753,25.0542462549469,25.1316754641953,25.2092248062607,25.2797047642841,
25.3557591657399,25.4317180853077,25.5075983137797,25.5834165609126,25.6591894742179,
25.7349418055907,25.8106859395986,25.8864368811234,25.9622096389604,26.0380580195377,
26.113949162002,26.1899412660023,26.2270156338182),.UNSPECIFIED.);
#3274=B_SPLINE_CURVE_WITH_KNOTS('',3,(#186196,#186197,#186198,#186199,#186200,
#186201,#186202,#186203,#186204,#186205,#186206,#186207,#186208,#186209,
#186210,#186211,#186212,#186213,#186214,#186215,#186216,#186217,#186218,
#186219,#186220,#186221,#186222,#186223,#186224,#186225,#186226,#186227,
#186228,#186229,#186230,#186231,#186232,#186233,#186234,#186235,#186236,
#186237,#186238,#186239,#186240,#186241,#186242,#186243,#186244,#186245,
#186246,#186247,#186248,#186249,#186250,#186251,#186252,#186253,#186254,
#186255,#186256,#186257,#186258,#186259,#186260,#186261,#186262,#186263,
#186264,#186265,#186266,#186267,#186268,#186269,#186270,#186271),
 .UNSPECIFIED.,.F.,.F.,(4,3,3,3,3,3,3,3,3,3,3,3,3,3,3,3,3,3,3,3,3,3,3,3,
3,4),(19.9446380862602,20.0270996900187,20.1095606278978,20.1920209272959,
20.274480615609,20.3569397202312,20.4393982685543,20.5218562879684,20.6043138058615,
20.6909909789407,20.7734577645493,20.8559228776805,20.9383864279875,21.0208485251015,
21.1033092786334,21.1857687981754,21.2682271933024,21.3506845735733,21.4331509593925,
21.5156141610166,21.5980746169651,21.6805327656015,21.7629983696133,21.8454582481907,
21.9279223599272,21.9911485751294),.UNSPECIFIED.);
#3275=B_SPLINE_CURVE_WITH_KNOTS('',3,(#186273,#186274,#186275,#186276,#186277,
#186278,#186279,#186280,#186281,#186282,#186283,#186284,#186285,#186286,
#186287,#186288,#186289,#186290,#186291,#186292,#186293,#186294,#186295,
#186296,#186297,#186298,#186299,#186300,#186301,#186302,#186303,#186304,
#186305,#186306,#186307,#186308,#186309,#186310,#186311,#186312,#186313,
#186314,#186315,#186316,#186317,#186318,#186319,#186320,#186321,#186322,
#186323,#186324,#186325,#186326,#186327,#186328,#186329,#186330,#186331,
#186332,#186333,#186334,#186335,#186336,#186337,#186338,#186339,#186340,
#186341,#186342,#186343,#186344,#186345,#186346,#186347,#186348,#186349,
#186350,#186351),.UNSPECIFIED.,.F.,.F.,(4,3,3,3,3,3,3,3,3,3,3,3,3,3,3,3,
3,3,3,3,3,3,3,3,3,3,4),(19.9450452040236,20.0246829033357,20.1043206026478,
20.1877984857314,20.271432448796,20.3553042128251,20.4392896029479,20.5234611307425,
20.6036904705788,20.6811895841971,20.758606693462,20.8359574260042,20.9132573618335,
20.9905220440399,21.0677799289761,21.1450369669192,21.2223072034865,21.2996046890923,
21.3769902053478,21.4544213269495,21.5319725714035,21.602430206441,21.6880000236565,
21.7731542207063,21.8580499988725,21.9425343151533,21.9911485750218),
 .UNSPECIFIED.);
#3276=B_SPLINE_CURVE_WITH_KNOTS('',3,(#186352,#186353,#186354,#186355,#186356,
#186357,#186358,#186359,#186360,#186361,#186362,#186363,#186364,#186365,
#186366,#186367,#186368,#186369,#186370,#186371,#186372,#186373,#186374,
#186375,#186376,#186377,#186378,#186379,#186380,#186381,#186382,#186383,
#186384,#186385,#186386,#186387,#186388,#186389,#186390,#186391,#186392,
#186393,#186394,#186395,#186396,#186397,#186398,#186399,#186400,#186401,
#186402,#186403,#186404,#186405,#186406,#186407,#186408,#186409,#186410,
#186411,#186412,#186413,#186414,#186415,#186416,#186417,#186418,#186419,
#186420,#186421,#186422,#186423,#186424,#186425,#186426,#186427,#186428,
#186429,#186430,#186431,#186432,#186433,#186434,#186435,#186436,#186437,
#186438,#186439,#186440,#186441,#186442,#186443,#186444,#186445,#186446,
#186447,#186448,#186449,#186450,#186451,#186452,#186453,#186454,#186455,
#186456,#186457,#186458,#186459,#186460,#186461,#186462,#186463,#186464,
#186465,#186466,#186467,#186468,#186469,#186470,#186471,#186472,#186473,
#186474,#186475,#186476,#186477,#186478,#186479,#186480,#186481,#186482,
#186483,#186484,#186485,#186486,#186487,#186488,#186489,#186490,#186491,
#186492,#186493,#186494,#186495,#186496,#186497,#186498,#186499,#186500,
#186501,#186502,#186503,#186504,#186505,#186506,#186507,#186508,#186509,
#186510,#186511,#186512,#186513,#186514,#186515,#186516,#186517),
 .UNSPECIFIED.,.F.,.F.,(4,3,3,3,3,3,3,3,3,3,3,3,3,3,3,3,3,3,3,3,3,3,3,3,
3,3,3,3,3,3,3,3,3,3,3,3,3,3,3,3,3,3,3,3,3,3,3,3,3,3,3,3,3,3,3,4),(21.9911485751293,
22.0674915472375,22.1438420973543,22.2202147938274,22.2966242166123,22.3731393315767,
22.4497090626853,22.5264184263459,22.6011699423032,22.6797052338162,22.758147708736,
22.8365118763931,22.9148121906576,22.9930630597149,23.0712819476143,23.1494841985966,
23.2276828124449,23.3058907843889,23.3841537662605,23.462445209092,23.5408203684972,
23.5999096781654,23.6795524499783,23.7591249324589,23.8386380197198,23.9180942011272,
23.9975162177901,24.0769137064076,24.0992795460965,24.180509249891,24.2617877412199,
24.3460031594218,24.4274336038537,24.5130415089407,24.5986494140276,24.6838926817792,
24.7690577231954,24.8540720556098,24.9389793277104,25.0236937917839,25.0980192819587,
25.1745623672306,25.2510999951783,25.3276467728086,25.4042493995774,25.4808832323577,
25.5576007087503,25.5973891498898,25.6769295574756,25.7564129775381,25.8358505730622,
25.9152534756883,25.9946399097677,26.0740134122289,26.1534040307968,26.2275350298928),
 .UNSPECIFIED.);
#3277=B_SPLINE_CURVE_WITH_KNOTS('',3,(#186523,#186524,#186525,#186526,#186527,
#186528,#186529,#186530,#186531,#186532,#186533,#186534,#186535,#186536,
#186537,#186538,#186539,#186540,#186541,#186542,#186543,#186544,#186545,
#186546,#186547,#186548,#186549,#186550,#186551,#186552,#186553,#186554,
#186555,#186556,#186557,#186558,#186559,#186560,#186561,#186562,#186563,
#186564,#186565,#186566,#186567,#186568,#186569,#186570,#186571,#186572,
#186573,#186574,#186575,#186576,#186577,#186578,#186579,#186580,#186581,
#186582,#186583,#186584,#186585,#186586,#186587,#186588,#186589,#186590,
#186591,#186592,#186593,#186594,#186595,#186596,#186597,#186598,#186599,
#186600,#186601,#186602,#186603,#186604,#186605,#186606,#186607,#186608,
#186609,#186610,#186611,#186612,#186613,#186614,#186615,#186616,#186617,
#186618,#186619,#186620,#186621,#186622,#186623,#186624,#186625,#186626,
#186627,#186628,#186629,#186630,#186631,#186632,#186633,#186634,#186635,
#186636,#186637,#186638,#186639,#186640,#186641,#186642,#186643,#186644,
#186645,#186646,#186647,#186648,#186649,#186650,#186651,#186652,#186653,
#186654,#186655,#186656,#186657,#186658,#186659,#186660,#186661,#186662,
#186663,#186664,#186665,#186666,#186667,#186668,#186669,#186670,#186671,
#186672,#186673,#186674,#186675,#186676,#186677,#186678,#186679,#186680,
#186681,#186682,#186683,#186684,#186685,#186686,#186687,#186688,#186689,
#186690,#186691,#186692,#186693,#186694),.UNSPECIFIED.,.F.,.F.,(4,3,3,3,
3,3,3,3,3,3,3,3,3,3,3,3,3,3,3,3,3,3,3,3,3,3,3,3,3,3,3,3,3,3,3,3,3,3,3,3,
3,3,3,3,3,3,3,3,3,3,3,3,3,3,3,3,3,4),(28.274333882309,28.2759239718707,
28.3611672689883,28.4463323419476,28.5313467086318,28.6162540162447,28.7009685173684,
28.7752938398018,28.8518368432037,28.9283743879683,29.0049210811626,29.0815236218832,
29.1581573676352,29.2348747559209,29.2746637077329,29.3542108077167,29.4336976389849,
29.5131364664643,29.5925395176092,29.6719189913133,29.7512997134264,29.8306831170345,
29.9100802850296,29.9895023079184,30.0689957411893,30.1485275704695,30.2281482983423,
30.2734034435951,30.3510592018246,30.4286287675895,30.506126074255,30.5835547127227,
30.6609435588824,30.7383064530928,30.7727733115261,30.8562681185707,30.9399197955601,
31.0238101908009,31.1078146361851,31.1920055944091,31.2721431794572,31.3496405261199,
31.4270558444663,31.5044047641279,31.5817028670928,31.6589656984109,31.7362217115251,
31.8134768650799,31.8907452064159,31.9680407876647,32.0454243956414,32.1228536039036,
32.2004029450071,32.2708829153194,32.3469363365831,32.4229060797825,32.4987893170115,
32.5119151775653),.UNSPECIFIED.);
#3278=B_SPLINE_CURVE_WITH_KNOTS('',3,(#186695,#186696,#186697,#186698,#186699,
#186700,#186701,#186702,#186703,#186704,#186705,#186706,#186707,#186708,
#186709,#186710,#186711,#186712,#186713,#186714,#186715,#186716,#186717,
#186718,#186719,#186720,#186721,#186722,#186723,#186724,#186725,#186726,
#186727,#186728,#186729,#186730,#186731,#186732,#186733,#186734,#186735,
#186736,#186737,#186738,#186739,#186740,#186741,#186742,#186743,#186744,
#186745,#186746,#186747,#186748,#186749,#186750,#186751,#186752,#186753,
#186754,#186755,#186756,#186757,#186758,#186759,#186760,#186761,#186762,
#186763,#186764,#186765,#186766,#186767,#186768,#186769,#186770,#186771,
#186772,#186773,#186774,#186775,#186776),.UNSPECIFIED.,.F.,.F.,(4,3,3,3,
3,3,3,3,3,3,3,3,3,3,3,3,3,3,3,3,3,3,3,3,3,3,3,4),(26.2270156338182,26.2784445001463,
26.3569804390247,26.4354235674566,26.5137883938099,26.5920893709949,26.6703409062375,
26.7485604625677,26.8267633829094,26.9049626661928,26.9831713067947,27.0614349524559,
27.1397270569375,27.2181028689108,27.2771842360085,27.356826142552,27.4363977624051,
27.5159099914782,27.5953653252633,27.6747865014101,27.7541831630675,27.7765541039396,
27.8577521425003,27.938998564499,28.0228323939217,28.1042298637321,28.189281872961,
28.2743338821898),.UNSPECIFIED.);
#3279=B_SPLINE_CURVE_WITH_KNOTS('',3,(#186778,#186779,#186780,#186781,#186782,
#186783,#186784,#186785,#186786,#186787,#186788,#186789,#186790,#186791,
#186792,#186793,#186794,#186795,#186796,#186797,#186798,#186799,#186800,
#186801,#186802,#186803,#186804,#186805,#186806,#186807,#186808,#186809,
#186810,#186811,#186812,#186813,#186814,#186815,#186816,#186817,#186818,
#186819,#186820,#186821,#186822,#186823,#186824,#186825,#186826,#186827,
#186828,#186829,#186830,#186831,#186832,#186833,#186834,#186835,#186836,
#186837,#186838,#186839,#186840,#186841,#186842,#186843,#186844,#186845,
#186846,#186847,#186848,#186849,#186850,#186851,#186852,#186853,#186854,
#186855,#186856,#186857,#186858,#186859),.UNSPECIFIED.,.F.,.F.,(4,3,3,3,
3,3,3,3,3,3,3,3,3,3,3,3,3,3,3,3,3,3,3,3,3,3,3,4),(26.2275350298928,26.3069550152091,
26.3864462180847,26.4659751401512,26.5455941531207,26.5961288857519,26.6737846891537,
26.7513542999119,26.8288516513463,26.9062803341267,26.9836692243299,27.0610321620547,
27.095498753683,27.1789935344097,27.2626451839921,27.3465355506126,27.4305399668345,
27.5147308955004,27.5948686216141,27.6711802459415,27.7473856470892,27.8235298949968,
27.8996279536925,27.9756947522701,28.0517610378082,28.1278240927466,28.2039301637871,
28.2743338823088),.UNSPECIFIED.);
#3280=B_SPLINE_CURVE_WITH_KNOTS('',3,(#186860,#186861,#186862,#186863,#186864,
#186865,#186866,#186867,#186868,#186869,#186870,#186871,#186872,#186873,
#186874,#186875,#186876,#186877,#186878,#186879,#186880,#186881,#186882,
#186883,#186884,#186885,#186886,#186887,#186888,#186889,#186890,#186891,
#186892,#186893,#186894,#186895,#186896,#186897,#186898,#186899,#186900,
#186901,#186902,#186903,#186904,#186905,#186906,#186907,#186908,#186909,
#186910,#186911,#186912,#186913,#186914,#186915,#186916,#186917,#186918,
#186919,#186920,#186921,#186922,#186923,#186924,#186925,#186926,#186927,
#186928,#186929,#186930,#186931,#186932,#186933,#186934,#186935,#186936,
#186937,#186938,#186939,#186940,#186941,#186942,#186943,#186944,#186945,
#186946,#186947,#186948,#186949,#186950,#186951,#186952,#186953,#186954,
#186955,#186956,#186957,#186958,#186959,#186960,#186961,#186962,#186963,
#186964,#186965,#186966,#186967,#186968,#186969,#186970,#186971,#186972,
#186973,#186974,#186975,#186976,#186977,#186978,#186979,#186980,#186981,
#186982,#186983,#186984,#186985,#186986,#186987,#186988,#186989,#186990,
#186991,#186992,#186993,#186994,#186995,#186996,#186997,#186998,#186999,
#187000,#187001,#187002,#187003,#187004,#187005,#187006,#187007,#187008,
#187009,#187010,#187011,#187012,#187013,#187014,#187015,#187016,#187017,
#187018,#187019,#187020,#187021,#187022,#187023,#187024,#187025,#187026,
#187027,#187028),.UNSPECIFIED.,.F.,.F.,(4,3,3,3,3,3,3,3,3,3,3,3,3,3,3,3,
3,3,3,3,3,3,3,3,3,3,3,3,3,3,3,3,3,3,3,3,3,3,3,3,3,3,3,3,3,3,3,3,3,3,3,3,
3,3,3,3,4),(28.2743338824115,28.3702372203524,28.4672653007767,28.5654433825602,
28.5936083574763,28.669659806962,28.7456163996417,28.8214949223753,28.8973120818936,
28.9730845234877,29.050492469719,29.1262405199265,29.2019965838076,29.2777756722776,
29.3564187775428,29.4323316922924,29.5083020741959,29.584379569782,29.5923480933385,
29.6708840322169,29.7493271606488,29.8276919870021,29.9059929641869,29.9842444994295,
30.0624640557597,30.1406669761014,30.2188662593847,30.2970748999866,30.3753385456478,
30.4536306501294,30.5320064621028,30.5910878292007,30.6707297357442,30.7503013555972,
30.8298135846705,30.9092689184556,30.9886900946024,31.0680867562597,31.0904576971318,
31.1716877944818,31.2529666862774,31.3371819059738,31.4186127601752,31.504220162619,
31.5898275650629,31.6750708621805,31.7602359351399,31.8452503018241,31.9301576094371,
32.0148721105607,32.0891974329939,32.165737337151,32.2422704943354,32.3188353761641,
32.3954178255919,32.4720627947504,32.5104908631869),.UNSPECIFIED.);
#3281=B_SPLINE_CURVE_WITH_KNOTS('',3,(#187034,#187035,#187036,#187037,#187038,
#187039,#187040,#187041,#187042,#187043,#187044,#187045,#187046,#187047,
#187048,#187049,#187050,#187051,#187052,#187053,#187054,#187055,#187056,
#187057,#187058,#187059,#187060,#187061,#187062,#187063,#187064,#187065,
#187066,#187067,#187068,#187069,#187070,#187071,#187072,#187073,#187074,
#187075,#187076,#187077,#187078,#187079,#187080,#187081,#187082,#187083,
#187084,#187085,#187086,#187087,#187088,#187089,#187090,#187091,#187092,
#187093,#187094,#187095,#187096,#187097,#187098,#187099,#187100,#187101,
#187102,#187103,#187104,#187105,#187106,#187107,#187108,#187109,#187110,
#187111,#187112,#187113,#187114,#187115,#187116,#187117,#187118,#187119,
#187120,#187121,#187122,#187123,#187124,#187125,#187126,#187127,#187128,
#187129,#187130,#187131,#187132,#187133,#187134,#187135,#187136,#187137,
#187138,#187139,#187140,#187141,#187142,#187143,#187144,#187145,#187146,
#187147,#187148,#187149,#187150,#187151,#187152,#187153,#187154,#187155,
#187156,#187157,#187158,#187159,#187160,#187161,#187162,#187163,#187164,
#187165,#187166,#187167,#187168,#187169,#187170,#187171,#187172,#187173,
#187174,#187175,#187176,#187177,#187178,#187179,#187180,#187181,#187182,
#187183,#187184,#187185,#187186,#187187,#187188,#187189,#187190,#187191,
#187192,#187193,#187194,#187195,#187196,#187197,#187198,#187199),
 .UNSPECIFIED.,.F.,.F.,(4,3,3,3,3,3,3,3,3,3,3,3,3,3,3,3,3,3,3,3,3,3,3,3,
3,3,3,3,3,3,3,3,3,3,3,3,3,3,3,3,3,3,3,3,3,3,3,3,3,3,3,3,3,3,3,4),(34.5575191896334,
34.6328940346518,34.7082620826187,34.7677322549749,34.8489623516055,34.9302412426614,
35.0144564627225,35.0958873161479,35.181494719527,35.267102122906,35.3523454212009,
35.4375104953517,35.5225248632253,35.6074321720173,35.6921466742857,35.7664719908371,
35.8430149938238,35.9195525381677,35.9960992309372,36.0727017712263,36.1493355165433,
36.2260529043906,36.2658418587681,36.3453889588483,36.4248757902154,36.5043146177953,
36.583717669043,36.6630971428506,36.7424778650691,36.8218612687835,36.9012584368857,
36.980680459882,37.0601738932601,37.1397057226475,37.2193264506264,37.2645815946303,
37.3422373528249,37.4198069185552,37.4973042251867,37.5747328636208,37.6521217097477,
37.7294846039253,37.7639514625614,37.8474462696074,37.9310979465984,38.0149883418392,
38.0989927872228,38.1831837454459,38.2633213304925,38.3408158465093,38.4182316833689,
38.4955830039888,38.5728791596455,38.650142327992,38.7273960430041,38.7941774417346),
 .UNSPECIFIED.);
#3282=B_SPLINE_CURVE_WITH_KNOTS('',3,(#187200,#187201,#187202,#187203,#187204,
#187205,#187206,#187207,#187208,#187209,#187210,#187211,#187212,#187213,
#187214,#187215,#187216,#187217,#187218,#187219,#187220,#187221,#187222,
#187223,#187224,#187225,#187226,#187227,#187228,#187229,#187230,#187231,
#187232,#187233,#187234,#187235,#187236,#187237,#187238,#187239,#187240,
#187241,#187242,#187243,#187244,#187245,#187246,#187247,#187248,#187249,
#187250,#187251,#187252,#187253,#187254,#187255,#187256,#187257,#187258,
#187259,#187260,#187261,#187262,#187263,#187264,#187265,#187266,#187267,
#187268,#187269,#187270,#187271,#187272,#187273,#187274,#187275,#187276,
#187277,#187278,#187279,#187280,#187281),.UNSPECIFIED.,.F.,.F.,(4,3,3,3,
3,3,3,3,3,3,3,3,3,3,3,3,3,3,3,3,3,3,3,3,3,3,3,4),(32.5119151775653,32.5877233929837,
32.6634897706898,32.7392563807513,32.8150046791788,32.8907632674804,32.9665471583332,
33.0424205102964,33.118339341866,33.1943848037333,33.2696226511816,33.3481585912356,
33.4266017208537,33.5049665484019,33.5832675267887,33.6615190632388,33.7397386207794,
33.8179415423325,33.8961408268268,33.9743494686376,34.0526131154981,34.1309052211746,
34.2092810343257,34.2683623870438,34.3540517742216,34.4396129126855,34.5249606887323,
34.5575191894886),.UNSPECIFIED.);
#3283=B_SPLINE_CURVE_WITH_KNOTS('',3,(#187283,#187284,#187285,#187286,#187287,
#187288,#187289,#187290,#187291,#187292,#187293,#187294,#187295,#187296,
#187297,#187298,#187299,#187300,#187301,#187302,#187303,#187304,#187305,
#187306,#187307,#187308,#187309,#187310,#187311,#187312,#187313,#187314,
#187315,#187316,#187317,#187318,#187319,#187320,#187321,#187322,#187323,
#187324,#187325,#187326,#187327,#187328,#187329,#187330,#187331,#187332,
#187333,#187334,#187335,#187336,#187337,#187338,#187339,#187340,#187341,
#187342,#187343,#187344,#187345,#187346,#187347,#187348,#187349,#187350,
#187351,#187352,#187353,#187354,#187355,#187356,#187357,#187358,#187359,
#187360,#187361,#187362,#187363,#187364),.UNSPECIFIED.,.F.,.F.,(4,3,3,3,
3,3,3,3,3,3,3,3,3,3,3,3,3,3,3,3,3,3,3,3,3,3,3,4),(32.5104908631869,32.588567300925,
32.6681144009088,32.7476012321771,32.8270400596564,32.9064431108012,32.9858225845053,
33.0652033066184,33.1445867102266,33.2239838782218,33.3034059011105,33.3828993343814,
33.4624311636617,33.5420518915345,33.5873070367872,33.6649627950167,33.7425323607817,
33.8200296674471,33.8974583059148,33.9748471520747,34.0522100462851,34.0866769047183,
34.1690285568191,34.2515062577281,34.3341851486432,34.4169666610317,34.4999193372927,
34.5575191894884),.UNSPECIFIED.);
#3284=B_SPLINE_CURVE_WITH_KNOTS('',3,(#187365,#187366,#187367,#187368,#187369,
#187370,#187371,#187372,#187373,#187374,#187375,#187376,#187377,#187378,
#187379,#187380,#187381,#187382,#187383,#187384,#187385,#187386,#187387,
#187388,#187389,#187390,#187391,#187392,#187393,#187394,#187395,#187396,
#187397,#187398,#187399,#187400,#187401,#187402,#187403,#187404,#187405,
#187406,#187407,#187408,#187409,#187410,#187411,#187412,#187413,#187414,
#187415,#187416,#187417,#187418,#187419,#187420,#187421,#187422,#187423,
#187424,#187425,#187426,#187427,#187428,#187429,#187430,#187431,#187432,
#187433,#187434,#187435,#187436,#187437,#187438,#187439,#187440,#187441,
#187442,#187443,#187444,#187445,#187446,#187447,#187448,#187449,#187450,
#187451,#187452,#187453,#187454,#187455,#187456,#187457,#187458,#187459,
#187460,#187461,#187462,#187463,#187464,#187465,#187466,#187467,#187468,
#187469,#187470,#187471,#187472,#187473,#187474,#187475,#187476,#187477,
#187478,#187479,#187480,#187481,#187482,#187483,#187484,#187485,#187486,
#187487,#187488,#187489,#187490,#187491,#187492,#187493,#187494,#187495,
#187496,#187497,#187498,#187499,#187500,#187501,#187502,#187503,#187504,
#187505,#187506,#187507,#187508,#187509,#187510,#187511,#187512,#187513,
#187514,#187515,#187516,#187517,#187518,#187519,#187520,#187521,#187522,
#187523,#187524,#187525,#187526,#187527,#187528,#187529,#187530,#187531,
#187532,#187533,#187534,#187535,#187536),.UNSPECIFIED.,.F.,.F.,(4,3,3,3,
3,3,3,3,3,3,3,3,3,3,3,3,3,3,3,3,3,3,3,3,3,3,3,3,3,3,3,3,3,3,3,3,3,3,3,3,
3,3,3,3,3,3,3,3,3,3,3,3,3,3,3,3,3,4),(34.5575191895731,34.5860467726494,
34.6635441193121,34.7409594376583,34.8183083573198,34.8956064602846,34.9728692916032,
35.0501253047173,35.1273804582721,35.2046487996079,35.2819443808566,35.3593279888334,
35.4367571970956,35.5143065381991,35.5847865085116,35.6608379562356,35.7367945471342,
35.8126730680686,35.8884902257706,35.9642626655325,36.0416706128877,36.117418661229,
36.1931747232324,36.2689538098139,36.3475969184539,36.4235098313013,36.499480211296,
36.5755577049752,36.5835262443738,36.6620621844278,36.7405053140459,36.8188701415938,
36.8971711199808,36.9754226564305,37.0536422139711,37.1318451355242,37.2100444200183,
37.288253061829,37.3665167086894,37.4448088143658,37.5231846275169,37.582265980236,
37.6619078866581,37.7414795063955,37.8209917353596,37.9004470690454,37.9798682450988,
38.0592649066717,38.081635848167,38.1628659447976,38.244144835853,38.3283600559143,
38.4097909093397,38.4953983127189,38.5810057160981,38.6662559661317,38.7514079237039,
38.7947201030774),.UNSPECIFIED.);
#3285=B_SPLINE_CURVE_WITH_KNOTS('',3,(#187542,#187543,#187544,#187545,#187546,
#187547,#187548,#187549,#187550,#187551,#187552,#187553,#187554,#187555,
#187556,#187557,#187558,#187559,#187560,#187561,#187562,#187563,#187564,
#187565,#187566,#187567,#187568,#187569,#187570,#187571,#187572,#187573,
#187574,#187575,#187576,#187577,#187578,#187579,#187580,#187581,#187582,
#187583,#187584,#187585,#187586,#187587,#187588,#187589,#187590,#187591,
#187592,#187593,#187594,#187595,#187596,#187597,#187598,#187599,#187600,
#187601,#187602,#187603,#187604,#187605,#187606,#187607,#187608,#187609,
#187610,#187611,#187612,#187613,#187614,#187615,#187616,#187617,#187618,
#187619,#187620,#187621,#187622,#187623,#187624,#187625,#187626,#187627,
#187628,#187629,#187630,#187631,#187632,#187633,#187634,#187635,#187636,
#187637,#187638,#187639,#187640,#187641,#187642,#187643,#187644,#187645,
#187646,#187647,#187648,#187649,#187650,#187651,#187652,#187653,#187654,
#187655,#187656,#187657,#187658,#187659,#187660,#187661,#187662,#187663,
#187664,#187665,#187666,#187667,#187668,#187669,#187670,#187671,#187672,
#187673,#187674,#187675,#187676,#187677,#187678,#187679,#187680,#187681,
#187682,#187683,#187684,#187685,#187686,#187687,#187688,#187689,#187690,
#187691,#187692,#187693,#187694,#187695,#187696,#187697,#187698,#187699,
#187700,#187701,#187702,#187703,#187704,#187705,#187706,#187707),
 .UNSPECIFIED.,.F.,.F.,(4,3,3,3,3,3,3,3,3,3,3,3,3,3,3,3,3,3,3,3,3,3,3,3,
3,3,3,3,3,3,3,3,3,3,3,3,3,3,3,3,3,3,3,3,3,3,3,3,3,3,3,3,3,3,3,4),(40.840704496776,
40.9237050242495,41.0076639027069,41.0909770223219,41.1752587802005,41.2595405380791,
41.3391824445055,41.4187540642474,41.4982662932161,41.5777216269065,41.657142802964,
41.736539464541,41.7589104060102,41.840140502636,41.9214193936874,42.0056346137509,
42.0870654671712,42.1726728705562,42.2582802739413,42.3435235722402,42.4286886463948,
42.5137030142724,42.5986103230683,42.6833248253405,42.7576501418723,42.8341931448579,
42.910730689201,42.9872773819693,43.0638799222574,43.1405136675733,43.2172310554195,
43.2570200098034,43.3365671098839,43.4160539412511,43.4954927688313,43.5748958200785,
43.654275293886,43.7336560161045,43.8130394198191,43.892436587921,43.9718586109174,
44.0513520442956,44.1308838736832,44.2105046016622,44.2557597456656,44.3334155038604,
44.4109850695909,44.488482376222,44.5659110146563,44.643299860783,44.7206627549609,
44.7551296135967,44.8386682155131,44.9223372298337,45.0062151375915,45.0768851922591),
 .UNSPECIFIED.);
#3286=B_SPLINE_CURVE_WITH_KNOTS('',3,(#187708,#187709,#187710,#187711,#187712,
#187713,#187714,#187715,#187716,#187717,#187718,#187719,#187720,#187721,
#187722,#187723,#187724,#187725,#187726,#187727,#187728,#187729,#187730,
#187731,#187732,#187733,#187734,#187735,#187736,#187737,#187738,#187739,
#187740,#187741,#187742,#187743,#187744,#187745,#187746,#187747,#187748,
#187749,#187750,#187751,#187752,#187753,#187754,#187755,#187756,#187757,
#187758,#187759,#187760,#187761,#187762,#187763,#187764,#187765,#187766,
#187767,#187768,#187769,#187770,#187771,#187772,#187773,#187774,#187775,
#187776,#187777,#187778,#187779,#187780,#187781,#187782,#187783,#187784,
#187785,#187786,#187787,#187788,#187789),.UNSPECIFIED.,.F.,.F.,(4,3,3,3,
3,3,3,3,3,3,3,3,3,3,3,3,3,3,3,3,3,3,3,3,3,3,3,4),(38.7941774417346,38.8714431711455,
38.9487342341965,39.027065942236,39.1044888483819,39.1832749573683,39.2620610663547,
39.3381125140738,39.4140691049675,39.4899476258966,39.5657647835933,39.6415372233501,
39.7189451707085,39.7946932190448,39.8704492810428,39.9462283676192,40.0248714762686,
40.1007843891105,40.1767547690997,40.2528322627735,40.2608008022169,40.3424778464143,
40.4240390918976,40.5054902891725,40.5892938410464,40.6705052510868,40.7556048738775,
40.8407044966682),.UNSPECIFIED.);
#3287=B_SPLINE_CURVE_WITH_KNOTS('',3,(#187791,#187792,#187793,#187794,#187795,
#187796,#187797,#187798,#187799,#187800,#187801,#187802,#187803,#187804,
#187805,#187806,#187807,#187808,#187809,#187810,#187811,#187812,#187813,
#187814,#187815,#187816,#187817,#187818,#187819,#187820,#187821,#187822,
#187823,#187824,#187825,#187826,#187827,#187828,#187829,#187830,#187831,
#187832,#187833,#187834,#187835,#187836,#187837,#187838,#187839,#187840,
#187841,#187842,#187843,#187844,#187845,#187846,#187847,#187848,#187849,
#187850,#187851,#187852,#187853,#187854,#187855,#187856,#187857,#187858,
#187859,#187860,#187861,#187862,#187863,#187864,#187865,#187866,#187867,
#187868,#187869,#187870,#187871,#187872),.UNSPECIFIED.,.F.,.F.,(4,3,3,3,
3,3,3,3,3,3,3,3,3,3,3,3,3,3,3,3,3,3,3,3,3,3,3,4),(38.7947201030774,38.8796814331916,
38.9645296960449,39.0491959488369,39.0803755840292,39.1569185870159,39.2334561313597,
39.3100028241287,39.3866053644178,39.4632391097346,39.5399564975818,39.5797454519603,
39.6592925520407,39.7387793834081,39.8182182109875,39.897621262235,39.9770007360423,
40.0563814582608,40.1357648619751,40.2151620300772,40.2945840530733,40.3740774864513,
40.4536093158385,40.5332300438175,40.5784851878225,40.6649478372961,40.752826166982,
40.840704496668),.UNSPECIFIED.);
#3288=B_SPLINE_CURVE_WITH_KNOTS('',3,(#187873,#187874,#187875,#187876,#187877,
#187878,#187879,#187880,#187881,#187882,#187883,#187884,#187885,#187886,
#187887,#187888,#187889,#187890,#187891,#187892,#187893,#187894,#187895,
#187896,#187897,#187898,#187899,#187900,#187901,#187902,#187903,#187904,
#187905,#187906,#187907,#187908,#187909,#187910,#187911,#187912,#187913,
#187914,#187915,#187916,#187917,#187918,#187919,#187920,#187921,#187922,
#187923,#187924,#187925,#187926,#187927,#187928,#187929,#187930,#187931,
#187932,#187933,#187934,#187935,#187936,#187937,#187938,#187939,#187940,
#187941,#187942,#187943,#187944,#187945,#187946,#187947,#187948,#187949,
#187950,#187951,#187952,#187953,#187954,#187955,#187956,#187957,#187958,
#187959,#187960,#187961,#187962,#187963,#187964,#187965,#187966,#187967,
#187968,#187969,#187970,#187971,#187972,#187973,#187974,#187975,#187976,
#187977,#187978,#187979,#187980,#187981,#187982,#187983,#187984,#187985,
#187986,#187987,#187988,#187989,#187990,#187991,#187992,#187993,#187994,
#187995,#187996,#187997,#187998,#187999,#188000,#188001,#188002,#188003,
#188004,#188005,#188006,#188007,#188008,#188009,#188010,#188011,#188012,
#188013,#188014,#188015,#188016,#188017,#188018,#188019,#188020,#188021,
#188022,#188023,#188024,#188025,#188026,#188027,#188028,#188029),
 .UNSPECIFIED.,.F.,.F.,(4,3,3,3,3,3,3,3,3,3,3,3,3,3,3,3,3,3,3,3,3,3,3,3,
3,3,3,3,3,3,3,3,3,3,3,3,3,3,3,3,3,3,3,3,3,3,3,3,3,3,3,3,4),(40.840704496668,
40.9231667027535,41.0056285605417,41.0880900768827,41.1705512586267,41.2530121126234,
41.3354726457222,41.4179328647724,41.5003927766228,41.5828523881221,41.6653117061188,
41.7477707374609,41.8302294889962,41.9126879675725,41.9951461800371,42.0776041332372,
42.1600618340199,42.2425192892318,42.3249765057192,42.4109890935085,42.4943137879295,
42.5767803934878,42.6592461548385,42.7417110993968,42.8241752545748,42.906638647782,
42.9891013064255,43.0715632579094,43.1540245296357,43.2364851490039,43.3189451434111,
43.4014045402525,43.4838633669209,43.5663216508072,43.6487794193006,43.7312366997883,
43.8153706132377,43.8978366115361,43.9803009880848,44.0627638525268,44.1452253144836,
44.2276854835575,44.3101444693322,44.3926023813751,44.4781994980755,44.5606642350192,
44.6431260073173,44.7255852534083,44.808042411587,44.8905049304858,44.9729626017693,
45.0554213926776,45.0773793149784),.UNSPECIFIED.);
#3289=B_SPLINE_CURVE_WITH_KNOTS('',3,(#188035,#188036,#188037,#188038,#188039,
#188040,#188041,#188042,#188043,#188044,#188045,#188046,#188047,#188048,
#188049,#188050,#188051,#188052,#188053,#188054,#188055,#188056,#188057,
#188058,#188059,#188060,#188061,#188062,#188063,#188064,#188065,#188066,
#188067,#188068,#188069,#188070,#188071,#188072,#188073,#188074,#188075,
#188076,#188077,#188078,#188079,#188080,#188081,#188082,#188083,#188084,
#188085,#188086,#188087,#188088,#188089,#188090,#188091,#188092,#188093,
#188094,#188095,#188096,#188097,#188098,#188099,#188100,#188101,#188102,
#188103,#188104,#188105,#188106,#188107,#188108,#188109,#188110,#188111,
#188112,#188113,#188114,#188115,#188116,#188117,#188118,#188119,#188120,
#188121,#188122,#188123,#188124,#188125,#188126,#188127,#188128,#188129,
#188130,#188131,#188132,#188133,#188134,#188135,#188136,#188137,#188138,
#188139,#188140,#188141,#188142,#188143,#188144,#188145,#188146,#188147,
#188148,#188149,#188150,#188151,#188152,#188153,#188154,#188155,#188156,
#188157,#188158,#188159,#188160,#188161,#188162,#188163,#188164,#188165,
#188166,#188167,#188168,#188169,#188170,#188171,#188172,#188173,#188174,
#188175,#188176,#188177,#188178,#188179,#188180,#188181,#188182,#188183,
#188184,#188185,#188186,#188187,#188188,#188189,#188190,#188191,#188192,
#188193,#188194,#188195,#188196,#188197,#188198,#188199,#188200),
 .UNSPECIFIED.,.F.,.F.,(4,3,3,3,3,3,3,3,3,3,3,3,3,3,3,3,3,3,3,3,3,3,3,3,
3,3,3,3,3,3,3,3,3,3,3,3,3,3,3,3,3,3,3,3,3,3,3,3,3,3,3,3,3,3,3,4),(47.1238898038478,
47.2519789532522,47.3305148933068,47.4089580229256,47.4873228504744,47.5656238288619,
47.6438753653124,47.7220949228536,47.8002978444074,47.8784971289024,47.9567057707139,
48.0349694175751,48.1132615232523,48.191637336404,48.2507186891144,48.3303605955408,
48.4099322152827,48.4894444442513,48.5688997779416,48.6483209539991,48.7277176155761,
48.7500885570454,48.8313186536713,48.9125975447225,48.996812764786,49.0782436182063,
49.1638510215914,49.2494584249765,49.3347017232755,49.4198667974303,49.5048811653079,
49.5897884741038,49.674502976376,49.7488282929076,49.8253712958932,49.9019088402362,
49.9784555330044,50.0550580732925,50.1316918186085,50.2084092064547,50.2481981608387,
50.3277452609192,50.4072320922864,50.4866709198666,50.566073971114,50.6454534449221,
50.7248341671407,50.8042175708552,50.8836147389574,50.9630367619537,51.0425301953319,
51.1220620247194,51.2016827526985,51.2469378967009,51.3245982517907,51.3612654433028),
 .UNSPECIFIED.);
#3290=B_SPLINE_CURVE_WITH_KNOTS('',3,(#188201,#188202,#188203,#188204,#188205,
#188206,#188207,#188208,#188209,#188210,#188211,#188212,#188213,#188214,
#188215,#188216,#188217,#188218,#188219,#188220,#188221,#188222,#188223,
#188224,#188225,#188226,#188227,#188228,#188229,#188230,#188231,#188232,
#188233,#188234,#188235,#188236,#188237,#188238,#188239,#188240,#188241,
#188242,#188243,#188244,#188245,#188246,#188247,#188248,#188249,#188250,
#188251,#188252,#188253,#188254,#188255,#188256,#188257,#188258,#188259,
#188260,#188261,#188262,#188263,#188264,#188265,#188266,#188267,#188268,
#188269,#188270,#188271,#188272,#188273,#188274,#188275,#188276,#188277,
#188278,#188279,#188280,#188281,#188282,#188283,#188284,#188285),
 .UNSPECIFIED.,.F.,.F.,(4,3,3,3,3,3,3,3,3,3,3,3,3,3,3,3,3,3,3,3,3,3,3,3,
3,3,3,3,4),(45.0768851922591,45.1609818802953,45.2452240064905,45.2544994815278,
45.3319968281964,45.409412146549,45.4867610662168,45.5640591691881,45.6413220005125,
45.7185780136331,45.7958331671945,45.8731015085371,45.9503970897929,46.0277806977766,
46.1052099060459,46.1827592471565,46.25323921739,46.328304170038,46.4032756128253,
46.4781708251655,46.553006967628,46.6278037590125,46.7025804818811,46.7773525137875,
46.8521352282683,46.9269801359669,47.0018586874943,47.0768308934441,47.1238898037031),
 .UNSPECIFIED.);
#3291=B_SPLINE_CURVE_WITH_KNOTS('',3,(#188287,#188288,#188289,#188290,#188291,
#188292,#188293,#188294,#188295,#188296,#188297,#188298,#188299,#188300,
#188301,#188302,#188303,#188304,#188305,#188306,#188307,#188308,#188309,
#188310,#188311,#188312,#188313,#188314,#188315,#188316,#188317,#188318,
#188319,#188320,#188321,#188322,#188323,#188324,#188325,#188326,#188327,
#188328,#188329,#188330,#188331,#188332,#188333,#188334,#188335,#188336,
#188337,#188338,#188339,#188340,#188341,#188342,#188343,#188344,#188345,
#188346,#188347,#188348,#188349,#188350,#188351,#188352,#188353,#188354,
#188355,#188356,#188357,#188358,#188359,#188360,#188361,#188362),
 .UNSPECIFIED.,.F.,.F.,(4,3,3,3,3,3,3,3,3,3,3,3,3,3,3,3,3,3,3,3,3,3,3,3,
3,4),(45.0773793149784,45.1598409187369,45.242301856616,45.3247621560141,
45.4072218443272,45.4896809489494,45.5721394972725,45.6545975166866,45.7370550345797,
45.8237322076589,45.9061989932676,45.9886641063988,46.0711276567057,46.1535897538197,
46.2360505073517,46.3185100268937,46.4009684220207,46.4834258022916,46.5658921881108,
46.648355389735,46.7308158456834,46.8132739943198,46.8957395983315,46.9781994769089,
47.0606635886454,47.1238898038476),.UNSPECIFIED.);
#3292=B_SPLINE_CURVE_WITH_KNOTS('',3,(#188363,#188364,#188365,#188366,#188367,
#188368,#188369,#188370,#188371,#188372,#188373,#188374,#188375,#188376,
#188377,#188378,#188379,#188380,#188381,#188382,#188383,#188384,#188385,
#188386,#188387,#188388,#188389,#188390,#188391,#188392,#188393,#188394,
#188395,#188396,#188397,#188398,#188399,#188400,#188401,#188402,#188403,
#188404,#188405,#188406,#188407,#188408,#188409,#188410,#188411,#188412,
#188413,#188414,#188415,#188416,#188417,#188418,#188419,#188420,#188421,
#188422,#188423,#188424,#188425,#188426,#188427,#188428,#188429,#188430,
#188431,#188432,#188433,#188434,#188435,#188436,#188437,#188438,#188439,
#188440,#188441,#188442,#188443,#188444,#188445,#188446,#188447,#188448,
#188449,#188450,#188451,#188452,#188453,#188454,#188455,#188456,#188457,
#188458,#188459,#188460,#188461,#188462,#188463,#188464,#188465,#188466,
#188467,#188468,#188469,#188470,#188471,#188472,#188473,#188474,#188475,
#188476,#188477,#188478,#188479,#188480,#188481,#188482,#188483,#188484,
#188485,#188486,#188487,#188488,#188489,#188490,#188491,#188492,#188493,
#188494,#188495,#188496,#188497,#188498,#188499,#188500,#188501,#188502,
#188503,#188504,#188505,#188506,#188507,#188508,#188509,#188510,#188511,
#188512,#188513,#188514,#188515,#188516,#188517,#188518,#188519,#188520,
#188521,#188522,#188523,#188524,#188525,#188526,#188527,#188528,#188529,
#188530,#188531),.UNSPECIFIED.,.F.,.F.,(4,3,3,3,3,3,3,3,3,3,3,3,3,3,3,3,
3,3,3,3,3,3,3,3,3,3,3,3,3,3,3,3,3,3,3,3,3,3,3,3,3,3,3,3,3,3,3,3,3,3,3,3,
3,3,3,3,4),(47.1238898038476,47.2096860330639,47.2996803595124,47.3859918106304,
47.4724364228933,47.5590287646913,47.5696633388578,47.6473190970526,47.724888662783,
47.8023859694146,47.8798146078488,47.9572034539753,48.0345663481531,48.0690332067889,
48.1525280138346,48.2361796908249,48.3200700860656,48.4040745314492,48.4882654896721,
48.56840307472,48.6459004213886,48.7233157397411,48.8006646594089,48.8779627623801,
48.9552255937045,49.0324816068252,49.1097367603867,49.1870051017294,49.264300682985,
49.3416842909687,49.4191134992377,49.4966628403483,49.5671428105821,49.6431942583012,
49.7191508491948,49.7950293701242,49.8708465278211,49.9466189675774,50.0240269149358,
50.0997749632719,50.17553102527,50.2513101118463,50.3299532204958,50.4058661333378,
50.4818365133272,50.5579140070008,50.5658825464443,50.644430733797,50.7228840545284,
50.8025633954618,50.8808565526102,50.9591043756868,51.0373198985842,51.118069619437,
51.1962715095341,51.2782951457648,51.3603187819955),.UNSPECIFIED.);
#3293=B_SPLINE_CURVE_WITH_KNOTS('',3,(#188537,#188538,#188539,#188540,#188541,
#188542,#188543,#188544,#188545,#188546,#188547,#188548,#188549,#188550,
#188551,#188552,#188553,#188554,#188555,#188556,#188557,#188558,#188559,
#188560,#188561,#188562,#188563,#188564,#188565,#188566,#188567,#188568,
#188569,#188570,#188571,#188572,#188573,#188574,#188575,#188576,#188577,
#188578,#188579,#188580,#188581,#188582,#188583,#188584,#188585,#188586,
#188587,#188588,#188589,#188590,#188591,#188592,#188593,#188594,#188595,
#188596,#188597,#188598,#188599,#188600,#188601,#188602,#188603,#188604,
#188605,#188606,#188607,#188608,#188609,#188610,#188611,#188612,#188613,
#188614,#188615,#188616,#188617,#188618,#188619,#188620,#188621,#188622,
#188623,#188624,#188625,#188626,#188627,#188628,#188629,#188630,#188631,
#188632,#188633,#188634,#188635,#188636,#188637,#188638,#188639,#188640,
#188641,#188642,#188643,#188644,#188645,#188646,#188647,#188648,#188649,
#188650,#188651,#188652,#188653,#188654,#188655,#188656,#188657,#188658,
#188659,#188660,#188661,#188662,#188663,#188664,#188665,#188666,#188667,
#188668,#188669,#188670,#188671,#188672,#188673,#188674,#188675,#188676,
#188677,#188678,#188679,#188680,#188681,#188682,#188683,#188684,#188685,
#188686,#188687,#188688,#188689,#188690,#188691,#188692,#188693,#188694,
#188695,#188696,#188697,#188698,#188699,#188700,#188701,#188702,#188703,
#188704,#188705),.UNSPECIFIED.,.F.,.F.,(4,3,3,3,3,3,3,3,3,3,3,3,3,3,3,3,
3,3,3,3,3,3,3,3,3,3,3,3,3,3,3,3,3,3,3,3,3,3,3,3,3,3,3,3,3,3,3,3,3,3,3,3,
3,3,3,3,4),(53.407075111169,53.4818186122275,53.5564918818662,53.6311121197668,
53.7076177428319,53.7821957165587,53.856775421336,53.9313722927244,54.0093184956152,
54.0840378541353,54.1588108193862,54.2336875061842,54.2431571042874,54.3216930443421,
54.4001361739608,54.4785010015096,54.5568019798971,54.6350535163474,54.7132730738886,
54.7914759954425,54.8696752799374,54.947883921749,55.0261475686102,55.1044396742875,
55.1828154874391,55.2418968401496,55.321538746576,55.401110366318,55.4806225952867,
55.5600779289768,55.6394991050345,55.7188957666113,55.7412667080807,55.8224968047066,
55.9037756957573,55.9879909158209,56.0694217692412,56.1550291726265,56.2406365760118,
56.3258798743107,56.4110449484651,56.4960593163427,56.5809666251388,56.665681127411,
56.7400064439429,56.8165494469285,56.8930869912719,56.9696336840399,57.0462362243281,
57.1228699696442,57.1995873574904,57.239376311874,57.3189296601009,57.4001097541118,
57.4795461996596,57.5615981179021,57.6436500361446),.UNSPECIFIED.);
#3294=B_SPLINE_CURVE_WITH_KNOTS('',3,(#188706,#188707,#188708,#188709,#188710,
#188711,#188712,#188713,#188714,#188715,#188716,#188717,#188718,#188719,
#188720,#188721,#188722,#188723,#188724,#188725,#188726,#188727,#188728,
#188729,#188730,#188731,#188732,#188733,#188734,#188735,#188736,#188737,
#188738,#188739,#188740,#188741,#188742,#188743,#188744,#188745,#188746,
#188747,#188748,#188749,#188750,#188751,#188752,#188753,#188754,#188755,
#188756,#188757,#188758,#188759,#188760,#188761,#188762,#188763,#188764,
#188765,#188766,#188767,#188768,#188769,#188770,#188771,#188772,#188773,
#188774,#188775,#188776,#188777,#188778,#188779,#188780,#188781,#188782,
#188783,#188784),.UNSPECIFIED.,.F.,.F.,(4,3,3,3,3,3,3,3,3,3,3,3,3,3,3,3,
3,3,3,3,3,3,3,3,3,3,4),(51.3612654433028,51.4387991235156,51.5162537536312,
51.5936620423316,51.6710398777053,51.746307764632,51.8298025716777,51.9134542486678,
51.9973446439085,52.0813490892922,52.1655400475151,52.2456776325631,52.3231749792317,
52.4005902975842,52.477939217252,52.555237320223,52.6325001515477,52.7097561646683,
52.7870113182299,52.8642796595726,52.9415752408281,53.0189588488118,53.0963880570809,
53.1739373981914,53.2444173684253,53.3640063522608,53.4070751110274),
 .UNSPECIFIED.);
#3295=B_SPLINE_CURVE_WITH_KNOTS('',3,(#188786,#188787,#188788,#188789,#188790,
#188791,#188792,#188793,#188794,#188795,#188796,#188797,#188798,#188799,
#188800,#188801,#188802,#188803,#188804,#188805,#188806,#188807,#188808,
#188809,#188810,#188811,#188812,#188813,#188814,#188815,#188816,#188817,
#188818,#188819,#188820,#188821,#188822,#188823,#188824,#188825,#188826,
#188827,#188828,#188829,#188830,#188831,#188832,#188833,#188834,#188835,
#188836,#188837,#188838,#188839,#188840,#188841,#188842,#188843,#188844,
#188845,#188846,#188847,#188848,#188849,#188850,#188851,#188852,#188853,
#188854,#188855,#188856,#188857,#188858,#188859,#188860,#188861,#188862,
#188863,#188864,#188865,#188866,#188867),.UNSPECIFIED.,.F.,.F.,(4,3,3,3,
3,3,3,3,3,3,3,3,3,3,3,3,3,3,3,3,3,3,3,3,3,3,3,4),(51.3603187819955,51.4386160327591,
51.5169947417649,51.5646222823065,51.6442641887329,51.723835808475,51.8033480374435,
51.8828033711338,51.9622245471915,52.0416212087684,52.0639921502376,52.1452222468635,
52.2265011379145,52.310716357978,52.3921472113984,52.4777546147836,52.5633620181687,
52.6486053164676,52.7337703906224,52.8187847585,52.9036920672959,52.9884065695682,
53.0627318860998,53.1365034122465,53.2102786527495,53.2840539656421,53.3578729667789,
53.4064687028836),.UNSPECIFIED.);
#3296=B_SPLINE_CURVE_WITH_KNOTS('',3,(#188868,#188869,#188870,#188871,#188872,
#188873,#188874,#188875,#188876,#188877,#188878,#188879,#188880,#188881,
#188882,#188883,#188884,#188885,#188886,#188887,#188888,#188889,#188890,
#188891,#188892,#188893,#188894,#188895,#188896,#188897,#188898,#188899,
#188900,#188901,#188902,#188903,#188904,#188905,#188906,#188907,#188908,
#188909,#188910,#188911,#188912,#188913,#188914,#188915,#188916,#188917,
#188918,#188919,#188920,#188921,#188922,#188923,#188924,#188925,#188926,
#188927,#188928,#188929,#188930,#188931,#188932,#188933,#188934,#188935,
#188936,#188937,#188938,#188939,#188940,#188941,#188942,#188943,#188944,
#188945,#188946,#188947,#188948,#188949,#188950,#188951,#188952,#188953,
#188954,#188955,#188956,#188957,#188958,#188959,#188960,#188961,#188962,
#188963,#188964,#188965,#188966,#188967,#188968,#188969,#188970,#188971,
#188972,#188973,#188974,#188975,#188976,#188977,#188978,#188979,#188980,
#188981,#188982,#188983,#188984,#188985,#188986,#188987,#188988,#188989,
#188990,#188991,#188992,#188993,#188994,#188995,#188996,#188997,#188998,
#188999,#189000,#189001,#189002,#189003,#189004,#189005,#189006,#189007,
#189008,#189009,#189010,#189011,#189012,#189013,#189014,#189015,#189016,
#189017,#189018,#189019,#189020,#189021,#189022,#189023,#189024),
 .UNSPECIFIED.,.F.,.F.,(4,3,3,3,3,3,3,3,3,3,3,3,3,3,3,3,3,3,3,3,3,3,3,3,
3,3,3,3,3,3,3,3,3,3,3,3,3,3,3,3,3,3,3,3,3,3,3,3,3,3,3,3,4),(53.4070751110272,
53.4895373171128,53.5719991749009,53.6544606912419,53.7369218729858,53.8193827269824,
53.9018432600811,53.9843034791314,54.0667633909818,54.1492230024812,54.2316823204779,
54.3141413518198,54.3966001033552,54.4790585819315,54.5615167943962,54.6439747475963,
54.7264324483789,54.8088899035909,54.8913471200785,54.9773597078678,55.0606844022887,
55.1431510078471,55.2256167691978,55.308081713756,55.3905458689339,55.4730092621412,
55.5554719207847,55.6379338722686,55.7203951439949,55.8028557633631,55.8853157577703,
55.9677751546117,56.0502339812801,56.1326922651665,56.2151500336598,56.2976073141475,
56.3817412275969,56.4642072258953,56.546671602444,56.629134466886,56.7115959288428,
56.7940560979166,56.8765150836914,56.9589729957343,57.0445701124347,57.1270348493784,
57.2094966216766,57.2919558677675,57.3744130259463,57.4568755448451,57.5393332161285,
57.6217920070367,57.6437499293376),.UNSPECIFIED.);
#3297=B_SPLINE_CURVE_WITH_KNOTS('',3,(#189030,#189031,#189032,#189033,#189034,
#189035,#189036,#189037,#189038,#189039,#189040,#189041,#189042,#189043,
#189044,#189045,#189046,#189047,#189048,#189049,#189050,#189051,#189052,
#189053,#189054,#189055,#189056,#189057,#189058,#189059,#189060,#189061,
#189062,#189063,#189064,#189065,#189066,#189067,#189068,#189069,#189070,
#189071,#189072,#189073,#189074,#189075,#189076,#189077,#189078,#189079,
#189080,#189081,#189082,#189083,#189084,#189085,#189086,#189087,#189088,
#189089,#189090,#189091,#189092,#189093,#189094,#189095,#189096,#189097,
#189098,#189099,#189100,#189101,#189102,#189103,#189104,#189105,#189106,
#189107,#189108,#189109,#189110,#189111,#189112,#189113,#189114,#189115,
#189116,#189117,#189118,#189119,#189120,#189121,#189122,#189123,#189124,
#189125,#189126,#189127,#189128,#189129,#189130,#189131,#189132,#189133,
#189134,#189135,#189136,#189137,#189138,#189139,#189140,#189141,#189142,
#189143,#189144,#189145,#189146,#189147,#189148,#189149,#189150,#189151,
#189152,#189153,#189154,#189155,#189156,#189157,#189158,#189159,#189160,
#189161,#189162,#189163,#189164,#189165,#189166,#189167,#189168,#189169,
#189170,#189171,#189172,#189173,#189174,#189175,#189176,#189177,#189178,
#189179,#189180,#189181,#189182,#189183,#189184,#189185,#189186,#189187,
#189188,#189189,#189190,#189191,#189192,#189193,#189194,#189195,#189196,
#189197,#189198),.UNSPECIFIED.,.F.,.F.,(4,3,3,3,3,3,3,3,3,3,3,3,3,3,3,3,
3,3,3,3,3,3,3,3,3,3,3,3,3,3,3,3,3,3,3,3,3,3,3,3,3,3,3,3,3,3,3,3,3,3,3,3,
3,3,3,3,4),(59.690260418207,59.7714338090463,59.8527099136974,59.9340935351152,
60.015661963685,60.0973276863695,60.1791662424323,60.2355955194606,60.3116469671796,
60.3876035580731,60.4634820790026,60.5392992366994,60.6150716764559,60.6924796238143,
60.7682276721505,60.8439837341485,60.9197628207247,60.9984059293742,61.0743188422161,
61.1502892222055,61.2263667158793,61.2343352553227,61.3128711953773,61.391314324996,
61.4696791525447,61.5479801309325,61.6262316673828,61.704451224924,61.7826541464778,
61.8608534309728,61.9390620727846,62.0173257196457,62.0956178253228,62.1739936384745,
62.2330749911849,62.3127168976113,62.3922885173533,62.4718007463221,62.5512560800124,
62.63067725607,62.7100739176467,62.732444859116,62.8136749557419,62.8949538467934,
62.9791690668568,63.0605999202773,63.1462073236622,63.2318147270471,63.3170580253461,
63.4022230995004,63.4872374673781,63.5721447761732,63.6568592784457,63.7311845949782,
63.8077235797901,63.8842647097723,63.926723068348),.UNSPECIFIED.);
#3298=B_SPLINE_CURVE_WITH_KNOTS('',3,(#189199,#189200,#189201,#189202,#189203,
#189204,#189205,#189206,#189207,#189208,#189209,#189210,#189211,#189212,
#189213,#189214,#189215,#189216,#189217,#189218,#189219,#189220,#189221,
#189222,#189223,#189224,#189225,#189226,#189227,#189228,#189229,#189230,
#189231,#189232,#189233,#189234,#189235,#189236,#189237,#189238,#189239,
#189240,#189241,#189242,#189243,#189244,#189245,#189246,#189247,#189248,
#189249,#189250,#189251,#189252,#189253,#189254,#189255,#189256,#189257,
#189258,#189259,#189260,#189261,#189262,#189263,#189264,#189265,#189266,
#189267,#189268,#189269,#189270,#189271,#189272,#189273,#189274,#189275,
#189276,#189277,#189278,#189279,#189280),.UNSPECIFIED.,.F.,.F.,(4,3,3,3,
3,3,3,3,3,3,3,3,3,3,3,3,3,3,3,3,3,3,3,3,3,3,3,4),(57.6436500361446,57.7230305488865,
57.8024147228682,57.8818136413679,57.9612383959083,58.040734811436,58.120270524691,
58.199893569992,58.2381160477362,58.3157718059308,58.3933413716611,58.4708386782927,
58.5482673167271,58.6256561628535,58.7030190570312,58.7374859156673,58.8209807227125,
58.9046323997037,58.9885227949444,59.0725272403283,59.1567181985513,59.2368557835984,
59.3178587346514,59.3987378950705,59.4794550555494,59.5600762076632,59.6405734332376,
59.6902604181083),.UNSPECIFIED.);
#3299=B_SPLINE_CURVE_WITH_KNOTS('',3,(#189282,#189283,#189284,#189285,#189286,
#189287,#189288,#189289,#189290,#189291,#189292,#189293,#189294,#189295,
#189296,#189297,#189298,#189299,#189300,#189301,#189302,#189303,#189304,
#189305,#189306,#189307,#189308,#189309,#189310,#189311,#189312,#189313,
#189314,#189315,#189316,#189317,#189318,#189319,#189320,#189321,#189322,
#189323,#189324,#189325,#189326,#189327,#189328,#189329,#189330,#189331,
#189332,#189333,#189334,#189335,#189336,#189337,#189338,#189339,#189340,
#189341,#189342,#189343,#189344,#189345,#189346,#189347,#189348,#189349,
#189350,#189351,#189352,#189353,#189354,#189355,#189356,#189357),
 .UNSPECIFIED.,.F.,.F.,(4,3,3,3,3,3,3,3,3,3,3,3,3,3,3,3,3,3,3,3,3,3,3,3,
3,4),(57.6437499293376,57.7262115330961,57.8086724709752,57.8911327703733,
57.9735924586864,58.0560515633085,58.1385101116317,58.2209681310457,58.3034256489388,
58.3901028220181,58.4725696076267,58.5550347207579,58.6374982710648,58.7199603681788,
58.8024211217109,58.8848806412531,58.96733903638,59.0497964166511,59.1322628024703,
59.2147260040945,59.2971864600429,59.3796446086792,59.4621102126909,59.5445700912683,
59.6270342030048,59.6902604182068),.UNSPECIFIED.);
#3300=B_SPLINE_CURVE_WITH_KNOTS('',3,(#189358,#189359,#189360,#189361,#189362,
#189363,#189364,#189365,#189366,#189367,#189368,#189369,#189370,#189371,
#189372,#189373,#189374,#189375,#189376,#189377,#189378,#189379,#189380,
#189381,#189382,#189383,#189384,#189385,#189386,#189387,#189388,#189389,
#189390,#189391,#189392,#189393,#189394,#189395,#189396,#189397,#189398,
#189399,#189400,#189401,#189402,#189403,#189404,#189405,#189406,#189407,
#189408,#189409,#189410,#189411,#189412,#189413,#189414,#189415,#189416,
#189417,#189418,#189419,#189420,#189421,#189422,#189423,#189424,#189425,
#189426,#189427,#189428,#189429,#189430,#189431,#189432,#189433,#189434,
#189435,#189436,#189437,#189438,#189439,#189440,#189441,#189442,#189443,
#189444,#189445,#189446,#189447,#189448,#189449,#189450,#189451,#189452,
#189453,#189454,#189455,#189456,#189457,#189458,#189459,#189460,#189461,
#189462,#189463,#189464,#189465,#189466,#189467,#189468,#189469,#189470,
#189471,#189472,#189473,#189474,#189475,#189476,#189477,#189478,#189479,
#189480,#189481,#189482,#189483,#189484,#189485,#189486,#189487,#189488,
#189489,#189490,#189491,#189492,#189493,#189494,#189495,#189496,#189497,
#189498,#189499,#189500,#189501,#189502,#189503,#189504,#189505,#189506,
#189507,#189508,#189509,#189510,#189511,#189512,#189513,#189514,#189515,
#189516,#189517,#189518,#189519,#189520,#189521,#189522,#189523,#189524,
#189525,#189526),.UNSPECIFIED.,.F.,.F.,(4,3,3,3,3,3,3,3,3,3,3,3,3,3,3,3,
3,3,3,3,3,3,3,3,3,3,3,3,3,3,3,3,3,3,3,3,3,3,3,3,3,3,3,3,3,3,3,3,3,3,3,3,
3,3,3,3,4),(59.6906622995972,59.7735023348937,59.8562048725928,59.9388187775212,
60.0213101921048,60.0539100371351,60.1304530401207,60.2069905844637,60.2835372772316,
60.3601398175197,60.4367735628356,60.5134909506818,60.5532799050662,60.6328270051466,
60.7123138365137,60.7917526640939,60.8711557153416,60.9505351891497,61.0299159113684,
61.1092993150829,61.1886964831849,61.2681185061813,61.3476119395595,61.427143768947,
61.5067644969261,61.5520196409283,61.6296753991229,61.7072449648534,61.7847422714853,
61.8621709099195,61.9395597560468,62.0169226502247,62.0513895088594,62.1348843159051,
62.2185359928955,62.3024263881361,62.3864308335196,62.4706217917426,62.5507593767905,
62.628256723459,62.7056720418116,62.7830209614793,62.8603190644503,62.9375818957749,
63.0148379088958,63.0920930624573,63.1693614037999,63.246656985055,63.3240405930387,
63.401469801308,63.4790191424186,63.5494991126527,63.625565547796,63.7015113736145,
63.7773881367892,63.8532008171584,63.9274178287548),.UNSPECIFIED.);
#3301=B_SPLINE_CURVE_WITH_KNOTS('',3,(#189532,#189533,#189534,#189535,#189536,
#189537,#189538,#189539,#189540,#189541,#189542,#189543,#189544,#189545,
#189546,#189547,#189548,#189549,#189550,#189551,#189552,#189553,#189554,
#189555,#189556,#189557,#189558,#189559,#189560,#189561,#189562,#189563,
#189564,#189565,#189566,#189567,#189568,#189569,#189570,#189571,#189572,
#189573,#189574,#189575,#189576,#189577,#189578,#189579,#189580,#189581,
#189582,#189583,#189584,#189585,#189586,#189587,#189588,#189589,#189590,
#189591,#189592,#189593,#189594,#189595,#189596,#189597,#189598,#189599,
#189600,#189601,#189602,#189603,#189604,#189605,#189606,#189607,#189608,
#189609,#189610,#189611,#189612,#189613,#189614,#189615,#189616,#189617,
#189618,#189619,#189620,#189621,#189622,#189623,#189624,#189625,#189626,
#189627,#189628,#189629,#189630,#189631,#189632,#189633,#189634,#189635,
#189636,#189637,#189638,#189639,#189640,#189641,#189642,#189643,#189644,
#189645,#189646,#189647,#189648,#189649,#189650,#189651,#189652,#189653,
#189654,#189655,#189656,#189657,#189658,#189659,#189660,#189661,#189662,
#189663,#189664,#189665,#189666,#189667,#189668,#189669,#189670,#189671,
#189672,#189673,#189674,#189675,#189676,#189677,#189678,#189679,#189680,
#189681,#189682,#189683,#189684,#189685,#189686,#189687,#189688,#189689,
#189690,#189691,#189692,#189693,#189694,#189695,#189696,#189697,#189698,
#189699,#189700),.UNSPECIFIED.,.F.,.F.,(4,3,3,3,3,3,3,3,3,3,3,3,3,3,3,3,
3,3,3,3,3,3,3,3,3,3,3,3,3,3,3,3,3,3,3,3,3,3,3,3,3,3,3,3,3,3,3,3,3,3,3,3,
3,3,3,3,4),(65.9734457253866,66.0711042468504,66.1699732343143,66.2280339346336,
66.3055312813023,66.3829465996547,66.4602955193225,66.5375936222937,66.6148564536183,
66.692112466739,66.7693676203005,66.8466359616432,66.9239315428988,67.0013151508825,
67.0787443591515,67.1562937002621,67.2267736704958,67.3028251182149,67.3787817091085,
67.4546602300379,67.5304773877348,67.6062498274911,67.6836577748495,67.7594058231856,
67.8351618851837,67.91094097176,67.9895840804095,68.0654969932515,68.141467373241,
68.2175448669146,68.225513406358,68.3040493464127,68.3824924760314,68.4608573035802,
68.5391582819678,68.6174098184182,68.6956293759595,68.7738322975133,68.8520315820083,
68.9302402238199,69.008503870681,69.0867959763583,69.1651717895099,69.2242531422202,
69.3038950486466,69.3834666683886,69.4629788973572,69.5424342310475,69.6218554071051,
69.701252068682,69.7236230101513,69.8048514931,69.8861287412328,69.9675063542346,
70.0489314636608,70.1304618817983,70.2100096701984),.UNSPECIFIED.);
#3302=B_SPLINE_CURVE_WITH_KNOTS('',3,(#189701,#189702,#189703,#189704,#189705,
#189706,#189707,#189708,#189709,#189710,#189711,#189712,#189713,#189714,
#189715,#189716,#189717,#189718,#189719,#189720,#189721,#189722,#189723,
#189724,#189725,#189726,#189727,#189728,#189729,#189730,#189731,#189732,
#189733,#189734,#189735,#189736,#189737,#189738,#189739,#189740,#189741,
#189742,#189743,#189744,#189745,#189746,#189747,#189748,#189749,#189750,
#189751,#189752,#189753,#189754,#189755,#189756,#189757,#189758,#189759,
#189760,#189761,#189762,#189763,#189764,#189765,#189766,#189767,#189768,
#189769,#189770,#189771,#189772,#189773,#189774,#189775,#189776,#189777,
#189778,#189779,#189780,#189781,#189782,#189783,#189784,#189785),
 .UNSPECIFIED.,.F.,.F.,(4,3,3,3,3,3,3,3,3,3,3,3,3,3,3,3,3,3,3,3,3,3,3,3,
3,3,3,3,4),(63.926723068348,64.0033159369046,64.0799341730901,64.1566430225131,
64.2305544629093,64.3101015629897,64.3895883943566,64.4690272219369,64.5484302731841,
64.6278097469924,64.7071904692108,64.7865738729253,64.8659710410277,64.9453930640241,
65.0248864974022,65.1044183267901,65.1840390547689,65.2292941987715,65.3069499569662,
65.3845195226964,65.4620168293273,65.5394454677618,65.6168343138883,65.6941972080664,
65.7286640667025,65.8058153750841,65.8830026586947,65.9602676708148,65.9734457253088),
 .UNSPECIFIED.);
#3303=B_SPLINE_CURVE_WITH_KNOTS('',3,(#189787,#189788,#189789,#189790,#189791,
#189792,#189793,#189794,#189795,#189796,#189797,#189798,#189799,#189800,
#189801,#189802,#189803,#189804,#189805,#189806,#189807,#189808,#189809,
#189810,#189811,#189812,#189813,#189814,#189815,#189816,#189817,#189818,
#189819,#189820,#189821,#189822,#189823,#189824,#189825,#189826,#189827,
#189828,#189829,#189830,#189831,#189832,#189833,#189834,#189835,#189836,
#189837,#189838,#189839,#189840,#189841,#189842,#189843,#189844,#189845,
#189846,#189847,#189848,#189849,#189850,#189851,#189852,#189853,#189854,
#189855,#189856,#189857,#189858,#189859,#189860,#189861,#189862,#189863,
#189864,#189865,#189866,#189867,#189868,#189869,#189870,#189871),
 .UNSPECIFIED.,.F.,.F.,(4,3,3,3,3,3,3,3,3,3,3,3,3,3,3,3,3,3,3,3,3,3,3,3,
3,3,3,3,4),(63.9274178287548,64.0050204562248,64.0807684977985,64.1565242830619,
64.2323028227389,64.3112868291829,64.3871990601391,64.4631685755102,64.5392454837294,
64.5482388485149,64.6267747885695,64.7052179181885,64.7835827457373,64.861883724125,
64.9401352605756,65.018354818117,65.0965577396707,65.1747570241658,65.252965665978,
65.3312293128392,65.4095214185164,65.4878972316681,65.5469785843771,65.6279655672961,
65.7088722640397,65.789683790522,65.8704366165766,65.9511241904645,65.9734457252612),
 .UNSPECIFIED.);
#3304=B_SPLINE_CURVE_WITH_KNOTS('',3,(#189872,#189873,#189874,#189875,#189876,
#189877,#189878,#189879,#189880,#189881,#189882,#189883,#189884,#189885,
#189886,#189887,#189888,#189889,#189890,#189891,#189892,#189893,#189894,
#189895,#189896,#189897,#189898,#189899,#189900,#189901,#189902,#189903,
#189904,#189905,#189906,#189907,#189908,#189909,#189910,#189911,#189912,
#189913,#189914,#189915,#189916,#189917,#189918,#189919,#189920,#189921,
#189922,#189923,#189924,#189925,#189926,#189927,#189928,#189929,#189930,
#189931,#189932,#189933,#189934,#189935,#189936,#189937,#189938,#189939,
#189940,#189941,#189942,#189943,#189944,#189945,#189946,#189947,#189948,
#189949,#189950,#189951,#189952,#189953,#189954,#189955,#189956,#189957,
#189958,#189959,#189960,#189961,#189962,#189963,#189964,#189965,#189966,
#189967,#189968,#189969,#189970,#189971,#189972,#189973,#189974,#189975,
#189976,#189977,#189978,#189979,#189980,#189981,#189982,#189983,#189984,
#189985,#189986,#189987,#189988,#189989,#189990,#189991,#189992,#189993,
#189994,#189995,#189996,#189997,#189998,#189999,#190000,#190001,#190002,
#190003,#190004,#190005,#190006,#190007,#190008,#190009,#190010,#190011,
#190012,#190013,#190014,#190015,#190016,#190017,#190018,#190019,#190020,
#190021,#190022,#190023,#190024,#190025,#190026,#190027,#190028,#190029,
#190030,#190031,#190032,#190033,#190034,#190035,#190036,#190037),
 .UNSPECIFIED.,.F.,.F.,(4,3,3,3,3,3,3,3,3,3,3,3,3,3,3,3,3,3,3,3,3,3,3,3,
3,3,3,3,3,3,3,3,3,3,3,3,3,3,3,3,3,3,3,3,3,3,3,3,3,3,3,3,3,3,3,4),(65.9734457253864,
66.0463484523082,66.1275785489341,66.2088574399853,66.2930726600488,66.3745035134692,
66.4601109168542,66.5457183202393,66.6309616185382,66.7161266926928,66.8011410605704,
66.8860483693661,66.9707628716383,67.0450881881704,67.121631191156,67.1981687354991,
67.2747154282674,67.3513179685556,67.4279517138715,67.5046691017177,67.5444580561014,
67.6240051561819,67.7034919875491,67.7829308151293,67.8623338663768,67.9417133401849,
68.0210940624036,68.100477466118,68.1798746342201,68.2592966572163,68.3387900905945,
68.4183219199819,68.497942647961,68.5431977919636,68.6208535501583,68.6984231158888,
68.7759204225202,68.8533490609544,68.930737907081,69.0081008012588,69.0425676598947,
69.1260624669404,69.2097141439304,69.2936045391711,69.3776089845548,69.4617999427777,
69.5419375278258,69.6194523907518,69.696859920406,69.7742050948759,69.8515020304642,
69.9287648132369,70.0060176813371,70.083263625084,70.1605369550174,70.2098018511721),
 .UNSPECIFIED.);
#3305=B_SPLINE_CURVE_WITH_KNOTS('',3,(#190043,#190044,#190045,#190046,#190047,
#190048,#190049,#190050,#190051,#190052,#190053,#190054,#190055,#190056,
#190057,#190058,#190059,#190060,#190061,#190062,#190063,#190064,#190065,
#190066,#190067,#190068,#190069,#190070,#190071,#190072,#190073,#190074,
#190075,#190076,#190077,#190078,#190079,#190080,#190081,#190082,#190083,
#190084,#190085,#190086,#190087,#190088,#190089,#190090,#190091,#190092,
#190093,#190094,#190095,#190096,#190097,#190098,#190099,#190100,#190101,
#190102,#190103,#190104,#190105,#190106,#190107,#190108,#190109,#190110,
#190111,#190112,#190113,#190114,#190115,#190116,#190117,#190118,#190119,
#190120,#190121,#190122,#190123,#190124,#190125,#190126,#190127,#190128,
#190129,#190130,#190131,#190132,#190133,#190134,#190135,#190136,#190137,
#190138,#190139,#190140,#190141,#190142,#190143,#190144,#190145,#190146,
#190147,#190148,#190149,#190150,#190151,#190152,#190153,#190154,#190155,
#190156,#190157,#190158,#190159,#190160,#190161,#190162,#190163,#190164,
#190165,#190166,#190167,#190168,#190169,#190170,#190171,#190172,#190173,
#190174,#190175,#190176,#190177,#190178,#190179,#190180,#190181,#190182,
#190183,#190184,#190185,#190186,#190187,#190188,#190189,#190190,#190191,
#190192,#190193,#190194,#190195,#190196,#190197,#190198,#190199,#190200,
#190201,#190202,#190203,#190204,#190205,#190206,#190207,#190208,#190209,
#190210,#190211),.UNSPECIFIED.,.F.,.F.,(4,3,3,3,3,3,3,3,3,3,3,3,3,3,3,3,
3,3,3,3,3,3,3,3,3,3,3,3,3,3,3,3,3,3,3,3,3,3,3,3,3,3,3,3,3,3,3,3,3,3,3,3,
3,3,3,3,4),(72.256631032664,72.3331585331301,72.4096077409919,72.4871663601784,
72.5634973406898,72.6416697792138,72.7198422177378,72.8033370247836,72.8869887017734,
72.9708790970142,73.0548835423979,73.1390745006208,73.2192120856689,73.2967094323376,
73.3741247506899,73.4514736703576,73.5287717733287,73.6060346046528,73.6832906177735,
73.7605457713351,73.8378141126778,73.915109693933,73.9924933019167,74.0699225101859,
74.1474718512964,74.2179518215311,74.2940032692501,74.3699598601438,74.4458383810733,
74.52165553877,74.5974279785262,74.6748359258846,74.7505839742207,74.8263400362187,
74.902119122795,74.9807622314445,75.0566751442866,75.1326455242761,75.2087230179496,
75.2166915573933,75.295227497448,75.3736706270668,75.4520354546155,75.530336433003,
75.6085879694537,75.686807526995,75.7650104485489,75.8432097330439,75.9214183748554,
75.9996820217166,76.0779741273936,76.1563499405453,76.2154312932555,76.2950688021106,
76.3746420616796,76.4541474077323,76.4935350358379),.UNSPECIFIED.);
#3306=B_SPLINE_CURVE_WITH_KNOTS('',3,(#190212,#190213,#190214,#190215,#190216,
#190217,#190218,#190219,#190220,#190221,#190222,#190223,#190224,#190225,
#190226,#190227,#190228,#190229,#190230,#190231,#190232,#190233,#190234,
#190235,#190236,#190237,#190238,#190239,#190240,#190241,#190242,#190243,
#190244,#190245,#190246,#190247,#190248,#190249,#190250,#190251,#190252,
#190253,#190254,#190255,#190256,#190257,#190258,#190259,#190260,#190261,
#190262,#190263,#190264,#190265,#190266,#190267,#190268,#190269,#190270,
#190271,#190272,#190273,#190274,#190275,#190276,#190277,#190278,#190279,
#190280,#190281,#190282,#190283,#190284,#190285,#190286,#190287,#190288,
#190289,#190290,#190291,#190292,#190293,#190294,#190295,#190296),
 .UNSPECIFIED.,.F.,.F.,(4,3,3,3,3,3,3,3,3,3,3,3,3,3,3,3,3,3,3,3,3,3,3,3,
3,3,3,3,4),(70.2100096701984,70.2229928780824,70.3082361763814,70.3934012505361,
70.4784156184137,70.5633229272095,70.6480374294818,70.7223627460135,70.7989057489991,
70.8754432933422,70.9519899861104,71.0285925263986,71.1052262717146,71.1819436595607,
71.2217326139446,71.3012797140251,71.3807665453923,71.4602053729725,71.53960842422,
71.6189878980283,71.6983686202469,71.7777520239615,71.8571491920635,71.9365712150598,
72.0160646484379,72.0955964778254,72.1752172058044,72.2204723498067,72.2566310325662),
 .UNSPECIFIED.);
#3307=B_SPLINE_CURVE_WITH_KNOTS('',3,(#190298,#190299,#190300,#190301,#190302,
#190303,#190304,#190305,#190306,#190307,#190308,#190309,#190310,#190311,
#190312,#190313,#190314,#190315,#190316,#190317,#190318,#190319,#190320,
#190321,#190322,#190323,#190324,#190325,#190326,#190327,#190328,#190329,
#190330,#190331,#190332,#190333,#190334,#190335,#190336,#190337,#190338,
#190339,#190340,#190341,#190342,#190343,#190344,#190345,#190346,#190347,
#190348,#190349,#190350,#190351,#190352,#190353,#190354,#190355,#190356,
#190357,#190358,#190359,#190360,#190361,#190362,#190363,#190364,#190365,
#190366,#190367,#190368,#190369,#190370,#190371,#190372,#190373,#190374,
#190375,#190376,#190377,#190378,#190379,#190380,#190381,#190382),
 .UNSPECIFIED.,.F.,.F.,(4,3,3,3,3,3,3,3,3,3,3,3,3,3,3,3,3,3,3,3,3,3,3,3,
3,3,3,3,4),(70.2098018511721,70.2871221325254,70.3645333234971,70.4419981804235,
70.5195694389141,70.540677263688,70.6167287114071,70.6926853023007,70.7685638232301,
70.844380980927,70.9201534206834,70.9975613680417,71.0733094163779,71.1490654783759,
71.2248445649522,71.3034876736017,71.3794005864437,71.4553709664332,71.5314484601067,
71.5394169995502,71.6181874416752,71.6979928905366,71.7765557243939,71.8550549720682,
71.9335033793759,72.0142852926734,72.0926727142568,72.1746518734114,72.256631032566),
 .UNSPECIFIED.);
#3308=B_SPLINE_CURVE_WITH_KNOTS('',3,(#190383,#190384,#190385,#190386,#190387,
#190388,#190389,#190390,#190391,#190392,#190393,#190394,#190395,#190396,
#190397,#190398,#190399,#190400,#190401,#190402,#190403,#190404,#190405,
#190406,#190407,#190408,#190409,#190410,#190411,#190412,#190413,#190414,
#190415,#190416,#190417,#190418,#190419,#190420,#190421,#190422,#190423,
#190424,#190425,#190426,#190427,#190428,#190429,#190430,#190431,#190432,
#190433,#190434,#190435,#190436,#190437,#190438,#190439,#190440,#190441,
#190442,#190443,#190444,#190445,#190446,#190447,#190448,#190449,#190450,
#190451,#190452,#190453,#190454,#190455,#190456,#190457,#190458,#190459,
#190460,#190461,#190462,#190463,#190464,#190465,#190466,#190467,#190468,
#190469,#190470,#190471,#190472,#190473,#190474,#190475,#190476,#190477,
#190478,#190479,#190480,#190481,#190482,#190483,#190484,#190485,#190486,
#190487,#190488,#190489,#190490,#190491,#190492,#190493,#190494,#190495,
#190496,#190497,#190498,#190499,#190500,#190501,#190502,#190503,#190504,
#190505,#190506,#190507,#190508,#190509,#190510,#190511,#190512,#190513,
#190514,#190515,#190516,#190517,#190518,#190519,#190520,#190521,#190522,
#190523,#190524,#190525,#190526,#190527,#190528,#190529,#190530,#190531,
#190532,#190533,#190534,#190535,#190536,#190537,#190538,#190539,#190540,
#190541,#190542,#190543,#190544,#190545,#190546,#190547,#190548),
 .UNSPECIFIED.,.F.,.F.,(4,3,3,3,3,3,3,3,3,3,3,3,3,3,3,3,3,3,3,3,3,3,3,3,
3,3,3,3,3,3,3,3,3,3,3,3,3,3,3,3,3,3,3,3,3,3,3,3,3,3,3,3,3,3,3,4),(72.2566310326855,
72.3483969715894,72.4432768535009,72.5381567354124,72.6177986418387,72.6973702615807,
72.7768824905492,72.8563378242394,72.9357590002969,73.0151556618737,73.0375266033435,
73.1187566999694,73.2000355910207,73.2842508110841,73.3656816645046,73.4512890678896,
73.5368964712745,73.6221397695734,73.7073048437281,73.7923192116057,73.8772265204015,
73.9619410226737,74.0362663392056,74.1128093421912,74.1893468865343,74.2658935793025,
74.3424961195907,74.4191298649066,74.4958472527529,74.5356362071367,74.6151833072172,
74.6946701385845,74.7741089661647,74.8535120174121,74.9328914912201,75.0122722134388,
75.0916556171533,75.1710527852555,75.2504748082516,75.3299682416298,75.4095000710173,
75.4891207989964,75.5343759429989,75.6120317011936,75.6896012669241,75.7670985735555,
75.8445272119897,75.9219160581163,75.9992789522941,76.03374581093,76.1172286053278,
76.2008689671098,76.2847376552225,76.3687219964419,76.4528751460584,76.4932994035531),
 .UNSPECIFIED.);
#3309=B_SPLINE_CURVE_WITH_KNOTS('',3,(#190554,#190555,#190556,#190557,#190558,
#190559,#190560,#190561,#190562,#190563,#190564,#190565,#190566,#190567,
#190568,#190569,#190570,#190571,#190572,#190573,#190574,#190575,#190576,
#190577,#190578,#190579,#190580,#190581,#190582,#190583,#190584,#190585,
#190586,#190587,#190588,#190589,#190590,#190591,#190592,#190593,#190594,
#190595,#190596,#190597,#190598,#190599,#190600,#190601,#190602,#190603,
#190604,#190605,#190606,#190607,#190608,#190609,#190610,#190611,#190612,
#190613,#190614,#190615,#190616,#190617,#190618,#190619,#190620,#190621,
#190622,#190623,#190624,#190625,#190626,#190627,#190628,#190629,#190630,
#190631,#190632,#190633,#190634,#190635,#190636,#190637,#190638,#190639,
#190640,#190641,#190642,#190643,#190644,#190645,#190646,#190647,#190648,
#190649,#190650,#190651,#190652,#190653,#190654,#190655,#190656,#190657,
#190658,#190659,#190660,#190661,#190662,#190663,#190664,#190665,#190666,
#190667,#190668,#190669,#190670,#190671,#190672,#190673,#190674,#190675,
#190676,#190677,#190678,#190679,#190680,#190681,#190682,#190683,#190684,
#190685,#190686,#190687,#190688,#190689,#190690,#190691,#190692,#190693,
#190694,#190695,#190696,#190697,#190698,#190699,#190700,#190701,#190702,
#190703,#190704,#190705,#190706,#190707,#190708,#190709,#190710),
 .UNSPECIFIED.,.F.,.F.,(4,3,3,3,3,3,3,3,3,3,3,3,3,3,3,3,3,3,3,3,3,3,3,3,
3,3,3,3,3,3,3,3,3,3,3,3,3,3,3,3,3,3,3,3,3,3,3,3,3,3,3,3,4),(78.5398163397457,
78.6222785458313,78.7047404036194,78.7872019199604,78.8696631017043,78.952123955701,
79.0345844887998,79.11704470785,79.1995046197004,79.2819642311997,79.3644235491964,
79.4468825805385,79.529341332074,79.6117998106502,79.694258023115,79.7767159763152,
79.8591736770979,79.9416311323097,80.0240883487972,80.1101009365866,80.1934256310075,
80.2758922365658,80.3583579979165,80.4408229424747,80.5232870976527,80.60575049086,
80.6882131495035,80.7706751009875,80.8531363727139,80.9355969920821,81.0180569864893,
81.1005163833306,81.1829752099989,81.2654334938853,81.3478912623787,81.4303485428664,
81.5144824563158,81.5969484546142,81.6794128311629,81.7618756956048,81.8443371575617,
81.9267973266356,82.0092563124103,82.0917142244532,82.1773113411536,82.2597760780973,
82.3422378503955,82.4246970964865,82.5071542546652,82.589616773564,82.6720744448474,
82.7545332357556,82.7764911580561),.UNSPECIFIED.);
#3310=B_SPLINE_CURVE_WITH_KNOTS('',3,(#190711,#190712,#190713,#190714,#190715,
#190716,#190717,#190718,#190719,#190720,#190721,#190722,#190723,#190724,
#190725,#190726,#190727,#190728,#190729,#190730,#190731,#190732,#190733,
#190734,#190735,#190736,#190737,#190738,#190739,#190740,#190741,#190742,
#190743,#190744,#190745,#190746,#190747,#190748,#190749,#190750,#190751,
#190752,#190753,#190754,#190755,#190756,#190757,#190758,#190759,#190760,
#190761,#190762,#190763,#190764,#190765,#190766,#190767,#190768,#190769,
#190770,#190771,#190772,#190773,#190774,#190775,#190776,#190777,#190778,
#190779,#190780,#190781,#190782,#190783,#190784,#190785,#190786,#190787,
#190788,#190789),.UNSPECIFIED.,.F.,.F.,(4,3,3,3,3,3,3,3,3,3,3,3,3,3,3,3,
3,3,3,3,3,3,3,3,3,3,4),(76.4935350358379,76.5729722034727,76.6523811635924,
76.7148011611866,76.7960312578123,76.8773101488636,76.9615253689272,77.0429562223475,
77.1285636257326,77.2141710291177,77.2994143274164,77.3845794015709,77.4695937694484,
77.5545010782443,77.6392155805164,77.7135408970487,77.7900839000344,77.8666214443776,
77.9431681371463,78.0197706774343,78.09640442275,78.1731218105964,78.2129107649798,
78.3067930419023,78.4004431333198,78.4934298877469,78.5398163397457),
 .UNSPECIFIED.);
#3311=B_SPLINE_CURVE_WITH_KNOTS('',3,(#190791,#190792,#190793,#190794,#190795,
#190796,#190797,#190798,#190799,#190800,#190801,#190802,#190803,#190804,
#190805,#190806,#190807,#190808,#190809,#190810,#190811,#190812,#190813,
#190814,#190815,#190816,#190817,#190818,#190819,#190820,#190821,#190822,
#190823,#190824,#190825,#190826,#190827,#190828,#190829,#190830,#190831,
#190832,#190833,#190834,#190835,#190836,#190837,#190838,#190839,#190840,
#190841,#190842,#190843,#190844,#190845,#190846,#190847,#190848,#190849,
#190850,#190851,#190852,#190853,#190854,#190855,#190856,#190857,#190858,
#190859,#190860,#190861,#190862,#190863,#190864,#190865,#190866,#190867,
#190868,#190869,#190870,#190871,#190872,#190873,#190874,#190875,#190876,
#190877,#190878),.UNSPECIFIED.,.F.,.F.,(4,3,3,3,3,3,3,3,3,3,3,3,3,3,3,3,
3,3,3,3,3,3,3,3,3,3,3,3,3,4),(76.4932994035531,76.5331156788611,76.6106130255297,
76.6880283438822,76.76537726355,76.8426753665212,76.9199381978456,76.9971942109663,
77.0744493645278,77.1517177058706,77.2290132871261,77.3063968951098,77.3838261033788,
77.4613754444894,77.5318554147233,77.6079068624424,77.683863453336,77.7597419742654,
77.8355591319623,77.9113315717187,77.9887395190771,78.0644875674132,78.1402436294113,
78.2160227159876,78.2946658246371,78.370578737479,78.4465491174684,78.5226266111422,
78.5305951505855,78.5398163397456),.UNSPECIFIED.);
#3312=B_SPLINE_CURVE_WITH_KNOTS('',3,(#190879,#190880,#190881,#190882,#190883,
#190884,#190885,#190886,#190887,#190888,#190889,#190890,#190891,#190892,
#190893,#190894,#190895,#190896,#190897,#190898,#190899,#190900,#190901,
#190902,#190903,#190904,#190905,#190906,#190907,#190908,#190909,#190910,
#190911,#190912,#190913,#190914,#190915,#190916,#190917,#190918,#190919,
#190920,#190921,#190922,#190923,#190924,#190925,#190926,#190927,#190928,
#190929,#190930,#190931,#190932,#190933,#190934,#190935,#190936,#190937,
#190938,#190939,#190940,#190941,#190942,#190943,#190944,#190945,#190946,
#190947,#190948,#190949,#190950,#190951,#190952,#190953,#190954,#190955,
#190956,#190957,#190958,#190959,#190960,#190961,#190962,#190963,#190964,
#190965,#190966,#190967,#190968,#190969,#190970,#190971,#190972,#190973,
#190974,#190975,#190976,#190977,#190978,#190979,#190980,#190981,#190982,
#190983,#190984,#190985,#190986,#190987,#190988,#190989,#190990,#190991,
#190992,#190993,#190994,#190995,#190996,#190997,#190998,#190999,#191000,
#191001,#191002,#191003,#191004,#191005,#191006,#191007,#191008,#191009,
#191010,#191011,#191012,#191013,#191014,#191015,#191016,#191017,#191018,
#191019,#191020,#191021,#191022,#191023,#191024,#191025,#191026,#191027,
#191028,#191029,#191030,#191031,#191032,#191033,#191034,#191035,#191036,
#191037,#191038,#191039,#191040,#191041,#191042,#191043,#191044,#191045,
#191046,#191047),.UNSPECIFIED.,.F.,.F.,(4,3,3,3,3,3,3,3,3,3,3,3,3,3,3,3,
3,3,3,3,3,3,3,3,3,3,3,3,3,3,3,3,3,3,3,3,3,3,3,3,3,3,3,3,3,3,3,3,3,3,3,3,
3,3,3,3,4),(78.539816339824,78.6181976215257,78.6964854105407,78.7746944375514,
78.8528393777969,78.9309348609844,79.0089986587314,79.087046253989,79.1650908450107,
79.2431456257895,79.3212559760837,79.3993959103608,79.4776186213982,79.5293348864476,
79.608976792874,79.688548412616,79.7680606415843,79.8475159752746,79.9269371513323,
80.0063338129092,80.0287047543787,80.1099348510046,80.1912137420557,80.2754289621192,
80.3568598155396,80.4424672189247,80.5280746223098,80.6133179206088,80.6984829947637,
80.7834973626413,80.8684046714371,80.9531191737094,81.0274444902409,81.1039874932265,
81.1805250375696,81.2570717303378,81.3336742706259,81.4103080159419,81.4870254037881,
81.526814358172,81.6063614582525,81.6858482896197,81.7652871172,81.8446901684473,
81.9240696422554,82.0034503644741,82.0828337681886,82.1622309362907,82.2416529592869,
82.3211463926651,82.4006782220526,82.4802989500318,82.5255540940342,82.6032094524399,
82.680786144195,82.7582804784433,82.7771312059986),.UNSPECIFIED.);
#3313=B_SPLINE_CURVE_WITH_KNOTS('',3,(#191053,#191054,#191055,#191056,#191057,
#191058,#191059,#191060,#191061,#191062,#191063,#191064,#191065,#191066,
#191067,#191068,#191069,#191070,#191071,#191072,#191073,#191074,#191075,
#191076,#191077,#191078,#191079,#191080,#191081,#191082,#191083,#191084,
#191085,#191086,#191087,#191088,#191089,#191090,#191091,#191092,#191093,
#191094,#191095,#191096,#191097,#191098,#191099,#191100,#191101,#191102,
#191103,#191104,#191105,#191106,#191107,#191108,#191109,#191110,#191111,
#191112,#191113,#191114,#191115,#191116,#191117,#191118,#191119,#191120,
#191121,#191122,#191123,#191124,#191125,#191126,#191127,#191128,#191129,
#191130,#191131,#191132,#191133,#191134,#191135,#191136,#191137,#191138,
#191139,#191140,#191141,#191142,#191143,#191144,#191145,#191146,#191147,
#191148,#191149,#191150,#191151,#191152,#191153,#191154,#191155,#191156,
#191157,#191158,#191159,#191160,#191161,#191162,#191163,#191164,#191165,
#191166,#191167,#191168,#191169,#191170,#191171,#191172,#191173,#191174,
#191175,#191176,#191177,#191178,#191179,#191180,#191181,#191182,#191183,
#191184,#191185,#191186,#191187,#191188,#191189,#191190,#191191,#191192,
#191193,#191194,#191195,#191196,#191197,#191198,#191199,#191200,#191201,
#191202,#191203,#191204,#191205,#191206,#191207,#191208,#191209,#191210,
#191211,#191212,#191213,#191214,#191215,#191216,#191217,#191218,#191219,
#191220,#191221),.UNSPECIFIED.,.F.,.F.,(4,3,3,3,3,3,3,3,3,3,3,3,3,3,3,3,
3,3,3,3,3,3,3,3,3,3,3,3,3,3,3,3,3,3,3,3,3,3,3,3,3,3,3,3,3,3,3,3,3,3,3,3,
3,3,3,3,4),(84.8230016469253,84.9016360502303,84.9803592002422,85.0591284898765,
85.1380107058712,85.2040889160151,85.2836360160956,85.3631228474628,85.4425616750429,
85.5219647262902,85.601344200098,85.6807249223166,85.7601083260311,85.8395054941333,
85.9189275171295,85.9984209505077,86.0779527798951,86.1575735078742,86.2028286518773,
86.280484410072,86.3580539758025,86.4355512824339,86.5129799208681,86.5903687669946,
86.6677316611725,86.7021985198084,86.7856933268541,86.8693450038441,86.9532353990847,
87.0372398444685,87.1214308026914,87.2015683877395,87.2790657344081,87.3564810527606,
87.4338299724283,87.5111280753995,87.5883909067241,87.6656469198448,87.7429020734063,
87.820170414749,87.8974659960045,87.9748496039882,88.0522788122573,88.1298281533679,
88.2003081236017,88.2763679139956,88.3523311401638,88.4282145998417,88.5070125135111,
88.5827841972536,88.658531741077,88.73427015711,88.8100144490699,88.8858076076066,
88.9616299313289,89.0375258059729,89.058597909197),.UNSPECIFIED.);
#3314=B_SPLINE_CURVE_WITH_KNOTS('',3,(#191222,#191223,#191224,#191225,#191226,
#191227,#191228,#191229,#191230,#191231,#191232,#191233,#191234,#191235,
#191236,#191237,#191238,#191239,#191240,#191241,#191242,#191243,#191244,
#191245,#191246,#191247,#191248,#191249,#191250,#191251,#191252,#191253,
#191254,#191255,#191256,#191257,#191258,#191259,#191260,#191261,#191262,
#191263,#191264,#191265,#191266,#191267,#191268,#191269,#191270,#191271,
#191272,#191273,#191274,#191275,#191276,#191277,#191278,#191279,#191280,
#191281,#191282,#191283,#191284,#191285,#191286,#191287,#191288,#191289,
#191290,#191291,#191292,#191293,#191294,#191295,#191296,#191297),
 .UNSPECIFIED.,.F.,.F.,(4,3,3,3,3,3,3,3,3,3,3,3,3,3,3,3,3,3,3,3,3,3,3,3,
3,4),(82.7764911580561,82.8589527618145,82.9414136996937,83.0238739990917,
83.1063336874048,83.188792792027,83.2712513403501,83.3537093597642,83.4361668776573,
83.5228440507365,83.6053108363451,83.6877759494763,83.7702394997832,83.8527015968972,
83.9351623504291,84.0176218699713,84.1000802650985,84.1825376453695,84.2650040311887,
84.3474672328128,84.4299276887613,84.5123858373977,84.5948514414094,84.6773113199869,
84.7597754317234,84.8230016469253),.UNSPECIFIED.);
#3315=B_SPLINE_CURVE_WITH_KNOTS('',3,(#191299,#191300,#191301,#191302,#191303,
#191304,#191305,#191306,#191307,#191308,#191309,#191310,#191311,#191312,
#191313,#191314,#191315,#191316,#191317,#191318,#191319,#191320,#191321,
#191322,#191323,#191324,#191325,#191326,#191327,#191328,#191329,#191330,
#191331,#191332,#191333,#191334,#191335,#191336,#191337,#191338,#191339,
#191340,#191341,#191342,#191343,#191344,#191345,#191346,#191347,#191348,
#191349,#191350,#191351,#191352,#191353,#191354,#191355,#191356,#191357,
#191358,#191359,#191360,#191361,#191362,#191363,#191364,#191365,#191366,
#191367,#191368,#191369,#191370,#191371,#191372,#191373,#191374,#191375,
#191376,#191377,#191378,#191379,#191380),.UNSPECIFIED.,.F.,.F.,(4,3,3,3,
3,3,3,3,3,3,3,3,3,3,3,3,3,3,3,3,3,3,3,3,3,3,3,4),(82.7771312059986,82.8545490138819,
82.9319300501453,83.0092874835167,83.0249239619653,83.1084187690111,83.1920704460012,
83.2759608412419,83.3599652866256,83.4441562448485,83.5242938298964,83.601791176565,
83.6792064949175,83.7565554145853,83.8338535175563,83.9111163488808,83.9883723620015,
84.0656275155629,84.1428958569057,84.2201914381612,84.2975750461449,84.375004254414,
84.4525535955245,84.5230335657586,84.6158752198683,84.7080796541723,84.7992061973053,
84.8230016467793),.UNSPECIFIED.);
#3316=B_SPLINE_CURVE_WITH_KNOTS('',3,(#191381,#191382,#191383,#191384,#191385,
#191386,#191387,#191388,#191389,#191390,#191391,#191392,#191393,#191394,
#191395,#191396,#191397,#191398,#191399,#191400,#191401,#191402,#191403,
#191404,#191405,#191406,#191407,#191408,#191409,#191410,#191411,#191412,
#191413,#191414,#191415,#191416,#191417,#191418,#191419,#191420,#191421,
#191422,#191423,#191424,#191425,#191426,#191427,#191428,#191429,#191430,
#191431,#191432,#191433,#191434,#191435,#191436,#191437,#191438,#191439,
#191440,#191441,#191442,#191443,#191444,#191445,#191446,#191447,#191448,
#191449,#191450,#191451,#191452,#191453,#191454,#191455,#191456,#191457,
#191458,#191459,#191460,#191461,#191462,#191463,#191464,#191465,#191466,
#191467,#191468,#191469,#191470,#191471,#191472,#191473,#191474,#191475,
#191476,#191477,#191478,#191479,#191480,#191481,#191482,#191483,#191484,
#191485,#191486,#191487,#191488,#191489,#191490,#191491,#191492,#191493,
#191494,#191495,#191496,#191497,#191498,#191499,#191500,#191501,#191502,
#191503,#191504,#191505,#191506,#191507,#191508,#191509,#191510,#191511,
#191512,#191513,#191514,#191515,#191516,#191517,#191518,#191519,#191520,
#191521,#191522,#191523,#191524,#191525,#191526,#191527,#191528,#191529,
#191530,#191531,#191532,#191533,#191534,#191535,#191536,#191537,#191538,
#191539,#191540,#191541,#191542,#191543,#191544,#191545,#191546,#191547,
#191548,#191549),.UNSPECIFIED.,.F.,.F.,(4,3,3,3,3,3,3,3,3,3,3,3,3,3,3,3,
3,3,3,3,3,3,3,3,3,3,3,3,3,3,3,3,3,3,3,3,3,3,3,3,3,3,3,3,3,3,3,3,3,3,3,3,
3,3,3,3,4),(84.8230016469252,84.8981957460114,84.9761429404625,85.0513035388916,
85.126469067077,85.2016547669266,85.2768759001131,85.3521896409006,85.4275584136209,
85.5030372070134,85.5217733016207,85.6003092416753,85.6787523712939,85.7571171988428,
85.83541817723,85.9136697136805,85.9918892712217,86.0700921927756,86.1482914772705,
86.2265001190823,86.3047637659434,86.3830558716207,86.4614316847723,86.5205130374829,
86.6001549439093,86.6797265636513,86.7592387926201,86.8386941263103,86.9181153023685,
86.997511963945,87.019882905414,87.1011130020399,87.1823918930907,87.2666071131543,
87.3480379665746,87.4336453699599,87.5192527733451,87.6044960716438,87.689661145799,
87.7746755136765,87.8595828224724,87.9442973247445,88.0186226412762,88.0951656442619,
88.1717031886047,88.2482498813727,88.3248524216608,88.4014861669768,88.4782035548231,
88.5179925092073,88.59753722332,88.677023957123,88.756463877152,88.8358679414933,
88.9152488021237,88.9946280383445,89.0594462566544),.UNSPECIFIED.);
#3317=B_SPLINE_CURVE_WITH_KNOTS('',3,(#191555,#191556,#191557,#191558,#191559,
#191560,#191561,#191562,#191563,#191564,#191565,#191566,#191567,#191568,
#191569,#191570,#191571,#191572,#191573,#191574,#191575,#191576,#191577,
#191578,#191579,#191580,#191581,#191582,#191583,#191584,#191585,#191586,
#191587,#191588,#191589,#191590,#191591,#191592,#191593,#191594,#191595,
#191596,#191597,#191598,#191599,#191600,#191601,#191602,#191603,#191604,
#191605,#191606,#191607,#191608,#191609,#191610,#191611,#191612,#191613,
#191614,#191615,#191616,#191617,#191618,#191619,#191620,#191621,#191622,
#191623,#191624,#191625,#191626,#191627,#191628,#191629,#191630,#191631,
#191632,#191633,#191634,#191635,#191636,#191637,#191638,#191639,#191640,
#191641,#191642,#191643,#191644,#191645,#191646,#191647,#191648,#191649,
#191650,#191651,#191652,#191653,#191654,#191655,#191656,#191657,#191658,
#191659,#191660,#191661,#191662,#191663,#191664,#191665,#191666,#191667,
#191668,#191669,#191670,#191671,#191672,#191673,#191674,#191675,#191676,
#191677,#191678,#191679,#191680,#191681,#191682,#191683,#191684,#191685,
#191686,#191687,#191688,#191689,#191690,#191691,#191692,#191693,#191694,
#191695,#191696,#191697,#191698,#191699,#191700,#191701,#191702,#191703,
#191704,#191705,#191706,#191707,#191708,#191709,#191710,#191711,#191712,
#191713,#191714,#191715,#191716,#191717,#191718,#191719,#191720),
 .UNSPECIFIED.,.F.,.F.,(4,3,3,3,3,3,3,3,3,3,3,3,3,3,3,3,3,3,3,3,3,3,3,3,
3,3,3,3,3,3,3,3,3,3,3,3,3,3,3,3,3,3,3,3,3,3,3,3,3,3,3,3,3,3,3,4),(91.1061869541049,
91.1965273311882,91.2817706294871,91.3669357036419,91.4519500715196,91.5368573803156,
91.6215718825877,91.6958971991193,91.7724402021049,91.8489777464479,91.9255244392161,
92.0021269795043,92.0787607248203,92.1554781126665,92.1952670670504,92.2748141671309,
92.3543009984982,92.4337398260784,92.5131428773258,92.5925223511339,92.6719030733525,
92.751286477067,92.8306836451692,92.9101056681653,92.9895991015435,93.0691309309309,
93.14875165891,93.1940068029126,93.2716625611073,93.3492321268378,93.4267294334692,
93.5041580719034,93.58154691803,93.6589098122078,93.6933766708437,93.7768714778894,
93.8605231548795,93.9444135501201,94.0284179955038,94.1126089537267,94.1927465387748,
94.2702438854434,94.3476592037959,94.4250081234637,94.5023062264348,94.5795690577594,
94.65682507088,94.7340802244415,94.8113485657843,94.8886441470398,94.9660277550235,
95.0434569632925,95.1210063044031,95.191486274637,95.2676491241019,95.3438119735668),
 .UNSPECIFIED.);
#3318=B_SPLINE_CURVE_WITH_KNOTS('',3,(#191721,#191722,#191723,#191724,#191725,
#191726,#191727,#191728,#191729,#191730,#191731,#191732,#191733,#191734,
#191735,#191736,#191737,#191738,#191739,#191740,#191741,#191742,#191743,
#191744,#191745,#191746,#191747,#191748,#191749,#191750,#191751,#191752,
#191753,#191754,#191755,#191756,#191757,#191758,#191759,#191760,#191761,
#191762,#191763,#191764,#191765,#191766,#191767,#191768,#191769,#191770,
#191771,#191772,#191773,#191774,#191775,#191776,#191777,#191778,#191779,
#191780,#191781,#191782,#191783,#191784,#191785,#191786,#191787,#191788,
#191789,#191790,#191791,#191792,#191793,#191794,#191795,#191796,#191797,
#191798,#191799,#191800,#191801,#191802),.UNSPECIFIED.,.F.,.F.,(4,3,3,3,
3,3,3,3,3,3,3,3,3,3,3,3,3,3,3,3,3,3,3,3,3,3,3,4),(89.058597909197,89.1346476530498,
89.1990478594639,89.2775837995186,89.3560269291372,89.4343917566861,89.5126927350737,
89.590944271524,89.6691638290653,89.7473667506191,89.8255660351141,89.9037746769256,
89.9820383237868,90.0603304294641,90.1387062426157,90.197787595326,90.2774295017524,
90.3570011214944,90.4365133504632,90.5159686841535,90.5953898602109,90.6747865217878,
90.6971574632571,90.7769810610411,90.8592825342846,90.9392150863258,91.0227010201705,
91.1061869540151),.UNSPECIFIED.);
#3319=B_SPLINE_CURVE_WITH_KNOTS('',3,(#191804,#191805,#191806,#191807,#191808,
#191809,#191810,#191811,#191812,#191813,#191814,#191815,#191816,#191817,
#191818,#191819,#191820,#191821,#191822,#191823,#191824,#191825,#191826,
#191827,#191828,#191829,#191830,#191831,#191832,#191833,#191834,#191835,
#191836,#191837,#191838,#191839,#191840,#191841,#191842,#191843,#191844,
#191845,#191846,#191847,#191848,#191849,#191850,#191851,#191852,#191853,
#191854,#191855,#191856,#191857,#191858,#191859,#191860,#191861,#191862,
#191863,#191864,#191865,#191866,#191867,#191868,#191869,#191870,#191871,
#191872,#191873,#191874,#191875,#191876,#191877,#191878,#191879,#191880,
#191881,#191882,#191883,#191884,#191885),.UNSPECIFIED.,.F.,.F.,(4,3,3,3,
3,3,3,3,3,3,3,3,3,3,3,3,3,3,3,3,3,3,3,3,3,3,3,4),(89.0594462566544,89.1388400688914,
89.2182567002861,89.2977441991114,89.3772682231841,89.4568844740184,89.5167322450695,
89.5943880032642,89.6719575689949,89.7494548756267,89.8268835140609,89.9042723601875,
89.9816352543653,90.0161021130006,90.0995969200461,90.1832485970364,90.2671389922769,
90.35114343766,90.4353343958829,90.5154719809317,90.5929183426514,90.6702799673374,
90.7475710092086,90.8248055785584,90.9019963422042,90.9791610576861,91.0563236669859,
91.1061869541047),.UNSPECIFIED.);
#3320=B_SPLINE_CURVE_WITH_KNOTS('',3,(#191886,#191887,#191888,#191889,#191890,
#191891,#191892,#191893,#191894,#191895,#191896,#191897,#191898,#191899,
#191900,#191901,#191902,#191903,#191904,#191905,#191906,#191907,#191908,
#191909,#191910,#191911,#191912,#191913,#191914,#191915,#191916,#191917,
#191918,#191919,#191920,#191921,#191922,#191923,#191924,#191925,#191926,
#191927,#191928,#191929,#191930,#191931,#191932,#191933,#191934,#191935,
#191936,#191937,#191938,#191939,#191940,#191941,#191942,#191943,#191944,
#191945,#191946,#191947,#191948,#191949,#191950,#191951,#191952,#191953,
#191954,#191955,#191956,#191957,#191958,#191959,#191960,#191961,#191962,
#191963,#191964,#191965,#191966,#191967,#191968,#191969,#191970,#191971,
#191972,#191973,#191974,#191975,#191976,#191977,#191978,#191979,#191980,
#191981,#191982,#191983,#191984,#191985,#191986,#191987,#191988,#191989,
#191990,#191991,#191992,#191993,#191994,#191995,#191996,#191997,#191998,
#191999,#192000,#192001,#192002,#192003,#192004,#192005,#192006,#192007,
#192008,#192009,#192010,#192011,#192012,#192013,#192014,#192015,#192016,
#192017,#192018,#192019,#192020,#192021,#192022,#192023,#192024,#192025,
#192026,#192027,#192028,#192029,#192030,#192031,#192032,#192033,#192034,
#192035,#192036,#192037,#192038,#192039,#192040,#192041,#192042,#192043,
#192044,#192045,#192046,#192047,#192048,#192049,#192050,#192051,#192052,
#192053,#192054),.UNSPECIFIED.,.F.,.F.,(4,3,3,3,3,3,3,3,3,3,3,3,3,3,3,3,
3,3,3,3,3,3,3,3,3,3,3,3,3,3,3,3,3,3,3,3,3,3,3,3,3,3,3,3,3,3,3,3,3,3,3,3,
3,3,3,3,4),(91.1061869542419,91.1938025881983,91.2820948836687,91.3707154500607,
91.4597496548414,91.5142117167938,91.5902631645129,91.6662197554065,91.7420982763358,
91.8179154340327,91.893687873789,91.9710958211474,92.0468438694835,92.1225999314816,
92.1983790180579,92.2770221267074,92.3529350395494,92.4289054195389,92.5049829132124,
92.512951452656,92.5914873927107,92.6699305223293,92.7482953498781,92.8265963282656,
92.904847864716,92.9830674222573,93.0612703438111,93.139469628306,93.2176782701176,
93.2959419169788,93.3742340226561,93.4526098358077,93.5116911885182,93.5913330949446,
93.6709047146866,93.7504169436552,93.8298722773454,93.9092934534031,93.98869011498,
94.0110610564493,94.0922911530752,94.1735700441262,94.2577852641898,94.3392161176101,
94.4248235209953,94.5104309243804,94.5956742226793,94.6808392968341,94.7658536647118,
94.8507609735076,94.9354754757799,95.0098007923115,95.0863384425137,95.1628822781568,
95.2394299895684,95.3160157765372,95.3423550910411),.UNSPECIFIED.);
#3321=B_SPLINE_CURVE_WITH_KNOTS('',3,(#192060,#192061,#192062,#192063,#192064,
#192065,#192066,#192067,#192068,#192069,#192070,#192071,#192072,#192073,
#192074,#192075,#192076,#192077,#192078,#192079,#192080,#192081,#192082,
#192083,#192084,#192085,#192086,#192087,#192088,#192089,#192090,#192091,
#192092,#192093,#192094,#192095,#192096,#192097,#192098,#192099,#192100,
#192101,#192102,#192103,#192104,#192105,#192106,#192107,#192108,#192109,
#192110,#192111,#192112,#192113,#192114,#192115,#192116,#192117,#192118,
#192119,#192120,#192121,#192122,#192123,#192124,#192125,#192126,#192127,
#192128,#192129,#192130,#192131,#192132,#192133,#192134,#192135,#192136,
#192137,#192138,#192139,#192140,#192141,#192142,#192143,#192144,#192145,
#192146,#192147,#192148,#192149,#192150,#192151,#192152,#192153,#192154,
#192155,#192156,#192157,#192158,#192159,#192160,#192161,#192162,#192163,
#192164,#192165,#192166,#192167,#192168,#192169,#192170,#192171,#192172,
#192173,#192174,#192175,#192176,#192177,#192178,#192179,#192180,#192181,
#192182,#192183,#192184,#192185,#192186,#192187,#192188,#192189,#192190,
#192191,#192192,#192193,#192194,#192195,#192196,#192197,#192198,#192199,
#192200,#192201,#192202,#192203,#192204,#192205,#192206,#192207,#192208,
#192209,#192210,#192211,#192212,#192213,#192214,#192215,#192216,#192217,
#192218,#192219,#192220,#192221,#192222,#192223,#192224,#192225),
 .UNSPECIFIED.,.F.,.F.,(4,3,3,3,3,3,3,3,3,3,3,3,3,3,3,3,3,3,3,3,3,3,3,3,
3,3,3,3,3,3,3,3,3,3,3,3,3,3,3,3,3,3,3,3,3,3,3,3,3,3,3,3,3,3,3,4),(97.3893722613826,
97.4652312909182,97.5410553653612,97.6168713919726,97.6883356142924,97.7695657109184,
97.8508446019692,97.9350598220328,98.0164906754531,98.1020980788383,98.1877054822235,
98.2729487805224,98.3581138546769,98.4431282225546,98.5280355313507,98.612750033623,
98.6870753501546,98.7636183531402,98.8401558974831,98.916702590252,98.9933051305401,
99.069938875856,99.1466562637022,99.1864452180857,99.2659923181663,99.3454791495333,
99.4249179771133,99.5043210283606,99.5837005021682,99.6630812243868,99.7424646281013,
99.8218617962035,99.9012838191999,99.9807772525781,100.060309081966,100.139929809945,
100.185184953948,100.262840712143,100.340410277873,100.417907584505,100.495336222939,
100.572725069066,100.650087963244,100.684554821879,100.768049628925,100.851701305914,
100.935591701155,101.019596146539,101.103787104761,101.18392468981,101.261427571921,
101.338850375907,101.416193775241,101.49349100672,101.570755819008,101.626277039953),
 .UNSPECIFIED.);
#3322=B_SPLINE_CURVE_WITH_KNOTS('',3,(#192226,#192227,#192228,#192229,#192230,
#192231,#192232,#192233,#192234,#192235,#192236,#192237,#192238,#192239,
#192240,#192241,#192242,#192243,#192244,#192245,#192246,#192247,#192248,
#192249,#192250,#192251,#192252,#192253,#192254,#192255,#192256,#192257,
#192258,#192259,#192260,#192261,#192262,#192263,#192264,#192265,#192266,
#192267,#192268,#192269,#192270,#192271,#192272,#192273,#192274,#192275,
#192276,#192277,#192278,#192279,#192280,#192281,#192282,#192283,#192284,
#192285,#192286,#192287,#192288,#192289,#192290,#192291,#192292,#192293,
#192294,#192295,#192296,#192297,#192298,#192299,#192300,#192301,#192302,
#192303,#192304,#192305,#192306,#192307),.UNSPECIFIED.,.F.,.F.,(4,3,3,3,
3,3,3,3,3,3,3,3,3,3,3,3,3,3,3,3,3,3,3,3,3,3,3,4),(95.3438119735668,95.4196902029664,
95.4955071389005,95.5712794264404,95.6486477494477,95.7243957997551,95.8001519186736,
95.8759311171591,95.9545048404941,96.0304178924257,96.1103219514624,96.1902260104991,
96.2687619505538,96.3472050801724,96.4255699077212,96.5038708861088,96.5821224225593,
96.6603419801005,96.7385449016544,96.8167441861493,96.8949528279609,96.973216474822,
97.0515085804993,97.129884393651,97.1889657463613,97.280334839224,97.371304386611,
97.3893722612845),.UNSPECIFIED.);
#3323=B_SPLINE_CURVE_WITH_KNOTS('',3,(#192309,#192310,#192311,#192312,#192313,
#192314,#192315,#192316,#192317,#192318,#192319,#192320,#192321,#192322,
#192323,#192324,#192325,#192326,#192327,#192328,#192329,#192330,#192331,
#192332,#192333,#192334,#192335,#192336,#192337,#192338,#192339,#192340,
#192341,#192342,#192343,#192344,#192345,#192346,#192347,#192348,#192349,
#192350,#192351,#192352,#192353,#192354,#192355,#192356,#192357,#192358,
#192359,#192360,#192361,#192362,#192363,#192364,#192365,#192366,#192367,
#192368,#192369,#192370,#192371,#192372,#192373,#192374,#192375,#192376,
#192377,#192378,#192379,#192380,#192381,#192382,#192383,#192384,#192385,
#192386,#192387,#192388,#192389,#192390,#192391,#192392,#192393),
 .UNSPECIFIED.,.F.,.F.,(4,3,3,3,3,3,3,3,3,3,3,3,3,3,3,3,3,3,3,3,3,3,3,3,
3,3,3,3,4),(95.3423550910411,95.419002585791,95.4957287477094,95.5091706602426,
95.5887177603231,95.6682045916903,95.7476434192705,95.8270464705179,95.9064259443261,
95.9858066665447,96.0651900702593,96.1445872383614,96.2240092613575,96.3035026947357,
96.3830345241231,96.4626552521022,96.5079103961047,96.5855661542994,96.6631357200298,
96.7406330266612,96.8180616650954,96.895450511222,96.9728134053998,97.0072802640358,
97.0868812783776,97.1666126545292,97.2464127750382,97.3263553451898,97.3893722611653),
 .UNSPECIFIED.);
#3324=B_SPLINE_CURVE_WITH_KNOTS('',3,(#192394,#192395,#192396,#192397,#192398,
#192399,#192400,#192401,#192402,#192403,#192404,#192405,#192406,#192407,
#192408,#192409,#192410,#192411,#192412,#192413,#192414,#192415,#192416,
#192417,#192418,#192419,#192420,#192421,#192422,#192423,#192424,#192425,
#192426,#192427,#192428,#192429,#192430,#192431,#192432,#192433,#192434,
#192435,#192436,#192437,#192438,#192439,#192440,#192441,#192442,#192443,
#192444,#192445,#192446,#192447,#192448,#192449,#192450,#192451,#192452,
#192453,#192454,#192455,#192456,#192457,#192458,#192459,#192460,#192461,
#192462,#192463,#192464,#192465,#192466,#192467,#192468,#192469,#192470,
#192471,#192472,#192473,#192474,#192475,#192476,#192477,#192478,#192479,
#192480,#192481,#192482,#192483,#192484,#192485,#192486,#192487,#192488,
#192489,#192490,#192491,#192492,#192493,#192494,#192495,#192496,#192497,
#192498,#192499,#192500,#192501,#192502,#192503,#192504,#192505,#192506,
#192507,#192508,#192509,#192510,#192511,#192512,#192513,#192514,#192515,
#192516,#192517,#192518,#192519,#192520,#192521,#192522,#192523,#192524,
#192525,#192526,#192527,#192528,#192529,#192530,#192531,#192532,#192533,
#192534,#192535,#192536,#192537,#192538,#192539,#192540,#192541,#192542,
#192543,#192544,#192545,#192546,#192547,#192548,#192549,#192550,#192551,
#192552,#192553,#192554,#192555,#192556,#192557,#192558,#192559,#192560,
#192561,#192562),.UNSPECIFIED.,.F.,.F.,(4,3,3,3,3,3,3,3,3,3,3,3,3,3,3,3,
3,3,3,3,3,3,3,3,3,3,3,3,3,3,3,3,3,3,3,3,3,3,3,3,3,3,3,3,3,3,3,3,3,3,3,3,
3,3,3,3,4),(97.3893722612844,97.5066501319669,97.5841474786355,97.661562796988,
97.738911716656,97.8162098196274,97.8934726509519,97.9707286640726,98.0479838176341,
98.1252521589769,98.2025477402324,98.2799313482162,98.3573605564852,98.4349098975958,
98.5053898678291,98.5814413155481,98.6573979064417,98.733276427371,98.8090935850679,
98.8848660248241,98.9622739721825,99.0380220205186,99.1137780825166,99.1895571690929,
99.2682002777425,99.3441131905844,99.4200835705738,99.4961610642474,99.5041296036913,
99.582665543746,99.6611086733647,99.7394735009136,99.8177744793012,99.8960260157516,
99.9742455732929,100.052448494847,100.130647779342,100.208856421153,100.287120068014,
100.365412173692,100.443787986843,100.502869339553,100.582511245979,100.662082865721,
100.74159509469,100.82105042838,100.900471604438,100.979868266015,101.002239207485,
101.083469304111,101.164748195163,101.248963415226,101.330394268647,101.416001672031,
101.501609075416,101.586852402349,101.626377961936),.UNSPECIFIED.);
#3325=B_SPLINE_CURVE_WITH_KNOTS('',3,(#192568,#192569,#192570,#192571,#192572,
#192573,#192574,#192575,#192576,#192577,#192578,#192579,#192580,#192581,
#192582,#192583,#192584,#192585,#192586,#192587,#192588,#192589,#192590,
#192591,#192592,#192593,#192594,#192595,#192596,#192597,#192598,#192599,
#192600,#192601,#192602,#192603,#192604,#192605,#192606,#192607,#192608,
#192609,#192610,#192611,#192612,#192613,#192614,#192615,#192616,#192617,
#192618,#192619,#192620,#192621,#192622,#192623,#192624,#192625,#192626,
#192627,#192628,#192629,#192630,#192631,#192632,#192633,#192634,#192635,
#192636,#192637,#192638,#192639,#192640,#192641,#192642,#192643,#192644,
#192645,#192646,#192647,#192648,#192649,#192650,#192651,#192652,#192653,
#192654,#192655,#192656,#192657,#192658,#192659,#192660,#192661,#192662,
#192663,#192664,#192665,#192666,#192667,#192668,#192669,#192670,#192671,
#192672,#192673,#192674,#192675,#192676,#192677,#192678,#192679,#192680,
#192681,#192682,#192683,#192684,#192685,#192686,#192687,#192688,#192689,
#192690,#192691,#192692,#192693,#192694,#192695,#192696,#192697,#192698,
#192699,#192700,#192701,#192702,#192703,#192704,#192705,#192706,#192707,
#192708,#192709,#192710,#192711,#192712,#192713,#192714,#192715,#192716,
#192717,#192718,#192719,#192720,#192721,#192722,#192723,#192724),
 .UNSPECIFIED.,.F.,.F.,(4,3,3,3,3,3,3,3,3,3,3,3,3,3,3,3,3,3,3,3,3,3,3,3,
3,3,3,3,3,3,3,3,3,3,3,3,3,3,3,3,3,3,3,3,3,3,3,3,3,3,3,3,4),(103.672557568464,
103.75501977455,103.837481632338,103.919943148679,104.002404330423,104.084865184419,
104.167325717518,104.249785936568,104.332245848419,104.414705459918,104.497164777915,
104.579623809257,104.662082560792,104.744541039368,104.826999251833,104.909457205033,
104.991914905816,105.074372361028,105.156829577515,105.242842165305,105.326166859726,
105.408633465284,105.491099226635,105.573564171193,105.656028326371,105.738491719578,
105.820954378222,105.903416329706,105.985877601432,106.0683382208,106.150798215207,
106.233257612049,106.315716438717,106.398174722603,106.480632491097,106.563089771585,
106.647223685034,106.729689683332,106.812154059881,106.894616924323,106.97707838628,
107.059538555354,107.141997541128,107.224455453171,107.310052569872,107.392517306815,
107.474979079114,107.557438325205,107.639895483383,107.722358002282,107.804815673566,
107.887274464474,107.909232386775),.UNSPECIFIED.);
#3326=B_SPLINE_CURVE_WITH_KNOTS('',3,(#192725,#192726,#192727,#192728,#192729,
#192730,#192731,#192732,#192733,#192734,#192735,#192736,#192737,#192738,
#192739,#192740,#192741,#192742,#192743,#192744,#192745,#192746,#192747,
#192748,#192749,#192750,#192751,#192752,#192753,#192754,#192755,#192756,
#192757,#192758,#192759,#192760,#192761,#192762,#192763,#192764,#192765,
#192766,#192767,#192768,#192769,#192770,#192771,#192772,#192773,#192774,
#192775,#192776,#192777,#192778,#192779,#192780,#192781,#192782,#192783,
#192784,#192785,#192786,#192787,#192788,#192789,#192790,#192791,#192792,
#192793,#192794,#192795,#192796,#192797,#192798,#192799,#192800,#192801,
#192802,#192803,#192804,#192805,#192806,#192807,#192808,#192809),
 .UNSPECIFIED.,.F.,.F.,(4,3,3,3,3,3,3,3,3,3,3,3,3,3,3,3,3,3,3,3,3,3,3,3,
3,3,3,3,4),(101.626277039953,101.703531015496,101.780794228109,101.858080727786,
101.939226652258,102.016644139276,102.094116948687,102.171693488692,102.182664425672,
102.258715873391,102.334672464285,102.410550985214,102.486368142911,102.562140582667,
102.639548530025,102.715296578361,102.79105264036,102.866831726936,102.945474835586,
103.021387748428,103.097358128417,103.173435622091,103.181404161534,103.266548277653,
103.351528959913,103.436236242929,103.520771012648,103.605017726543,103.672557568464),
 .UNSPECIFIED.);
#3327=B_SPLINE_CURVE_WITH_KNOTS('',3,(#192811,#192812,#192813,#192814,#192815,
#192816,#192817,#192818,#192819,#192820,#192821,#192822,#192823,#192824,
#192825,#192826,#192827,#192828,#192829,#192830,#192831,#192832,#192833,
#192834,#192835,#192836,#192837,#192838,#192839,#192840,#192841,#192842,
#192843,#192844,#192845,#192846,#192847,#192848,#192849,#192850,#192851,
#192852,#192853,#192854,#192855,#192856,#192857,#192858,#192859,#192860,
#192861,#192862,#192863,#192864,#192865,#192866,#192867,#192868,#192869,
#192870,#192871,#192872,#192873,#192874,#192875,#192876,#192877,#192878,
#192879,#192880,#192881,#192882,#192883,#192884,#192885,#192886,#192887,
#192888,#192889,#192890,#192891,#192892),.UNSPECIFIED.,.F.,.F.,(4,3,3,3,
3,3,3,3,3,3,3,3,3,3,3,3,3,3,3,3,3,3,3,3,3,3,3,4),(101.626377961936,101.71150068053,
101.796466817973,101.881320416128,101.965990945276,102.000978943347,102.077521946333,
102.154059490676,102.230606183444,102.307208723732,102.383842469048,102.460559856894,
102.500348811278,102.579895911359,102.659382742726,102.738821570306,102.818224621553,
102.897604095361,102.97698481758,103.056368221294,103.135765389396,103.215187412392,
103.29468084577,103.374212675158,103.453833403137,103.49908854714,103.592986426315,
103.672557568464),.UNSPECIFIED.);
#3328=B_SPLINE_CURVE_WITH_KNOTS('',3,(#192893,#192894,#192895,#192896,#192897,
#192898,#192899,#192900,#192901,#192902,#192903,#192904,#192905,#192906,
#192907,#192908,#192909,#192910,#192911,#192912,#192913,#192914,#192915,
#192916,#192917,#192918,#192919,#192920,#192921,#192922,#192923,#192924,
#192925,#192926,#192927,#192928,#192929,#192930,#192931,#192932,#192933,
#192934,#192935,#192936,#192937,#192938,#192939,#192940,#192941,#192942,
#192943,#192944,#192945,#192946,#192947,#192948,#192949,#192950,#192951,
#192952,#192953,#192954,#192955,#192956,#192957,#192958,#192959,#192960,
#192961,#192962,#192963,#192964,#192965,#192966,#192967,#192968,#192969,
#192970,#192971,#192972,#192973,#192974,#192975,#192976,#192977,#192978,
#192979,#192980,#192981,#192982,#192983,#192984,#192985,#192986,#192987,
#192988,#192989,#192990,#192991,#192992,#192993,#192994,#192995,#192996,
#192997,#192998,#192999,#193000,#193001,#193002,#193003,#193004,#193005,
#193006,#193007,#193008,#193009,#193010,#193011,#193012,#193013,#193014,
#193015,#193016,#193017,#193018,#193019,#193020,#193021,#193022,#193023,
#193024,#193025,#193026,#193027,#193028,#193029,#193030,#193031,#193032,
#193033,#193034,#193035,#193036,#193037,#193038,#193039,#193040,#193041,
#193042,#193043,#193044,#193045,#193046,#193047,#193048,#193049,#193050,
#193051,#193052,#193053,#193054,#193055,#193056,#193057,#193058,#193059,
#193060,#193061,#193062,#193063,#193064),.UNSPECIFIED.,.F.,.F.,(4,3,3,3,
3,3,3,3,3,3,3,3,3,3,3,3,3,3,3,3,3,3,3,3,3,3,3,3,3,3,3,3,3,3,3,3,3,3,3,3,
3,3,3,3,3,3,3,3,3,3,3,3,3,3,3,3,3,4),(103.67255756858,103.746175586763,
103.819744102075,103.893283544664,103.966817544084,103.998458415071,104.081953222117,
104.165604899106,104.249495294347,104.33349973973,104.417690697953,104.497828283002,
104.575325629671,104.652740948023,104.730089867691,104.807387970662,104.884650801987,
104.961906815107,105.039161968669,105.116430310012,105.193725891267,105.271109499251,
105.34853870752,105.426088048631,105.496568018864,105.572619466583,105.648576057477,
105.724454578406,105.800271736103,105.876044175859,105.953452123218,106.029200171554,
106.104956233552,106.180735320128,106.259378428778,106.33529134162,106.41126172161,
106.487339215283,106.495307754727,106.573843694782,106.652286824401,106.73065165195,
106.808952630337,106.887204166788,106.96542372433,107.043626645884,107.121825930379,
107.20003457219,107.278298219051,107.356590324728,107.43496613788,107.494047490589,
107.573696677105,107.653274666236,107.732778556315,107.812238285843,107.891659120703,
107.909226129751),.UNSPECIFIED.);
#3329=B_SPLINE_CURVE_WITH_KNOTS('',3,(#193070,#193071,#193072,#193073,#193074,
#193075,#193076,#193077,#193078,#193079,#193080,#193081,#193082,#193083,
#193084,#193085,#193086,#193087,#193088,#193089,#193090,#193091,#193092,
#193093,#193094,#193095,#193096,#193097,#193098,#193099,#193100,#193101,
#193102,#193103,#193104,#193105,#193106,#193107,#193108,#193109,#193110,
#193111,#193112,#193113,#193114,#193115,#193116,#193117,#193118,#193119,
#193120,#193121,#193122,#193123,#193124,#193125,#193126,#193127,#193128,
#193129,#193130,#193131,#193132,#193133,#193134,#193135,#193136,#193137,
#193138,#193139,#193140,#193141,#193142,#193143,#193144,#193145,#193146,
#193147,#193148,#193149,#193150,#193151,#193152,#193153,#193154,#193155,
#193156,#193157,#193158,#193159,#193160,#193161,#193162,#193163,#193164,
#193165,#193166,#193167,#193168,#193169,#193170,#193171,#193172,#193173,
#193174,#193175,#193176,#193177,#193178,#193179,#193180,#193181,#193182,
#193183,#193184,#193185,#193186,#193187,#193188,#193189,#193190,#193191,
#193192,#193193,#193194,#193195,#193196,#193197,#193198,#193199,#193200,
#193201,#193202,#193203,#193204,#193205,#193206,#193207,#193208,#193209,
#193210,#193211,#193212,#193213,#193214,#193215,#193216,#193217,#193218,
#193219,#193220,#193221,#193222,#193223,#193224,#193225,#193226,#193227,
#193228,#193229,#193230,#193231,#193232,#193233,#193234,#193235,#193236,
#193237,#193238),.UNSPECIFIED.,.F.,.F.,(4,3,3,3,3,3,3,3,3,3,3,3,3,3,3,3,
3,3,3,3,3,3,3,3,3,3,3,3,3,3,3,3,3,3,3,3,3,3,3,3,3,3,3,3,3,3,3,3,3,3,3,3,
3,3,3,3,4),(109.955742875644,110.055365128407,110.157813204224,110.17258231257,
110.251118252625,110.329561382243,110.407926209792,110.48622718818,110.56447872463,
110.642698282171,110.720901203725,110.79910048822,110.877309130032,110.955572776893,
111.03386488257,111.112240695722,111.171322048432,111.250963954858,111.3305355746,
111.410047803569,111.489503137259,111.568924313317,111.648320974894,111.670691916363,
111.751922012989,111.83320090404,111.917416124103,111.998846977524,112.084454380909,
112.170061784294,112.255305082593,112.340470156748,112.425484524625,112.510391833421,
112.595106335693,112.669431652225,112.745974655211,112.822512199553,112.899058892321,
112.975661432609,113.052295177925,113.129012565771,113.168801520156,113.248348620237,
113.327835451604,113.407274279184,113.486677330432,113.56605680424,113.645437526458,
113.724820930173,113.804218098275,113.883640121271,113.96313355465,114.042665384037,
114.122286112016,114.167541256018,114.192890879176),.UNSPECIFIED.);
#3330=B_SPLINE_CURVE_WITH_KNOTS('',3,(#193239,#193240,#193241,#193242,#193243,
#193244,#193245,#193246,#193247,#193248,#193249,#193250,#193251,#193252,
#193253,#193254,#193255,#193256,#193257,#193258,#193259,#193260,#193261,
#193262,#193263,#193264,#193265,#193266,#193267,#193268,#193269,#193270,
#193271,#193272,#193273,#193274,#193275,#193276,#193277,#193278,#193279,
#193280,#193281,#193282,#193283,#193284,#193285,#193286,#193287,#193288,
#193289,#193290,#193291,#193292,#193293,#193294,#193295,#193296,#193297,
#193298,#193299,#193300,#193301,#193302,#193303,#193304,#193305,#193306,
#193307,#193308,#193309,#193310,#193311,#193312,#193313,#193314),
 .UNSPECIFIED.,.F.,.F.,(4,3,3,3,3,3,3,3,3,3,3,3,3,3,3,3,3,3,3,3,3,3,3,3,
3,4),(107.909232386775,107.991693990533,108.074154928412,108.15661522781,
108.239074916123,108.321534020746,108.403992569069,108.486450588483,108.568908106376,
108.655585279455,108.738052065064,108.820517178195,108.902980728502,108.985442825616,
109.067903579148,109.15036309869,109.232821493817,109.315278874088,109.397745259907,
109.480208461531,109.56266891748,109.645127066116,109.727592670128,109.810052548705,
109.892516660442,109.955742875644),.UNSPECIFIED.);
#3331=B_SPLINE_CURVE_WITH_KNOTS('',3,(#193316,#193317,#193318,#193319,#193320,
#193321,#193322,#193323,#193324,#193325,#193326,#193327,#193328,#193329,
#193330,#193331,#193332,#193333,#193334,#193335,#193336,#193337,#193338,
#193339,#193340,#193341,#193342,#193343,#193344,#193345,#193346,#193347,
#193348,#193349,#193350,#193351,#193352,#193353,#193354,#193355,#193356,
#193357,#193358,#193359,#193360,#193361,#193362,#193363,#193364,#193365,
#193366,#193367,#193368,#193369,#193370,#193371,#193372,#193373,#193374,
#193375,#193376,#193377,#193378,#193379,#193380,#193381,#193382,#193383,
#193384,#193385,#193386,#193387,#193388,#193389,#193390,#193391,#193392,
#193393,#193394,#193395,#193396,#193397),.UNSPECIFIED.,.F.,.F.,(4,3,3,3,
3,3,3,3,3,3,3,3,3,3,3,3,3,3,3,3,3,3,3,3,3,3,3,4),(107.909226129751,107.988618440932,
107.99341735852,108.074647455146,108.155926346196,108.24014156626,108.32157241968,
108.407179823066,108.492787226451,108.57803052475,108.663195598904,108.748209966782,
108.833117275578,108.91783177785,108.992157094382,109.068700097368,109.145237641711,
109.221784334479,109.298386874767,109.375020620084,109.45173800793,109.491526962313,
109.576384599114,109.661154257058,109.745770463507,109.830278775386,109.9146126653,
109.955655827855),.UNSPECIFIED.);
#3332=B_SPLINE_CURVE_WITH_KNOTS('',3,(#193398,#193399,#193400,#193401,#193402,
#193403,#193404,#193405,#193406,#193407,#193408,#193409,#193410,#193411,
#193412,#193413,#193414,#193415,#193416,#193417,#193418,#193419,#193420,
#193421,#193422,#193423,#193424,#193425,#193426,#193427,#193428,#193429,
#193430,#193431,#193432,#193433,#193434,#193435,#193436,#193437,#193438,
#193439,#193440,#193441,#193442,#193443,#193444,#193445,#193446,#193447,
#193448,#193449,#193450,#193451,#193452,#193453,#193454,#193455,#193456,
#193457,#193458,#193459,#193460,#193461,#193462,#193463,#193464,#193465,
#193466,#193467,#193468,#193469,#193470,#193471,#193472,#193473,#193474,
#193475,#193476,#193477,#193478,#193479,#193480,#193481,#193482,#193483,
#193484,#193485,#193486,#193487,#193488,#193489,#193490,#193491,#193492,
#193493,#193494,#193495,#193496,#193497,#193498,#193499,#193500,#193501,
#193502,#193503,#193504,#193505,#193506,#193507,#193508,#193509,#193510,
#193511,#193512,#193513,#193514,#193515,#193516,#193517,#193518,#193519,
#193520,#193521,#193522,#193523,#193524,#193525,#193526,#193527,#193528,
#193529,#193530,#193531,#193532,#193533,#193534,#193535,#193536,#193537,
#193538,#193539,#193540,#193541,#193542,#193543,#193544,#193545,#193546,
#193547,#193548,#193549,#193550,#193551,#193552,#193553,#193554),
 .UNSPECIFIED.,.F.,.F.,(4,3,3,3,3,3,3,3,3,3,3,3,3,3,3,3,3,3,3,3,3,3,3,3,
3,3,3,3,3,3,3,3,3,3,3,3,3,3,3,3,3,3,3,3,3,3,3,3,3,3,3,3,4),(109.95577038367,
110.038232589638,110.120694447311,110.203155963539,110.285617145173,110.368077999061,
110.450538532054,110.532998751001,110.61545866275,110.69791827415,110.78037759205,
110.862836623298,110.945295374741,111.027753853227,111.110212065604,111.192670018719,
111.275127719419,111.35758517455,111.440042390959,111.526054119178,111.609377980889,
111.691844586179,111.77431034727,111.856775291577,111.939239446512,112.021702839485,
112.104165497903,112.18662744917,112.269088720687,112.351549339856,112.434009334072,
112.51646873073,112.598927557224,112.681385840945,112.763843609281,112.846300889621,
112.930433189891,113.012899187698,113.095363563787,113.177826427801,113.260287889363,
113.342748058073,113.425207043517,113.507664955261,113.593259047597,113.675723783724,
113.758185555317,113.840644800816,113.923101958515,114.005564475944,114.088022146208,
114.170480934839,114.192417693954),.UNSPECIFIED.);
#3333=B_SPLINE_CURVE_WITH_KNOTS('',3,(#193560,#193561,#193562,#193563,#193564,
#193565,#193566,#193567,#193568,#193569,#193570,#193571,#193572,#193573,
#193574,#193575,#193576,#193577,#193578,#193579,#193580,#193581,#193582,
#193583,#193584,#193585,#193586,#193587,#193588,#193589,#193590,#193591,
#193592,#193593,#193594,#193595,#193596,#193597,#193598,#193599,#193600,
#193601,#193602,#193603,#193604,#193605,#193606,#193607,#193608,#193609,
#193610,#193611,#193612,#193613,#193614,#193615,#193616,#193617,#193618,
#193619,#193620,#193621,#193622,#193623,#193624,#193625,#193626,#193627,
#193628,#193629,#193630,#193631,#193632,#193633,#193634,#193635,#193636,
#193637,#193638,#193639,#193640,#193641,#193642,#193643,#193644,#193645,
#193646,#193647,#193648,#193649,#193650,#193651,#193652,#193653,#193654,
#193655,#193656,#193657,#193658,#193659,#193660,#193661,#193662,#193663,
#193664,#193665,#193666,#193667,#193668,#193669,#193670,#193671,#193672,
#193673,#193674,#193675,#193676,#193677,#193678,#193679,#193680,#193681,
#193682,#193683,#193684,#193685,#193686,#193687,#193688,#193689,#193690,
#193691,#193692,#193693,#193694,#193695,#193696,#193697,#193698,#193699,
#193700,#193701,#193702,#193703,#193704,#193705,#193706,#193707,#193708,
#193709,#193710,#193711,#193712,#193713,#193714,#193715,#193716,#193717,
#193718,#193719,#193720,#193721,#193722,#193723,#193724,#193725,#193726,
#193727,#193728),.UNSPECIFIED.,.F.,.F.,(4,3,3,3,3,3,3,3,3,3,3,3,3,3,3,3,
3,3,3,3,3,3,3,3,3,3,3,3,3,3,3,3,3,3,3,3,3,3,3,3,3,3,3,3,3,3,3,3,3,3,3,3,
3,3,3,3,4),(116.238928182907,116.314137825691,116.389260630726,116.464313746745,
116.539314224263,116.617370004181,116.692328870866,116.767289769362,116.842268021846,
116.917278970001,116.992379284292,117.067532383174,117.142793754632,117.163760463605,
117.24229640366,117.320739533279,117.399104360828,117.477405339215,117.555656875666,
117.633876433207,117.712079354761,117.790278639256,117.868487281067,117.946750927929,
118.025043033606,118.103418846758,118.162500199467,118.242142105893,118.321713725635,
118.401225954604,118.480681288294,118.560102464352,118.639499125928,118.661870067398,
118.743100164024,118.824379055075,118.908594275139,118.990025128559,119.075632531944,
119.161239935329,119.246483233628,119.331648307784,119.416662675662,119.501569984457,
119.58628448673,119.66060980326,119.737152806246,119.813690350589,119.890237043357,
119.966839583645,120.043473328961,120.120190716807,120.159979671192,120.239520074869,
120.319006382661,120.398442502006,120.475571182131),.UNSPECIFIED.);
#3334=B_SPLINE_CURVE_WITH_KNOTS('',3,(#193729,#193730,#193731,#193732,#193733,
#193734,#193735,#193736,#193737,#193738,#193739,#193740,#193741,#193742,
#193743,#193744,#193745,#193746,#193747,#193748,#193749,#193750,#193751,
#193752,#193753,#193754,#193755,#193756,#193757,#193758,#193759,#193760,
#193761,#193762,#193763,#193764,#193765,#193766,#193767,#193768,#193769,
#193770,#193771,#193772,#193773,#193774,#193775,#193776,#193777,#193778,
#193779,#193780,#193781,#193782,#193783,#193784,#193785,#193786,#193787,
#193788,#193789,#193790,#193791,#193792,#193793,#193794,#193795,#193796,
#193797,#193798,#193799,#193800,#193801,#193802,#193803,#193804,#193805,
#193806,#193807),.UNSPECIFIED.,.F.,.F.,(4,3,3,3,3,3,3,3,3,3,3,3,3,3,3,3,
3,3,3,3,3,3,3,3,3,3,4),(114.192890879176,114.270516977951,114.3480614362,
114.427773858137,114.505186939995,114.586049031973,114.66691112395,114.750405930996,
114.834057607986,114.917948003227,115.001952448611,115.086143406834,115.166280991881,
115.24377833855,115.321193656902,115.39854257657,115.475840679541,115.553103510865,
115.630359523986,115.707614677547,115.78488301889,115.862178600146,115.939562208129,
116.016991416398,116.094540757509,116.165020727743,116.238928182823),
 .UNSPECIFIED.);
#3335=B_SPLINE_CURVE_WITH_KNOTS('',3,(#193809,#193810,#193811,#193812,#193813,
#193814,#193815,#193816,#193817,#193818,#193819,#193820,#193821,#193822,
#193823,#193824,#193825,#193826,#193827,#193828,#193829,#193830,#193831,
#193832,#193833,#193834,#193835,#193836,#193837,#193838,#193839,#193840,
#193841,#193842,#193843,#193844,#193845,#193846,#193847,#193848,#193849,
#193850,#193851,#193852,#193853,#193854,#193855,#193856,#193857,#193858,
#193859,#193860,#193861,#193862,#193863,#193864,#193865,#193866,#193867,
#193868,#193869,#193870,#193871,#193872,#193873,#193874,#193875,#193876,
#193877,#193878,#193879,#193880,#193881,#193882,#193883,#193884),
 .UNSPECIFIED.,.F.,.F.,(4,3,3,3,3,3,3,3,3,3,3,3,3,3,3,3,3,3,3,3,3,3,3,3,
3,4),(114.192417693954,114.274879297712,114.357340235592,114.43980053499,
114.522260223303,114.604719327925,114.687177876248,114.769635895662,114.852093413555,
114.938770586626,115.021237372234,115.103702485365,115.186166035672,115.268628132786,
115.351088886318,115.43354840586,115.516006800987,115.598464181258,115.680930567077,
115.763393768702,115.84585422465,115.928312373286,116.010777977298,116.093237855875,
116.175701967612,116.238928182684),.UNSPECIFIED.);
#3336=B_SPLINE_CURVE_WITH_KNOTS('',3,(#193885,#193886,#193887,#193888,#193889,
#193890,#193891,#193892,#193893,#193894,#193895,#193896,#193897,#193898,
#193899,#193900,#193901,#193902,#193903,#193904,#193905,#193906,#193907,
#193908,#193909,#193910,#193911,#193912,#193913,#193914,#193915,#193916,
#193917,#193918,#193919,#193920,#193921,#193922,#193923,#193924,#193925,
#193926,#193927,#193928,#193929,#193930,#193931,#193932,#193933,#193934,
#193935,#193936,#193937,#193938,#193939,#193940,#193941,#193942,#193943,
#193944,#193945,#193946,#193947,#193948,#193949,#193950,#193951,#193952,
#193953,#193954,#193955,#193956,#193957,#193958,#193959,#193960,#193961,
#193962,#193963,#193964,#193965,#193966,#193967,#193968,#193969,#193970,
#193971,#193972,#193973,#193974,#193975,#193976,#193977,#193978,#193979,
#193980,#193981,#193982,#193983,#193984,#193985,#193986,#193987,#193988,
#193989,#193990,#193991,#193992,#193993,#193994,#193995,#193996,#193997,
#193998,#193999,#194000,#194001,#194002,#194003,#194004,#194005,#194006,
#194007,#194008,#194009,#194010,#194011,#194012,#194013,#194014,#194015,
#194016,#194017,#194018,#194019,#194020,#194021,#194022,#194023,#194024,
#194025,#194026,#194027,#194028,#194029,#194030,#194031,#194032,#194033,
#194034,#194035,#194036,#194037,#194038,#194039,#194040,#194041),
 .UNSPECIFIED.,.F.,.F.,(4,3,3,3,3,3,3,3,3,3,3,3,3,3,3,3,3,3,3,3,3,3,3,3,
3,3,3,3,3,3,3,3,3,3,3,3,3,3,3,3,3,3,3,3,3,3,3,3,3,3,3,3,4),(116.238928182823,
116.321390388909,116.403852246697,116.486313763038,116.568774944782,116.651235798778,
116.733696331877,116.816156550927,116.898616462778,116.981076074277,117.063535392274,
117.145994423616,117.228453175152,117.310911653728,117.393369866193,117.475827819393,
117.558285520175,117.640742975387,117.723200191875,117.809212779664,117.892537474085,
117.975004079643,118.057469840994,118.139934785552,118.22239894073,118.304862333937,
118.387324992581,118.469786944065,118.552248215791,118.634708835159,118.717168829567,
118.799628226408,118.882087053076,118.964545336963,119.047003105456,119.129460385944,
119.213594299393,119.296060297691,119.37852467424,119.460987538682,119.543449000639,
119.625909169713,119.708368155488,119.790826067531,119.876423184231,119.958887921175,
120.041349693473,120.123808939564,120.206266097742,120.288728616641,120.371186287925,
120.453645078833,120.475603001134),.UNSPECIFIED.);
#3337=B_SPLINE_CURVE_WITH_KNOTS('',3,(#194047,#194048,#194049,#194050,#194051,
#194052,#194053,#194054,#194055,#194056,#194057,#194058,#194059,#194060,
#194061,#194062,#194063,#194064,#194065,#194066,#194067,#194068,#194069,
#194070,#194071,#194072,#194073,#194074,#194075,#194076,#194077,#194078,
#194079,#194080,#194081,#194082,#194083,#194084,#194085,#194086,#194087,
#194088,#194089,#194090,#194091,#194092,#194093,#194094,#194095,#194096,
#194097,#194098,#194099,#194100,#194101,#194102,#194103,#194104,#194105,
#194106,#194107,#194108,#194109,#194110,#194111,#194112,#194113,#194114,
#194115,#194116,#194117,#194118,#194119,#194120,#194121,#194122,#194123,
#194124,#194125,#194126,#194127,#194128,#194129,#194130,#194131,#194132,
#194133,#194134,#194135,#194136,#194137,#194138,#194139,#194140,#194141,
#194142,#194143,#194144,#194145,#194146,#194147,#194148,#194149,#194150,
#194151,#194152,#194153,#194154,#194155,#194156,#194157,#194158,#194159,
#194160,#194161,#194162,#194163,#194164,#194165,#194166,#194167,#194168,
#194169,#194170,#194171,#194172,#194173,#194174,#194175,#194176,#194177,
#194178,#194179,#194180,#194181,#194182,#194183,#194184,#194185,#194186,
#194187,#194188,#194189,#194190,#194191,#194192,#194193,#194194,#194195,
#194196,#194197,#194198,#194199,#194200,#194201,#194202,#194203,#194204,
#194205,#194206,#194207,#194208,#194209,#194210,#194211,#194212,#194213,
#194214,#194215),.UNSPECIFIED.,.F.,.F.,(4,3,3,3,3,3,3,3,3,3,3,3,3,3,3,3,
3,3,3,3,3,3,3,3,3,3,3,3,3,3,3,3,3,3,3,3,3,3,3,3,3,3,3,3,3,3,3,3,3,3,3,3,
3,3,3,3,4),(122.522113490003,122.6013741636,122.680240720641,122.75914499531,
122.838098684334,122.917623732945,122.996756414602,123.07647764669,123.156198878778,
123.232250326497,123.308206917391,123.38408543832,123.459902596017,123.535675035773,
123.613082983131,123.688831031467,123.764587093465,123.840366180041,123.919009288691,
123.994922201533,124.070892581522,124.146970075196,124.15493861464,124.233474554695,
124.311917684314,124.390282511863,124.46858349025,124.5468350267,124.625054584241,
124.703257505795,124.78145679029,124.859665432102,124.937929078963,125.01622118464,
125.094596997792,125.153678350502,125.233320256929,125.312891876671,125.392404105639,
125.47185943933,125.551280615387,125.630677276964,125.653048218434,125.73427831506,
125.815557206111,125.899772426174,125.981203279595,126.06681068298,126.152418086365,
126.237661384664,126.322826458819,126.407840826696,126.492748135492,126.577462637764,
126.651787954296,126.728328092807,126.758858075524),.UNSPECIFIED.);
#3338=B_SPLINE_CURVE_WITH_KNOTS('',3,(#194216,#194217,#194218,#194219,#194220,
#194221,#194222,#194223,#194224,#194225,#194226,#194227,#194228,#194229,
#194230,#194231,#194232,#194233,#194234,#194235,#194236,#194237,#194238,
#194239,#194240,#194241,#194242,#194243,#194244,#194245,#194246,#194247,
#194248,#194249,#194250,#194251,#194252,#194253,#194254,#194255,#194256,
#194257,#194258,#194259,#194260,#194261,#194262,#194263,#194264,#194265,
#194266,#194267,#194268,#194269,#194270,#194271,#194272,#194273,#194274,
#194275,#194276,#194277,#194278,#194279,#194280,#194281,#194282,#194283,
#194284,#194285,#194286,#194287,#194288,#194289,#194290,#194291,#194292,
#194293,#194294,#194295,#194296,#194297),.UNSPECIFIED.,.F.,.F.,(4,3,3,3,
3,3,3,3,3,3,3,3,3,3,3,3,3,3,3,3,3,3,3,3,3,3,3,4),(120.475571182131,120.55495116409,
120.634331973151,120.713715144904,120.793111762126,120.872532915006,120.952025395174,
121.031555977971,121.111175974327,121.158719407054,121.236375165248,121.313944730979,
121.39144203761,121.468870676044,121.54625952217,121.623622416347,121.658089274985,
121.741584082031,121.825235759021,121.909126154262,121.993130599645,122.077321557868,
122.157459142916,122.242489520718,122.327223768168,122.411766191998,122.496020247112,
122.522113489888),.UNSPECIFIED.);
#3339=B_SPLINE_CURVE_WITH_KNOTS('',3,(#194299,#194300,#194301,#194302,#194303,
#194304,#194305,#194306,#194307,#194308,#194309,#194310,#194311,#194312,
#194313,#194314,#194315,#194316,#194317,#194318,#194319,#194320,#194321,
#194322,#194323,#194324,#194325,#194326,#194327,#194328,#194329,#194330,
#194331,#194332,#194333,#194334,#194335,#194336,#194337,#194338,#194339,
#194340,#194341,#194342,#194343,#194344,#194345,#194346,#194347,#194348,
#194349,#194350,#194351,#194352,#194353,#194354,#194355,#194356,#194357,
#194358,#194359,#194360,#194361,#194362,#194363,#194364,#194365,#194366,
#194367,#194368,#194369,#194370,#194371,#194372,#194373,#194374),
 .UNSPECIFIED.,.F.,.F.,(4,3,3,3,3,3,3,3,3,3,3,3,3,3,3,3,3,3,3,3,3,3,3,3,
3,4),(120.475603001134,120.558064604892,120.640525542771,120.722985842169,
120.805445530482,120.887904635105,120.970363183428,121.052821202842,121.135278720735,
121.221955893814,121.304422679423,121.386887792554,121.469351342861,121.551813439975,
121.634274193507,121.716733713049,121.799192108176,121.881649488447,121.964115874266,
122.04657907589,122.129039531839,122.211497680475,122.293963284487,122.376423163064,
122.458887274801,122.522113490003),.UNSPECIFIED.);
#3340=B_SPLINE_CURVE_WITH_KNOTS('',3,(#194375,#194376,#194377,#194378,#194379,
#194380,#194381,#194382,#194383,#194384,#194385,#194386,#194387,#194388,
#194389,#194390,#194391,#194392,#194393,#194394,#194395,#194396,#194397,
#194398,#194399,#194400,#194401,#194402,#194403,#194404,#194405,#194406,
#194407,#194408,#194409,#194410,#194411,#194412,#194413,#194414,#194415,
#194416,#194417,#194418,#194419,#194420,#194421,#194422,#194423,#194424,
#194425,#194426,#194427,#194428,#194429,#194430,#194431,#194432,#194433,
#194434,#194435,#194436,#194437,#194438,#194439,#194440,#194441,#194442,
#194443,#194444,#194445,#194446,#194447,#194448,#194449,#194450,#194451,
#194452,#194453,#194454,#194455,#194456,#194457,#194458,#194459,#194460,
#194461,#194462,#194463,#194464,#194465,#194466,#194467,#194468,#194469,
#194470,#194471,#194472,#194473,#194474,#194475,#194476,#194477,#194478,
#194479,#194480,#194481,#194482,#194483,#194484,#194485,#194486,#194487,
#194488,#194489,#194490,#194491,#194492,#194493,#194494,#194495,#194496,
#194497,#194498,#194499,#194500,#194501,#194502,#194503,#194504,#194505,
#194506,#194507,#194508,#194509,#194510,#194511,#194512,#194513,#194514,
#194515,#194516,#194517,#194518,#194519,#194520,#194521,#194522,#194523,
#194524,#194525,#194526,#194527,#194528,#194529,#194530,#194531,#194532,
#194533,#194534,#194535,#194536,#194537,#194538,#194539,#194540,#194541,
#194542,#194543),.UNSPECIFIED.,.F.,.F.,(4,3,3,3,3,3,3,3,3,3,3,3,3,3,3,3,
3,3,3,3,3,3,3,3,3,3,3,3,3,3,3,3,3,3,3,3,3,3,3,3,3,3,3,3,3,3,3,3,3,3,3,3,
3,3,3,3,4),(122.522220451277,122.606401533941,122.690490111526,122.774431321878,
122.858272049895,122.941960963335,122.974513396453,123.051056399439,123.127593943782,
123.204140636549,123.280743176838,123.357376922153,123.434094309999,123.473883264384,
123.553430364464,123.632917195832,123.712356023412,123.791759074659,123.871138548467,
123.950519270686,124.0299026744,124.109299842502,124.188721865498,124.268215298876,
124.347747128264,124.427367856243,124.472623000246,124.550278758441,124.627848324171,
124.705345630803,124.782774269237,124.860163115363,124.937526009541,124.971992868177,
125.055487675223,125.139139352212,125.223029747452,125.307034192836,125.391225151059,
125.471362736108,125.548860082777,125.626275401129,125.703624320797,125.780922423768,
125.858185255093,125.935441268213,126.012696421775,126.089964763117,126.167260344372,
126.244643952356,126.322073160625,126.399622501736,126.47010247197,126.546145536087,
126.622105287442,126.697977128334,126.759584805783),.UNSPECIFIED.);
#3341=B_SPLINE_CURVE_WITH_KNOTS('',3,(#194549,#194550,#194551,#194552,#194553,
#194554,#194555,#194556,#194557,#194558,#194559,#194560,#194561,#194562,
#194563,#194564,#194565,#194566,#194567,#194568,#194569,#194570,#194571,
#194572,#194573,#194574,#194575,#194576,#194577,#194578,#194579,#194580,
#194581,#194582,#194583,#194584,#194585,#194586,#194587,#194588,#194589,
#194590,#194591,#194592,#194593,#194594,#194595,#194596,#194597,#194598,
#194599,#194600,#194601,#194602,#194603,#194604,#194605,#194606,#194607,
#194608,#194609,#194610,#194611,#194612,#194613,#194614,#194615,#194616,
#194617,#194618,#194619,#194620,#194621,#194622,#194623,#194624,#194625,
#194626,#194627,#194628,#194629,#194630,#194631,#194632,#194633,#194634,
#194635,#194636,#194637,#194638,#194639,#194640,#194641,#194642,#194643,
#194644,#194645,#194646,#194647,#194648,#194649,#194650,#194651,#194652,
#194653,#194654,#194655,#194656,#194657,#194658,#194659,#194660,#194661,
#194662,#194663,#194664,#194665,#194666,#194667,#194668,#194669,#194670,
#194671,#194672,#194673,#194674,#194675,#194676,#194677,#194678,#194679,
#194680,#194681,#194682,#194683,#194684,#194685,#194686,#194687,#194688,
#194689,#194690,#194691,#194692,#194693,#194694,#194695,#194696,#194697,
#194698,#194699,#194700,#194701,#194702,#194703,#194704,#194705,#194706,
#194707,#194708,#194709,#194710,#194711,#194712,#194713,#194714,#194715,
#194716,#194717),.UNSPECIFIED.,.F.,.F.,(4,3,3,3,3,3,3,3,3,3,3,3,3,3,3,3,
3,3,3,3,3,3,3,3,3,3,3,3,3,3,3,3,3,3,3,3,3,3,3,3,3,3,3,3,3,3,3,3,3,3,3,3,
3,3,3,3,4),(128.805298797316,128.895499662665,128.986091025251,129.077130579346,
129.148637293951,129.22613464062,129.303549958972,129.38089887864,129.458196981611,
129.535459812936,129.612715826056,129.689970979618,129.767239320961,129.844534902216,
129.9219185102,129.999347718469,130.07689705958,130.147377029813,130.223428477532,
130.299385068426,130.375263589355,130.451080747052,130.526853186808,130.604261134167,
130.680009182503,130.755765244501,130.831544331078,130.910187439727,130.986100352569,
131.062070732559,131.138148226232,131.146116765676,131.224652705731,131.303095835349,
131.381460662898,131.459761641286,131.538013177737,131.616232735278,131.694435656832,
131.772634941327,131.850843583138,131.92910723,132.007399335677,132.085775148829,
132.144856501538,132.224498407964,132.304070027706,132.383582256675,132.463037590365,
132.542458766422,132.621855427999,132.644226369469,132.725444205775,132.806752399596,
132.888103408676,132.969548948727,133.041617861985),.UNSPECIFIED.);
#3342=B_SPLINE_CURVE_WITH_KNOTS('',3,(#194718,#194719,#194720,#194721,#194722,
#194723,#194724,#194725,#194726,#194727,#194728,#194729,#194730,#194731,
#194732,#194733,#194734,#194735,#194736,#194737,#194738,#194739,#194740,
#194741,#194742,#194743,#194744,#194745,#194746,#194747,#194748,#194749,
#194750,#194751,#194752,#194753,#194754,#194755,#194756,#194757,#194758,
#194759,#194760,#194761,#194762,#194763,#194764,#194765,#194766,#194767,
#194768,#194769,#194770,#194771,#194772,#194773,#194774,#194775,#194776,
#194777,#194778,#194779,#194780,#194781,#194782,#194783,#194784,#194785,
#194786,#194787,#194788,#194789,#194790,#194791,#194792,#194793,#194794,
#194795,#194796,#194797,#194798,#194799),.UNSPECIFIED.,.F.,.F.,(4,3,3,3,
3,3,3,3,3,3,3,3,3,3,3,3,3,3,3,3,3,3,3,3,3,3,3,4),(126.758858075524,126.835397517614,
126.914337593767,126.990951939283,127.071054880755,127.151157822227,127.230704922307,
127.310191753675,127.389630581255,127.469033632501,127.54841310631,127.627793828529,
127.707177232243,127.786574400345,127.865996423342,127.94548985672,128.025021686108,
128.104642414087,128.149897558089,128.227553316283,128.305122882014,128.382620188644,
128.460048827078,128.537437673205,128.614800567382,128.64926742602,128.727283111602,
128.805298797183),.UNSPECIFIED.);
#3343=B_SPLINE_CURVE_WITH_KNOTS('',3,(#194801,#194802,#194803,#194804,#194805,
#194806,#194807,#194808,#194809,#194810,#194811,#194812,#194813,#194814,
#194815,#194816,#194817,#194818,#194819,#194820,#194821,#194822,#194823,
#194824,#194825,#194826,#194827,#194828,#194829,#194830,#194831,#194832,
#194833,#194834,#194835,#194836,#194837,#194838,#194839,#194840,#194841,
#194842,#194843,#194844,#194845,#194846,#194847,#194848,#194849,#194850,
#194851,#194852,#194853,#194854,#194855,#194856,#194857,#194858,#194859,
#194860,#194861,#194862,#194863,#194864,#194865,#194866,#194867,#194868,
#194869,#194870,#194871,#194872,#194873,#194874,#194875,#194876,#194877,
#194878,#194879,#194880,#194881,#194882),.UNSPECIFIED.,.F.,.F.,(4,3,3,3,
3,3,3,3,3,3,3,3,3,3,3,3,3,3,3,3,3,3,3,3,3,3,3,4),(126.759584805783,126.835364369514,
126.914549099304,126.990297266019,127.066050982518,127.141825258102,127.217635116655,
127.293538098483,127.369495818183,127.445564880084,127.468842207832,127.547378147886,
127.625821277505,127.704186105054,127.782487083442,127.860738619892,127.938958177434,
128.017161098987,128.095360383483,128.173569025294,128.251832672155,128.330124777833,
128.408500590984,128.467581943695,128.552011157067,128.635508513281,128.720403655231,
128.805298797182),.UNSPECIFIED.);
#3344=B_SPLINE_CURVE_WITH_KNOTS('',3,(#194883,#194884,#194885,#194886,#194887,
#194888,#194889,#194890,#194891,#194892,#194893,#194894,#194895,#194896,
#194897,#194898,#194899,#194900,#194901,#194902,#194903,#194904,#194905,
#194906,#194907,#194908,#194909,#194910,#194911,#194912,#194913,#194914,
#194915,#194916,#194917,#194918,#194919,#194920,#194921,#194922,#194923,
#194924,#194925,#194926,#194927,#194928,#194929,#194930,#194931,#194932,
#194933,#194934,#194935,#194936,#194937,#194938,#194939,#194940,#194941,
#194942,#194943,#194944,#194945,#194946,#194947,#194948,#194949,#194950,
#194951,#194952,#194953,#194954,#194955,#194956,#194957,#194958,#194959,
#194960,#194961,#194962,#194963,#194964,#194965,#194966,#194967,#194968,
#194969,#194970,#194971,#194972,#194973,#194974,#194975,#194976,#194977,
#194978,#194979,#194980,#194981,#194982,#194983,#194984,#194985,#194986,
#194987,#194988,#194989,#194990,#194991,#194992,#194993,#194994,#194995,
#194996,#194997,#194998,#194999,#195000,#195001,#195002,#195003,#195004,
#195005,#195006,#195007,#195008,#195009,#195010,#195011,#195012,#195013,
#195014,#195015,#195016,#195017,#195018,#195019,#195020,#195021,#195022,
#195023,#195024,#195025,#195026,#195027,#195028,#195029,#195030,#195031,
#195032,#195033,#195034,#195035,#195036,#195037,#195038,#195039,#195040,
#195041,#195042,#195043,#195044,#195045,#195046,#195047,#195048,#195049,
#195050,#195051),.UNSPECIFIED.,.F.,.F.,(4,3,3,3,3,3,3,3,3,3,3,3,3,3,3,3,
3,3,3,3,3,3,3,3,3,3,3,3,3,3,3,3,3,3,3,3,3,3,3,3,3,3,3,3,3,3,3,3,3,3,3,3,
3,3,3,3,4),(128.805298797286,128.880674391654,128.95604640739,128.966951811626,
129.048181908252,129.129460799303,129.213676019366,129.295106872787,129.380714276172,
129.466321679557,129.551564977856,129.63673005201,129.721744419888,129.806651728683,
129.891366230955,129.965691547488,130.042234550474,130.118772094817,130.195318787584,
130.271921327873,130.348555073189,130.425272461035,130.465061415419,130.544608515499,
130.624095346867,130.703534174447,130.782937225694,130.862316699502,130.941697421721,
131.021080825435,131.100477993537,131.179900016534,131.259393449912,131.338925279299,
131.418546007278,131.463801151281,131.541456909475,131.619026475206,131.696523781837,
131.773952420271,131.851341266397,131.928704160575,131.963171019212,132.046665826258,
132.130317503248,132.214207898489,132.298212343873,132.382403302096,132.462540887143,
132.540031362984,132.617443924814,132.694792732576,132.772091906516,132.849356943872,
132.926601905208,133.003851393021,133.041832180143),.UNSPECIFIED.);
#3345=B_SPLINE_CURVE_WITH_KNOTS('',3,(#195057,#195058,#195059,#195060,#195061,
#195062,#195063,#195064,#195065,#195066,#195067,#195068,#195069,#195070,
#195071,#195072,#195073,#195074,#195075,#195076,#195077,#195078,#195079,
#195080,#195081,#195082,#195083,#195084,#195085,#195086,#195087,#195088,
#195089,#195090,#195091,#195092,#195093,#195094,#195095,#195096,#195097,
#195098,#195099,#195100,#195101,#195102,#195103,#195104,#195105,#195106,
#195107,#195108,#195109,#195110,#195111,#195112,#195113,#195114,#195115,
#195116,#195117,#195118,#195119,#195120,#195121,#195122,#195123,#195124,
#195125,#195126,#195127,#195128,#195129,#195130,#195131,#195132,#195133,
#195134,#195135,#195136,#195137,#195138,#195139,#195140,#195141,#195142,
#195143,#195144,#195145,#195146,#195147,#195148,#195149,#195150,#195151,
#195152,#195153,#195154,#195155,#195156,#195157,#195158,#195159,#195160,
#195161,#195162,#195163,#195164,#195165,#195166,#195167,#195168,#195169,
#195170,#195171,#195172,#195173,#195174,#195175,#195176,#195177,#195178,
#195179,#195180,#195181,#195182,#195183,#195184,#195185,#195186,#195187,
#195188,#195189,#195190,#195191,#195192,#195193,#195194,#195195,#195196,
#195197,#195198,#195199,#195200,#195201,#195202,#195203,#195204,#195205,
#195206,#195207,#195208,#195209,#195210,#195211,#195212,#195213,#195214,
#195215,#195216,#195217,#195218,#195219,#195220,#195221,#195222,#195223,
#195224,#195225,#195226,#195227,#195228),.UNSPECIFIED.,.F.,.F.,(4,3,3,3,
3,3,3,3,3,3,3,3,3,3,3,3,3,3,3,3,3,3,3,3,3,3,3,3,3,3,3,3,3,3,3,3,3,3,3,3,
3,3,3,3,3,3,3,3,3,3,3,3,3,3,3,3,3,4),(135.088484104362,135.141075709124,
135.218731467319,135.296301033049,135.37379833968,135.451226978114,135.528615824241,
135.605978718418,135.640445577055,135.723940384101,135.807592061091,135.891482456332,
135.975486901716,136.059677859939,136.139815444986,136.217312791655,136.294728110007,
136.372077029675,136.449375132646,136.526637963971,136.603893977092,136.681149130653,
136.758417471996,136.835713053252,136.913096661236,136.990525869505,137.068075210615,
137.138555180849,137.214606628568,137.290563219462,137.366441740391,137.442258898088,
137.518031337845,137.595439285203,137.67118733354,137.746943395538,137.822722482114,
137.901365590763,137.977278503605,138.053248883594,138.129326377268,138.137294916711,
138.215830856766,138.294273986384,138.372638813933,138.450939792321,138.529191328772,
138.607410886313,138.685613807867,138.763813092361,138.842021734173,138.920285381034,
138.998577486712,139.076953299863,139.136034652573,139.215687266484,139.295257544978,
139.325441263557),.UNSPECIFIED.);
#3346=B_SPLINE_CURVE_WITH_KNOTS('',3,(#195229,#195230,#195231,#195232,#195233,
#195234,#195235,#195236,#195237,#195238,#195239,#195240,#195241,#195242,
#195243,#195244,#195245,#195246,#195247,#195248,#195249,#195250,#195251,
#195252,#195253,#195254,#195255,#195256,#195257,#195258,#195259,#195260,
#195261,#195262,#195263,#195264,#195265,#195266,#195267,#195268,#195269,
#195270,#195271,#195272,#195273,#195274,#195275,#195276,#195277,#195278,
#195279,#195280,#195281,#195282,#195283,#195284,#195285,#195286,#195287,
#195288,#195289,#195290,#195291,#195292,#195293,#195294,#195295,#195296,
#195297,#195298,#195299,#195300,#195301,#195302,#195303,#195304,#195305,
#195306,#195307,#195308,#195309,#195310),.UNSPECIFIED.,.F.,.F.,(4,3,3,3,
3,3,3,3,3,3,3,3,3,3,3,3,3,3,3,3,3,3,3,3,3,3,3,4),(133.041617861985,133.123183016486,
133.1435962374,133.228839535699,133.314004609853,133.399018977731,133.483926286527,
133.568640788799,133.642966105331,133.719509108317,133.79604665266,133.872593345428,
133.949195885716,134.025829631032,134.102547018878,134.142335973262,134.221219674072,
134.300040126623,134.378810938376,134.457545679513,134.536412982609,134.615128988621,
134.693851432986,134.772592595606,134.851565472774,134.930412978058,135.009448541169,
135.088484104279),.UNSPECIFIED.);
#3347=B_SPLINE_CURVE_WITH_KNOTS('',3,(#195312,#195313,#195314,#195315,#195316,
#195317,#195318,#195319,#195320,#195321,#195322,#195323,#195324,#195325,
#195326,#195327,#195328,#195329,#195330,#195331,#195332,#195333,#195334,
#195335,#195336,#195337,#195338,#195339,#195340,#195341,#195342,#195343,
#195344,#195345,#195346,#195347,#195348,#195349,#195350,#195351,#195352,
#195353,#195354,#195355,#195356,#195357,#195358,#195359,#195360,#195361,
#195362,#195363,#195364,#195365,#195366,#195367,#195368,#195369,#195370,
#195371,#195372,#195373,#195374,#195375,#195376,#195377,#195378,#195379,
#195380,#195381,#195382,#195383,#195384,#195385,#195386,#195387,#195388,
#195389,#195390,#195391,#195392,#195393,#195394,#195395,#195396),
 .UNSPECIFIED.,.F.,.F.,(4,3,3,3,3,3,3,3,3,3,3,3,3,3,3,3,3,3,3,3,3,3,3,3,
3,3,3,3,4),(133.041832180143,133.119112147236,133.196426261864,133.27383067654,
133.351286907555,133.42885258256,133.461280623006,133.537332070725,133.613288661619,
133.689167182548,133.764984340245,133.840756780002,133.91816472736,133.993912775696,
134.069668837694,134.14544792427,134.22409103292,134.300003945762,134.375974325751,
134.452051819425,134.460020358868,134.54038040468,134.620637838083,134.700802381432,
134.780883694742,134.860868989518,134.940796938601,135.020664980668,135.088484104362),
 .UNSPECIFIED.);
#3348=B_SPLINE_CURVE_WITH_KNOTS('',3,(#195397,#195398,#195399,#195400,#195401,
#195402,#195403,#195404,#195405,#195406,#195407,#195408,#195409,#195410,
#195411,#195412,#195413,#195414,#195415,#195416,#195417,#195418,#195419,
#195420,#195421,#195422,#195423,#195424,#195425,#195426,#195427,#195428,
#195429,#195430,#195431,#195432,#195433,#195434,#195435,#195436,#195437,
#195438,#195439,#195440,#195441,#195442,#195443,#195444,#195445,#195446,
#195447,#195448,#195449,#195450,#195451,#195452,#195453,#195454,#195455,
#195456,#195457,#195458,#195459,#195460,#195461,#195462,#195463,#195464,
#195465,#195466,#195467,#195468,#195469,#195470,#195471,#195472,#195473,
#195474,#195475,#195476,#195477,#195478,#195479,#195480,#195481,#195482,
#195483,#195484,#195485,#195486,#195487,#195488,#195489,#195490,#195491,
#195492,#195493,#195494,#195495,#195496,#195497,#195498,#195499,#195500,
#195501,#195502,#195503,#195504,#195505,#195506,#195507,#195508,#195509,
#195510,#195511,#195512,#195513,#195514,#195515,#195516,#195517,#195518,
#195519,#195520,#195521,#195522,#195523,#195524,#195525,#195526,#195527,
#195528,#195529,#195530,#195531,#195532,#195533,#195534,#195535,#195536,
#195537,#195538,#195539,#195540,#195541,#195542,#195543,#195544,#195545,
#195546,#195547,#195548,#195549,#195550,#195551,#195552,#195553,#195554,
#195555,#195556,#195557,#195558,#195559,#195560,#195561,#195562,#195563,
#195564,#195565),.UNSPECIFIED.,.F.,.F.,(4,3,3,3,3,3,3,3,3,3,3,3,3,3,3,3,
3,3,3,3,3,3,3,3,3,3,3,3,3,3,3,3,3,3,3,3,3,3,3,3,3,3,3,3,3,3,3,3,3,3,3,3,
3,3,3,3,4),(135.088484104466,135.173794025916,135.259420181161,135.345202545235,
135.431180372423,135.45876009473,135.538402001156,135.617973620898,135.697485849867,
135.776941183557,135.856362359615,135.935759021192,135.958129962661,136.039360059287,
136.120638950338,136.204854170401,136.286285023822,136.371892427207,136.457499830592,
136.542743128891,136.627908203046,136.712922570923,136.797829879719,136.882544381991,
136.956869698523,137.033412701509,137.109950245852,137.18649693862,137.263099478908,
137.339733224224,137.41645061207,137.456239566454,137.535786666534,137.615273497902,
137.694712325482,137.774115376729,137.853494850537,137.932875572756,138.01225897647,
138.091656144572,138.171078167568,138.250571600946,138.330103430334,138.409724158313,
138.454979302316,138.532635060511,138.610204626241,138.687701932873,138.765130571307,
138.842519417434,138.919882311612,138.954349170247,139.037805216196,139.121502012315,
139.205322739821,139.289322335834,139.324800290729),.UNSPECIFIED.);
#3349=B_SPLINE_CURVE_WITH_KNOTS('',3,(#195571,#195572,#195573,#195574,#195575,
#195576,#195577,#195578,#195579,#195580,#195581,#195582,#195583,#195584,
#195585,#195586,#195587,#195588,#195589,#195590,#195591,#195592,#195593,
#195594,#195595,#195596,#195597,#195598,#195599,#195600,#195601,#195602,
#195603,#195604,#195605,#195606,#195607,#195608,#195609,#195610,#195611,
#195612,#195613,#195614,#195615,#195616,#195617,#195618,#195619,#195620,
#195621,#195622,#195623,#195624,#195625,#195626,#195627,#195628,#195629,
#195630,#195631,#195632,#195633,#195634,#195635,#195636,#195637,#195638,
#195639,#195640,#195641,#195642,#195643,#195644,#195645,#195646,#195647,
#195648,#195649,#195650,#195651,#195652,#195653,#195654,#195655,#195656,
#195657,#195658,#195659,#195660,#195661,#195662,#195663,#195664,#195665,
#195666,#195667,#195668,#195669,#195670,#195671,#195672,#195673,#195674,
#195675,#195676,#195677,#195678,#195679,#195680,#195681,#195682,#195683,
#195684,#195685,#195686,#195687,#195688,#195689,#195690,#195691,#195692,
#195693,#195694,#195695,#195696,#195697,#195698,#195699,#195700,#195701,
#195702,#195703,#195704,#195705,#195706,#195707,#195708,#195709,#195710,
#195711,#195712,#195713,#195714,#195715,#195716,#195717,#195718,#195719,
#195720,#195721,#195722,#195723,#195724,#195725,#195726,#195727),
 .UNSPECIFIED.,.F.,.F.,(4,3,3,3,3,3,3,3,3,3,3,3,3,3,3,3,3,3,3,3,3,3,3,3,
3,3,3,3,3,3,3,3,3,3,3,3,3,3,3,3,3,3,3,3,3,3,3,3,3,3,3,3,4),(141.371669411542,
141.454131617628,141.536593475416,141.619054991757,141.701516173501,141.783977027497,
141.866437560596,141.948897779646,142.031357691497,142.113817302996,142.196276620993,
142.278735652335,142.36119440387,142.443652882447,142.526111094911,142.608569048111,
142.691026748894,142.773484204106,142.855941420593,142.941954008383,143.025278702804,
143.107745308362,143.190211069713,143.272676014271,143.355140169449,143.437603562656,
143.5200662213,143.602528172784,143.68498944451,143.767450063878,143.849910058285,
143.932369455127,144.014828281795,144.097286565681,144.179744334175,144.262201614663,
144.346335528112,144.42880152641,144.511265902959,144.593728767401,144.676190229358,
144.758650398432,144.841109384206,144.923567296249,145.00916441295,145.091629149893,
145.174090922191,145.256550168282,145.339007326461,145.42146984536,145.503927516643,
145.586386307552,145.608344229852),.UNSPECIFIED.);
#3350=B_SPLINE_CURVE_WITH_KNOTS('',3,(#195728,#195729,#195730,#195731,#195732,
#195733,#195734,#195735,#195736,#195737,#195738,#195739,#195740,#195741,
#195742,#195743,#195744,#195745,#195746,#195747,#195748,#195749,#195750,
#195751,#195752,#195753,#195754,#195755,#195756,#195757,#195758,#195759,
#195760,#195761,#195762,#195763,#195764,#195765,#195766,#195767,#195768,
#195769,#195770,#195771,#195772,#195773,#195774,#195775,#195776,#195777,
#195778,#195779,#195780,#195781,#195782,#195783,#195784,#195785,#195786,
#195787,#195788,#195789,#195790,#195791,#195792,#195793,#195794,#195795,
#195796,#195797,#195798,#195799,#195800,#195801,#195802,#195803,#195804,
#195805,#195806),.UNSPECIFIED.,.F.,.F.,(4,3,3,3,3,3,3,3,3,3,3,3,3,3,3,3,
3,3,3,3,3,3,3,3,3,3,4),(139.325441263557,139.404922780061,139.484363981108,
139.563776237547,139.635404520504,139.71663461713,139.797913508182,139.882128728245,
139.963559581665,140.04916698505,140.134774388435,140.220017686734,140.305182760888,
140.390197128765,140.475104437561,140.559818939832,140.634144256366,140.710687259352,
140.787224803695,140.863771496464,140.940374036752,141.017007782067,141.093725169914,
141.133514124297,141.240036454045,141.344973964139,141.371669411542),
 .UNSPECIFIED.);
#3351=B_SPLINE_CURVE_WITH_KNOTS('',3,(#195808,#195809,#195810,#195811,#195812,
#195813,#195814,#195815,#195816,#195817,#195818,#195819,#195820,#195821,
#195822,#195823,#195824,#195825,#195826,#195827,#195828,#195829,#195830,
#195831,#195832,#195833,#195834,#195835,#195836,#195837,#195838,#195839,
#195840,#195841,#195842,#195843,#195844,#195845,#195846,#195847,#195848,
#195849,#195850,#195851,#195852,#195853,#195854,#195855,#195856,#195857,
#195858,#195859,#195860,#195861,#195862,#195863,#195864,#195865,#195866,
#195867,#195868,#195869,#195870,#195871,#195872,#195873,#195874,#195875,
#195876,#195877,#195878,#195879,#195880,#195881,#195882,#195883,#195884,
#195885,#195886,#195887,#195888,#195889,#195890,#195891,#195892),
 .UNSPECIFIED.,.F.,.F.,(4,3,3,3,3,3,3,3,3,3,3,3,3,3,3,3,3,3,3,3,3,3,3,3,
3,3,3,3,4),(139.324800290729,139.409016625214,139.453719038179,139.531216384848,
139.6086317032,139.685980622868,139.763278725839,139.840541557164,139.917797570284,
139.995052723846,140.072321065189,140.149616646444,140.227000254428,140.304429462697,
140.381978803807,140.452458774041,140.527741820882,140.60293120538,140.678044107417,
140.753097598991,140.83041907555,140.905413675403,140.980403801278,141.055404759923,
141.130431870016,141.205537522519,141.280690322145,141.355940608412,141.371669411466),
 .UNSPECIFIED.);
#3352=B_SPLINE_CURVE_WITH_KNOTS('',3,(#195893,#195894,#195895,#195896,#195897,
#195898,#195899,#195900,#195901,#195902,#195903,#195904,#195905,#195906,
#195907,#195908,#195909,#195910,#195911,#195912,#195913,#195914,#195915,
#195916,#195917,#195918,#195919,#195920,#195921,#195922,#195923,#195924,
#195925,#195926,#195927,#195928,#195929,#195930,#195931,#195932,#195933,
#195934,#195935,#195936,#195937,#195938,#195939,#195940,#195941,#195942,
#195943,#195944,#195945,#195946,#195947,#195948,#195949,#195950,#195951,
#195952,#195953,#195954,#195955,#195956,#195957,#195958,#195959,#195960,
#195961,#195962,#195963,#195964,#195965,#195966,#195967,#195968,#195969,
#195970,#195971,#195972,#195973,#195974,#195975,#195976,#195977,#195978,
#195979,#195980,#195981,#195982,#195983,#195984,#195985,#195986,#195987,
#195988,#195989,#195990,#195991,#195992,#195993,#195994,#195995,#195996,
#195997,#195998,#195999,#196000,#196001,#196002,#196003,#196004,#196005,
#196006,#196007,#196008,#196009,#196010,#196011,#196012,#196013,#196014,
#196015,#196016,#196017,#196018,#196019,#196020,#196021,#196022,#196023,
#196024,#196025,#196026,#196027,#196028,#196029,#196030,#196031,#196032,
#196033,#196034,#196035,#196036,#196037,#196038,#196039,#196040,#196041,
#196042,#196043,#196044,#196045,#196046,#196047,#196048,#196049,#196050,
#196051,#196052,#196053,#196054,#196055,#196056,#196057,#196058),
 .UNSPECIFIED.,.F.,.F.,(4,3,3,3,3,3,3,3,3,3,3,3,3,3,3,3,3,3,3,3,3,3,3,3,
3,3,3,3,3,3,3,3,3,3,3,3,3,3,3,3,3,3,3,3,3,3,3,3,3,3,3,3,3,3,3,4),(141.371669411541,
141.451198509903,141.529734449958,141.608177579576,141.686542407125,141.764843385513,
141.843094921964,141.921314479505,141.999517401059,142.077716685554,142.155925327365,
142.234188974226,142.312481079904,142.390856893055,142.449938245765,142.529580152191,
142.609151771933,142.688664000902,142.768119334592,142.84754051065,142.926937172227,
142.949308113696,143.030538210322,143.111817101372,143.196032321436,143.277463174856,
143.363070578242,143.448677981627,143.533921279926,143.619086354082,143.70410072196,
143.789008030756,143.873722533028,143.948047849558,144.024590852544,144.101128396887,
144.177675089655,144.254277629943,144.330911375259,144.407628763105,144.44741771749,
144.526964817571,144.606451648938,144.685890476518,144.765293527766,144.844673001574,
144.924053723792,145.003437127507,145.082834295609,145.162256318606,145.241749751984,
145.321281581371,145.40090230935,145.446157453352,145.5276156997,145.609073946049),
 .UNSPECIFIED.);
#3353=B_SPLINE_CURVE_WITH_KNOTS('',3,(#196064,#196065,#196066,#196067,#196068,
#196069,#196070,#196071,#196072,#196073,#196074,#196075,#196076,#196077,
#196078,#196079,#196080,#196081,#196082,#196083,#196084,#196085,#196086,
#196087,#196088,#196089,#196090,#196091,#196092,#196093,#196094,#196095,
#196096,#196097,#196098,#196099,#196100,#196101,#196102,#196103,#196104,
#196105,#196106,#196107,#196108,#196109,#196110,#196111,#196112,#196113,
#196114,#196115,#196116,#196117,#196118,#196119,#196120,#196121,#196122,
#196123,#196124,#196125,#196126,#196127,#196128,#196129,#196130,#196131,
#196132,#196133,#196134,#196135,#196136,#196137,#196138,#196139,#196140,
#196141,#196142,#196143,#196144,#196145,#196146,#196147,#196148,#196149,
#196150,#196151,#196152,#196153,#196154,#196155,#196156,#196157,#196158,
#196159,#196160,#196161,#196162,#196163,#196164,#196165,#196166,#196167,
#196168,#196169,#196170,#196171,#196172,#196173,#196174,#196175,#196176,
#196177,#196178,#196179,#196180,#196181,#196182,#196183,#196184,#196185,
#196186,#196187,#196188,#196189,#196190,#196191,#196192,#196193,#196194,
#196195,#196196,#196197,#196198,#196199,#196200,#196201,#196202,#196203,
#196204,#196205,#196206,#196207,#196208,#196209,#196210,#196211,#196212,
#196213,#196214,#196215,#196216,#196217,#196218,#196219,#196220,#196221,
#196222,#196223,#196224,#196225,#196226,#196227,#196228,#196229),
 .UNSPECIFIED.,.F.,.F.,(4,3,3,3,3,3,3,3,3,3,3,3,3,3,3,3,3,3,3,3,3,3,3,3,
3,3,3,3,3,3,3,3,3,3,3,3,3,3,3,3,3,3,3,3,3,3,3,3,3,3,3,3,3,3,3,4),(147.655171343303,
147.73209130362,147.809015725201,147.887934862734,147.964942280489,148.044817277911,
148.124692275333,148.204239375413,148.283726206781,148.363165034361,148.442568085608,
148.521947559416,148.601328281635,148.68071168535,148.760108853452,148.839530876448,
148.919024309826,148.998556139214,149.078176867193,149.123432011195,149.20108776939,
149.27865733512,149.356154641751,149.433583280185,149.510972126311,149.588335020489,
149.622801879126,149.706296686172,149.789948363162,149.873838758403,149.957843203787,
150.042034162009,150.122171747057,150.199669093726,150.277084412078,150.354433331746,
150.431731434717,150.508994266042,150.586250279162,150.663505432724,150.740773774066,
150.818069355322,150.895452963306,150.972882171574,151.050431512685,151.120911482919,
151.196977001861,151.272944877175,151.350133540636,151.425945761604,151.501716956229,
151.577462159768,151.655710166041,151.73146722759,151.810960706224,151.890454184858),
 .UNSPECIFIED.);
#3354=B_SPLINE_CURVE_WITH_KNOTS('',3,(#196230,#196231,#196232,#196233,#196234,
#196235,#196236,#196237,#196238,#196239,#196240,#196241,#196242,#196243,
#196244,#196245,#196246,#196247,#196248,#196249,#196250,#196251,#196252,
#196253,#196254,#196255,#196256,#196257,#196258,#196259,#196260,#196261,
#196262,#196263,#196264,#196265,#196266,#196267,#196268,#196269,#196270,
#196271,#196272,#196273,#196274,#196275,#196276,#196277,#196278,#196279,
#196280,#196281,#196282,#196283,#196284,#196285,#196286,#196287,#196288,
#196289,#196290,#196291,#196292,#196293,#196294,#196295,#196296,#196297,
#196298,#196299,#196300,#196301,#196302,#196303,#196304,#196305),
 .UNSPECIFIED.,.F.,.F.,(4,3,3,3,3,3,3,3,3,3,3,3,3,3,3,3,3,3,3,3,3,3,3,3,
3,4),(145.608344229852,145.69080583361,145.77326677149,145.855727070888,
145.938186759201,146.020645863823,146.103104412146,146.18556243156,146.268019949453,
146.354697122532,146.437163908141,146.519629021272,146.602092571579,146.684554668693,
146.767015422225,146.849474941767,146.931933336894,147.014390717165,147.096857102985,
147.179320304609,147.261780760557,147.344238909193,147.426704513205,147.509164391782,
147.591628503519,147.654854718721),.UNSPECIFIED.);
#3355=B_SPLINE_CURVE_WITH_KNOTS('',3,(#196307,#196308,#196309,#196310,#196311,
#196312,#196313,#196314,#196315,#196316,#196317,#196318,#196319,#196320,
#196321,#196322,#196323,#196324,#196325,#196326,#196327,#196328,#196329,
#196330,#196331,#196332,#196333,#196334,#196335,#196336,#196337,#196338,
#196339,#196340,#196341,#196342,#196343,#196344,#196345,#196346,#196347,
#196348,#196349,#196350,#196351,#196352,#196353,#196354,#196355,#196356,
#196357,#196358,#196359,#196360,#196361,#196362,#196363,#196364,#196365,
#196366,#196367,#196368,#196369,#196370,#196371,#196372,#196373,#196374,
#196375,#196376,#196377,#196378,#196379,#196380,#196381,#196382,#196383,
#196384,#196385),.UNSPECIFIED.,.F.,.F.,(4,3,3,3,3,3,3,3,3,3,3,3,3,3,3,3,
3,3,3,3,3,3,3,3,3,3,4),(145.609073946049,145.68656484209,145.763988977529,
145.841374551929,145.918735111077,145.945527321283,146.029022128329,146.112673805319,
146.19656420056,146.280568645943,146.364759604166,146.444897189214,146.522394535883,
146.599809854235,146.677158773903,146.754456876874,146.831719708198,146.908975721319,
146.986230874881,147.063499216223,147.140794797479,147.218178405462,147.295607613731,
147.373156954842,147.443636925076,147.549245821898,147.654854718721),
 .UNSPECIFIED.);
#3356=B_SPLINE_CURVE_WITH_KNOTS('',3,(#196386,#196387,#196388,#196389,#196390,
#196391,#196392,#196393,#196394,#196395,#196396,#196397,#196398,#196399,
#196400,#196401,#196402,#196403,#196404,#196405,#196406,#196407,#196408,
#196409,#196410,#196411,#196412,#196413,#196414,#196415,#196416,#196417,
#196418,#196419,#196420,#196421,#196422,#196423,#196424,#196425,#196426,
#196427,#196428,#196429,#196430,#196431,#196432,#196433,#196434,#196435,
#196436,#196437,#196438,#196439,#196440,#196441,#196442,#196443,#196444,
#196445,#196446,#196447,#196448,#196449,#196450,#196451,#196452,#196453,
#196454,#196455,#196456,#196457,#196458,#196459,#196460,#196461,#196462,
#196463,#196464,#196465,#196466,#196467,#196468,#196469,#196470,#196471,
#196472,#196473,#196474,#196475,#196476,#196477,#196478,#196479,#196480,
#196481,#196482,#196483,#196484,#196485,#196486,#196487,#196488,#196489,
#196490,#196491,#196492,#196493,#196494,#196495,#196496,#196497,#196498,
#196499,#196500,#196501,#196502,#196503,#196504,#196505,#196506,#196507,
#196508,#196509,#196510,#196511,#196512,#196513,#196514,#196515,#196516,
#196517,#196518,#196519,#196520,#196521,#196522,#196523,#196524,#196525,
#196526,#196527,#196528,#196529,#196530,#196531,#196532,#196533,#196534,
#196535,#196536,#196537,#196538,#196539,#196540,#196541,#196542,#196543,
#196544,#196545,#196546,#196547,#196548,#196549,#196550,#196551,#196552,
#196553,#196554),.UNSPECIFIED.,.F.,.F.,(4,3,3,3,3,3,3,3,3,3,3,3,3,3,3,3,
3,3,3,3,3,3,3,3,3,3,3,3,3,3,3,3,3,3,3,3,3,3,3,3,3,3,3,3,3,3,3,3,3,3,3,3,
3,3,3,3,4),(147.654854718845,147.729591060665,147.804268784978,147.878905015242,
147.953528146011,148.028147561493,148.102778681513,148.177436942878,148.252181161896,
148.326973368477,148.401877963143,148.442376660938,148.520912600993,148.599355730611,
148.67772055816,148.756021536547,148.834273072998,148.912492630539,148.990695552093,
149.068894836588,149.147103478399,149.225367125261,149.303659230938,149.38203504409,
149.4411163968,149.520758303226,149.600329922968,149.679842151936,149.759297485627,
149.838718661684,149.918115323261,149.940486264732,150.021716361358,150.102995252409,
150.187210472473,150.268641325893,150.354248729278,150.439856132663,150.525099430962,
150.610264505116,150.695278872994,150.78018618179,150.864900684061,150.939226000594,
151.01576900358,151.092306547923,151.168853240691,151.245455780979,151.322089526295,
151.398806914141,151.438595868525,151.518145880864,151.597636918564,151.677073113388,
151.756475815793,151.835859086637,151.891383072134),.UNSPECIFIED.);
#3357=B_SPLINE_CURVE_WITH_KNOTS('',3,(#196560,#196561,#196562,#196563,#196564,
#196565,#196566,#196567,#196568,#196569,#196570,#196571,#196572,#196573,
#196574,#196575,#196576,#196577,#196578,#196579,#196580,#196581,#196582,
#196583,#196584,#196585,#196586,#196587,#196588,#196589,#196590,#196591,
#196592,#196593,#196594,#196595,#196596,#196597,#196598,#196599,#196600,
#196601,#196602,#196603,#196604,#196605,#196606,#196607,#196608,#196609,
#196610,#196611,#196612,#196613,#196614,#196615,#196616,#196617,#196618,
#196619,#196620,#196621,#196622,#196623,#196624,#196625,#196626,#196627,
#196628,#196629,#196630,#196631,#196632,#196633,#196634,#196635,#196636,
#196637,#196638,#196639,#196640,#196641,#196642,#196643,#196644,#196645,
#196646,#196647,#196648,#196649,#196650,#196651,#196652,#196653,#196654,
#196655,#196656,#196657,#196658,#196659,#196660,#196661,#196662,#196663,
#196664,#196665,#196666,#196667,#196668,#196669,#196670,#196671,#196672,
#196673,#196674,#196675,#196676,#196677,#196678,#196679,#196680,#196681,
#196682,#196683,#196684,#196685,#196686,#196687,#196688,#196689,#196690,
#196691,#196692,#196693,#196694,#196695,#196696,#196697,#196698,#196699,
#196700,#196701,#196702,#196703,#196704,#196705,#196706,#196707,#196708,
#196709,#196710,#196711,#196712,#196713,#196714,#196715,#196716,#196717,
#196718,#196719,#196720,#196721,#196722,#196723,#196724,#196725),
 .UNSPECIFIED.,.F.,.F.,(4,3,3,3,3,3,3,3,3,3,3,3,3,3,3,3,3,3,3,3,3,3,3,3,
3,3,3,3,3,3,3,3,3,3,3,3,3,3,3,3,3,3,3,3,3,3,3,3,3,3,3,3,3,3,3,4),(153.938040025994,
154.027615078815,154.117130690506,154.202373988805,154.28753906296,154.372553430837,
154.457460739633,154.542175241905,154.616500558437,154.693043561423,154.769581105765,
154.846127798534,154.922730338822,154.999364084138,155.076081471984,155.115870426368,
155.195417526448,155.274904357816,155.354343185396,155.433746236643,155.513125710451,
155.59250643267,155.671889836384,155.751287004487,155.830709027483,155.910202460861,
155.989734290248,156.069355018227,156.11461016223,156.192265920425,156.269835486155,
156.347332792786,156.42476143122,156.502150277347,156.579513171524,156.613980030161,
156.697474837207,156.781126514197,156.865016909438,156.949021354822,157.033212313045,
157.113349898092,157.190847244761,157.268262563113,157.345611482781,157.422909585752,
157.500172417077,157.577428430198,157.654683583759,157.731951925102,157.809247506357,
157.886631114341,157.96406032261,158.041609663721,158.112089633955,158.17544691121),
 .UNSPECIFIED.);
#3358=B_SPLINE_CURVE_WITH_KNOTS('',3,(#196726,#196727,#196728,#196729,#196730,
#196731,#196732,#196733,#196734,#196735,#196736,#196737,#196738,#196739,
#196740,#196741,#196742,#196743,#196744,#196745,#196746,#196747,#196748,
#196749,#196750,#196751,#196752,#196753,#196754,#196755,#196756,#196757,
#196758,#196759,#196760,#196761,#196762,#196763,#196764,#196765,#196766,
#196767,#196768,#196769,#196770,#196771,#196772,#196773,#196774,#196775,
#196776,#196777,#196778,#196779,#196780,#196781,#196782,#196783,#196784,
#196785,#196786,#196787,#196788,#196789,#196790,#196791,#196792,#196793,
#196794,#196795,#196796,#196797,#196798,#196799,#196800,#196801,#196802,
#196803,#196804,#196805,#196806,#196807),.UNSPECIFIED.,.F.,.F.,(4,3,3,3,
3,3,3,3,3,3,3,3,3,3,3,3,3,3,3,3,3,3,3,3,3,3,3,4),(151.890454184858,151.966371647742,
152.043011433262,152.119651218781,152.198187158836,152.276630288454,152.354995116003,
152.433296094391,152.511547630842,152.589767188383,152.667970109937,152.746169394432,
152.824378036243,152.902641683104,152.980933788782,153.059309601933,153.118390954644,
153.198032861071,153.277604480813,153.357116709783,153.436572043473,153.515993219531,
153.595389881108,153.617760822575,153.697830623407,153.777060453003,153.857550239452,
153.938040025901),.UNSPECIFIED.);
#3359=B_SPLINE_CURVE_WITH_KNOTS('',3,(#196809,#196810,#196811,#196812,#196813,
#196814,#196815,#196816,#196817,#196818,#196819,#196820,#196821,#196822,
#196823,#196824,#196825,#196826,#196827,#196828,#196829,#196830,#196831,
#196832,#196833,#196834,#196835,#196836,#196837,#196838,#196839,#196840,
#196841,#196842,#196843,#196844,#196845,#196846,#196847,#196848,#196849,
#196850,#196851,#196852,#196853,#196854,#196855,#196856,#196857,#196858,
#196859,#196860,#196861,#196862,#196863,#196864,#196865,#196866,#196867,
#196868,#196869,#196870,#196871,#196872,#196873,#196874,#196875,#196876,
#196877,#196878,#196879,#196880,#196881,#196882,#196883,#196884,#196885,
#196886,#196887,#196888,#196889,#196890),.UNSPECIFIED.,.F.,.F.,(4,3,3,3,
3,3,3,3,3,3,3,3,3,3,3,3,3,3,3,3,3,3,3,3,3,3,3,4),(151.891383072134,151.97076450571,
152.05015637347,152.129569762885,152.209053657481,152.288572885094,152.368186515532,
152.437335604387,152.514991362581,152.592560928312,152.670058234943,152.747486873377,
152.824875719503,152.902238613681,152.936705472318,153.020200279363,153.103851956354,
153.187742351595,153.271746796978,153.355937755201,153.436075340249,153.515525194001,
153.594871057291,153.674124288318,153.753272553693,153.832358942751,153.911381727581,
153.938040025901),.UNSPECIFIED.);
#3360=B_SPLINE_CURVE_WITH_KNOTS('',3,(#196891,#196892,#196893,#196894,#196895,
#196896,#196897,#196898,#196899,#196900,#196901,#196902,#196903,#196904,
#196905,#196906,#196907,#196908,#196909,#196910,#196911,#196912,#196913,
#196914,#196915,#196916,#196917,#196918,#196919,#196920,#196921,#196922,
#196923,#196924,#196925,#196926,#196927,#196928,#196929,#196930,#196931,
#196932,#196933,#196934,#196935,#196936,#196937,#196938,#196939,#196940,
#196941,#196942,#196943,#196944,#196945,#196946,#196947,#196948,#196949,
#196950,#196951,#196952,#196953,#196954,#196955,#196956,#196957,#196958,
#196959,#196960,#196961,#196962,#196963,#196964,#196965,#196966,#196967,
#196968,#196969,#196970,#196971,#196972,#196973,#196974,#196975,#196976,
#196977,#196978,#196979,#196980,#196981,#196982,#196983,#196984,#196985,
#196986,#196987,#196988,#196989,#196990,#196991,#196992,#196993,#196994,
#196995,#196996,#196997,#196998,#196999,#197000,#197001,#197002,#197003,
#197004,#197005,#197006,#197007,#197008,#197009,#197010,#197011,#197012,
#197013,#197014,#197015,#197016,#197017,#197018,#197019,#197020,#197021,
#197022,#197023,#197024,#197025,#197026,#197027,#197028,#197029,#197030,
#197031,#197032,#197033,#197034,#197035,#197036,#197037,#197038,#197039,
#197040,#197041,#197042,#197043,#197044,#197045,#197046,#197047,#197048,
#197049,#197050,#197051,#197052,#197053,#197054,#197055,#197056,#197057,
#197058,#197059),.UNSPECIFIED.,.F.,.F.,(4,3,3,3,3,3,3,3,3,3,3,3,3,3,3,3,
3,3,3,3,3,3,3,3,3,3,3,3,3,3,3,3,3,3,3,3,3,3,3,3,3,3,3,3,3,3,3,3,3,3,3,3,
3,3,3,3,4),(153.938040026018,154.021006808716,154.104150032445,154.187570243097,
154.271128008187,154.354917908727,154.434815076111,154.51086652383,154.586823114724,
154.662701635653,154.73851879335,154.814291233106,154.891699180465,154.967447228801,
155.043203290799,155.118982377375,155.197625486025,155.273538398867,155.349508778856,
155.42558627253,155.433554811974,155.512090752029,155.590533881648,155.668898709196,
155.747199687584,155.825451224035,155.903670781576,155.98187370313,156.060072987625,
156.138281629436,156.216545276298,156.294837381975,156.373213195127,156.432294547836,
156.511936454262,156.591508074004,156.671020302973,156.750475636663,156.82989681272,
156.909293474297,156.931664415767,157.012894512393,157.094173403444,157.178388623507,
157.259819476928,157.345426880313,157.431034283698,157.516277581997,157.601442656152,
157.686457024029,157.771364332825,157.856078835097,157.930404151629,158.006946635292,
158.083479310245,158.16002739832,158.174370687208),.UNSPECIFIED.);
#3361=B_SPLINE_CURVE_WITH_KNOTS('',3,(#197065,#197066,#197067,#197068,#197069,
#197070,#197071,#197072,#197073,#197074,#197075,#197076,#197077,#197078,
#197079,#197080,#197081,#197082,#197083,#197084,#197085,#197086,#197087,
#197088,#197089,#197090,#197091,#197092,#197093,#197094,#197095,#197096,
#197097,#197098,#197099,#197100,#197101,#197102,#197103,#197104,#197105,
#197106,#197107,#197108,#197109,#197110,#197111,#197112,#197113,#197114,
#197115,#197116,#197117,#197118,#197119,#197120,#197121,#197122,#197123,
#197124,#197125,#197126,#197127,#197128,#197129,#197130,#197131,#197132,
#197133,#197134,#197135,#197136,#197137,#197138,#197139,#197140,#197141,
#197142,#197143,#197144,#197145,#197146,#197147,#197148,#197149,#197150,
#197151,#197152,#197153,#197154,#197155,#197156,#197157,#197158,#197159,
#197160,#197161,#197162,#197163,#197164,#197165,#197166,#197167,#197168,
#197169,#197170,#197171,#197172,#197173,#197174,#197175,#197176,#197177,
#197178,#197179,#197180,#197181,#197182,#197183,#197184,#197185,#197186,
#197187,#197188,#197189,#197190,#197191,#197192,#197193,#197194,#197195,
#197196,#197197,#197198,#197199,#197200,#197201,#197202,#197203,#197204,
#197205,#197206,#197207,#197208,#197209,#197210,#197211,#197212,#197213,
#197214,#197215,#197216,#197217,#197218,#197219,#197220,#197221,#197222,
#197223,#197224,#197225,#197226,#197227,#197228,#197229,#197230),
 .UNSPECIFIED.,.F.,.F.,(4,3,3,3,3,3,3,3,3,3,3,3,3,3,3,3,3,3,3,3,3,3,3,3,
3,3,3,3,3,3,3,3,3,3,3,3,3,3,3,3,3,3,3,3,3,3,3,3,3,3,3,3,3,3,3,4),(160.221225333176,
160.298250388259,160.375922534597,160.452848578413,160.530893776012,160.60893897361,
160.690169070236,160.771447961287,160.85566318135,160.937094034771,161.022701438156,
161.108308841541,161.19355213984,161.278717213994,161.363731581872,161.448638890667,
161.533353392939,161.607678709472,161.684221712458,161.7607592568,161.837305949568,
161.913908489857,161.990542235172,162.067259623018,162.107048577403,162.186595677484,
162.266082508851,162.345521336431,162.424924387679,162.504303861487,162.583684583706,
162.66306798742,162.742465155522,162.821887178519,162.901380611897,162.980912441285,
163.060533169264,163.105788313265,163.18344407146,163.26101363719,163.338510943822,
163.415939582256,163.493328428382,163.57069132256,163.605158181197,163.688652988243,
163.772304665233,163.856195060474,163.940199505858,164.024390464081,164.104528049128,
164.182040570407,164.259450079704,164.33680020683,164.414096438049,164.458358196858),
 .UNSPECIFIED.);
#3362=B_SPLINE_CURVE_WITH_KNOTS('',3,(#197231,#197232,#197233,#197234,#197235,
#197236,#197237,#197238,#197239,#197240,#197241,#197242,#197243,#197244,
#197245,#197246,#197247,#197248,#197249,#197250,#197251,#197252,#197253,
#197254,#197255,#197256,#197257,#197258,#197259,#197260,#197261,#197262,
#197263,#197264,#197265,#197266,#197267,#197268,#197269,#197270,#197271,
#197272,#197273,#197274,#197275,#197276,#197277,#197278,#197279,#197280,
#197281,#197282,#197283,#197284,#197285,#197286,#197287,#197288,#197289,
#197290,#197291,#197292,#197293,#197294,#197295,#197296,#197297,#197298,
#197299,#197300,#197301,#197302,#197303,#197304,#197305,#197306,#197307,
#197308,#197309,#197310,#197311,#197312,#197313,#197314,#197315),
 .UNSPECIFIED.,.F.,.F.,(4,3,3,3,3,3,3,3,3,3,3,3,3,3,3,3,3,3,3,3,3,3,3,3,
3,3,3,3,4),(158.17544691121,158.251418173854,158.3273085691,158.403134815705,
158.478913568005,158.557903043232,158.633651177154,158.709405131614,158.785179916075,
158.860990554791,158.936894403711,159.012853234892,159.088923024484,159.110829369817,
159.189365309872,159.26780843949,159.346173267039,159.424474245426,159.502725781877,
159.580945339418,159.659148260972,159.737347545467,159.815556187278,159.893819834139,
159.972111939817,160.050487752968,160.109569105679,160.211051659851,160.22122533308),
 .UNSPECIFIED.);
#3363=B_SPLINE_CURVE_WITH_KNOTS('',3,(#197317,#197318,#197319,#197320,#197321,
#197322,#197323,#197324,#197325,#197326,#197327,#197328,#197329,#197330,
#197331,#197332,#197333,#197334,#197335,#197336,#197337,#197338,#197339,
#197340,#197341,#197342,#197343,#197344,#197345,#197346,#197347,#197348,
#197349,#197350,#197351,#197352,#197353,#197354,#197355,#197356,#197357,
#197358,#197359,#197360,#197361,#197362,#197363,#197364,#197365,#197366,
#197367,#197368,#197369,#197370,#197371,#197372,#197373,#197374,#197375,
#197376,#197377,#197378,#197379,#197380,#197381,#197382,#197383,#197384,
#197385,#197386,#197387,#197388,#197389,#197390,#197391,#197392,#197393,
#197394,#197395,#197396,#197397,#197398,#197399,#197400,#197401),
 .UNSPECIFIED.,.F.,.F.,(4,3,3,3,3,3,3,3,3,3,3,3,3,3,3,3,3,3,3,3,3,3,3,3,
3,3,3,3,4),(158.174370687208,158.250978071601,158.327619117061,158.404341050154,
158.42977401956,158.50932111964,158.588807951008,158.668246778588,158.747649829835,
158.827029303643,158.906410025862,158.985793429576,159.065190597678,159.144612620674,
159.224106054052,159.30363788344,159.383258611419,159.428513755422,159.506169513617,
159.583739079347,159.661236385978,159.738665024412,159.816053870539,159.893416764717,
159.927883623353,160.005717791887,160.083593193719,160.161573552186,160.221225332989),
 .UNSPECIFIED.);
#3364=B_SPLINE_CURVE_WITH_KNOTS('',3,(#197402,#197403,#197404,#197405,#197406,
#197407,#197408,#197409,#197410,#197411,#197412,#197413,#197414,#197415,
#197416,#197417,#197418,#197419,#197420,#197421,#197422,#197423,#197424,
#197425,#197426,#197427,#197428,#197429,#197430,#197431,#197432,#197433,
#197434,#197435,#197436,#197437,#197438,#197439,#197440,#197441,#197442,
#197443,#197444,#197445,#197446,#197447,#197448,#197449,#197450,#197451,
#197452,#197453,#197454,#197455,#197456,#197457,#197458,#197459,#197460,
#197461,#197462,#197463,#197464,#197465,#197466,#197467,#197468,#197469,
#197470,#197471,#197472,#197473,#197474,#197475,#197476,#197477,#197478,
#197479,#197480,#197481,#197482,#197483,#197484,#197485,#197486,#197487,
#197488,#197489,#197490,#197491,#197492,#197493,#197494,#197495,#197496,
#197497,#197498,#197499,#197500,#197501,#197502,#197503,#197504,#197505,
#197506,#197507,#197508,#197509,#197510,#197511,#197512,#197513,#197514,
#197515,#197516,#197517,#197518,#197519,#197520,#197521,#197522,#197523,
#197524,#197525,#197526,#197527,#197528,#197529,#197530,#197531,#197532,
#197533,#197534,#197535,#197536,#197537,#197538,#197539,#197540,#197541,
#197542,#197543,#197544,#197545,#197546,#197547,#197548,#197549,#197550,
#197551,#197552,#197553,#197554,#197555,#197556,#197557,#197558,#197559,
#197560,#197561,#197562,#197563,#197564,#197565,#197566,#197567,#197568,
#197569,#197570),.UNSPECIFIED.,.F.,.F.,(4,3,3,3,3,3,3,3,3,3,3,3,3,3,3,3,
3,3,3,3,3,3,3,3,3,3,3,3,3,3,3,3,3,3,3,3,3,3,3,3,3,3,3,3,3,3,3,3,3,3,3,3,
3,3,3,3,4),(160.22122533308,160.326650068649,160.427253491284,160.504750837953,
160.582166156305,160.659515075973,160.736813178944,160.814076010268,160.891332023389,
160.968587176951,161.045855518293,161.123151099549,161.200534707533,161.277963915802,
161.355513256912,161.425993227147,161.502044674866,161.57800126576,161.653879786689,
161.729696944386,161.805469384142,161.882877331501,161.958625379837,162.034381441835,
162.110160528411,162.188803637061,162.264716549903,162.340686929892,162.416764423566,
162.424732963009,162.503268903064,162.581712032682,162.660076860231,162.738377838619,
162.816629375069,162.89484893261,162.973051854164,163.051251138659,163.12945978047,
163.207723427332,163.286015533009,163.36439134616,163.423472698871,163.503114605297,
163.582686225039,163.662198454008,163.741653787698,163.821074963756,163.900471625333,
163.922842566802,164.004072663428,164.085351554479,164.169566774542,164.250997627963,
164.336605031348,164.422212434733,164.457960367931),.UNSPECIFIED.);
#3365=B_SPLINE_CURVE_WITH_KNOTS('',3,(#197576,#197577,#197578,#197579,#197580,
#197581,#197582,#197583,#197584,#197585,#197586,#197587,#197588,#197589,
#197590,#197591,#197592,#197593,#197594,#197595,#197596,#197597,#197598,
#197599,#197600,#197601,#197602,#197603,#197604,#197605,#197606,#197607,
#197608,#197609,#197610,#197611,#197612,#197613,#197614,#197615,#197616,
#197617,#197618,#197619,#197620,#197621,#197622,#197623,#197624,#197625,
#197626,#197627,#197628,#197629,#197630,#197631,#197632,#197633,#197634,
#197635,#197636,#197637,#197638,#197639,#197640,#197641,#197642,#197643,
#197644,#197645,#197646,#197647,#197648,#197649,#197650,#197651,#197652,
#197653,#197654,#197655,#197656,#197657,#197658,#197659,#197660,#197661,
#197662,#197663,#197664,#197665,#197666,#197667,#197668,#197669,#197670,
#197671,#197672,#197673,#197674,#197675,#197676,#197677,#197678,#197679,
#197680,#197681,#197682,#197683,#197684,#197685,#197686,#197687,#197688,
#197689,#197690,#197691,#197692,#197693,#197694,#197695,#197696,#197697,
#197698,#197699,#197700,#197701,#197702,#197703,#197704,#197705,#197706,
#197707,#197708,#197709,#197710,#197711,#197712,#197713,#197714,#197715,
#197716,#197717,#197718,#197719,#197720,#197721,#197722,#197723,#197724,
#197725,#197726,#197727,#197728,#197729,#197730,#197731,#197732),
 .UNSPECIFIED.,.F.,.F.,(4,3,3,3,3,3,3,3,3,3,3,3,3,3,3,3,3,3,3,3,3,3,3,3,
3,3,3,3,3,3,3,3,3,3,3,3,3,3,3,3,3,3,3,3,3,3,3,3,3,3,3,3,4),(166.50441064026,
166.586872846346,166.669334704134,166.751796220475,166.834257402219,166.916718256215,
166.999178789314,167.081639008364,167.164098920215,167.246558531714,167.329017849711,
167.411476881053,167.493935632588,167.576394111165,167.658852323629,167.74131027683,
167.823767977612,167.906225432824,167.988682649311,168.074695237101,168.158019931522,
168.24048653708,168.322952298431,168.405417242989,168.487881398167,168.570344791374,
168.652807450018,168.735269401502,168.817730673228,168.900191292596,168.982651287003,
169.065110683845,169.147569510513,169.2300277944,169.312485562893,169.394942843381,
169.47907675683,169.561542755128,169.644007131677,169.726469996119,169.808931458076,
169.89139162715,169.973850612924,170.056308524967,170.141905641668,170.224370378611,
170.30683215091,170.389291397001,170.471748555179,170.554211074078,170.636668745362,
170.71912753627,170.74108545857),.UNSPECIFIED.);
#3366=B_SPLINE_CURVE_WITH_KNOTS('',3,(#197733,#197734,#197735,#197736,#197737,
#197738,#197739,#197740,#197741,#197742,#197743,#197744,#197745,#197746,
#197747,#197748,#197749,#197750,#197751,#197752,#197753,#197754,#197755,
#197756,#197757,#197758,#197759,#197760,#197761,#197762,#197763,#197764,
#197765,#197766,#197767,#197768,#197769,#197770,#197771,#197772,#197773,
#197774,#197775,#197776,#197777,#197778,#197779,#197780,#197781,#197782,
#197783,#197784,#197785,#197786,#197787,#197788,#197789,#197790,#197791,
#197792,#197793,#197794,#197795,#197796,#197797,#197798,#197799,#197800,
#197801,#197802,#197803,#197804,#197805,#197806,#197807,#197808,#197809,
#197810,#197811,#197812,#197813,#197814,#197815,#197816,#197817),
 .UNSPECIFIED.,.F.,.F.,(4,3,3,3,3,3,3,3,3,3,3,3,3,3,3,3,3,3,3,3,3,3,3,3,
3,3,3,3,4),(164.458358196858,164.538971895374,164.616225717916,164.69348733951,
164.770770809529,164.84809018696,164.925500388357,165.002963990101,165.080534426416,
165.10326778499,165.179319232709,165.255275823603,165.331154344532,165.406971502229,
165.482743941986,165.560151889344,165.63589993768,165.711655999678,165.787435086255,
165.866078194904,165.941991107746,166.017961487735,166.094038981409,166.102007520852,
166.192747188222,166.283004388607,166.372894866779,166.462116729469,166.50441064026),
 .UNSPECIFIED.);
#3367=B_SPLINE_CURVE_WITH_KNOTS('',3,(#197819,#197820,#197821,#197822,#197823,
#197824,#197825,#197826,#197827,#197828,#197829,#197830,#197831,#197832,
#197833,#197834,#197835,#197836,#197837,#197838,#197839,#197840,#197841,
#197842,#197843,#197844,#197845,#197846,#197847,#197848,#197849,#197850,
#197851,#197852,#197853,#197854,#197855,#197856,#197857,#197858,#197859,
#197860,#197861,#197862,#197863,#197864,#197865,#197866,#197867,#197868,
#197869,#197870,#197871,#197872,#197873,#197874,#197875,#197876,#197877,
#197878,#197879,#197880,#197881,#197882,#197883,#197884,#197885,#197886,
#197887,#197888,#197889,#197890,#197891,#197892,#197893,#197894,#197895,
#197896,#197897,#197898,#197899,#197900),.UNSPECIFIED.,.F.,.F.,(4,3,3,3,
3,3,3,3,3,3,3,3,3,3,3,3,3,3,3,3,3,3,3,3,3,3,3,4),(164.457960367931,164.543173052602,
164.628300019108,164.713270916212,164.798129799875,164.882804581115,164.921582302664,
164.99812530565,165.074662849993,165.151209542761,165.227812083049,165.304445828365,
165.381163216212,165.420952170595,165.500499270676,165.579986102043,165.659424929623,
165.73882798087,165.818207454679,165.897588176897,165.976971580612,166.056368748714,
166.13579077171,166.215284205088,166.294816034476,166.374436762455,166.419691906458,
166.50441064026),.UNSPECIFIED.);
#3368=B_SPLINE_CURVE_WITH_KNOTS('',3,(#197901,#197902,#197903,#197904,#197905,
#197906,#197907,#197908,#197909,#197910,#197911,#197912,#197913,#197914,
#197915,#197916,#197917,#197918,#197919,#197920,#197921,#197922,#197923,
#197924,#197925,#197926,#197927,#197928,#197929,#197930,#197931,#197932,
#197933,#197934,#197935,#197936,#197937,#197938,#197939,#197940,#197941,
#197942,#197943,#197944,#197945,#197946,#197947,#197948,#197949,#197950,
#197951,#197952,#197953,#197954,#197955,#197956,#197957,#197958,#197959,
#197960,#197961,#197962,#197963,#197964,#197965,#197966,#197967,#197968,
#197969,#197970,#197971,#197972,#197973,#197974,#197975,#197976,#197977,
#197978,#197979,#197980,#197981,#197982,#197983,#197984,#197985,#197986,
#197987,#197988,#197989,#197990,#197991,#197992,#197993,#197994,#197995,
#197996,#197997,#197998,#197999,#198000,#198001,#198002,#198003,#198004,
#198005,#198006,#198007,#198008,#198009,#198010,#198011,#198012,#198013,
#198014,#198015,#198016,#198017,#198018,#198019,#198020,#198021,#198022,
#198023,#198024,#198025,#198026,#198027,#198028,#198029,#198030,#198031,
#198032,#198033,#198034,#198035,#198036,#198037,#198038,#198039,#198040,
#198041,#198042,#198043,#198044,#198045,#198046,#198047,#198048,#198049,
#198050,#198051,#198052,#198053,#198054,#198055,#198056,#198057,#198058,
#198059,#198060,#198061,#198062,#198063,#198064,#198065,#198066,#198067,
#198068,#198069),.UNSPECIFIED.,.F.,.F.,(4,3,3,3,3,3,3,3,3,3,3,3,3,3,3,3,
3,3,3,3,3,3,3,3,3,3,3,3,3,3,3,3,3,3,3,3,3,3,3,3,3,3,3,3,3,3,3,3,3,3,3,3,
3,3,3,3,4),(166.504410640392,166.579684414951,166.654890959035,166.730040860453,
166.805157710638,166.880263168721,166.919061774389,167.002556581435,167.086208258425,
167.170098653666,167.25410309905,167.338294057273,167.41843164232,167.495928988989,
167.573344307341,167.650693227009,167.727991329979,167.805254161304,167.882510174425,
167.959765327986,168.037033669329,168.114329250584,168.191712858568,168.269142066837,
168.346691407948,168.417171378182,168.493222825901,168.569179416795,168.645057937724,
168.720875095421,168.796647535178,168.874055482536,168.949803530872,169.02555959287,
169.101338679446,169.179981788096,169.255894700938,169.331865080927,169.4079425746,
169.415911114044,169.494447054099,169.572890183717,169.651255011266,169.729555989654,
169.807807526105,169.886027083646,169.9642300052,170.042429289695,170.120637931507,
170.198901578368,170.277193684045,170.355569497197,170.414650849906,170.496300351367,
170.575865621596,170.658557238673,170.74124885575),.UNSPECIFIED.);
#3369=B_SPLINE_CURVE_WITH_KNOTS('',3,(#198075,#198076,#198077,#198078,#198079,
#198080,#198081,#198082,#198083,#198084,#198085,#198086,#198087,#198088,
#198089,#198090,#198091,#198092,#198093,#198094,#198095,#198096,#198097,
#198098,#198099,#198100,#198101,#198102,#198103,#198104,#198105,#198106,
#198107,#198108,#198109,#198110,#198111,#198112,#198113,#198114,#198115,
#198116,#198117,#198118,#198119,#198120,#198121,#198122,#198123,#198124,
#198125,#198126,#198127,#198128,#198129,#198130,#198131,#198132,#198133,
#198134,#198135,#198136,#198137,#198138,#198139,#198140,#198141,#198142,
#198143,#198144,#198145,#198146,#198147,#198148,#198149,#198150,#198151,
#198152,#198153,#198154,#198155,#198156,#198157,#198158,#198159,#198160,
#198161,#198162,#198163,#198164,#198165,#198166,#198167,#198168,#198169,
#198170,#198171,#198172,#198173,#198174,#198175,#198176,#198177,#198178,
#198179,#198180,#198181,#198182,#198183,#198184,#198185,#198186,#198187,
#198188,#198189,#198190,#198191,#198192,#198193,#198194,#198195,#198196,
#198197,#198198,#198199,#198200,#198201,#198202,#198203,#198204,#198205,
#198206,#198207,#198208,#198209,#198210,#198211,#198212,#198213,#198214,
#198215,#198216,#198217,#198218,#198219,#198220,#198221,#198222,#198223,
#198224,#198225,#198226,#198227,#198228,#198229,#198230,#198231,#198232,
#198233,#198234,#198235,#198236,#198237,#198238,#198239,#198240),
 .UNSPECIFIED.,.F.,.F.,(4,3,3,3,3,3,3,3,3,3,3,3,3,3,3,3,3,3,3,3,3,3,3,3,
3,3,3,3,3,3,3,3,3,3,3,3,3,3,3,3,3,3,3,3,3,3,3,3,3,3,3,3,3,3,3,4),(172.787595947439,
172.876862502991,172.966706250952,173.057285678573,173.093185671887,173.171721611942,
173.25016474156,173.328529569109,173.406830547497,173.485082083947,173.563301641489,
173.641504563043,173.719703847538,173.79791248935,173.876176136211,173.954468241888,
174.03284405504,174.091925407749,174.171567314175,174.251138933917,174.330651162886,
174.410106496576,174.489527672634,174.568924334211,174.591295275681,174.672525372307,
174.753804263359,174.838019483422,174.919450336843,175.005057740227,175.090665143612,
175.175908441911,175.261073516065,175.346087883942,175.430995192738,175.51570969501,
175.590035011543,175.666578014529,175.743115558872,175.81966225164,175.896264791928,
175.972898537244,176.04961592509,176.089404879474,176.168953942453,176.248442212459,
176.327881956182,176.407285402419,176.486671556819,176.566048604272,176.645427626364,
176.724819704607,176.804267800039,176.883744007039,176.96329955227,177.02436573765),
 .UNSPECIFIED.);
#3370=B_SPLINE_CURVE_WITH_KNOTS('',3,(#198241,#198242,#198243,#198244,#198245,
#198246,#198247,#198248,#198249,#198250,#198251,#198252,#198253,#198254,
#198255,#198256,#198257,#198258,#198259,#198260,#198261,#198262,#198263,
#198264,#198265,#198266,#198267,#198268,#198269,#198270,#198271,#198272,
#198273,#198274,#198275,#198276,#198277,#198278,#198279,#198280,#198281,
#198282,#198283,#198284,#198285,#198286,#198287,#198288,#198289,#198290,
#198291,#198292,#198293,#198294,#198295,#198296,#198297,#198298,#198299,
#198300,#198301,#198302,#198303,#198304,#198305,#198306,#198307,#198308,
#198309,#198310,#198311,#198312,#198313,#198314,#198315,#198316),
 .UNSPECIFIED.,.F.,.F.,(4,3,3,3,3,3,3,3,3,3,3,3,3,3,3,3,3,3,3,3,3,3,3,3,
3,4),(170.74108545857,170.823547062329,170.906008000208,170.988468299606,
171.070927987919,171.153387092541,171.235845640864,171.318303660278,171.400761178171,
171.48743835125,171.569905136859,171.65237024999,171.734833800297,171.817295897411,
171.899756650943,171.982216170485,172.064674565612,172.147131945883,172.229598331702,
172.312061533327,172.394521989275,172.476980137911,172.559445741923,172.6419056205,
172.724369732237,172.787595947439),.UNSPECIFIED.);
#3371=B_SPLINE_CURVE_WITH_KNOTS('',3,(#198318,#198319,#198320,#198321,#198322,
#198323,#198324,#198325,#198326,#198327,#198328,#198329,#198330,#198331,
#198332,#198333,#198334,#198335,#198336,#198337,#198338,#198339,#198340,
#198341,#198342,#198343,#198344,#198345,#198346,#198347,#198348,#198349,
#198350,#198351,#198352,#198353,#198354,#198355,#198356,#198357,#198358,
#198359,#198360,#198361,#198362,#198363,#198364,#198365,#198366,#198367,
#198368,#198369,#198370,#198371,#198372,#198373,#198374,#198375,#198376,
#198377,#198378,#198379,#198380,#198381,#198382,#198383,#198384,#198385,
#198386,#198387,#198388,#198389,#198390,#198391,#198392,#198393,#198394,
#198395,#198396,#198397,#198398,#198399),.UNSPECIFIED.,.F.,.F.,(4,3,3,3,
3,3,3,3,3,3,3,3,3,3,3,3,3,3,3,3,3,3,3,3,3,3,3,4),(170.74124885575,170.820666993372,
170.900061492849,170.914020717837,170.995250814463,171.076529705514,171.160744925578,
171.242175778998,171.327783182383,171.413390585768,171.498633884067,171.583798958223,
171.668813326101,171.753720634897,171.83843513717,171.9127604537,171.989303456686,
172.065841001029,172.142387693797,172.218990234086,172.295623979402,172.372341367248,
172.412130321631,172.505996728083,172.595652790931,172.685089950228,172.774119132675,
172.787595947439),.UNSPECIFIED.);
#3372=B_SPLINE_CURVE_WITH_KNOTS('',3,(#198400,#198401,#198402,#198403,#198404,
#198405,#198406,#198407,#198408,#198409,#198410,#198411,#198412,#198413,
#198414,#198415,#198416,#198417,#198418,#198419,#198420,#198421,#198422,
#198423,#198424,#198425,#198426,#198427,#198428,#198429,#198430,#198431,
#198432,#198433,#198434,#198435,#198436,#198437,#198438,#198439,#198440,
#198441,#198442,#198443,#198444,#198445,#198446,#198447,#198448,#198449,
#198450,#198451,#198452,#198453,#198454,#198455,#198456,#198457,#198458,
#198459,#198460,#198461,#198462,#198463,#198464,#198465,#198466,#198467,
#198468,#198469,#198470,#198471,#198472,#198473,#198474,#198475,#198476,
#198477,#198478,#198479,#198480,#198481,#198482,#198483,#198484,#198485,
#198486,#198487,#198488,#198489,#198490,#198491,#198492,#198493,#198494,
#198495,#198496,#198497,#198498,#198499,#198500,#198501,#198502,#198503,
#198504,#198505,#198506,#198507,#198508,#198509,#198510,#198511,#198512,
#198513,#198514,#198515,#198516,#198517,#198518,#198519,#198520,#198521,
#198522,#198523,#198524,#198525,#198526,#198527,#198528,#198529,#198530,
#198531,#198532,#198533,#198534,#198535,#198536,#198537,#198538,#198539,
#198540,#198541,#198542,#198543,#198544,#198545,#198546,#198547,#198548,
#198549,#198550,#198551,#198552,#198553,#198554,#198555,#198556),
 .UNSPECIFIED.,.F.,.F.,(4,3,3,3,3,3,3,3,3,3,3,3,3,3,3,3,3,3,3,3,3,3,3,3,
3,3,3,3,3,3,3,3,3,3,3,3,3,3,3,3,3,3,3,3,3,3,3,3,3,3,3,3,4),(172.787595947439,
172.870058153525,172.952520011313,173.034981527654,173.117442709398,173.199903563394,
173.282364096493,173.364824315543,173.447284227394,173.529743838893,173.61220315689,
173.694662188232,173.777120939767,173.859579418344,173.942037630808,174.024495584008,
174.106953284791,174.189410740003,174.271867956491,174.35788054428,174.441205238701,
174.523671844259,174.60613760561,174.688602550168,174.771066705346,174.853530098553,
174.935992757197,175.018454708681,175.100915980407,175.183376599775,175.265836594182,
175.348295991024,175.430754817692,175.513213101579,175.595670870072,175.67812815056,
175.762262064009,175.844728062307,175.927192438856,176.009655303298,176.092116765255,
176.174576934329,176.257035920104,176.339493832146,176.425090948847,176.507555685791,
176.590017458089,176.67247670418,176.754933862358,176.837396381257,176.919854052541,
177.002312843449,177.02427076575),.UNSPECIFIED.);
#3373=B_SPLINE_CURVE_WITH_KNOTS('',3,(#198562,#198563,#198564,#198565,#198566,
#198567,#198568,#198569,#198570,#198571,#198572,#198573,#198574,#198575,
#198576,#198577,#198578,#198579,#198580,#198581,#198582,#198583,#198584,
#198585,#198586,#198587,#198588,#198589,#198590,#198591,#198592,#198593,
#198594,#198595,#198596,#198597,#198598,#198599,#198600,#198601,#198602,
#198603,#198604,#198605,#198606,#198607,#198608,#198609,#198610,#198611,
#198612,#198613,#198614,#198615,#198616,#198617,#198618,#198619,#198620,
#198621,#198622,#198623,#198624,#198625,#198626,#198627,#198628,#198629,
#198630,#198631,#198632,#198633,#198634,#198635,#198636,#198637,#198638,
#198639,#198640,#198641,#198642,#198643,#198644,#198645,#198646,#198647,
#198648,#198649,#198650,#198651,#198652,#198653,#198654,#198655,#198656,
#198657,#198658,#198659,#198660,#198661,#198662,#198663,#198664,#198665,
#198666,#198667,#198668,#198669,#198670,#198671,#198672,#198673,#198674,
#198675,#198676,#198677,#198678,#198679,#198680,#198681,#198682,#198683,
#198684,#198685,#198686,#198687,#198688,#198689,#198690,#198691,#198692,
#198693,#198694,#198695,#198696,#198697,#198698,#198699,#198700,#198701,
#198702,#198703,#198704,#198705,#198706,#198707,#198708,#198709,#198710,
#198711,#198712,#198713,#198714,#198715,#198716,#198717,#198718,#198719,
#198720,#198721,#198722,#198723,#198724,#198725,#198726,#198727,#198728,
#198729,#198730,#198731,#198732,#198733),.UNSPECIFIED.,.F.,.F.,(4,3,3,3,
3,3,3,3,3,3,3,3,3,3,3,3,3,3,3,3,3,3,3,3,3,3,3,3,3,3,3,3,3,3,3,3,3,3,3,3,
3,3,3,3,3,3,3,3,3,3,3,3,3,3,3,3,3,4),(179.070781254619,179.08562408706,
179.161675534779,179.237632125673,179.313510646602,179.389327804299,179.465100244055,
179.542508191414,179.61825623975,179.694012301748,179.769791388324,179.848434496974,
179.924347409816,180.000317789805,180.076395283479,180.084363822923,180.162899762978,
180.241342892596,180.319707720146,180.398008698533,180.476260234983,180.554479792525,
180.632682714078,180.710881998573,180.789090640385,180.867354287246,180.945646392924,
181.024022206075,181.083103558785,181.162745465211,181.242317084953,181.321829313921,
181.401284647611,181.480705823669,181.560102485245,181.582473426716,181.663703523342,
181.744982414393,181.829197634456,181.910628487877,181.996235891262,182.081843294647,
182.167086592946,182.252251667101,182.337266034979,182.422173343774,182.506887846047,
182.581213162578,182.657756165564,182.734293709907,182.810840402675,182.887442942963,
182.964076688279,183.040794076125,183.080583030509,183.160132981289,183.239615331457,
183.307446438644),.UNSPECIFIED.);
#3374=B_SPLINE_CURVE_WITH_KNOTS('',3,(#198734,#198735,#198736,#198737,#198738,
#198739,#198740,#198741,#198742,#198743,#198744,#198745,#198746,#198747,
#198748,#198749,#198750,#198751,#198752,#198753,#198754,#198755,#198756,
#198757,#198758,#198759,#198760,#198761,#198762,#198763,#198764,#198765,
#198766,#198767,#198768,#198769,#198770,#198771,#198772,#198773,#198774,
#198775,#198776,#198777,#198778,#198779,#198780,#198781,#198782,#198783,
#198784,#198785,#198786,#198787,#198788,#198789,#198790,#198791,#198792,
#198793,#198794,#198795,#198796,#198797,#198798,#198799,#198800,#198801,
#198802,#198803,#198804,#198805,#198806,#198807,#198808,#198809,#198810,
#198811,#198812,#198813,#198814,#198815),.UNSPECIFIED.,.F.,.F.,(4,3,3,3,
3,3,3,3,3,3,3,3,3,3,3,3,3,3,3,3,3,3,3,3,3,3,3,4),(177.02436573765,177.088144615336,
177.165800373531,177.243369939261,177.320867245892,177.398295884327,177.475684730453,
177.553047624631,177.587514483267,177.671009290313,177.754660967303,177.838551362544,
177.922555807927,178.00674676615,178.086884351198,178.164139151355,178.241311843178,
178.318418290553,178.395474308542,178.472495674665,178.549511188248,178.626526849768,
178.703556916167,178.780615650056,178.857762652621,178.934956926078,179.012268091969,
179.070781254542),.UNSPECIFIED.);
#3375=B_SPLINE_CURVE_WITH_KNOTS('',3,(#198817,#198818,#198819,#198820,#198821,
#198822,#198823,#198824,#198825,#198826,#198827,#198828,#198829,#198830,
#198831,#198832,#198833,#198834,#198835,#198836,#198837,#198838,#198839,
#198840,#198841,#198842,#198843,#198844,#198845,#198846,#198847,#198848,
#198849,#198850,#198851,#198852,#198853,#198854,#198855,#198856,#198857,
#198858,#198859,#198860,#198861,#198862,#198863,#198864,#198865,#198866,
#198867,#198868,#198869,#198870,#198871,#198872,#198873,#198874,#198875,
#198876,#198877,#198878,#198879,#198880,#198881,#198882,#198883,#198884,
#198885,#198886,#198887,#198888,#198889,#198890,#198891,#198892),
 .UNSPECIFIED.,.F.,.F.,(4,3,3,3,3,3,3,3,3,3,3,3,3,3,3,3,3,3,3,3,3,3,3,3,
3,4),(177.02427076575,177.106732369508,177.189193307387,177.271653606785,
177.354113295099,177.436572399721,177.519030948044,177.601488967458,177.683946485351,
177.77062365843,177.853090444039,177.93555555717,178.018019107477,178.100481204591,
178.182941958123,178.265401477665,178.347859872792,178.430317253063,178.512783638882,
178.595246840506,178.677707296455,178.760165445091,178.842631049103,178.92509092768,
179.007555039417,179.070781254619),.UNSPECIFIED.);
#3376=B_SPLINE_CURVE_WITH_KNOTS('',3,(#198893,#198894,#198895,#198896,#198897,
#198898,#198899,#198900,#198901,#198902,#198903,#198904,#198905,#198906,
#198907,#198908,#198909,#198910,#198911,#198912,#198913,#198914,#198915,
#198916,#198917,#198918,#198919,#198920,#198921,#198922,#198923,#198924,
#198925,#198926,#198927,#198928,#198929,#198930,#198931,#198932,#198933,
#198934,#198935,#198936,#198937,#198938,#198939,#198940,#198941,#198942,
#198943,#198944,#198945,#198946,#198947,#198948,#198949,#198950,#198951,
#198952,#198953,#198954,#198955,#198956,#198957,#198958,#198959,#198960,
#198961,#198962,#198963,#198964,#198965,#198966,#198967,#198968,#198969,
#198970,#198971,#198972,#198973,#198974,#198975,#198976,#198977,#198978,
#198979,#198980,#198981,#198982,#198983,#198984,#198985,#198986,#198987,
#198988,#198989,#198990,#198991,#198992,#198993,#198994,#198995,#198996,
#198997,#198998,#198999,#199000,#199001,#199002,#199003,#199004,#199005,
#199006,#199007,#199008,#199009,#199010,#199011,#199012,#199013,#199014,
#199015,#199016,#199017,#199018,#199019,#199020,#199021,#199022,#199023,
#199024,#199025,#199026,#199027,#199028,#199029,#199030,#199031,#199032,
#199033,#199034,#199035,#199036,#199037,#199038,#199039,#199040,#199041,
#199042,#199043,#199044,#199045,#199046,#199047,#199048,#199049,#199050,
#199051,#199052,#199053,#199054,#199055,#199056,#199057,#199058,#199059,
#199060,#199061),.UNSPECIFIED.,.F.,.F.,(4,3,3,3,3,3,3,3,3,3,3,3,3,3,3,3,
3,3,3,3,3,3,3,3,3,3,3,3,3,3,3,3,3,3,3,3,3,3,3,3,3,3,3,3,3,3,3,3,3,3,3,3,
3,3,3,3,4),(179.070781254619,179.153913059131,179.234053402285,179.314265484234,
179.394594630683,179.403308472666,179.482855572747,179.562342404114,179.641781231694,
179.721184282941,179.800563756749,179.879944478968,179.959327882683,180.038725050785,
180.118147073781,180.197640507159,180.277172336546,180.356793064525,180.402048208528,
180.479703966723,180.557273532453,180.634770839085,180.712199477519,180.789588323645,
180.866951217823,180.901418076459,180.984912883505,181.068564560495,181.152454955735,
181.236459401119,181.320650359341,181.40078794439,181.478285291059,181.555700609411,
181.633049529079,181.71034763205,181.787610463375,181.864866476496,181.942121630057,
182.0193899714,182.096685552655,182.174069160639,182.251498368908,182.329047710019,
182.399527680252,182.475584479301,182.551545305904,182.627426953978,182.703246135693,
182.779020318668,182.854770603365,182.930512001994,183.006259518897,183.082065779061,
183.15790101961,183.233833983586,183.306487245332),.UNSPECIFIED.);
#3377=B_SPLINE_CURVE_WITH_KNOTS('',3,(#199067,#199068,#199069,#199070,#199071,
#199072,#199073,#199074,#199075,#199076,#199077,#199078,#199079,#199080,
#199081,#199082,#199083,#199084,#199085,#199086,#199087,#199088,#199089,
#199090,#199091,#199092,#199093,#199094,#199095,#199096,#199097,#199098,
#199099,#199100,#199101,#199102,#199103,#199104,#199105,#199106,#199107,
#199108,#199109,#199110,#199111,#199112,#199113,#199114,#199115,#199116,
#199117,#199118,#199119,#199120,#199121,#199122,#199123,#199124,#199125,
#199126,#199127,#199128,#199129,#199130,#199131,#199132,#199133,#199134,
#199135,#199136,#199137,#199138,#199139,#199140,#199141,#199142,#199143,
#199144,#199145,#199146,#199147,#199148,#199149,#199150,#199151,#199152,
#199153,#199154,#199155,#199156,#199157,#199158,#199159,#199160,#199161,
#199162,#199163,#199164,#199165,#199166,#199167,#199168,#199169,#199170,
#199171,#199172,#199173,#199174,#199175,#199176,#199177,#199178,#199179,
#199180,#199181,#199182,#199183,#199184,#199185,#199186,#199187,#199188,
#199189,#199190,#199191,#199192,#199193,#199194,#199195,#199196,#199197,
#199198,#199199,#199200,#199201,#199202,#199203,#199204,#199205,#199206,
#199207,#199208,#199209,#199210,#199211,#199212,#199213,#199214,#199215,
#199216,#199217,#199218,#199219,#199220,#199221,#199222,#199223,#199224,
#199225,#199226,#199227,#199228,#199229,#199230,#199231,#199232,#199233,
#199234,#199235,#199236,#199237,#199238),.UNSPECIFIED.,.F.,.F.,(4,3,3,3,
3,3,3,3,3,3,3,3,3,3,3,3,3,3,3,3,3,3,3,3,3,3,3,3,3,3,3,3,3,3,3,3,3,3,3,3,
3,3,3,3,3,3,3,3,3,3,3,3,3,3,3,3,3,4),(185.353966561799,185.431397596384,
185.512073176598,185.589494048608,185.66692687484,185.744385501764,185.821883787648,
185.899477736777,185.977127970281,186.054888344769,186.076802238096,186.152853685815,
186.228810276709,186.304688797638,186.380505955335,186.456278395092,186.53368634245,
186.609434390786,186.685190452784,186.76096953936,186.83961264801,186.915525560852,
186.991495940841,187.067573434515,187.075541973958,187.154077914013,187.232521043631,
187.31088587118,187.389186849568,187.467438386018,187.545657943559,187.623860865113,
187.702060149608,187.78026879142,187.858532438281,187.936824543958,188.015200357109,
188.07428170982,188.153923616247,188.233495235989,188.313007464958,188.392462798648,
188.471883974706,188.551280636283,188.573651577751,188.654881674376,188.736160565427,
188.82037578549,188.90180663891,188.987414042296,189.073021445682,189.158264743983,
189.24342981814,189.32844418602,189.413351494817,189.498065997092,189.572391313613,
189.59099683695),.UNSPECIFIED.);
#3378=B_SPLINE_CURVE_WITH_KNOTS('',3,(#199239,#199240,#199241,#199242,#199243,
#199244,#199245,#199246,#199247,#199248,#199249,#199250,#199251,#199252,
#199253,#199254,#199255,#199256,#199257,#199258,#199259,#199260,#199261,
#199262,#199263,#199264,#199265,#199266,#199267,#199268,#199269,#199270,
#199271,#199272,#199273,#199274,#199275,#199276,#199277,#199278,#199279,
#199280,#199281,#199282,#199283,#199284,#199285,#199286,#199287,#199288,
#199289,#199290,#199291,#199292,#199293,#199294,#199295,#199296,#199297,
#199298,#199299,#199300,#199301,#199302,#199303,#199304,#199305,#199306,
#199307,#199308,#199309,#199310,#199311,#199312,#199313,#199314,#199315,
#199316,#199317),.UNSPECIFIED.,.F.,.F.,(4,3,3,3,3,3,3,3,3,3,3,3,3,3,3,3,
3,3,3,3,3,3,3,3,3,3,4),(183.307446438644,183.386853957618,183.466236117432,
183.54561737589,183.624999696255,183.7043941609,183.783811858775,183.863300537031,
183.942826121031,184.022443246328,184.079322766371,184.156978524565,184.234548090295,
184.312045396926,184.38947403536,184.466862881487,184.544225775665,184.578692634302,
184.662187441348,184.745839118338,184.829729513579,184.913733958962,184.997924917185,
185.078062502233,185.169457246868,185.261711904271,185.353966561674),
 .UNSPECIFIED.);
#3379=B_SPLINE_CURVE_WITH_KNOTS('',3,(#199319,#199320,#199321,#199322,#199323,
#199324,#199325,#199326,#199327,#199328,#199329,#199330,#199331,#199332,
#199333,#199334,#199335,#199336,#199337,#199338,#199339,#199340,#199341,
#199342,#199343,#199344,#199345,#199346,#199347,#199348,#199349,#199350,
#199351,#199352,#199353,#199354,#199355,#199356,#199357,#199358,#199359,
#199360,#199361,#199362,#199363,#199364,#199365,#199366,#199367,#199368,
#199369,#199370,#199371,#199372,#199373,#199374,#199375,#199376,#199377,
#199378,#199379,#199380,#199381,#199382,#199383,#199384,#199385,#199386,
#199387,#199388,#199389,#199390,#199391,#199392,#199393,#199394,#199395,
#199396,#199397,#199398,#199399,#199400,#199401,#199402,#199403),
 .UNSPECIFIED.,.F.,.F.,(4,3,3,3,3,3,3,3,3,3,3,3,3,3,3,3,3,3,3,3,3,3,3,3,
3,3,3,3,4),(183.306487245332,183.382560392752,183.398267416115,183.47680335617,
183.555246485789,183.633611313337,183.711912291725,183.790163828176,183.868383385717,
183.946586307271,184.024785591766,184.102994233577,184.181257880439,184.259549986116,
184.337925799268,184.397007151977,184.476649058403,184.556220678145,184.635732907114,
184.715188240804,184.794609416862,184.874006078439,184.896377019908,184.976854947956,
185.057372730165,185.13797882469,185.218630132761,185.299378318199,185.353966561691),
 .UNSPECIFIED.);
#3380=B_SPLINE_CURVE_WITH_KNOTS('',3,(#199404,#199405,#199406,#199407,#199408,
#199409,#199410,#199411,#199412,#199413,#199414,#199415,#199416,#199417,
#199418,#199419,#199420,#199421,#199422,#199423,#199424,#199425,#199426,
#199427,#199428,#199429,#199430,#199431,#199432,#199433,#199434,#199435,
#199436,#199437,#199438,#199439,#199440,#199441,#199442,#199443,#199444,
#199445,#199446,#199447,#199448,#199449,#199450,#199451,#199452,#199453,
#199454,#199455,#199456,#199457,#199458,#199459,#199460,#199461,#199462,
#199463,#199464,#199465,#199466,#199467,#199468,#199469,#199470,#199471,
#199472,#199473,#199474,#199475,#199476,#199477,#199478,#199479,#199480,
#199481,#199482,#199483,#199484,#199485,#199486,#199487,#199488,#199489,
#199490,#199491,#199492,#199493,#199494,#199495,#199496,#199497,#199498,
#199499,#199500,#199501,#199502,#199503,#199504,#199505,#199506,#199507,
#199508,#199509,#199510,#199511,#199512,#199513,#199514,#199515,#199516,
#199517,#199518,#199519,#199520,#199521,#199522,#199523,#199524,#199525,
#199526,#199527,#199528,#199529,#199530,#199531,#199532,#199533,#199534,
#199535,#199536,#199537,#199538,#199539,#199540,#199541,#199542,#199543,
#199544,#199545,#199546,#199547,#199548,#199549,#199550,#199551,#199552,
#199553,#199554,#199555,#199556,#199557,#199558,#199559,#199560,#199561,
#199562,#199563,#199564,#199565,#199566,#199567,#199568,#199569,#199570,
#199571,#199572),.UNSPECIFIED.,.F.,.F.,(4,3,3,3,3,3,3,3,3,3,3,3,3,3,3,3,
3,3,3,3,3,3,3,3,3,3,3,3,3,3,3,3,3,3,3,3,3,3,3,3,3,3,3,3,3,3,3,3,3,3,3,3,
3,3,3,3,4),(185.353966561798,185.395746887839,185.480990186138,185.566155260292,
185.65116962817,185.736076936966,185.820791439238,185.89511675577,185.971659758756,
186.048197303098,186.124743995867,186.201346536155,186.277980281471,186.354697669317,
186.394486623701,186.474033723781,186.553520555149,186.632959382729,186.712362433976,
186.791741907784,186.871122630003,186.950506033717,187.029903201819,187.109325224816,
187.188818658194,187.268350487581,187.34797121556,187.393226359563,187.470882117758,
187.548451683488,187.62594899012,187.703377628554,187.780766474681,187.858129368859,
187.892596227494,187.97609103454,188.05974271153,188.143633106771,188.227637552155,
188.311828510378,188.391966095426,188.469463442095,188.546878760447,188.624227680115,
188.701525783086,188.778788614411,188.856044627531,188.933299781093,189.010568122436,
189.087863703691,189.165247311675,189.242676519944,189.320225861055,189.390705831288,
189.466769112667,189.542722467021,189.591595664567),.UNSPECIFIED.);
#3381=B_SPLINE_CURVE_WITH_KNOTS('',3,(#199578,#199579,#199580,#199581,#199582,
#199583,#199584,#199585,#199586,#199587,#199588,#199589,#199590,#199591,
#199592,#199593,#199594,#199595,#199596,#199597,#199598,#199599,#199600,
#199601,#199602,#199603,#199604,#199605,#199606,#199607,#199608,#199609,
#199610,#199611,#199612,#199613,#199614,#199615,#199616,#199617,#199618,
#199619,#199620,#199621,#199622,#199623,#199624,#199625,#199626,#199627,
#199628,#199629,#199630,#199631,#199632,#199633,#199634,#199635,#199636,
#199637,#199638,#199639,#199640,#199641,#199642,#199643,#199644,#199645,
#199646,#199647,#199648,#199649,#199650,#199651,#199652,#199653,#199654,
#199655,#199656,#199657,#199658,#199659,#199660,#199661,#199662,#199663,
#199664,#199665,#199666,#199667,#199668,#199669,#199670,#199671,#199672,
#199673,#199674,#199675,#199676,#199677,#199678,#199679,#199680,#199681,
#199682,#199683,#199684,#199685,#199686,#199687,#199688,#199689,#199690,
#199691,#199692,#199693,#199694,#199695,#199696,#199697,#199698,#199699,
#199700,#199701,#199702,#199703,#199704,#199705,#199706,#199707,#199708,
#199709,#199710,#199711,#199712,#199713,#199714,#199715,#199716,#199717,
#199718,#199719,#199720,#199721,#199722,#199723,#199724,#199725,#199726,
#199727,#199728,#199729,#199730,#199731,#199732,#199733,#199734,#199735,
#199736,#199737,#199738,#199739,#199740,#199741,#199742,#199743,#199744,
#199745,#199746),.UNSPECIFIED.,.F.,.F.,(4,3,3,3,3,3,3,3,3,3,3,3,3,3,3,3,
3,3,3,3,3,3,3,3,3,3,3,3,3,3,3,3,3,3,3,3,3,3,3,3,3,3,3,3,3,3,3,3,3,3,3,3,
3,3,3,3,4),(191.637151869054,191.722777560031,191.809393333341,191.89558240367,
191.982411528469,192.069240653269,192.146737999944,192.224153318303,192.301502237977,
192.378800340955,192.456063172286,192.533319185413,192.610574338981,192.687842680331,
192.765138261593,192.842521869583,192.919951077859,192.997500418976,193.067980389131,
193.144031836845,193.219988427734,193.295866948658,193.37168410635,193.447456546102,
193.524864493463,193.600612541795,193.676368603788,193.752147690359,193.830790799018,
193.906703711855,193.98267409184,194.058751585509,194.066720124993,194.14525606503,
194.22369919463,194.302064022161,194.38036500053,194.458616536963,194.536836094486,
194.615039016022,194.693238300499,194.771446942293,194.849710589137,194.928002694797,
195.006378507932,195.065459860855,195.145101767453,195.224673387365,195.304185616502,
195.383640950358,195.463062126579,195.542458788317,195.564829728786,195.646075149419,
195.727358735464,195.808726488626,195.873338800186),.UNSPECIFIED.);
#3382=B_SPLINE_CURVE_WITH_KNOTS('',3,(#199747,#199748,#199749,#199750,#199751,
#199752,#199753,#199754,#199755,#199756,#199757,#199758,#199759,#199760,
#199761,#199762,#199763,#199764,#199765,#199766,#199767,#199768,#199769,
#199770,#199771,#199772,#199773,#199774,#199775,#199776,#199777,#199778,
#199779,#199780,#199781,#199782,#199783,#199784,#199785,#199786,#199787,
#199788,#199789,#199790,#199791,#199792,#199793,#199794,#199795,#199796,
#199797,#199798,#199799,#199800,#199801,#199802,#199803,#199804,#199805,
#199806,#199807,#199808,#199809,#199810,#199811,#199812,#199813,#199814,
#199815,#199816,#199817,#199818,#199819,#199820,#199821,#199822,#199823,
#199824,#199825,#199826,#199827,#199828,#199829,#199830,#199831),
 .UNSPECIFIED.,.F.,.F.,(4,3,3,3,3,3,3,3,3,3,3,3,3,3,3,3,3,3,3,3,3,3,3,3,
3,3,3,3,4),(189.59099683695,189.667537169314,189.744075593563,189.820626716693,
189.897235631924,189.973878939468,190.050602334764,190.071761181544,190.151308281625,
190.230795112993,190.310233940575,190.389636991823,190.46901646563,190.54839718785,
190.627780591565,190.707177759668,190.786599782666,190.866093216045,190.945625045432,
191.025245773412,191.070500917407,191.148156675604,191.225726241338,191.303223547972,
191.380652186409,191.458041032538,191.535403926719,191.569870785338,191.637151868978),
 .UNSPECIFIED.);
#3383=B_SPLINE_CURVE_WITH_KNOTS('',3,(#199833,#199834,#199835,#199836,#199837,
#199838,#199839,#199840,#199841,#199842,#199843,#199844,#199845,#199846,
#199847,#199848,#199849,#199850,#199851,#199852,#199853,#199854,#199855,
#199856,#199857,#199858,#199859,#199860,#199861,#199862,#199863,#199864,
#199865,#199866,#199867,#199868,#199869,#199870,#199871,#199872,#199873,
#199874,#199875,#199876,#199877,#199878,#199879,#199880,#199881,#199882,
#199883,#199884,#199885,#199886,#199887,#199888,#199889,#199890,#199891,
#199892,#199893,#199894,#199895,#199896,#199897,#199898,#199899,#199900,
#199901,#199902,#199903,#199904,#199905,#199906,#199907,#199908,#199909,
#199910,#199911,#199912,#199913,#199914),.UNSPECIFIED.,.F.,.F.,(4,3,3,3,
3,3,3,3,3,3,3,3,3,3,3,3,3,3,3,3,3,3,3,3,3,3,3,4),(189.591595664567,189.667432750365,
189.743219200234,189.818971628897,189.894720555063,189.970471825777,190.04624044869,
190.122041443609,190.197934494988,190.273879391914,190.349940250266,190.38944556715,
190.467981507205,190.546424636823,190.624789464372,190.70309044276,190.78134197921,
190.859561536751,190.937764458305,191.0159637428,191.094172384611,191.172436031473,
191.25072813715,191.329103950301,191.388185303012,191.476084222021,191.563689717781,
191.637151868978),.UNSPECIFIED.);
#3384=B_SPLINE_CURVE_WITH_KNOTS('',3,(#199915,#199916,#199917,#199918,#199919,
#199920,#199921,#199922,#199923,#199924,#199925,#199926,#199927,#199928,
#199929,#199930,#199931,#199932,#199933,#199934,#199935,#199936,#199937,
#199938,#199939,#199940,#199941,#199942,#199943,#199944,#199945,#199946,
#199947,#199948,#199949,#199950,#199951,#199952,#199953,#199954,#199955,
#199956,#199957,#199958,#199959,#199960,#199961,#199962,#199963,#199964,
#199965,#199966,#199967,#199968,#199969,#199970,#199971,#199972,#199973,
#199974,#199975,#199976,#199977,#199978,#199979,#199980,#199981,#199982,
#199983,#199984,#199985,#199986,#199987,#199988,#199989,#199990,#199991,
#199992,#199993,#199994,#199995,#199996,#199997,#199998,#199999,#200000,
#200001,#200002,#200003,#200004,#200005,#200006,#200007,#200008,#200009,
#200010,#200011,#200012,#200013,#200014,#200015,#200016,#200017,#200018,
#200019,#200020,#200021,#200022,#200023,#200024,#200025,#200026,#200027,
#200028,#200029,#200030,#200031,#200032,#200033,#200034,#200035,#200036,
#200037,#200038,#200039,#200040,#200041,#200042,#200043,#200044,#200045,
#200046,#200047,#200048,#200049,#200050,#200051,#200052,#200053,#200054,
#200055,#200056,#200057,#200058,#200059,#200060,#200061,#200062,#200063,
#200064,#200065,#200066,#200067,#200068,#200069,#200070,#200071,#200072,
#200073,#200074,#200075,#200076,#200077,#200078,#200079,#200080,#200081,
#200082,#200083),.UNSPECIFIED.,.F.,.F.,(4,3,3,3,3,3,3,3,3,3,3,3,3,3,3,3,
3,3,3,3,3,3,3,3,3,3,3,3,3,3,3,3,3,3,3,3,3,3,3,3,3,3,3,3,3,3,3,3,3,3,3,3,
3,3,3,3,4),(191.63715186911,191.712667239094,191.788156227102,191.863640540428,
191.887555170943,191.968785267568,192.050064158618,192.134279378682,192.215710232102,
192.301317635488,192.386925038874,192.472168337175,192.557333411333,192.642347779213,
192.727255088011,192.811969590285,192.886294906805,192.962837909789,193.03937545413,
193.115922146896,193.192524687182,193.269158432496,193.34587582034,193.385664774736,
193.465211874817,193.544698706185,193.624137533766,193.703540585014,193.782920058823,
193.862300781042,193.941684184758,194.021081352861,194.100503375858,194.179996809237,
194.259528638625,194.339149366605,194.384404510599,194.462060268796,194.539629834529,
194.617127141162,194.694555779599,194.771944625727,194.849307519907,194.88377437853,
194.967269185567,195.050920862549,195.134811257781,195.218815703156,195.303006661369,
195.383144246461,195.46064239363,195.538061228243,195.615414915786,195.692710924807,
195.769973698718,195.847219668722,195.873920875799),.UNSPECIFIED.);
#3385=B_SPLINE_CURVE_WITH_KNOTS('',3,(#200089,#200090,#200091,#200092,#200093,
#200094,#200095,#200096,#200097,#200098,#200099,#200100,#200101,#200102,
#200103,#200104,#200105,#200106,#200107,#200108,#200109,#200110,#200111,
#200112,#200113,#200114,#200115,#200116,#200117,#200118,#200119,#200120,
#200121,#200122,#200123,#200124,#200125,#200126,#200127,#200128,#200129,
#200130,#200131,#200132,#200133,#200134,#200135,#200136,#200137,#200138,
#200139,#200140,#200141,#200142,#200143,#200144,#200145,#200146,#200147,
#200148,#200149,#200150,#200151,#200152,#200153,#200154,#200155,#200156,
#200157,#200158,#200159,#200160,#200161,#200162,#200163,#200164,#200165,
#200166,#200167,#200168,#200169,#200170,#200171,#200172,#200173,#200174,
#200175,#200176,#200177,#200178,#200179,#200180,#200181,#200182,#200183,
#200184,#200185,#200186,#200187,#200188,#200189,#200190,#200191,#200192,
#200193,#200194,#200195,#200196,#200197,#200198,#200199,#200200,#200201,
#200202,#200203,#200204,#200205,#200206,#200207,#200208,#200209,#200210,
#200211,#200212,#200213,#200214,#200215,#200216,#200217,#200218,#200219,
#200220,#200221,#200222,#200223,#200224,#200225,#200226,#200227,#200228,
#200229,#200230,#200231,#200232,#200233,#200234,#200235,#200236,#200237,
#200238,#200239,#200240,#200241,#200242,#200243,#200244,#200245),
 .UNSPECIFIED.,.F.,.F.,(4,3,3,3,3,3,3,3,3,3,3,3,3,3,3,3,3,3,3,3,3,3,3,3,
3,3,3,3,3,3,3,3,3,3,3,3,3,3,3,3,3,3,3,3,3,3,3,3,3,3,3,3,4),(197.920337176158,
198.002799382244,198.085261240032,198.167722756373,198.250183938117,198.332644792113,
198.415105325212,198.497565544262,198.580025456113,198.662485067612,198.744944385609,
198.827403416951,198.909862168486,198.992320647062,199.074778859527,199.157236812727,
199.239694513509,199.322151968721,199.404609185209,199.490621772998,199.573946467419,
199.656413072977,199.738878834328,199.821343778886,199.903807934064,199.986271327272,
200.068733985915,200.151195937399,200.233657209125,200.316117828494,200.398577822901,
200.481037219742,200.56349604641,200.645954330297,200.72841209879,200.810869379278,
200.895003292727,200.977469291026,201.059933667574,201.142396532016,201.224857993973,
201.307318163047,201.389777148822,201.472235060865,201.557832177565,201.640296914509,
201.722758686807,201.805217932898,201.887675091076,201.970137609975,202.052595281259,
202.135054072167,202.157011994468),.UNSPECIFIED.);
#3386=B_SPLINE_CURVE_WITH_KNOTS('',3,(#200246,#200247,#200248,#200249,#200250,
#200251,#200252,#200253,#200254,#200255,#200256,#200257,#200258,#200259,
#200260,#200261,#200262,#200263,#200264,#200265,#200266,#200267,#200268,
#200269,#200270,#200271,#200272,#200273,#200274,#200275,#200276,#200277,
#200278,#200279,#200280,#200281,#200282,#200283,#200284,#200285,#200286,
#200287,#200288,#200289,#200290,#200291,#200292,#200293,#200294,#200295,
#200296,#200297,#200298,#200299,#200300,#200301,#200302,#200303,#200304,
#200305,#200306,#200307,#200308,#200309,#200310,#200311,#200312,#200313,
#200314,#200315,#200316,#200317,#200318,#200319,#200320,#200321,#200322,
#200323,#200324,#200325,#200326,#200327),.UNSPECIFIED.,.F.,.F.,(4,3,3,3,
3,3,3,3,3,3,3,3,3,3,3,3,3,3,3,3,3,3,3,3,3,3,3,4),(195.873338800186,195.954809490736,
196.0363716785,196.064199596717,196.149442895975,196.234607971085,196.319622339893,
196.404529649599,196.489244152733,196.563569464649,196.640112467048,196.716650010802,
196.79319670298,196.869799242676,196.946432987399,197.023150374653,197.06293933258,
197.141254613705,197.219504647999,197.297703969043,197.375870244731,197.454019045512,
197.532163481228,197.610316656745,197.688526923362,197.766765200274,197.845093906415,
197.920020567871),.UNSPECIFIED.);
#3387=B_SPLINE_CURVE_WITH_KNOTS('',3,(#200329,#200330,#200331,#200332,#200333,
#200334,#200335,#200336,#200337,#200338,#200339,#200340,#200341,#200342,
#200343,#200344,#200345,#200346,#200347,#200348,#200349,#200350,#200351,
#200352,#200353,#200354,#200355,#200356,#200357,#200358,#200359,#200360,
#200361,#200362,#200363,#200364,#200365,#200366,#200367,#200368,#200369,
#200370,#200371,#200372,#200373,#200374,#200375,#200376,#200377,#200378,
#200379,#200380,#200381,#200382,#200383,#200384,#200385,#200386,#200387,
#200388,#200389,#200390,#200391,#200392,#200393,#200394,#200395,#200396,
#200397,#200398,#200399,#200400,#200401,#200402,#200403,#200404,#200405,
#200406,#200407,#200408,#200409,#200410,#200411,#200412,#200413),
 .UNSPECIFIED.,.F.,.F.,(4,3,3,3,3,3,3,3,3,3,3,3,3,3,3,3,3,3,3,3,3,3,3,3,
3,3,3,3,4),(195.873920875799,195.951178998411,196.028455164163,196.105763428659,
196.183161355019,196.260609253835,196.338169692647,196.381883982323,196.457935430037,
196.533892020926,196.60977054185,196.685587699543,196.761360139294,196.838768086655,
196.914516134987,196.99027219698,197.066051283551,197.14469439221,197.220607305047,
197.296577685031,197.3726551787,197.380623718185,197.463675812328,197.54659562608,
197.629382895476,197.71197907297,197.794456993383,197.876765736192,197.920337176158),
 .UNSPECIFIED.);
#3388=B_SPLINE_CURVE_WITH_KNOTS('',3,(#200414,#200415,#200416,#200417,#200418,
#200419,#200420,#200421,#200422,#200423,#200424,#200425,#200426,#200427,
#200428,#200429,#200430,#200431,#200432,#200433,#200434,#200435,#200436,
#200437,#200438,#200439,#200440,#200441,#200442,#200443,#200444,#200445,
#200446,#200447,#200448,#200449,#200450,#200451,#200452,#200453,#200454,
#200455,#200456,#200457,#200458,#200459,#200460,#200461,#200462,#200463,
#200464,#200465,#200466,#200467,#200468,#200469,#200470,#200471,#200472,
#200473,#200474,#200475,#200476,#200477,#200478,#200479,#200480,#200481,
#200482,#200483,#200484,#200485,#200486,#200487,#200488,#200489,#200490,
#200491,#200492,#200493,#200494,#200495,#200496,#200497,#200498,#200499,
#200500,#200501,#200502,#200503,#200504,#200505,#200506,#200507,#200508,
#200509,#200510,#200511,#200512,#200513,#200514,#200515,#200516,#200517,
#200518,#200519,#200520,#200521,#200522,#200523,#200524,#200525,#200526,
#200527,#200528,#200529,#200530,#200531,#200532,#200533,#200534,#200535,
#200536,#200537,#200538,#200539,#200540,#200541,#200542,#200543,#200544,
#200545,#200546,#200547,#200548,#200549,#200550,#200551,#200552,#200553,
#200554,#200555,#200556,#200557,#200558,#200559,#200560,#200561,#200562,
#200563,#200564,#200565,#200566,#200567,#200568,#200569,#200570,#200571,
#200572,#200573,#200574,#200575,#200576,#200577,#200578,#200579,#200580,
#200581,#200582),.UNSPECIFIED.,.F.,.F.,(4,3,3,3,3,3,3,3,3,3,3,3,3,3,3,3,
3,3,3,3,3,3,3,3,3,3,3,3,3,3,3,3,3,3,3,3,3,3,3,3,3,3,3,3,3,3,3,3,3,3,3,3,
3,3,3,3,4),(197.920337176249,198.001811496667,198.083366322772,198.16506079004,
198.246827236305,198.328722029106,198.379363454047,198.459005360645,198.538576980557,
198.618089209695,198.697544543551,198.776965719773,198.856362381511,198.878733321978,
198.959963418148,199.041242308738,199.125457529031,199.206888381984,199.292495785947,
199.37810318991,199.463346489168,199.548511564278,199.633525933087,199.718433242792,
199.803147745927,199.877473057841,199.95401606024,200.030553603994,200.107100296171,
200.183702835867,200.26033658059,200.337053967844,200.376842925772,200.456390025619,
200.535876856751,200.615315684094,200.694718735104,200.774098208674,200.853478930655,
200.932862334133,201.012259502,201.091681524763,201.171174957912,201.250706787073,
201.330327514831,201.375582661634,201.453238422483,201.530807990849,201.608305300095,
201.685733941103,201.763122789781,201.840485686468,201.874952529565,201.958466595275,
202.042112648761,202.125946971428,202.156438065284),.UNSPECIFIED.);
#3389=B_SPLINE_CURVE_WITH_KNOTS('',3,(#200588,#200589,#200590,#200591,#200592,
#200593,#200594,#200595,#200596,#200597,#200598,#200599,#200600,#200601,
#200602,#200603,#200604,#200605,#200606,#200607,#200608,#200609,#200610,
#200611,#200612,#200613,#200614,#200615,#200616,#200617,#200618,#200619,
#200620,#200621,#200622,#200623,#200624,#200625,#200626,#200627,#200628,
#200629,#200630,#200631,#200632,#200633,#200634,#200635,#200636,#200637,
#200638,#200639,#200640,#200641,#200642,#200643,#200644,#200645,#200646,
#200647,#200648,#200649,#200650,#200651,#200652,#200653,#200654,#200655,
#200656,#200657,#200658,#200659,#200660,#200661,#200662,#200663,#200664,
#200665,#200666,#200667,#200668,#200669,#200670,#200671,#200672,#200673,
#200674,#200675,#200676,#200677,#200678,#200679,#200680,#200681,#200682,
#200683,#200684,#200685,#200686,#200687,#200688,#200689,#200690,#200691,
#200692,#200693,#200694,#200695,#200696,#200697,#200698,#200699,#200700,
#200701,#200702,#200703,#200704,#200705,#200706,#200707,#200708,#200709,
#200710,#200711,#200712,#200713,#200714,#200715,#200716,#200717,#200718,
#200719,#200720,#200721,#200722,#200723,#200724,#200725,#200726,#200727,
#200728,#200729,#200730,#200731,#200732,#200733,#200734,#200735,#200736,
#200737,#200738,#200739,#200740,#200741,#200742,#200743,#200744,#200745,
#200746,#200747,#200748,#200749,#200750,#200751,#200752,#200753,#200754,
#200755,#200756),.UNSPECIFIED.,.F.,.F.,(4,3,3,3,3,3,3,3,3,3,3,3,3,3,3,3,
3,3,3,3,3,3,3,3,3,3,3,3,3,3,3,3,3,3,3,3,3,3,3,3,3,3,3,3,3,3,3,3,3,3,3,3,
3,3,3,3,4),(204.203659867042,204.282057378475,204.36039811403,204.438696428595,
204.516973582366,204.595240588629,204.673510413808,204.751796023574,204.830147683781,
204.908533223077,204.987014140183,205.052857219477,205.130514306352,205.208085189046,
205.285583799584,205.36301371886,205.440403832364,205.517767970131,205.552227087408,
205.635719308127,205.71936831139,205.803255943232,205.887257587671,205.971445730659,
206.051596955339,206.129094684765,206.206510387096,206.283859691591,206.361158179864,
206.438421396594,206.515677793993,206.592933331113,206.670202054961,206.747498017334,
206.82488200221,206.902311585639,206.97986129538,207.050336691201,207.126389643378,
207.202347740836,207.27822776957,207.354046435493,207.429820383108,207.507227388603,
207.582976938562,207.658734499003,207.734515080148,207.813155416877,207.889069804123,
207.965041652723,208.041120598871,208.049076427064,208.127620794225,208.206046135226,
208.284403138728,208.362691339206,208.440597004682),.UNSPECIFIED.);
#3390=B_SPLINE_CURVE_WITH_KNOTS('',3,(#200757,#200758,#200759,#200760,#200761,
#200762,#200763,#200764,#200765,#200766,#200767,#200768,#200769,#200770,
#200771,#200772,#200773,#200774,#200775,#200776,#200777,#200778,#200779,
#200780,#200781,#200782,#200783,#200784,#200785,#200786,#200787,#200788,
#200789,#200790,#200791,#200792,#200793,#200794,#200795,#200796,#200797,
#200798,#200799,#200800,#200801,#200802,#200803,#200804,#200805,#200806,
#200807,#200808,#200809,#200810,#200811,#200812,#200813,#200814,#200815,
#200816,#200817,#200818,#200819,#200820,#200821,#200822,#200823,#200824,
#200825,#200826,#200827,#200828,#200829,#200830,#200831,#200832),
 .UNSPECIFIED.,.F.,.F.,(4,3,3,3,3,3,3,3,3,3,3,3,3,3,3,3,3,3,3,3,3,3,3,3,
3,4),(202.157011994468,202.239473598227,202.321934536106,202.404394835504,
202.486854523817,202.569313628439,202.651772176762,202.734230196176,202.816687714069,
202.903364887149,202.985831672757,203.068296785888,203.150760336195,203.233222433309,
203.315683186841,203.398142706383,203.48060110151,203.563058481781,203.645524867601,
203.727988069225,203.810448525173,203.89290667381,203.975372277821,204.057832156399,
204.140296268135,204.203522483337),.UNSPECIFIED.);
#3391=B_SPLINE_CURVE_WITH_KNOTS('',3,(#200834,#200835,#200836,#200837,#200838,
#200839,#200840,#200841,#200842,#200843,#200844,#200845,#200846,#200847,
#200848,#200849,#200850,#200851,#200852,#200853,#200854,#200855,#200856,
#200857,#200858,#200859,#200860,#200861,#200862,#200863,#200864,#200865,
#200866,#200867,#200868,#200869,#200870,#200871,#200872,#200873,#200874,
#200875,#200876,#200877,#200878,#200879,#200880,#200881,#200882,#200883,
#200884,#200885,#200886,#200887,#200888,#200889,#200890,#200891,#200892,
#200893,#200894,#200895,#200896,#200897,#200898,#200899,#200900,#200901,
#200902,#200903,#200904,#200905,#200906,#200907,#200908,#200909,#200910,
#200911,#200912,#200913,#200914,#200915),.UNSPECIFIED.,.F.,.F.,(4,3,3,3,
3,3,3,3,3,3,3,3,3,3,3,3,3,3,3,3,3,3,3,3,3,3,3,4),(202.156438065284,202.240482660956,
202.324695436608,202.374322397496,202.451819746577,202.529235067353,202.606583989454,
202.683882094865,202.761144928634,202.838400944198,202.915656100203,202.992924443985,
203.070220027675,203.147603638072,203.225032848747,203.302582192226,203.373062133358,
203.448085410478,203.523014838254,203.597867719145,203.673574564657,203.748326540048,
203.823058147509,203.897784777458,203.974219203903,204.049010926107,204.126266704672,
204.203522483237),.UNSPECIFIED.);
#3392=B_SPLINE_CURVE_WITH_KNOTS('',3,(#200916,#200917,#200918,#200919,#200920,
#200921,#200922,#200923,#200924,#200925,#200926,#200927,#200928,#200929,
#200930,#200931,#200932,#200933,#200934,#200935,#200936,#200937,#200938,
#200939,#200940,#200941,#200942,#200943,#200944,#200945,#200946,#200947,
#200948,#200949,#200950,#200951,#200952,#200953,#200954,#200955,#200956,
#200957,#200958,#200959,#200960,#200961,#200962,#200963,#200964,#200965,
#200966,#200967,#200968,#200969,#200970,#200971,#200972,#200973,#200974,
#200975,#200976,#200977,#200978,#200979,#200980,#200981,#200982,#200983,
#200984,#200985,#200986,#200987,#200988,#200989,#200990,#200991,#200992,
#200993,#200994,#200995,#200996,#200997,#200998,#200999,#201000,#201001,
#201002,#201003,#201004,#201005,#201006,#201007,#201008,#201009,#201010,
#201011,#201012,#201013,#201014,#201015,#201016,#201017,#201018,#201019,
#201020,#201021,#201022,#201023,#201024,#201025,#201026,#201027,#201028,
#201029,#201030,#201031,#201032,#201033,#201034,#201035,#201036,#201037,
#201038,#201039,#201040,#201041,#201042,#201043,#201044,#201045,#201046,
#201047,#201048,#201049,#201050,#201051,#201052,#201053,#201054,#201055,
#201056,#201057,#201058,#201059,#201060,#201061,#201062,#201063,#201064,
#201065,#201066,#201067,#201068,#201069,#201070,#201071,#201072,#201073,
#201074,#201075,#201076,#201077,#201078,#201079,#201080,#201081),
 .UNSPECIFIED.,.F.,.F.,(4,3,3,3,3,3,3,3,3,3,3,3,3,3,3,3,3,3,3,3,3,3,3,3,
3,3,3,3,3,3,3,3,3,3,3,3,3,3,3,3,3,3,3,3,3,3,3,3,3,3,3,3,3,3,3,4),(204.203522483337,
204.315702114456,204.37180186922,204.450337797205,204.528780914758,204.607145730263,
204.685446696645,204.763698221147,204.841917766874,204.920120676704,204.998319949582,
205.076528579899,205.154792215521,205.233084310092,205.311460112448,205.370541605083,
205.450183583791,205.529755275205,205.609267575084,205.688722978227,205.768144222806,
205.847540951289,205.869911473014,205.951141426241,206.032420172309,206.116635464468,
206.198066171773,206.283673756359,206.369281340945,206.454524813157,206.539690059704,
206.624704594246,206.709612065255,206.794326720147,206.868651208876,206.945194212473,
207.021731757981,207.098278452464,207.174880995286,207.251514743603,207.328232135144,
207.368021076807,207.447567895918,207.527054444051,207.606492986769,207.685895752165,
207.765274939768,207.844655376906,207.924038496621,208.003435382372,208.08285712523,
208.162350283778,208.241881841262,208.321502304389,208.366760812669,208.440825084745),
 .UNSPECIFIED.);
#3393=B_SPLINE_CURVE_WITH_KNOTS('',3,(#201087,#201088,#201089,#201090,#201091,
#201092,#201093,#201094,#201095,#201096,#201097,#201098,#201099,#201100,
#201101,#201102,#201103,#201104,#201105,#201106,#201107,#201108,#201109,
#201110,#201111,#201112,#201113,#201114,#201115,#201116,#201117,#201118,
#201119,#201120,#201121,#201122,#201123,#201124,#201125,#201126,#201127,
#201128,#201129,#201130,#201131,#201132,#201133,#201134,#201135,#201136,
#201137,#201138,#201139,#201140,#201141,#201142,#201143,#201144,#201145,
#201146,#201147,#201148,#201149,#201150,#201151,#201152,#201153,#201154,
#201155,#201156,#201157,#201158,#201159,#201160,#201161,#201162,#201163,
#201164,#201165,#201166,#201167,#201168,#201169,#201170,#201171,#201172,
#201173,#201174,#201175,#201176,#201177,#201178,#201179,#201180,#201181,
#201182,#201183,#201184,#201185,#201186,#201187,#201188,#201189,#201190,
#201191,#201192,#201193,#201194,#201195,#201196,#201197,#201198,#201199,
#201200,#201201,#201202,#201203,#201204,#201205,#201206,#201207,#201208,
#201209,#201210,#201211,#201212,#201213,#201214,#201215,#201216,#201217,
#201218,#201219,#201220,#201221,#201222,#201223,#201224,#201225,#201226,
#201227,#201228,#201229,#201230,#201231,#201232,#201233,#201234,#201235,
#201236,#201237,#201238,#201239,#201240,#201241,#201242,#201243),
 .UNSPECIFIED.,.F.,.F.,(4,3,3,3,3,3,3,3,3,3,3,3,3,3,3,3,3,3,3,3,3,3,3,3,
3,3,3,3,3,3,3,3,3,3,3,3,3,3,3,3,3,3,3,3,3,3,3,3,3,3,3,3,4),(210.486707790517,
210.569169996603,210.651631854391,210.734093370732,210.816554552476,210.899015406472,
210.981475939571,211.063936158621,211.146396070472,211.228855681971,211.311314999968,
211.39377403131,211.476232782845,211.558691261421,211.641149473886,211.723607427086,
211.806065127869,211.888522583081,211.970979799568,212.056992387357,212.140317081778,
212.222783687337,212.305249448687,212.387714393245,212.470178548423,212.552641941631,
212.635104600274,212.717566551758,212.800027823484,212.882488442853,212.96494843726,
213.047407834101,213.12986666077,213.212324944656,213.294782713149,213.377239993637,
213.461373907087,213.543839905385,213.626304281934,213.708767146376,213.791228608333,
213.873688777406,213.956147763181,214.038605675224,214.124202791924,214.206667528868,
214.289129301166,214.371588547257,214.454045705436,214.536508224335,214.618965895618,
214.701424686527,214.723382608827),.UNSPECIFIED.);
#3394=B_SPLINE_CURVE_WITH_KNOTS('',3,(#201244,#201245,#201246,#201247,#201248,
#201249,#201250,#201251,#201252,#201253,#201254,#201255,#201256,#201257,
#201258,#201259,#201260,#201261,#201262,#201263,#201264,#201265,#201266,
#201267,#201268,#201269,#201270,#201271,#201272,#201273,#201274,#201275,
#201276,#201277,#201278,#201279,#201280,#201281,#201282,#201283,#201284,
#201285,#201286,#201287,#201288,#201289,#201290,#201291,#201292,#201293,
#201294,#201295,#201296,#201297,#201298,#201299,#201300,#201301,#201302,
#201303,#201304,#201305,#201306,#201307,#201308,#201309,#201310,#201311,
#201312,#201313,#201314,#201315,#201316,#201317,#201318,#201319,#201320,
#201321,#201322,#201323,#201324,#201325),.UNSPECIFIED.,.F.,.F.,(4,3,3,3,
3,3,3,3,3,3,3,3,3,3,3,3,3,3,3,3,3,3,3,3,3,3,3,4),(208.440597004682,208.518812276007,
208.597010896499,208.675205870884,208.753410199333,208.831669612429,208.909957488982,
208.988329272838,209.047816162926,209.12747366929,209.207060694072,209.286588100935,
209.366058206105,209.44549389951,209.524904654142,209.547186030857,209.628406451149,
209.709675712718,209.793895759235,209.875317275478,209.960936587133,210.046555898788,
210.132401266205,210.220977897283,210.306584737466,210.392072940271,210.477374349878,
210.486707790517),.UNSPECIFIED.);
#3395=B_SPLINE_CURVE_WITH_KNOTS('',3,(#201327,#201328,#201329,#201330,#201331,
#201332,#201333,#201334,#201335,#201336,#201337,#201338,#201339,#201340,
#201341,#201342,#201343,#201344,#201345,#201346,#201347,#201348,#201349,
#201350,#201351,#201352,#201353,#201354,#201355,#201356,#201357,#201358,
#201359,#201360,#201361,#201362,#201363,#201364,#201365,#201366,#201367,
#201368,#201369,#201370,#201371,#201372,#201373,#201374,#201375,#201376,
#201377,#201378,#201379,#201380,#201381,#201382,#201383,#201384,#201385,
#201386,#201387,#201388,#201389,#201390,#201391,#201392,#201393,#201394,
#201395,#201396,#201397,#201398,#201399,#201400,#201401,#201402,#201403,
#201404,#201405),.UNSPECIFIED.,.F.,.F.,(4,3,3,3,3,3,3,3,3,3,3,3,3,3,3,3,
3,3,3,3,3,3,3,3,3,3,4),(208.440825084745,208.518399650002,208.59590129923,
208.673333362129,208.750725044706,208.828090323961,208.8661306806,208.94962290132,
209.033271904583,209.117159536426,209.201161180865,209.285349323853,209.365500548531,
209.442998277957,209.520413980288,209.597763284783,209.675061773056,209.752324989785,
209.829581387185,209.906836924305,209.984105648153,210.061401610526,210.138785595401,
210.21621517883,210.293764888572,210.364240284394,210.486707790517),
 .UNSPECIFIED.);
#3396=B_SPLINE_CURVE_WITH_KNOTS('',3,(#201406,#201407,#201408,#201409,#201410,
#201411,#201412,#201413,#201414,#201415,#201416,#201417,#201418,#201419,
#201420,#201421,#201422,#201423,#201424,#201425,#201426,#201427,#201428,
#201429,#201430,#201431,#201432,#201433,#201434,#201435,#201436,#201437,
#201438,#201439,#201440,#201441,#201442,#201443,#201444,#201445,#201446,
#201447,#201448,#201449,#201450,#201451,#201452,#201453,#201454,#201455,
#201456,#201457,#201458,#201459,#201460,#201461,#201462,#201463,#201464,
#201465,#201466,#201467,#201468,#201469,#201470,#201471,#201472,#201473,
#201474,#201475,#201476,#201477,#201478,#201479,#201480,#201481,#201482,
#201483,#201484,#201485,#201486,#201487,#201488,#201489,#201490,#201491,
#201492,#201493,#201494,#201495,#201496,#201497,#201498,#201499,#201500,
#201501,#201502,#201503,#201504,#201505,#201506,#201507,#201508,#201509,
#201510,#201511,#201512,#201513,#201514,#201515,#201516,#201517,#201518,
#201519,#201520,#201521,#201522,#201523,#201524,#201525,#201526,#201527,
#201528,#201529,#201530,#201531,#201532,#201533,#201534,#201535,#201536,
#201537,#201538,#201539,#201540,#201541,#201542,#201543,#201544,#201545,
#201546,#201547,#201548,#201549,#201550,#201551,#201552,#201553,#201554,
#201555,#201556,#201557,#201558,#201559,#201560,#201561,#201562,#201563,
#201564,#201565,#201566,#201567,#201568,#201569,#201570,#201571,#201572,
#201573,#201574),.UNSPECIFIED.,.F.,.F.,(4,3,3,3,3,3,3,3,3,3,3,3,3,3,3,3,
3,3,3,3,3,3,3,3,3,3,3,3,3,3,3,3,3,3,3,3,3,3,3,3,3,3,3,3,3,3,3,3,3,3,3,3,
3,3,3,3,4),(210.486707790606,210.561591694908,210.636397075426,210.711141145154,
210.785841020379,210.86052438242,210.935201569189,211.009887983622,211.084599042084,
211.159395255186,211.234237161341,211.30919544728,211.362980020256,211.44151141379,
211.519950009753,211.598310322816,211.676606812219,211.754853891543,211.833069058421,
211.911267633218,211.989462620625,212.067667020809,212.145926536013,212.224214567682,
212.30258643611,212.361719756118,212.441377262482,212.520964287265,212.600491694128,
212.679961799299,212.759397492703,212.838808247335,212.861089624049,212.942310044341,
213.023579305909,213.107799352426,213.189220868669,213.274840180325,213.36045949198,
213.445640227046,213.530742457118,213.615694795245,213.70054100553,213.785196810594,
213.859829359911,213.936480639936,214.01312726593,214.089783766943,214.166496860638,
214.243241660399,214.320070344098,214.359199227842,214.438616377869,214.517958670035,
214.59725648799,214.67651754967,214.723306029336),.UNSPECIFIED.);
#3397=B_SPLINE_CURVE_WITH_KNOTS('',3,(#201580,#201581,#201582,#201583,#201584,
#201585,#201586,#201587,#201588,#201589,#201590,#201591,#201592,#201593,
#201594,#201595,#201596,#201597,#201598,#201599,#201600,#201601,#201602,
#201603,#201604,#201605,#201606,#201607,#201608,#201609,#201610,#201611,
#201612,#201613,#201614,#201615,#201616,#201617,#201618,#201619,#201620,
#201621,#201622,#201623,#201624,#201625,#201626,#201627,#201628,#201629,
#201630,#201631,#201632,#201633,#201634,#201635,#201636,#201637,#201638,
#201639,#201640,#201641,#201642,#201643,#201644,#201645,#201646,#201647,
#201648,#201649,#201650,#201651,#201652,#201653,#201654,#201655,#201656,
#201657,#201658,#201659,#201660,#201661,#201662,#201663,#201664,#201665,
#201666,#201667,#201668,#201669,#201670,#201671,#201672,#201673,#201674,
#201675,#201676,#201677,#201678,#201679,#201680,#201681,#201682,#201683,
#201684,#201685,#201686,#201687,#201688,#201689,#201690,#201691,#201692,
#201693,#201694,#201695,#201696,#201697,#201698,#201699,#201700,#201701,
#201702,#201703,#201704,#201705,#201706,#201707,#201708,#201709,#201710,
#201711,#201712,#201713,#201714,#201715,#201716,#201717,#201718,#201719,
#201720,#201721,#201722,#201723,#201724,#201725,#201726,#201727,#201728,
#201729,#201730,#201731,#201732,#201733,#201734,#201735,#201736),
 .UNSPECIFIED.,.F.,.F.,(4,3,3,3,3,3,3,3,3,3,3,3,3,3,3,3,3,3,3,3,3,3,3,3,
3,3,3,3,3,3,3,3,3,3,3,3,3,3,3,3,3,3,3,3,3,3,3,3,3,3,3,3,4),(216.769893097833,
216.852355303918,216.934817161707,217.017278678048,217.099739859792,217.182200713788,
217.264661246887,217.347121465937,217.429581377788,217.512040989287,217.594500307284,
217.676959338626,217.759418090161,217.841876568737,217.924334781202,218.006792734402,
218.089250435185,218.171707890397,218.254165106884,218.34017769467,218.423502389086,
218.505968994645,218.588434755995,218.670899700554,218.753363855732,218.835827248939,
218.918289907582,219.000751859066,219.083213130793,219.165673750161,219.248133744568,
219.330593141409,219.413051968078,219.495510251964,219.577968020457,219.660425300945,
219.744559214386,219.827025212685,219.909489589234,219.991952453676,220.074413915632,
220.156874084706,220.239333070481,220.321790982524,220.407388099209,220.489852836153,
220.572314608451,220.654773854542,220.737231012721,220.81969353162,220.902151202903,
220.984609993811,221.006567916007),.UNSPECIFIED.);
#3398=B_SPLINE_CURVE_WITH_KNOTS('',3,(#201737,#201738,#201739,#201740,#201741,
#201742,#201743,#201744,#201745,#201746,#201747,#201748,#201749,#201750,
#201751,#201752,#201753,#201754,#201755,#201756,#201757,#201758,#201759,
#201760,#201761,#201762,#201763,#201764,#201765,#201766,#201767,#201768,
#201769,#201770,#201771,#201772,#201773,#201774,#201775,#201776,#201777,
#201778,#201779,#201780,#201781,#201782,#201783,#201784,#201785,#201786,
#201787,#201788,#201789,#201790,#201791,#201792,#201793,#201794,#201795,
#201796,#201797,#201798,#201799,#201800,#201801,#201802,#201803,#201804,
#201805,#201806,#201807,#201808,#201809,#201810,#201811,#201812),
 .UNSPECIFIED.,.F.,.F.,(4,3,3,3,3,3,3,3,3,3,3,3,3,3,3,3,3,3,3,3,3,3,3,3,
3,4),(214.723382608827,214.805844212586,214.888305150465,214.970765449863,
215.053225138176,215.135684242798,215.218142791121,215.300600810535,215.383058328428,
215.469735501508,215.552202287116,215.634667400247,215.717130950554,215.799593047668,
215.8820538012,215.964513320742,216.04697171587,216.12942909614,216.21189548196,
216.294358683584,216.376819139532,216.459277288168,216.54174289218,216.624202770757,
216.706666882494,216.769893097696),.UNSPECIFIED.);
#3399=B_SPLINE_CURVE_WITH_KNOTS('',3,(#201814,#201815,#201816,#201817,#201818,
#201819,#201820,#201821,#201822,#201823,#201824,#201825,#201826,#201827,
#201828,#201829,#201830,#201831,#201832,#201833,#201834,#201835,#201836,
#201837,#201838,#201839,#201840,#201841,#201842,#201843,#201844,#201845,
#201846,#201847,#201848,#201849,#201850,#201851,#201852,#201853,#201854,
#201855,#201856,#201857,#201858,#201859,#201860,#201861,#201862,#201863,
#201864,#201865,#201866,#201867,#201868,#201869,#201870,#201871,#201872,
#201873,#201874,#201875,#201876,#201877,#201878,#201879,#201880,#201881,
#201882,#201883,#201884,#201885,#201886,#201887,#201888,#201889,#201890,
#201891,#201892),.UNSPECIFIED.,.F.,.F.,(4,3,3,3,3,3,3,3,3,3,3,3,3,3,3,3,
3,3,3,3,3,3,3,3,3,3,4),(214.723306029336,214.802635146132,214.881875088531,
214.961124965084,215.040396134553,215.119781841841,215.199161307098,215.278640892757,
215.357938963704,215.435976917764,215.513924367901,215.591794836693,215.669588534833,
215.747337684786,215.825052758298,215.857308831636,215.940275422997,216.023384773408,
216.10671977981,216.190163817788,216.273795292611,216.356678699567,216.439821239611,
216.522721408167,216.605477260346,216.688004917172,216.769893097696),
 .UNSPECIFIED.);
#3400=B_SPLINE_CURVE_WITH_KNOTS('',3,(#201893,#201894,#201895,#201896,#201897,
#201898,#201899,#201900,#201901,#201902,#201903,#201904,#201905,#201906,
#201907,#201908,#201909,#201910,#201911,#201912,#201913,#201914,#201915,
#201916,#201917,#201918,#201919,#201920,#201921,#201922,#201923,#201924,
#201925,#201926,#201927,#201928,#201929,#201930,#201931,#201932,#201933,
#201934,#201935,#201936,#201937,#201938,#201939,#201940,#201941,#201942,
#201943,#201944,#201945,#201946,#201947,#201948,#201949,#201950,#201951,
#201952,#201953,#201954,#201955,#201956,#201957,#201958,#201959,#201960,
#201961,#201962,#201963,#201964,#201965,#201966,#201967,#201968,#201969,
#201970,#201971,#201972,#201973,#201974,#201975,#201976,#201977,#201978,
#201979,#201980,#201981,#201982,#201983,#201984,#201985,#201986,#201987,
#201988,#201989,#201990,#201991,#201992,#201993,#201994,#201995,#201996,
#201997,#201998,#201999,#202000,#202001,#202002,#202003,#202004,#202005,
#202006,#202007,#202008,#202009,#202010,#202011,#202012,#202013,#202014,
#202015,#202016,#202017,#202018,#202019,#202020,#202021,#202022,#202023,
#202024,#202025,#202026,#202027,#202028,#202029,#202030,#202031,#202032,
#202033,#202034,#202035,#202036,#202037,#202038,#202039,#202040,#202041,
#202042,#202043,#202044,#202045,#202046,#202047,#202048,#202049),
 .UNSPECIFIED.,.F.,.F.,(4,3,3,3,3,3,3,3,3,3,3,3,3,3,3,3,3,3,3,3,3,3,3,3,
3,3,3,3,3,3,3,3,3,3,3,3,3,3,3,3,3,3,3,3,3,3,3,3,3,3,3,3,4),(216.769893097696,
216.852355303782,216.93481716157,217.017278677911,217.099739859655,217.182200713651,
217.26466124675,217.3471214658,217.429581377651,217.51204098915,217.594500307147,
217.676959338489,217.759418090024,217.8418765686,217.924334781065,218.006792734265,
218.089250435048,218.171707890259,218.254165106747,218.340177694536,218.423502388957,
218.505968994516,218.588434755866,218.670899700425,218.753363855603,218.83582724881,
218.918289907453,219.000751858937,219.083213130664,219.165673750032,219.248133744439,
219.330593141281,219.413051967949,219.495510251835,219.577968020329,219.660425300816,
219.744559214266,219.827025212564,219.909489589113,219.991952453555,220.074413915512,
220.156874084585,220.23933307036,220.321790982403,220.407388099104,220.489852836047,
220.572314608345,220.654773854437,220.737231012615,220.819693531514,220.902151202797,
220.984609993706,221.006567916007),.UNSPECIFIED.);
#3401=B_SPLINE_CURVE_WITH_KNOTS('',3,(#202055,#202056,#202057,#202058,#202059,
#202060,#202061,#202062,#202063,#202064,#202065,#202066,#202067,#202068,
#202069,#202070,#202071,#202072,#202073,#202074,#202075,#202076,#202077,
#202078,#202079,#202080,#202081,#202082,#202083,#202084,#202085,#202086,
#202087,#202088,#202089,#202090,#202091,#202092,#202093,#202094,#202095,
#202096,#202097,#202098,#202099,#202100,#202101,#202102,#202103,#202104,
#202105,#202106,#202107,#202108,#202109,#202110,#202111,#202112,#202113,
#202114,#202115,#202116,#202117,#202118,#202119,#202120,#202121,#202122,
#202123,#202124,#202125,#202126,#202127,#202128,#202129,#202130,#202131,
#202132,#202133,#202134,#202135,#202136,#202137,#202138,#202139,#202140,
#202141,#202142,#202143,#202144,#202145,#202146,#202147,#202148,#202149,
#202150,#202151,#202152,#202153,#202154,#202155,#202156,#202157,#202158,
#202159,#202160,#202161,#202162,#202163,#202164,#202165,#202166,#202167,
#202168,#202169,#202170,#202171,#202172,#202173,#202174,#202175,#202176,
#202177,#202178,#202179,#202180,#202181,#202182,#202183,#202184,#202185,
#202186,#202187,#202188,#202189,#202190,#202191,#202192,#202193,#202194,
#202195,#202196,#202197,#202198,#202199,#202200,#202201,#202202,#202203,
#202204,#202205,#202206,#202207,#202208,#202209,#202210,#202211),
 .UNSPECIFIED.,.F.,.F.,(4,3,3,3,3,3,3,3,3,3,3,3,3,3,3,3,3,3,3,3,3,3,3,3,
3,3,3,3,3,3,3,3,3,3,3,3,3,3,3,3,3,3,3,3,3,3,3,3,3,3,3,3,4),(223.053078404876,
223.135540610962,223.21800246875,223.300463985091,223.382925166835,223.465386020831,
223.54784655393,223.63030677298,223.712766684831,223.79522629633,223.877685614327,
223.960144645669,224.042603397204,224.125061875781,224.207520088245,224.289978041446,
224.372435742228,224.45489319744,224.537350413927,224.623363001717,224.706687696138,
224.789154301696,224.871620063047,224.954085007605,225.036549162783,225.11901255599,
225.201475214634,225.283937166118,225.366398437844,225.448859057212,225.531319051619,
225.613778448461,225.696237275129,225.778695559015,225.861153327509,225.943610607997,
226.027744521446,226.110210519744,226.192674896293,226.275137760735,226.357599222692,
226.440059391766,226.52251837754,226.604976289583,226.690573406284,226.773038143227,
226.855499915526,226.937959161617,227.020416319795,227.102878838694,227.185336509978,
227.267795300886,227.289753223187),.UNSPECIFIED.);
#3402=B_SPLINE_CURVE_WITH_KNOTS('',3,(#202212,#202213,#202214,#202215,#202216,
#202217,#202218,#202219,#202220,#202221,#202222,#202223,#202224,#202225,
#202226,#202227,#202228,#202229,#202230,#202231,#202232,#202233,#202234,
#202235,#202236,#202237,#202238,#202239,#202240,#202241,#202242,#202243,
#202244,#202245,#202246,#202247,#202248,#202249,#202250,#202251,#202252,
#202253,#202254,#202255,#202256,#202257,#202258,#202259,#202260,#202261,
#202262,#202263,#202264,#202265,#202266,#202267,#202268,#202269,#202270,
#202271,#202272,#202273,#202274,#202275,#202276,#202277,#202278,#202279,
#202280,#202281,#202282,#202283,#202284,#202285,#202286,#202287),
 .UNSPECIFIED.,.F.,.F.,(4,3,3,3,3,3,3,3,3,3,3,3,3,3,3,3,3,3,3,3,3,3,3,3,
3,4),(221.006567916007,221.089029519765,221.171490457645,221.253950757043,
221.336410445356,221.418869549978,221.501328098301,221.583786117715,221.666243635608,
221.752920808681,221.83538759429,221.917852707421,222.000316257728,222.082778354842,
222.165239108374,222.247698627916,222.330157023043,222.412614403314,222.495080789133,
222.577543990757,222.660004446706,222.742462595342,222.824928199354,222.907388077931,
222.989852189668,223.053078404776),.UNSPECIFIED.);
#3403=B_SPLINE_CURVE_WITH_KNOTS('',3,(#202289,#202290,#202291,#202292,#202293,
#202294,#202295,#202296,#202297,#202298,#202299,#202300,#202301,#202302,
#202303,#202304,#202305,#202306,#202307,#202308,#202309,#202310,#202311,
#202312,#202313,#202314,#202315,#202316,#202317,#202318,#202319,#202320,
#202321,#202322,#202323,#202324,#202325,#202326,#202327,#202328,#202329,
#202330,#202331,#202332,#202333,#202334,#202335,#202336,#202337,#202338,
#202339,#202340,#202341,#202342,#202343,#202344,#202345,#202346,#202347,
#202348,#202349,#202350,#202351,#202352,#202353,#202354,#202355,#202356,
#202357,#202358,#202359,#202360,#202361,#202362,#202363,#202364),
 .UNSPECIFIED.,.F.,.F.,(4,3,3,3,3,3,3,3,3,3,3,3,3,3,3,3,3,3,3,3,3,3,3,3,
3,4),(221.006567916007,221.089029519765,221.171490457645,221.253950757043,
221.336410445356,221.418869549978,221.501328098301,221.583786117715,221.666243635608,
221.752920808687,221.835387594296,221.917852707427,222.000316257734,222.082778354848,
222.16523910838,222.247698627922,222.330157023049,222.41261440332,222.49508078914,
222.577543990764,222.660004446712,222.742462595349,222.82492819936,222.907388077938,
222.989852189674,223.053078404876),.UNSPECIFIED.);
#3404=B_SPLINE_CURVE_WITH_KNOTS('',3,(#202365,#202366,#202367,#202368,#202369,
#202370,#202371,#202372,#202373,#202374,#202375,#202376,#202377,#202378,
#202379,#202380,#202381,#202382,#202383,#202384,#202385,#202386,#202387,
#202388,#202389,#202390,#202391,#202392,#202393,#202394,#202395,#202396,
#202397,#202398,#202399,#202400,#202401,#202402,#202403,#202404,#202405,
#202406,#202407,#202408,#202409,#202410,#202411,#202412,#202413,#202414,
#202415,#202416,#202417,#202418,#202419,#202420,#202421,#202422,#202423,
#202424,#202425,#202426,#202427,#202428,#202429,#202430,#202431,#202432,
#202433,#202434,#202435,#202436,#202437,#202438,#202439,#202440,#202441,
#202442,#202443,#202444,#202445,#202446,#202447,#202448,#202449,#202450,
#202451,#202452,#202453,#202454,#202455,#202456,#202457,#202458,#202459,
#202460,#202461,#202462,#202463,#202464,#202465,#202466,#202467,#202468,
#202469,#202470,#202471,#202472,#202473,#202474,#202475,#202476,#202477,
#202478,#202479,#202480,#202481,#202482,#202483,#202484,#202485,#202486,
#202487,#202488,#202489,#202490,#202491,#202492,#202493,#202494,#202495,
#202496,#202497,#202498,#202499,#202500,#202501,#202502,#202503,#202504,
#202505,#202506,#202507,#202508,#202509,#202510,#202511,#202512,#202513,
#202514,#202515,#202516,#202517,#202518,#202519,#202520,#202521,#202522,
#202523,#202524,#202525,#202526,#202527,#202528,#202529,#202530,#202531,
#202532,#202533),.UNSPECIFIED.,.F.,.F.,(4,3,3,3,3,3,3,3,3,3,3,3,3,3,3,3,
3,3,3,3,3,3,3,3,3,3,3,3,3,3,3,3,3,3,3,3,3,3,3,3,3,3,3,3,3,3,3,3,3,3,3,3,
3,3,3,3,4),(223.053078404876,223.146044225602,223.239870824975,223.334650264296,
223.347856850602,223.425228790324,223.50250728684,223.57970819008,223.656847293021,
223.733940343337,223.811010726514,223.88807060416,223.965134183421,224.042215670963,
224.11937156828,224.196565293471,224.27386814163,224.346596586464,224.430258111719,
224.513792070736,224.597126498715,224.680337882208,224.763350731037,224.845966454395,
224.923687048301,225.001432708213,225.079216808168,225.157095805485,225.235029123069,
225.313073998632,225.345336322326,225.424826154287,225.504240563609,225.583592175005,
225.662893565209,225.742157272041,225.821401806291,225.900636566179,225.97987290514,
226.059122176085,226.138425714033,226.217757875254,226.297165193625,226.344076058189,
226.420902169192,226.497660888859,226.574366832784,226.651035335283,226.727681881201,
226.804331550368,226.84344592612,226.928048974059,227.012797780636,227.097735349666,
227.182762072976,227.267898039824,227.289635416186),.UNSPECIFIED.);
#3405=B_SPLINE_CURVE_WITH_KNOTS('',3,(#202539,#202540,#202541,#202542,#202543,
#202544,#202545,#202546,#202547,#202548,#202549,#202550,#202551,#202552,
#202553,#202554,#202555,#202556,#202557,#202558,#202559,#202560,#202561,
#202562,#202563,#202564,#202565,#202566,#202567,#202568,#202569,#202570,
#202571,#202572,#202573,#202574,#202575,#202576,#202577,#202578,#202579,
#202580,#202581,#202582,#202583,#202584,#202585,#202586,#202587,#202588,
#202589,#202590,#202591,#202592,#202593,#202594,#202595,#202596,#202597,
#202598,#202599,#202600,#202601,#202602,#202603,#202604,#202605,#202606,
#202607,#202608,#202609,#202610,#202611,#202612,#202613,#202614,#202615,
#202616,#202617,#202618,#202619,#202620,#202621,#202622,#202623,#202624,
#202625,#202626,#202627,#202628,#202629,#202630,#202631,#202632,#202633,
#202634,#202635,#202636,#202637,#202638,#202639,#202640,#202641,#202642,
#202643,#202644,#202645,#202646,#202647,#202648,#202649,#202650,#202651,
#202652,#202653,#202654,#202655,#202656,#202657,#202658,#202659,#202660,
#202661,#202662,#202663,#202664,#202665,#202666,#202667,#202668,#202669,
#202670,#202671,#202672,#202673,#202674,#202675,#202676,#202677,#202678,
#202679,#202680,#202681,#202682,#202683,#202684,#202685,#202686,#202687,
#202688,#202689,#202690,#202691,#202692,#202693,#202694,#202695),
 .UNSPECIFIED.,.F.,.F.,(4,3,3,3,3,3,3,3,3,3,3,3,3,3,3,3,3,3,3,3,3,3,3,3,
3,3,3,3,3,3,3,3,3,3,3,3,3,3,3,3,3,3,3,3,3,3,3,3,3,3,3,3,4),(229.336263712056,
229.418725918142,229.50118777593,229.583649292271,229.666110474015,229.748571328011,
229.83103186111,229.91349208016,229.995951992011,230.07841160351,230.160870921507,
230.243329952849,230.325788704384,230.40824718296,230.490705395425,230.573163348626,
230.655621049408,230.73807850462,230.820535721107,230.906548308897,230.989873003318,
231.072339608876,231.154805370227,231.237270314785,231.319734469963,231.40219786317,
231.484660521814,231.567122473298,231.649583745024,231.732044364392,231.814504358799,
231.896963755641,231.979422582309,232.061880866195,232.144338634689,232.226795915176,
232.310929828626,232.393395826924,232.475860203473,232.558323067915,232.640784529872,
232.723244698946,232.80570368472,232.888161596763,232.973758713464,233.056223450407,
233.138685222705,233.221144468796,233.303601626975,233.386064145874,233.468521817157,
233.550980608065,233.572938530366),.UNSPECIFIED.);
#3406=B_SPLINE_CURVE_WITH_KNOTS('',3,(#202696,#202697,#202698,#202699,#202700,
#202701,#202702,#202703,#202704,#202705,#202706,#202707,#202708,#202709,
#202710,#202711,#202712,#202713,#202714,#202715,#202716,#202717,#202718,
#202719,#202720,#202721,#202722,#202723,#202724,#202725,#202726,#202727,
#202728,#202729,#202730,#202731,#202732,#202733,#202734,#202735,#202736,
#202737,#202738,#202739,#202740,#202741,#202742,#202743,#202744,#202745,
#202746,#202747,#202748,#202749,#202750,#202751,#202752,#202753,#202754,
#202755,#202756,#202757,#202758,#202759,#202760,#202761,#202762,#202763,
#202764,#202765,#202766,#202767,#202768,#202769,#202770,#202771),
 .UNSPECIFIED.,.F.,.F.,(4,3,3,3,3,3,3,3,3,3,3,3,3,3,3,3,3,3,3,3,3,3,3,3,
3,4),(227.289753223187,227.372214826945,227.454675764825,227.537136064223,
227.619595752536,227.702054857158,227.784513405481,227.866971424895,227.949428942788,
228.036106115859,228.118572901467,228.201038014598,228.283501564905,228.365963662019,
228.448424415551,228.530883935093,228.61334233022,228.695799710491,228.778266096311,
228.860729297935,228.943189753883,229.025647902519,229.108113506531,229.190573385109,
229.273037496845,229.336263711915),.UNSPECIFIED.);
#3407=B_SPLINE_CURVE_WITH_KNOTS('',3,(#202773,#202774,#202775,#202776,#202777,
#202778,#202779,#202780,#202781,#202782,#202783,#202784,#202785,#202786,
#202787,#202788,#202789,#202790,#202791,#202792,#202793,#202794,#202795,
#202796,#202797,#202798,#202799,#202800,#202801,#202802,#202803,#202804,
#202805,#202806,#202807,#202808,#202809,#202810,#202811,#202812,#202813,
#202814,#202815,#202816,#202817,#202818,#202819,#202820,#202821,#202822,
#202823,#202824,#202825,#202826,#202827,#202828,#202829,#202830,#202831,
#202832,#202833,#202834,#202835,#202836,#202837,#202838,#202839,#202840,
#202841,#202842,#202843,#202844,#202845,#202846,#202847,#202848,#202849,
#202850,#202851,#202852,#202853,#202854),.UNSPECIFIED.,.F.,.F.,(4,3,3,3,
3,3,3,3,3,3,3,3,3,3,3,3,3,3,3,3,3,3,3,3,3,3,3,4),(227.289635416186,227.342815794051,
227.424363071555,227.505834823778,227.589922533329,227.671238744506,227.756712203244,
227.842185661982,227.92160317053,228.001039463831,228.0805052851,228.160044679029,
228.239626033312,228.319291542762,228.341555529913,228.419862015423,228.498101914488,
228.576289748601,228.654440001667,228.732567129521,228.810702261164,228.888845478722,
228.967009877278,229.045208561738,229.123500253565,229.201842044087,229.280300540696,
229.336263712055),.UNSPECIFIED.);
#3408=B_SPLINE_CURVE_WITH_KNOTS('',3,(#202855,#202856,#202857,#202858,#202859,
#202860,#202861,#202862,#202863,#202864,#202865,#202866,#202867,#202868,
#202869,#202870,#202871,#202872,#202873,#202874,#202875,#202876,#202877,
#202878,#202879,#202880,#202881,#202882,#202883,#202884,#202885,#202886,
#202887,#202888,#202889,#202890,#202891,#202892,#202893,#202894,#202895,
#202896,#202897,#202898,#202899,#202900,#202901,#202902,#202903,#202904,
#202905,#202906,#202907,#202908,#202909,#202910,#202911,#202912,#202913,
#202914,#202915,#202916,#202917,#202918,#202919,#202920,#202921,#202922,
#202923,#202924,#202925,#202926,#202927,#202928,#202929,#202930,#202931,
#202932,#202933,#202934,#202935,#202936,#202937,#202938,#202939,#202940,
#202941,#202942,#202943,#202944,#202945,#202946,#202947,#202948,#202949,
#202950,#202951,#202952,#202953,#202954,#202955,#202956,#202957,#202958,
#202959,#202960,#202961,#202962,#202963,#202964,#202965,#202966,#202967,
#202968,#202969,#202970,#202971,#202972,#202973,#202974,#202975,#202976,
#202977,#202978,#202979,#202980,#202981,#202982,#202983,#202984,#202985,
#202986,#202987,#202988,#202989,#202990,#202991,#202992,#202993,#202994,
#202995,#202996,#202997,#202998,#202999,#203000,#203001,#203002,#203003,
#203004,#203005,#203006,#203007,#203008,#203009,#203010,#203011,#203012,
#203013,#203014,#203015,#203016,#203017,#203018,#203019,#203020,#203021,
#203022,#203023,#203024,#203025,#203026,#203027,#203028,#203029),
 .UNSPECIFIED.,.F.,.F.,(4,3,3,3,3,3,3,3,3,3,3,3,3,3,3,3,3,3,3,3,3,3,3,3,
3,3,3,3,3,3,3,3,3,3,3,3,3,3,3,3,3,3,3,3,3,3,3,3,3,3,3,3,3,3,3,3,3,3,4),
(229.336263712185,229.340295265775,229.416353221658,229.492315499975,229.568198891192,
229.644020104713,229.719795787656,229.797200689403,229.872949950271,229.948706465713,
230.024485245331,230.103122684408,230.179033385957,230.255000894413,230.331074602357,
230.339035001637,230.416594219665,230.494061133937,230.571451411116,230.648780662822,
230.726064456727,230.803325886015,230.880576971315,230.957831759866,231.035104298339,
231.112450023129,231.189833183896,231.267323063712,231.337774737499,231.421991210269,
231.506081087413,231.589964966738,231.673719256124,231.757258365679,231.837144605431,
231.914513048451,231.991899904669,232.069318971392,232.14682519985,232.224381119235,
232.302043799002,232.336514473362,232.416134948255,232.4956825069,232.575169462654,
232.654608082181,232.73401059438,232.813395523447,232.892771468578,232.972149511684,
233.051540734651,233.130985683765,233.210458979456,233.290005809806,233.335254209224,
233.411970858466,233.492647251187,233.569241113093,233.573323643909),
 .UNSPECIFIED.);
#3409=B_SPLINE_CURVE_WITH_KNOTS('',3,(#203035,#203036,#203037,#203038,#203039,
#203040,#203041,#203042,#203043,#203044,#203045,#203046,#203047,#203048,
#203049,#203050,#203051,#203052,#203053,#203054,#203055,#203056,#203057,
#203058,#203059,#203060,#203061,#203062,#203063,#203064,#203065,#203066,
#203067,#203068,#203069,#203070,#203071,#203072,#203073,#203074,#203075,
#203076,#203077,#203078,#203079,#203080,#203081,#203082,#203083,#203084,
#203085,#203086,#203087,#203088,#203089,#203090,#203091,#203092,#203093,
#203094,#203095,#203096,#203097,#203098,#203099,#203100,#203101,#203102,
#203103,#203104,#203105,#203106,#203107,#203108,#203109,#203110,#203111,
#203112,#203113,#203114,#203115,#203116,#203117,#203118,#203119,#203120,
#203121,#203122,#203123,#203124,#203125,#203126,#203127,#203128,#203129,
#203130,#203131,#203132,#203133,#203134,#203135,#203136,#203137,#203138,
#203139,#203140,#203141,#203142,#203143,#203144,#203145,#203146,#203147,
#203148,#203149,#203150,#203151,#203152,#203153,#203154,#203155,#203156,
#203157,#203158,#203159,#203160,#203161,#203162,#203163,#203164,#203165,
#203166,#203167,#203168,#203169,#203170,#203171,#203172,#203173,#203174,
#203175,#203176,#203177,#203178,#203179,#203180,#203181,#203182,#203183,
#203184,#203185,#203186,#203187,#203188,#203189,#203190,#203191,#203192,
#203193,#203194,#203195,#203196,#203197,#203198,#203199,#203200),
 .UNSPECIFIED.,.F.,.F.,(4,3,3,3,3,3,3,3,3,3,3,3,3,3,3,3,3,3,3,3,3,3,3,3,
3,3,3,3,3,3,3,3,3,3,3,3,3,3,3,3,3,3,3,3,3,3,3,3,3,3,3,3,3,3,3,4),(235.619449019235,
235.699335060132,235.779370913976,235.859484258981,235.939758663195,236.013789031205,
236.093409769729,236.172957597161,236.252444826208,236.33188372289,236.411286515463,
236.490671728125,236.57004795844,236.649426287752,236.728817797384,236.808263031978,
236.887736612522,236.967283724338,237.012528767067,237.089243773325,237.165891685097,
237.242487196245,237.319046093354,237.395583476844,237.47212499671,237.511898634998,
237.596574974064,237.681397459474,237.766419831286,237.851528714047,237.936758254381,
238.011268502929,238.092824765124,238.174305704323,238.258388870958,238.339714623005,
238.425176496933,238.51063837086,238.590041711906,238.669463483232,238.74891446104,
238.82843862743,238.908004538146,238.987654386521,239.010008238791,239.088392843705,
239.166709649306,239.244973074348,239.323198686606,239.401404021146,239.479602079275,
239.55780585563,239.636059705318,239.714338858029,239.792698452621,239.855869977774),
 .UNSPECIFIED.);
#3410=B_SPLINE_CURVE_WITH_KNOTS('',3,(#203201,#203202,#203203,#203204,#203205,
#203206,#203207,#203208,#203209,#203210,#203211,#203212,#203213,#203214,
#203215,#203216,#203217,#203218,#203219,#203220,#203221,#203222,#203223,
#203224,#203225,#203226,#203227,#203228,#203229,#203230,#203231,#203232,
#203233,#203234,#203235,#203236,#203237,#203238,#203239,#203240,#203241,
#203242,#203243,#203244,#203245,#203246,#203247,#203248,#203249,#203250,
#203251,#203252,#203253,#203254,#203255,#203256,#203257,#203258,#203259,
#203260,#203261,#203262,#203263,#203264,#203265,#203266,#203267,#203268,
#203269,#203270,#203271,#203272,#203273,#203274,#203275,#203276),
 .UNSPECIFIED.,.F.,.F.,(4,3,3,3,3,3,3,3,3,3,3,3,3,3,3,3,3,3,3,3,3,3,3,3,
3,4),(233.572938530366,233.655400134125,233.737861072004,233.820321371402,
233.902781059715,233.985240164337,234.06769871266,234.150156732074,234.232614249967,
234.319291423047,234.401758208655,234.484223321786,234.566686872093,234.649148969207,
234.731609722739,234.814069242281,234.896527637408,234.978985017679,235.061451403499,
235.143914605123,235.226375061071,235.308833209708,235.391298813719,235.473758692297,
235.556222804033,235.619449019235),.UNSPECIFIED.);
#3411=B_SPLINE_CURVE_WITH_KNOTS('',3,(#203278,#203279,#203280,#203281,#203282,
#203283,#203284,#203285,#203286,#203287,#203288,#203289,#203290,#203291,
#203292,#203293,#203294,#203295,#203296,#203297,#203298,#203299,#203300,
#203301,#203302,#203303,#203304,#203305,#203306,#203307,#203308,#203309,
#203310,#203311,#203312,#203313,#203314,#203315,#203316,#203317,#203318,
#203319,#203320,#203321,#203322,#203323,#203324,#203325,#203326,#203327,
#203328,#203329,#203330,#203331,#203332,#203333,#203334,#203335,#203336,
#203337,#203338,#203339,#203340,#203341,#203342,#203343,#203344,#203345,
#203346,#203347,#203348,#203349,#203350,#203351,#203352,#203353,#203354,
#203355,#203356,#203357,#203358,#203359),.UNSPECIFIED.,.F.,.F.,(4,3,3,3,
3,3,3,3,3,3,3,3,3,3,3,3,3,3,3,3,3,3,3,3,3,3,3,4),(233.573323643909,233.649879644271,
233.726415517639,233.802955814209,233.834624077155,233.919300567095,234.004123210958,
234.08914574956,234.174254802649,234.259484515824,234.333993945086,234.415550063061,
234.497030857161,234.581114096125,234.662439703222,234.74790175812,234.833363813017,
234.912767221105,234.992189060828,235.071640108233,235.15116434557,235.230730327984,
235.310380248706,235.332733680948,235.424797298135,235.516554834754,235.607711152124,
235.619449019114),.UNSPECIFIED.);
#3412=B_SPLINE_CURVE_WITH_KNOTS('',3,(#203360,#203361,#203362,#203363,#203364,
#203365,#203366,#203367,#203368,#203369,#203370,#203371,#203372,#203373,
#203374,#203375,#203376,#203377,#203378,#203379,#203380,#203381,#203382,
#203383,#203384,#203385,#203386,#203387,#203388,#203389,#203390,#203391,
#203392,#203393,#203394,#203395,#203396,#203397,#203398,#203399,#203400,
#203401,#203402,#203403,#203404,#203405,#203406,#203407,#203408,#203409,
#203410,#203411,#203412,#203413,#203414,#203415,#203416,#203417,#203418,
#203419,#203420,#203421,#203422,#203423,#203424,#203425,#203426,#203427,
#203428,#203429,#203430,#203431,#203432,#203433,#203434,#203435,#203436,
#203437,#203438,#203439,#203440,#203441,#203442,#203443,#203444,#203445,
#203446,#203447,#203448,#203449,#203450,#203451,#203452,#203453,#203454,
#203455,#203456,#203457,#203458,#203459,#203460,#203461,#203462,#203463,
#203464,#203465,#203466,#203467,#203468,#203469,#203470,#203471,#203472,
#203473,#203474,#203475,#203476,#203477,#203478,#203479,#203480,#203481,
#203482,#203483,#203484,#203485,#203486,#203487,#203488,#203489,#203490,
#203491,#203492,#203493,#203494,#203495,#203496,#203497,#203498,#203499,
#203500,#203501,#203502,#203503,#203504,#203505,#203506,#203507,#203508,
#203509,#203510,#203511,#203512,#203513,#203514,#203515,#203516,#203517,
#203518,#203519,#203520,#203521,#203522,#203523,#203524,#203525,#203526,
#203527,#203528),.UNSPECIFIED.,.F.,.F.,(4,3,3,3,3,3,3,3,3,3,3,3,3,3,3,3,
3,3,3,3,3,3,3,3,3,3,3,3,3,3,3,3,3,3,3,3,3,3,3,3,3,3,3,3,3,3,3,3,3,3,3,3,
3,3,3,3,4),(235.619449019235,235.697894778131,235.777092107966,235.855561918656,
235.934054701829,236.012583029286,236.092305626167,236.170984086526,236.251228751668,
236.33147341681,236.407529924543,236.483490743517,236.559372665115,236.635192399599,
236.710966594905,236.788372414626,236.864120171709,236.9398751782,237.01565244439,
237.09429262146,237.170201808871,237.24616780175,237.322240000284,237.330213152673,
237.407772006574,237.485238552846,237.562628458535,237.639957335639,237.717240752206,
237.794501801216,237.871752504505,237.949006909641,238.026279063626,238.10362440421,
238.18100718038,238.258496678449,238.328952888535,238.41317216454,238.497264836661,
238.581151455782,238.664908438605,238.748450134982,238.828322756466,238.905689954775,
238.983075546777,239.060493331147,239.13799825538,239.215552857275,239.29321420689,
239.327692624397,239.407311064205,239.486859579851,239.566349380978,239.645784629109,
239.725186637447,239.804569105013,239.856287383305),.UNSPECIFIED.);
#3413=B_SPLINE_CURVE_WITH_KNOTS('',3,(#203534,#203535,#203536,#203537,#203538,
#203539,#203540,#203541,#203542,#203543,#203544,#203545,#203546,#203547,
#203548,#203549,#203550,#203551,#203552,#203553,#203554,#203555,#203556,
#203557,#203558,#203559,#203560,#203561,#203562,#203563,#203564,#203565,
#203566,#203567,#203568,#203569,#203570,#203571,#203572,#203573,#203574,
#203575,#203576,#203577,#203578,#203579,#203580,#203581,#203582,#203583,
#203584,#203585,#203586,#203587,#203588,#203589,#203590,#203591,#203592,
#203593,#203594,#203595,#203596,#203597,#203598,#203599,#203600,#203601,
#203602,#203603,#203604,#203605,#203606,#203607,#203608,#203609,#203610,
#203611,#203612,#203613,#203614,#203615,#203616,#203617,#203618,#203619,
#203620,#203621,#203622,#203623,#203624,#203625,#203626,#203627,#203628,
#203629,#203630,#203631,#203632,#203633,#203634,#203635,#203636,#203637,
#203638,#203639,#203640,#203641,#203642,#203643,#203644,#203645,#203646,
#203647,#203648,#203649,#203650,#203651,#203652,#203653,#203654,#203655,
#203656,#203657,#203658,#203659,#203660,#203661,#203662,#203663,#203664,
#203665,#203666,#203667,#203668,#203669,#203670,#203671,#203672,#203673,
#203674,#203675,#203676,#203677,#203678,#203679,#203680,#203681,#203682,
#203683,#203684,#203685,#203686,#203687,#203688,#203689,#203690,#203691,
#203692,#203693,#203694,#203695,#203696,#203697,#203698,#203699),
 .UNSPECIFIED.,.F.,.F.,(4,3,3,3,3,3,3,3,3,3,3,3,3,3,3,3,3,3,3,3,3,3,3,3,
3,3,3,3,3,3,3,3,3,3,3,3,3,3,3,3,3,3,3,3,3,3,3,3,3,3,3,3,3,3,3,4),(241.902634326415,
242.006227446378,242.090446729262,242.174539408226,242.258426034031,242.342183023408,
242.425724726058,242.505597314309,242.582964510105,242.660350099558,242.737767881348,
242.815272802963,242.892827402217,242.970488749172,243.00496718224,243.084587920985,
243.164135748642,243.243622977918,243.323061874832,243.402464667639,243.481849880538,
243.561226111091,243.640604440643,243.719995950514,243.799441185346,243.878914766127,
243.958461878178,244.003706918102,244.080421924948,244.15706983731,244.233665349047,
244.310224246743,244.38676163082,244.46330315127,244.503076786033,244.587753124243,
244.67257560876,244.757597979638,244.84270686145,244.927936400827,245.002446653964,
245.084002916623,245.165483856288,245.24956702269,245.330892775201,245.416354648549,
245.501816521896,245.581219862781,245.660641633943,245.740092611585,245.819616777805,
245.899182688351,245.978832536554,246.001186389827,246.079561984822,246.139559773273),
 .UNSPECIFIED.);
#3414=B_SPLINE_CURVE_WITH_KNOTS('',3,(#203700,#203701,#203702,#203703,#203704,
#203705,#203706,#203707,#203708,#203709,#203710,#203711,#203712,#203713,
#203714,#203715,#203716,#203717,#203718,#203719,#203720,#203721,#203722,
#203723,#203724,#203725,#203726,#203727,#203728,#203729,#203730,#203731,
#203732,#203733,#203734,#203735,#203736,#203737,#203738,#203739,#203740,
#203741,#203742,#203743,#203744,#203745,#203746,#203747,#203748,#203749,
#203750,#203751,#203752,#203753,#203754,#203755,#203756,#203757,#203758,
#203759,#203760,#203761,#203762,#203763,#203764,#203765,#203766,#203767,
#203768,#203769,#203770,#203771,#203772,#203773,#203774,#203775,#203776,
#203777,#203778,#203779,#203780,#203781,#203782,#203783,#203784),
 .UNSPECIFIED.,.F.,.F.,(4,3,3,3,3,3,3,3,3,3,3,3,3,3,3,3,3,3,3,3,3,3,3,3,
3,3,3,3,4),(239.855869977774,239.934394266809,240.008747974654,240.084804481403,
240.160765299393,240.236647220008,240.31246695351,240.388241147837,240.465646968172,
240.541394724282,240.617149729805,240.692926995031,240.771567173902,240.847476360366,
240.923442352304,240.999514549909,241.007487710516,241.084375069617,241.161170469761,
241.23789018103,241.314550412522,241.391167984801,241.467763329302,241.5443510339,
241.620945679481,241.697594875386,241.774273250137,241.851037515127,241.902634326295),
 .UNSPECIFIED.);
#3415=B_SPLINE_CURVE_WITH_KNOTS('',3,(#203786,#203787,#203788,#203789,#203790,
#203791,#203792,#203793,#203794,#203795,#203796,#203797,#203798,#203799,
#203800,#203801,#203802,#203803,#203804,#203805,#203806,#203807,#203808,
#203809,#203810,#203811,#203812,#203813,#203814,#203815,#203816,#203817,
#203818,#203819,#203820,#203821,#203822,#203823,#203824,#203825,#203826,
#203827,#203828,#203829,#203830,#203831,#203832,#203833,#203834,#203835,
#203836,#203837,#203838,#203839,#203840,#203841,#203842,#203843,#203844,
#203845,#203846,#203847,#203848,#203849,#203850,#203851,#203852,#203853,
#203854,#203855,#203856,#203857,#203858,#203859,#203860,#203861,#203862,
#203863,#203864),.UNSPECIFIED.,.F.,.F.,(4,3,3,3,3,3,3,3,3,3,3,3,3,3,3,3,
3,3,3,3,3,3,3,3,3,3,4),(239.856287383305,239.935663723181,240.015049380833,
240.094487130204,240.173949680295,240.25349100907,240.326432360259,240.403147366517,
240.479795278289,240.556390789437,240.632949686546,240.709487070035,240.786028589902,
240.82580222819,240.910478567256,240.995301052666,241.080323424478,241.165432307238,
241.250661847573,241.325172096121,241.406728358316,241.488209297516,241.57229246415,
241.653618216198,241.739080090125,241.824541964052,241.902634326414),
 .UNSPECIFIED.);
#3416=B_SPLINE_CURVE_WITH_KNOTS('',3,(#203865,#203866,#203867,#203868,#203869,
#203870,#203871,#203872,#203873,#203874,#203875,#203876,#203877,#203878,
#203879,#203880,#203881,#203882,#203883,#203884,#203885,#203886,#203887,
#203888,#203889,#203890,#203891,#203892,#203893,#203894,#203895,#203896,
#203897,#203898,#203899,#203900,#203901,#203902,#203903,#203904,#203905,
#203906,#203907,#203908,#203909,#203910,#203911,#203912,#203913,#203914,
#203915,#203916,#203917,#203918,#203919,#203920,#203921,#203922,#203923,
#203924,#203925,#203926,#203927,#203928,#203929,#203930,#203931,#203932,
#203933,#203934,#203935,#203936,#203937,#203938,#203939,#203940,#203941,
#203942,#203943,#203944,#203945,#203946,#203947,#203948,#203949,#203950,
#203951,#203952,#203953,#203954,#203955,#203956,#203957,#203958,#203959,
#203960,#203961,#203962,#203963,#203964,#203965,#203966,#203967,#203968,
#203969,#203970,#203971,#203972,#203973,#203974,#203975,#203976,#203977,
#203978,#203979,#203980,#203981,#203982,#203983,#203984,#203985,#203986,
#203987,#203988,#203989,#203990,#203991,#203992,#203993,#203994,#203995,
#203996,#203997,#203998,#203999,#204000,#204001,#204002,#204003,#204004,
#204005,#204006,#204007,#204008,#204009,#204010,#204011,#204012,#204013,
#204014,#204015,#204016,#204017,#204018,#204019,#204020,#204021,#204022,
#204023,#204024,#204025,#204026,#204027,#204028,#204029,#204030,#204031,
#204032,#204033),.UNSPECIFIED.,.F.,.F.,(4,3,3,3,3,3,3,3,3,3,3,3,3,3,3,3,
3,3,3,3,3,3,3,3,3,3,3,3,3,3,3,3,3,3,3,3,3,3,3,3,3,3,3,3,3,3,3,3,3,3,3,3,
3,3,3,3,4),(241.902634326536,241.983440650617,242.064301316456,242.145262351786,
242.226279264729,242.307391413021,242.323911831983,242.402290852836,242.480603604135,
242.558864500272,242.637087918053,242.715288206196,242.793496395342,242.871712448815,
242.949949366026,243.028220156162,243.106583735617,243.184996865057,243.263527247552,
243.322651567846,243.398708074595,243.474668892585,243.5505508132,243.626370546702,
243.702144741029,243.779550561364,243.855298317474,243.931053322997,244.006830588223,
244.085470767094,244.161379953558,244.237345945495,244.313418143101,244.321391303708,
244.39895015526,244.476416699161,244.55380660246,244.63113547716,244.708418891309,
244.785679937888,244.862930638738,244.94018504143,245.017457192969,245.094802531113,
245.172185304844,245.249674800498,245.32013103957,245.404350322454,245.488443001418,
245.572329627223,245.656086616601,245.739628319251,245.819500907501,245.899271539307,
245.976664252389,246.057623843556,246.138583434724),.UNSPECIFIED.);
#3417=B_SPLINE_CURVE_WITH_KNOTS('',3,(#204039,#204040,#204041,#204042,#204043,
#204044,#204045,#204046,#204047,#204048,#204049,#204050,#204051,#204052,
#204053,#204054,#204055,#204056,#204057,#204058,#204059,#204060,#204061,
#204062,#204063,#204064,#204065,#204066,#204067,#204068,#204069,#204070,
#204071,#204072,#204073,#204074,#204075,#204076,#204077,#204078,#204079,
#204080,#204081,#204082,#204083,#204084,#204085,#204086,#204087,#204088,
#204089,#204090,#204091,#204092,#204093,#204094,#204095,#204096,#204097,
#204098,#204099,#204100,#204101,#204102,#204103,#204104,#204105,#204106,
#204107,#204108,#204109,#204110,#204111,#204112,#204113,#204114,#204115,
#204116,#204117,#204118,#204119,#204120,#204121,#204122,#204123,#204124,
#204125,#204126,#204127,#204128,#204129,#204130,#204131,#204132,#204133,
#204134,#204135,#204136,#204137,#204138,#204139,#204140,#204141,#204142,
#204143,#204144,#204145,#204146,#204147,#204148,#204149,#204150,#204151,
#204152,#204153,#204154,#204155,#204156,#204157,#204158,#204159,#204160,
#204161,#204162,#204163,#204164,#204165,#204166,#204167,#204168,#204169,
#204170,#204171,#204172,#204173,#204174,#204175,#204176,#204177,#204178,
#204179,#204180,#204181,#204182,#204183,#204184,#204185,#204186,#204187,
#204188,#204189,#204190,#204191,#204192,#204193,#204194,#204195,#204196,
#204197,#204198,#204199,#204200,#204201,#204202,#204203,#204204,#204205,
#204206,#204207),.UNSPECIFIED.,.F.,.F.,(4,3,3,3,3,3,3,3,3,3,3,3,3,3,3,3,
3,3,3,3,3,3,3,3,3,3,3,3,3,3,3,3,3,3,3,3,3,3,3,3,3,3,3,3,3,3,3,3,3,3,3,3,
3,3,3,3,4),(248.185819633708,248.261585952686,248.337281052035,248.412921758733,
248.488529494103,248.564121002797,248.639711417477,248.715315869224,248.790988245108,
248.866696742503,248.942505670427,248.997405597413,249.081624880306,249.165717559279,
249.249604185092,249.333361174478,249.416902877136,249.496775465344,249.574142661138,
249.651528250589,249.728946032378,249.806450953991,249.884005553243,249.961666900196,
249.996145333275,250.075766072019,250.155313899675,250.234801128951,250.314240025864,
250.39364281867,250.473028031569,250.552404262121,250.631782591672,250.711174101543,
250.790619336374,250.870092917155,250.949640029205,250.994885069138,251.071600075987,
251.148247988351,251.224843500091,251.301402397789,251.377939781868,251.454481302321,
251.494254937069,251.578931275277,251.66375375979,251.748776130666,251.833885012474,
251.919114551848,251.993624805,252.075187818711,252.15667533995,252.238070811612,
252.319408121063,252.400678092138,252.422853579701),.UNSPECIFIED.);
#3418=B_SPLINE_CURVE_WITH_KNOTS('',3,(#204208,#204209,#204210,#204211,#204212,
#204213,#204214,#204215,#204216,#204217,#204218,#204219,#204220,#204221,
#204222,#204223,#204224,#204225,#204226,#204227,#204228,#204229,#204230,
#204231,#204232,#204233,#204234,#204235,#204236,#204237,#204238,#204239,
#204240,#204241,#204242,#204243,#204244,#204245,#204246,#204247,#204248,
#204249,#204250,#204251,#204252,#204253,#204254,#204255,#204256,#204257,
#204258,#204259,#204260,#204261,#204262,#204263,#204264,#204265,#204266,
#204267,#204268,#204269,#204270,#204271,#204272,#204273,#204274,#204275,
#204276,#204277,#204278,#204279,#204280,#204281,#204282,#204283,#204284,
#204285,#204286,#204287,#204288,#204289),.UNSPECIFIED.,.F.,.F.,(4,3,3,3,
3,3,3,3,3,3,3,3,3,3,3,3,3,3,3,3,3,3,3,3,3,3,3,4),(246.139559773273,246.217831512834,
246.296062413031,246.374266828305,246.452475053539,246.53068810268,246.608918973935,
246.687180673534,246.76553436775,246.843934857852,246.922457968968,246.999926125689,
247.075982632443,247.151943450437,247.227825371056,247.303645104563,247.379419298894,
247.456825119226,247.532572875341,247.608327880869,247.6841051461,247.762745324963,
247.838654511431,247.914620503374,247.990692700984,247.998665861551,248.133851106609,
248.185819633594),.UNSPECIFIED.);
#3419=B_SPLINE_CURVE_WITH_KNOTS('',3,(#204291,#204292,#204293,#204294,#204295,
#204296,#204297,#204298,#204299,#204300,#204301,#204302,#204303,#204304,
#204305,#204306,#204307,#204308,#204309,#204310,#204311,#204312,#204313,
#204314,#204315,#204316,#204317,#204318,#204319,#204320,#204321,#204322,
#204323,#204324,#204325,#204326,#204327,#204328,#204329,#204330,#204331,
#204332,#204333,#204334,#204335,#204336,#204337,#204338,#204339,#204340,
#204341,#204342,#204343,#204344,#204345,#204346,#204347,#204348,#204349,
#204350,#204351,#204352,#204353,#204354,#204355,#204356,#204357,#204358,
#204359,#204360,#204361,#204362,#204363,#204364,#204365,#204366,#204367,
#204368,#204369,#204370,#204371,#204372,#204373,#204374,#204375),
 .UNSPECIFIED.,.F.,.F.,(4,3,3,3,3,3,3,3,3,3,3,3,3,3,3,3,3,3,3,3,3,3,3,3,
3,3,3,3,4),(246.138583434724,246.216144908096,246.293810662186,246.318870775432,
246.398491514177,246.478039341834,246.55752657111,246.636965468024,246.716368260831,
246.79575347373,246.875129704283,246.954508033835,247.033899543706,247.113344778538,
247.192818359319,247.27236547137,247.317610511294,247.394325518141,247.470973430503,
247.547568942239,247.624127839936,247.700665224013,247.777206744463,247.816980379225,
247.899501894936,247.982178186873,248.064933619021,248.147813992888,248.185432795619),
 .UNSPECIFIED.);
#3420=B_SPLINE_CURVE_WITH_KNOTS('',3,(#204376,#204377,#204378,#204379,#204380,
#204381,#204382,#204383,#204384,#204385,#204386,#204387,#204388,#204389,
#204390,#204391,#204392,#204393,#204394,#204395,#204396,#204397,#204398,
#204399,#204400,#204401,#204402,#204403,#204404,#204405,#204406,#204407,
#204408,#204409,#204410,#204411,#204412,#204413,#204414,#204415,#204416,
#204417,#204418,#204419,#204420,#204421,#204422,#204423,#204424,#204425,
#204426,#204427,#204428,#204429,#204430,#204431,#204432,#204433,#204434,
#204435,#204436,#204437,#204438,#204439,#204440,#204441,#204442,#204443,
#204444,#204445,#204446,#204447,#204448,#204449,#204450,#204451,#204452,
#204453,#204454,#204455,#204456,#204457,#204458,#204459,#204460,#204461,
#204462,#204463,#204464,#204465,#204466,#204467,#204468,#204469,#204470,
#204471,#204472,#204473,#204474,#204475,#204476,#204477,#204478,#204479,
#204480,#204481,#204482,#204483,#204484,#204485,#204486,#204487,#204488,
#204489,#204490,#204491,#204492,#204493,#204494,#204495,#204496,#204497,
#204498,#204499,#204500,#204501,#204502,#204503,#204504,#204505,#204506,
#204507,#204508,#204509,#204510,#204511,#204512,#204513,#204514,#204515,
#204516,#204517,#204518,#204519,#204520,#204521,#204522,#204523,#204524,
#204525,#204526,#204527,#204528,#204529,#204530,#204531,#204532),
 .UNSPECIFIED.,.F.,.F.,(4,3,3,3,3,3,3,3,3,3,3,3,3,3,3,3,3,3,3,3,3,3,3,3,
3,3,3,3,3,3,3,3,3,3,3,3,3,3,3,3,3,3,3,3,3,3,3,3,3,3,3,3,4),(248.185819633594,
248.26828183968,248.350743697468,248.433205213809,248.515666395553,248.598127249549,
248.680587782648,248.763048001698,248.845507913549,248.927967525048,249.010426843045,
249.092885874387,249.175344625922,249.257803104499,249.340261316964,249.422719270164,
249.505176970946,249.587634426158,249.670091642646,249.756104230435,249.839428924856,
249.921895530414,250.004361291765,250.086826236323,250.169290391501,250.251753784709,
250.334216443352,250.416678394836,250.499139666562,250.581600285931,250.664060280338,
250.746519677179,250.828978503847,250.911436787734,250.993894556227,251.076351836715,
251.160485750164,251.242951748463,251.325416125011,251.407878989453,251.49034045141,
251.572800620484,251.655259606259,251.737717518302,251.823314635002,251.905779371946,
251.988241144244,252.070700390335,252.153157548514,252.235620067412,252.318077738696,
252.400536529604,252.422494451905),.UNSPECIFIED.);
#3421=B_SPLINE_CURVE_WITH_KNOTS('',3,(#204538,#204539,#204540,#204541,#204542,
#204543,#204544,#204545,#204546,#204547,#204548,#204549,#204550,#204551,
#204552,#204553,#204554,#204555,#204556,#204557,#204558,#204559,#204560,
#204561,#204562,#204563,#204564,#204565,#204566,#204567,#204568,#204569,
#204570,#204571,#204572,#204573,#204574,#204575,#204576,#204577,#204578,
#204579,#204580,#204581,#204582,#204583,#204584,#204585,#204586,#204587,
#204588,#204589,#204590,#204591,#204592,#204593,#204594,#204595,#204596,
#204597,#204598,#204599,#204600,#204601,#204602,#204603,#204604,#204605,
#204606,#204607,#204608,#204609,#204610,#204611,#204612,#204613,#204614,
#204615,#204616,#204617,#204618,#204619,#204620,#204621,#204622,#204623,
#204624,#204625,#204626,#204627,#204628,#204629,#204630,#204631,#204632,
#204633,#204634,#204635,#204636,#204637,#204638,#204639,#204640,#204641,
#204642,#204643,#204644,#204645,#204646,#204647,#204648,#204649,#204650,
#204651,#204652,#204653,#204654,#204655,#204656,#204657,#204658,#204659,
#204660,#204661,#204662,#204663,#204664,#204665,#204666,#204667,#204668,
#204669,#204670,#204671,#204672,#204673,#204674,#204675,#204676,#204677,
#204678,#204679,#204680,#204681,#204682,#204683,#204684,#204685,#204686,
#204687,#204688,#204689,#204690,#204691,#204692,#204693,#204694),
 .UNSPECIFIED.,.F.,.F.,(4,3,3,3,3,3,3,3,3,3,3,3,3,3,3,3,3,3,3,3,3,3,3,3,
3,3,3,3,3,3,3,3,3,3,3,3,3,3,3,3,3,3,3,3,3,3,3,3,3,3,3,3,4),(254.469004940774,
254.55146714686,254.633929004648,254.716390520989,254.798851702733,254.881312556729,
254.963773089828,255.046233308878,255.128693220729,255.211152832228,255.293612150225,
255.376071181567,255.458529933102,255.540988411679,255.623446624143,255.705904577343,
255.788362278126,255.870819733338,255.953276949825,256.039289537614,256.122614232035,
256.205080837594,256.287546598944,256.370011543503,256.452475698681,256.534939091888,
256.617401750531,256.699863702015,256.782324973742,256.86478559311,256.947245587517,
257.029704984358,257.112163811027,257.194622094913,257.277079863406,257.359537143894,
257.443671057344,257.526137055642,257.608601432191,257.691064296633,257.773525758589,
257.855985927663,257.938444913438,258.020902825481,258.106499942181,258.188964679125,
258.271426451423,258.353885697514,258.436342855693,258.518805374592,258.601263045875,
258.683721836783,258.705679759084),.UNSPECIFIED.);
#3422=B_SPLINE_CURVE_WITH_KNOTS('',3,(#204695,#204696,#204697,#204698,#204699,
#204700,#204701,#204702,#204703,#204704,#204705,#204706,#204707,#204708,
#204709,#204710,#204711,#204712,#204713,#204714,#204715,#204716,#204717,
#204718,#204719,#204720,#204721,#204722,#204723,#204724,#204725,#204726,
#204727,#204728,#204729,#204730,#204731,#204732,#204733,#204734,#204735,
#204736,#204737,#204738,#204739,#204740,#204741,#204742,#204743,#204744,
#204745,#204746,#204747,#204748,#204749,#204750,#204751,#204752,#204753,
#204754,#204755,#204756,#204757,#204758,#204759,#204760,#204761,#204762,
#204763,#204764,#204765,#204766,#204767,#204768,#204769,#204770,#204771,
#204772,#204773,#204774,#204775,#204776),.UNSPECIFIED.,.F.,.F.,(4,3,3,3,
3,3,3,3,3,3,3,3,3,3,3,3,3,3,3,3,3,3,3,3,3,3,3,4),(252.422853579701,252.492994672931,
252.572398013815,252.651819784978,252.731270762618,252.810794928837,252.890360839383,
252.970010687586,252.992364540862,253.070743561732,253.149056313048,253.227317209201,
253.305540627,253.38374091516,253.461949104325,253.540165157816,253.618402075045,
253.696672865199,253.775036444672,253.853449574132,253.931979956645,253.991104276724,
254.07139109245,254.151529610741,254.231469705656,254.311296548631,254.390970577163,
254.469004940774),.UNSPECIFIED.);
#3423=B_SPLINE_CURVE_WITH_KNOTS('',3,(#204778,#204779,#204780,#204781,#204782,
#204783,#204784,#204785,#204786,#204787,#204788,#204789,#204790,#204791,
#204792,#204793,#204794,#204795,#204796,#204797,#204798,#204799,#204800,
#204801,#204802,#204803,#204804,#204805,#204806,#204807,#204808,#204809,
#204810,#204811,#204812,#204813,#204814,#204815,#204816,#204817,#204818,
#204819,#204820,#204821,#204822,#204823,#204824,#204825,#204826,#204827,
#204828,#204829,#204830,#204831,#204832,#204833,#204834,#204835,#204836,
#204837,#204838,#204839,#204840,#204841,#204842,#204843,#204844,#204845,
#204846,#204847,#204848,#204849,#204850,#204851,#204852,#204853),
 .UNSPECIFIED.,.F.,.F.,(4,3,3,3,3,3,3,3,3,3,3,3,3,3,3,3,3,3,3,3,3,3,3,3,
3,4),(252.422494451905,252.504956055664,252.587416993543,252.669877292941,
252.752336981254,252.834796085876,252.917254634199,252.999712653613,253.082170171506,
253.168847344586,253.251314130194,253.333779243325,253.416242793632,253.498704890746,
253.581165644278,253.66362516382,253.746083558948,253.828540939219,253.911007325038,
253.993470526662,254.075930982611,254.158389131247,254.240854735259,254.323314613836,
254.405778725573,254.469004940774),.UNSPECIFIED.);
#3424=B_SPLINE_CURVE_WITH_KNOTS('',3,(#204854,#204855,#204856,#204857,#204858,
#204859,#204860,#204861,#204862,#204863,#204864,#204865,#204866,#204867,
#204868,#204869,#204870,#204871,#204872,#204873,#204874,#204875,#204876,
#204877,#204878,#204879,#204880,#204881,#204882,#204883,#204884,#204885,
#204886,#204887,#204888,#204889,#204890,#204891,#204892,#204893,#204894,
#204895,#204896,#204897,#204898,#204899,#204900,#204901,#204902,#204903,
#204904,#204905,#204906,#204907,#204908,#204909,#204910,#204911,#204912,
#204913,#204914,#204915,#204916,#204917,#204918,#204919,#204920,#204921,
#204922,#204923,#204924,#204925,#204926,#204927,#204928,#204929,#204930,
#204931,#204932,#204933,#204934,#204935,#204936,#204937,#204938,#204939,
#204940,#204941,#204942,#204943,#204944,#204945,#204946,#204947,#204948,
#204949,#204950,#204951,#204952,#204953,#204954,#204955,#204956,#204957,
#204958,#204959,#204960,#204961,#204962,#204963,#204964,#204965,#204966,
#204967,#204968,#204969,#204970,#204971,#204972,#204973,#204974,#204975,
#204976,#204977,#204978,#204979,#204980,#204981,#204982,#204983,#204984,
#204985,#204986,#204987,#204988,#204989,#204990,#204991,#204992,#204993,
#204994,#204995,#204996,#204997,#204998,#204999,#205000,#205001,#205002,
#205003,#205004,#205005,#205006,#205007,#205008,#205009,#205010,#205011,
#205012,#205013,#205014,#205015,#205016,#205017,#205018,#205019,#205020,
#205021,#205022,#205023,#205024,#205025),.UNSPECIFIED.,.F.,.F.,(4,3,3,3,
3,3,3,3,3,3,3,3,3,3,3,3,3,3,3,3,3,3,3,3,3,3,3,3,3,3,3,3,3,3,3,3,3,3,3,3,
3,3,3,3,3,3,3,3,3,3,3,3,3,3,3,3,3,4),(254.46960918162,254.543372393565,
254.617102384427,254.690811973322,254.764532044339,254.808158530261,254.892834868469,
254.977657352983,255.062679723859,255.147788605667,255.233018145042,255.307528398192,
255.389084660852,255.470565600517,255.554648766919,255.635974519431,255.721436392777,
255.806898266123,255.886301607007,255.96572337817,256.045174355811,256.124698522031,
256.204264432576,256.283914280779,256.306268134054,256.384647154924,256.46295990624,
256.541220802393,256.619444220193,256.697644508353,256.775852697518,256.854068751008,
256.932305668238,257.010576458391,257.088940037864,257.167353167323,257.245883549836,
257.305007869916,257.38106437667,257.457025194664,257.532907115283,257.60872684879,
257.684501043121,257.761906863454,257.837654619569,257.913409625097,257.989186890327,
258.06782706919,258.143736255659,258.219702247601,258.295774445211,258.303747605778,
258.381317928865,258.46245396008,258.539836629605,258.617165310272,258.694446707613,
258.705862053727),.UNSPECIFIED.);
#3425=B_SPLINE_CURVE_WITH_KNOTS('',3,(#205031,#205032,#205033,#205034,#205035,
#205036,#205037,#205038,#205039,#205040,#205041,#205042,#205043,#205044,
#205045,#205046,#205047,#205048,#205049,#205050,#205051,#205052,#205053,
#205054,#205055,#205056,#205057,#205058,#205059,#205060,#205061,#205062,
#205063,#205064,#205065,#205066,#205067,#205068,#205069,#205070,#205071,
#205072,#205073,#205074,#205075,#205076,#205077,#205078,#205079,#205080,
#205081,#205082,#205083,#205084,#205085,#205086,#205087,#205088,#205089,
#205090,#205091,#205092,#205093,#205094,#205095,#205096,#205097,#205098,
#205099,#205100,#205101,#205102,#205103,#205104,#205105,#205106,#205107,
#205108,#205109,#205110,#205111,#205112,#205113,#205114,#205115,#205116,
#205117,#205118,#205119,#205120,#205121,#205122,#205123,#205124,#205125,
#205126,#205127,#205128,#205129,#205130,#205131,#205132,#205133,#205134,
#205135,#205136,#205137,#205138,#205139,#205140,#205141,#205142,#205143,
#205144,#205145,#205146,#205147,#205148,#205149,#205150,#205151,#205152,
#205153,#205154,#205155,#205156,#205157,#205158,#205159,#205160,#205161,
#205162,#205163,#205164,#205165,#205166,#205167,#205168,#205169,#205170,
#205171,#205172,#205173,#205174,#205175,#205176,#205177,#205178,#205179,
#205180,#205181,#205182,#205183,#205184,#205185,#205186,#205187,#205188,
#205189,#205190,#205191,#205192,#205193,#205194,#205195,#205196,#205197,
#205198,#205199),.UNSPECIFIED.,.F.,.F.,(4,3,3,3,3,3,3,3,3,3,3,3,3,3,3,3,
3,3,3,3,3,3,3,3,3,3,3,3,3,3,3,3,3,3,3,3,3,3,3,3,3,3,3,3,3,3,3,3,3,3,3,3,
3,3,3,3,4),(260.752190247953,260.870697092815,260.982282427759,261.058338934513,
261.134299752507,261.210181673126,261.286001406633,261.361775600964,261.439181421297,
261.514929177412,261.59068418294,261.66646144817,261.745101627033,261.821010813502,
261.896976805445,261.973049003055,261.981022163622,262.058581015167,262.136047559062,
262.213437462355,262.290766337048,262.368049751191,262.445310797763,262.522561498607,
262.599815901293,262.677088052825,262.754433390962,262.831816164687,262.909305660335,
262.979761899484,263.063981182377,263.14807386135,263.231960487163,263.31571747655,
263.399259179208,263.479131767415,263.556498963208,263.633884552659,263.711302334447,
263.78880725606,263.866361855312,263.944023202264,263.978501635346,264.05812237409,
264.137670201746,264.217157431022,264.296596327935,264.375999120742,264.45538433364,
264.534760564193,264.614138893743,264.693530403614,264.772975638445,264.852449219226,
264.931996331276,264.977241371208,264.989258096655),.UNSPECIFIED.);
#3426=B_SPLINE_CURVE_WITH_KNOTS('',3,(#205200,#205201,#205202,#205203,#205204,
#205205,#205206,#205207,#205208,#205209,#205210,#205211,#205212,#205213,
#205214,#205215,#205216,#205217,#205218,#205219,#205220,#205221,#205222,
#205223,#205224,#205225,#205226,#205227,#205228,#205229,#205230,#205231,
#205232,#205233,#205234,#205235,#205236,#205237,#205238,#205239,#205240,
#205241,#205242,#205243,#205244,#205245,#205246,#205247,#205248,#205249,
#205250,#205251,#205252,#205253,#205254,#205255,#205256,#205257,#205258,
#205259,#205260,#205261,#205262,#205263,#205264,#205265,#205266,#205267,
#205268,#205269,#205270,#205271,#205272,#205273,#205274,#205275),
 .UNSPECIFIED.,.F.,.F.,(4,3,3,3,3,3,3,3,3,3,3,3,3,3,3,3,3,3,3,3,3,3,3,3,
3,4),(258.705679759084,258.788141362843,258.870602300722,258.95306260012,
259.035522288433,259.117981393055,259.200439941378,259.282897960792,259.365355478686,
259.452032651765,259.534499437373,259.616964550504,259.699428100811,259.781890197925,
259.864350951457,259.946810471,260.029268866127,260.111726246397,260.194192632217,
260.276655833841,260.359116289789,260.441574438425,260.524040042437,260.606499921014,
260.688964032751,260.752190247953),.UNSPECIFIED.);
#3427=B_SPLINE_CURVE_WITH_KNOTS('',3,(#205277,#205278,#205279,#205280,#205281,
#205282,#205283,#205284,#205285,#205286,#205287,#205288,#205289,#205290,
#205291,#205292,#205293,#205294,#205295,#205296,#205297,#205298,#205299,
#205300,#205301,#205302,#205303,#205304,#205305,#205306,#205307,#205308,
#205309,#205310,#205311,#205312,#205313,#205314,#205315,#205316,#205317,
#205318,#205319,#205320,#205321,#205322,#205323,#205324,#205325,#205326,
#205327,#205328,#205329,#205330,#205331,#205332,#205333,#205334,#205335,
#205336,#205337,#205338,#205339,#205340,#205341,#205342,#205343,#205344,
#205345,#205346,#205347,#205348,#205349,#205350,#205351,#205352,#205353,
#205354,#205355,#205356,#205357,#205358),.UNSPECIFIED.,.F.,.F.,(4,3,3,3,
3,3,3,3,3,3,3,3,3,3,3,3,3,3,3,3,3,3,3,3,3,3,3,4),(258.705862053727,258.783119976353,
258.860370296477,258.937627060954,259.014904317578,259.09225596849,259.169647521608,
259.247141993696,259.302487341641,259.386706624534,259.470799303508,259.554685929322,
259.638442918708,259.721984621366,259.801857209572,259.879224405365,259.956609994816,
260.034027776602,260.111532698215,260.189087297467,260.266748644419,260.301227077503,
260.387540615977,260.473730924891,260.55969365616,260.645493440371,260.731032807719,
260.752190247953),.UNSPECIFIED.);
#3428=B_SPLINE_CURVE_WITH_KNOTS('',3,(#205359,#205360,#205361,#205362,#205363,
#205364,#205365,#205366,#205367,#205368,#205369,#205370,#205371,#205372,
#205373,#205374,#205375,#205376,#205377,#205378,#205379,#205380,#205381,
#205382,#205383,#205384,#205385,#205386,#205387,#205388,#205389,#205390,
#205391,#205392,#205393,#205394,#205395,#205396,#205397,#205398,#205399,
#205400,#205401,#205402,#205403,#205404,#205405,#205406,#205407,#205408,
#205409,#205410,#205411,#205412,#205413,#205414,#205415,#205416,#205417,
#205418,#205419,#205420,#205421,#205422,#205423,#205424,#205425,#205426,
#205427,#205428,#205429,#205430,#205431,#205432,#205433,#205434,#205435,
#205436,#205437,#205438,#205439,#205440,#205441,#205442,#205443,#205444,
#205445,#205446,#205447,#205448,#205449,#205450,#205451,#205452,#205453,
#205454,#205455,#205456,#205457,#205458,#205459,#205460,#205461,#205462,
#205463,#205464,#205465,#205466,#205467,#205468,#205469,#205470,#205471,
#205472,#205473,#205474,#205475,#205476,#205477,#205478,#205479,#205480,
#205481,#205482,#205483,#205484,#205485,#205486,#205487,#205488,#205489,
#205490,#205491,#205492,#205493,#205494,#205495,#205496,#205497,#205498,
#205499,#205500,#205501,#205502,#205503,#205504,#205505,#205506,#205507,
#205508,#205509,#205510,#205511,#205512,#205513,#205514,#205515),
 .UNSPECIFIED.,.F.,.F.,(4,3,3,3,3,3,3,3,3,3,3,3,3,3,3,3,3,3,3,3,3,3,3,3,
3,3,3,3,3,3,3,3,3,3,3,3,3,3,3,3,3,3,3,3,3,3,3,3,3,3,3,3,4),(260.752190247953,
260.834652454039,260.917114311827,260.999575828168,261.082037009912,261.164497863908,
261.246958397007,261.329418616057,261.411878527908,261.494338139407,261.576797457404,
261.659256488746,261.741715240281,261.824173718857,261.906631931322,261.989089884522,
262.071547585305,262.154005040516,262.236462257004,262.322474844793,262.405799539214,
262.488266144772,262.570731906123,262.653196850681,262.735661005859,262.818124399067,
262.90058705771,262.983049009194,263.06551028092,263.147970900289,263.230430894696,
263.312890291537,263.395349118206,263.477807402092,263.560265170585,263.642722451073,
263.726856364523,263.809322362821,263.89178673937,263.974249603812,264.056711065768,
264.139171234842,264.221630220617,264.30408813266,264.38968524936,264.472149986304,
264.554611758602,264.637071004693,264.719528162872,264.801990681771,264.884448353054,
264.966907143962,264.988865066264),.UNSPECIFIED.);
#3429=B_SPLINE_CURVE_WITH_KNOTS('',3,(#205521,#205522,#205523,#205524,#205525,
#205526,#205527,#205528,#205529,#205530,#205531,#205532,#205533,#205534,
#205535,#205536,#205537,#205538,#205539,#205540,#205541,#205542,#205543,
#205544,#205545,#205546,#205547,#205548,#205549,#205550,#205551,#205552,
#205553,#205554,#205555,#205556,#205557,#205558,#205559,#205560,#205561,
#205562,#205563,#205564,#205565,#205566,#205567,#205568,#205569,#205570,
#205571,#205572,#205573,#205574,#205575,#205576,#205577,#205578,#205579,
#205580,#205581,#205582,#205583,#205584,#205585,#205586,#205587,#205588,
#205589,#205590,#205591,#205592,#205593,#205594,#205595,#205596,#205597,
#205598,#205599,#205600,#205601,#205602,#205603,#205604,#205605,#205606,
#205607,#205608,#205609,#205610,#205611,#205612,#205613,#205614,#205615,
#205616,#205617,#205618,#205619,#205620,#205621,#205622,#205623,#205624,
#205625,#205626,#205627,#205628,#205629,#205630,#205631,#205632,#205633,
#205634,#205635,#205636,#205637,#205638,#205639,#205640,#205641,#205642,
#205643,#205644,#205645,#205646,#205647,#205648,#205649,#205650,#205651,
#205652,#205653,#205654,#205655,#205656,#205657,#205658,#205659,#205660,
#205661,#205662,#205663,#205664,#205665,#205666,#205667,#205668,#205669,
#205670,#205671,#205672,#205673,#205674,#205675,#205676,#205677,#205678,
#205679,#205680,#205681,#205682,#205683,#205684,#205685,#205686,#205687,
#205688,#205689),.UNSPECIFIED.,.F.,.F.,(4,3,3,3,3,3,3,3,3,3,3,3,3,3,3,3,
3,3,3,3,3,3,3,3,3,3,3,3,3,3,3,3,3,3,3,3,3,3,3,3,3,3,3,3,3,3,3,3,3,3,3,3,
3,3,3,3,4),(267.035375555214,267.113226162742,267.191012379613,267.268749321261,
267.346452067757,267.424828131637,267.502524314221,267.580233460035,267.657969206467,
267.736842049549,267.814710913995,267.894085746395,267.973460578795,268.049517085549,
268.125477903543,268.201359824162,268.277179557669,268.352953752,268.430359572332,
268.506107328447,268.581862333975,268.657639599206,268.736279778069,268.812188964538,
268.88815495648,268.96422715409,268.972200314657,269.049759166202,269.127225710097,
269.20461561339,269.281944488083,269.359227902226,269.436488948798,269.513739649642,
269.590994052327,269.668266203859,269.745611541997,269.822994315722,269.900483811369,
269.970940050519,270.055159333412,270.139252012385,270.223138638198,270.306895627585,
270.390437330243,270.47030991845,270.547677114243,270.625062703694,270.702480485482,
270.779985407095,270.857540006347,270.935201353299,270.969679786381,271.049292724175,
271.128841433105,271.208322864593,271.272348741102),.UNSPECIFIED.);
#3430=B_SPLINE_CURVE_WITH_KNOTS('',3,(#205690,#205691,#205692,#205693,#205694,
#205695,#205696,#205697,#205698,#205699,#205700,#205701,#205702,#205703,
#205704,#205705,#205706,#205707,#205708,#205709,#205710,#205711,#205712,
#205713,#205714,#205715,#205716,#205717,#205718,#205719,#205720,#205721,
#205722,#205723,#205724,#205725,#205726,#205727,#205728,#205729,#205730,
#205731,#205732,#205733,#205734,#205735,#205736,#205737,#205738,#205739,
#205740,#205741,#205742,#205743,#205744,#205745,#205746,#205747,#205748,
#205749,#205750,#205751,#205752,#205753,#205754,#205755,#205756,#205757,
#205758,#205759,#205760,#205761,#205762,#205763,#205764,#205765,#205766,
#205767,#205768,#205769,#205770,#205771),.UNSPECIFIED.,.F.,.F.,(4,3,3,3,
3,3,3,3,3,3,3,3,3,3,3,3,3,3,3,3,3,3,3,3,3,3,3,4),(264.989258096655,265.06596162616,
265.142600364666,265.21918899973,265.295743664136,265.372278865214,265.448818639486,
265.476611239139,265.561287577347,265.646110061861,265.731132432737,265.816241314545,
265.90147085392,265.97598110707,266.057537369729,266.139018309395,266.223101475797,
266.304427228308,266.389889101655,266.475350975001,266.554754315885,266.634176087048,
266.713627064688,266.793151230908,266.872717141453,266.952366989656,266.974720842932,
267.035375555133),.UNSPECIFIED.);
#3431=B_SPLINE_CURVE_WITH_KNOTS('',3,(#205773,#205774,#205775,#205776,#205777,
#205778,#205779,#205780,#205781,#205782,#205783,#205784,#205785,#205786,
#205787,#205788,#205789,#205790,#205791,#205792,#205793,#205794,#205795,
#205796,#205797,#205798,#205799,#205800,#205801,#205802,#205803,#205804,
#205805,#205806,#205807,#205808,#205809,#205810,#205811,#205812,#205813,
#205814,#205815,#205816,#205817,#205818,#205819,#205820,#205821,#205822,
#205823,#205824,#205825,#205826,#205827,#205828,#205829,#205830,#205831,
#205832,#205833,#205834,#205835,#205836,#205837,#205838,#205839,#205840,
#205841,#205842,#205843,#205844,#205845,#205846,#205847,#205848),
 .UNSPECIFIED.,.F.,.F.,(4,3,3,3,3,3,3,3,3,3,3,3,3,3,3,3,3,3,3,3,3,3,3,3,
3,4),(264.988865066264,265.071326670023,265.153787607902,265.2362479073,
265.318707595613,265.401166700235,265.483625248558,265.566083267972,265.648540785865,
265.735217958945,265.817684744553,265.900149857685,265.982613407991,266.065075505105,
266.147536258637,266.22999577818,266.312454173307,266.394911553578,266.477377939397,
266.559841141021,266.642301596969,266.724759745606,266.807225349617,266.889685228195,
266.972149339931,267.035375555133),.UNSPECIFIED.);
#3432=B_SPLINE_CURVE_WITH_KNOTS('',3,(#205849,#205850,#205851,#205852,#205853,
#205854,#205855,#205856,#205857,#205858,#205859,#205860,#205861,#205862,
#205863,#205864,#205865,#205866,#205867,#205868,#205869,#205870,#205871,
#205872,#205873,#205874,#205875,#205876,#205877,#205878,#205879,#205880,
#205881,#205882,#205883,#205884,#205885,#205886,#205887,#205888,#205889,
#205890,#205891,#205892,#205893,#205894,#205895,#205896,#205897,#205898,
#205899,#205900,#205901,#205902,#205903,#205904,#205905,#205906,#205907,
#205908,#205909,#205910,#205911,#205912,#205913,#205914,#205915,#205916,
#205917,#205918,#205919,#205920,#205921,#205922,#205923,#205924,#205925,
#205926,#205927,#205928,#205929,#205930,#205931,#205932,#205933,#205934,
#205935,#205936,#205937,#205938,#205939,#205940,#205941,#205942,#205943,
#205944,#205945,#205946,#205947,#205948,#205949,#205950,#205951,#205952,
#205953,#205954,#205955,#205956,#205957,#205958,#205959,#205960,#205961,
#205962,#205963,#205964,#205965,#205966,#205967,#205968,#205969,#205970,
#205971,#205972,#205973,#205974,#205975,#205976,#205977,#205978,#205979,
#205980,#205981,#205982,#205983,#205984,#205985,#205986,#205987,#205988,
#205989,#205990,#205991,#205992,#205993,#205994,#205995,#205996,#205997,
#205998,#205999,#206000,#206001,#206002,#206003,#206004,#206005,#206006,
#206007,#206008,#206009,#206010,#206011,#206012,#206013,#206014),
 .UNSPECIFIED.,.F.,.F.,(4,3,3,3,3,3,3,3,3,3,3,3,3,3,3,3,3,3,3,3,3,3,3,3,
3,3,3,3,3,3,3,3,3,3,3,3,3,3,3,3,3,3,3,3,3,3,3,3,3,3,3,3,3,3,3,4),(267.035375555133,
267.121673149256,267.208406509972,267.292405228538,267.372025967282,267.451573794938,
267.531061024214,267.610499921127,267.689902713933,267.769287926832,267.848664157384,
267.928042486935,268.007433996806,268.086879231637,268.166352812418,268.245899924467,
268.2911449644,268.367859971249,268.444507883613,268.521103395352,268.597662293051,
268.67419967713,268.750741197582,268.790514832331,268.875191170539,268.960013655052,
269.045036025928,269.130144907736,269.21537444711,269.289884700262,269.371440962922,
269.452921902588,269.537005068989,269.618330821502,269.703792694847,269.789254568193,
269.868657909077,269.94807968024,270.027530657881,270.107054824101,270.186620734646,
270.266270582849,270.288624436125,270.36700396344,270.445317071958,270.523578176484,
270.601801654128,270.6800018538,270.758208900558,270.836423602087,270.914658957359,
270.992927974971,271.071286312509,271.149694125371,271.228211424852,271.272446552927),
 .UNSPECIFIED.);
#3433=B_SPLINE_CURVE_WITH_KNOTS('',3,(#206020,#206021,#206022,#206023,#206024,
#206025,#206026,#206027,#206028,#206029,#206030,#206031,#206032,#206033,
#206034,#206035,#206036,#206037,#206038,#206039,#206040,#206041,#206042,
#206043,#206044,#206045,#206046,#206047,#206048,#206049,#206050,#206051,
#206052,#206053,#206054,#206055,#206056,#206057,#206058,#206059,#206060,
#206061,#206062,#206063,#206064,#206065,#206066,#206067,#206068,#206069,
#206070,#206071,#206072,#206073,#206074,#206075,#206076,#206077,#206078,
#206079,#206080,#206081,#206082,#206083,#206084,#206085,#206086,#206087,
#206088,#206089,#206090,#206091,#206092,#206093,#206094,#206095,#206096,
#206097,#206098,#206099,#206100,#206101,#206102,#206103,#206104,#206105,
#206106,#206107,#206108,#206109,#206110,#206111,#206112,#206113,#206114,
#206115,#206116,#206117,#206118,#206119,#206120,#206121,#206122,#206123,
#206124,#206125,#206126,#206127,#206128,#206129,#206130,#206131,#206132,
#206133,#206134,#206135,#206136,#206137,#206138,#206139,#206140,#206141,
#206142,#206143,#206144,#206145,#206146,#206147,#206148,#206149,#206150,
#206151,#206152,#206153,#206154,#206155,#206156,#206157,#206158,#206159,
#206160,#206161,#206162,#206163,#206164,#206165,#206166,#206167,#206168,
#206169,#206170,#206171,#206172,#206173,#206174,#206175,#206176),
 .UNSPECIFIED.,.F.,.F.,(4,3,3,3,3,3,3,3,3,3,3,3,3,3,3,3,3,3,3,3,3,3,3,3,
3,3,3,3,3,3,3,3,3,3,3,3,3,3,3,3,3,3,3,3,3,3,3,3,3,3,3,3,4),(273.318560862312,
273.401023068398,273.483484926186,273.565946442527,273.648407624271,273.730868478267,
273.813329011366,273.895789230416,273.978249142267,274.060708753766,274.143168071763,
274.225627103105,274.30808585464,274.390544333217,274.473002545681,274.555460498881,
274.637918199664,274.720375654876,274.802832871364,274.888845459153,274.972170153574,
275.054636759132,275.137102520483,275.219567465041,275.302031620219,275.384495013426,
275.46695767207,275.549419623554,275.63188089528,275.714341514648,275.796801509056,
275.879260905897,275.961719732565,276.044178016452,276.126635784945,276.209093065433,
276.293226978882,276.375692977181,276.458157353729,276.540620218171,276.623081680128,
276.705541849202,276.788000834977,276.87045874702,276.95605586372,277.038520600664,
277.120982372962,277.203441619053,277.285898777232,277.36836129613,277.450818967414,
277.533277758322,277.555235680623),.UNSPECIFIED.);
#3434=B_SPLINE_CURVE_WITH_KNOTS('',3,(#206177,#206178,#206179,#206180,#206181,
#206182,#206183,#206184,#206185,#206186,#206187,#206188,#206189,#206190,
#206191,#206192,#206193,#206194,#206195,#206196,#206197,#206198,#206199,
#206200,#206201,#206202,#206203,#206204,#206205,#206206,#206207,#206208,
#206209,#206210,#206211,#206212,#206213,#206214,#206215,#206216,#206217,
#206218,#206219,#206220,#206221,#206222,#206223,#206224,#206225,#206226,
#206227,#206228,#206229,#206230,#206231,#206232,#206233,#206234,#206235,
#206236,#206237,#206238,#206239,#206240,#206241,#206242,#206243,#206244,
#206245,#206246,#206247,#206248,#206249,#206250,#206251,#206252,#206253,
#206254,#206255,#206256,#206257,#206258),.UNSPECIFIED.,.F.,.F.,(4,3,3,3,
3,3,3,3,3,3,3,3,3,3,3,3,3,3,3,3,3,3,3,3,3,3,3,4),(271.272348741102,271.351757590811,
271.431145833752,271.51052294159,271.589899996501,271.669288079255,271.748728990676,
271.828196272274,271.907739962812,271.968419522243,272.045134529092,272.121782441457,
272.198377953196,272.274936850894,272.351474234974,272.428015755426,272.467789390175,
272.552465728384,272.637288212897,272.722310583774,272.807419465583,272.892649004958,
272.967159258106,273.055009659157,273.138354386056,273.221613149921,273.304753508643,
273.318560862312),.UNSPECIFIED.);
#3435=B_SPLINE_CURVE_WITH_KNOTS('',3,(#206260,#206261,#206262,#206263,#206264,
#206265,#206266,#206267,#206268,#206269,#206270,#206271,#206272,#206273,
#206274,#206275,#206276,#206277,#206278,#206279,#206280,#206281,#206282,
#206283,#206284,#206285,#206286,#206287,#206288,#206289,#206290,#206291,
#206292,#206293,#206294,#206295,#206296,#206297,#206298,#206299,#206300,
#206301,#206302,#206303,#206304,#206305,#206306,#206307,#206308,#206309,
#206310,#206311,#206312,#206313,#206314,#206315,#206316,#206317,#206318,
#206319,#206320,#206321,#206322,#206323,#206324,#206325,#206326,#206327,
#206328,#206329,#206330,#206331,#206332,#206333,#206334,#206335,#206336,
#206337,#206338,#206339,#206340,#206341,#206342,#206343,#206344,#206345,
#206346,#206347),.UNSPECIFIED.,.F.,.F.,(4,3,3,3,3,3,3,3,3,3,3,3,3,3,3,3,
3,3,3,3,3,3,3,3,3,3,3,3,3,4),(271.272446552927,271.287364171987,271.363420678741,
271.439381496735,271.515263417354,271.591083150861,271.666857345192,271.744263165524,
271.82001092164,271.895765927168,271.971543192398,272.050183371261,272.12609255773,
272.202058549672,272.278130747282,272.286103907849,272.363662759394,272.441129303289,
272.518519206582,272.595848081275,272.673131495418,272.75039254199,272.827643242834,
272.904897645519,272.982169797051,273.059515135189,273.136897908914,273.214387404561,
273.284843643711,273.318560862174),.UNSPECIFIED.);
#3436=B_SPLINE_CURVE_WITH_KNOTS('',3,(#206348,#206349,#206350,#206351,#206352,
#206353,#206354,#206355,#206356,#206357,#206358,#206359,#206360,#206361,
#206362,#206363,#206364,#206365,#206366,#206367,#206368,#206369,#206370,
#206371,#206372,#206373,#206374,#206375,#206376,#206377,#206378,#206379,
#206380,#206381,#206382,#206383,#206384,#206385,#206386,#206387,#206388,
#206389,#206390,#206391,#206392,#206393,#206394,#206395,#206396,#206397,
#206398,#206399,#206400,#206401,#206402,#206403,#206404,#206405,#206406,
#206407,#206408,#206409,#206410,#206411,#206412,#206413,#206414,#206415,
#206416,#206417,#206418,#206419,#206420,#206421,#206422,#206423,#206424,
#206425,#206426,#206427,#206428,#206429,#206430,#206431,#206432,#206433,
#206434,#206435,#206436,#206437,#206438,#206439,#206440,#206441,#206442,
#206443,#206444,#206445,#206446,#206447,#206448,#206449,#206450,#206451,
#206452,#206453,#206454,#206455,#206456,#206457,#206458,#206459,#206460,
#206461,#206462,#206463,#206464,#206465,#206466,#206467,#206468,#206469,
#206470,#206471,#206472,#206473,#206474,#206475,#206476,#206477,#206478,
#206479,#206480,#206481,#206482,#206483,#206484,#206485,#206486,#206487,
#206488,#206489,#206490,#206491,#206492,#206493,#206494,#206495,#206496,
#206497,#206498,#206499,#206500,#206501,#206502,#206503,#206504,#206505,
#206506,#206507,#206508,#206509,#206510,#206511,#206512,#206513,#206514,
#206515,#206516),.UNSPECIFIED.,.F.,.F.,(4,3,3,3,3,3,3,3,3,3,3,3,3,3,3,3,
3,3,3,3,3,3,3,3,3,3,3,3,3,3,3,3,3,3,3,3,3,3,3,3,3,3,3,3,3,3,3,3,3,3,3,3,
3,3,3,3,4),(273.318560862312,273.401319579048,273.483951878501,273.566402426066,
273.648741291947,273.730919046419,273.784213511642,273.861580707435,273.938966296886,
274.016384078674,274.093889000286,274.171443599539,274.249104946491,274.283583379573,
274.363204118317,274.442751945973,274.522239175248,274.601678072162,274.681080864968,
274.760466077867,274.839842308419,274.919220637969,274.99861214784,275.078057382671,
275.157530963452,275.237078075502,275.282323115435,275.359038122284,275.435686034648,
275.512281546387,275.588840444086,275.665377828165,275.741919348617,275.781692983366,
275.866369321574,275.951191806088,276.036214176964,276.121323058773,276.206552598148,
276.281062851298,276.362619113958,276.444100053624,276.528183220025,276.609508972537,
276.694970845883,276.780432719229,276.859836060113,276.939257831275,277.018708808916,
277.098232975136,277.177798885681,277.257448733884,277.27980258716,277.358178317146,
277.436494507362,277.514754126766,277.555413490998),.UNSPECIFIED.);
#3437=B_SPLINE_CURVE_WITH_KNOTS('',3,(#206522,#206523,#206524,#206525,#206526,
#206527,#206528,#206529,#206530,#206531,#206532,#206533,#206534,#206535,
#206536,#206537,#206538,#206539,#206540,#206541,#206542,#206543,#206544,
#206545,#206546,#206547,#206548,#206549,#206550,#206551,#206552,#206553,
#206554,#206555,#206556,#206557,#206558,#206559,#206560,#206561,#206562,
#206563,#206564,#206565,#206566,#206567,#206568,#206569,#206570,#206571,
#206572,#206573,#206574,#206575,#206576,#206577,#206578,#206579,#206580,
#206581,#206582,#206583,#206584,#206585,#206586,#206587,#206588,#206589,
#206590,#206591,#206592,#206593,#206594,#206595,#206596,#206597,#206598,
#206599,#206600,#206601,#206602,#206603,#206604,#206605,#206606,#206607,
#206608,#206609,#206610,#206611,#206612,#206613,#206614,#206615,#206616,
#206617,#206618,#206619,#206620,#206621,#206622,#206623,#206624,#206625,
#206626,#206627,#206628,#206629,#206630,#206631,#206632,#206633,#206634,
#206635,#206636,#206637,#206638,#206639,#206640,#206641,#206642,#206643,
#206644,#206645,#206646,#206647,#206648,#206649,#206650,#206651,#206652,
#206653,#206654,#206655,#206656,#206657,#206658,#206659,#206660,#206661,
#206662,#206663,#206664,#206665,#206666,#206667,#206668,#206669,#206670,
#206671,#206672,#206673,#206674,#206675,#206676,#206677,#206678,#206679,
#206680,#206681,#206682,#206683,#206684,#206685,#206686,#206687,#206688,
#206689,#206690),.UNSPECIFIED.,.F.,.F.,(4,3,3,3,3,3,3,3,3,3,3,3,3,3,3,3,
3,3,3,3,3,3,3,3,3,3,3,3,3,3,3,3,3,3,3,3,3,3,3,3,3,3,3,3,3,3,3,3,3,3,3,3,
3,3,3,3,4),(279.601746169492,279.690893979404,279.778229212141,279.868283310641,
279.958337409141,280.039893671801,280.121374611467,280.205457777868,280.28678353038,
280.372245403726,280.457707277072,280.537110617956,280.616532389119,280.69598336676,
280.77550753298,280.855073443525,280.934723291728,280.957077145003,281.035456165873,
281.113768917189,281.192029813342,281.270253231142,281.348453519301,281.426661708466,
281.504877761956,281.583114679186,281.66138546934,281.739749048813,281.818162178272,
281.896692560785,281.955816880865,282.031873387619,282.107834205613,282.183716126232,
282.259535859739,282.33531005407,282.412715874402,282.488463630518,282.564218636046,
282.639995901276,282.718636080139,282.794545266608,282.87051125855,282.94658345616,
282.954556616727,283.032122093181,283.109593983157,283.186987958972,283.268342910669,
283.345623807737,283.422879230533,283.500123234353,283.577369865329,283.654659144348,
283.731973167213,283.80935508972,283.837827572545),.UNSPECIFIED.);
#3438=B_SPLINE_CURVE_WITH_KNOTS('',3,(#206691,#206692,#206693,#206694,#206695,
#206696,#206697,#206698,#206699,#206700,#206701,#206702,#206703,#206704,
#206705,#206706,#206707,#206708,#206709,#206710,#206711,#206712,#206713,
#206714,#206715,#206716,#206717,#206718,#206719,#206720,#206721,#206722,
#206723,#206724,#206725,#206726,#206727,#206728,#206729,#206730,#206731,
#206732,#206733,#206734,#206735,#206736,#206737,#206738,#206739,#206740,
#206741,#206742,#206743,#206744,#206745,#206746,#206747,#206748,#206749,
#206750,#206751,#206752,#206753,#206754,#206755,#206756,#206757,#206758,
#206759,#206760,#206761,#206762,#206763,#206764,#206765,#206766),
 .UNSPECIFIED.,.F.,.F.,(4,3,3,3,3,3,3,3,3,3,3,3,3,3,3,3,3,3,3,3,3,3,3,3,
3,4),(277.555235680623,277.637697284382,277.720158222261,277.802618521659,
277.885078209972,277.967537314594,278.049995862917,278.132453882331,278.214911400224,
278.301588573303,278.384055358912,278.466520472043,278.54898402235,278.631446119464,
278.713906872996,278.796366392538,278.878824787665,278.961282167936,279.043748553756,
279.12621175538,279.208672211328,279.291130359965,279.373595963976,279.456055842554,
279.53851995429,279.601746169492),.UNSPECIFIED.);
#3439=B_SPLINE_CURVE_WITH_KNOTS('',3,(#206768,#206769,#206770,#206771,#206772,
#206773,#206774,#206775,#206776,#206777,#206778,#206779,#206780,#206781,
#206782,#206783,#206784,#206785,#206786,#206787,#206788,#206789,#206790,
#206791,#206792,#206793,#206794,#206795,#206796,#206797,#206798,#206799,
#206800,#206801,#206802,#206803,#206804,#206805,#206806,#206807,#206808,
#206809,#206810,#206811,#206812,#206813,#206814,#206815,#206816,#206817,
#206818,#206819,#206820,#206821,#206822,#206823,#206824,#206825,#206826,
#206827,#206828,#206829,#206830,#206831,#206832,#206833,#206834,#206835,
#206836,#206837,#206838,#206839,#206840,#206841,#206842,#206843,#206844,
#206845,#206846,#206847,#206848,#206849,#206850,#206851,#206852),
 .UNSPECIFIED.,.F.,.F.,(4,3,3,3,3,3,3,3,3,3,3,3,3,3,3,3,3,3,3,3,3,3,3,3,
3,3,3,3,4),(277.555413490998,277.633623098407,277.714238001484,277.792448912532,
277.870674844257,277.948928800526,278.03133218115,278.109724211507,278.18817289723,
278.266725737398,278.278542323022,278.354598829776,278.43055964777,278.506441568389,
278.582261301896,278.658035496228,278.73544131656,278.811189072675,278.886944078203,
278.962721343433,279.041361522296,279.117270708765,279.193236700707,279.269308898317,
279.277282058884,279.374587676882,279.471153022842,279.566208583516,279.601746169384),
 .UNSPECIFIED.);
#3440=B_SPLINE_CURVE_WITH_KNOTS('',3,(#206853,#206854,#206855,#206856,#206857,
#206858,#206859,#206860,#206861,#206862,#206863,#206864,#206865,#206866,
#206867,#206868,#206869,#206870,#206871,#206872,#206873,#206874,#206875,
#206876,#206877,#206878,#206879,#206880,#206881,#206882,#206883,#206884,
#206885,#206886,#206887,#206888,#206889,#206890,#206891,#206892,#206893,
#206894,#206895,#206896,#206897,#206898,#206899,#206900,#206901,#206902,
#206903,#206904,#206905,#206906,#206907,#206908,#206909,#206910,#206911,
#206912,#206913,#206914,#206915,#206916,#206917,#206918,#206919,#206920,
#206921,#206922,#206923,#206924,#206925,#206926,#206927,#206928,#206929,
#206930,#206931,#206932,#206933,#206934,#206935,#206936,#206937,#206938,
#206939,#206940,#206941,#206942,#206943,#206944,#206945,#206946,#206947,
#206948,#206949,#206950,#206951,#206952,#206953,#206954,#206955,#206956,
#206957,#206958,#206959,#206960,#206961,#206962,#206963,#206964,#206965,
#206966,#206967,#206968,#206969,#206970,#206971,#206972,#206973,#206974,
#206975,#206976,#206977,#206978,#206979,#206980,#206981,#206982,#206983,
#206984,#206985,#206986,#206987,#206988,#206989,#206990,#206991,#206992,
#206993,#206994,#206995,#206996,#206997,#206998,#206999,#207000,#207001,
#207002,#207003,#207004,#207005,#207006,#207007,#207008,#207009,#207010,
#207011,#207012,#207013,#207014,#207015,#207016,#207017,#207018),
 .UNSPECIFIED.,.F.,.F.,(4,3,3,3,3,3,3,3,3,3,3,3,3,3,3,3,3,3,3,3,3,3,3,3,
3,3,3,3,3,3,3,3,3,3,3,3,3,3,3,3,3,3,3,3,3,3,3,3,3,3,3,3,3,3,3,4),(279.601746169492,
279.677896898556,279.754018294861,279.830125479646,279.906233317609,279.982356672213,
280.058551322595,280.13478287845,280.211120338645,280.276021794746,280.360241077639,
280.444333756613,280.528220382426,280.611977371813,280.695519074471,280.775391662677,
280.85275885847,280.930144447921,281.00756222971,281.085067151323,281.162621750575,
281.240283097528,281.274761530609,281.354382269353,281.43393009701,281.513417326285,
281.592856223199,281.672259016005,281.751644228904,281.831020459456,281.910398789006,
281.989790298877,282.069235533708,282.148709114489,282.228256226539,282.273501266471,
282.350216273319,282.426864185683,282.503459697422,282.58001859512,282.656555979199,
282.733097499651,282.772871134402,282.85754747261,282.942369957124,283.027392328,
283.112501209809,283.197730749184,283.272241002333,283.353797264993,283.435278204658,
283.51936137106,283.600687123572,283.686148996918,283.771610870264,283.838466116601),
 .UNSPECIFIED.);
#3441=B_SPLINE_CURVE_WITH_KNOTS('',3,(#207024,#207025,#207026,#207027,#207028,
#207029,#207030,#207031,#207032,#207033,#207034,#207035,#207036,#207037,
#207038,#207039,#207040,#207041,#207042,#207043,#207044,#207045,#207046,
#207047,#207048,#207049,#207050,#207051,#207052,#207053,#207054,#207055,
#207056,#207057,#207058,#207059,#207060,#207061,#207062,#207063,#207064,
#207065,#207066,#207067,#207068,#207069,#207070,#207071,#207072,#207073,
#207074,#207075,#207076,#207077,#207078,#207079,#207080,#207081,#207082,
#207083,#207084,#207085,#207086,#207087,#207088,#207089,#207090,#207091,
#207092,#207093,#207094,#207095,#207096,#207097,#207098,#207099,#207100,
#207101,#207102,#207103,#207104,#207105,#207106,#207107,#207108,#207109,
#207110,#207111,#207112,#207113,#207114,#207115,#207116,#207117,#207118,
#207119,#207120,#207121,#207122,#207123,#207124,#207125,#207126,#207127,
#207128,#207129,#207130,#207131,#207132,#207133,#207134,#207135,#207136,
#207137,#207138,#207139,#207140,#207141,#207142,#207143,#207144,#207145,
#207146,#207147,#207148,#207149,#207150,#207151,#207152,#207153,#207154,
#207155,#207156,#207157,#207158,#207159,#207160,#207161,#207162,#207163,
#207164,#207165,#207166,#207167,#207168,#207169,#207170,#207171,#207172,
#207173,#207174,#207175,#207176,#207177,#207178,#207179,#207180),
 .UNSPECIFIED.,.F.,.F.,(4,3,3,3,3,3,3,3,3,3,3,3,3,3,3,3,3,3,3,3,3,3,3,3,
3,3,3,3,3,3,3,3,3,3,3,3,3,3,3,3,3,3,3,3,3,3,3,3,3,3,3,3,4),(285.884931476672,
285.967393682758,286.049855540546,286.132317056887,286.214778238631,286.297239092627,
286.379699625726,286.462159844776,286.544619756627,286.627079368126,286.709538686123,
286.791997717465,286.874456469,286.956914947577,287.039373160041,287.121831113241,
287.204288814024,287.286746269236,287.369203485723,287.455216073513,287.538540767934,
287.621007373492,287.703473134843,287.785938079401,287.868402234579,287.950865627786,
288.033328286429,288.115790237913,288.19825150964,288.280712129008,288.363172123415,
288.445631520256,288.528090346925,288.610548630811,288.693006399305,288.775463679792,
288.859597593242,288.94206359154,289.024527968089,289.106990832531,289.189452294488,
289.271912463561,289.354371449336,289.436829361379,289.52242647808,289.604891215023,
289.687352987321,289.769812233412,289.852269391591,289.93473191049,290.017189581773,
290.099648372681,290.121606294983),.UNSPECIFIED.);
#3442=B_SPLINE_CURVE_WITH_KNOTS('',3,(#207181,#207182,#207183,#207184,#207185,
#207186,#207187,#207188,#207189,#207190,#207191,#207192,#207193,#207194,
#207195,#207196,#207197,#207198,#207199,#207200,#207201,#207202,#207203,
#207204,#207205,#207206,#207207,#207208,#207209,#207210,#207211,#207212,
#207213,#207214,#207215,#207216,#207217,#207218,#207219,#207220,#207221,
#207222,#207223,#207224,#207225,#207226,#207227,#207228,#207229,#207230,
#207231,#207232,#207233,#207234,#207235,#207236,#207237,#207238,#207239,
#207240,#207241,#207242,#207243,#207244,#207245,#207246,#207247,#207248,
#207249,#207250,#207251,#207252,#207253,#207254,#207255,#207256,#207257,
#207258,#207259,#207260,#207261,#207262),.UNSPECIFIED.,.F.,.F.,(4,3,3,3,
3,3,3,3,3,3,3,3,3,3,3,3,3,3,3,3,3,3,3,3,3,3,3,4),(283.837827572545,283.91532849993,
283.95329635259,284.037515635483,284.121608314457,284.20549494027,284.289251929657,
284.372793632315,284.452666220521,284.530033416314,284.607419005765,284.684836787553,
284.762341709166,284.839896308418,284.91755765537,284.952036088452,285.030919142487,
285.109727320616,285.188474397012,285.267174100836,285.345843525019,285.42449680193,
285.50314632775,285.581804494266,285.660516220107,285.739254640006,285.818075735445,
285.884931476672),.UNSPECIFIED.);
#3443=B_SPLINE_CURVE_WITH_KNOTS('',3,(#207264,#207265,#207266,#207267,#207268,
#207269,#207270,#207271,#207272,#207273,#207274,#207275,#207276,#207277,
#207278,#207279,#207280,#207281,#207282,#207283,#207284,#207285,#207286,
#207287,#207288,#207289,#207290,#207291,#207292,#207293,#207294,#207295,
#207296,#207297,#207298,#207299,#207300,#207301,#207302,#207303,#207304,
#207305,#207306,#207307,#207308,#207309,#207310,#207311,#207312,#207313,
#207314,#207315,#207316,#207317,#207318,#207319,#207320,#207321,#207322,
#207323,#207324,#207325,#207326,#207327,#207328,#207329,#207330,#207331,
#207332,#207333,#207334,#207335,#207336,#207337,#207338,#207339,#207340,
#207341,#207342,#207343,#207344,#207345),.UNSPECIFIED.,.F.,.F.,(4,3,3,3,
3,3,3,3,3,3,3,3,3,3,3,3,3,3,3,3,3,3,3,3,3,3,3,4),(283.838466116601,283.917884258935,
283.997329903907,284.076848386575,284.156407041973,284.236052385932,284.270980738195,
284.349359759065,284.427672510381,284.505933406534,284.584156824334,284.662357112494,
284.740565301659,284.818781355149,284.897018272379,284.975289062533,285.053652642006,
285.132065771465,285.210596153978,285.269720474057,285.346621849384,285.423135263213,
285.49956483542,285.575925339308,285.653176873649,285.729441285927,285.807186381299,
285.884931476671),.UNSPECIFIED.);
#3444=B_SPLINE_CURVE_WITH_KNOTS('',3,(#207346,#207347,#207348,#207349,#207350,
#207351,#207352,#207353,#207354,#207355,#207356,#207357,#207358,#207359,
#207360,#207361,#207362,#207363,#207364,#207365,#207366,#207367,#207368,
#207369,#207370,#207371,#207372,#207373,#207374,#207375,#207376,#207377,
#207378,#207379,#207380,#207381,#207382,#207383,#207384,#207385,#207386,
#207387,#207388,#207389,#207390,#207391,#207392,#207393,#207394,#207395,
#207396,#207397,#207398,#207399,#207400,#207401,#207402,#207403,#207404,
#207405,#207406,#207407,#207408,#207409,#207410,#207411,#207412,#207413,
#207414,#207415,#207416,#207417,#207418,#207419,#207420,#207421,#207422,
#207423,#207424,#207425,#207426,#207427,#207428,#207429,#207430,#207431,
#207432,#207433,#207434,#207435,#207436,#207437,#207438,#207439,#207440,
#207441,#207442,#207443,#207444,#207445,#207446,#207447,#207448,#207449,
#207450,#207451,#207452,#207453,#207454,#207455,#207456,#207457,#207458,
#207459,#207460,#207461,#207462,#207463,#207464,#207465,#207466,#207467,
#207468,#207469,#207470,#207471,#207472,#207473,#207474,#207475,#207476,
#207477,#207478,#207479,#207480,#207481,#207482,#207483,#207484,#207485,
#207486,#207487,#207488,#207489,#207490,#207491,#207492,#207493,#207494,
#207495,#207496,#207497,#207498,#207499,#207500,#207501,#207502,#207503,
#207504,#207505,#207506,#207507,#207508,#207509,#207510,#207511,#207512,
#207513,#207514),.UNSPECIFIED.,.F.,.F.,(4,3,3,3,3,3,3,3,3,3,3,3,3,3,3,3,
3,3,3,3,3,3,3,3,3,3,3,3,3,3,3,3,3,3,3,3,3,3,3,3,3,3,3,3,3,3,3,3,3,3,3,3,
3,3,3,3,4),(285.884931476781,285.969634154445,286.054843488019,286.140319279605,
286.226170945113,286.268460209919,286.346019061464,286.423485605359,286.500875508652,
286.578204383345,286.655487797488,286.73274884406,286.809999544904,286.88725394759,
286.964526099121,287.041871437259,287.119254210984,287.196743706632,287.267199945782,
287.351419228675,287.435511907649,287.519398533462,287.603155522849,287.686697225507,
287.766569813713,287.843937009506,287.921322598957,287.998740380744,288.076245302357,
288.153799901609,288.231461248562,288.265939681644,288.345560420388,288.425108248044,
288.50459547732,288.584034374233,288.66343716704,288.742822379939,288.822198610491,
288.901576940041,288.980968449912,289.060413684743,289.139887265524,289.219434377574,
289.264679417506,289.341394424355,289.418042336719,289.494637848458,289.571196746156,
289.647734130235,289.724275650687,289.764049285437,289.848685666388,289.933540329203,
290.018502099263,290.103596709339,290.121230634672),.UNSPECIFIED.);
#3445=B_SPLINE_CURVE_WITH_KNOTS('',3,(#207520,#207521,#207522,#207523,#207524,
#207525,#207526,#207527,#207528,#207529,#207530,#207531,#207532,#207533,
#207534,#207535,#207536,#207537,#207538,#207539,#207540,#207541,#207542,
#207543,#207544,#207545,#207546,#207547,#207548,#207549,#207550,#207551,
#207552,#207553,#207554,#207555,#207556,#207557,#207558,#207559,#207560,
#207561,#207562,#207563,#207564,#207565,#207566,#207567,#207568,#207569,
#207570,#207571,#207572,#207573,#207574,#207575,#207576,#207577,#207578,
#207579,#207580,#207581,#207582,#207583,#207584,#207585,#207586,#207587,
#207588,#207589,#207590,#207591,#207592,#207593,#207594,#207595,#207596,
#207597,#207598,#207599,#207600,#207601,#207602,#207603,#207604,#207605,
#207606,#207607,#207608,#207609,#207610,#207611,#207612,#207613,#207614,
#207615,#207616,#207617,#207618,#207619,#207620,#207621,#207622,#207623,
#207624,#207625,#207626,#207627,#207628,#207629,#207630,#207631,#207632,
#207633,#207634,#207635,#207636,#207637,#207638,#207639,#207640,#207641,
#207642,#207643,#207644,#207645,#207646,#207647,#207648,#207649,#207650,
#207651,#207652,#207653,#207654,#207655,#207656,#207657,#207658,#207659,
#207660,#207661,#207662,#207663,#207664,#207665,#207666,#207667,#207668,
#207669,#207670,#207671,#207672,#207673,#207674,#207675,#207676),
 .UNSPECIFIED.,.F.,.F.,(4,3,3,3,3,3,3,3,3,3,3,3,3,3,3,3,3,3,3,3,3,3,3,3,
3,3,3,3,3,3,3,3,3,3,3,3,3,3,3,3,3,3,3,3,3,3,3,3,3,3,3,3,4),(292.168116783851,
292.250578989937,292.333040847725,292.415502364066,292.49796354581,292.580424399806,
292.662884932905,292.745345151956,292.827805063806,292.910264675305,292.992723993302,
293.075183024644,293.157641776179,293.240100254756,293.32255846722,293.405016420421,
293.487474121203,293.569931576415,293.652388792902,293.738401380692,293.821726075113,
293.904192680671,293.986658442022,294.06912338658,294.151587541758,294.234050934965,
294.316513593609,294.398975545093,294.481436816819,294.563897436187,294.646357430594,
294.728816827435,294.811275654104,294.89373393799,294.976191706484,295.058648986971,
295.142782900421,295.225248898719,295.307713275268,295.39017613971,295.472637601667,
295.555097770741,295.637556756515,295.720014668558,295.805611785259,295.888076522202,
295.970538294501,296.052997540592,296.13545469877,296.217917217669,296.300374888952,
296.382833679861,296.404791602162),.UNSPECIFIED.);
#3446=B_SPLINE_CURVE_WITH_KNOTS('',3,(#207677,#207678,#207679,#207680,#207681,
#207682,#207683,#207684,#207685,#207686,#207687,#207688,#207689,#207690,
#207691,#207692,#207693,#207694,#207695,#207696,#207697,#207698,#207699,
#207700,#207701,#207702,#207703,#207704,#207705,#207706,#207707,#207708,
#207709,#207710,#207711,#207712,#207713,#207714,#207715,#207716,#207717,
#207718,#207719,#207720,#207721,#207722,#207723,#207724,#207725,#207726,
#207727,#207728,#207729,#207730,#207731,#207732,#207733,#207734,#207735,
#207736,#207737,#207738,#207739,#207740,#207741,#207742,#207743,#207744,
#207745,#207746,#207747,#207748,#207749,#207750,#207751,#207752),
 .UNSPECIFIED.,.F.,.F.,(4,3,3,3,3,3,3,3,3,3,3,3,3,3,3,3,3,3,3,3,3,3,3,3,
3,4),(290.121606294983,290.204067898741,290.28652883662,290.368989136018,
290.451448824331,290.533907928953,290.616366477277,290.698824496691,290.781282014584,
290.867959187655,290.950425973264,291.032891086395,291.115354636702,291.197816733816,
291.280277487348,291.36273700689,291.445195402017,291.527652782288,291.610119168107,
291.692582369731,291.77504282568,291.857500974316,291.939966578328,292.022426456905,
292.104890568642,292.168116783727),.UNSPECIFIED.);
#3447=B_SPLINE_CURVE_WITH_KNOTS('',3,(#207754,#207755,#207756,#207757,#207758,
#207759,#207760,#207761,#207762,#207763,#207764,#207765,#207766,#207767,
#207768,#207769,#207770,#207771,#207772,#207773,#207774,#207775,#207776,
#207777,#207778,#207779,#207780,#207781,#207782,#207783,#207784,#207785,
#207786,#207787,#207788,#207789,#207790,#207791,#207792,#207793,#207794,
#207795,#207796,#207797,#207798,#207799,#207800,#207801,#207802,#207803,
#207804,#207805,#207806,#207807,#207808,#207809,#207810,#207811,#207812,
#207813,#207814,#207815,#207816,#207817,#207818,#207819,#207820,#207821,
#207822,#207823,#207824,#207825,#207826,#207827,#207828,#207829,#207830,
#207831,#207832,#207833,#207834,#207835),.UNSPECIFIED.,.F.,.F.,(4,3,3,3,
3,3,3,3,3,3,3,3,3,3,3,3,3,3,3,3,3,3,3,3,3,3,3,4),(290.121230634672,290.206467138343,
290.263419153368,290.344975416028,290.426456355693,290.510539522095,290.591865274607,
290.677327147953,290.762789021299,290.842192362183,290.921614133346,291.001065110987,
291.080589277207,291.160155187752,291.239805035956,291.26215888923,291.339336164723,
291.416444333208,291.493499236476,291.570516676688,291.647524024901,291.724528938895,
291.801545691994,291.878588561729,291.955715695224,292.032887936344,292.110173370506,
292.168116783776),.UNSPECIFIED.);
#3448=B_SPLINE_CURVE_WITH_KNOTS('',3,(#207836,#207837,#207838,#207839,#207840,
#207841,#207842,#207843,#207844,#207845,#207846,#207847,#207848,#207849,
#207850,#207851,#207852,#207853,#207854,#207855,#207856,#207857,#207858,
#207859,#207860,#207861,#207862,#207863,#207864,#207865,#207866,#207867,
#207868,#207869,#207870,#207871,#207872,#207873,#207874,#207875,#207876,
#207877,#207878,#207879,#207880,#207881,#207882,#207883,#207884,#207885,
#207886,#207887,#207888,#207889,#207890,#207891,#207892,#207893,#207894,
#207895,#207896,#207897,#207898,#207899,#207900,#207901,#207902,#207903,
#207904,#207905,#207906,#207907,#207908,#207909,#207910,#207911,#207912,
#207913,#207914,#207915,#207916,#207917,#207918,#207919,#207920,#207921,
#207922,#207923,#207924,#207925,#207926,#207927,#207928,#207929,#207930,
#207931,#207932,#207933,#207934,#207935,#207936,#207937,#207938,#207939,
#207940,#207941,#207942,#207943,#207944,#207945,#207946,#207947,#207948,
#207949,#207950,#207951,#207952,#207953,#207954,#207955,#207956,#207957,
#207958,#207959,#207960,#207961,#207962,#207963,#207964,#207965,#207966,
#207967,#207968,#207969,#207970,#207971,#207972,#207973,#207974,#207975,
#207976,#207977,#207978,#207979,#207980,#207981,#207982,#207983,#207984,
#207985,#207986,#207987,#207988,#207989,#207990,#207991,#207992,#207993,
#207994,#207995,#207996,#207997,#207998,#207999,#208000,#208001,#208002,
#208003,#208004),.UNSPECIFIED.,.F.,.F.,(4,3,3,3,3,3,3,3,3,3,3,3,3,3,3,3,
3,3,3,3,3,3,3,3,3,3,3,3,3,3,3,3,3,3,3,3,3,3,3,3,3,3,3,3,3,3,3,3,3,3,3,3,
3,3,3,3,4),(292.168116783851,292.260898625093,292.336955131847,292.412915949841,
292.48879787046,292.564617603967,292.640391798298,292.71779761863,292.793545374746,
292.869300380274,292.945077645504,293.023717824367,293.099627010836,293.175593002778,
293.251665200388,293.259638360955,293.3371972125,293.414663756395,293.492053659688,
293.569382534381,293.646665948524,293.723926995096,293.80117769594,293.878432098625,
293.955704250157,294.033049588295,294.110432362019,294.187921857667,294.258378096817,
294.34259737971,294.426690058683,294.510576684497,294.594333673883,294.677875376541,
294.757747964748,294.835115160541,294.912500749992,294.98991853178,295.067423453393,
295.144978052645,295.222639399597,295.257117832679,295.336738571423,295.416286399079,
295.495773628355,295.575212525268,295.654615318075,295.734000530974,295.813376761526,
295.892755091076,295.972146600947,296.051591835778,296.131065416559,296.210612528609,
296.255857568541,296.332566656646,296.405314229998),.UNSPECIFIED.);
#3449=B_SPLINE_CURVE_WITH_KNOTS('',3,(#208010,#208011,#208012,#208013,#208014,
#208015,#208016,#208017,#208018,#208019,#208020,#208021,#208022,#208023,
#208024,#208025,#208026,#208027,#208028,#208029,#208030,#208031,#208032,
#208033,#208034,#208035,#208036,#208037,#208038,#208039,#208040,#208041,
#208042,#208043,#208044,#208045,#208046,#208047,#208048,#208049,#208050,
#208051,#208052,#208053,#208054,#208055,#208056,#208057,#208058,#208059,
#208060,#208061,#208062,#208063,#208064,#208065,#208066,#208067,#208068,
#208069,#208070,#208071,#208072,#208073,#208074,#208075,#208076,#208077,
#208078,#208079,#208080,#208081,#208082,#208083,#208084,#208085,#208086,
#208087,#208088,#208089,#208090,#208091,#208092,#208093,#208094,#208095,
#208096,#208097,#208098,#208099,#208100,#208101,#208102,#208103,#208104,
#208105,#208106,#208107,#208108,#208109,#208110,#208111,#208112,#208113,
#208114,#208115,#208116,#208117,#208118,#208119,#208120,#208121,#208122,
#208123,#208124,#208125,#208126,#208127,#208128,#208129,#208130,#208131,
#208132,#208133,#208134,#208135,#208136,#208137,#208138,#208139,#208140,
#208141,#208142,#208143,#208144,#208145,#208146,#208147,#208148,#208149,
#208150,#208151,#208152,#208153,#208154,#208155,#208156,#208157,#208158,
#208159,#208160,#208161,#208162,#208163,#208164,#208165,#208166,#208167,
#208168,#208169,#208170,#208171,#208172,#208173,#208174,#208175,#208176,
#208177,#208178),.UNSPECIFIED.,.F.,.F.,(4,3,3,3,3,3,3,3,3,3,3,3,3,3,3,3,
3,3,3,3,3,3,3,3,3,3,3,3,3,3,3,3,3,3,3,3,3,3,3,3,3,3,3,3,3,3,3,3,3,3,3,3,
3,3,3,3,4),(298.451450161677,298.529117122841,298.606810096865,298.684542527595,
298.76236807435,298.840249052095,298.918235314131,298.934392390522,299.014013129267,
299.093560956922,299.173048186198,299.252487083111,299.331889875918,299.411275088816,
299.490651319369,299.570029648919,299.64942115879,299.728866393621,299.808339974402,
299.887887086451,299.933132126385,300.009847133234,300.086495045598,300.163090557338,
300.239649455036,300.316186839115,300.392728359568,300.432501994316,300.517178332524,
300.602000817038,300.687023187913,300.772132069722,300.857361609096,300.931871862247,
301.013428124907,301.094909064573,301.178992230974,301.260317983486,301.345779856832,
301.431241730178,301.510645071062,301.590066842225,301.669517819866,301.749041986087,
301.828607896631,301.908257744834,301.930611598109,302.008999852534,302.087319417554,
302.165577787803,302.243801614261,302.322003913219,302.400197685959,302.47841807422,
302.556651617678,302.634942192783,302.687552226885),.UNSPECIFIED.);
#3450=B_SPLINE_CURVE_WITH_KNOTS('',3,(#208179,#208180,#208181,#208182,#208183,
#208184,#208185,#208186,#208187,#208188,#208189,#208190,#208191,#208192,
#208193,#208194,#208195,#208196,#208197,#208198,#208199,#208200,#208201,
#208202,#208203,#208204,#208205,#208206,#208207,#208208,#208209,#208210,
#208211,#208212,#208213,#208214,#208215,#208216,#208217,#208218,#208219,
#208220,#208221,#208222,#208223,#208224,#208225,#208226,#208227,#208228,
#208229,#208230,#208231,#208232,#208233,#208234,#208235,#208236,#208237,
#208238,#208239,#208240,#208241,#208242,#208243,#208244,#208245,#208246,
#208247,#208248,#208249,#208250,#208251,#208252,#208253,#208254),
 .UNSPECIFIED.,.F.,.F.,(4,3,3,3,3,3,3,3,3,3,3,3,3,3,3,3,3,3,3,3,3,3,3,3,
3,4),(296.404791602162,296.487253205921,296.5697141438,296.652174443198,
296.734634131511,296.817093236133,296.899551784456,296.98200980387,297.064467321763,
297.151144494843,297.233611280451,297.316076393582,297.398539943889,297.481002041003,
297.563462794535,297.645922314077,297.728380709205,297.810838089475,297.893304475295,
297.975767676919,298.058228132867,298.140686281504,298.223151885515,298.305611764093,
298.388075875829,298.451302091031),.UNSPECIFIED.);
#3451=B_SPLINE_CURVE_WITH_KNOTS('',3,(#208256,#208257,#208258,#208259,#208260,
#208261,#208262,#208263,#208264,#208265,#208266,#208267,#208268,#208269,
#208270,#208271,#208272,#208273,#208274,#208275,#208276,#208277,#208278,
#208279,#208280,#208281,#208282,#208283,#208284,#208285,#208286,#208287,
#208288,#208289,#208290,#208291,#208292,#208293,#208294,#208295,#208296,
#208297,#208298,#208299,#208300,#208301,#208302,#208303,#208304,#208305,
#208306,#208307,#208308,#208309,#208310,#208311,#208312,#208313,#208314,
#208315,#208316,#208317,#208318,#208319,#208320,#208321,#208322,#208323,
#208324,#208325,#208326,#208327,#208328,#208329,#208330,#208331,#208332,
#208333,#208334),.UNSPECIFIED.,.F.,.F.,(4,3,3,3,3,3,3,3,3,3,3,3,3,3,3,3,
3,3,3,3,3,3,3,3,3,3,4),(296.405314229998,296.481912058359,296.558472403764,
296.635010567897,296.711552741933,296.755227436472,296.83990377468,296.924726259194,
297.009748630071,297.094857511879,297.180087051255,297.254597304403,297.336153567063,
297.417634506729,297.50171767313,297.583043425642,297.668505298989,297.753967172335,
297.83337051322,297.912792284383,297.992243262024,298.071767428245,298.15133333879,
298.230983186994,298.253337040266,298.356769259851,298.451302090931),
 .UNSPECIFIED.);
#3452=B_SPLINE_CURVE_WITH_KNOTS('',3,(#208335,#208336,#208337,#208338,#208339,
#208340,#208341,#208342,#208343,#208344,#208345,#208346,#208347,#208348,
#208349,#208350,#208351,#208352,#208353,#208354,#208355,#208356,#208357,
#208358,#208359,#208360,#208361,#208362,#208363,#208364,#208365,#208366,
#208367,#208368,#208369,#208370,#208371,#208372,#208373,#208374,#208375,
#208376,#208377,#208378,#208379,#208380,#208381,#208382,#208383,#208384,
#208385,#208386,#208387,#208388,#208389,#208390,#208391,#208392,#208393,
#208394,#208395,#208396,#208397,#208398,#208399,#208400,#208401,#208402,
#208403,#208404,#208405,#208406,#208407,#208408,#208409,#208410,#208411,
#208412,#208413,#208414,#208415,#208416,#208417,#208418,#208419,#208420,
#208421,#208422,#208423,#208424,#208425,#208426,#208427,#208428,#208429,
#208430,#208431,#208432,#208433,#208434,#208435,#208436,#208437,#208438,
#208439,#208440,#208441,#208442,#208443,#208444,#208445,#208446,#208447,
#208448,#208449,#208450,#208451,#208452,#208453,#208454,#208455,#208456,
#208457,#208458,#208459,#208460,#208461,#208462,#208463,#208464,#208465,
#208466,#208467,#208468,#208469,#208470,#208471,#208472,#208473,#208474,
#208475,#208476,#208477,#208478,#208479,#208480,#208481,#208482,#208483,
#208484,#208485,#208486,#208487,#208488,#208489,#208490,#208491,#208492,
#208493,#208494,#208495,#208496,#208497,#208498,#208499,#208500,#208501,
#208502,#208503,#208504,#208505,#208506),.UNSPECIFIED.,.F.,.F.,(4,3,3,3,
3,3,3,3,3,3,3,3,3,3,3,3,3,3,3,3,3,3,3,3,3,3,3,3,3,3,3,3,3,3,3,3,3,3,3,3,
3,3,3,3,3,3,3,3,3,3,3,3,3,3,3,3,3,4),(298.451302091031,298.529010392149,
298.606680654895,298.687355170049,298.765010704575,298.842676268073,298.920365536129,
298.998092194966,299.075910410184,299.153782671309,299.231760731932,299.252076776128,
299.328133282882,299.404094100876,299.479976021495,299.555795755002,299.631569949333,
299.708975769665,299.784723525781,299.860478531309,299.936255796539,300.014895975402,
300.09080516187,300.166771153813,300.242843351423,300.25081651199,300.328375363535,
300.40584190743,300.483231810723,300.560560685416,300.637844099558,300.71510514613,
300.792355846974,300.86961024966,300.946882401192,301.024227739329,301.101610513054,
301.179100008702,301.249556247852,301.333775530745,301.417868209718,301.501754835531,
301.585511824918,301.669053527576,301.748926115783,301.826293311576,301.903678901027,
301.981096682815,302.058601604427,302.13615620368,302.213817550632,302.248295983714,
302.327921744234,302.407476581218,302.486958355055,302.56639657612,302.645798576232,
302.688221398627),.UNSPECIFIED.);
#3453=B_SPLINE_CURVE_WITH_KNOTS('',3,(#208512,#208513,#208514,#208515,#208516,
#208517,#208518,#208519,#208520,#208521,#208522,#208523,#208524,#208525,
#208526,#208527,#208528,#208529,#208530,#208531,#208532,#208533,#208534,
#208535,#208536,#208537,#208538,#208539,#208540,#208541,#208542,#208543,
#208544,#208545,#208546,#208547,#208548,#208549,#208550,#208551,#208552,
#208553,#208554,#208555,#208556,#208557,#208558,#208559,#208560,#208561,
#208562,#208563,#208564,#208565,#208566,#208567,#208568,#208569,#208570,
#208571,#208572,#208573,#208574,#208575,#208576,#208577,#208578,#208579,
#208580,#208581,#208582,#208583,#208584,#208585,#208586,#208587,#208588,
#208589,#208590,#208591,#208592,#208593,#208594,#208595,#208596,#208597,
#208598,#208599,#208600,#208601,#208602,#208603,#208604,#208605,#208606,
#208607,#208608,#208609,#208610,#208611,#208612,#208613,#208614,#208615,
#208616,#208617,#208618,#208619,#208620,#208621,#208622,#208623,#208624,
#208625,#208626,#208627,#208628,#208629,#208630,#208631,#208632,#208633,
#208634,#208635,#208636,#208637,#208638,#208639,#208640,#208641,#208642,
#208643,#208644,#208645,#208646,#208647,#208648,#208649,#208650,#208651,
#208652,#208653,#208654,#208655,#208656,#208657,#208658,#208659,#208660,
#208661,#208662,#208663,#208664,#208665,#208666,#208667,#208668,#208669,
#208670,#208671,#208672,#208673,#208674,#208675,#208676,#208677),
 .UNSPECIFIED.,.F.,.F.,(4,3,3,3,3,3,3,3,3,3,3,3,3,3,3,3,3,3,3,3,3,3,3,3,
3,3,3,3,3,3,3,3,3,3,3,3,3,3,3,3,3,3,3,3,3,3,3,3,3,3,3,3,3,3,3,4),(304.734487398304,
304.836061119486,304.926830805695,305.011050088588,305.095142767561,305.179029393374,
305.262786382761,305.346328085419,305.426200673627,305.50356786942,305.580953458871,
305.658371240659,305.735876162272,305.813430761524,305.891092108477,305.925570541558,
306.005191280302,306.084739107958,306.164226337234,306.243665234147,306.323068026953,
306.402453239852,306.481829470404,306.561207799955,306.640599309826,306.720044544657,
306.799518125437,306.879065237487,306.92431027742,307.001025284269,307.077673196633,
307.154268708372,307.23082760607,307.307364990149,307.383906510601,307.423680145351,
307.508356483559,307.593178968073,307.678201338949,307.763310220757,307.848539760132,
307.923050013282,308.004606275942,308.086087215608,308.170170382009,308.251496134521,
308.336958007867,308.422419881213,308.501823222097,308.581244993259,308.6606959709,
308.74022013712,308.819786047665,308.899435895868,308.921789749144,308.971301374524),
 .UNSPECIFIED.);
#3454=B_SPLINE_CURVE_WITH_KNOTS('',3,(#208678,#208679,#208680,#208681,#208682,
#208683,#208684,#208685,#208686,#208687,#208688,#208689,#208690,#208691,
#208692,#208693,#208694,#208695,#208696,#208697,#208698,#208699,#208700,
#208701,#208702,#208703,#208704,#208705,#208706,#208707,#208708,#208709,
#208710,#208711,#208712,#208713,#208714,#208715,#208716,#208717,#208718,
#208719,#208720,#208721,#208722,#208723,#208724,#208725,#208726,#208727,
#208728,#208729,#208730,#208731,#208732,#208733,#208734,#208735,#208736,
#208737,#208738,#208739,#208740,#208741,#208742,#208743,#208744,#208745,
#208746,#208747,#208748,#208749,#208750,#208751,#208752,#208753,#208754,
#208755,#208756,#208757,#208758,#208759,#208760,#208761,#208762),
 .UNSPECIFIED.,.F.,.F.,(4,3,3,3,3,3,3,3,3,3,3,3,3,3,3,3,3,3,3,3,3,3,3,3,
3,3,3,3,4),(302.687552226885,302.76594779,302.847649561986,302.929351333971,
303.005407840725,303.081368658719,303.157250579338,303.233070312845,303.308844507176,
303.386250327508,303.461998083623,303.537753089152,303.613530354382,303.692170533245,
303.768079719713,303.844045711655,303.920117909266,303.928091069833,304.005110795359,
304.082036975103,304.158885782019,304.235664478819,304.312404053226,304.389119020399,
304.465823878307,304.542555067192,304.61930074801,304.696103995048,304.73448739821),
 .UNSPECIFIED.);
#3455=B_SPLINE_CURVE_WITH_KNOTS('',3,(#208764,#208765,#208766,#208767,#208768,
#208769,#208770,#208771,#208772,#208773,#208774,#208775,#208776,#208777,
#208778,#208779,#208780,#208781,#208782,#208783,#208784,#208785,#208786,
#208787,#208788,#208789,#208790,#208791,#208792,#208793,#208794,#208795,
#208796,#208797,#208798,#208799,#208800,#208801,#208802,#208803,#208804,
#208805,#208806,#208807,#208808,#208809,#208810,#208811,#208812,#208813,
#208814,#208815,#208816,#208817,#208818,#208819,#208820,#208821,#208822,
#208823,#208824,#208825,#208826,#208827,#208828,#208829,#208830,#208831,
#208832,#208833,#208834,#208835,#208836,#208837,#208838,#208839,#208840,
#208841,#208842),.UNSPECIFIED.,.F.,.F.,(4,3,3,3,3,3,3,3,3,3,3,3,3,3,3,3,
3,3,3,3,3,3,3,3,3,3,4),(302.688221398627,302.76760043219,302.846976406087,
302.926360400764,303.006529230468,303.085988619068,303.166512169322,303.247035719577,
303.323750726426,303.40039863879,303.476994150529,303.553553048227,303.630090432306,
303.706631952759,303.746405587508,303.831081925716,303.91590441023,304.000926781105,
304.086035662914,304.171265202288,304.245775455439,304.327392409246,304.408933645812,
304.490379591283,304.571766001586,304.653126699898,304.73448739821),
 .UNSPECIFIED.);
#3456=B_SPLINE_CURVE_WITH_KNOTS('',3,(#208843,#208844,#208845,#208846,#208847,
#208848,#208849,#208850,#208851,#208852,#208853,#208854,#208855,#208856,
#208857,#208858,#208859,#208860,#208861,#208862,#208863,#208864,#208865,
#208866,#208867,#208868,#208869,#208870,#208871,#208872,#208873,#208874,
#208875,#208876,#208877,#208878,#208879,#208880,#208881,#208882,#208883,
#208884,#208885,#208886,#208887,#208888,#208889,#208890,#208891,#208892,
#208893,#208894,#208895,#208896,#208897,#208898,#208899,#208900,#208901,
#208902,#208903,#208904,#208905,#208906,#208907,#208908,#208909,#208910,
#208911,#208912,#208913,#208914,#208915,#208916,#208917,#208918,#208919,
#208920,#208921,#208922,#208923,#208924,#208925,#208926,#208927,#208928,
#208929,#208930,#208931,#208932,#208933,#208934,#208935,#208936,#208937,
#208938,#208939,#208940,#208941,#208942,#208943,#208944,#208945,#208946,
#208947,#208948,#208949,#208950,#208951,#208952,#208953,#208954,#208955,
#208956,#208957,#208958,#208959,#208960,#208961,#208962,#208963,#208964,
#208965,#208966,#208967,#208968,#208969,#208970,#208971,#208972,#208973,
#208974,#208975,#208976,#208977,#208978,#208979,#208980,#208981,#208982,
#208983,#208984,#208985,#208986,#208987,#208988,#208989,#208990,#208991,
#208992,#208993,#208994,#208995,#208996,#208997,#208998,#208999),
 .UNSPECIFIED.,.F.,.F.,(4,3,3,3,3,3,3,3,3,3,3,3,3,3,3,3,3,3,3,3,3,3,3,3,
3,3,3,3,3,3,3,3,3,3,3,3,3,3,3,3,3,3,3,3,3,3,3,3,3,3,3,3,4),(304.73448739821,
304.816949604296,304.899411462084,304.981872978425,305.064334160169,305.146795014165,
305.229255547264,305.311715766314,305.394175678165,305.476635289664,305.559094607661,
305.641553639003,305.724012390538,305.806470869114,305.888929081579,305.971387034779,
306.053844735562,306.136302190773,306.218759407261,306.30477199505,306.388096689471,
306.47056329503,306.55302905638,306.635494000938,306.717958156116,306.800421549324,
306.882884207967,306.965346159451,307.047807431178,307.130268050546,307.212728044953,
307.295187441794,307.377646268463,307.460104552349,307.542562320842,307.62501960133,
307.70915351478,307.791619513078,307.874083889627,307.956546754069,308.039008216026,
308.121468385099,308.203927370874,308.286385282917,308.371982399617,308.454447136561,
308.536908908859,308.61936815495,308.701825313129,308.784287832028,308.866745503311,
308.94920429422,308.971162216521),.UNSPECIFIED.);
#3457=B_SPLINE_CURVE_WITH_KNOTS('',3,(#209005,#209006,#209007,#209008,#209009,
#209010,#209011,#209012,#209013,#209014,#209015,#209016,#209017,#209018,
#209019,#209020,#209021,#209022,#209023,#209024,#209025,#209026,#209027,
#209028,#209029,#209030,#209031,#209032,#209033,#209034,#209035,#209036,
#209037,#209038,#209039,#209040,#209041,#209042,#209043,#209044,#209045,
#209046,#209047,#209048,#209049,#209050,#209051,#209052,#209053,#209054,
#209055,#209056,#209057,#209058,#209059,#209060,#209061,#209062,#209063,
#209064,#209065,#209066,#209067,#209068,#209069,#209070,#209071,#209072,
#209073,#209074,#209075,#209076,#209077,#209078,#209079,#209080,#209081,
#209082,#209083,#209084,#209085,#209086,#209087,#209088,#209089,#209090,
#209091,#209092,#209093,#209094,#209095,#209096,#209097,#209098,#209099,
#209100,#209101,#209102,#209103,#209104,#209105,#209106,#209107,#209108,
#209109,#209110,#209111,#209112,#209113,#209114,#209115,#209116,#209117,
#209118,#209119,#209120,#209121,#209122,#209123,#209124,#209125,#209126,
#209127,#209128,#209129,#209130,#209131,#209132,#209133,#209134,#209135,
#209136,#209137,#209138,#209139,#209140,#209141,#209142,#209143,#209144,
#209145,#209146,#209147,#209148,#209149,#209150,#209151,#209152,#209153,
#209154,#209155,#209156,#209157,#209158,#209159,#209160,#209161,#209162,
#209163,#209164,#209165,#209166,#209167,#209168,#209169,#209170,#209171,
#209172,#209173),.UNSPECIFIED.,.F.,.F.,(4,3,3,3,3,3,3,3,3,3,3,3,3,3,3,3,
3,3,3,3,3,3,3,3,3,3,3,3,3,3,3,3,3,3,3,3,3,3,3,3,3,3,3,3,3,3,3,3,3,3,3,3,
3,3,3,3,4),(311.01767270548,311.093953767193,311.170148397586,311.246273239023,
311.322344867964,311.398384892228,311.474409360757,311.550433196865,311.626471321894,
311.702578658091,311.778721948788,311.854968836195,311.918008956731,312.002228239624,
312.086320918597,312.170207544411,312.253964533797,312.337506236455,312.417378824662,
312.494746020455,312.572131609906,312.649549391694,312.727054313307,312.804608912559,
312.882270259511,312.916748692593,312.996369431337,313.075917258994,313.155404488269,
313.234843385183,313.314246177989,313.393631390888,313.47300762144,313.55238595099,
313.631777460861,313.711222695692,313.790696276473,313.870243388523,313.915488428455,
313.992203435304,314.068851347668,314.145446859406,314.222005757105,314.298543141184,
314.375084661636,314.414858296386,314.499534634594,314.584357119108,314.669379489983,
314.754488371792,314.839717911167,314.914228164317,314.999378556216,315.080847967622,
315.162254743281,315.243589025594,315.254829731915),.UNSPECIFIED.);
#3458=B_SPLINE_CURVE_WITH_KNOTS('',3,(#209174,#209175,#209176,#209177,#209178,
#209179,#209180,#209181,#209182,#209183,#209184,#209185,#209186,#209187,
#209188,#209189,#209190,#209191,#209192,#209193,#209194,#209195,#209196,
#209197,#209198,#209199,#209200,#209201,#209202,#209203,#209204,#209205,
#209206,#209207,#209208,#209209,#209210,#209211,#209212,#209213,#209214,
#209215,#209216,#209217,#209218,#209219,#209220,#209221,#209222,#209223,
#209224,#209225,#209226,#209227,#209228,#209229,#209230,#209231,#209232,
#209233,#209234,#209235,#209236,#209237,#209238,#209239,#209240,#209241,
#209242,#209243,#209244,#209245,#209246,#209247,#209248,#209249,#209250,
#209251,#209252,#209253,#209254,#209255),.UNSPECIFIED.,.F.,.F.,(4,3,3,3,
3,3,3,3,3,3,3,3,3,3,3,3,3,3,3,3,3,3,3,3,3,3,3,4),(308.971301374524,309.049636861122,
309.127915186984,309.206150741656,309.284357883102,309.36387933334,309.44209114063,
309.520319240875,309.598576638973,309.679064850481,309.757460633806,309.838995059406,
309.920529485006,309.99658599176,310.072546809754,310.148428730373,310.22424846388,
310.300022658211,310.377428478544,310.453176234659,310.528931240187,310.604708505418,
310.68334868428,310.759257870749,310.835223862692,310.911296060302,310.919269220869,
311.01767270539),.UNSPECIFIED.);
#3459=B_SPLINE_CURVE_WITH_KNOTS('',3,(#209257,#209258,#209259,#209260,#209261,
#209262,#209263,#209264,#209265,#209266,#209267,#209268,#209269,#209270,
#209271,#209272,#209273,#209274,#209275,#209276,#209277,#209278,#209279,
#209280,#209281,#209282,#209283,#209284,#209285,#209286,#209287,#209288,
#209289,#209290,#209291,#209292,#209293,#209294,#209295,#209296,#209297,
#209298,#209299,#209300,#209301,#209302,#209303,#209304,#209305,#209306,
#209307,#209308,#209309,#209310,#209311,#209312,#209313,#209314,#209315,
#209316,#209317,#209318,#209319,#209320,#209321,#209322,#209323,#209324,
#209325,#209326,#209327,#209328,#209329,#209330,#209331,#209332),
 .UNSPECIFIED.,.F.,.F.,(4,3,3,3,3,3,3,3,3,3,3,3,3,3,3,3,3,3,3,3,3,3,3,3,
3,4),(308.971162216521,309.05362382028,309.136084758159,309.218545057557,
309.30100474587,309.383463850492,309.465922398815,309.548380418229,309.630837936122,
309.717515109202,309.79998189481,309.882447007941,309.964910558248,310.047372655362,
310.129833408894,310.212292928437,310.294751323564,310.377208703835,310.459675089654,
310.542138291278,310.624598747227,310.707056895863,310.789522499874,310.871982378452,
310.954446490188,311.01767270539),.UNSPECIFIED.);
#3460=B_SPLINE_CURVE_WITH_KNOTS('',3,(#209333,#209334,#209335,#209336,#209337,
#209338,#209339,#209340,#209341,#209342,#209343,#209344,#209345,#209346,
#209347,#209348,#209349,#209350,#209351,#209352,#209353,#209354,#209355,
#209356,#209357,#209358,#209359,#209360,#209361,#209362,#209363,#209364,
#209365,#209366,#209367,#209368,#209369,#209370,#209371,#209372,#209373,
#209374,#209375,#209376,#209377,#209378,#209379,#209380,#209381,#209382,
#209383,#209384,#209385,#209386,#209387,#209388,#209389,#209390,#209391,
#209392,#209393,#209394,#209395,#209396,#209397,#209398,#209399,#209400,
#209401,#209402,#209403,#209404,#209405,#209406,#209407,#209408,#209409,
#209410,#209411,#209412,#209413,#209414,#209415,#209416,#209417,#209418,
#209419,#209420,#209421,#209422,#209423,#209424,#209425,#209426,#209427,
#209428,#209429,#209430,#209431,#209432,#209433,#209434,#209435,#209436,
#209437,#209438,#209439,#209440,#209441,#209442,#209443,#209444,#209445,
#209446,#209447,#209448,#209449,#209450,#209451,#209452,#209453,#209454,
#209455,#209456,#209457,#209458,#209459,#209460,#209461,#209462,#209463,
#209464,#209465,#209466,#209467,#209468,#209469,#209470,#209471,#209472,
#209473,#209474,#209475,#209476,#209477,#209478,#209479,#209480,#209481,
#209482,#209483,#209484,#209485,#209486,#209487,#209488,#209489),
 .UNSPECIFIED.,.F.,.F.,(4,3,3,3,3,3,3,3,3,3,3,3,3,3,3,3,3,3,3,3,3,3,3,3,
3,3,3,3,3,3,3,3,3,3,3,3,3,3,3,3,3,3,3,3,3,3,3,3,3,3,3,3,4),(311.017672705512,
311.100134911598,311.182596769386,311.265058285727,311.347519467471,311.429980321467,
311.512440854566,311.594901073616,311.677360985467,311.759820596966,311.842279914962,
311.924738946305,312.00719769784,312.089656176416,312.172114388881,312.254572342081,
312.337030042864,312.419487498075,312.501944714563,312.587957302349,312.671281996766,
312.753748602324,312.836214363675,312.918679308233,313.001143463411,313.083606856618,
313.166069515262,313.248531466746,313.330992738472,313.41345335784,313.495913352248,
313.578372749089,313.660831575757,313.743289859644,313.825747628137,313.908204908625,
313.992338822067,314.074804820365,314.157269196914,314.239732061356,314.322193523313,
314.404653692387,314.487112678161,314.569570590204,314.655167706891,314.737632443835,
314.820094216133,314.902553462224,314.985010620403,315.067473139302,315.149930810585,
315.232389601493,315.254347523701),.UNSPECIFIED.);
#3461=B_SPLINE_CURVE_WITH_KNOTS('',3,(#209495,#209496,#209497,#209498,#209499,
#209500,#209501,#209502,#209503,#209504,#209505,#209506,#209507,#209508,
#209509,#209510,#209511,#209512,#209513,#209514,#209515,#209516,#209517,
#209518,#209519,#209520,#209521,#209522,#209523,#209524,#209525,#209526,
#209527,#209528,#209529,#209530,#209531,#209532,#209533,#209534,#209535,
#209536,#209537,#209538,#209539,#209540,#209541,#209542,#209543,#209544,
#209545,#209546,#209547,#209548,#209549,#209550,#209551,#209552,#209553,
#209554,#209555,#209556,#209557,#209558,#209559,#209560,#209561,#209562,
#209563,#209564,#209565,#209566,#209567,#209568,#209569,#209570,#209571,
#209572,#209573,#209574,#209575,#209576,#209577,#209578,#209579,#209580,
#209581,#209582,#209583,#209584,#209585,#209586,#209587,#209588,#209589,
#209590,#209591,#209592,#209593,#209594,#209595,#209596,#209597,#209598,
#209599,#209600,#209601,#209602,#209603,#209604,#209605,#209606,#209607,
#209608,#209609,#209610,#209611,#209612,#209613,#209614,#209615,#209616,
#209617,#209618,#209619,#209620,#209621,#209622,#209623,#209624,#209625,
#209626,#209627,#209628,#209629,#209630,#209631,#209632,#209633,#209634,
#209635,#209636,#209637,#209638,#209639,#209640,#209641,#209642,#209643,
#209644,#209645,#209646,#209647,#209648,#209649,#209650,#209651),
 .UNSPECIFIED.,.F.,.F.,(4,3,3,3,3,3,3,3,3,3,3,3,3,3,3,3,3,3,3,3,3,3,3,3,
3,3,3,3,3,3,3,3,3,3,3,3,3,3,3,3,3,3,3,3,3,3,3,3,3,3,3,3,4),(317.300858012569,
317.383320218654,317.465782076443,317.548243592784,317.630704774528,317.713165628524,
317.795626161623,317.878086380673,317.960546292524,318.043005904023,318.12546522202,
318.207924253362,318.290383004897,318.372841483474,318.455299695938,318.537757649138,
318.620215349921,318.702672805133,318.785130021621,318.87114260941,318.954467303831,
319.036933909389,319.11939967074,319.201864615298,319.284328770476,319.366792163684,
319.449254822327,319.531716773811,319.614178045537,319.696638664905,319.779098659313,
319.861558056154,319.944016882822,320.026475166709,320.108932935202,320.19139021569,
320.275524129139,320.357990127438,320.440454503986,320.522917368428,320.605378830385,
320.687838999459,320.770297985234,320.852755897277,320.938353013977,321.020817750921,
321.103279523219,321.18573876931,321.268195927489,321.350658446387,321.433116117671,
321.515574908579,321.53753283088),.UNSPECIFIED.);
#3462=B_SPLINE_CURVE_WITH_KNOTS('',3,(#209652,#209653,#209654,#209655,#209656,
#209657,#209658,#209659,#209660,#209661,#209662,#209663,#209664,#209665,
#209666,#209667,#209668,#209669,#209670,#209671,#209672,#209673,#209674,
#209675,#209676,#209677,#209678,#209679,#209680,#209681,#209682,#209683,
#209684,#209685,#209686,#209687,#209688,#209689,#209690,#209691,#209692,
#209693,#209694,#209695,#209696,#209697,#209698,#209699,#209700,#209701,
#209702,#209703,#209704,#209705,#209706,#209707,#209708,#209709,#209710,
#209711,#209712,#209713,#209714,#209715,#209716,#209717,#209718,#209719,
#209720,#209721,#209722,#209723,#209724,#209725,#209726,#209727,#209728,
#209729,#209730,#209731,#209732,#209733),.UNSPECIFIED.,.F.,.F.,(4,3,3,3,
3,3,3,3,3,3,3,3,3,3,3,3,3,3,3,3,3,3,3,3,3,3,3,4),(315.254829731915,315.336077616719,
315.413598032248,315.493001373132,315.572423144295,315.651874121936,315.731398288156,
315.810964198701,315.890614046905,315.912967900179,315.991346921049,316.069659672365,
316.147920568519,316.226143986317,316.304344274478,316.382552463643,316.460768517133,
316.539005434362,316.617276224517,316.69563980399,316.774052933449,316.852583315962,
316.911707636042,316.996155050202,317.080227623508,317.164072839184,317.247562802763,
317.300858012569),.UNSPECIFIED.);
#3463=B_SPLINE_CURVE_WITH_KNOTS('',3,(#209735,#209736,#209737,#209738,#209739,
#209740,#209741,#209742,#209743,#209744,#209745,#209746,#209747,#209748,
#209749,#209750,#209751,#209752,#209753,#209754,#209755,#209756,#209757,
#209758,#209759,#209760,#209761,#209762,#209763,#209764,#209765,#209766,
#209767,#209768,#209769,#209770,#209771,#209772,#209773,#209774,#209775,
#209776,#209777,#209778,#209779,#209780,#209781,#209782,#209783,#209784,
#209785,#209786,#209787,#209788,#209789,#209790,#209791,#209792,#209793,
#209794,#209795,#209796,#209797,#209798,#209799,#209800,#209801,#209802,
#209803,#209804,#209805,#209806,#209807,#209808,#209809,#209810),
 .UNSPECIFIED.,.F.,.F.,(4,3,3,3,3,3,3,3,3,3,3,3,3,3,3,3,3,3,3,3,3,3,3,3,
3,4),(315.254347523701,315.33680912722,315.419270064869,315.501730364046,
315.584190052149,315.66664915657,315.749107704702,315.831565723934,315.914023241655,
316.000698597585,316.083165382623,316.165630495219,316.248094045028,316.33055614168,
316.413016894785,316.495476413938,316.577934808711,316.660392188665,316.742858573359,
316.825321774004,316.907782229117,316.990240377063,317.072705978894,317.155165855869,
317.237629963513,317.300828936529),.UNSPECIFIED.);
#3464=B_SPLINE_CURVE_WITH_KNOTS('',3,(#209811,#209812,#209813,#209814,#209815,
#209816,#209817,#209818,#209819,#209820,#209821,#209822,#209823,#209824,
#209825,#209826,#209827,#209828,#209829,#209830,#209831,#209832,#209833,
#209834,#209835,#209836,#209837,#209838,#209839,#209840,#209841,#209842,
#209843,#209844,#209845,#209846,#209847,#209848,#209849,#209850,#209851,
#209852,#209853,#209854,#209855,#209856,#209857,#209858,#209859,#209860,
#209861,#209862,#209863,#209864,#209865,#209866,#209867,#209868,#209869,
#209870,#209871,#209872,#209873,#209874,#209875,#209876,#209877,#209878,
#209879,#209880,#209881,#209882,#209883,#209884,#209885,#209886,#209887,
#209888,#209889,#209890,#209891,#209892,#209893,#209894,#209895,#209896,
#209897,#209898,#209899,#209900,#209901,#209902,#209903,#209904,#209905,
#209906,#209907,#209908,#209909,#209910,#209911,#209912,#209913,#209914,
#209915,#209916,#209917,#209918,#209919,#209920,#209921,#209922,#209923,
#209924,#209925,#209926,#209927,#209928,#209929,#209930,#209931,#209932,
#209933,#209934,#209935,#209936,#209937,#209938,#209939,#209940,#209941,
#209942,#209943,#209944,#209945,#209946,#209947,#209948,#209949,#209950,
#209951,#209952,#209953,#209954,#209955,#209956,#209957,#209958,#209959,
#209960,#209961,#209962,#209963,#209964,#209965,#209966,#209967,#209968,
#209969,#209970,#209971,#209972,#209973,#209974,#209975,#209976,#209977,
#209978,#209979),.UNSPECIFIED.,.F.,.F.,(4,3,3,3,3,3,3,3,3,3,3,3,3,3,3,3,
3,3,3,3,3,3,3,3,3,3,3,3,3,3,3,3,3,3,3,3,3,3,3,3,3,3,3,3,3,3,3,3,3,3,3,3,
3,3,3,3,4),(317.301372217802,317.376455735683,317.451484791519,317.526477606148,
317.601448232661,317.676427587139,317.728761889578,317.813438227786,317.898260712299,
317.983283083175,318.068391964983,318.153621504358,318.228131757509,318.309688020169,
318.391168959835,318.475252126236,318.556577878748,318.642039752094,318.72750162544,
318.806904966324,318.886326737487,318.965777715128,319.045301881349,319.124867791894,
319.204517640097,319.226871493372,319.305250514242,319.383563265558,319.461824161712,
319.54004757951,319.618247867671,319.696456056835,319.774672110326,319.852909027555,
319.931179817709,320.009543397182,320.087956526641,320.166486909154,320.225611229234,
320.301667735988,320.377628553982,320.453510474601,320.529330208108,320.60510440244,
320.682510222772,320.758257978887,320.834012984415,320.909790249645,320.988430428508,
321.064339614977,321.140305606919,321.216377804529,321.224350965096,321.302732003581,
321.380196773245,321.459035946141,321.537875119036),.UNSPECIFIED.);
#3465=B_SPLINE_CURVE_WITH_KNOTS('',3,(#209985,#209986,#209987,#209988,#209989,
#209990,#209991,#209992,#209993,#209994,#209995,#209996,#209997,#209998,
#209999,#210000,#210001,#210002,#210003,#210004,#210005,#210006,#210007,
#210008,#210009,#210010,#210011,#210012,#210013,#210014,#210015,#210016,
#210017,#210018,#210019,#210020,#210021,#210022,#210023,#210024,#210025,
#210026,#210027,#210028,#210029,#210030,#210031,#210032,#210033,#210034,
#210035,#210036,#210037,#210038,#210039,#210040,#210041,#210042,#210043,
#210044,#210045,#210046,#210047,#210048,#210049,#210050,#210051,#210052,
#210053,#210054,#210055,#210056,#210057,#210058,#210059,#210060,#210061,
#210062,#210063,#210064,#210065,#210066,#210067,#210068,#210069,#210070,
#210071,#210072,#210073,#210074,#210075,#210076,#210077,#210078,#210079,
#210080,#210081,#210082,#210083,#210084,#210085,#210086,#210087,#210088,
#210089,#210090,#210091,#210092,#210093,#210094,#210095,#210096,#210097,
#210098,#210099,#210100,#210101,#210102,#210103,#210104,#210105,#210106,
#210107,#210108,#210109,#210110,#210111,#210112,#210113,#210114,#210115,
#210116,#210117,#210118,#210119,#210120,#210121,#210122,#210123,#210124,
#210125,#210126,#210127,#210128,#210129,#210130,#210131,#210132,#210133,
#210134,#210135,#210136,#210137,#210138,#210139,#210140,#210141,#210142,
#210143,#210144,#210145,#210146,#210147,#210148,#210149,#210150,#210151,
#210152,#210153),.UNSPECIFIED.,.F.,.F.,(4,3,3,3,3,3,3,3,3,3,3,3,3,3,3,3,
3,3,3,3,3,3,3,3,3,3,3,3,3,3,3,3,3,3,3,3,3,3,3,3,3,3,3,3,3,3,3,3,3,3,3,3,
3,3,3,3,4),(323.584043319749,323.68144335902,323.780080950349,323.879872029107,
323.902885787077,323.978942293831,324.054903111825,324.130785032444,324.206604765951,
324.282378960282,324.359784780614,324.43553253673,324.511287542258,324.587064807488,
324.665704986351,324.74161417282,324.817580164762,324.893652362372,324.901625522939,
324.979184374484,325.056650918379,325.134040821672,325.211369696365,325.288653110508,
325.365914157079,325.443164857923,325.520419260609,325.597691412141,325.675036750278,
325.752419524003,325.829909019651,325.900365258801,325.984584541694,326.068677220668,
326.152563846481,326.236320835868,326.319862538526,326.399735126732,326.477102322525,
326.554487911977,326.631905693764,326.709410615377,326.78696521463,326.864626561582,
326.899104994664,326.978728931666,327.058279322512,327.137768482614,327.217208680182,
327.296612065701,327.375994527022,327.455367152634,327.534741023188,327.614150901509,
327.693578847173,327.773065486166,327.820873168898),.UNSPECIFIED.);
#3466=B_SPLINE_CURVE_WITH_KNOTS('',3,(#210154,#210155,#210156,#210157,#210158,
#210159,#210160,#210161,#210162,#210163,#210164,#210165,#210166,#210167,
#210168,#210169,#210170,#210171,#210172,#210173,#210174,#210175,#210176,
#210177,#210178,#210179,#210180,#210181,#210182,#210183,#210184,#210185,
#210186,#210187,#210188,#210189,#210190,#210191,#210192,#210193,#210194,
#210195,#210196,#210197,#210198,#210199,#210200,#210201,#210202,#210203,
#210204,#210205,#210206,#210207,#210208,#210209,#210210,#210211,#210212,
#210213,#210214,#210215,#210216,#210217,#210218,#210219,#210220,#210221,
#210222,#210223,#210224,#210225,#210226,#210227,#210228,#210229),
 .UNSPECIFIED.,.F.,.F.,(4,3,3,3,3,3,3,3,3,3,3,3,3,3,3,3,3,3,3,3,3,3,3,3,
3,4),(321.53753283088,321.619994434639,321.702455372518,321.784915671916,
321.867375360229,321.949834464851,322.032293013174,322.114751032588,322.197208550481,
322.283885723561,322.366352509169,322.448817622301,322.531281172607,322.613743269721,
322.696204023253,322.778663542796,322.861121937922,322.943579318193,323.026045704013,
323.108508905637,323.190969361585,323.273427510222,323.355893114233,323.438352992811,
323.520817104547,323.584043319749),.UNSPECIFIED.);
#3467=B_SPLINE_CURVE_WITH_KNOTS('',3,(#210231,#210232,#210233,#210234,#210235,
#210236,#210237,#210238,#210239,#210240,#210241,#210242,#210243,#210244,
#210245,#210246,#210247,#210248,#210249,#210250,#210251,#210252,#210253,
#210254,#210255,#210256,#210257,#210258,#210259,#210260,#210261,#210262,
#210263,#210264,#210265,#210266,#210267,#210268,#210269,#210270,#210271,
#210272,#210273,#210274,#210275,#210276,#210277,#210278,#210279,#210280,
#210281,#210282,#210283,#210284,#210285,#210286,#210287,#210288,#210289,
#210290,#210291,#210292,#210293,#210294,#210295,#210296,#210297,#210298,
#210299,#210300,#210301,#210302,#210303,#210304,#210305,#210306,#210307,
#210308,#210309),.UNSPECIFIED.,.F.,.F.,(4,3,3,3,3,3,3,3,3,3,3,3,3,3,3,3,
3,3,3,3,3,3,3,3,3,3,4),(321.537875119036,321.615156708834,321.692416922816,
321.76966747806,321.846922421929,321.924195801598,322.001542675429,322.078927602483,
322.156418288634,322.223090700958,322.307309983851,322.391402662824,322.475289288637,
322.559046278023,322.642587980681,322.722460568889,322.799827764682,322.877213354133,
322.95463113592,323.032136057532,323.109690656785,323.187352003737,323.22183043682,
323.31390668278,323.405745640809,323.496945780501,323.584043319749),
 .UNSPECIFIED.);
#3468=B_SPLINE_CURVE_WITH_KNOTS('',3,(#210310,#210311,#210312,#210313,#210314,
#210315,#210316,#210317,#210318,#210319,#210320,#210321,#210322,#210323,
#210324,#210325,#210326,#210327,#210328,#210329,#210330,#210331,#210332,
#210333,#210334,#210335,#210336,#210337,#210338,#210339,#210340,#210341,
#210342,#210343,#210344,#210345,#210346,#210347,#210348,#210349,#210350,
#210351,#210352,#210353,#210354,#210355,#210356,#210357,#210358,#210359,
#210360,#210361,#210362,#210363,#210364,#210365,#210366,#210367,#210368,
#210369,#210370,#210371,#210372,#210373,#210374,#210375,#210376,#210377,
#210378,#210379,#210380,#210381,#210382,#210383,#210384,#210385,#210386,
#210387,#210388,#210389,#210390,#210391,#210392,#210393,#210394,#210395,
#210396,#210397,#210398,#210399,#210400,#210401,#210402,#210403,#210404,
#210405,#210406,#210407,#210408,#210409,#210410,#210411,#210412,#210413,
#210414,#210415,#210416,#210417,#210418,#210419,#210420,#210421,#210422,
#210423,#210424,#210425,#210426,#210427,#210428,#210429,#210430,#210431,
#210432,#210433,#210434,#210435,#210436,#210437,#210438,#210439,#210440,
#210441,#210442,#210443,#210444,#210445,#210446,#210447,#210448,#210449,
#210450,#210451,#210452,#210453,#210454,#210455,#210456,#210457,#210458,
#210459,#210460,#210461,#210462,#210463,#210464,#210465,#210466),
 .UNSPECIFIED.,.F.,.F.,(4,3,3,3,3,3,3,3,3,3,3,3,3,3,3,3,3,3,3,3,3,3,3,3,
3,3,3,3,3,3,3,3,3,3,3,3,3,3,3,3,3,3,3,3,3,3,3,3,3,3,3,3,4),(323.584043319749,
323.666505525835,323.748967383623,323.831428899964,323.913890081708,323.996350935704,
324.078811468803,324.161271687853,324.243731599704,324.326191211203,324.4086505292,
324.491109560542,324.573568312077,324.656026790653,324.738485003118,324.820942956318,
324.903400657101,324.985858112313,325.0683153288,325.154327916589,325.23765261101,
325.320119216569,325.402584977919,325.485049922478,325.567514077656,325.649977470863,
325.732440129506,325.81490208099,325.897363352717,325.979823972085,326.062283966492,
326.144743363333,326.227202190002,326.309660473888,326.392118242381,326.474575522869,
326.558709436318,326.641175434617,326.723639811166,326.806102675608,326.888564137564,
326.971024306638,327.053483292413,327.135941204456,327.221538321156,327.3040030581,
327.386464830398,327.468924076489,327.551381234668,327.633843753567,327.71630142485,
327.798760215758,327.82071813806),.UNSPECIFIED.);
#3469=B_SPLINE_CURVE_WITH_KNOTS('',3,(#210472,#210473,#210474,#210475,#210476,
#210477,#210478,#210479,#210480,#210481,#210482,#210483,#210484,#210485,
#210486,#210487,#210488,#210489,#210490,#210491,#210492,#210493,#210494,
#210495,#210496,#210497,#210498,#210499,#210500,#210501,#210502,#210503,
#210504,#210505,#210506,#210507,#210508,#210509,#210510,#210511,#210512,
#210513,#210514,#210515,#210516,#210517,#210518,#210519,#210520,#210521,
#210522,#210523,#210524,#210525,#210526,#210527,#210528,#210529,#210530,
#210531,#210532,#210533,#210534,#210535,#210536,#210537,#210538,#210539,
#210540,#210541,#210542,#210543,#210544,#210545,#210546,#210547,#210548,
#210549,#210550,#210551,#210552,#210553,#210554,#210555,#210556,#210557,
#210558,#210559,#210560,#210561,#210562,#210563,#210564,#210565,#210566,
#210567,#210568,#210569,#210570,#210571,#210572,#210573,#210574,#210575,
#210576,#210577,#210578,#210579,#210580,#210581,#210582,#210583,#210584,
#210585,#210586,#210587,#210588,#210589,#210590,#210591,#210592,#210593,
#210594,#210595,#210596,#210597,#210598,#210599,#210600,#210601,#210602,
#210603,#210604,#210605,#210606,#210607,#210608,#210609,#210610,#210611,
#210612,#210613,#210614,#210615,#210616,#210617,#210618,#210619,#210620,
#210621,#210622,#210623,#210624,#210625,#210626,#210627,#210628,#210629,
#210630,#210631,#210632,#210633,#210634,#210635,#210636,#210637,#210638,
#210639,#210640,#210641,#210642,#210643),.UNSPECIFIED.,.F.,.F.,(4,3,3,3,
3,3,3,3,3,3,3,3,3,3,3,3,3,3,3,3,3,3,3,3,3,3,3,3,3,3,3,3,3,3,3,3,3,3,3,3,
3,3,3,3,3,3,3,3,3,3,3,3,3,3,3,3,3,4),(329.867228627072,329.89532420225,
329.97370322312,330.052015974436,330.130276870589,330.208500288388,330.286700576548,
330.364908765713,330.443124819203,330.521361736433,330.599632526587,330.67799610606,
330.756409235519,330.834939618032,330.894063938112,330.970120444866,331.04608126286,
331.121963183479,331.197782916987,331.273557111318,331.35096293165,331.426710687765,
331.502465693293,331.578242958524,331.656883137386,331.732792323855,331.808758315797,
331.884830513407,331.892803673974,331.970362525519,332.047829069414,332.125218972707,
332.2025478474,332.279831261543,332.357092308115,332.434343008959,332.511597411645,
332.588869563177,332.666214901314,332.743597675039,332.821087170687,332.891543409837,
332.97576269273,333.059855371704,333.143741997517,333.227498986904,333.311040689562,
333.390913277768,333.468280473561,333.545666063012,333.6230838448,333.700588766412,
333.778143365665,333.855804712617,333.890283145699,333.969909993848,334.049453245317,
334.104148056147),.UNSPECIFIED.);
#3470=B_SPLINE_CURVE_WITH_KNOTS('',3,(#210644,#210645,#210646,#210647,#210648,
#210649,#210650,#210651,#210652,#210653,#210654,#210655,#210656,#210657,
#210658,#210659,#210660,#210661,#210662,#210663,#210664,#210665,#210666,
#210667,#210668,#210669,#210670,#210671,#210672,#210673,#210674,#210675,
#210676,#210677,#210678,#210679,#210680,#210681,#210682,#210683,#210684,
#210685,#210686,#210687,#210688,#210689,#210690,#210691,#210692,#210693,
#210694,#210695,#210696,#210697,#210698,#210699,#210700,#210701,#210702,
#210703,#210704,#210705,#210706,#210707,#210708,#210709,#210710,#210711,
#210712,#210713,#210714,#210715,#210716,#210717,#210718,#210719,#210720,
#210721,#210722),.UNSPECIFIED.,.F.,.F.,(4,3,3,3,3,3,3,3,3,3,3,3,3,3,3,3,
3,3,3,3,3,3,3,3,3,3,4),(327.820873168898,327.897844730526,327.974559737375,
328.051207649739,328.127803161478,328.204362059176,328.280899443255,328.357440963707,
328.397214598457,328.481890936665,328.566713421179,328.651735792055,328.736844673863,
328.822074213238,328.896584466388,328.978140729048,329.059621668714,329.143704835115,
329.225030587627,329.310492460973,329.395954334319,329.474589036795,329.553236576592,
329.631945717837,329.710684832125,329.789516502116,329.867228626929),
 .UNSPECIFIED.);
#3471=B_SPLINE_CURVE_WITH_KNOTS('',3,(#210724,#210725,#210726,#210727,#210728,
#210729,#210730,#210731,#210732,#210733,#210734,#210735,#210736,#210737,
#210738,#210739,#210740,#210741,#210742,#210743,#210744,#210745,#210746,
#210747,#210748,#210749,#210750,#210751,#210752,#210753,#210754,#210755,
#210756,#210757,#210758,#210759,#210760,#210761,#210762,#210763,#210764,
#210765,#210766,#210767,#210768,#210769,#210770,#210771,#210772,#210773,
#210774,#210775,#210776,#210777,#210778,#210779,#210780,#210781,#210782,
#210783,#210784,#210785,#210786,#210787,#210788,#210789,#210790,#210791,
#210792,#210793,#210794,#210795,#210796,#210797,#210798,#210799),
 .UNSPECIFIED.,.F.,.F.,(4,3,3,3,3,3,3,3,3,3,3,3,3,3,3,3,3,3,3,3,3,3,3,3,
3,4),(327.82071813806,327.903179741818,327.985640679697,328.068100979095,
328.150560667408,328.233019772031,328.315478320354,328.397936339768,328.480393857661,
328.56707103074,328.649537816349,328.73200292948,328.814466479787,328.896928576901,
328.979389330433,329.061848849975,329.144307245102,329.226764625373,329.309231011192,
329.391694212816,329.474154668765,329.556612817401,329.639078421413,329.72153829999,
329.804002411727,329.867228626928),.UNSPECIFIED.);
#3472=B_SPLINE_CURVE_WITH_KNOTS('',3,(#210800,#210801,#210802,#210803,#210804,
#210805,#210806,#210807,#210808,#210809),.UNSPECIFIED.,.F.,.F.,(4,1,1,1,
1,1,1,4),(329.867228626928,330.213008587855,331.211748323718,331.711118191649,
332.21048805958,332.709857927511,333.209227795442,334.10365230637),
 .UNSPECIFIED.);
#3473=B_SPLINE_CURVE_WITH_KNOTS('',3,(#210815,#210816,#210817,#210818,#210819,
#210820,#210821,#210822,#210823,#210824,#210825,#210826,#210827,#210828,
#210829,#210830,#210831,#210832,#210833,#210834,#210835,#210836,#210837,
#210838,#210839,#210840,#210841,#210842,#210843,#210844,#210845,#210846,
#210847,#210848,#210849,#210850,#210851,#210852,#210853,#210854,#210855,
#210856,#210857,#210858,#210859,#210860,#210861,#210862,#210863,#210864,
#210865,#210866,#210867,#210868,#210869,#210870,#210871,#210872,#210873,
#210874,#210875,#210876,#210877,#210878,#210879,#210880,#210881,#210882,
#210883,#210884,#210885,#210886,#210887,#210888,#210889,#210890,#210891,
#210892,#210893,#210894,#210895,#210896,#210897,#210898,#210899,#210900,
#210901,#210902,#210903,#210904,#210905,#210906,#210907,#210908,#210909,
#210910,#210911,#210912,#210913,#210914,#210915,#210916,#210917,#210918,
#210919,#210920,#210921,#210922,#210923,#210924,#210925,#210926,#210927,
#210928,#210929,#210930,#210931,#210932,#210933,#210934,#210935,#210936,
#210937,#210938,#210939,#210940,#210941,#210942,#210943,#210944,#210945,
#210946,#210947,#210948,#210949,#210950,#210951,#210952,#210953,#210954,
#210955,#210956,#210957,#210958,#210959,#210960,#210961,#210962,#210963,
#210964,#210965,#210966,#210967,#210968,#210969,#210970,#210971),
 .UNSPECIFIED.,.F.,.F.,(4,3,3,3,3,3,3,3,3,3,3,3,3,3,3,3,3,3,3,3,3,3,3,3,
3,3,3,3,3,3,3,3,3,3,3,3,3,3,3,3,3,3,3,3,3,3,3,3,3,3,3,3,4),(336.150413934108,
336.232876140193,336.315337997982,336.397799514323,336.480260696067,336.562721550063,
336.645182083162,336.727642302212,336.810102214063,336.892561825562,336.975021143559,
337.057480174901,337.139938926436,337.222397405013,337.304855617477,337.387313570677,
337.46977127146,337.552228726672,337.634685943159,337.720698530948,337.804023225369,
337.886489830928,337.968955592278,338.051420536837,338.133884692015,338.216348085222,
338.298810743865,338.381272695349,338.463733967076,338.546194586444,338.628654580851,
338.711113977693,338.793572804361,338.876031088247,338.958488856741,339.040946137228,
339.125080050678,339.207546048976,339.290010425525,339.372473289967,339.454934751924,
339.537394920998,339.619853906772,339.702311818815,339.787908935516,339.870373672459,
339.952835444758,340.035294690849,340.117751849027,340.200214367926,340.28267203921,
340.365130830118,340.387088752419),.UNSPECIFIED.);
#3474=B_SPLINE_CURVE_WITH_KNOTS('',3,(#210972,#210973,#210974,#210975,#210976,
#210977,#210978,#210979,#210980,#210981,#210982,#210983,#210984,#210985,
#210986,#210987,#210988,#210989,#210990,#210991,#210992,#210993,#210994,
#210995,#210996,#210997,#210998,#210999,#211000,#211001,#211002,#211003,
#211004,#211005,#211006,#211007,#211008,#211009,#211010,#211011,#211012,
#211013,#211014,#211015,#211016,#211017,#211018,#211019,#211020,#211021,
#211022,#211023,#211024,#211025,#211026,#211027,#211028,#211029,#211030,
#211031,#211032,#211033,#211034,#211035,#211036,#211037,#211038,#211039,
#211040,#211041,#211042,#211043,#211044,#211045,#211046,#211047,#211048,
#211049,#211050),.UNSPECIFIED.,.F.,.F.,(4,3,3,3,3,3,3,3,3,3,3,3,3,3,3,3,
3,3,3,3,3,3,3,3,3,3,4),(334.104148056147,334.183600716777,334.263013462116,
334.342403745438,334.421781588549,334.501158074259,334.580544283132,334.659982760416,
334.739446410458,334.818988270721,334.889022881561,334.96573788841,335.042385800774,
335.118981312513,335.195540210211,335.272077594291,335.348619114743,335.388392749492,
335.4730690877,335.557891572214,335.64291394309,335.728022824899,335.813252364273,
335.887762617423,335.973697967041,336.062055950575,336.150413934108),
 .UNSPECIFIED.);
#3475=B_SPLINE_CURVE_WITH_KNOTS('',3,(#211052,#211053,#211054,#211055,#211056,
#211057),.UNSPECIFIED.,.F.,.F.,(4,1,1,4),(334.10365230637,334.207967531304,
335.206707267166,336.150408590058),.UNSPECIFIED.);
#3476=B_SPLINE_CURVE_WITH_KNOTS('',3,(#211058,#211059,#211060,#211061,#211062,
#211063,#211064,#211065,#211066,#211067,#211068,#211069,#211070,#211071,
#211072,#211073,#211074,#211075,#211076,#211077,#211078,#211079,#211080,
#211081,#211082,#211083,#211084,#211085,#211086,#211087,#211088,#211089,
#211090,#211091,#211092,#211093,#211094,#211095,#211096,#211097,#211098,
#211099,#211100,#211101,#211102,#211103,#211104,#211105,#211106,#211107,
#211108,#211109,#211110,#211111,#211112,#211113,#211114,#211115,#211116,
#211117,#211118,#211119,#211120,#211121,#211122,#211123,#211124,#211125,
#211126,#211127,#211128,#211129,#211130,#211131,#211132,#211133,#211134,
#211135,#211136,#211137,#211138,#211139,#211140,#211141,#211142,#211143,
#211144,#211145,#211146,#211147,#211148,#211149,#211150,#211151,#211152,
#211153,#211154,#211155,#211156,#211157,#211158,#211159,#211160,#211161,
#211162,#211163,#211164,#211165,#211166,#211167,#211168,#211169,#211170,
#211171,#211172,#211173,#211174,#211175,#211176,#211177,#211178,#211179,
#211180,#211181,#211182,#211183,#211184,#211185,#211186,#211187,#211188,
#211189,#211190,#211191,#211192,#211193,#211194,#211195,#211196,#211197,
#211198,#211199,#211200,#211201,#211202,#211203,#211204,#211205,#211206,
#211207,#211208,#211209,#211210,#211211,#211212,#211213,#211214,#211215,
#211216,#211217,#211218,#211219,#211220,#211221,#211222,#211223,#211224,
#211225,#211226),.UNSPECIFIED.,.F.,.F.,(4,3,3,3,3,3,3,3,3,3,3,3,3,3,3,3,
3,3,3,3,3,3,3,3,3,3,3,3,3,3,3,3,3,3,3,3,3,3,3,3,3,3,3,3,3,3,3,3,3,3,3,3,
3,3,3,3,4),(336.150413934108,336.205447003029,336.289666285922,336.373758964895,
336.457645590708,336.541402580095,336.624944282753,336.70481687096,336.782184066753,
336.859569656204,336.936987437992,337.014492359605,337.092046958857,337.169708305809,
337.204186738891,337.283807477635,337.363355305291,337.442842534567,337.52228143148,
337.601684224287,337.681069437185,337.760445667738,337.839823997288,337.919215507159,
337.99866074199,338.078134322771,338.157681434821,338.202926474753,338.279641481602,
338.356289393966,338.432884905705,338.509443803403,338.585981187482,338.662522707934,
338.702296342684,338.786972680892,338.871795165406,338.956817536282,339.04192641809,
339.127155957465,339.201666210615,339.283222473274,339.36470341294,339.448786579342,
339.530112331853,339.6155742052,339.701036078546,339.780439419431,339.859861190593,
339.939312168234,340.018836334454,340.098402245,340.178052093203,340.200405946477,
340.278794595193,340.357108620971,340.387341982143),.UNSPECIFIED.);
#3477=B_SPLINE_CURVE_WITH_KNOTS('',3,(#211232,#211233,#211234,#211235,#211236,
#211237,#211238,#211239,#211240,#211241,#211242,#211243,#211244,#211245,
#211246,#211247,#211248,#211249,#211250,#211251,#211252,#211253,#211254,
#211255,#211256,#211257,#211258,#211259,#211260,#211261,#211262,#211263,
#211264,#211265,#211266,#211267,#211268,#211269,#211270,#211271,#211272,
#211273,#211274,#211275,#211276,#211277,#211278,#211279,#211280,#211281,
#211282,#211283,#211284,#211285,#211286,#211287,#211288,#211289,#211290,
#211291,#211292,#211293,#211294,#211295,#211296,#211297,#211298,#211299,
#211300,#211301,#211302,#211303,#211304,#211305,#211306,#211307,#211308,
#211309,#211310,#211311,#211312,#211313,#211314,#211315,#211316,#211317,
#211318,#211319,#211320,#211321,#211322,#211323,#211324,#211325,#211326,
#211327,#211328,#211329,#211330,#211331,#211332,#211333,#211334,#211335,
#211336,#211337,#211338,#211339,#211340,#211341,#211342,#211343,#211344,
#211345,#211346,#211347,#211348,#211349,#211350,#211351,#211352,#211353,
#211354,#211355,#211356,#211357,#211358,#211359,#211360,#211361,#211362,
#211363,#211364,#211365,#211366,#211367,#211368,#211369,#211370,#211371,
#211372,#211373,#211374,#211375,#211376,#211377,#211378,#211379,#211380,
#211381,#211382,#211383,#211384,#211385,#211386,#211387,#211388,#211389,
#211390,#211391,#211392,#211393,#211394,#211395,#211396,#211397,#211398,
#211399,#211400,#211401,#211402,#211403),.UNSPECIFIED.,.F.,.F.,(4,3,3,3,
3,3,3,3,3,3,3,3,3,3,3,3,3,3,3,3,3,3,3,3,3,3,3,3,3,3,3,3,3,3,3,3,3,3,3,3,
3,3,3,3,3,3,3,3,3,3,3,3,3,3,3,3,3,4),(342.433599241288,342.518884947016,
342.604327876792,342.689963352961,342.775685721844,342.86150384477,342.878940768458,
342.960497031118,343.041977970784,343.126061137185,343.207386889697,343.292848763043,
343.37831063639,343.457713977275,343.537135748437,343.616586726078,343.696110892299,
343.775676802844,343.855326651047,343.877680504321,343.956059525191,344.034372276507,
344.11263317266,344.19085659046,344.26905687862,344.347265067784,344.425481121274,
344.503718038504,344.581988828658,344.660352408131,344.73876553759,344.817295920103,
344.876420240183,344.952476746937,345.028437564931,345.10431948555,345.180139219057,
345.255913413388,345.33331923372,345.409066989835,345.484821995364,345.560599260594,
345.639239439457,345.715148625926,345.791114617868,345.867186815478,345.875159976045,
345.952730916243,346.030207285946,346.110132834588,346.187454824317,346.264735602648,
346.341989243777,346.419229803829,346.49648848957,346.573758516221,346.65107369651,
346.669611675086),.UNSPECIFIED.);
#3478=B_SPLINE_CURVE_WITH_KNOTS('',3,(#211404,#211405,#211406,#211407,#211408,
#211409,#211410,#211411,#211412,#211413,#211414,#211415,#211416,#211417,
#211418,#211419,#211420,#211421,#211422,#211423,#211424,#211425,#211426,
#211427,#211428,#211429,#211430,#211431,#211432,#211433,#211434,#211435,
#211436,#211437,#211438,#211439,#211440,#211441,#211442,#211443,#211444,
#211445,#211446,#211447,#211448,#211449,#211450,#211451,#211452,#211453,
#211454,#211455,#211456,#211457,#211458,#211459,#211460,#211461,#211462,
#211463,#211464,#211465,#211466,#211467,#211468,#211469,#211470,#211471,
#211472,#211473,#211474,#211475,#211476,#211477,#211478,#211479),
 .UNSPECIFIED.,.F.,.F.,(4,3,3,3,3,3,3,3,3,3,3,3,3,3,3,3,3,3,3,3,3,3,3,3,
3,4),(340.387088752419,340.469550356178,340.552011294057,340.634471593455,
340.716931281768,340.79939038639,340.881848934713,340.964306954127,341.04676447202,
341.1334416451,341.215908430708,341.298373543839,341.380837094146,341.46329919126,
341.545759944792,341.628219464335,341.710677859461,341.793135239732,341.875601625552,
341.958064827176,342.040525283124,342.122983431761,342.205449035772,342.28790891435,
342.370373026086,342.433599241288),.UNSPECIFIED.);
#3479=B_SPLINE_CURVE_WITH_KNOTS('',3,(#211481,#211482,#211483,#211484,#211485,
#211486,#211487,#211488,#211489,#211490,#211491,#211492,#211493,#211494,
#211495,#211496,#211497,#211498,#211499,#211500,#211501,#211502,#211503,
#211504,#211505,#211506,#211507,#211508,#211509,#211510,#211511,#211512,
#211513,#211514,#211515,#211516,#211517,#211518,#211519,#211520,#211521,
#211522,#211523,#211524,#211525,#211526,#211527,#211528,#211529,#211530,
#211531,#211532,#211533,#211534,#211535,#211536,#211537,#211538,#211539,
#211540,#211541,#211542,#211543,#211544,#211545,#211546,#211547,#211548,
#211549,#211550,#211551,#211552,#211553,#211554,#211555,#211556,#211557,
#211558,#211559,#211560,#211561,#211562,#211563,#211564,#211565),
 .UNSPECIFIED.,.F.,.F.,(4,3,3,3,3,3,3,3,3,3,3,3,3,3,3,3,3,3,3,3,3,3,3,3,
3,3,3,3,4),(340.387341982143,340.465586694626,340.543799475709,340.625717751538,
340.703927756916,340.782151266517,340.860401283073,340.938690822348,341.017074441985,
341.095512723419,341.17405872535,341.19914568234,341.275202189094,341.351163007088,
341.427044927707,341.502864661214,341.578638855545,341.656044675877,341.731792431993,
341.807547437521,341.883324702751,341.961964881614,342.037874068083,342.113840060025,
342.189912257635,342.197885418202,342.315742329745,342.42587465463,342.433599241287),
 .UNSPECIFIED.);
#3480=B_SPLINE_CURVE_WITH_KNOTS('',3,(#211566,#211567,#211568,#211569,#211570,
#211571,#211572,#211573,#211574,#211575,#211576,#211577,#211578,#211579,
#211580,#211581,#211582,#211583,#211584,#211585,#211586,#211587,#211588,
#211589,#211590,#211591,#211592,#211593,#211594,#211595,#211596,#211597,
#211598,#211599,#211600,#211601,#211602,#211603,#211604,#211605,#211606,
#211607,#211608,#211609,#211610,#211611,#211612,#211613,#211614,#211615,
#211616,#211617,#211618,#211619,#211620,#211621,#211622,#211623,#211624,
#211625,#211626,#211627,#211628,#211629,#211630,#211631,#211632,#211633,
#211634,#211635,#211636,#211637,#211638,#211639,#211640,#211641,#211642,
#211643,#211644,#211645,#211646,#211647,#211648,#211649,#211650,#211651,
#211652,#211653,#211654,#211655,#211656,#211657,#211658,#211659,#211660,
#211661,#211662,#211663,#211664,#211665,#211666,#211667,#211668,#211669,
#211670,#211671,#211672,#211673,#211674,#211675,#211676,#211677,#211678,
#211679,#211680,#211681,#211682,#211683,#211684,#211685,#211686,#211687,
#211688,#211689,#211690,#211691,#211692,#211693,#211694,#211695,#211696,
#211697,#211698,#211699,#211700,#211701,#211702,#211703,#211704,#211705,
#211706,#211707,#211708,#211709,#211710,#211711,#211712,#211713,#211714,
#211715,#211716,#211717,#211718,#211719,#211720,#211721,#211722,#211723,
#211724,#211725,#211726,#211727,#211728,#211729,#211730,#211731),
 .UNSPECIFIED.,.F.,.F.,(4,3,3,3,3,3,3,3,3,3,3,3,3,3,3,3,3,3,3,3,3,3,3,3,
3,3,3,3,3,3,3,3,3,3,3,3,3,3,3,3,3,3,3,3,3,3,3,3,3,3,3,3,3,3,3,4),(342.433599241378,
342.509334181514,342.585008870166,342.661460905653,342.737073109975,342.812679087942,
342.888293962241,342.965376760197,343.041089123994,343.118857139029,343.196625154064,
343.280844436957,343.364937115931,343.448823741744,343.532580731131,343.616122433789,
343.695995021995,343.773362217788,343.850747807239,343.928165589027,344.005670510639,
344.083225109892,344.160886456844,344.195364889926,344.27498562867,344.354533456326,
344.434020685602,344.513459582515,344.592862375321,344.67224758822,344.751623818773,
344.831002148323,344.910393658194,344.989838893025,345.069312473806,345.148859585856,
345.194104625788,345.270819632637,345.347467545,345.424063056739,345.500621954437,
345.577159338516,345.653700858968,345.693474493719,345.778150831927,345.862973316441,
345.947995687317,346.033104569126,346.118334108501,346.19284436165,346.274402663091,
346.355885589217,346.437274666338,346.518605081455,346.599864769658,346.670532447169),
 .UNSPECIFIED.);
#3481=B_SPLINE_CURVE_WITH_KNOTS('',3,(#211737,#211738,#211739,#211740,#211741,
#211742,#211743,#211744,#211745,#211746,#211747,#211748,#211749,#211750,
#211751,#211752,#211753,#211754,#211755,#211756,#211757,#211758,#211759,
#211760,#211761,#211762,#211763,#211764,#211765,#211766,#211767,#211768,
#211769,#211770,#211771,#211772,#211773,#211774,#211775,#211776,#211777,
#211778,#211779,#211780,#211781,#211782,#211783,#211784,#211785,#211786,
#211787,#211788,#211789,#211790,#211791,#211792,#211793,#211794,#211795,
#211796,#211797,#211798,#211799,#211800,#211801,#211802,#211803,#211804,
#211805,#211806,#211807,#211808,#211809,#211810,#211811,#211812,#211813,
#211814,#211815,#211816,#211817,#211818,#211819,#211820,#211821,#211822,
#211823,#211824,#211825,#211826,#211827,#211828,#211829,#211830,#211831,
#211832,#211833,#211834,#211835,#211836,#211837,#211838,#211839,#211840,
#211841,#211842,#211843,#211844,#211845,#211846,#211847,#211848,#211849,
#211850,#211851,#211852,#211853,#211854,#211855,#211856,#211857,#211858,
#211859,#211860,#211861,#211862,#211863,#211864,#211865,#211866,#211867,
#211868,#211869,#211870,#211871,#211872,#211873,#211874,#211875,#211876,
#211877,#211878,#211879,#211880,#211881,#211882,#211883,#211884,#211885,
#211886,#211887,#211888,#211889,#211890,#211891,#211892,#211893),
 .UNSPECIFIED.,.F.,.F.,(4,3,3,3,3,3,3,3,3,3,3,3,3,3,3,3,3,3,3,3,3,3,3,3,
3,3,3,3,3,3,3,3,3,3,3,3,3,3,3,3,3,3,3,3,3,3,3,3,3,3,3,3,4),(348.716784548467,
348.799246754552,348.881708612341,348.964170128682,349.046631310426,349.129092164422,
349.211552697521,349.294012916571,349.376472828422,349.458932439921,349.541391757918,
349.62385078926,349.706309540795,349.788768019372,349.871226231836,349.953684185037,
350.036141885819,350.118599341031,350.201056557519,350.287069145308,350.370393839729,
350.452860445287,350.535326206638,350.617791151196,350.700255306374,350.782718699581,
350.865181358225,350.947643309709,351.030104581435,351.112565200803,351.195025195211,
351.277484592052,351.35994341872,351.442401702607,351.5248594711,351.607316751588,
351.691450665037,351.773916663336,351.856381039885,351.938843904326,352.021305366283,
352.103765535357,352.186224521132,352.268682433175,352.354279549875,352.436744286819,
352.519206059117,352.601665305208,352.684122463387,352.766584982286,352.849042653569,
352.931501444477,352.953459366778),.UNSPECIFIED.);
#3482=B_SPLINE_CURVE_WITH_KNOTS('',3,(#211894,#211895,#211896,#211897,#211898,
#211899,#211900,#211901,#211902,#211903,#211904,#211905,#211906,#211907,
#211908,#211909,#211910,#211911,#211912,#211913,#211914,#211915,#211916,
#211917,#211918,#211919,#211920,#211921,#211922,#211923,#211924,#211925,
#211926,#211927,#211928,#211929,#211930,#211931,#211932,#211933,#211934,
#211935,#211936,#211937,#211938,#211939,#211940,#211941,#211942,#211943,
#211944,#211945,#211946,#211947,#211948,#211949,#211950,#211951,#211952,
#211953,#211954,#211955,#211956,#211957,#211958,#211959,#211960,#211961,
#211962,#211963,#211964,#211965,#211966,#211967,#211968,#211969,#211970,
#211971,#211972,#211973,#211974,#211975),.UNSPECIFIED.,.F.,.F.,(4,3,3,3,
3,3,3,3,3,3,3,3,3,3,3,3,3,3,3,3,3,3,3,3,3,3,3,4),(346.669611675086,346.747006816302,
346.824503410128,346.873899711907,346.9581189948,347.042211673773,347.126098299586,
347.209855288973,347.293396991631,347.373269579838,347.450636775631,347.528022365082,
347.60544014687,347.682945068483,347.760499667735,347.838161014688,347.872639447769,
347.951128287047,348.029541293079,348.107892883974,348.186194357667,348.264468019272,
348.342726853174,348.420983832666,348.499278733754,348.577592411052,348.655974971976,
348.716634548041),.UNSPECIFIED.);
#3483=B_SPLINE_CURVE_WITH_KNOTS('',3,(#211977,#211978,#211979,#211980,#211981,
#211982,#211983,#211984,#211985,#211986,#211987,#211988,#211989,#211990,
#211991,#211992,#211993,#211994,#211995,#211996,#211997,#211998,#211999,
#212000,#212001,#212002,#212003,#212004,#212005,#212006,#212007,#212008,
#212009,#212010,#212011,#212012,#212013,#212014,#212015,#212016,#212017,
#212018,#212019,#212020,#212021,#212022,#212023,#212024,#212025,#212026,
#212027,#212028,#212029,#212030,#212031,#212032,#212033,#212034,#212035,
#212036,#212037,#212038,#212039,#212040,#212041,#212042,#212043,#212044,
#212045,#212046,#212047,#212048,#212049,#212050,#212051,#212052,#212053,
#212054,#212055,#212056,#212057,#212058,#212059,#212060,#212061),
 .UNSPECIFIED.,.F.,.F.,(4,3,3,3,3,3,3,3,3,3,3,3,3,3,3,3,3,3,3,3,3,3,3,3,
3,3,3,3,4),(346.670532447169,346.692214229582,346.771617570467,346.851039341629,
346.930490319271,347.010014485491,347.089580396036,347.169230244239,347.191584097513,
347.269963118383,347.348275869698,347.426536765852,347.504760183652,347.582960471812,
347.661168660977,347.739384714467,347.817621631696,347.89589242185,347.974256001323,
348.052669130781,348.131199513294,348.190323833375,348.269008312196,348.347569787422,
348.426020943107,348.504342215918,348.582588647594,348.660753693213,348.716784548467),
 .UNSPECIFIED.);
#3484=B_SPLINE_CURVE_WITH_KNOTS('',3,(#212062,#212063,#212064,#212065,#212066,
#212067,#212068,#212069,#212070,#212071,#212072,#212073,#212074,#212075,
#212076,#212077,#212078,#212079,#212080,#212081,#212082,#212083,#212084,
#212085,#212086,#212087,#212088,#212089,#212090,#212091,#212092,#212093,
#212094,#212095,#212096,#212097,#212098,#212099,#212100,#212101,#212102,
#212103,#212104,#212105,#212106,#212107,#212108,#212109,#212110,#212111,
#212112,#212113,#212114,#212115,#212116,#212117,#212118,#212119,#212120,
#212121,#212122,#212123,#212124,#212125,#212126,#212127,#212128,#212129,
#212130,#212131,#212132,#212133,#212134,#212135,#212136,#212137,#212138,
#212139,#212140,#212141,#212142,#212143,#212144,#212145,#212146,#212147,
#212148,#212149,#212150,#212151,#212152,#212153,#212154,#212155,#212156,
#212157,#212158,#212159,#212160,#212161,#212162,#212163,#212164,#212165,
#212166,#212167,#212168,#212169,#212170,#212171,#212172,#212173,#212174,
#212175,#212176,#212177,#212178,#212179,#212180,#212181,#212182,#212183,
#212184,#212185,#212186,#212187,#212188,#212189,#212190,#212191,#212192,
#212193,#212194,#212195,#212196,#212197,#212198,#212199,#212200,#212201,
#212202,#212203,#212204,#212205,#212206,#212207,#212208,#212209,#212210,
#212211,#212212,#212213,#212214,#212215,#212216,#212217,#212218,#212219,
#212220,#212221,#212222,#212223,#212224,#212225,#212226,#212227,#212228,
#212229,#212230),.UNSPECIFIED.,.F.,.F.,(4,3,3,3,3,3,3,3,3,3,3,3,3,3,3,3,
3,3,3,3,3,3,3,3,3,3,3,3,3,3,3,3,3,3,3,3,3,3,3,3,3,3,3,3,3,3,3,3,3,3,3,3,
3,3,3,3,4),(348.716784548553,348.797305153374,348.877955810068,348.95883364991,
349.039831377576,349.121049133391,349.189063569237,349.266622420782,349.344088964677,
349.42147886797,349.498807742663,349.576091156806,349.653352203378,349.730602904222,
349.807857306907,349.885129458439,349.962474796577,350.039857570302,350.117347065949,
350.187803305099,350.272022587992,350.356115266965,350.440001892778,350.523758882165,
350.607300584823,350.68717317303,350.764540368823,350.841925958274,350.919343740062,
350.996848661674,351.074403260927,351.152064607879,351.186543040961,351.266163779705,
351.345711607362,351.425198836637,351.504637733551,351.584040526357,351.663425739256,
351.742801969808,351.822180299359,351.90157180923,351.981017044061,352.060490624842,
352.140037736892,352.185282776823,352.261997783672,352.338645696036,352.415241207775,
352.491800105473,352.568337489552,352.644879010005,352.684652644755,352.769339370933,
352.854150045697,352.939116054778,352.952905577053),.UNSPECIFIED.);
#3485=B_SPLINE_CURVE_WITH_KNOTS('',3,(#212236,#212237,#212238,#212239,#212240,
#212241,#212242,#212243,#212244,#212245,#212246,#212247,#212248,#212249,
#212250,#212251,#212252,#212253,#212254,#212255,#212256,#212257,#212258,
#212259,#212260,#212261,#212262,#212263,#212264,#212265,#212266,#212267,
#212268,#212269,#212270,#212271,#212272,#212273,#212274,#212275,#212276,
#212277,#212278,#212279,#212280,#212281,#212282,#212283,#212284,#212285,
#212286,#212287,#212288,#212289,#212290,#212291,#212292,#212293,#212294,
#212295,#212296,#212297,#212298,#212299,#212300,#212301,#212302,#212303,
#212304,#212305,#212306,#212307,#212308,#212309,#212310,#212311,#212312,
#212313,#212314,#212315,#212316,#212317,#212318,#212319,#212320,#212321,
#212322,#212323,#212324,#212325,#212326,#212327,#212328,#212329,#212330,
#212331,#212332,#212333,#212334,#212335,#212336,#212337,#212338,#212339,
#212340,#212341,#212342,#212343,#212344,#212345,#212346,#212347,#212348,
#212349,#212350,#212351,#212352,#212353,#212354,#212355,#212356,#212357,
#212358,#212359,#212360,#212361,#212362,#212363,#212364,#212365,#212366,
#212367,#212368,#212369,#212370,#212371,#212372,#212373,#212374,#212375,
#212376,#212377,#212378,#212379,#212380,#212381,#212382,#212383,#212384,
#212385,#212386,#212387,#212388,#212389,#212390,#212391,#212392,#212393,
#212394,#212395,#212396,#212397,#212398,#212399,#212400,#212401),
 .UNSPECIFIED.,.F.,.F.,(4,3,3,3,3,3,3,3,3,3,3,3,3,3,3,3,3,3,3,3,3,3,3,3,
3,3,3,3,3,3,3,3,3,3,3,3,3,3,3,3,3,3,3,3,3,3,3,3,3,3,3,3,3,3,3,4),(355.000265717516,
355.07862633194,355.156915835323,355.235148756737,355.313574828978,355.391742837346,
355.469901025712,355.54806247983,355.626686193539,355.704920289582,355.783738812124,
355.862557334667,355.939272341516,356.01592025388,356.092515765619,356.169074663317,
356.245612047396,356.322153567848,356.361927202598,356.446603540806,356.53142602532,
356.616448396195,356.701557278004,356.786786817379,356.861297070529,356.942853333189,
357.024334272855,357.108417439256,357.189743191768,357.275205065114,357.36066693846,
357.440070279344,357.519492050507,357.598943028148,357.678467194368,357.758033104913,
357.837682953116,357.860036806391,357.938415827261,358.016728578577,358.09498947473,
358.17321289253,358.25141318069,358.329621369855,358.407837423345,358.486074340575,
358.564345130729,358.642708710202,358.721121839661,358.799652222174,358.858776542253,
358.934848133081,359.01079790405,359.086677955374,359.162492894976,359.237285162207),
 .UNSPECIFIED.);
#3486=B_SPLINE_CURVE_WITH_KNOTS('',3,(#212402,#212403,#212404,#212405,#212406,
#212407,#212408,#212409,#212410,#212411,#212412,#212413,#212414,#212415,
#212416,#212417,#212418,#212419,#212420,#212421,#212422,#212423,#212424,
#212425,#212426,#212427,#212428,#212429,#212430,#212431,#212432,#212433,
#212434,#212435,#212436,#212437,#212438,#212439,#212440,#212441,#212442,
#212443,#212444,#212445,#212446,#212447,#212448,#212449,#212450,#212451,
#212452,#212453,#212454,#212455,#212456,#212457,#212458,#212459,#212460,
#212461,#212462,#212463,#212464,#212465,#212466,#212467,#212468,#212469,
#212470,#212471,#212472,#212473,#212474,#212475,#212476,#212477),
 .UNSPECIFIED.,.F.,.F.,(4,3,3,3,3,3,3,3,3,3,3,3,3,3,3,3,3,3,3,3,3,3,3,3,
3,4),(352.953459366778,353.035920970537,353.118381908416,353.200842207814,
353.283301896127,353.365761000749,353.448219549072,353.530677568487,353.61313508638,
353.699812259459,353.782279045067,353.864744158199,353.947207708506,354.02966980562,
354.112130559152,354.194590078694,354.277048473821,354.359505854092,354.441972239911,
354.524435441535,354.606895897483,354.68935404612,354.771819650131,354.854279528709,
354.936743640445,354.999969855647),.UNSPECIFIED.);
#3487=B_SPLINE_CURVE_WITH_KNOTS('',3,(#212479,#212480,#212481,#212482,#212483,
#212484,#212485,#212486,#212487,#212488,#212489,#212490,#212491,#212492,
#212493,#212494,#212495,#212496,#212497,#212498,#212499,#212500,#212501,
#212502,#212503,#212504,#212505,#212506,#212507,#212508,#212509,#212510,
#212511,#212512,#212513,#212514,#212515,#212516,#212517,#212518,#212519,
#212520,#212521,#212522,#212523,#212524,#212525,#212526,#212527,#212528,
#212529,#212530,#212531,#212532,#212533,#212534,#212535,#212536,#212537,
#212538,#212539,#212540,#212541,#212542,#212543,#212544,#212545,#212546,
#212547,#212548,#212549,#212550,#212551,#212552,#212553,#212554,#212555,
#212556,#212557,#212558,#212559,#212560),.UNSPECIFIED.,.F.,.F.,(4,3,3,3,
3,3,3,3,3,3,3,3,3,3,3,3,3,3,3,3,3,3,3,3,3,3,3,4),(352.952905577053,353.038027293992,
353.12326229478,353.184022512686,353.265578775345,353.347059715011,353.431142881412,
353.512468633924,353.59793050727,353.683392380617,353.762795721502,353.842217492664,
353.921668470305,354.001192636525,354.08075854707,354.160408395273,354.182762248548,
354.259467848333,354.33610345867,354.412685321611,354.489233298249,354.565764476793,
354.642293487223,354.718834955904,354.795439462035,354.872077965804,354.94880981331,
354.999969855546),.UNSPECIFIED.);
#3488=B_SPLINE_CURVE_WITH_KNOTS('',3,(#212561,#212562,#212563,#212564,#212565,
#212566,#212567,#212568,#212569,#212570,#212571,#212572,#212573,#212574,
#212575,#212576,#212577,#212578,#212579,#212580,#212581,#212582,#212583,
#212584,#212585,#212586,#212587,#212588,#212589,#212590,#212591,#212592,
#212593,#212594,#212595,#212596,#212597,#212598,#212599,#212600,#212601,
#212602,#212603,#212604,#212605,#212606,#212607,#212608,#212609,#212610,
#212611,#212612,#212613,#212614,#212615,#212616,#212617,#212618,#212619,
#212620,#212621,#212622,#212623,#212624,#212625,#212626,#212627,#212628,
#212629,#212630,#212631,#212632,#212633,#212634,#212635,#212636,#212637,
#212638,#212639,#212640,#212641,#212642,#212643,#212644,#212645,#212646,
#212647,#212648,#212649,#212650,#212651,#212652,#212653,#212654,#212655,
#212656,#212657,#212658,#212659,#212660,#212661,#212662,#212663,#212664,
#212665,#212666,#212667,#212668,#212669,#212670,#212671,#212672,#212673,
#212674,#212675,#212676,#212677,#212678,#212679,#212680,#212681,#212682,
#212683,#212684,#212685,#212686,#212687,#212688,#212689,#212690,#212691,
#212692,#212693,#212694,#212695,#212696,#212697,#212698,#212699,#212700,
#212701,#212702,#212703,#212704,#212705,#212706,#212707,#212708,#212709,
#212710,#212711,#212712,#212713,#212714,#212715,#212716,#212717,#212718,
#212719,#212720,#212721,#212722,#212723,#212724,#212725,#212726,#212727,
#212728,#212729),.UNSPECIFIED.,.F.,.F.,(4,3,3,3,3,3,3,3,3,3,3,3,3,3,3,3,
3,3,3,3,3,3,3,3,3,3,3,3,3,3,3,3,3,3,3,3,3,3,3,3,3,3,3,3,3,3,3,3,3,3,3,3,
3,3,3,3,4),(354.999969855647,355.145499078777,355.18150198441,355.257558491164,
355.333519309158,355.409401229777,355.485220963284,355.560995157615,355.638400977947,
355.714148734062,355.78990373959,355.865681004821,355.944321183684,356.020230370152,
356.096196362095,356.172268559705,356.180241720272,356.257800571817,356.335267115712,
356.412657019005,356.489985893698,356.567269307841,356.644530354413,356.721781055257,
356.799035457942,356.876307609474,356.953652947612,357.031035721336,357.108525216984,
357.178981456134,357.263200739027,357.347293418001,357.431180043814,357.514937033201,
357.598478735859,357.678351324065,357.755718519858,357.833104109309,357.910521891097,
357.98802681271,358.065581411963,358.143242758915,358.177721191997,358.257341930741,
358.336889758398,358.416376987673,358.495815884586,358.575218677393,358.654603890292,
358.733980120844,358.813358450395,358.892749960266,358.972195195097,359.051668775877,
359.131215887927,359.176460927859,359.237141913219),.UNSPECIFIED.);
#3489=B_SPLINE_CURVE_WITH_KNOTS('',3,(#212735,#212736,#212737,#212738,#212739,
#212740,#212741,#212742,#212743,#212744,#212745,#212746,#212747,#212748,
#212749,#212750,#212751,#212752,#212753,#212754,#212755,#212756,#212757,
#212758,#212759,#212760,#212761,#212762,#212763,#212764,#212765,#212766,
#212767,#212768,#212769,#212770,#212771,#212772,#212773,#212774,#212775,
#212776,#212777,#212778,#212779,#212780,#212781,#212782,#212783,#212784,
#212785,#212786,#212787,#212788,#212789,#212790,#212791,#212792,#212793,
#212794,#212795,#212796,#212797,#212798,#212799,#212800,#212801,#212802,
#212803,#212804,#212805,#212806,#212807,#212808,#212809,#212810,#212811,
#212812,#212813,#212814,#212815,#212816,#212817,#212818,#212819,#212820,
#212821,#212822,#212823,#212824,#212825,#212826,#212827,#212828,#212829,
#212830,#212831,#212832,#212833,#212834,#212835,#212836,#212837,#212838,
#212839,#212840,#212841,#212842,#212843,#212844,#212845,#212846,#212847,
#212848,#212849,#212850,#212851,#212852,#212853,#212854,#212855,#212856,
#212857,#212858,#212859,#212860,#212861,#212862,#212863,#212864,#212865,
#212866,#212867,#212868,#212869,#212870,#212871,#212872,#212873,#212874,
#212875,#212876,#212877,#212878,#212879,#212880,#212881,#212882,#212883,
#212884,#212885,#212886,#212887,#212888,#212889,#212890,#212891,#212892,
#212893,#212894,#212895,#212896,#212897,#212898,#212899,#212900,#212901,
#212902,#212903),.UNSPECIFIED.,.F.,.F.,(4,3,3,3,3,3,3,3,3,3,3,3,3,3,3,3,
3,3,3,3,3,3,3,3,3,3,3,3,3,3,3,3,3,3,3,3,3,3,3,3,3,3,3,3,3,3,3,3,3,3,3,3,
3,3,3,3,4),(361.283155162826,361.355625881909,361.432993077702,361.510378667153,
361.58779644894,361.665301370553,361.742855969805,361.820517316757,361.85499574984,
361.934616488584,362.01416431624,362.093651545516,362.173090442429,362.252493235236,
362.331878448134,362.411254678687,362.490633008237,362.570024518108,362.649469752939,
362.72894333372,362.808490445769,362.853735485702,362.930450492551,363.007098404915,
363.083693916654,363.160252814353,363.236790198432,363.313331718884,363.353105353633,
363.437781691841,363.522604176355,363.607626547231,363.692735429039,363.777964968414,
363.852475221564,363.934031484224,364.015512423889,364.099595590291,364.180921342802,
364.266383216149,364.351845089495,364.43124843038,364.510670201542,364.590121179183,
364.669645345403,364.749211255948,364.828861104151,364.851214957426,364.929607149855,
365.007915006163,365.086174026984,365.164397253256,365.242597702528,365.320801928763,
365.39900717539,365.477247391082,365.519381429312),.UNSPECIFIED.);
#3490=B_SPLINE_CURVE_WITH_KNOTS('',3,(#212904,#212905,#212906,#212907,#212908,
#212909,#212910,#212911,#212912,#212913,#212914,#212915,#212916,#212917,
#212918,#212919,#212920,#212921,#212922,#212923,#212924,#212925,#212926,
#212927,#212928,#212929,#212930,#212931,#212932,#212933,#212934,#212935,
#212936,#212937,#212938,#212939,#212940,#212941,#212942,#212943,#212944,
#212945,#212946,#212947,#212948,#212949,#212950,#212951,#212952,#212953,
#212954,#212955,#212956,#212957,#212958,#212959,#212960,#212961,#212962,
#212963,#212964,#212965,#212966,#212967,#212968,#212969,#212970,#212971,
#212972,#212973,#212974,#212975,#212976,#212977,#212978,#212979,#212980,
#212981,#212982,#212983,#212984,#212985),.UNSPECIFIED.,.F.,.F.,(4,3,3,3,
3,3,3,3,3,3,3,3,3,3,3,3,3,3,3,3,3,3,3,3,3,3,3,4),(359.237285162207,359.314814051696,
359.390561811662,359.466316650378,359.54209357802,359.620949253044,359.696858013785,
359.772823464503,359.848895295443,359.857516278115,359.93507512966,360.012541673555,
360.089931576848,360.167260451541,360.244543865684,360.321804912256,360.399055613099,
360.476310015785,360.553582167317,360.630927505455,360.708310279179,360.785799774827,
360.856256013978,360.942974708954,361.029430442254,361.115706269608,361.201641256815,
361.283155162746),.UNSPECIFIED.);
#3491=B_SPLINE_CURVE_WITH_KNOTS('',3,(#212987,#212988,#212989,#212990,#212991,
#212992,#212993,#212994,#212995,#212996,#212997,#212998,#212999,#213000,
#213001,#213002,#213003,#213004,#213005,#213006,#213007,#213008,#213009,
#213010,#213011,#213012,#213013,#213014,#213015,#213016,#213017,#213018,
#213019,#213020,#213021,#213022,#213023,#213024,#213025,#213026,#213027,
#213028,#213029,#213030,#213031,#213032,#213033,#213034,#213035,#213036,
#213037,#213038,#213039,#213040,#213041,#213042,#213043,#213044,#213045,
#213046,#213047,#213048,#213049,#213050,#213051,#213052,#213053,#213054,
#213055,#213056,#213057,#213058,#213059,#213060,#213061,#213062,#213063,
#213064,#213065),.UNSPECIFIED.,.F.,.F.,(4,3,3,3,3,3,3,3,3,3,3,3,3,3,3,3,
3,3,3,3,3,3,3,3,3,3,4),(359.237141913219,359.313802637782,359.390407892746,
359.466972944385,359.543513743999,359.620058210566,359.67583079579,359.760507133998,
359.845329618512,359.930351989387,360.015460871196,360.100690410571,360.175200663721,
360.256756926381,360.338237866047,360.422321032448,360.50364678496,360.589108658306,
360.674570531652,360.753973872537,360.833395643699,360.91284662134,360.99237078756,
361.071936698105,361.151586546308,361.173940399583,361.283155162826),
 .UNSPECIFIED.);
#3492=B_SPLINE_CURVE_WITH_KNOTS('',3,(#213066,#213067,#213068,#213069,#213070,
#213071,#213072,#213073,#213074,#213075,#213076,#213077,#213078,#213079,
#213080,#213081,#213082,#213083,#213084,#213085,#213086,#213087,#213088,
#213089,#213090,#213091,#213092,#213093,#213094,#213095,#213096,#213097,
#213098,#213099,#213100,#213101,#213102,#213103,#213104,#213105,#213106,
#213107,#213108,#213109,#213110,#213111,#213112,#213113,#213114,#213115,
#213116,#213117,#213118,#213119,#213120,#213121,#213122,#213123,#213124,
#213125,#213126,#213127,#213128,#213129,#213130,#213131,#213132,#213133,
#213134,#213135,#213136,#213137,#213138,#213139,#213140,#213141,#213142,
#213143,#213144,#213145,#213146,#213147,#213148,#213149,#213150,#213151,
#213152,#213153,#213154,#213155,#213156,#213157,#213158,#213159,#213160,
#213161,#213162,#213163,#213164,#213165,#213166,#213167,#213168,#213169,
#213170,#213171,#213172,#213173,#213174,#213175,#213176,#213177,#213178,
#213179,#213180,#213181,#213182,#213183,#213184,#213185,#213186,#213187,
#213188,#213189,#213190,#213191,#213192,#213193,#213194,#213195,#213196,
#213197,#213198,#213199,#213200,#213201,#213202,#213203,#213204,#213205,
#213206,#213207,#213208,#213209,#213210,#213211,#213212,#213213,#213214,
#213215,#213216,#213217,#213218,#213219,#213220,#213221,#213222,#213223,
#213224,#213225,#213226,#213227,#213228,#213229,#213230,#213231,#213232,
#213233,#213234,#213235,#213236,#213237),.UNSPECIFIED.,.F.,.F.,(4,3,3,3,
3,3,3,3,3,3,3,3,3,3,3,3,3,3,3,3,3,3,3,3,3,3,3,3,3,3,3,3,3,3,3,3,3,3,3,3,
3,3,3,3,3,3,3,3,3,3,3,3,3,3,3,3,3,4),(361.283155162933,361.360786413993,
361.438359570209,361.515889959261,361.593392877591,361.670898290541,361.748409428821,
361.825940131368,361.903504245392,361.981157765079,362.058862079906,362.136675654933,
362.172680135445,362.248736642199,362.324697460193,362.400579380812,362.476399114319,
362.552173308651,362.629579128983,362.705326885098,362.781081890626,362.856859155857,
362.93549933472,363.011408521188,363.087374513131,363.163446710741,363.171419871308,
363.248978722853,363.326445266748,363.403835170041,363.481164044734,363.558447458877,
363.635708505449,363.712959206293,363.790213608979,363.86748576051,363.944831098648,
364.022213872373,364.099703368021,364.17015960717,364.254378890063,364.338471569036,
364.422358194849,364.506115184235,364.589656886893,364.669529475101,364.746896670894,
364.824282260345,364.901700042133,364.979204963746,365.056759562998,365.134420909951,
365.168899343032,365.248533459538,365.328076371135,365.407565382026,365.487002394566,
365.5201243322),.UNSPECIFIED.);
#3493=B_SPLINE_CURVE_WITH_KNOTS('',3,(#213243,#213244,#213245,#213246,#213247,
#213248,#213249,#213250,#213251,#213252,#213253,#213254,#213255,#213256,
#213257,#213258,#213259,#213260,#213261,#213262,#213263,#213264,#213265,
#213266,#213267,#213268,#213269,#213270,#213271,#213272,#213273,#213274,
#213275,#213276,#213277,#213278,#213279,#213280,#213281,#213282,#213283,
#213284,#213285,#213286,#213287,#213288,#213289,#213290,#213291,#213292,
#213293,#213294,#213295,#213296,#213297,#213298,#213299,#213300,#213301,
#213302,#213303,#213304,#213305,#213306,#213307,#213308,#213309,#213310,
#213311,#213312,#213313,#213314,#213315,#213316,#213317,#213318,#213319,
#213320,#213321,#213322,#213323,#213324,#213325,#213326,#213327,#213328,
#213329,#213330,#213331,#213332,#213333,#213334,#213335,#213336,#213337,
#213338,#213339,#213340,#213341,#213342,#213343,#213344,#213345,#213346,
#213347,#213348,#213349,#213350,#213351,#213352,#213353,#213354,#213355,
#213356,#213357,#213358,#213359,#213360,#213361,#213362,#213363,#213364,
#213365,#213366,#213367,#213368,#213369,#213370,#213371,#213372,#213373,
#213374,#213375,#213376,#213377,#213378,#213379,#213380,#213381,#213382,
#213383,#213384,#213385,#213386,#213387,#213388,#213389,#213390,#213391,
#213392,#213393,#213394,#213395,#213396,#213397,#213398,#213399,#213400,
#213401,#213402,#213403,#213404,#213405,#213406,#213407,#213408),
 .UNSPECIFIED.,.F.,.F.,(4,3,3,3,3,3,3,3,3,3,3,3,3,3,3,3,3,3,3,3,3,3,3,3,
3,3,3,3,3,3,3,3,3,3,3,3,3,3,3,3,3,3,3,3,3,3,3,3,3,3,3,3,3,3,3,4),(367.566340470133,
367.65634728685,367.746832996282,367.837849218279,367.847434165013,367.931653447906,
368.015746126879,368.099632752693,368.183389742079,368.266931444738,368.346804032944,
368.424171228737,368.501556818188,368.578974599976,368.656479521589,368.734034120841,
368.811695467793,368.846173900875,368.925794639619,369.005342467275,369.084829696551,
369.164268593464,369.24367138627,369.323056599169,369.402432829721,369.481811159272,
369.561202669143,369.640647903974,369.720121484754,369.799668596804,369.844913636737,
369.921628643586,369.99827655595,370.074872067689,370.151430965388,370.227968349467,
370.304509869919,370.344283504668,370.428959842876,370.51378232739,370.598804698266,
370.683913580075,370.76914311945,370.8436533726,370.92520963526,371.006690574926,
371.090773741327,371.172099493839,371.257561367185,371.343023240531,371.422423589424,
371.501841947507,371.581323390372,371.660836601941,371.740434855231,371.802906295849),
 .UNSPECIFIED.);
#3494=B_SPLINE_CURVE_WITH_KNOTS('',3,(#213409,#213410,#213411,#213412,#213413,
#213414,#213415,#213416,#213417,#213418,#213419,#213420,#213421,#213422,
#213423,#213424,#213425,#213426,#213427,#213428,#213429,#213430,#213431,
#213432,#213433,#213434,#213435,#213436,#213437,#213438,#213439,#213440,
#213441,#213442,#213443,#213444,#213445,#213446,#213447,#213448,#213449,
#213450,#213451,#213452,#213453,#213454,#213455,#213456,#213457,#213458,
#213459,#213460,#213461,#213462,#213463,#213464,#213465,#213466,#213467,
#213468,#213469,#213470,#213471,#213472,#213473,#213474,#213475,#213476,
#213477,#213478,#213479,#213480,#213481,#213482,#213483,#213484,#213485,
#213486,#213487,#213488,#213489,#213490,#213491,#213492,#213493,#213494,
#213495,#213496),.UNSPECIFIED.,.F.,.F.,(4,3,3,3,3,3,3,3,3,3,3,3,3,3,3,3,
3,3,3,3,3,3,3,3,3,3,3,3,3,4),(365.519381429312,365.597675845742,365.676064617682,
365.754509281994,365.833059455537,365.849954693289,365.926011200043,366.001972018037,
366.077853938656,366.153673672164,366.229447866494,366.306853686826,366.382601442942,
366.45835644847,366.5341337137,366.612773892563,366.688683079032,366.764649070974,
366.840721268584,366.848694429151,366.926527682873,367.006504281264,367.084132405596,
367.161700039667,367.239221020856,367.316709157361,367.394185738152,367.471656271798,
367.549146528326,367.566340470006),.UNSPECIFIED.);
#3495=B_SPLINE_CURVE_WITH_KNOTS('',3,(#213498,#213499,#213500,#213501,#213502,
#213503,#213504,#213505,#213506,#213507,#213508,#213509,#213510,#213511,
#213512,#213513,#213514,#213515,#213516,#213517,#213518,#213519,#213520,
#213521,#213522,#213523,#213524,#213525,#213526,#213527,#213528,#213529,
#213530,#213531,#213532,#213533,#213534,#213535,#213536,#213537,#213538,
#213539,#213540,#213541,#213542,#213543,#213544,#213545,#213546,#213547,
#213548,#213549,#213550,#213551,#213552,#213553,#213554,#213555,#213556,
#213557,#213558,#213559,#213560,#213561,#213562,#213563,#213564,#213565,
#213566,#213567,#213568,#213569,#213570,#213571,#213572,#213573,#213574,
#213575,#213576),.UNSPECIFIED.,.F.,.F.,(4,3,3,3,3,3,3,3,3,3,3,3,3,3,3,3,
3,3,3,3,3,3,3,3,3,3,4),(365.5201243322,365.601063675537,365.680443602888,
365.759819387226,365.839202109013,365.921311351483,366.000768657719,366.084203868307,
366.167639078894,366.244354085743,366.321001998106,366.397597509846,366.474156407544,
366.550693791622,366.627235312075,366.667008946825,366.751685285033,366.836507769547,
366.921530140422,367.006639022231,367.091868561606,367.166378814756,367.24895402029,
367.331412181403,367.413795867861,367.49607454044,367.566340470006),
 .UNSPECIFIED.);
#3496=B_SPLINE_CURVE_WITH_KNOTS('',3,(#213577,#213578,#213579,#213580,#213581,
#213582,#213583,#213584,#213585,#213586,#213587,#213588,#213589,#213590,
#213591,#213592,#213593,#213594,#213595,#213596,#213597,#213598,#213599,
#213600,#213601,#213602,#213603,#213604,#213605,#213606,#213607,#213608,
#213609,#213610,#213611,#213612,#213613,#213614,#213615,#213616,#213617,
#213618,#213619,#213620,#213621,#213622,#213623,#213624,#213625,#213626,
#213627,#213628,#213629,#213630,#213631,#213632,#213633,#213634,#213635,
#213636,#213637,#213638,#213639,#213640,#213641,#213642,#213643,#213644,
#213645,#213646,#213647,#213648,#213649,#213650,#213651,#213652,#213653,
#213654,#213655,#213656,#213657,#213658,#213659,#213660,#213661,#213662,
#213663,#213664,#213665,#213666,#213667,#213668,#213669,#213670,#213671,
#213672,#213673,#213674,#213675,#213676,#213677,#213678,#213679,#213680,
#213681,#213682,#213683,#213684,#213685,#213686,#213687,#213688,#213689,
#213690,#213691,#213692,#213693,#213694,#213695,#213696,#213697,#213698,
#213699,#213700,#213701,#213702,#213703,#213704,#213705,#213706,#213707,
#213708,#213709,#213710,#213711,#213712,#213713,#213714,#213715,#213716,
#213717,#213718,#213719,#213720,#213721,#213722,#213723,#213724,#213725,
#213726,#213727,#213728,#213729,#213730,#213731,#213732,#213733),
 .UNSPECIFIED.,.F.,.F.,(4,3,3,3,3,3,3,3,3,3,3,3,3,3,3,3,3,3,3,3,3,3,3,3,
3,3,3,3,3,3,3,3,3,3,3,3,3,3,3,3,3,3,3,3,3,3,3,3,3,3,3,3,4),(367.566340470006,
367.648802676092,367.73126453388,367.813726050221,367.896187231965,367.978648085961,
368.06110861906,368.14356883811,368.226028749961,368.30848836146,368.390947679457,
368.473406710799,368.555865462334,368.638323940911,368.720782153375,368.803240106575,
368.885697807358,368.96815526257,369.050612479058,369.136625066847,369.219949761268,
369.302416366826,369.384882128177,369.467347072735,369.549811227913,369.63227462112,
369.714737279764,369.797199231248,369.879660502974,369.962121122342,370.044581116749,
370.127040513591,370.209499340259,370.291957624145,370.374415392639,370.456872673126,
370.541006586576,370.623472584874,370.705936961423,370.788399825865,370.870861287822,
370.953321456895,371.03578044267,371.118238354713,371.203835471413,371.286300208357,
371.368761980655,371.451221226746,371.533678384925,371.616140903824,371.698598575107,
371.781057366015,371.803015288317),.UNSPECIFIED.);
#3497=B_SPLINE_CURVE_WITH_KNOTS('',3,(#213739,#213740,#213741,#213742,#213743,
#213744,#213745,#213746,#213747,#213748,#213749,#213750,#213751,#213752,
#213753,#213754,#213755,#213756,#213757,#213758,#213759,#213760,#213761,
#213762,#213763,#213764,#213765,#213766,#213767,#213768,#213769,#213770,
#213771,#213772,#213773,#213774,#213775,#213776,#213777,#213778,#213779,
#213780,#213781,#213782,#213783,#213784,#213785,#213786,#213787,#213788,
#213789,#213790,#213791,#213792,#213793,#213794,#213795,#213796,#213797,
#213798,#213799,#213800,#213801,#213802,#213803,#213804,#213805,#213806,
#213807,#213808,#213809,#213810,#213811,#213812,#213813,#213814,#213815,
#213816,#213817,#213818,#213819,#213820,#213821,#213822,#213823,#213824,
#213825,#213826,#213827,#213828,#213829,#213830,#213831,#213832,#213833,
#213834,#213835,#213836,#213837,#213838,#213839,#213840,#213841,#213842,
#213843,#213844,#213845,#213846,#213847,#213848,#213849,#213850,#213851,
#213852,#213853,#213854,#213855,#213856,#213857,#213858,#213859,#213860,
#213861,#213862,#213863,#213864,#213865,#213866,#213867,#213868,#213869,
#213870,#213871,#213872,#213873,#213874,#213875,#213876,#213877,#213878,
#213879,#213880,#213881,#213882,#213883,#213884,#213885,#213886,#213887,
#213888,#213889,#213890,#213891,#213892,#213893,#213894,#213895,#213896,
#213897,#213898,#213899,#213900,#213901,#213902,#213903,#213904),
 .UNSPECIFIED.,.F.,.F.,(4,3,3,3,3,3,3,3,3,3,3,3,3,3,3,3,3,3,3,3,3,3,3,3,
3,3,3,3,3,3,3,3,3,3,3,3,3,3,3,3,3,3,3,3,3,3,3,3,3,3,3,3,3,3,3,4),(373.849525777278,
373.926925065778,374.004231815205,374.081461850757,374.158630941525,374.235754812016,
374.312856778804,374.389948914552,374.467045407264,374.544160444793,374.621348780657,
374.698575531326,374.775907024984,374.838612316048,374.922831598941,375.006924277914,
375.090810903727,375.174567893114,375.258109595772,375.337982183979,375.415349379772,
375.492734969224,375.570152751011,375.647657672624,375.725212271877,375.802873618829,
375.83735205191,375.916972790654,375.996520618311,376.076007847586,376.155446744499,
376.234849537306,376.314234750205,376.393610980757,376.472989310308,376.552380820179,
376.63182605501,376.71129963579,376.79084674784,376.836091787773,376.912806794622,
376.989454706986,377.066050218725,377.142609116424,377.219146500503,377.295688020955,
377.335461655704,377.420137993912,377.504960478426,377.589982849301,377.67509173111,
377.760321270484,377.834831523635,377.916387377341,378.001553171997,378.086718966652),
 .UNSPECIFIED.);
#3498=B_SPLINE_CURVE_WITH_KNOTS('',3,(#213905,#213906,#213907,#213908,#213909,
#213910,#213911,#213912,#213913,#213914,#213915,#213916,#213917,#213918,
#213919,#213920,#213921,#213922,#213923,#213924,#213925,#213926,#213927,
#213928,#213929,#213930,#213931,#213932,#213933,#213934,#213935,#213936,
#213937,#213938,#213939,#213940,#213941,#213942,#213943,#213944,#213945,
#213946,#213947,#213948,#213949,#213950,#213951,#213952,#213953,#213954,
#213955,#213956,#213957,#213958,#213959,#213960,#213961,#213962,#213963,
#213964,#213965,#213966,#213967,#213968,#213969,#213970,#213971,#213972,
#213973,#213974,#213975,#213976,#213977,#213978,#213979,#213980,#213981,
#213982,#213983,#213984,#213985,#213986,#213987,#213988,#213989,#213990,
#213991,#213992),.UNSPECIFIED.,.F.,.F.,(4,3,3,3,3,3,3,3,3,3,3,3,3,3,3,3,
3,3,3,3,3,3,3,3,3,3,3,3,3,4),(371.802906295849,371.842393108462,371.920772129332,
371.999084880648,372.077345776802,372.155569194601,372.233769482761,372.311977671926,
372.390193725416,372.468430642645,372.546701432799,372.625065012272,372.703478141731,
372.782008524244,372.841132844324,372.917189351078,372.993150169072,373.069032089691,
373.144851823198,373.220626017529,373.298031837862,373.373779593977,373.449534599505,
373.525311864735,373.603952043598,373.679861230067,373.75582722201,373.83189941962,
373.839872580186,373.849525777185),.UNSPECIFIED.);
#3499=B_SPLINE_CURVE_WITH_KNOTS('',3,(#213994,#213995,#213996,#213997,#213998,
#213999,#214000,#214001,#214002,#214003,#214004,#214005,#214006,#214007,
#214008,#214009,#214010,#214011,#214012,#214013,#214014,#214015,#214016,
#214017,#214018,#214019,#214020,#214021,#214022,#214023,#214024,#214025,
#214026,#214027,#214028,#214029,#214030,#214031,#214032,#214033,#214034,
#214035,#214036,#214037,#214038,#214039,#214040,#214041,#214042,#214043,
#214044,#214045,#214046,#214047,#214048,#214049,#214050,#214051,#214052,
#214053,#214054,#214055,#214056,#214057,#214058,#214059,#214060,#214061,
#214062,#214063,#214064,#214065,#214066,#214067,#214068,#214069),
 .UNSPECIFIED.,.F.,.F.,(4,3,3,3,3,3,3,3,3,3,3,3,3,3,3,3,3,3,3,3,3,3,3,3,
3,4),(371.803015288317,371.885476892075,371.967937829954,372.050398129352,
372.132857817666,372.215316922288,372.297775470611,372.380233490025,372.462691007918,
372.549368180997,372.631834966606,372.714300079737,372.796763630044,372.879225727158,
372.96168648069,373.044146000232,373.126604395359,373.20906177563,373.291528161449,
373.373991363073,373.456451819022,373.538909967658,373.62137557167,373.703835450247,
373.786299561984,373.849525777185),.UNSPECIFIED.);
#3500=B_SPLINE_CURVE_WITH_KNOTS('',3,(#214070,#214071,#214072,#214073,#214074,
#214075,#214076,#214077,#214078,#214079,#214080,#214081,#214082,#214083,
#214084,#214085,#214086,#214087,#214088,#214089,#214090,#214091,#214092,
#214093,#214094,#214095,#214096,#214097,#214098,#214099,#214100,#214101,
#214102,#214103,#214104,#214105,#214106,#214107,#214108,#214109,#214110,
#214111,#214112,#214113,#214114,#214115,#214116,#214117,#214118,#214119,
#214120,#214121,#214122,#214123,#214124,#214125,#214126,#214127,#214128,
#214129,#214130,#214131,#214132,#214133,#214134,#214135,#214136,#214137,
#214138,#214139,#214140,#214141,#214142,#214143,#214144,#214145,#214146,
#214147,#214148,#214149,#214150,#214151,#214152,#214153,#214154,#214155,
#214156,#214157,#214158,#214159,#214160,#214161,#214162,#214163,#214164,
#214165,#214166,#214167,#214168,#214169,#214170,#214171,#214172,#214173,
#214174,#214175,#214176,#214177,#214178,#214179,#214180,#214181,#214182,
#214183,#214184,#214185,#214186,#214187,#214188,#214189,#214190,#214191,
#214192,#214193,#214194,#214195,#214196,#214197,#214198,#214199,#214200,
#214201,#214202,#214203,#214204,#214205,#214206,#214207,#214208,#214209,
#214210,#214211,#214212,#214213,#214214,#214215,#214216,#214217,#214218,
#214219,#214220,#214221,#214222,#214223,#214224,#214225,#214226),
 .UNSPECIFIED.,.F.,.F.,(4,3,3,3,3,3,3,3,3,3,3,3,3,3,3,3,3,3,3,3,3,3,3,3,
3,3,3,3,3,3,3,3,3,3,3,3,3,3,3,3,3,3,3,3,3,3,3,3,3,3,3,3,4),(373.849525777328,
373.931987983413,374.014449841201,374.096911357542,374.179372539286,374.261833393283,
374.344293926382,374.426754145432,374.509214057282,374.591673668782,374.674132986778,
374.756592018121,374.839050769656,374.921509248232,375.003967460697,375.086425413897,
375.16888311468,375.251340569892,375.333797786379,375.419810374164,375.50313506858,
375.585601674139,375.66806743549,375.750532380048,375.832996535226,375.915459928433,
375.997922587077,376.080384538561,376.162845810287,376.245306429655,376.327766424062,
376.410225820904,376.492684647572,376.575142931458,376.657600699952,376.740057980439,
376.82419189388,376.906657892179,376.989122268728,377.07158513317,377.154046595126,
377.2365067642,377.318965749975,377.401423662018,377.487020778703,377.569485515646,
377.651947287944,377.734406534036,377.816863692214,377.899326211113,377.981783882397,
378.064242673305,378.086200595497),.UNSPECIFIED.);
#3501=B_SPLINE_CURVE_WITH_KNOTS('',3,(#214232,#214233,#214234,#214235,#214236,
#214237,#214238,#214239,#214240,#214241,#214242,#214243,#214244,#214245,
#214246,#214247,#214248,#214249,#214250,#214251,#214252,#214253,#214254,
#214255,#214256,#214257,#214258,#214259,#214260,#214261,#214262,#214263,
#214264,#214265,#214266,#214267,#214268,#214269,#214270,#214271,#214272,
#214273,#214274,#214275,#214276,#214277,#214278,#214279,#214280,#214281,
#214282,#214283,#214284,#214285,#214286,#214287,#214288,#214289,#214290,
#214291,#214292,#214293,#214294,#214295,#214296,#214297,#214298,#214299,
#214300,#214301,#214302,#214303,#214304,#214305,#214306,#214307,#214308,
#214309,#214310,#214311,#214312,#214313,#214314,#214315,#214316,#214317,
#214318,#214319,#214320,#214321,#214322,#214323,#214324,#214325,#214326,
#214327,#214328,#214329,#214330,#214331,#214332,#214333,#214334,#214335,
#214336,#214337,#214338,#214339,#214340,#214341,#214342,#214343,#214344,
#214345,#214346,#214347,#214348,#214349,#214350,#214351,#214352,#214353,
#214354,#214355,#214356,#214357,#214358,#214359,#214360,#214361,#214362,
#214363,#214364,#214365,#214366,#214367,#214368,#214369,#214370,#214371,
#214372,#214373,#214374,#214375,#214376,#214377,#214378,#214379,#214380,
#214381,#214382,#214383,#214384,#214385,#214386,#214387,#214388),
 .UNSPECIFIED.,.F.,.F.,(4,3,3,3,3,3,3,3,3,3,3,3,3,3,3,3,3,3,3,3,3,3,3,3,
3,3,3,3,3,3,3,3,3,3,3,3,3,3,3,3,3,3,3,3,3,3,3,3,3,3,3,3,4),(380.132711084365,
380.215173290451,380.297635148239,380.38009666458,380.462557846323,380.54501870032,
380.627479233419,380.709939452469,380.79239936432,380.874858975819,380.957318293816,
381.039777325158,381.122236076693,381.204694555269,381.287152767734,381.369610720934,
381.452068421717,381.534525876928,381.616983093416,381.702995681205,381.786320375626,
381.868786981185,381.951252742535,382.033717687094,382.116181842272,382.198645235479,
382.281107894122,382.363569845606,382.446031117333,382.528491736701,382.610951731108,
382.693411127949,382.775869954618,382.858328238504,382.940786006997,383.023243287485,
383.107377200935,383.189843199233,383.272307575782,383.354770440224,383.437231902181,
383.519692071254,383.602151057029,383.684608969072,383.770206085773,383.852670822716,
383.935132595015,384.017591841106,384.100048999284,384.182511518183,384.264969189467,
384.347427980375,384.369385902676),.UNSPECIFIED.);
#3502=B_SPLINE_CURVE_WITH_KNOTS('',3,(#214389,#214390,#214391,#214392,#214393,
#214394,#214395,#214396,#214397,#214398,#214399,#214400,#214401,#214402,
#214403,#214404,#214405,#214406,#214407,#214408,#214409,#214410,#214411,
#214412,#214413,#214414,#214415,#214416,#214417,#214418,#214419,#214420,
#214421,#214422,#214423,#214424,#214425,#214426,#214427,#214428,#214429,
#214430,#214431,#214432,#214433,#214434,#214435,#214436,#214437,#214438,
#214439,#214440,#214441,#214442,#214443,#214444,#214445,#214446,#214447,
#214448,#214449,#214450,#214451,#214452,#214453,#214454,#214455,#214456,
#214457,#214458,#214459,#214460,#214461,#214462,#214463,#214464,#214465,
#214466,#214467,#214468,#214469,#214470),.UNSPECIFIED.,.F.,.F.,(4,3,3,3,
3,3,3,3,3,3,3,3,3,3,3,3,3,3,3,3,3,3,3,3,3,3,3,4),(378.086718966652,378.168041453345,
378.251121422455,378.334201391566,378.41360473245,378.493026503613,378.572477481254,
378.652001647474,378.731567558019,378.811217406222,378.833571259497,378.911950280367,
378.990263031683,379.068523927837,379.146747345636,379.224947633796,379.303155822961,
379.381371876451,379.45960879368,379.537879583834,379.616243163307,379.694656292766,
379.773186675279,379.832310995359,379.92329934872,380.013756059912,380.103324611181,
380.132711084365),.UNSPECIFIED.);
#3503=B_SPLINE_CURVE_WITH_KNOTS('',3,(#214472,#214473,#214474,#214475,#214476,
#214477,#214478,#214479,#214480,#214481,#214482,#214483,#214484,#214485,
#214486,#214487,#214488,#214489,#214490,#214491,#214492,#214493,#214494,
#214495,#214496,#214497,#214498,#214499,#214500,#214501,#214502,#214503,
#214504,#214505,#214506,#214507,#214508,#214509,#214510,#214511,#214512,
#214513,#214514,#214515,#214516,#214517,#214518,#214519,#214520,#214521,
#214522,#214523,#214524,#214525,#214526,#214527,#214528,#214529,#214530,
#214531,#214532,#214533,#214534,#214535,#214536,#214537,#214538,#214539,
#214540,#214541,#214542,#214543,#214544,#214545,#214546,#214547),
 .UNSPECIFIED.,.F.,.F.,(4,3,3,3,3,3,3,3,3,3,3,3,3,3,3,3,3,3,3,3,3,3,3,3,
3,4),(378.086200595497,378.168662199255,378.251123137134,378.333583436532,
378.416043124845,378.498502229467,378.580960777791,378.663418797205,378.745876315098,
378.832553488169,378.915020273777,378.997485386909,379.079948937216,379.16241103433,
379.244871787861,379.327331307404,379.409789702531,379.492247082802,379.574713468621,
379.657176670245,379.739637126194,379.82209527483,379.904560878842,379.987020757419,
380.069484869156,380.132711084236),.UNSPECIFIED.);
#3504=B_SPLINE_CURVE_WITH_KNOTS('',3,(#214548,#214549,#214550,#214551,#214552,
#214553,#214554,#214555,#214556,#214557,#214558,#214559,#214560,#214561,
#214562,#214563,#214564,#214565,#214566,#214567,#214568,#214569,#214570,
#214571,#214572,#214573,#214574,#214575,#214576,#214577,#214578,#214579,
#214580,#214581,#214582,#214583,#214584,#214585,#214586,#214587,#214588,
#214589,#214590,#214591,#214592,#214593,#214594,#214595,#214596,#214597,
#214598,#214599,#214600,#214601,#214602,#214603,#214604,#214605,#214606,
#214607,#214608,#214609,#214610,#214611,#214612,#214613,#214614,#214615,
#214616,#214617,#214618,#214619,#214620,#214621,#214622,#214623,#214624,
#214625,#214626,#214627,#214628,#214629,#214630,#214631,#214632,#214633,
#214634,#214635,#214636,#214637,#214638,#214639,#214640,#214641,#214642,
#214643,#214644,#214645,#214646,#214647,#214648,#214649,#214650,#214651,
#214652,#214653,#214654,#214655,#214656,#214657,#214658,#214659,#214660,
#214661,#214662,#214663,#214664,#214665,#214666,#214667,#214668,#214669,
#214670,#214671,#214672,#214673,#214674,#214675,#214676,#214677,#214678,
#214679,#214680,#214681,#214682,#214683,#214684,#214685,#214686,#214687,
#214688,#214689,#214690,#214691,#214692,#214693,#214694,#214695,#214696,
#214697,#214698,#214699,#214700,#214701,#214702,#214703,#214704),
 .UNSPECIFIED.,.F.,.F.,(4,3,3,3,3,3,3,3,3,3,3,3,3,3,3,3,3,3,3,3,3,3,3,3,
3,3,3,3,3,3,3,3,3,3,3,3,3,3,3,3,3,3,3,3,3,3,3,3,3,3,3,3,4),(380.132711084365,
380.215173290451,380.297635148239,380.38009666458,380.462557846324,380.54501870032,
380.627479233419,380.709939452469,380.79239936432,380.874858975819,380.957318293816,
381.039777325158,381.122236076693,381.204694555269,381.287152767734,381.369610720934,
381.452068421717,381.534525876929,381.616983093416,381.702995681206,381.786320375626,
381.868786981185,381.951252742535,382.033717687094,382.116181842272,382.198645235479,
382.281107894122,382.363569845606,382.446031117333,382.528491736701,382.610951731108,
382.69341112795,382.775869954618,382.858328238504,382.940786006997,383.023243287485,
383.107377200935,383.189843199233,383.272307575782,383.354770440224,383.43723190218,
383.519692071254,383.602151057029,383.684608969072,383.770206085772,383.852670822716,
383.935132595014,384.017591841105,384.100048999284,384.182511518183,384.264969189466,
384.347427980374,384.369385902676),.UNSPECIFIED.);
#3505=B_SPLINE_CURVE_WITH_KNOTS('',3,(#214710,#214711,#214712,#214713,#214714,
#214715,#214716,#214717,#214718,#214719,#214720,#214721,#214722,#214723,
#214724,#214725,#214726,#214727,#214728,#214729,#214730,#214731,#214732,
#214733,#214734,#214735,#214736,#214737,#214738,#214739,#214740,#214741,
#214742,#214743,#214744,#214745,#214746,#214747,#214748,#214749,#214750,
#214751,#214752,#214753,#214754,#214755,#214756,#214757,#214758,#214759,
#214760,#214761,#214762,#214763,#214764,#214765,#214766,#214767,#214768,
#214769,#214770,#214771,#214772,#214773,#214774,#214775,#214776,#214777,
#214778,#214779,#214780,#214781,#214782,#214783,#214784,#214785,#214786,
#214787,#214788,#214789,#214790,#214791,#214792,#214793,#214794,#214795,
#214796,#214797,#214798,#214799,#214800,#214801,#214802,#214803,#214804,
#214805,#214806,#214807,#214808,#214809,#214810,#214811,#214812,#214813,
#214814,#214815,#214816,#214817,#214818,#214819,#214820,#214821,#214822,
#214823,#214824,#214825,#214826,#214827,#214828,#214829,#214830,#214831,
#214832,#214833,#214834,#214835,#214836,#214837,#214838,#214839,#214840,
#214841,#214842,#214843,#214844,#214845,#214846,#214847,#214848,#214849,
#214850,#214851,#214852,#214853,#214854,#214855,#214856,#214857,#214858,
#214859,#214860,#214861,#214862,#214863,#214864,#214865,#214866,#214867,
#214868,#214869,#214870,#214871,#214872,#214873,#214874,#214875,#214876,
#214877,#214878),.UNSPECIFIED.,.F.,.F.,(4,3,3,3,3,3,3,3,3,3,3,3,3,3,3,3,
3,3,3,3,3,3,3,3,3,3,3,3,3,3,3,3,3,3,3,3,3,3,3,3,3,3,3,3,3,3,3,3,3,3,3,3,
3,3,3,3,4),(386.415896391545,386.504650454752,386.594152180165,386.684007274919,
386.77427201933,386.823489146394,386.899545653148,386.975506471142,387.051388391762,
387.127208125269,387.202982319599,387.280388139932,387.356135896047,387.431890901575,
387.507668166805,387.586308345668,387.662217532137,387.738183524079,387.814255721689,
387.822228882257,387.899787733802,387.977254277697,388.05464418099,388.131973055683,
388.209256469826,388.286517516398,388.363768217242,388.441022619928,388.51829477146,
388.595640109597,388.673022883322,388.75051237897,388.820968618119,388.905187901012,
388.989280579985,389.073167205799,389.156924195185,389.240465897844,389.32033848605,
389.397705681843,389.475091271294,389.552509053082,389.630013974694,389.707568573947,
389.785229920899,389.819708353981,389.899336225541,389.978889817429,390.058381448263,
390.137816628524,390.217218793118,390.29659904664,390.375968477917,390.455354592249,
390.534748496362,390.614182588444,390.652606861601),.UNSPECIFIED.);
#3506=B_SPLINE_CURVE_WITH_KNOTS('',3,(#214879,#214880,#214881,#214882,#214883,
#214884,#214885,#214886,#214887,#214888,#214889,#214890,#214891,#214892,
#214893,#214894,#214895,#214896,#214897,#214898,#214899,#214900,#214901,
#214902,#214903,#214904,#214905,#214906,#214907,#214908,#214909,#214910,
#214911,#214912,#214913,#214914,#214915,#214916,#214917,#214918,#214919,
#214920,#214921,#214922,#214923,#214924,#214925,#214926,#214927,#214928,
#214929,#214930,#214931,#214932,#214933,#214934,#214935,#214936,#214937,
#214938,#214939,#214940,#214941,#214942,#214943,#214944,#214945,#214946,
#214947,#214948,#214949,#214950,#214951,#214952,#214953,#214954),
 .UNSPECIFIED.,.F.,.F.,(4,3,3,3,3,3,3,3,3,3,3,3,3,3,3,3,3,3,3,3,3,3,3,3,
3,4),(384.369385902676,384.451847506435,384.534308444314,384.616768743712,
384.699228432025,384.781687536647,384.86414608497,384.946604104384,385.029061622277,
385.115738795357,385.198205580965,385.280670694097,385.363134244403,385.445596341517,
385.528057095049,385.610516614592,385.692975009719,385.77543238999,385.857898775809,
385.940361977433,386.022822433381,386.105280582018,386.18774618603,386.270206064607,
386.352670176344,386.415896391545),.UNSPECIFIED.);
#3507=B_SPLINE_CURVE_WITH_KNOTS('',3,(#214956,#214957,#214958,#214959,#214960,
#214961,#214962,#214963,#214964,#214965,#214966,#214967,#214968,#214969,
#214970,#214971,#214972,#214973,#214974,#214975,#214976,#214977,#214978,
#214979,#214980,#214981,#214982,#214983,#214984,#214985,#214986,#214987,
#214988,#214989,#214990,#214991,#214992,#214993,#214994,#214995,#214996,
#214997,#214998,#214999,#215000,#215001,#215002,#215003,#215004,#215005,
#215006,#215007,#215008,#215009,#215010,#215011,#215012,#215013,#215014,
#215015,#215016,#215017,#215018,#215019,#215020,#215021,#215022,#215023,
#215024,#215025,#215026,#215027,#215028,#215029,#215030,#215031),
 .UNSPECIFIED.,.F.,.F.,(4,3,3,3,3,3,3,3,3,3,3,3,3,3,3,3,3,3,3,3,3,3,3,3,
3,4),(384.369385902676,384.451847506434,384.534308444313,384.616768743711,
384.699228432025,384.781687536647,384.86414608497,384.946604104384,385.029061622277,
385.11573879535,385.198205580958,385.28067069409,385.363134244396,385.44559634151,
385.528057095042,385.610516614585,385.692975009712,385.775432389983,385.857898775802,
385.940361977426,386.022822433374,386.10528058201,386.187746186022,386.2702060646,
386.352670176336,386.415896391442),.UNSPECIFIED.);
#3508=B_SPLINE_CURVE_WITH_KNOTS('',3,(#215032,#215033,#215034,#215035,#215036,
#215037,#215038,#215039,#215040,#215041,#215042,#215043,#215044,#215045,
#215046,#215047,#215048,#215049,#215050,#215051,#215052,#215053,#215054,
#215055,#215056,#215057,#215058,#215059,#215060,#215061,#215062,#215063,
#215064,#215065,#215066,#215067,#215068,#215069,#215070,#215071,#215072,
#215073,#215074,#215075,#215076,#215077,#215078,#215079,#215080,#215081,
#215082,#215083,#215084,#215085,#215086,#215087,#215088,#215089,#215090,
#215091,#215092,#215093,#215094,#215095,#215096,#215097,#215098,#215099,
#215100,#215101,#215102,#215103,#215104,#215105,#215106,#215107,#215108,
#215109,#215110,#215111,#215112,#215113,#215114,#215115,#215116,#215117,
#215118,#215119,#215120,#215121,#215122,#215123,#215124,#215125,#215126,
#215127,#215128,#215129,#215130,#215131,#215132,#215133,#215134,#215135,
#215136,#215137,#215138,#215139,#215140,#215141,#215142,#215143,#215144,
#215145,#215146,#215147,#215148,#215149,#215150,#215151,#215152,#215153,
#215154,#215155,#215156,#215157,#215158,#215159,#215160,#215161,#215162,
#215163,#215164,#215165,#215166,#215167,#215168,#215169,#215170,#215171,
#215172,#215173,#215174,#215175,#215176,#215177,#215178,#215179,#215180,
#215181,#215182,#215183,#215184,#215185,#215186,#215187,#215188),
 .UNSPECIFIED.,.F.,.F.,(4,3,3,3,3,3,3,3,3,3,3,3,3,3,3,3,3,3,3,3,3,3,3,3,
3,3,3,3,3,3,3,3,3,3,3,3,3,3,3,3,3,3,3,3,3,3,3,3,3,3,3,3,4),(386.415896391544,
386.498358597629,386.580820455418,386.663281971759,386.745743153503,386.828204007499,
386.910664540598,386.993124759648,387.075584671499,387.158044282998,387.240503600995,
387.322962632337,387.405421383872,387.487879862449,387.570338074913,387.652796028114,
387.735253728896,387.817711184108,387.900168400596,387.986180988385,388.069505682806,
388.151972288365,388.234438049715,388.316902994273,388.399367149451,388.481830542659,
388.564293201302,388.646755152786,388.729216424513,388.811677043881,388.894137038288,
388.976596435129,389.059055261798,389.141513545684,389.223971314178,389.306428594666,
389.390562508115,389.473028506413,389.555492882962,389.637955747404,389.720417209361,
389.802877378435,389.885336364209,389.967794276252,390.053391392953,390.135856129896,
390.218317902195,390.300777148286,390.383234306464,390.465696825363,390.548154496647,
390.630613287555,390.652571209856),.UNSPECIFIED.);
#3509=B_SPLINE_CURVE_WITH_KNOTS('',3,(#215194,#215195,#215196,#215197,#215198,
#215199,#215200,#215201,#215202,#215203,#215204,#215205,#215206,#215207,
#215208,#215209,#215210,#215211,#215212,#215213,#215214,#215215,#215216,
#215217,#215218,#215219,#215220,#215221,#215222,#215223,#215224,#215225,
#215226,#215227,#215228,#215229,#215230,#215231,#215232,#215233,#215234,
#215235,#215236,#215237,#215238,#215239,#215240,#215241,#215242,#215243,
#215244,#215245,#215246,#215247,#215248,#215249,#215250,#215251,#215252,
#215253,#215254,#215255,#215256,#215257,#215258,#215259,#215260,#215261,
#215262,#215263,#215264,#215265,#215266,#215267,#215268,#215269,#215270,
#215271,#215272,#215273,#215274,#215275,#215276,#215277,#215278,#215279,
#215280,#215281,#215282,#215283,#215284,#215285,#215286,#215287,#215288,
#215289,#215290,#215291,#215292,#215293,#215294,#215295,#215296,#215297,
#215298,#215299,#215300,#215301,#215302,#215303,#215304,#215305,#215306,
#215307,#215308,#215309,#215310,#215311,#215312,#215313,#215314,#215315,
#215316,#215317,#215318,#215319,#215320,#215321,#215322,#215323,#215324,
#215325,#215326,#215327,#215328,#215329,#215330,#215331,#215332,#215333,
#215334,#215335,#215336,#215337,#215338,#215339,#215340,#215341,#215342,
#215343,#215344,#215345,#215346,#215347,#215348,#215349,#215350,#215351,
#215352,#215353,#215354,#215355,#215356,#215357,#215358,#215359,#215360,
#215361,#215362,#215363,#215364,#215365),.UNSPECIFIED.,.F.,.F.,(4,3,3,3,
3,3,3,3,3,3,3,3,3,3,3,3,3,3,3,3,3,3,3,3,3,3,3,3,3,3,3,3,3,3,3,3,3,3,3,3,
3,3,3,3,3,3,3,3,3,3,3,3,3,3,3,3,3,4),(392.699081698724,392.79972704102,
392.815927561568,392.894306582437,392.972619333752,393.050880229906,393.129103647704,
393.207303935863,393.285512125028,393.363728178517,393.441965095746,393.5202358859,
393.598599465372,393.67701259483,393.755542977343,393.81466729743,393.890723804189,
393.966684622188,394.042566542813,394.118386276325,394.194160470661,394.27156629099,
394.34731404711,394.423069052643,394.498846317879,394.577486496732,394.653395683206,
394.729361675153,394.805433872768,394.813407033292,394.89096588483,394.968432428718,
395.045822332004,395.12315120669,395.200434620826,395.277695667392,395.354946368229,
395.432200770908,395.509472922434,395.586818260565,395.664201034284,395.741690529925,
395.812146769154,395.896366052048,395.980458731022,396.064345356835,396.148102346221,
396.231644048878,396.311516637085,396.388883832911,396.466269422395,396.543687204217,
396.621192125864,396.698746725151,396.776408072139,396.810886505016,396.890507206535,
396.935844184755),.UNSPECIFIED.);
#3510=B_SPLINE_CURVE_WITH_KNOTS('',3,(#215366,#215367,#215368,#215369,#215370,
#215371,#215372,#215373,#215374,#215375,#215376,#215377,#215378,#215379,
#215380,#215381,#215382,#215383,#215384,#215385,#215386,#215387,#215388,
#215389,#215390,#215391,#215392,#215393,#215394,#215395,#215396,#215397,
#215398,#215399,#215400,#215401,#215402,#215403,#215404,#215405,#215406,
#215407,#215408,#215409,#215410,#215411,#215412,#215413,#215414,#215415,
#215416,#215417,#215418,#215419,#215420,#215421,#215422,#215423,#215424,
#215425,#215426,#215427,#215428,#215429,#215430,#215431,#215432,#215433,
#215434,#215435,#215436,#215437,#215438,#215439,#215440,#215441,#215442,
#215443,#215444),.UNSPECIFIED.,.F.,.F.,(4,3,3,3,3,3,3,3,3,3,3,3,3,3,3,3,
3,3,3,3,3,3,3,3,3,3,4),(390.652606861601,390.735527475722,390.818448089843,
390.895163096693,390.971811009058,391.048406520798,391.124965418497,391.201502802577,
391.278044323031,391.317817957774,391.402494295978,391.487316780488,391.572339151359,
391.657448033164,391.742677572534,391.817187825705,391.89874408837,391.980225028041,
392.06430819444,392.145633946956,392.231095820296,392.316557693636,392.393372171278,
392.470216316175,392.547073509146,392.624000772024,392.699081698624),
 .UNSPECIFIED.);
#3511=B_SPLINE_CURVE_WITH_KNOTS('',3,(#215446,#215447,#215448,#215449,#215450,
#215451,#215452,#215453,#215454,#215455,#215456,#215457,#215458,#215459,
#215460,#215461,#215462,#215463,#215464,#215465,#215466,#215467,#215468,
#215469,#215470,#215471,#215472,#215473,#215474,#215475,#215476,#215477,
#215478,#215479,#215480,#215481,#215482,#215483,#215484,#215485,#215486,
#215487,#215488,#215489,#215490,#215491,#215492,#215493,#215494,#215495,
#215496,#215497,#215498,#215499,#215500,#215501,#215502,#215503,#215504,
#215505,#215506,#215507,#215508,#215509,#215510,#215511,#215512,#215513,
#215514,#215515,#215516,#215517,#215518,#215519,#215520,#215521),
 .UNSPECIFIED.,.F.,.F.,(4,3,3,3,3,3,3,3,3,3,3,3,3,3,3,3,3,3,3,3,3,3,3,3,
3,4),(390.652571209856,390.735032813614,390.817493751493,390.899954050891,
390.982413739205,391.064872843827,391.14733139215,391.229789411564,391.312246929457,
391.398924102536,391.481390888145,391.563856001276,391.646319551583,391.728781648697,
391.811242402229,391.893701921771,391.976160316898,392.058617697169,392.141084082989,
392.223547284613,392.306007740561,392.388465889198,392.470931493209,392.553391371787,
392.635855483523,392.699081698724),.UNSPECIFIED.);
#3512=B_SPLINE_CURVE_WITH_KNOTS('',3,(#215522,#215523,#215524,#215525,#215526,
#215527,#215528,#215529,#215530,#215531,#215532,#215533,#215534,#215535,
#215536,#215537,#215538,#215539,#215540,#215541,#215542,#215543,#215544,
#215545,#215546,#215547,#215548,#215549,#215550,#215551,#215552,#215553,
#215554,#215555,#215556,#215557,#215558,#215559,#215560,#215561,#215562,
#215563,#215564,#215565,#215566,#215567,#215568,#215569,#215570,#215571,
#215572,#215573,#215574,#215575,#215576,#215577,#215578,#215579,#215580,
#215581,#215582,#215583,#215584,#215585,#215586,#215587,#215588,#215589,
#215590,#215591,#215592,#215593,#215594,#215595,#215596,#215597,#215598,
#215599,#215600,#215601,#215602,#215603,#215604,#215605,#215606,#215607,
#215608,#215609,#215610,#215611,#215612,#215613,#215614,#215615,#215616,
#215617,#215618,#215619,#215620,#215621,#215622,#215623,#215624,#215625,
#215626,#215627,#215628,#215629,#215630,#215631,#215632,#215633,#215634,
#215635,#215636,#215637,#215638,#215639,#215640,#215641,#215642,#215643,
#215644,#215645,#215646,#215647,#215648,#215649,#215650,#215651,#215652,
#215653,#215654,#215655,#215656,#215657,#215658,#215659,#215660,#215661,
#215662,#215663,#215664,#215665,#215666,#215667,#215668,#215669,#215670,
#215671,#215672,#215673,#215674,#215675,#215676,#215677,#215678,#215679,
#215680,#215681,#215682,#215683,#215684,#215685,#215686,#215687,#215688,
#215689,#215690),.UNSPECIFIED.,.F.,.F.,(4,3,3,3,3,3,3,3,3,3,3,3,3,3,3,3,
3,3,3,3,3,3,3,3,3,3,3,3,3,3,3,3,3,3,3,3,3,3,3,3,3,3,3,3,3,3,3,3,3,3,3,3,
3,3,3,3,4),(392.699081698724,392.777830761647,392.85663332107,392.935550977874,
393.014532882935,393.093641726665,393.133611947173,393.213232685917,393.292780513573,
393.372267742848,393.451706639762,393.531109432568,393.610494645467,393.689870876019,
393.769249205569,393.84864071544,393.928085950271,394.007559531051,394.087106643101,
394.132351683035,394.209066689885,394.28571460225,394.36231011399,394.438869011689,
394.515406395769,394.591947916223,394.631721550966,394.71639788917,394.801220373679,
394.886242744551,394.971351626355,395.056581165726,395.131091418897,395.212647681562,
395.294128621233,395.378211787632,395.459537540149,395.544999413488,395.630461286828,
395.709864627708,395.789286398866,395.868737376503,395.948261542719,396.02782745326,
396.107477301459,396.12983115476,396.208217376618,396.286535395908,396.36764403172,
396.445867701643,396.524071001022,396.602266930714,396.680468484783,396.75871325386,
396.836983558174,396.915317696091,396.935404482405),.UNSPECIFIED.);
#3513=B_SPLINE_CURVE_WITH_KNOTS('',3,(#215696,#215697,#215698,#215699,#215700,
#215701,#215702,#215703,#215704,#215705,#215706,#215707,#215708,#215709,
#215710,#215711,#215712,#215713,#215714,#215715,#215716,#215717,#215718,
#215719,#215720,#215721,#215722,#215723,#215724,#215725,#215726,#215727,
#215728,#215729,#215730,#215731,#215732,#215733,#215734,#215735,#215736,
#215737,#215738,#215739,#215740,#215741,#215742,#215743,#215744,#215745,
#215746,#215747,#215748,#215749,#215750,#215751,#215752,#215753,#215754,
#215755,#215756,#215757,#215758,#215759,#215760,#215761,#215762,#215763,
#215764,#215765,#215766,#215767,#215768,#215769,#215770,#215771,#215772,
#215773,#215774,#215775,#215776,#215777,#215778,#215779,#215780,#215781,
#215782,#215783,#215784,#215785,#215786,#215787,#215788,#215789,#215790,
#215791,#215792,#215793,#215794,#215795,#215796,#215797,#215798,#215799,
#215800,#215801,#215802,#215803,#215804,#215805,#215806,#215807,#215808,
#215809,#215810,#215811,#215812,#215813,#215814,#215815,#215816,#215817,
#215818,#215819,#215820,#215821,#215822,#215823,#215824,#215825,#215826,
#215827,#215828,#215829,#215830,#215831,#215832,#215833,#215834,#215835,
#215836,#215837,#215838,#215839,#215840,#215841,#215842,#215843,#215844,
#215845,#215846,#215847,#215848,#215849,#215850,#215851,#215852,#215853,
#215854,#215855,#215856,#215857,#215858,#215859,#215860,#215861,#215862,
#215863,#215864),.UNSPECIFIED.,.F.,.F.,(4,3,3,3,3,3,3,3,3,3,3,3,3,3,3,3,
3,3,3,3,3,3,3,3,3,3,3,3,3,3,3,3,3,3,3,3,3,3,3,3,3,3,3,3,3,3,3,3,3,3,3,3,
3,3,3,3,4),(398.982267005904,399.063634215596,399.142909954305,399.225322899488,
399.307735844672,399.387139185638,399.466560956889,399.546011934626,399.625536100951,
399.705102011607,399.784751859929,399.807105712603,399.885484732299,399.963797482429,
400.042058377388,400.120281793984,400.198482080935,400.276690268887,400.354906321163,
400.433143237177,400.511414026118,400.589777604387,400.668190732646,400.746721113976,
400.805845448465,400.881901957122,400.957862777017,401.033744699532,401.10956443493,
401.185338631146,401.262744450294,401.338492208272,401.414247215654,401.490024482729,
401.568664658129,401.644573846404,401.720539840141,401.79661203952,401.804585184327,
401.882144036821,401.959610581679,402.037000485951,402.114329361636,402.191612776783,
402.268873824374,402.346124526246,402.423378929968,402.500651082543,402.577996421729,
402.655379196506,402.732868693204,402.803324920189,402.88755931429,402.971602904374,
403.05552503406,403.139244949316,403.219444425455),.UNSPECIFIED.);
#3514=B_SPLINE_CURVE_WITH_KNOTS('',3,(#215865,#215866,#215867,#215868,#215869,
#215870,#215871,#215872,#215873,#215874,#215875,#215876,#215877,#215878,
#215879,#215880,#215881,#215882,#215883,#215884,#215885,#215886,#215887,
#215888,#215889,#215890,#215891,#215892,#215893,#215894,#215895,#215896,
#215897,#215898,#215899,#215900,#215901,#215902,#215903,#215904,#215905,
#215906,#215907,#215908,#215909,#215910,#215911,#215912,#215913,#215914,
#215915,#215916,#215917,#215918,#215919,#215920,#215921,#215922,#215923,
#215924,#215925,#215926,#215927,#215928,#215929,#215930,#215931,#215932,
#215933,#215934,#215935,#215936,#215937,#215938,#215939,#215940,#215941,
#215942,#215943),.UNSPECIFIED.,.F.,.F.,(4,3,3,3,3,3,3,3,3,3,3,3,3,3,3,3,
3,3,3,3,3,3,3,3,3,3,4),(396.935844184755,397.015355975617,397.094814162802,
397.174230989716,397.253655396111,397.333034128618,397.412410198368,397.491794685822,
397.571252574586,397.650712739704,397.730252956172,397.809626240879,397.886341248167,
397.962989160966,398.039584673138,398.116143571262,398.192680955763,398.269222476631,
398.30899610881,398.39367244587,398.478494929206,398.563517298882,398.648626179487,
398.733855717675,398.808365976741,398.898235537162,398.982267005821),
 .UNSPECIFIED.);
#3515=B_SPLINE_CURVE_WITH_KNOTS('',3,(#215945,#215946,#215947,#215948,#215949,
#215950,#215951,#215952,#215953,#215954,#215955,#215956,#215957,#215958,
#215959,#215960,#215961,#215962,#215963,#215964,#215965,#215966,#215967,
#215968,#215969,#215970,#215971,#215972,#215973,#215974,#215975,#215976,
#215977,#215978,#215979,#215980,#215981,#215982,#215983,#215984,#215985,
#215986,#215987,#215988,#215989,#215990,#215991,#215992,#215993,#215994,
#215995,#215996,#215997,#215998,#215999,#216000,#216001,#216002,#216003,
#216004,#216005,#216006,#216007,#216008,#216009,#216010,#216011,#216012,
#216013,#216014,#216015,#216016,#216017,#216018,#216019,#216020,#216021,
#216022,#216023,#216024,#216025,#216026,#216027,#216028,#216029),
 .UNSPECIFIED.,.F.,.F.,(4,3,3,3,3,3,3,3,3,3,3,3,3,3,3,3,3,3,3,3,3,3,3,3,
3,3,3,3,4),(396.935404482405,397.013834312093,397.092374912414,397.128570890622,
397.204627397381,397.28058821538,397.356470136005,397.432289869517,397.508064063853,
397.585469884182,397.661217640302,397.736972645836,397.812749911071,397.891390089924,
397.967299276398,398.043265268346,398.11933746596,398.127310626484,398.204177103907,
398.280951228283,398.3576492898,398.435726504298,398.512319806502,398.588890633907,
398.66545359003,398.74465694397,398.821274599742,398.901770802766,398.982267005789),
 .UNSPECIFIED.);
#3516=B_SPLINE_CURVE_WITH_KNOTS('',3,(#216030,#216031,#216032,#216033,#216034,
#216035,#216036,#216037,#216038,#216039,#216040,#216041,#216042,#216043,
#216044,#216045,#216046,#216047,#216048,#216049,#216050,#216051,#216052,
#216053,#216054,#216055,#216056,#216057,#216058,#216059,#216060,#216061,
#216062,#216063,#216064,#216065,#216066,#216067,#216068,#216069,#216070,
#216071,#216072,#216073,#216074,#216075,#216076,#216077,#216078,#216079,
#216080,#216081,#216082,#216083,#216084,#216085,#216086,#216087,#216088,
#216089,#216090,#216091,#216092,#216093,#216094,#216095,#216096,#216097,
#216098,#216099,#216100,#216101,#216102,#216103,#216104,#216105,#216106,
#216107,#216108,#216109,#216110,#216111,#216112,#216113,#216114,#216115,
#216116,#216117,#216118,#216119,#216120,#216121,#216122,#216123,#216124,
#216125,#216126,#216127,#216128,#216129,#216130,#216131,#216132,#216133,
#216134,#216135,#216136,#216137,#216138,#216139,#216140,#216141,#216142,
#216143,#216144,#216145,#216146,#216147,#216148,#216149,#216150,#216151,
#216152,#216153,#216154,#216155,#216156,#216157,#216158,#216159,#216160,
#216161,#216162,#216163,#216164,#216165,#216166,#216167,#216168,#216169,
#216170,#216171,#216172,#216173,#216174,#216175,#216176,#216177,#216178,
#216179,#216180,#216181,#216182,#216183,#216184,#216185,#216186,#216187,
#216188,#216189,#216190,#216191,#216192,#216193,#216194,#216195,#216196,
#216197,#216198),.UNSPECIFIED.,.F.,.F.,(4,3,3,3,3,3,3,3,3,3,3,3,3,3,3,3,
3,3,3,3,3,3,3,3,3,3,3,3,3,3,3,3,3,3,3,3,3,3,3,3,3,3,3,3,3,3,3,3,3,3,3,3,
3,3,3,3,4),(398.982267005904,399.095287094402,399.126050362346,399.21026964524,
399.294362324215,399.378248950028,399.462005939414,399.545547642071,399.625420230277,
399.702787426103,399.780173015587,399.857590797408,399.935095719056,400.012650318343,
400.09031166533,400.124790098208,400.204410836847,400.283958664396,400.363445893565,
400.442884790371,400.522287583071,400.601672795864,400.681049026311,400.760427355757,
400.839818865524,400.919264100254,400.998737680935,401.078284792888,401.12352983407,
401.200244841358,401.276892754157,401.353488266328,401.430047164452,401.506584548954,
401.583126069822,401.622899702002,401.707576039062,401.792398522399,401.877420892076,
401.962529772682,402.04775931087,402.122269569933,402.203825833388,402.285306773841,
402.369389939847,402.450715693115,402.536177565489,402.621639437864,402.70104277883,
402.780464550081,402.859915527818,402.939439694143,403.0190056048,403.098655453121,
403.121009305795,403.199396366739,403.219160745219),.UNSPECIFIED.);
#3517=B_SPLINE_CURVE_WITH_KNOTS('',3,(#216204,#216205,#216206,#216207,#216208,
#216209,#216210,#216211,#216212,#216213,#216214,#216215,#216216,#216217,
#216218,#216219,#216220,#216221,#216222,#216223,#216224,#216225,#216226,
#216227,#216228,#216229,#216230,#216231,#216232,#216233,#216234,#216235,
#216236,#216237,#216238,#216239,#216240,#216241,#216242,#216243,#216244,
#216245,#216246,#216247,#216248,#216249,#216250,#216251,#216252,#216253,
#216254,#216255,#216256,#216257,#216258,#216259,#216260,#216261,#216262,
#216263,#216264,#216265,#216266,#216267,#216268,#216269,#216270,#216271,
#216272,#216273,#216274,#216275,#216276,#216277,#216278,#216279,#216280,
#216281,#216282,#216283,#216284,#216285,#216286,#216287,#216288,#216289,
#216290,#216291,#216292,#216293,#216294,#216295,#216296,#216297,#216298,
#216299,#216300,#216301,#216302,#216303,#216304,#216305,#216306,#216307,
#216308,#216309,#216310,#216311,#216312,#216313,#216314,#216315,#216316,
#216317,#216318,#216319,#216320,#216321,#216322,#216323,#216324,#216325,
#216326,#216327,#216328,#216329,#216330,#216331,#216332,#216333,#216334,
#216335,#216336,#216337,#216338,#216339,#216340,#216341,#216342,#216343,
#216344,#216345,#216346,#216347,#216348,#216349,#216350,#216351,#216352,
#216353,#216354,#216355,#216356,#216357,#216358,#216359,#216360),
 .UNSPECIFIED.,.F.,.F.,(4,3,3,3,3,3,3,3,3,3,3,3,3,3,3,3,3,3,3,3,3,3,3,3,
3,3,3,3,3,3,3,3,3,3,3,3,3,3,3,3,3,3,3,3,3,3,3,3,3,3,3,3,4),(405.265452313083,
405.347914519169,405.430376376957,405.512837893298,405.595299075042,405.677759929038,
405.760220462137,405.842680681187,405.925140593038,406.007600204537,406.090059522534,
406.172518553876,406.254977305411,406.337435783987,406.419893996452,406.502351949652,
406.584809650435,406.667267105646,406.749724322134,406.835736909923,406.919061604344,
407.001528209903,407.083993971253,407.166458915812,407.24892307099,407.331386464197,
407.41384912284,407.496311074324,407.578772346051,407.661232965419,407.743692959826,
407.826152356668,407.908611183336,407.991069467222,408.073527235716,408.155984516203,
408.240118429653,408.322584427951,408.4050488045,408.487511668942,408.569973130899,
408.652433299973,408.734892285747,408.81735019779,408.902947314491,408.985412051434,
409.067873823733,409.150333069824,409.232790228002,409.315252746901,409.397710418185,
409.480169209093,409.502127131395),.UNSPECIFIED.);
#3518=B_SPLINE_CURVE_WITH_KNOTS('',3,(#216361,#216362,#216363,#216364,#216365,
#216366,#216367,#216368,#216369,#216370,#216371,#216372,#216373,#216374,
#216375,#216376,#216377,#216378,#216379,#216380,#216381,#216382,#216383,
#216384,#216385,#216386,#216387,#216388,#216389,#216390,#216391,#216392,
#216393,#216394,#216395,#216396,#216397,#216398,#216399,#216400,#216401,
#216402,#216403,#216404,#216405,#216406,#216407,#216408,#216409,#216410,
#216411,#216412,#216413,#216414,#216415,#216416,#216417,#216418,#216419,
#216420,#216421,#216422,#216423,#216424,#216425,#216426,#216427,#216428,
#216429,#216430,#216431,#216432,#216433,#216434,#216435,#216436,#216437,
#216438,#216439,#216440,#216441,#216442),.UNSPECIFIED.,.F.,.F.,(4,3,3,3,
3,3,3,3,3,3,3,3,3,3,3,3,3,3,3,3,3,3,3,3,3,3,3,4),(403.219444425455,403.302694788121,
403.380062027565,403.457447661111,403.534865487393,403.612370453918,403.689925098347,
403.767586490629,403.802064656052,403.881685351219,403.96123313507,404.040720320409,
404.120159173352,404.199561922249,404.278947091578,404.358323278832,404.437701565444,
404.517093032819,404.596538226116,404.676011765899,404.755558838146,404.800804391914,
404.877998399174,404.955121803432,405.03262963019,405.109651357303,405.187402233883,
405.265153110462),.UNSPECIFIED.);
#3519=B_SPLINE_CURVE_WITH_KNOTS('',3,(#216444,#216445,#216446,#216447,#216448,
#216449,#216450,#216451,#216452,#216453,#216454,#216455,#216456,#216457,
#216458,#216459,#216460,#216461,#216462,#216463,#216464,#216465,#216466,
#216467,#216468,#216469,#216470,#216471,#216472,#216473,#216474,#216475,
#216476,#216477,#216478,#216479,#216480,#216481,#216482,#216483,#216484,
#216485,#216486,#216487,#216488,#216489,#216490,#216491,#216492,#216493,
#216494,#216495,#216496,#216497,#216498,#216499,#216500,#216501,#216502,
#216503,#216504,#216505,#216506,#216507,#216508,#216509,#216510,#216511,
#216512,#216513,#216514,#216515,#216516,#216517,#216518,#216519,#216520,
#216521,#216522,#216523,#216524,#216525),.UNSPECIFIED.,.F.,.F.,(4,3,3,3,
3,3,3,3,3,3,3,3,3,3,3,3,3,3,3,3,3,3,3,3,3,3,3,4),(403.219160745219,403.297459048369,
403.375709128334,403.453925353941,403.532122068307,403.610331014814,403.688551105634,
403.766795341942,403.845076736576,403.923451700316,404.00187918644,404.080418314602,
404.119749041657,404.195805550314,404.271766370209,404.347648292724,404.423468028122,
404.499242224338,404.576648043486,404.652395801464,404.728150808847,404.803928075921,
404.882568251321,404.958477439596,405.034443433334,405.110515632713,405.118488777519,
405.265452313083),.UNSPECIFIED.);
#3520=B_SPLINE_CURVE_WITH_KNOTS('',3,(#216526,#216527,#216528,#216529,#216530,
#216531,#216532,#216533,#216534,#216535,#216536,#216537,#216538,#216539,
#216540,#216541,#216542,#216543,#216544,#216545,#216546,#216547,#216548,
#216549,#216550,#216551,#216552,#216553,#216554,#216555,#216556,#216557,
#216558,#216559,#216560,#216561,#216562,#216563,#216564,#216565,#216566,
#216567,#216568,#216569,#216570,#216571,#216572,#216573,#216574,#216575,
#216576,#216577,#216578,#216579,#216580,#216581,#216582,#216583,#216584,
#216585,#216586,#216587,#216588,#216589,#216590,#216591,#216592,#216593,
#216594,#216595,#216596,#216597,#216598,#216599,#216600,#216601,#216602,
#216603,#216604,#216605,#216606,#216607,#216608,#216609,#216610,#216611,
#216612,#216613,#216614,#216615,#216616,#216617,#216618,#216619,#216620,
#216621,#216622,#216623,#216624,#216625,#216626,#216627,#216628,#216629,
#216630,#216631,#216632,#216633,#216634,#216635,#216636,#216637,#216638,
#216639,#216640,#216641,#216642,#216643,#216644,#216645,#216646,#216647,
#216648,#216649,#216650,#216651,#216652,#216653,#216654,#216655,#216656,
#216657,#216658,#216659,#216660,#216661,#216662,#216663,#216664,#216665,
#216666,#216667,#216668,#216669,#216670,#216671,#216672,#216673,#216674,
#216675,#216676,#216677,#216678,#216679,#216680,#216681,#216682,#216683,
#216684,#216685,#216686,#216687,#216688,#216689,#216690,#216691,#216692,
#216693,#216694),.UNSPECIFIED.,.F.,.F.,(4,3,3,3,3,3,3,3,3,3,3,3,3,3,3,3,
3,3,3,3,3,3,3,3,3,3,3,3,3,3,3,3,3,3,3,3,3,3,3,3,3,3,3,3,3,3,3,3,3,3,3,3,
3,3,3,3,4),(405.265452313166,405.341378517376,405.417225780084,405.493010896021,
405.571038098191,405.646755981067,405.722466089584,405.798183499663,405.873923291857,
405.949735362879,406.02559095927,406.101538247612,406.117228513381,406.201447766723,
406.285540416405,406.369427013778,406.45318397536,406.536725651581,406.616598381312,
406.693965620755,406.771351254302,406.848769080582,406.926274047107,407.003828691536,
407.081490083817,407.115968249244,407.195588944411,407.275136728262,407.354623913601,
407.434062766544,407.513465515443,407.592850684772,407.672226872027,407.751605158638,
407.830996626014,407.910441819311,407.989915359094,408.069462431341,408.114707985106,
408.191423080311,408.268071080107,408.344666678293,408.421225660755,408.497763128661,
408.574304731257,408.614077853037,408.69875415266,408.783576599501,408.868598934868,
408.953707782589,409.038937290848,409.113447720968,409.19501438971,409.276478797015,
409.357879826288,409.439202918048,409.502552124195),.UNSPECIFIED.);
#3521=B_SPLINE_CURVE_WITH_KNOTS('',3,(#216700,#216701,#216702,#216703,#216704,
#216705,#216706,#216707,#216708,#216709,#216710,#216711,#216712,#216713,
#216714,#216715,#216716,#216717,#216718,#216719,#216720,#216721,#216722,
#216723,#216724,#216725,#216726,#216727,#216728,#216729,#216730,#216731,
#216732,#216733,#216734,#216735,#216736,#216737,#216738,#216739,#216740,
#216741,#216742,#216743,#216744,#216745,#216746,#216747,#216748,#216749,
#216750,#216751,#216752,#216753,#216754,#216755,#216756,#216757,#216758,
#216759,#216760,#216761,#216762,#216763,#216764,#216765,#216766,#216767,
#216768,#216769,#216770,#216771,#216772,#216773,#216774,#216775,#216776,
#216777,#216778,#216779,#216780,#216781,#216782,#216783,#216784,#216785,
#216786,#216787,#216788,#216789,#216790,#216791,#216792,#216793,#216794,
#216795,#216796,#216797,#216798,#216799,#216800,#216801,#216802,#216803,
#216804,#216805,#216806,#216807,#216808,#216809,#216810,#216811,#216812,
#216813,#216814,#216815,#216816,#216817,#216818,#216819,#216820,#216821,
#216822,#216823,#216824,#216825,#216826,#216827,#216828,#216829,#216830,
#216831,#216832,#216833,#216834,#216835,#216836,#216837,#216838,#216839,
#216840,#216841,#216842,#216843,#216844,#216845,#216846,#216847,#216848,
#216849,#216850,#216851,#216852,#216853,#216854,#216855,#216856),
 .UNSPECIFIED.,.F.,.F.,(4,3,3,3,3,3,3,3,3,3,3,3,3,3,3,3,3,3,3,3,3,3,3,3,
3,3,3,3,3,3,3,3,3,3,3,3,3,3,3,3,3,3,3,3,3,3,3,3,3,3,3,3,4),(411.548637620348,
411.631099826433,411.713561684221,411.796023200562,411.878484382306,411.960945236303,
412.043405769402,412.125865988452,412.208325900302,412.290785511802,412.373244829798,
412.45570386114,412.538162612676,412.620621091252,412.703079303717,412.785537256917,
412.8679949577,412.950452412912,413.032909629399,413.118922217186,413.202246911604,
413.284713517163,413.367179278513,413.449644223071,413.532108378249,413.614571771457,
413.6970344301,413.779496381584,413.86195765331,413.944418272679,414.026878267086,
414.109337663927,414.191796490595,414.274254774482,414.356712542975,414.439169823463,
414.523303736907,414.605769735206,414.688234111755,414.770696976197,414.853158438153,
414.935618607227,415.018077593002,415.100535505045,415.186132621736,415.26859735868,
415.351059130978,415.433518377069,415.515975535248,415.598438054146,415.68089572543,
415.763354516338,415.785312438575),.UNSPECIFIED.);
#3522=B_SPLINE_CURVE_WITH_KNOTS('',3,(#216857,#216858,#216859,#216860,#216861,
#216862,#216863,#216864,#216865,#216866,#216867,#216868,#216869,#216870,
#216871,#216872,#216873,#216874,#216875,#216876,#216877,#216878,#216879,
#216880,#216881,#216882,#216883,#216884,#216885,#216886,#216887,#216888,
#216889,#216890,#216891,#216892,#216893,#216894,#216895,#216896,#216897,
#216898,#216899,#216900,#216901,#216902,#216903,#216904,#216905,#216906,
#216907,#216908,#216909,#216910,#216911,#216912,#216913,#216914,#216915,
#216916,#216917,#216918,#216919,#216920,#216921,#216922,#216923,#216924,
#216925,#216926,#216927,#216928,#216929,#216930,#216931,#216932),
 .UNSPECIFIED.,.F.,.F.,(4,3,3,3,3,3,3,3,3,3,3,3,3,3,3,3,3,3,3,3,3,3,3,3,
3,4),(409.502127131395,409.584588735153,409.667049673032,409.74950997243,
409.831969660743,409.914428765366,409.996887313689,410.079345333103,410.161802850996,
410.248480024075,410.330946809684,410.413411922815,410.495875473122,410.578337570236,
410.660798323768,410.74325784331,410.825716238437,410.908173618708,410.990640004527,
411.073103206151,411.1555636621,411.238021810736,411.320487414748,411.402947293325,
411.485411405062,411.548637620263),.UNSPECIFIED.);
#3523=B_SPLINE_CURVE_WITH_KNOTS('',3,(#216934,#216935,#216936,#216937,#216938,
#216939,#216940,#216941,#216942,#216943,#216944,#216945,#216946,#216947,
#216948,#216949,#216950,#216951,#216952,#216953,#216954,#216955,#216956,
#216957,#216958,#216959,#216960,#216961,#216962,#216963,#216964,#216965,
#216966,#216967,#216968,#216969,#216970,#216971,#216972,#216973,#216974,
#216975,#216976,#216977,#216978,#216979,#216980,#216981,#216982,#216983,
#216984,#216985,#216986,#216987,#216988,#216989,#216990,#216991,#216992,
#216993,#216994,#216995,#216996,#216997,#216998,#216999,#217000,#217001,
#217002,#217003,#217004,#217005,#217006,#217007,#217008,#217009,#217010,
#217011,#217012,#217013,#217014,#217015,#217016,#217017,#217018),
 .UNSPECIFIED.,.F.,.F.,(4,3,3,3,3,3,3,3,3,3,3,3,3,3,3,3,3,3,3,3,3,3,3,3,
3,3,3,3,4),(409.502552124195,409.583774702256,409.612817588899,409.692221759622,
409.771644372142,409.851096200842,409.930621227469,410.010188003439,410.089838719134,
410.11218745683,410.190565826128,410.268877919999,410.347138153801,410.425360905306,
410.50356052419,410.581768042459,410.659983424392,410.738219670257,410.81648979009,
410.894852704906,410.973265172075,411.051794902507,411.110927192692,411.192868380011,
411.274627957284,411.356135717751,411.4374923654,411.518643713388,411.548637620263),
 .UNSPECIFIED.);
#3524=B_SPLINE_CURVE_WITH_KNOTS('',3,(#217019,#217020,#217021,#217022,#217023,
#217024,#217025,#217026,#217027,#217028,#217029,#217030,#217031,#217032,
#217033,#217034,#217035,#217036,#217037,#217038,#217039,#217040,#217041,
#217042,#217043,#217044,#217045,#217046,#217047,#217048,#217049,#217050,
#217051,#217052,#217053,#217054,#217055,#217056,#217057,#217058,#217059,
#217060,#217061,#217062,#217063,#217064,#217065,#217066,#217067,#217068,
#217069,#217070,#217071,#217072,#217073,#217074,#217075,#217076,#217077,
#217078,#217079,#217080,#217081,#217082,#217083,#217084,#217085,#217086,
#217087,#217088,#217089,#217090,#217091,#217092,#217093,#217094,#217095,
#217096,#217097,#217098,#217099,#217100,#217101,#217102,#217103,#217104,
#217105,#217106,#217107,#217108,#217109,#217110,#217111,#217112,#217113,
#217114,#217115,#217116,#217117,#217118,#217119,#217120,#217121,#217122,
#217123,#217124,#217125,#217126,#217127,#217128,#217129,#217130,#217131,
#217132,#217133,#217134,#217135,#217136,#217137,#217138,#217139,#217140,
#217141,#217142,#217143,#217144,#217145,#217146,#217147,#217148,#217149,
#217150,#217151,#217152,#217153,#217154,#217155,#217156,#217157,#217158,
#217159,#217160,#217161,#217162,#217163,#217164,#217165,#217166,#217167,
#217168,#217169,#217170,#217171,#217172,#217173,#217174,#217175),
 .UNSPECIFIED.,.F.,.F.,(4,3,3,3,3,3,3,3,3,3,3,3,3,3,3,3,3,3,3,3,3,3,3,3,
3,3,3,3,3,3,3,3,3,3,3,3,3,3,3,3,3,3,3,3,3,3,3,3,3,3,3,3,4),(411.548637620263,
411.631099826349,411.713561684137,411.796023200478,411.878484382222,411.960945236218,
412.043405769317,412.125865988367,412.208325900218,412.290785511717,412.373244829714,
412.455703861056,412.538162612591,412.620621091167,412.703079303632,412.785537256832,
412.867994957615,412.950452412826,413.032909629314,413.118922217103,413.202246911524,
413.284713517082,413.367179278433,413.449644222991,413.532108378169,413.614571771376,
413.69703443002,413.779496381504,413.86195765323,413.944418272598,414.026878267006,
414.109337663847,414.191796490515,414.274254774401,414.356712542895,414.439169823382,
414.523303736832,414.60576973513,414.688234111679,414.770696976121,414.853158438078,
414.935618607152,415.018077592926,415.100535504969,415.18613262167,415.268597358613,
415.351059130912,415.433518377003,415.515975535181,415.59843805408,415.680895725363,
415.763354516271,415.785312438574),.UNSPECIFIED.);
#3525=B_SPLINE_CURVE_WITH_KNOTS('',3,(#217179,#217180,#217181,#217182,#217183,
#217184,#217185,#217186),.UNSPECIFIED.,.F.,.F.,(4,2,2,4),(-4.09265929953245,
-3.25801350823579,-2.42309659634093,-2.07498647268395),.UNSPECIFIED.);
#3526=B_SPLINE_CURVE_WITH_KNOTS('',3,(#217190,#217191,#217192,#217193,#217194,
#217195,#217196,#217197,#217198,#217199,#217200,#217201,#217202,#217203,
#217204,#217205,#217206,#217207,#217208,#217209,#217210,#217211,#217212,
#217213,#217214,#217215,#217216,#217217,#217218,#217219,#217220,#217221,
#217222,#217223,#217224,#217225,#217226,#217227,#217228,#217229,#217230,
#217231,#217232,#217233,#217234,#217235,#217236,#217237,#217238,#217239,
#217240,#217241,#217242,#217243,#217244,#217245,#217246,#217247,#217248,
#217249,#217250,#217251,#217252,#217253,#217254,#217255,#217256,#217257,
#217258,#217259,#217260,#217261,#217262,#217263,#217264,#217265,#217266,
#217267,#217268,#217269,#217270,#217271,#217272,#217273,#217274,#217275,
#217276,#217277,#217278,#217279,#217280,#217281,#217282,#217283,#217284,
#217285,#217286,#217287,#217288,#217289,#217290,#217291,#217292,#217293,
#217294,#217295,#217296,#217297,#217298,#217299,#217300,#217301,#217302,
#217303,#217304,#217305,#217306,#217307,#217308,#217309,#217310,#217311,
#217312,#217313,#217314,#217315,#217316,#217317,#217318,#217319,#217320,
#217321,#217322,#217323,#217324,#217325,#217326,#217327,#217328,#217329,
#217330,#217331,#217332,#217333,#217334,#217335,#217336,#217337,#217338,
#217339,#217340,#217341,#217342,#217343,#217344,#217345,#217346,#217347,
#217348,#217349,#217350,#217351,#217352,#217353,#217354,#217355,#217356,
#217357,#217358,#217359,#217360,#217361,#217362,#217363,#217364,#217365,
#217366,#217367,#217368,#217369,#217370,#217371,#217372,#217373,#217374,
#217375,#217376,#217377,#217378,#217379,#217380,#217381,#217382,#217383,
#217384,#217385,#217386,#217387,#217388,#217389,#217390,#217391,#217392,
#217393,#217394,#217395,#217396,#217397,#217398,#217399,#217400,#217401,
#217402,#217403,#217404,#217405,#217406,#217407,#217408,#217409,#217410,
#217411,#217412,#217413,#217414,#217415,#217416,#217417,#217418,#217419,
#217420,#217421,#217422,#217423,#217424,#217425,#217426,#217427,#217428,
#217429,#217430,#217431,#217432,#217433,#217434,#217435,#217436,#217437,
#217438,#217439,#217440,#217441,#217442,#217443,#217444,#217445,#217446,
#217447,#217448,#217449,#217450,#217451,#217452,#217453,#217454,#217455,
#217456,#217457,#217458,#217459,#217460,#217461,#217462,#217463,#217464,
#217465,#217466,#217467,#217468,#217469,#217470,#217471,#217472,#217473,
#217474,#217475,#217476,#217477,#217478,#217479,#217480,#217481,#217482,
#217483,#217484,#217485,#217486,#217487,#217488,#217489,#217490,#217491,
#217492,#217493,#217494,#217495,#217496,#217497,#217498,#217499,#217500,
#217501,#217502,#217503,#217504,#217505,#217506,#217507,#217508,#217509,
#217510,#217511,#217512,#217513,#217514,#217515,#217516,#217517,#217518,
#217519,#217520,#217521,#217522,#217523,#217524,#217525,#217526,#217527,
#217528,#217529),.UNSPECIFIED.,.F.,.F.,(4,2,2,2,2,2,2,2,2,2,2,2,2,2,2,2,
2,2,2,2,2,2,2,2,2,2,2,2,2,2,2,2,2,2,2,2,2,2,2,2,2,2,2,2,2,2,2,2,2,2,2,2,
2,2,2,2,2,2,2,2,2,2,2,2,2,2,2,2,2,2,2,2,2,2,2,2,2,2,2,2,2,2,2,2,2,2,2,2,
2,2,2,2,2,2,2,2,2,2,2,2,2,2,2,2,2,2,2,2,2,2,2,2,2,2,2,2,2,2,2,2,2,2,2,2,
2,2,2,2,2,2,2,2,2,2,2,2,2,2,2,2,2,2,2,2,2,2,2,2,2,2,2,2,2,2,2,2,2,2,2,2,
2,2,2,2,2,2,2,2,2,4),(6.83182211809342E-5,0.00813194064434937,0.0198778020713646,
0.0650590852607454,0.10988907756809,0.147886015884265,0.161149076596335,
0.173369264417413,0.185313943124287,0.204539234926209,0.259607450626017,
0.34172790800698,0.375399223369378,0.376207524066527,0.376606503276033,
0.376798210729843,0.377691036208974,0.378363680416897,0.378860988397354,
0.379223179482051,0.379483920481797,0.379669996768885,0.37980193825668,
0.379895059126323,0.380302261087459,0.380662631698573,0.380980207630575,
0.381258937597082,0.387313997030125,0.392872299510832,0.399118600020562,
0.410621479147785,0.456960892354912,0.509380295962348,0.530567103295414,
0.542989346639929,0.552108935940903,0.56064813004894,0.569007847514817,
0.582398708581225,0.616963229120582,0.717998183839658,0.751536051927716,
0.770791678898915,0.77668925813288,0.780442588016263,0.783973071226936,
0.788616501153669,0.797174617955982,0.891962341029584,1.0218154441692,1.08265661945942,
1.09647157413381,1.10339455105421,1.1099420946198,1.11703205849066,1.12950987540703,
1.16821773172323,1.24014884072464,1.39726406724103,1.50889892192508,1.54509922288968,
1.54986837336914,1.55228702605543,1.55401808601761,1.55584309579,1.55890948915915,
1.56695922950712,1.68786179283197,1.8155517854012,1.90447107743777,1.9384382540311,
1.94370745644524,1.94643333169015,1.94863870114513,1.95083409042105,1.95479288025936,
1.96693738249264,2.14384450909385,2.2647004462708,2.35787451621018,2.36261987767432,
2.36442883202812,2.36567080008746,2.36688389733508,2.36834078830516,2.37195209780184,
2.40893574495947,2.50760030700269,2.61791378444164,2.68714104507969,2.73436756649004,
2.75904775885284,2.76347290999952,2.7658333594947,2.76759118112479,2.76951035739376,
2.77290287454548,2.78284204267499,2.93428352038161,3.15314642015992,3.16594785894354,
3.16831220917512,3.16979829194121,3.1709589357742,3.17224105427437,3.1743351734981,
3.18159703193165,3.22777277277377,3.27518482878292,3.40016820841547,3.57482013283156,
3.58631013108575,3.59004180820283,3.59237471060776,3.59448423928055,3.59714354444902,
3.60248222439886,3.641600060276,3.72672183690177,3.78819849223625,3.9732529671625,
3.98588269042508,3.98971065649067,3.9919993061417,3.99383274252603,3.99629987998103,
4.00094223777758,4.02756199341562,4.08886049692501,4.28939453883896,4.32185947805448,
4.33115974765688,4.33561232274636,4.33637642441593,4.4227666423236,4.4317996201652,
4.43967724692138,4.4452577148184,4.45111407188919,4.45878527367052,4.47531496023699,
4.57237173510791,4.7365848690502,4.74832440510131,4.75236543754039,4.75525761318156,
4.75800511292837,4.7618537875373,4.76964941969628,4.84909791600552,5.02473203876403,
5.05494477875511,5.06639780060826,5.07329823327692,5.08067591766276,5.09059779513613,
5.11342016595376,5.32851101505927,5.45982460552235,5.46964741486818,5.50510763749313,
5.51009630533926,5.51244372636196,5.51427262820719,5.51625843231705,5.51942774689967,
5.52977694117077,5.58817805985445,5.86891849949769),.UNSPECIFIED.);
#3527=B_SPLINE_CURVE_WITH_KNOTS('',3,(#217531,#217532,#217533,#217534,#217535,
#217536,#217537,#217538,#217539,#217540,#217541,#217542,#217543,#217544,
#217545,#217546,#217547,#217548),.UNSPECIFIED.,.F.,.F.,(4,2,2,2,2,2,2,2,
4),(7.4068340133238,8.24175092521866,9.07666783711352,9.91158474900838,
10.7465016609032,11.5814185727981,12.416335484693,13.2512523965878,13.6900193205034),
 .UNSPECIFIED.);
#3528=B_SPLINE_CURVE_WITH_KNOTS('',3,(#217550,#217551,#217552,#217553,#217554,
#217555,#217556,#217557,#217558,#217559,#217560,#217561),.UNSPECIFIED.,
 .F.,.F.,(4,1,1,1,1,1,1,1,1,4),(13.6900193205034,13.9823563020706,14.9810960379328,
15.4804659058639,15.9798357737949,16.9785755096571,17.9773152455193,18.9760549813814,
19.4754248493125,19.9732045334931),.UNSPECIFIED.);
#3529=B_SPLINE_CURVE_WITH_KNOTS('',3,(#217563,#217564,#217565,#217566,#217567,
#217568,#217569,#217570,#217571,#217572,#217573,#217574,#217575,#217576,
#217577,#217578,#217579,#217580,#217581,#217582,#217583,#217584,#217585,
#217586,#217587,#217588,#217589,#217590,#217591,#217592,#217593,#217594,
#217595,#217596,#217597,#217598,#217599,#217600,#217601,#217602,#217603,
#217604,#217605,#217606,#217607,#217608,#217609,#217610,#217611,#217612,
#217613,#217614,#217615,#217616,#217617,#217618,#217619,#217620,#217621,
#217622,#217623,#217624,#217625,#217626,#217627,#217628,#217629,#217630,
#217631,#217632,#217633,#217634,#217635,#217636,#217637,#217638,#217639,
#217640,#217641,#217642,#217643,#217644,#217645,#217646,#217647,#217648,
#217649,#217650,#217651,#217652,#217653,#217654,#217655,#217656,#217657,
#217658,#217659,#217660,#217661,#217662,#217663,#217664,#217665,#217666,
#217667,#217668,#217669,#217670,#217671,#217672,#217673,#217674,#217675,
#217676,#217677,#217678,#217679,#217680,#217681,#217682,#217683,#217684,
#217685,#217686,#217687,#217688,#217689,#217690,#217691,#217692,#217693,
#217694,#217695,#217696,#217697,#217698,#217699,#217700,#217701,#217702,
#217703,#217704,#217705,#217706,#217707,#217708,#217709,#217710,#217711,
#217712,#217713,#217714,#217715,#217716,#217717,#217718,#217719,#217720,
#217721,#217722,#217723,#217724,#217725,#217726,#217727,#217728,#217729,
#217730,#217731,#217732,#217733,#217734,#217735,#217736,#217737,#217738,
#217739,#217740,#217741,#217742,#217743,#217744,#217745,#217746,#217747,
#217748,#217749,#217750,#217751,#217752,#217753,#217754,#217755,#217756,
#217757,#217758,#217759,#217760,#217761,#217762,#217763,#217764,#217765,
#217766,#217767,#217768,#217769,#217770,#217771,#217772,#217773,#217774,
#217775,#217776,#217777,#217778,#217779,#217780,#217781,#217782,#217783,
#217784,#217785,#217786,#217787,#217788,#217789,#217790,#217791,#217792,
#217793,#217794,#217795,#217796,#217797,#217798,#217799,#217800,#217801,
#217802,#217803,#217804,#217805,#217806,#217807,#217808,#217809,#217810,
#217811,#217812,#217813,#217814,#217815,#217816,#217817,#217818,#217819,
#217820,#217821,#217822,#217823,#217824,#217825,#217826,#217827,#217828,
#217829,#217830,#217831,#217832,#217833,#217834,#217835,#217836,#217837,
#217838,#217839,#217840,#217841,#217842,#217843,#217844,#217845,#217846,
#217847,#217848,#217849,#217850,#217851,#217852,#217853,#217854,#217855,
#217856,#217857,#217858,#217859,#217860,#217861,#217862,#217863,#217864,
#217865,#217866,#217867,#217868,#217869,#217870,#217871,#217872,#217873,
#217874,#217875,#217876,#217877,#217878,#217879,#217880,#217881,#217882,
#217883,#217884,#217885,#217886,#217887,#217888,#217889,#217890,#217891,
#217892,#217893,#217894,#217895,#217896,#217897,#217898,#217899,#217900,
#217901,#217902,#217903,#217904,#217905,#217906,#217907,#217908,#217909,
#217910,#217911,#217912,#217913,#217914,#217915,#217916,#217917,#217918,
#217919,#217920,#217921,#217922,#217923,#217924,#217925,#217926,#217927,
#217928,#217929,#217930,#217931,#217932,#217933,#217934,#217935,#217936,
#217937,#217938,#217939,#217940,#217941,#217942,#217943,#217944,#217945,
#217946,#217947,#217948,#217949,#217950,#217951,#217952,#217953,#217954,
#217955,#217956,#217957,#217958,#217959,#217960,#217961,#217962,#217963,
#217964,#217965,#217966,#217967,#217968,#217969,#217970,#217971,#217972,
#217973,#217974,#217975,#217976,#217977,#217978,#217979,#217980,#217981,
#217982,#217983,#217984,#217985,#217986,#217987,#217988,#217989,#217990,
#217991,#217992,#217993,#217994,#217995,#217996,#217997,#217998,#217999,
#218000,#218001,#218002,#218003,#218004,#218005,#218006,#218007,#218008,
#218009,#218010,#218011,#218012,#218013,#218014,#218015,#218016,#218017,
#218018,#218019,#218020,#218021,#218022,#218023,#218024,#218025,#218026,
#218027,#218028,#218029,#218030,#218031,#218032,#218033,#218034,#218035,
#218036,#218037,#218038,#218039,#218040,#218041,#218042,#218043,#218044,
#218045,#218046,#218047,#218048,#218049,#218050,#218051,#218052,#218053,
#218054,#218055,#218056,#218057,#218058,#218059,#218060,#218061,#218062,
#218063,#218064,#218065,#218066,#218067,#218068,#218069,#218070,#218071,
#218072,#218073,#218074,#218075,#218076,#218077,#218078,#218079,#218080,
#218081,#218082,#218083,#218084,#218085,#218086,#218087,#218088,#218089,
#218090,#218091,#218092,#218093,#218094,#218095,#218096,#218097,#218098,
#218099,#218100,#218101,#218102,#218103,#218104,#218105,#218106,#218107,
#218108,#218109,#218110,#218111,#218112,#218113,#218114,#218115,#218116,
#218117,#218118,#218119,#218120),.UNSPECIFIED.,.F.,.F.,(4,2,2,2,2,2,2,2,
2,2,2,2,2,2,2,2,2,2,2,2,2,2,2,2,2,2,2,2,2,2,2,2,2,2,2,2,2,2,2,2,2,2,2,2,
2,2,2,2,2,2,2,2,2,2,2,2,2,2,2,2,2,2,2,2,2,2,2,2,2,2,2,2,2,2,2,2,2,2,2,2,
2,2,2,2,2,2,2,2,2,2,2,2,2,2,2,2,2,2,2,2,2,2,2,2,2,2,2,2,2,2,2,2,2,2,2,2,
2,2,2,2,2,2,2,2,2,2,2,2,2,2,2,2,2,2,2,2,2,2,2,2,2,2,2,2,2,2,2,2,2,2,2,2,
2,2,2,2,2,2,2,2,2,2,2,2,2,2,2,2,2,2,2,2,2,2,2,2,2,2,2,2,2,2,2,2,2,2,2,2,
2,2,2,2,2,2,2,2,2,2,2,2,2,2,2,2,2,2,2,2,2,2,2,2,2,2,2,2,2,2,2,2,2,2,2,2,
2,2,2,2,2,2,2,2,2,2,2,2,2,2,2,2,2,2,2,2,2,2,2,2,2,2,2,2,2,2,2,2,2,2,2,2,
2,2,2,2,2,2,2,2,2,2,2,2,2,2,2,2,2,2,4),(0.00169250605834049,0.00408492138346118,
0.00757146341587593,0.0104864642879784,0.0134044379630337,0.0183187848536681,
0.0314251930669086,0.170038641662356,0.288246616778126,0.303248212676448,
0.312682850283399,0.319857774097023,0.327213302003405,0.334137907385634,
0.343805750427874,0.369913030709805,0.562493239480834,0.640272395212907,
0.674141160188036,0.732738320347233,0.751326615247076,0.758775020538961,
0.762603997553388,0.765004968465602,0.767247262050247,0.768895084349338,
0.77067322912686,0.773229532147553,0.780358226058807,0.865845819473271,
0.896627539123426,0.978030374063007,1.00338420047898,1.01849216416434,1.0626314665659,
1.13137426030897,1.17561627716773,1.18130973484367,1.18415594285482,1.1861996184324,
1.18835985464576,1.19200138044488,1.20163274021882,1.34763609525156,1.4273558872268,
1.48825106811496,1.54725716368977,1.56915114537342,1.58430708370833,1.59053896738361,
1.59378562833104,1.5958241951731,1.59773785231902,1.59913069596616,1.6006205429543,
1.60274150729589,1.60852089541209,1.70882652927395,1.84704032343686,1.89224868409987,
1.94901072472249,1.95825172610291,1.96209714212466,1.96600399601449,1.96959157879376,
1.97443528270748,1.98644363037358,2.10215848865768,2.27256193946883,2.33179304626633,
2.33819999325205,2.34160411413638,2.34379967855223,2.34551519579621,2.34711574192009,
2.34879671462028,2.351138022787,2.35722339457166,2.4346307920901,2.59667988280613,
2.65653767337051,2.70613894044412,2.73315286120499,2.73789419156163,2.74041154798166,
2.74228120926014,2.74461205927209,2.74850354985693,2.76127656976108,2.94347847968625,
3.06926256755972,3.12101512251245,3.14792657802399,3.16128693409591,3.16378260552575,
3.16512570652083,3.16622886772128,3.16735729484487,3.16947526759535,3.17676381392457,
3.28659948840381,3.44275564633209,3.55810092319401,3.56439981975234,3.5671565354901,
3.56918369910067,3.57105386631777,3.57358831673009,3.5798093370713,3.6434540856021,
3.708218896661,3.85523515638434,3.93931329880087,3.95883825116561,3.96161595928014,
3.96306038870735,3.96412093688517,3.96526408580681,3.96724603487886,3.97280923666566,
4.06468950815282,4.27806378875624,4.34417272045854,4.37505049827141,4.38012302218407,
4.38277775757291,4.38494101065096,4.38710742101876,4.3910498836419,4.40340717404014,
4.59468766717309,4.70527731609155,4.76821509348387,4.77573909733512,4.78156659470898,
4.78426380338545,4.78630902555112,4.78824231565617,4.79093666606993,4.79643627835568,
4.8563966320353,4.97943746243127,5.20349855664505,5.22591289852476,5.23408251376757,
5.23986005413012,5.24591639475465,5.25384118221521,5.27089992227968,5.41277846909467,
5.46850400980107,5.53603061013568,5.54345542429789,5.5471741372855,5.55021127681729,
5.55371510377716,5.55981632388456,5.58614692827814,5.70555379263311,5.80627537059302,
5.84329942029978,5.85570857535668,5.86278843508173,5.86934832450355,5.87832378549833,
5.89600420093851,5.99798307266371,6.13762691073564,6.25372136397141,6.25537273886839,
6.26069619722776,6.26911253365382,6.29910436423473,6.30382632800519,6.30618796733963,
6.30802320036033,6.31004176844181,6.31332062783319,6.3245485906103,6.39171605715386,
6.47045998545857,6.6485050995784,6.71307142051247,6.71933933256134,6.72237710036844,
6.72453900608407,6.72676399898738,6.72964425496292,6.7328019897907,6.73797991129445,
6.74830442920889,6.85302303013423,6.97746713791533,7.12353440073216,7.13308325901777,
7.13597938253975,7.13753729060472,7.13891874512614,7.14070981831484,7.1438741669414,
7.15791391799086,7.36512096624578,7.48566039335019,7.49679831909093,7.5019343165621,
7.50579404884994,7.50986757345893,7.51604961002203,7.53341279020593,7.71048193025695,
7.82771867433625,7.8742635524245,7.88163892036583,7.88417885528428,7.88591447386092,
7.88750001477075,7.88962301904988,7.89358556669983,7.91531693470139,7.95696201534709,
7.99687150909349,8.02403016709019,8.04779918487014,8.17876796890253,8.26919365609497,
8.27617767497506,8.27890618167616,8.28087904052705,8.28293749679372,8.2856483366552,
8.28863594887332,8.29359339851161,8.30360728892195,8.32931143734312,8.42580297939014,
8.65738212694162,8.66455037223573,8.66687914679954,8.69954650177493,8.70269062899539,
8.70420579870868,8.7052803061511,8.7062928117296,8.70769776547701,8.7105468061881,
8.73489968386801,8.81210712490254,8.87419522441539,8.96201943344826,9.01642874047259,
9.09713008757062,9.10374547253827,9.1065790505427,9.10859790483142,9.11046947939199,
9.11329741265741,9.12000181378065,9.23548856557561,9.48720757802478,9.49930824374196,
9.50164941912221,9.50314039560235,9.50431750755878,9.50563092405126,9.50780632775749,
9.51565405453653,9.56766377902952,9.609289670219,9.88657725912831,9.89905812311192,
9.91660666896944,9.9206670629974,9.9233367074833,9.92537035669844,9.92740178011608,
9.92978761312891,9.93321467079975,9.942862547507,9.95915312357805),
 .UNSPECIFIED.);
#3530=B_SPLINE_CURVE_WITH_KNOTS('',3,(#218122,#218123,#218124,#218125,#218126,
#218127,#218128,#218129,#218130,#218131,#218132,#218133,#218134,#218135,
#218136,#218137,#218138,#218139,#218140,#218141,#218142,#218143,#218144,
#218145,#218146,#218147,#218148,#218149,#218150,#218151,#218152,#218153,
#218154,#218155,#218156,#218157,#218158,#218159,#218160,#218161,#218162,
#218163,#218164,#218165,#218166,#218167,#218168,#218169,#218170,#218171,
#218172,#218173,#218174,#218175,#218176,#218177,#218178,#218179,#218180,
#218181,#218182,#218183,#218184,#218185,#218186,#218187,#218188,#218189,
#218190,#218191,#218192,#218193,#218194,#218195,#218196,#218197,#218198,
#218199,#218200,#218201,#218202,#218203,#218204,#218205,#218206,#218207,
#218208,#218209,#218210,#218211,#218212,#218213,#218214,#218215,#218216,
#218217,#218218,#218219,#218220,#218221,#218222,#218223,#218224,#218225,
#218226,#218227,#218228,#218229,#218230,#218231,#218232,#218233,#218234,
#218235,#218236,#218237,#218238,#218239,#218240,#218241,#218242,#218243,
#218244,#218245,#218246,#218247,#218248,#218249,#218250,#218251,#218252,
#218253,#218254,#218255,#218256,#218257,#218258,#218259,#218260,#218261,
#218262,#218263,#218264,#218265,#218266,#218267,#218268,#218269,#218270,
#218271,#218272,#218273,#218274,#218275,#218276,#218277,#218278,#218279,
#218280,#218281,#218282,#218283,#218284,#218285,#218286,#218287,#218288,
#218289,#218290,#218291,#218292,#218293,#218294,#218295,#218296,#218297,
#218298,#218299,#218300,#218301,#218302,#218303,#218304,#218305,#218306,
#218307,#218308,#218309,#218310,#218311,#218312,#218313,#218314,#218315,
#218316,#218317,#218318,#218319,#218320,#218321,#218322,#218323,#218324,
#218325,#218326,#218327,#218328,#218329,#218330,#218331,#218332,#218333,
#218334,#218335,#218336,#218337,#218338,#218339,#218340,#218341,#218342,
#218343,#218344,#218345,#218346,#218347,#218348,#218349,#218350,#218351,
#218352,#218353,#218354,#218355,#218356,#218357,#218358,#218359,#218360,
#218361,#218362,#218363,#218364,#218365,#218366,#218367,#218368,#218369,
#218370,#218371,#218372,#218373,#218374,#218375,#218376,#218377,#218378,
#218379,#218380,#218381,#218382,#218383,#218384,#218385,#218386,#218387,
#218388,#218389,#218390,#218391,#218392,#218393,#218394,#218395,#218396,
#218397,#218398,#218399,#218400,#218401,#218402,#218403,#218404,#218405,
#218406,#218407,#218408,#218409,#218410,#218411,#218412,#218413,#218414,
#218415,#218416,#218417,#218418,#218419,#218420,#218421,#218422,#218423,
#218424,#218425,#218426,#218427,#218428,#218429,#218430,#218431,#218432,
#218433,#218434,#218435,#218436,#218437,#218438,#218439,#218440,#218441,
#218442,#218443,#218444,#218445,#218446,#218447,#218448,#218449,#218450,
#218451,#218452,#218453,#218454,#218455,#218456,#218457,#218458,#218459,
#218460,#218461,#218462,#218463,#218464,#218465,#218466,#218467,#218468,
#218469,#218470,#218471,#218472,#218473,#218474,#218475,#218476,#218477,
#218478,#218479,#218480,#218481,#218482,#218483,#218484,#218485,#218486,
#218487,#218488,#218489,#218490,#218491,#218492,#218493,#218494,#218495,
#218496,#218497,#218498,#218499,#218500,#218501,#218502,#218503,#218504,
#218505,#218506,#218507,#218508,#218509,#218510,#218511,#218512,#218513,
#218514,#218515,#218516,#218517,#218518,#218519,#218520,#218521,#218522,
#218523,#218524,#218525,#218526,#218527,#218528,#218529,#218530,#218531,
#218532,#218533,#218534,#218535,#218536,#218537,#218538,#218539,#218540,
#218541,#218542,#218543,#218544,#218545,#218546,#218547,#218548,#218549,
#218550,#218551,#218552,#218553,#218554,#218555,#218556,#218557,#218558,
#218559,#218560,#218561,#218562,#218563,#218564,#218565,#218566,#218567,
#218568,#218569,#218570,#218571,#218572,#218573,#218574,#218575,#218576,
#218577,#218578,#218579,#218580,#218581,#218582,#218583,#218584,#218585,
#218586,#218587,#218588,#218589,#218590,#218591,#218592,#218593,#218594,
#218595,#218596,#218597,#218598,#218599,#218600,#218601,#218602,#218603,
#218604,#218605,#218606,#218607,#218608,#218609,#218610,#218611,#218612,
#218613,#218614,#218615,#218616,#218617,#218618,#218619,#218620,#218621,
#218622,#218623,#218624,#218625,#218626,#218627,#218628,#218629,#218630,
#218631,#218632,#218633,#218634,#218635,#218636,#218637,#218638,#218639,
#218640,#218641,#218642,#218643,#218644,#218645,#218646,#218647,#218648,
#218649,#218650,#218651,#218652,#218653,#218654,#218655,#218656,#218657,
#218658,#218659,#218660,#218661),.UNSPECIFIED.,.F.,.F.,(4,2,2,2,2,2,2,2,
2,2,2,2,2,2,2,2,2,2,2,2,2,2,2,2,2,2,2,2,2,2,2,2,2,2,2,2,2,2,2,2,2,2,2,2,
2,2,2,2,2,2,2,2,2,2,2,2,2,2,2,2,2,2,2,2,2,2,2,2,2,2,2,2,2,2,2,2,2,2,2,2,
2,2,2,2,2,2,2,2,2,2,2,2,2,2,2,2,2,2,2,2,2,2,2,2,2,2,2,2,2,2,2,2,2,2,2,2,
2,2,2,2,2,2,2,2,2,2,2,2,2,2,2,2,2,2,2,2,2,2,2,2,2,2,2,2,2,2,2,2,2,2,2,2,
2,2,2,2,2,2,2,2,2,2,2,2,2,2,2,2,2,2,2,2,2,2,2,2,2,2,2,2,2,2,2,2,2,2,2,2,
2,2,2,2,2,2,2,2,2,2,2,2,2,2,2,2,2,2,2,2,2,2,2,2,2,2,2,2,2,2,2,2,2,2,2,2,
2,2,2,2,2,2,2,2,2,2,2,2,2,2,2,2,2,2,2,2,2,2,2,2,2,2,2,2,2,2,2,2,2,2,2,2,
2,2,2,2,2,2,2,2,2,4),(0.00342832916621827,0.283631051066085,0.360738473639449,
0.366797125569613,0.369537630895681,0.371589629870451,0.373510316724189,
0.376157013520932,0.381465250250319,0.432135927861035,0.473970987694638,
0.490486145040209,0.584839881414579,0.691087837363955,0.801282838340406,
0.815459201201547,0.822813041199435,0.828809321060278,0.835736835233664,
0.84735815397142,0.892187224478493,1.04746644909393,1.09924798175357,1.12420104845123,
1.12976531983696,1.13313236569669,1.1361899876218,1.14012329694035,1.14645018770221,
1.1816016496431,1.31811911670678,1.4118220678103,1.43413700425487,1.4439979941693,
1.4513614006176,1.45827482030023,1.46789692429219,1.49358380062198,1.65834149976674,
1.77082316864897,1.87340462439512,1.88203448487255,1.88825472558852,1.89086137921176,
1.89273639802437,1.89443731040081,1.89669984513036,1.90216842222589,1.97189398654687,
2.17230806268736,2.28620335969344,2.29696219672158,2.30229945725151,2.30552354574051,
2.30844927291627,2.31068166452595,2.31282721003923,2.31580423992278,2.32347794845796,
2.42800880184614,2.51245035823726,2.64226377992633,2.70849358663467,2.71831979341818,
2.72112254116228,2.72283294847891,2.72437793238283,2.7263517871531,2.73025071001662,
2.7534621401755,2.89089511894278,2.99469886179372,3.04677265934644,3.0769198821813,
3.08436300465291,3.08871596073143,3.09214832312508,3.09658795674793,3.10446383611405,
3.13394951671107,3.2380065296938,3.39171787465741,3.44146890328936,3.4641601490627,
3.4681679228941,3.47030058874123,3.4718864342716,3.47386674964624,3.47718018814749,
3.4881085630761,3.64600810064209,3.69452879427424,3.79563316629203,3.84355904471498,
3.85905433570377,3.86304739246538,3.86540110551595,3.86747546329156,3.87005689151794,
3.8740255176707,3.89179165012771,4.17260635888201,4.23218988615659,4.27991414095278,
4.28723786676528,4.28929305289678,4.29053916104202,4.29165932937067,4.29308462615784,
4.29537028085317,4.30735870013929,4.50781327429289,4.67175734946823,4.68740606904522,
4.69130256378998,4.69357417159628,4.69556088189839,4.69801344246082,4.70174769521128,
4.7179349414876,4.98462416316624,4.98640371520551,4.98797115128335,4.98927285779437,
4.99025736250648,4.99091502581435,4.99130249642403,4.99150992298686,4.99161467056005,
4.99166594882272,5.00290355910937,5.08189136805791,5.08666560298956,5.08832601182001,
5.08947459829621,5.09053399564449,5.09196758474482,5.09469026088453,5.11072116907735,
5.14183346642671,5.19886310977924,5.36794208954646,5.40082839601826,5.42890278799879,
5.49828699802399,5.50506274644153,5.50782447757898,5.50986291418035,5.5120730653388,
5.51507970493303,5.52195515677048,5.61413902983783,5.84797672258699,5.90221721621993,
5.90802918384602,5.91069515282231,5.91274371284757,5.91493965746252,5.91838501415116,
5.92916171878568,5.9966346150914,6.13243771161565,6.33082436739837,6.35273173101311,
6.36083386186514,6.3665956032699,6.37266410510324,6.38065277495144,6.39803990893885,
6.41081100567521,6.43331815879127,6.51728848904986,6.65578103514687,6.66806336491171,
6.67216064998922,6.67507810398222,6.67784133499532,6.6816988442517,6.68946370183121,
6.76387410146639,6.91303364304987,6.92260088605829,6.96836281161855,6.98178444596241,
6.98987768752092,6.996443709225,7.00544207032008,7.0232210543294,7.124062306916,
7.26183738034302,7.37628984888066,7.41969381060556,7.42938938532284,7.43249542089468,
7.43427866588673,7.43605644464604,7.43831188856129,7.4426932598588,7.44820461570782,
7.48862257626653,7.54733320482364,7.73424366049973,7.77865576003307,7.84073978613646,
7.84763438440298,7.85040589420224,7.85270962487712,7.85506494955559,7.85849038164818,
7.86745379035613,7.98415770133822,8.03869460398933,8.21843992788006,8.25844297081749,
8.26237820602357,8.26436871234709,8.26582412541662,8.26730005760225,8.26931006642183,
8.27355776354944,8.27917321500773,8.29251559902873,8.33646720731166,8.43294670762758,
8.47179719311355,8.61321292700364,8.62475967353734,8.62942923604514,8.63333113315084,
8.63734518131892,8.64323975335657,8.65873142482336,8.72792152962356,8.76295041431008,
8.78815340392706,8.95887154948812,9.00540038507769,9.01014231011597,9.01247728302127,
9.01415734390665,9.01584514546417,9.01810087529382,9.02271114402907,9.02863198887763,
9.04189400673035,9.07602654671143,9.12113227238289,9.33054316393754,9.39829674171379,
9.40480874191826,9.40745729289208,9.40941006394441,9.41152525907372,9.41439910568962,
9.4209547454346,9.53727160818928,9.62474678035204,9.66328134892579,9.68298682188908,
9.70441564373435,9.80395315570567,9.82822705663885,9.83139999642303,9.83288808372516,
9.83402107797487,9.83522519082486,9.83644837802485,9.8382170637605,9.84130640182385,
9.96378201833553),.UNSPECIFIED.);
#3531=B_SPLINE_CURVE_WITH_KNOTS('',3,(#218663,#218664,#218665,#218666,#218667,
#218668,#218669,#218670,#218671,#218672,#218673,#218674,#218675,#218676,
#218677,#218678,#218679,#218680,#218681,#218682,#218683,#218684,#218685,
#218686,#218687,#218688,#218689,#218690,#218691,#218692,#218693,#218694,
#218695,#218696,#218697,#218698,#218699,#218700,#218701,#218702,#218703,
#218704,#218705,#218706,#218707,#218708,#218709,#218710,#218711,#218712,
#218713,#218714,#218715,#218716,#218717,#218718,#218719,#218720,#218721,
#218722,#218723,#218724,#218725,#218726,#218727,#218728,#218729,#218730,
#218731,#218732,#218733,#218734,#218735,#218736,#218737,#218738,#218739,
#218740,#218741,#218742,#218743,#218744,#218745,#218746,#218747,#218748,
#218749,#218750,#218751,#218752,#218753,#218754,#218755,#218756,#218757,
#218758,#218759,#218760,#218761,#218762,#218763,#218764,#218765,#218766,
#218767,#218768,#218769,#218770,#218771,#218772,#218773,#218774,#218775,
#218776,#218777,#218778,#218779,#218780,#218781,#218782,#218783,#218784,
#218785,#218786,#218787,#218788,#218789,#218790,#218791,#218792,#218793,
#218794,#218795,#218796,#218797,#218798,#218799,#218800,#218801,#218802,
#218803,#218804,#218805,#218806,#218807,#218808,#218809,#218810,#218811,
#218812,#218813,#218814,#218815,#218816,#218817,#218818,#218819,#218820,
#218821,#218822,#218823,#218824,#218825,#218826,#218827,#218828,#218829,
#218830,#218831,#218832,#218833,#218834,#218835,#218836,#218837,#218838,
#218839,#218840,#218841,#218842,#218843,#218844,#218845,#218846,#218847,
#218848,#218849,#218850,#218851,#218852,#218853,#218854,#218855,#218856,
#218857,#218858,#218859,#218860,#218861,#218862,#218863,#218864,#218865,
#218866,#218867,#218868,#218869,#218870,#218871,#218872,#218873,#218874,
#218875,#218876,#218877,#218878,#218879,#218880,#218881,#218882,#218883,
#218884,#218885,#218886,#218887,#218888,#218889,#218890,#218891,#218892,
#218893,#218894,#218895,#218896,#218897,#218898,#218899,#218900,#218901,
#218902,#218903,#218904,#218905,#218906,#218907,#218908,#218909,#218910,
#218911,#218912,#218913,#218914,#218915,#218916,#218917,#218918,#218919,
#218920,#218921,#218922,#218923,#218924,#218925,#218926,#218927,#218928,
#218929,#218930,#218931,#218932,#218933,#218934,#218935,#218936,#218937,
#218938,#218939,#218940,#218941,#218942,#218943,#218944,#218945,#218946,
#218947,#218948,#218949,#218950,#218951,#218952,#218953,#218954,#218955,
#218956,#218957,#218958,#218959,#218960,#218961,#218962,#218963,#218964,
#218965,#218966,#218967,#218968,#218969,#218970,#218971,#218972,#218973,
#218974,#218975,#218976,#218977,#218978,#218979,#218980,#218981,#218982,
#218983,#218984,#218985,#218986,#218987,#218988,#218989,#218990,#218991,
#218992,#218993,#218994,#218995,#218996,#218997,#218998,#218999,#219000,
#219001,#219002,#219003,#219004,#219005,#219006,#219007,#219008,#219009,
#219010,#219011,#219012,#219013,#219014,#219015,#219016,#219017,#219018,
#219019,#219020,#219021,#219022,#219023,#219024,#219025,#219026,#219027,
#219028,#219029,#219030,#219031,#219032,#219033,#219034,#219035,#219036,
#219037,#219038,#219039,#219040,#219041,#219042,#219043,#219044,#219045,
#219046,#219047,#219048,#219049,#219050,#219051,#219052,#219053,#219054,
#219055,#219056,#219057,#219058,#219059,#219060,#219061,#219062,#219063,
#219064,#219065,#219066,#219067,#219068,#219069,#219070,#219071,#219072,
#219073,#219074,#219075,#219076,#219077,#219078,#219079,#219080,#219081,
#219082,#219083,#219084,#219085,#219086,#219087,#219088,#219089,#219090,
#219091,#219092,#219093,#219094,#219095,#219096,#219097,#219098,#219099,
#219100,#219101,#219102,#219103,#219104,#219105,#219106,#219107,#219108,
#219109,#219110,#219111,#219112,#219113,#219114,#219115,#219116,#219117,
#219118,#219119,#219120,#219121,#219122,#219123,#219124,#219125,#219126,
#219127,#219128,#219129,#219130,#219131,#219132,#219133,#219134,#219135,
#219136,#219137,#219138,#219139,#219140,#219141,#219142,#219143,#219144,
#219145,#219146,#219147,#219148,#219149,#219150,#219151,#219152,#219153,
#219154,#219155,#219156,#219157,#219158,#219159,#219160,#219161,#219162,
#219163,#219164,#219165,#219166,#219167,#219168,#219169,#219170,#219171,
#219172,#219173,#219174,#219175,#219176,#219177,#219178,#219179,#219180,
#219181,#219182,#219183,#219184,#219185,#219186,#219187,#219188,#219189,
#219190,#219191,#219192),.UNSPECIFIED.,.F.,.F.,(4,2,2,2,2,2,2,2,2,2,2,2,
2,2,2,2,2,2,2,2,2,2,2,2,2,2,2,2,2,2,2,2,2,2,2,2,2,2,2,2,2,2,2,2,2,2,2,2,
2,2,2,2,2,2,2,2,2,2,2,2,2,2,2,2,2,2,2,2,2,2,2,2,2,2,2,2,2,2,2,2,2,2,2,2,
2,2,2,2,2,2,2,2,2,2,2,2,2,2,2,2,2,2,2,2,2,2,2,2,2,2,2,2,2,2,2,2,2,2,2,2,
2,2,2,2,2,2,2,2,2,2,2,2,2,2,2,2,2,2,2,2,2,2,2,2,2,2,2,2,2,2,2,2,2,2,2,2,
2,2,2,2,2,2,2,2,2,2,2,2,2,2,2,2,2,2,2,2,2,2,2,2,2,2,2,2,2,2,2,2,2,2,2,2,
2,2,2,2,2,2,2,2,2,2,2,2,2,2,2,2,2,2,2,2,2,2,2,2,2,2,2,2,2,2,2,2,2,2,2,2,
2,2,2,2,2,2,2,2,2,2,2,2,2,2,2,2,2,2,2,2,2,2,2,2,2,2,2,2,2,2,2,2,2,2,2,2,
4),(0.00135678833193775,0.0849112974682599,0.250362026703773,0.267416405184458,
0.271424401168757,0.273720086164047,0.275503948011275,0.277837536064323,
0.281905370935197,0.297768962655745,0.548144917578907,0.590757060622519,
0.658429813576954,0.665967591826151,0.66752938957349,0.668705623442331,
0.669901750382023,0.671006917428027,0.67250706999984,0.675442522770863,
0.698087591735058,0.775060481717971,0.819621842294523,0.856102387606388,
0.930047452729326,1.07845551366674,1.08501040120155,1.08795794536467,1.09015716006998,
1.09220892133065,1.09502499788795,1.10211996924262,1.18681820743318,1.35770560184273,
1.42578010787449,1.45604870462433,1.47364666932529,1.481262367681,1.48531240554683,
1.48878495046406,1.4909669948675,1.49300388787056,1.49564254820917,1.50116619853498,
1.54010957802893,1.73066308911003,1.86619755748685,1.92232050471461,1.93615723713239,
1.94344110930975,1.9488519562787,1.95562686122702,1.96707702717865,2.00755677830743,
2.12701218859459,2.2390115302356,2.24811954978529,2.25211398087694,2.25501391663153,
2.25818456154083,2.26303368368701,2.27634795535934,2.38380555866663,2.50302811984098,
2.53258948623283,2.55468037168967,2.56450204876064,2.57185935669029,2.57878402114594,
2.58844931832276,2.61452482236272,2.80178771241284,2.89190820002709,3.00075531870213,
3.00583445434993,3.00985558001541,3.01203502086102,3.01385721669238,3.01596298371126,
3.01953765921016,3.0324932441244,3.29615033944627,3.41815386923108,3.42570700543658,
3.42890210481325,3.4312106978574,3.43331237939667,3.43611876500823,3.44295023998168,
3.50608673802949,3.73789791419254,3.78531174673087,3.81929929419335,3.83825218452709,
3.84167395243639,3.84352105606655,3.84490650921318,3.84642901445017,3.84914653949791,
3.8573006734907,3.86514335002146,3.87223044585572,3.95851715611277,4.05917177086544,
4.19075736560386,4.20265954231791,4.20791191821989,4.2118008342834,4.21541290355264,
4.22035282655244,4.23261840055454,4.39093366564085,4.51525006242259,4.56320312513134,
4.58530239462114,4.5892810631282,4.59140749903535,4.59314690995691,4.59518631559077,
4.59867162217512,4.61152270672273,4.85716944564892,4.91272030567231,4.97082441324231,
4.98142451881819,4.98490309334031,4.98691779298153,4.98879252427598,4.99135479671747,
4.99630940899933,5.02823687628295,5.09990645506393,5.31358328234852,5.35016422589624,
5.36360158692659,5.37206007109417,5.40565409288447,5.40912680533124,5.41053384363057,
5.41158004344229,5.41272172306244,5.41429355756304,5.4180601653288,5.49590390544152,
5.67890047502349,5.74268343905978,5.80407864277238,5.81024455641712,5.81276924339384,
5.81463686185594,5.81666576885071,5.81943288069444,5.82579053885241,5.93389233704926,
6.11491083760101,6.20126556599649,6.20651059715833,6.2084256932473,6.2095552797128,
6.2106196138646,6.21209493525669,6.21501928685218,6.23635714518638,6.31773781865796,
6.45834865378636,6.61360636289424,6.6236797545484,6.6273079130548,6.62941124156517,
6.63136978096582,6.63404872322197,6.63923623375321,6.67294704222562,6.7502242588908,
6.9476979251212,7.02137505619447,7.02682530116526,7.02951134725714,7.03144230396704,
7.0332830136525,7.03586981784371,7.04067747924981,7.04703829465804,7.10063066007351,
7.20815699909149,7.34182013975535,7.35142628432431,7.3747712178758,7.38048596022667,
7.46305795471251,7.47524427712935,7.48289869735073,7.48892093247349,7.49453120091331,
7.50442000585867,7.53384700936255,7.57982322846128,7.68079260201834,7.71168068145007,
7.78163222917901,7.78909067834207,7.79281531994721,7.79578107269749,7.79910884046136,
7.80269930766009,7.80810667311621,7.81803337042311,7.8413464288574,7.94950972258716,
8.08127755737829,8.09624288142532,8.10556879378987,8.11285833400293,8.11969721084495,
8.13168331848794,8.17057963374346,8.23775088025926,8.36692615312483,8.49716252185221,
8.50371452653134,8.50750235320915,8.54433828515561,8.54889750221964,8.55122753263064,
8.55294558950003,8.55480699207006,8.55663437350001,8.56101574365353,8.59065994101801,
8.61522211780292,8.71309035524783,8.94841616827017,8.96320862286803,8.9675392510887,
8.97009273776712,8.97211862896137,8.9748178210844,8.97981096434038,9.00617830229802,
9.05766916499873,9.16378168996786,9.2067956661907,9.25444323354422,9.37134331817222,
9.37916210360649,9.38183564811077,9.38334845915371,9.38473458039316,9.38659682619818,
9.38857936531182,9.39170553119581,9.42561522673847,9.49852059576848,9.53022821423388,
9.56274593904948,9.73050279021206,9.74106333724318,9.74619334311474,9.74985475586656,
9.75371383150755,9.75749518935319,9.76243558929581,9.77025600448147,9.77104986109147,
9.96040829415487),.UNSPECIFIED.);
#3532=B_SPLINE_CURVE_WITH_KNOTS('',3,(#219194,#219195,#219196,#219197,#219198,
#219199,#219200,#219201,#219202,#219203,#219204,#219205,#219206,#219207,
#219208,#219209,#219210,#219211,#219212,#219213,#219214,#219215,#219216,
#219217,#219218,#219219,#219220,#219221,#219222,#219223,#219224,#219225,
#219226,#219227,#219228,#219229,#219230,#219231,#219232,#219233,#219234,
#219235,#219236,#219237,#219238,#219239,#219240,#219241,#219242,#219243,
#219244,#219245,#219246,#219247,#219248,#219249,#219250,#219251,#219252,
#219253,#219254,#219255,#219256,#219257,#219258,#219259,#219260,#219261,
#219262,#219263,#219264,#219265,#219266,#219267,#219268,#219269,#219270,
#219271,#219272,#219273,#219274,#219275,#219276,#219277,#219278,#219279,
#219280,#219281,#219282,#219283,#219284,#219285,#219286,#219287,#219288,
#219289,#219290,#219291,#219292,#219293,#219294,#219295,#219296,#219297,
#219298,#219299,#219300,#219301,#219302,#219303,#219304,#219305,#219306,
#219307,#219308,#219309,#219310,#219311,#219312,#219313,#219314,#219315,
#219316,#219317,#219318,#219319,#219320,#219321,#219322,#219323,#219324,
#219325,#219326,#219327,#219328,#219329,#219330,#219331,#219332,#219333,
#219334,#219335,#219336,#219337,#219338,#219339,#219340,#219341,#219342,
#219343,#219344,#219345,#219346,#219347,#219348,#219349,#219350,#219351,
#219352,#219353,#219354,#219355,#219356,#219357,#219358,#219359,#219360,
#219361,#219362,#219363,#219364,#219365,#219366,#219367,#219368,#219369,
#219370,#219371,#219372,#219373,#219374,#219375,#219376,#219377,#219378,
#219379,#219380,#219381,#219382,#219383,#219384,#219385,#219386,#219387,
#219388,#219389,#219390,#219391,#219392,#219393,#219394,#219395,#219396,
#219397,#219398,#219399,#219400,#219401,#219402,#219403,#219404,#219405,
#219406,#219407,#219408,#219409,#219410,#219411,#219412,#219413,#219414,
#219415,#219416,#219417,#219418,#219419,#219420,#219421,#219422,#219423,
#219424,#219425,#219426,#219427,#219428,#219429,#219430,#219431,#219432,
#219433,#219434,#219435,#219436,#219437,#219438,#219439,#219440,#219441,
#219442,#219443,#219444,#219445,#219446,#219447,#219448,#219449,#219450,
#219451,#219452),.UNSPECIFIED.,.F.,.F.,(4,3,3,3,3,3,3,3,3,3,3,3,3,3,3,3,
3,3,3,3,3,3,3,3,3,3,3,3,3,3,3,3,3,3,3,3,3,3,3,3,3,3,3,3,3,3,3,3,3,3,3,3,
3,3,3,3,3,3,3,3,3,3,3,3,3,3,3,3,3,3,3,3,3,3,3,3,3,3,3,3,3,3,3,3,3,3,4),
(57.6723164707605,57.7662350129566,57.8613028416319,57.9269046800067,58.0014341497759,
58.0758874780915,58.1502785677462,58.2246212803993,58.2989294454143,58.3732168683317,
58.447512414101,58.5218169201686,58.5961428835196,58.6705028101348,58.7449484930452,
58.8194433462206,58.8940402919011,58.9256444158688,58.9987833595532,59.0718342768603,
59.1448121008823,59.2177316953978,59.290607870374,59.3634553959561,59.4363028931159,
59.5091540416538,59.5820221907546,59.6549207008071,59.72790614237,59.8009389551458,
59.8740833792634,59.924384151731,59.9999124403979,60.0753546357312,60.1507236434258,
60.2260323213889,60.3012934877895,60.3790222877649,60.4542324850901,60.5294367097886,
60.6046465200537,60.6798734750397,60.7551563646492,60.8304724115199,60.9058593207772,
60.9231238875932,60.9997157879941,61.0762424899349,61.1527136858269,61.2291305460875,
61.3055145849215,61.3818747483341,61.4224937555243,61.5006130240034,61.5787773274772,
61.6569914044661,61.7352965271544,61.8136499537537,61.8920890435195,61.9218636234553,
62.003842402042,62.0857491512826,62.1696202363085,62.251285648823,62.3362595701047,
62.4212334913864,62.4948451654926,62.5684515323452,62.6420655842472,62.7157318767762,
62.7894254047999,62.8632008778658,62.9206033593175,62.9971040841234,63.0735488513046,
63.1499485708849,63.2263141204909,63.302656352682,63.3797421954942,63.4560840088709,
63.5324360965132,63.6088083206211,63.6864420142607,63.7629136912539,63.8411283932168,
63.9193430951797,63.9555017779401),.UNSPECIFIED.);
#3533=B_SPLINE_CURVE_WITH_KNOTS('',3,(#219454,#219455,#219456,#219457,#219458,
#219459,#219460,#219461,#219462,#219463,#219464,#219465,#219466),
 .UNSPECIFIED.,.F.,.F.,(4,1,1,1,1,1,1,1,1,1,4),(63.955503203756,64.4187129631108,
64.9180828310419,65.9168225669041,66.9155623027663,67.9143020386285,68.4136719065595,
68.9130417744906,69.4124116424217,69.9117815103529,70.2386870851197),
 .UNSPECIFIED.);
#3534=B_SPLINE_CURVE_WITH_KNOTS('',3,(#219468,#219469,#219470,#219471,#219472,
#219473,#219474,#219475,#219476,#219477,#219478,#219479,#219480,#219481,
#219482,#219483,#219484,#219485),.UNSPECIFIED.,.F.,.F.,(4,2,2,2,2,2,2,2,
4),(70.2386870851197,71.0736039970146,71.9085209089094,72.7434378208043,
73.5783547326992,74.413271644594,75.2481885564889,76.0831054683838,76.5218723922993),
 .UNSPECIFIED.);
#3535=B_SPLINE_CURVE_WITH_KNOTS('',3,(#219487,#219488,#219489,#219490,#219491,
#219492,#219493,#219494,#219495,#219496,#219497,#219498,#219499,#219500,
#219501,#219502,#219503,#219504,#219505,#219506,#219507,#219508,#219509,
#219510,#219511,#219512,#219513,#219514,#219515,#219516,#219517,#219518,
#219519,#219520,#219521,#219522,#219523,#219524,#219525,#219526,#219527,
#219528,#219529,#219530,#219531,#219532,#219533,#219534,#219535,#219536,
#219537,#219538,#219539,#219540,#219541,#219542,#219543,#219544,#219545,
#219546,#219547,#219548,#219549,#219550,#219551,#219552,#219553,#219554,
#219555,#219556,#219557,#219558,#219559,#219560,#219561,#219562,#219563,
#219564,#219565,#219566,#219567,#219568,#219569,#219570,#219571,#219572,
#219573,#219574,#219575,#219576,#219577,#219578,#219579,#219580,#219581,
#219582,#219583,#219584,#219585,#219586,#219587,#219588,#219589,#219590,
#219591,#219592,#219593,#219594,#219595,#219596,#219597,#219598,#219599,
#219600,#219601,#219602,#219603,#219604,#219605,#219606,#219607,#219608,
#219609,#219610,#219611,#219612,#219613,#219614,#219615,#219616,#219617,
#219618,#219619,#219620,#219621,#219622,#219623,#219624,#219625,#219626,
#219627,#219628,#219629,#219630,#219631,#219632,#219633,#219634,#219635,
#219636,#219637,#219638,#219639,#219640,#219641,#219642,#219643,#219644,
#219645,#219646,#219647,#219648,#219649,#219650,#219651,#219652,#219653,
#219654,#219655,#219656,#219657,#219658,#219659,#219660,#219661,#219662,
#219663,#219664,#219665,#219666,#219667,#219668,#219669,#219670,#219671,
#219672,#219673,#219674,#219675,#219676,#219677,#219678,#219679,#219680,
#219681,#219682,#219683,#219684,#219685,#219686,#219687,#219688,#219689,
#219690,#219691,#219692,#219693,#219694,#219695,#219696,#219697,#219698,
#219699,#219700,#219701,#219702,#219703,#219704,#219705,#219706,#219707,
#219708,#219709,#219710,#219711,#219712,#219713,#219714,#219715,#219716,
#219717,#219718,#219719,#219720,#219721,#219722,#219723,#219724,#219725,
#219726,#219727,#219728,#219729,#219730,#219731,#219732,#219733,#219734,
#219735,#219736,#219737,#219738,#219739,#219740,#219741,#219742,#219743,
#219744,#219745,#219746,#219747,#219748),.UNSPECIFIED.,.F.,.F.,(4,3,3,3,
3,3,3,3,3,3,3,3,3,3,3,3,3,3,3,3,3,3,3,3,3,3,3,3,3,3,3,3,3,3,3,3,3,3,3,3,
3,3,3,3,3,3,3,3,3,3,3,3,3,3,3,3,3,3,3,3,3,3,3,3,3,3,3,3,3,3,3,3,3,3,3,3,
3,3,3,3,3,3,3,3,3,3,3,4),(76.5218723922993,76.5974953734188,76.6738614454111,
76.749610786608,76.826285223998,76.9029596613881,76.979460386194,77.0559051533751,
77.1323048729554,77.2086704225614,77.2850126547524,77.3620984975647,77.4384403109414,
77.5147923985836,77.5911646226914,77.6687983163311,77.7452699933244,77.8234846952873,
77.9016993972503,77.9763812119391,78.0509830640905,78.1255173476643,78.1999859051987,
78.2744161207925,78.3488210325928,78.4010692651814,78.4813665136047,78.5618089865093,
78.6464665231601,78.7272466695768,78.8081281805109,78.8891449809138,78.9004391331125,
78.9749686028818,79.0494219311975,79.1238130208523,79.1981557335055,79.2724638985205,
79.346751321438,79.4210468672074,79.4953513732751,79.5696773366261,79.6440372632414,
79.7184829461518,79.7929777993273,79.8675747450079,79.8991788689747,79.9723178126591,
80.0453687299662,80.1183465539882,80.1912661485037,80.2641423234798,80.3369898490617,
80.4098373462215,80.4826884947594,80.5555566438602,80.6284551539126,80.7014405954755,
80.7744734082513,80.8476178323689,80.8979186048369,80.9734468935038,81.048889088837,
81.1242580965317,81.1995667744947,81.2748279408952,81.3525567408707,81.4277669381958,
81.5029711628943,81.5781809731595,81.6534079281456,81.728690817755,81.8040068646258,
81.8793937738832,81.896658340699,81.9732502410998,82.0497769430406,82.1262481389325,
82.2026649991931,82.2790490380269,82.3554092014394,82.3960282086301,82.4727948422462,
82.5495919908356,82.62645942842,82.7033661826157,82.7803503634339,82.8050576994789),
 .UNSPECIFIED.);
#3536=B_SPLINE_CURVE_WITH_KNOTS('',3,(#219750,#219751,#219752,#219753,#219754,
#219755,#219756,#219757,#219758,#219759,#219760,#219761,#219762),
 .UNSPECIFIED.,.F.,.F.,(4,1,1,1,1,1,1,1,1,1,4),(82.8050576994789,82.8953980765612,
83.3947679444923,83.8941378124234,84.8928775482856,85.3922474162167,85.8916172841478,
86.8903570200099,87.8890967558721,88.8878364917343,89.0882430066585),
 .UNSPECIFIED.);
#3537=B_SPLINE_CURVE_WITH_KNOTS('',3,(#219764,#219765,#219766,#219767,#219768,
#219769,#219770,#219771,#219772,#219773,#219774,#219775,#219776,#219777,
#219778,#219779,#219780,#219781,#219782,#219783,#219784,#219785,#219786,
#219787,#219788,#219789,#219790,#219791,#219792,#219793,#219794,#219795,
#219796,#219797,#219798,#219799,#219800,#219801,#219802,#219803,#219804,
#219805,#219806,#219807,#219808,#219809,#219810,#219811,#219812,#219813,
#219814,#219815,#219816,#219817,#219818,#219819,#219820,#219821,#219822,
#219823,#219824,#219825,#219826,#219827,#219828,#219829,#219830,#219831,
#219832,#219833,#219834,#219835,#219836,#219837,#219838,#219839,#219840,
#219841,#219842,#219843,#219844,#219845,#219846,#219847,#219848,#219849,
#219850,#219851,#219852,#219853,#219854,#219855,#219856,#219857,#219858,
#219859,#219860,#219861,#219862,#219863,#219864,#219865,#219866,#219867,
#219868,#219869,#219870,#219871,#219872,#219873,#219874,#219875,#219876,
#219877,#219878,#219879,#219880,#219881,#219882,#219883,#219884,#219885,
#219886,#219887,#219888,#219889,#219890,#219891,#219892,#219893,#219894,
#219895,#219896,#219897,#219898,#219899,#219900,#219901,#219902,#219903,
#219904,#219905,#219906,#219907,#219908,#219909,#219910,#219911,#219912,
#219913,#219914,#219915,#219916,#219917,#219918,#219919,#219920,#219921,
#219922,#219923,#219924,#219925,#219926,#219927,#219928,#219929,#219930,
#219931,#219932,#219933,#219934,#219935,#219936,#219937,#219938,#219939,
#219940,#219941,#219942,#219943,#219944,#219945,#219946,#219947,#219948,
#219949,#219950,#219951,#219952,#219953,#219954,#219955,#219956,#219957,
#219958,#219959,#219960,#219961,#219962,#219963,#219964,#219965,#219966,
#219967,#219968,#219969,#219970,#219971,#219972,#219973,#219974,#219975,
#219976,#219977,#219978,#219979,#219980,#219981,#219982,#219983,#219984,
#219985,#219986,#219987,#219988,#219989,#219990,#219991,#219992,#219993,
#219994,#219995,#219996,#219997,#219998,#219999,#220000,#220001,#220002,
#220003,#220004,#220005,#220006,#220007,#220008,#220009,#220010,#220011,
#220012,#220013,#220014,#220015,#220016,#220017,#220018,#220019),
 .UNSPECIFIED.,.F.,.F.,(4,3,3,3,3,3,3,3,3,3,3,3,3,3,3,3,3,3,3,3,3,3,3,3,
3,3,3,3,3,3,3,3,3,3,3,3,3,3,3,3,3,3,3,3,3,3,3,3,3,3,3,3,3,3,3,3,3,3,3,3,
3,3,3,3,3,3,3,3,3,3,3,3,3,3,3,3,3,3,3,3,3,3,3,3,3,4),(89.0882430066585,
89.1629838449102,89.2359045239601,89.3115554418127,89.3872063596654,89.4653256281447,
89.5434899316183,89.6217040086076,89.7000091312961,89.7783625578954,89.8568016476615,
89.8865762275965,89.9685550061832,90.0504617554236,90.1343328404496,90.2159982529641,
90.3009721742459,90.3859460955276,90.4595577696338,90.5331641364866,90.6067781883886,
90.6804444809175,90.7541380089414,90.8279134820071,90.8853159634587,90.9618166882646,
91.0382614554458,91.1146611750261,91.1910267246322,91.2673689568237,91.3444547996359,
91.4207966130128,91.4971487006549,91.5735209247626,91.6511546184022,91.7276262953954,
91.8058409973582,91.8840556993209,91.9587375140096,92.0333393661611,92.1078736497346,
92.1823422072689,92.2567724228627,92.3311773346629,92.3834255672519,92.463722815675,
92.5441652885799,92.6288228252307,92.7096029716479,92.7904844825828,92.8715012829858,
92.8827954351831,92.9573249049524,93.0317782332682,93.106169322923,93.1805120355759,
93.2548202005907,93.3291076235081,93.4034031692775,93.4777076753451,93.552033638696,
93.6263935653112,93.7008392482215,93.7753341013972,93.8499310470776,93.8815351710452,
93.9546741147296,94.0277250320366,94.1007028560584,94.173622450574,94.2464986255501,
94.3193461511323,94.3921936482919,94.4650447968299,94.5379129459309,94.6108114559836,
94.6837968975463,94.7568297103218,94.8299741344395,94.8802749069074,94.9621583016442,
95.0438908023668,95.1257751802347,95.2070912819773,95.2892597979077,95.3714283138381),
 .UNSPECIFIED.);
#3538=B_SPLINE_CURVE_WITH_KNOTS('',3,(#220021,#220022,#220023,#220024,#220025,
#220026,#220027,#220028,#220029,#220030,#220031,#220032,#220033,#220034,
#220035,#220036,#220037,#220038,#220039,#220040,#220041,#220042,#220043,
#220044,#220045,#220046,#220047,#220048,#220049,#220050,#220051,#220052,
#220053,#220054,#220055,#220056,#220057,#220058,#220059,#220060,#220061,
#220062,#220063,#220064,#220065,#220066,#220067,#220068,#220069,#220070,
#220071,#220072,#220073,#220074,#220075,#220076,#220077,#220078,#220079,
#220080,#220081,#220082,#220083,#220084,#220085,#220086,#220087,#220088,
#220089,#220090,#220091,#220092,#220093,#220094,#220095,#220096,#220097,
#220098,#220099,#220100,#220101,#220102,#220103,#220104,#220105,#220106,
#220107,#220108,#220109,#220110,#220111,#220112,#220113,#220114,#220115,
#220116,#220117,#220118,#220119,#220120,#220121,#220122,#220123,#220124,
#220125,#220126,#220127,#220128,#220129,#220130,#220131,#220132,#220133,
#220134,#220135,#220136,#220137,#220138,#220139,#220140,#220141,#220142,
#220143,#220144,#220145,#220146,#220147,#220148,#220149,#220150,#220151,
#220152,#220153,#220154,#220155,#220156,#220157,#220158,#220159,#220160,
#220161,#220162,#220163,#220164,#220165,#220166,#220167,#220168,#220169,
#220170,#220171,#220172,#220173,#220174,#220175,#220176,#220177,#220178,
#220179,#220180,#220181,#220182,#220183,#220184,#220185,#220186,#220187,
#220188,#220189,#220190,#220191,#220192,#220193,#220194,#220195,#220196,
#220197,#220198,#220199,#220200,#220201,#220202,#220203,#220204,#220205,
#220206,#220207,#220208,#220209,#220210,#220211,#220212,#220213,#220214,
#220215,#220216,#220217,#220218,#220219,#220220,#220221,#220222,#220223,
#220224,#220225,#220226,#220227,#220228,#220229,#220230,#220231,#220232,
#220233,#220234,#220235,#220236,#220237,#220238,#220239,#220240,#220241,
#220242,#220243,#220244,#220245,#220246,#220247,#220248,#220249,#220250,
#220251,#220252,#220253,#220254,#220255,#220256,#220257,#220258,#220259,
#220260,#220261,#220262,#220263,#220264,#220265,#220266,#220267,#220268,
#220269,#220270,#220271,#220272,#220273,#220274,#220275,#220276,#220277,
#220278,#220279,#220280,#220281,#220282,#220283,#220284,#220285,#220286,
#220287,#220288,#220289,#220290,#220291,#220292,#220293,#220294,#220295,
#220296,#220297,#220298,#220299,#220300,#220301,#220302,#220303,#220304,
#220305,#220306,#220307,#220308,#220309,#220310,#220311,#220312,#220313,
#220314,#220315,#220316,#220317,#220318,#220319,#220320,#220321,#220322,
#220323,#220324,#220325,#220326,#220327,#220328,#220329,#220330,#220331,
#220332,#220333,#220334,#220335,#220336,#220337,#220338,#220339,#220340,
#220341,#220342,#220343,#220344,#220345,#220346,#220347,#220348,#220349,
#220350,#220351,#220352,#220353,#220354,#220355,#220356,#220357,#220358,
#220359,#220360,#220361,#220362,#220363,#220364,#220365,#220366,#220367,
#220368,#220369,#220370,#220371,#220372,#220373,#220374,#220375,#220376,
#220377,#220378,#220379,#220380,#220381,#220382,#220383,#220384,#220385,
#220386,#220387,#220388,#220389,#220390,#220391,#220392,#220393,#220394,
#220395,#220396,#220397,#220398,#220399,#220400,#220401,#220402,#220403,
#220404,#220405,#220406,#220407,#220408,#220409,#220410,#220411,#220412,
#220413,#220414,#220415,#220416,#220417,#220418,#220419,#220420,#220421,
#220422,#220423,#220424,#220425,#220426,#220427,#220428,#220429,#220430,
#220431,#220432,#220433,#220434,#220435,#220436,#220437,#220438,#220439,
#220440,#220441,#220442,#220443,#220444,#220445,#220446,#220447,#220448,
#220449,#220450,#220451,#220452,#220453,#220454,#220455,#220456,#220457,
#220458,#220459,#220460,#220461,#220462,#220463,#220464,#220465,#220466,
#220467,#220468,#220469,#220470,#220471,#220472,#220473,#220474,#220475,
#220476,#220477,#220478,#220479,#220480,#220481,#220482,#220483,#220484,
#220485,#220486,#220487,#220488,#220489,#220490,#220491,#220492,#220493,
#220494,#220495,#220496,#220497,#220498,#220499,#220500,#220501,#220502,
#220503,#220504,#220505,#220506,#220507,#220508,#220509,#220510,#220511,
#220512,#220513,#220514,#220515,#220516,#220517,#220518,#220519,#220520,
#220521,#220522,#220523,#220524,#220525,#220526,#220527,#220528,#220529,
#220530,#220531,#220532,#220533,#220534,#220535,#220536,#220537,#220538,
#220539,#220540,#220541,#220542,#220543,#220544,#220545,#220546,#220547,
#220548,#220549,#220550,#220551,#220552,#220553,#220554,#220555,#220556,
#220557,#220558),.UNSPECIFIED.,.F.,.F.,(4,2,2,2,2,2,2,2,2,2,2,2,2,2,2,2,
2,2,2,2,2,2,2,2,2,2,2,2,2,2,2,2,2,2,2,2,2,2,2,2,2,2,2,2,2,2,2,2,2,2,2,2,
2,2,2,2,2,2,2,2,2,2,2,2,2,2,2,2,2,2,2,2,2,2,2,2,2,2,2,2,2,2,2,2,2,2,2,2,
2,2,2,2,2,2,2,2,2,2,2,2,2,2,2,2,2,2,2,2,2,2,2,2,2,2,2,2,2,2,2,2,2,2,2,2,
2,2,2,2,2,2,2,2,2,2,2,2,2,2,2,2,2,2,2,2,2,2,2,2,2,2,2,2,2,2,2,2,2,2,2,2,
2,2,2,2,2,2,2,2,2,2,2,2,2,2,2,2,2,2,2,2,2,2,2,2,2,2,2,2,2,2,2,2,2,2,2,2,
2,2,2,2,2,2,2,2,2,2,2,2,2,2,2,2,2,2,2,2,2,2,2,2,2,2,2,2,2,2,2,2,2,2,2,2,
2,2,2,2,2,2,2,2,2,2,2,2,2,2,2,2,2,2,2,2,2,2,2,2,2,2,2,2,2,2,2,2,2,2,2,2,
4),(0.00144023023890332,0.0188352441522348,0.0286240747235862,0.0320264665064641,
0.034401950934542,0.0364310360599029,0.0384721181132475,0.0411577116316496,
0.0452708277222326,0.0634610453250711,0.0760085167908262,0.352519182779323,
0.373658015965884,0.423576959264981,0.433506795172639,0.436846024628858,
0.439017742336696,0.441074958351601,0.443798416142434,0.449926042113504,
0.510964764186585,0.655162687143893,0.858795601058024,0.880268179166108,
0.888940947904201,0.895122893279219,0.900711915761007,0.908143516087384,
0.913790892828657,0.948548411783089,1.16549407514662,1.19259001574114,1.19828764660113,
1.20168164513884,1.20473368822417,1.20861837620083,1.21478406144893,1.24704524323629,
1.32729344738685,1.43982947292849,1.49458470983966,1.50821191257729,1.51634732222258,
1.52363249898271,1.53291882318514,1.55220293962084,1.57982827843173,1.64256155500931,
1.8211317721868,1.90989618222559,1.95287835821233,1.95765014281574,1.95998924026183,
1.96165093475284,1.96339150443963,1.96580849772034,1.97069945568749,2.03322229580789,
2.26757814736068,2.35742605323967,2.36690386149683,2.3717662308098,2.37479174050958,
2.37757361565507,2.37978623446255,2.38198524778634,2.38515830116659,2.39407408555732,
2.53621071498992,2.69152738339444,2.70956712254707,2.77734345088054,2.78728155706024,
2.79009575634249,2.79180883892596,2.79335344003183,2.79532295066489,2.79920105508675,
2.82200422641208,2.83021153916663,2.83806875528213,2.84860838412361,2.85163575133896,
2.88918425693327,2.9818226688322,3.13783646361113,3.15037392426803,3.15573872948844,
3.15964768256213,3.16323419892985,3.16807853487824,3.17979513073606,3.28524022044815,
3.40284750589108,3.52028170954202,3.53422586185235,3.53768064061847,3.53969265320981,
3.54145127212847,3.54362109605788,3.54691995754242,3.5611722394563,3.80260460346203,
3.91301657289305,3.92846852468512,3.93245753268311,3.93481022159704,3.93688451468692,
3.93946695952734,3.94343919726604,3.96125229793376,4.26476507035458,4.3530851174613,
4.35756796736892,4.35927277032363,4.36044189402177,4.3615827862087,4.36295557908335,
4.36630940139405,4.39757533309571,4.4075722626596,4.45999316779878,4.62981835601763,
4.68654418773814,4.73232327747958,4.7558611664724,4.76028759756685,4.76267562172917,
4.76446576367316,4.76671909321462,4.77053308599018,4.78348822409693,4.98221680467369,
5.14432299168534,5.15459965785234,5.15681531121783,5.15826746538052,5.15944108709222,
5.16077990766441,5.16306828961999,5.1721426027617,5.24031539593307,5.35941274712733,
5.46605877873562,5.46928864799795,5.49685230089605,5.5673330761146,5.57413581157382,
5.57690228970075,5.57894195542656,5.58115124680858,5.58415281721192,5.59099981010166,
5.6961298515114,5.77014561470142,5.83936481622827,5.85790850607198,5.96769864668797,
5.97560875774998,5.97844386007364,5.98041572498261,5.98224295359785,5.98472936221921,
5.98950033826606,6.01952346240784,6.09156508481059,6.25393037786808,6.27481435911482,
6.40537180532509,6.42338818380982,6.4313936839041,6.43748431914233,6.44398016216563,
6.45415631574082,6.4867195625245,6.53874938699504,6.68394184829103,6.73185830236833,
6.73873685294598,6.74241527817458,6.74545121175061,6.74898962280641,6.75524529526294,
6.78378187726126,6.91678785863251,6.99764802407582,7.00417155628134,7.03913997633799,
7.05125760652064,7.05828206084589,7.06486048783464,7.07397123416969,7.09233334477615,
7.20291984640308,7.36292443563327,7.49156309097314,7.49824352238908,7.50095236925486,
7.50282960572948,7.50466862267205,7.50726360245302,7.51341161203112,7.59934647328734,
7.8972450792491,7.91328942986097,7.91770518649558,7.92030410315222,7.92255161646135,
7.92529407213015,7.93048681649165,7.96081504083705,8.01427203493585,8.06724767933589,
8.10991975273886,8.12423205614896,8.13660174287348,8.1475548872055,8.15785302321648,
8.16755211428555,8.17674004568409,8.32040272382137,8.3293531831775,8.33212045499302,
8.33381487393204,8.3353239644011,8.3372332553652,8.3409476579724,8.36570580076754,
8.42761507744329,8.57824115777725,8.68204003919545,8.69203550369335,8.69702611196787,
8.70065145344625,8.70453164618465,8.70972874845631,8.72125556241187,8.90719934899358,
9.0077235406749,9.07290673418962,9.07846548217621,9.08089527502724,9.08267459918955,
9.0843234831423,9.08685937845684,9.09298559287519,9.18523492126532,9.41381663160004,
9.46700189852647,9.47323485054633,9.47576803623214,9.47788458640844,9.48005975562622,
9.4832436704937,9.4916907266521,9.6062770726423,9.83863674155126,9.84567994066315,
9.86899345205559,9.89643833095047,9.89943482306625,9.90091372081988,9.90197866263517,
9.9030504309227,9.90414428284082,9.90556436281459,9.90780983704934,9.90931945351448,
9.96250952171965),.UNSPECIFIED.);
#3539=B_SPLINE_CURVE_WITH_KNOTS('',3,(#220560,#220561,#220562,#220563,#220564,
#220565,#220566,#220567,#220568,#220569,#220570,#220571,#220572),
 .UNSPECIFIED.,.F.,.F.,(4,1,1,1,1,1,1,1,1,1,4),(107.938353794554,108.862631208978,
109.86137094484,110.360740812771,110.860110680702,111.359480548633,111.858850416565,
112.857590152427,113.356960020358,113.856329888289,114.220975245612),
 .UNSPECIFIED.);
#3540=B_SPLINE_CURVE_WITH_KNOTS('',3,(#220574,#220575,#220576,#220577,#220578,
#220579,#220580,#220581,#220582,#220583,#220584,#220585,#220586,#220587,
#220588,#220589,#220590,#220591,#220592,#220593,#220594,#220595,#220596,
#220597,#220598,#220599,#220600,#220601,#220602,#220603,#220604,#220605,
#220606,#220607,#220608,#220609,#220610,#220611,#220612,#220613,#220614,
#220615,#220616,#220617,#220618,#220619,#220620,#220621,#220622,#220623,
#220624,#220625,#220626,#220627,#220628,#220629,#220630,#220631,#220632,
#220633,#220634,#220635,#220636,#220637,#220638,#220639,#220640,#220641,
#220642,#220643,#220644,#220645,#220646,#220647,#220648,#220649,#220650,
#220651,#220652,#220653,#220654,#220655,#220656,#220657,#220658,#220659,
#220660,#220661,#220662,#220663,#220664,#220665,#220666,#220667,#220668,
#220669,#220670,#220671,#220672,#220673,#220674,#220675,#220676,#220677,
#220678,#220679,#220680,#220681,#220682,#220683,#220684,#220685,#220686,
#220687,#220688,#220689,#220690,#220691,#220692,#220693,#220694,#220695,
#220696,#220697,#220698,#220699,#220700,#220701,#220702,#220703,#220704,
#220705,#220706,#220707,#220708,#220709,#220710,#220711,#220712,#220713,
#220714,#220715,#220716,#220717,#220718,#220719,#220720,#220721,#220722,
#220723,#220724,#220725,#220726,#220727,#220728,#220729,#220730,#220731,
#220732,#220733,#220734,#220735,#220736,#220737,#220738,#220739,#220740,
#220741,#220742,#220743,#220744,#220745,#220746,#220747,#220748,#220749,
#220750,#220751,#220752,#220753,#220754,#220755,#220756,#220757,#220758,
#220759,#220760,#220761,#220762,#220763,#220764,#220765,#220766,#220767,
#220768,#220769,#220770,#220771,#220772,#220773,#220774,#220775,#220776,
#220777,#220778,#220779,#220780,#220781,#220782,#220783,#220784,#220785,
#220786,#220787,#220788,#220789,#220790,#220791,#220792,#220793,#220794,
#220795,#220796,#220797,#220798,#220799,#220800,#220801,#220802,#220803,
#220804,#220805,#220806,#220807,#220808,#220809,#220810,#220811,#220812,
#220813,#220814,#220815,#220816,#220817,#220818,#220819,#220820,#220821,
#220822,#220823,#220824,#220825,#220826,#220827,#220828,#220829,#220830,
#220831,#220832,#220833,#220834,#220835),.UNSPECIFIED.,.F.,.F.,(4,3,3,3,
3,3,3,3,3,3,3,3,3,3,3,3,3,3,3,3,3,3,3,3,3,3,3,3,3,3,3,3,3,3,3,3,3,3,3,3,
3,3,3,3,3,3,3,3,3,3,3,3,3,3,3,3,3,3,3,3,3,3,3,3,3,3,3,3,3,3,3,3,3,3,3,3,
3,3,3,3,3,3,3,3,3,3,3,4),(114.220984235377,114.300244908974,114.376091153155,
114.451972074714,114.527898076741,114.603879587423,114.679971804733,114.756128068702,
114.832399526875,114.855069624151,114.928208567835,115.001259485142,115.074237309164,
115.14715690368,115.220033078656,115.292880604238,115.365728101397,115.438579249935,
115.511447399036,115.584345909089,115.657331350652,115.730364163428,115.803508587545,
115.853809360013,115.92933764868,116.004779844013,116.080148851707,116.15545752967,
116.23071869607,116.308447496046,116.383657693371,116.458861918069,116.534071728334,
116.60929868332,116.684581572929,116.7598976198,116.835284529057,116.852549095875,
116.929140996276,117.005667698218,117.08213889411,117.158555754371,117.234939793206,
117.311299956619,117.351918963807,117.430038232286,117.50820253576,117.586416612749,
117.664721735438,117.743075162037,117.821514251804,117.851288831738,117.933267610324,
118.015174359564,118.09904544459,118.180710857104,118.265684778387,118.350658699669,
118.424270373775,118.497876740628,118.571490792531,118.64515708506,118.718850613084,
118.79262608615,118.8500285676,118.926529292406,119.002974059587,119.079373779167,
119.155739328773,119.232081560963,119.309167403776,119.385509217152,119.461861304794,
119.538233528902,119.615867222542,119.692338899535,119.770553601498,119.848768303462,
119.923450118151,119.998051970303,120.072586253877,120.147054811412,120.221485027006,
120.295889938807,120.348138171393,120.421620020599,120.495149820344,120.504169542556),
 .UNSPECIFIED.);
#3541=B_SPLINE_CURVE_WITH_KNOTS('',3,(#220837,#220838,#220839,#220840,#220841,
#220842,#220843,#220844,#220845,#220846,#220847,#220848),.UNSPECIFIED.,
 .F.,.F.,(4,1,1,1,1,1,1,1,1,4),(120.504170804088,120.847508039324,121.846247775186,
122.844987511049,123.843727246911,124.343097114842,124.842466982773,125.341836850704,
125.841206718635,126.787354849736),.UNSPECIFIED.);
#3542=B_SPLINE_CURVE_WITH_KNOTS('',3,(#220850,#220851,#220852,#220853,#220854,
#220855,#220856,#220857,#220858,#220859,#220860,#220861,#220862,#220863,
#220864,#220865,#220866,#220867,#220868,#220869,#220870,#220871,#220872,
#220873,#220874,#220875,#220876,#220877,#220878,#220879,#220880,#220881,
#220882,#220883,#220884,#220885,#220886,#220887,#220888,#220889,#220890,
#220891,#220892,#220893,#220894,#220895,#220896,#220897,#220898,#220899,
#220900,#220901,#220902,#220903,#220904,#220905,#220906,#220907,#220908,
#220909,#220910,#220911,#220912,#220913,#220914,#220915,#220916,#220917,
#220918,#220919,#220920,#220921,#220922,#220923,#220924,#220925,#220926,
#220927,#220928,#220929,#220930,#220931,#220932,#220933,#220934,#220935,
#220936,#220937,#220938,#220939,#220940,#220941,#220942,#220943,#220944,
#220945,#220946,#220947,#220948,#220949,#220950,#220951,#220952,#220953,
#220954,#220955,#220956,#220957,#220958,#220959,#220960,#220961,#220962,
#220963,#220964,#220965,#220966,#220967,#220968,#220969,#220970,#220971,
#220972,#220973,#220974,#220975,#220976,#220977,#220978,#220979,#220980,
#220981,#220982,#220983,#220984,#220985,#220986,#220987,#220988,#220989,
#220990,#220991,#220992,#220993,#220994,#220995,#220996,#220997,#220998,
#220999,#221000,#221001,#221002,#221003,#221004,#221005,#221006,#221007,
#221008,#221009,#221010,#221011,#221012,#221013,#221014,#221015,#221016,
#221017,#221018,#221019,#221020,#221021,#221022,#221023,#221024,#221025,
#221026,#221027,#221028,#221029,#221030,#221031,#221032,#221033,#221034,
#221035,#221036,#221037,#221038,#221039,#221040,#221041,#221042,#221043,
#221044,#221045,#221046,#221047,#221048,#221049,#221050,#221051,#221052,
#221053,#221054,#221055,#221056,#221057,#221058,#221059,#221060,#221061,
#221062,#221063,#221064,#221065,#221066,#221067,#221068,#221069,#221070,
#221071,#221072,#221073,#221074,#221075,#221076,#221077,#221078,#221079,
#221080,#221081,#221082,#221083,#221084,#221085,#221086,#221087,#221088,
#221089,#221090,#221091,#221092,#221093,#221094,#221095,#221096,#221097,
#221098,#221099,#221100,#221101,#221102,#221103,#221104,#221105,#221106,
#221107,#221108,#221109,#221110,#221111,#221112,#221113,#221114,#221115,
#221116,#221117,#221118,#221119,#221120,#221121,#221122,#221123,#221124,
#221125,#221126,#221127,#221128,#221129,#221130,#221131,#221132,#221133,
#221134,#221135,#221136,#221137,#221138,#221139,#221140,#221141,#221142,
#221143,#221144,#221145,#221146,#221147,#221148,#221149,#221150,#221151,
#221152,#221153,#221154,#221155,#221156,#221157,#221158,#221159,#221160,
#221161,#221162,#221163,#221164,#221165,#221166,#221167,#221168,#221169,
#221170,#221171,#221172,#221173,#221174,#221175,#221176,#221177,#221178,
#221179,#221180,#221181,#221182,#221183,#221184,#221185,#221186,#221187,
#221188,#221189,#221190,#221191,#221192,#221193,#221194,#221195,#221196,
#221197,#221198,#221199,#221200,#221201,#221202,#221203,#221204,#221205,
#221206,#221207,#221208,#221209,#221210,#221211,#221212,#221213,#221214,
#221215,#221216,#221217,#221218,#221219,#221220,#221221,#221222,#221223,
#221224,#221225,#221226,#221227,#221228,#221229,#221230,#221231,#221232,
#221233,#221234,#221235,#221236,#221237,#221238,#221239,#221240,#221241,
#221242,#221243,#221244,#221245,#221246,#221247,#221248,#221249,#221250,
#221251,#221252,#221253,#221254,#221255,#221256,#221257,#221258,#221259,
#221260,#221261,#221262,#221263,#221264,#221265,#221266,#221267,#221268,
#221269,#221270,#221271,#221272,#221273,#221274,#221275,#221276,#221277,
#221278,#221279,#221280,#221281,#221282,#221283,#221284,#221285,#221286,
#221287,#221288,#221289,#221290,#221291,#221292,#221293,#221294,#221295,
#221296,#221297,#221298,#221299,#221300,#221301,#221302,#221303,#221304,
#221305,#221306,#221307,#221308,#221309,#221310,#221311,#221312,#221313,
#221314,#221315,#221316,#221317,#221318,#221319,#221320,#221321,#221322,
#221323,#221324,#221325,#221326,#221327,#221328,#221329,#221330,#221331,
#221332,#221333,#221334,#221335,#221336,#221337,#221338,#221339,#221340,
#221341,#221342,#221343,#221344,#221345,#221346,#221347,#221348,#221349,
#221350,#221351,#221352,#221353,#221354,#221355,#221356,#221357,#221358,
#221359,#221360,#221361,#221362,#221363,#221364,#221365,#221366,#221367,
#221368,#221369,#221370,#221371,#221372,#221373,#221374,#221375,#221376,
#221377,#221378,#221379,#221380,#221381,#221382,#221383,#221384,#221385,
#221386,#221387,#221388,#221389),.UNSPECIFIED.,.F.,.F.,(4,2,2,2,2,2,2,2,
2,2,2,2,2,2,2,2,2,2,2,2,2,2,2,2,2,2,2,2,2,2,2,2,2,2,2,2,2,2,2,2,2,2,2,2,
2,2,2,2,2,2,2,2,2,2,2,2,2,2,2,2,2,2,2,2,2,2,2,2,2,2,2,2,2,2,2,2,2,2,2,2,
2,2,2,2,2,2,2,2,2,2,2,2,2,2,2,2,2,2,2,2,2,2,2,2,2,2,2,2,2,2,2,2,2,2,2,2,
2,2,2,2,2,2,2,2,2,2,2,2,2,2,2,2,2,2,2,2,2,2,2,2,2,2,2,2,2,2,2,2,2,2,2,2,
2,2,2,2,2,2,2,2,2,2,2,2,2,2,2,2,2,2,2,2,2,2,2,2,2,2,2,2,2,2,2,2,2,2,2,2,
2,2,2,2,2,2,2,2,2,2,2,2,2,2,2,2,2,2,2,2,2,2,2,2,2,2,2,2,2,2,2,2,2,2,2,2,
2,2,2,2,2,2,2,2,2,2,2,2,2,2,2,2,2,2,2,2,2,2,2,2,2,2,2,2,2,2,2,2,2,2,2,2,
2,2,2,2,2,2,2,2,2,4),(0.00190372001199662,0.0478014467504751,0.0515987046793617,
0.0538690362872017,0.0554968680757349,0.0569311409708447,0.0584885609762871,
0.0605190974258305,0.0649568043178509,0.0998653319031922,0.111694939859996,
0.121789696784997,0.334545570911788,0.391911534125962,0.405631968002068,
0.416256389217015,0.42127042259101,0.425121226471219,0.428801565723861,
0.434003369235636,0.444803483155246,0.551988386604616,0.700426860411103,
0.762525122245161,0.785881086988788,0.794621043971917,0.798885153758925,
0.802368847880747,0.804374498566845,0.805973795575332,0.808032480248983,
0.811602664083345,0.825313450549338,0.943719966405224,0.954530695091559,
0.966520891886942,0.979995208431586,0.995334756667944,1.01308128280235,
1.03409192175351,1.05992385904713,1.15312596805555,1.19067635209875,1.19582725624681,
1.19842987272194,1.20030954294169,1.20230652010343,1.20512594836215,1.21098601534292,
1.27314098509753,1.47991116819721,1.5612497809114,1.60166180571516,1.61908016711595,
1.62175388831596,1.62287592646669,1.6240133112277,1.62506407795409,1.62649567105522,
1.6293567876305,1.65398201881818,1.72463604636923,1.84051827173563,2.0045064395514,
2.02002008436021,2.02390406786188,2.02617227177171,2.02815835790718,2.03061318171153,
2.03435645970311,2.05066237850186,2.31263760833465,2.37831262379276,2.41284562919197,
2.4187943957808,2.42073158153679,2.42183051281163,2.42300610602772,2.42448549078746,
2.42679195528197,2.43759645850929,2.47479509871719,2.50235015129785,2.71507719902023,
2.82821809505195,2.83686943076858,2.84016836381979,2.84243432121922,2.84464875639419,
2.84731059889031,2.85392008642146,2.91296163152424,3.10607723271175,3.16718566201027,
3.19041142713024,3.23022539778443,3.23596626748258,3.23926402402234,3.24153327329948,
3.24371993197974,3.24570813771416,3.24830837923052,3.25346145107911,3.28515815924116,
3.41943174105194,3.59169782035772,3.67629644569596,3.6894033965237,3.69653438374018,
3.70193245967649,3.70882649745226,3.72050984361697,3.76494841721059,3.76897255286623,
3.97792542616526,3.99142434773547,4.00091886147739,4.00497159761806,4.00804606250772,
4.01095584193143,4.01582572459138,4.02864038780943,4.15070151705689,4.24802021138349,
4.29981686693513,4.31321130681746,4.32129572033366,4.32859113996387,4.33796845864933,
4.35773918125188,4.39982416404737,4.47273269220943,4.74302592758338,4.75983300239487,
4.76359384413405,4.76572010237776,4.76735910887676,4.76948591241028,4.77314926725199,
4.78696847988592,4.98101737441762,5.16558161563544,5.17739938983049,5.18136180545413,
5.18358634300746,5.18561369847494,5.18832125489988,5.19335023114117,5.22035843894141,
5.27326045298571,5.37439563585434,5.58005860617515,5.59213481847676,5.59524968660384,
5.59704893669209,5.59843052497715,5.60021650589705,5.60335667618863,5.61705761770723,
5.82453883876432,5.94526275797642,5.95648364888428,5.96117372787941,5.96507992193408,
5.96908520114785,5.97494251292185,5.9902114594954,6.05778111991776,6.15317653689984,
6.31024172892292,6.33809154781145,6.34260962610404,6.34487979730575,6.34664863636598,
6.34859874066813,6.35177616355349,6.36274016658653,6.42827605828702,6.56235265701554,
6.67415497418702,6.73014367100642,6.73583202834632,6.738609749072,6.74059613447953,
6.74248140872586,6.74511666062975,6.75042338893551,6.79324536349012,6.86084017489016,
6.99643068922566,7.15077154268055,7.16090776949416,7.16309123406323,7.16449530997177,
7.16561334339644,7.1668708803443,7.16900483380658,7.1774837112125,7.24133518760423,
7.4142420867406,7.55314772555149,7.56263848752108,7.56600501203437,7.56794284305434,
7.56973853601016,7.57218130131141,7.57686556793127,7.5827171077293,7.62621886333501,
7.7110296962799,7.8001268369048,7.94979572261828,7.95921812197263,7.96157798184844,
7.96294671294924,7.96400069130473,7.96536633663348,7.96777628539521,7.97839266170175,
8.12768976201616,8.20684312721434,8.36689851981268,8.37731056456854,8.38098891766631,
8.38310250841461,8.38505880746532,8.38771669513652,8.39280244714941,8.42398018514736,
8.4915599645707,8.61424263812748,8.76856000716874,8.77924692897137,8.78281656317761,
8.78481647954515,8.78682098659246,8.78933484415522,8.79423906742558,8.82788074055006,
8.92027696197014,8.96427528803267,9.18571119328004,9.22174880095856,9.23263758814886,
9.2392874529066,9.24510470968616,9.25262605699279,9.26776789106154,9.28723466643923,
9.3323087500676,9.41267182213248,9.52825665043426,9.54078303159781,9.54490906369171,
9.54783292401341,9.55059148983615,9.55355318276258,9.55732613971713,9.56317466939706,
9.61292305907635,9.7696249262346,9.81517981302183,9.84510538447672,9.85650810045179,
9.86339513813875,9.87038522851126,9.87760419649299,9.88711035937725,9.91381911129815,
9.96048377331572),.UNSPECIFIED.);
#3543=B_SPLINE_CURVE_WITH_KNOTS('',3,(#221391,#221392,#221393,#221394,#221395,
#221396,#221397,#221398,#221399,#221400,#221401,#221402,#221403,#221404,
#221405,#221406,#221407,#221408,#221409,#221410,#221411,#221412,#221413,
#221414,#221415,#221416,#221417,#221418,#221419,#221420,#221421,#221422,
#221423,#221424,#221425,#221426,#221427,#221428,#221429,#221430,#221431,
#221432,#221433,#221434,#221435,#221436,#221437,#221438,#221439,#221440,
#221441,#221442,#221443,#221444,#221445,#221446,#221447,#221448,#221449,
#221450,#221451,#221452,#221453,#221454,#221455,#221456,#221457,#221458,
#221459,#221460,#221461,#221462,#221463,#221464,#221465,#221466,#221467,
#221468,#221469,#221470,#221471,#221472,#221473,#221474,#221475,#221476,
#221477,#221478,#221479,#221480,#221481,#221482,#221483,#221484,#221485,
#221486,#221487,#221488,#221489,#221490,#221491,#221492,#221493,#221494,
#221495,#221496,#221497,#221498,#221499,#221500,#221501,#221502,#221503,
#221504,#221505,#221506,#221507,#221508,#221509,#221510,#221511,#221512,
#221513,#221514,#221515,#221516,#221517,#221518,#221519,#221520,#221521,
#221522,#221523,#221524,#221525,#221526,#221527,#221528,#221529,#221530,
#221531,#221532,#221533,#221534,#221535,#221536,#221537,#221538,#221539,
#221540,#221541,#221542,#221543,#221544,#221545,#221546,#221547,#221548,
#221549,#221550,#221551,#221552,#221553,#221554,#221555,#221556,#221557,
#221558,#221559,#221560,#221561,#221562,#221563,#221564,#221565,#221566,
#221567,#221568,#221569,#221570,#221571,#221572,#221573,#221574,#221575,
#221576,#221577,#221578,#221579,#221580,#221581,#221582,#221583,#221584,
#221585,#221586,#221587,#221588,#221589,#221590,#221591,#221592,#221593,
#221594,#221595,#221596,#221597,#221598,#221599,#221600,#221601,#221602,
#221603,#221604,#221605,#221606,#221607,#221608,#221609,#221610,#221611,
#221612,#221613,#221614,#221615,#221616,#221617,#221618,#221619,#221620,
#221621,#221622,#221623,#221624,#221625,#221626,#221627,#221628,#221629,
#221630,#221631,#221632,#221633,#221634,#221635,#221636,#221637,#221638,
#221639,#221640,#221641,#221642,#221643,#221644,#221645,#221646,#221647,
#221648,#221649,#221650,#221651,#221652,#221653,#221654,#221655,#221656,
#221657,#221658,#221659,#221660,#221661,#221662,#221663,#221664,#221665,
#221666,#221667,#221668,#221669,#221670,#221671,#221672,#221673,#221674,
#221675,#221676,#221677,#221678,#221679,#221680,#221681,#221682,#221683,
#221684,#221685,#221686,#221687,#221688,#221689,#221690,#221691,#221692,
#221693,#221694,#221695,#221696,#221697,#221698,#221699,#221700,#221701,
#221702,#221703,#221704,#221705,#221706,#221707,#221708,#221709,#221710,
#221711,#221712,#221713,#221714,#221715,#221716,#221717,#221718,#221719,
#221720,#221721,#221722,#221723,#221724,#221725,#221726,#221727,#221728,
#221729,#221730,#221731,#221732,#221733,#221734,#221735,#221736,#221737,
#221738,#221739,#221740,#221741,#221742,#221743,#221744,#221745,#221746,
#221747,#221748,#221749,#221750,#221751,#221752,#221753,#221754,#221755,
#221756,#221757,#221758,#221759,#221760,#221761,#221762,#221763,#221764,
#221765,#221766,#221767,#221768,#221769,#221770,#221771,#221772,#221773,
#221774,#221775,#221776,#221777,#221778,#221779,#221780,#221781,#221782,
#221783,#221784,#221785,#221786,#221787,#221788,#221789,#221790,#221791,
#221792,#221793,#221794,#221795,#221796,#221797,#221798,#221799,#221800,
#221801,#221802,#221803,#221804,#221805,#221806,#221807,#221808,#221809,
#221810,#221811,#221812,#221813,#221814,#221815,#221816,#221817,#221818,
#221819,#221820,#221821,#221822,#221823,#221824,#221825,#221826,#221827,
#221828,#221829,#221830,#221831,#221832,#221833,#221834,#221835,#221836,
#221837,#221838,#221839,#221840,#221841,#221842,#221843,#221844,#221845,
#221846,#221847,#221848,#221849,#221850,#221851,#221852,#221853,#221854,
#221855,#221856,#221857,#221858,#221859,#221860,#221861,#221862,#221863,
#221864,#221865,#221866,#221867,#221868,#221869,#221870,#221871,#221872,
#221873,#221874,#221875,#221876,#221877,#221878,#221879,#221880,#221881,
#221882,#221883,#221884,#221885,#221886,#221887,#221888,#221889,#221890,
#221891,#221892,#221893,#221894,#221895,#221896,#221897,#221898,#221899,
#221900,#221901,#221902,#221903,#221904,#221905,#221906,#221907,#221908,
#221909,#221910,#221911,#221912,#221913,#221914,#221915,#221916,#221917,
#221918,#221919,#221920,#221921,#221922,#221923,#221924,#221925,#221926,
#221927,#221928,#221929,#221930,#221931,#221932,#221933,#221934,#221935,
#221936,#221937,#221938,#221939,#221940,#221941,#221942,#221943,#221944,
#221945,#221946,#221947,#221948,#221949,#221950,#221951,#221952,#221953,
#221954,#221955,#221956,#221957,#221958,#221959,#221960,#221961,#221962,
#221963,#221964,#221965,#221966,#221967,#221968,#221969,#221970,#221971,
#221972,#221973,#221974,#221975,#221976,#221977,#221978,#221979,#221980,
#221981,#221982,#221983,#221984,#221985,#221986,#221987,#221988,#221989,
#221990,#221991,#221992,#221993,#221994,#221995,#221996,#221997,#221998,
#221999,#222000,#222001,#222002,#222003,#222004),.UNSPECIFIED.,.F.,.F.,
(4,2,2,2,2,2,2,2,2,2,2,2,2,2,2,2,2,2,2,2,2,2,2,2,2,2,2,2,2,2,2,2,2,2,2,
2,2,2,2,2,2,2,2,2,2,2,2,2,2,2,2,2,2,2,2,2,2,2,2,2,2,2,2,2,2,2,2,2,2,2,2,
2,2,2,2,2,2,2,2,2,2,2,2,2,2,2,2,2,2,2,2,2,2,2,2,2,2,2,2,2,2,2,2,2,2,2,2,
2,2,2,2,2,2,2,2,2,2,2,2,2,2,2,2,2,2,2,2,2,2,2,2,2,2,2,2,2,2,2,2,2,2,2,2,
2,2,2,2,2,2,2,2,2,2,2,2,2,2,2,2,2,2,2,2,2,2,2,2,2,2,2,2,2,2,2,2,2,2,2,2,
2,2,2,2,2,2,2,2,2,2,2,2,2,2,2,2,2,2,2,2,2,2,2,2,2,2,2,2,2,2,2,2,2,2,2,2,
2,2,2,2,2,2,2,2,2,2,2,2,2,2,2,2,2,2,2,2,2,2,2,2,2,2,2,2,2,2,2,2,2,2,2,2,
2,2,2,2,2,2,2,2,2,2,2,2,2,2,2,2,2,2,2,2,2,2,2,2,2,2,2,2,2,2,2,2,2,2,2,2,
2,2,2,2,2,2,2,2,2,2,2,2,2,2,2,2,2,2,2,4),(0.00200445933661479,0.257562155059745,
0.316274882700235,0.341574413126625,0.345807148728994,0.348035012614877,
0.349857302511951,0.351960882756546,0.355526363625104,0.368395116683556,
0.532759139362108,0.574442149897183,0.587286486297553,0.605148138983943,
0.754921073955549,0.761703681846437,0.764761431261892,0.767046088233661,
0.769179874062017,0.772112168996419,0.77951926167843,0.869020137795594,
0.980654931082344,1.03865010382674,1.09909585660219,1.16491261869436,1.174708423841,
1.17750808782124,1.17921780549224,1.18076294359186,1.18273806958325,1.18664293058622,
1.20997057423235,1.21825303911419,1.22820064143878,1.22891386269151,1.41087196010116,
1.49061553569335,1.51758453081015,1.5357313333722,1.54192029068296,1.54595627159197,
1.54595733660975,1.5459584021784,1.54595946731916,1.54596053185663,1.54596159731891,
1.54596266374587,1.54596372973979,1.54596479547363,1.54596586141477,1.54596692798112,
1.54596799433288,1.54596906087551,1.54597012751087,1.54597119404546,1.54597226001324,
1.54597332620561,1.54597439292839,1.54597545926682,1.54597652562873,1.54597759221494,
1.54597865941157,1.54597972675294,1.54598079418779,1.54598186128828,1.54598292821321,
1.54598399556114,1.54598506284928,1.54598613069444,1.54598719933944,1.54598826766137,
1.54598933534996,1.54599040346131,1.54599147178244,1.54599253971556,1.54599360756868,
1.54599467601479,1.54987863171109,1.55501595061203,1.56379944330618,1.61386156826146,
1.83972786939599,1.90262466217746,1.92115777257303,1.92493877921191,1.92702228319894,
1.9286036212427,1.93036054009782,1.93355146565727,1.94349208004349,2.08120188211125,
2.23710547049427,2.28741975754036,2.31430639676666,2.31904113969932,2.32155689427955,
2.32342617853064,2.32546296550913,2.32905272656481,2.33950108669311,2.49832925086366,
2.63556079002027,2.74038932741481,2.74415769859847,2.74574654320756,2.74689225997345,
2.74793344460349,2.74932520104005,2.75202811306479,2.77227766855203,2.90679891325944,
3.0269351401939,3.07846506811425,3.13959144144883,3.1455196358291,3.14820849671315,
3.15022402602026,3.15211111284459,3.15471159111842,3.1613176581111,3.24196515857597,
3.27392709476174,3.43861951918611,3.53831774259555,3.54206117452088,3.54368869580022,
3.54488558796346,3.54598989922357,3.54748650815047,3.55115893198215,3.58835073661744,
3.68457627658784,3.84868505509515,3.91309732211954,3.95517812542462,3.96064453750795,
3.96338093778996,3.96534721200938,3.96742693740111,3.97034823442838,3.9763728402556,
4.03829248779477,4.18429186786753,4.34445851041227,4.35963643615124,4.36353239791952,
4.36582793083678,4.36785097408873,4.37036912336293,4.37424826947605,4.39183838641528,
4.40168267924723,4.4327367824747,4.52799371074605,4.70253413940462,4.76759391394344,
4.80334573141613,4.81380397408981,4.82035831299367,4.82642317567252,4.8342774424765,
4.84737840414369,4.98102876442705,5.0499437550147,5.11638298519625,5.12379022516316,
5.12750540482588,5.13054181913247,5.13404722512841,5.14015740530248,5.16662221891198,
5.2207413622884,5.35939993422906,5.37365096605442,5.42130155451077,5.43486760685969,
5.44298825593349,5.44954266096578,5.45847977156309,5.47597232963744,5.57571399612995,
5.65099074577087,5.85357165165343,5.87975480239824,5.88389122758383,5.88632991175477,
5.88818265097178,5.89014852572189,5.89319123313548,5.90238176234558,5.95012347399396,
5.9816168363335,6.28201837390373,6.29802224606703,6.3024324409306,6.30502929367345,
6.30727576369897,6.31001787852728,6.31521278893304,6.34562842023349,6.40155217281647,
6.55976297581316,6.70497822124924,6.71399837732852,6.71683027724222,6.71837489961005,
6.71987976775037,6.72170012714423,6.72366296325356,6.72674218300685,6.73261116721234,
6.94462507295509,7.06632597099788,7.07755306653769,7.08224264953312,7.08614712579224,
7.09014930679843,7.09599962392249,7.11123780317845,7.17860846332306,7.27279030415763,
7.43568959212578,7.45931710530968,7.46323200104254,7.465562003216,7.4673077930834,
7.46916324122535,7.47199502299718,7.47525928277452,7.48123821805066,7.52863975413416,
7.56006660705792,7.83951581558997,7.85476455496277,7.85887944735428,7.86128356957373,
7.86335181254644,7.86586196120119,7.8705740931098,7.89702611390657,7.94551986511262,
7.98887676023074,8.01590077986302,8.03732487544955,8.18257536128988,8.20979173530086,
8.21389035885154,8.27890476410037,8.28299653005717,8.28451921441541,8.28559532550958,
8.28660634317125,8.28768145338652,8.28996704928214,8.30051906358285,8.32039596883359,
8.37608838564092,8.43872892097657,8.52236232126092,8.67275158479116,8.68269592280739,
8.68612593590125,8.68807542390742,8.68986659730358,8.69228019292654,8.69683233013144,
8.72291130557021,8.76231548052929,8.83262914957418,8.85260257459218,8.86903421769268,
8.88290461776496,8.89480487674223,8.90512905407852,8.98816205325646,9.07463893131991,
9.07989220957653,9.08180749768764,9.08293660622949,9.08400010448483,9.08513543316742,
9.08657462669668,9.09206338453848,9.10031640289146,9.12479578442805,9.19883708865226,
9.47824368637398,9.49557089306043,9.50000519443093,9.50254759244992,9.50449034737361,
9.50698979746876,9.51135164416166,9.52989600276192,9.70504086677498,9.85628699878259,
9.86637980922595,9.89599042482016,9.90106993892853,9.90365431863312,9.90560914742451,
9.90750818051455,9.90970720603225,9.91283938594869,9.9182320202591,9.95798028600589),
 .UNSPECIFIED.);
#3544=B_SPLINE_CURVE_WITH_KNOTS('',3,(#222006,#222007,#222008,#222009,#222010,
#222011,#222012,#222013,#222014,#222015,#222016,#222017,#222018),
 .UNSPECIFIED.,.F.,.F.,(4,1,1,1,1,1,1,1,1,1,4),(151.920096078454,152.307809718983,
152.807179586914,153.306549454845,153.805919322776,154.804659058638,155.30402892657,
155.803398794501,156.802138530363,157.800878266225,158.203281385634),
 .UNSPECIFIED.);
#3545=B_SPLINE_CURVE_WITH_KNOTS('',3,(#222020,#222021,#222022,#222023,#222024,
#222025,#222026,#222027,#222028,#222029,#222030,#222031,#222032,#222033,
#222034,#222035,#222036,#222037),.UNSPECIFIED.,.F.,.F.,(4,2,2,2,2,2,2,2,
4),(158.203281385634,159.038198297529,159.873115209424,160.708032121318,
161.542949033213,162.377865945108,163.212782857003,164.047699768898,164.486466692813),
 .UNSPECIFIED.);
#3546=B_SPLINE_CURVE_WITH_KNOTS('',3,(#222039,#222040,#222041,#222042,#222043,
#222044,#222045,#222046,#222047,#222048,#222049,#222050,#222051),
 .UNSPECIFIED.,.F.,.F.,(4,1,1,1,1,1,1,1,1,1,4),(164.486466692813,164.79205641726,
165.790796153122,166.290166021054,166.789535888985,167.288905756916,167.788275624847,
168.787015360709,169.28638522864,169.785755096571,170.769649602841),
 .UNSPECIFIED.);
#3547=B_SPLINE_CURVE_WITH_KNOTS('',3,(#222053,#222054,#222055,#222056,#222057,
#222058,#222059,#222060,#222061,#222062,#222063,#222064,#222065,#222066,
#222067,#222068,#222069,#222070,#222071,#222072,#222073,#222074,#222075,
#222076,#222077,#222078,#222079,#222080,#222081,#222082,#222083,#222084,
#222085,#222086,#222087,#222088,#222089,#222090,#222091,#222092,#222093,
#222094,#222095,#222096,#222097,#222098,#222099,#222100,#222101,#222102,
#222103,#222104,#222105,#222106,#222107,#222108,#222109,#222110,#222111,
#222112,#222113,#222114,#222115,#222116,#222117,#222118,#222119,#222120,
#222121,#222122,#222123,#222124,#222125,#222126,#222127,#222128,#222129,
#222130,#222131,#222132,#222133,#222134,#222135,#222136,#222137,#222138,
#222139,#222140,#222141,#222142,#222143,#222144,#222145,#222146,#222147,
#222148,#222149,#222150,#222151,#222152,#222153,#222154,#222155,#222156,
#222157,#222158,#222159,#222160,#222161,#222162,#222163,#222164,#222165,
#222166,#222167,#222168,#222169,#222170,#222171,#222172,#222173,#222174,
#222175,#222176,#222177,#222178,#222179,#222180,#222181,#222182,#222183,
#222184,#222185,#222186,#222187,#222188,#222189,#222190,#222191,#222192,
#222193,#222194,#222195,#222196,#222197,#222198,#222199,#222200,#222201,
#222202,#222203,#222204,#222205,#222206,#222207,#222208,#222209,#222210,
#222211,#222212,#222213,#222214,#222215,#222216,#222217,#222218,#222219,
#222220,#222221,#222222,#222223,#222224,#222225,#222226,#222227,#222228,
#222229,#222230,#222231,#222232,#222233,#222234,#222235,#222236,#222237,
#222238,#222239,#222240,#222241,#222242,#222243,#222244,#222245,#222246,
#222247,#222248,#222249,#222250,#222251,#222252,#222253,#222254,#222255,
#222256,#222257,#222258,#222259,#222260,#222261,#222262,#222263,#222264,
#222265,#222266,#222267,#222268,#222269,#222270,#222271,#222272,#222273,
#222274,#222275,#222276,#222277,#222278,#222279,#222280,#222281,#222282,
#222283,#222284,#222285,#222286,#222287,#222288,#222289,#222290,#222291,
#222292,#222293,#222294,#222295,#222296,#222297,#222298,#222299,#222300,
#222301,#222302,#222303,#222304,#222305,#222306,#222307,#222308,#222309,
#222310,#222311,#222312,#222313,#222314),.UNSPECIFIED.,.F.,.F.,(4,3,3,3,
3,3,3,3,3,3,3,3,3,3,3,3,3,3,3,3,3,3,3,3,3,3,3,3,3,3,3,3,3,3,3,3,3,3,3,3,
3,3,3,3,3,3,3,3,3,3,3,3,3,3,3,3,3,3,3,3,3,3,3,3,3,3,3,3,3,3,3,3,3,3,3,3,
3,3,3,3,3,3,3,3,3,3,3,4),(170.769651999993,170.784494832433,170.857633776118,
170.930684693425,171.003662517447,171.076582111962,171.149458286939,171.22230581252,
171.29515330968,171.368004458218,171.440872607319,171.513771117372,171.586756558935,
171.659789371711,171.732933795829,171.783234568296,171.858762856963,171.934205052296,
172.009574059991,172.084882737954,172.160143904354,172.23787270433,172.313082901655,
172.388287126354,172.463496936619,172.538723891604,172.614006781214,172.689322828085,
172.764709737342,172.781974304158,172.858566204559,172.935092906499,173.011564102391,
173.087980962652,173.164365001485,173.240725164898,173.281344172089,173.359463440568,
173.437627744043,173.515841821031,173.594146943719,173.672500370318,173.750939460084,
173.78071404002,173.862692818607,173.944599567848,174.028470652873,174.110136065388,
174.195109986669,174.280083907951,174.353695582057,174.42730194891,174.500916000811,
174.57458229334,174.648275821364,174.722051294429,174.779453775882,174.855954500688,
174.932399267869,175.008798987449,175.085164537056,175.161506769247,175.238592612059,
175.314934425435,175.391286513078,175.467658737185,175.545292430825,175.621764107818,
175.699978809781,175.778193511744,175.852875326433,175.927477178584,176.002011462157,
176.076480019692,176.150910235284,176.225315147085,176.277563379675,176.357860628097,
176.438303101,176.522960637651,176.603740784067,176.684622295,176.765639095402,
176.776933247606,176.864827893909,176.952337296125,177.039186513869,177.052837150721),
 .UNSPECIFIED.);
#3548=B_SPLINE_CURVE_WITH_KNOTS('',3,(#222316,#222317,#222318,#222319,#222320,
#222321,#222322,#222323,#222324,#222325,#222326,#222327,#222328),
 .UNSPECIFIED.,.F.,.F.,(4,1,1,1,1,1,1,1,1,1,4),(177.052837307173,177.775672983469,
178.774412719331,179.773152455193,180.272522323124,180.771892191055,181.271262058986,
181.770631926917,182.76937166278,183.268741530711,183.336022614352),
 .UNSPECIFIED.);
#3549=B_SPLINE_CURVE_WITH_KNOTS('',3,(#222330,#222331,#222332,#222333,#222334,
#222335,#222336,#222337,#222338,#222339,#222340,#222341,#222342,#222343,
#222344,#222345,#222346,#222347,#222348,#222349,#222350,#222351,#222352,
#222353,#222354,#222355,#222356,#222357,#222358,#222359,#222360,#222361,
#222362,#222363,#222364,#222365,#222366,#222367,#222368,#222369,#222370,
#222371,#222372,#222373,#222374,#222375,#222376,#222377,#222378,#222379,
#222380,#222381,#222382,#222383,#222384,#222385,#222386,#222387,#222388,
#222389,#222390,#222391,#222392,#222393,#222394,#222395,#222396,#222397,
#222398,#222399,#222400,#222401,#222402,#222403,#222404,#222405,#222406,
#222407,#222408,#222409,#222410,#222411,#222412,#222413,#222414,#222415,
#222416,#222417,#222418,#222419,#222420,#222421,#222422,#222423,#222424,
#222425,#222426,#222427,#222428,#222429,#222430,#222431,#222432,#222433,
#222434,#222435,#222436,#222437,#222438,#222439,#222440,#222441,#222442,
#222443,#222444,#222445,#222446,#222447,#222448,#222449,#222450,#222451,
#222452,#222453,#222454,#222455,#222456,#222457,#222458,#222459,#222460,
#222461,#222462,#222463,#222464,#222465,#222466,#222467,#222468,#222469,
#222470,#222471,#222472,#222473,#222474,#222475,#222476,#222477,#222478,
#222479,#222480,#222481,#222482,#222483,#222484,#222485,#222486,#222487,
#222488,#222489,#222490,#222491,#222492,#222493,#222494,#222495,#222496,
#222497,#222498,#222499,#222500,#222501,#222502,#222503,#222504,#222505,
#222506,#222507,#222508,#222509,#222510,#222511,#222512,#222513,#222514,
#222515,#222516,#222517,#222518,#222519,#222520,#222521,#222522,#222523,
#222524,#222525,#222526,#222527,#222528,#222529,#222530,#222531,#222532,
#222533,#222534,#222535,#222536,#222537,#222538,#222539,#222540,#222541,
#222542,#222543,#222544,#222545,#222546,#222547,#222548,#222549,#222550,
#222551,#222552,#222553,#222554,#222555,#222556,#222557,#222558,#222559,
#222560,#222561,#222562,#222563,#222564,#222565,#222566,#222567,#222568,
#222569,#222570,#222571,#222572,#222573,#222574,#222575,#222576,#222577,
#222578,#222579,#222580,#222581,#222582,#222583,#222584,#222585,#222586,
#222587,#222588,#222589,#222590,#222591),.UNSPECIFIED.,.F.,.F.,(4,3,3,3,
3,3,3,3,3,3,3,3,3,3,3,3,3,3,3,3,3,3,3,3,3,3,3,3,3,3,3,3,3,3,3,3,3,3,3,3,
3,3,3,3,3,3,3,3,3,3,3,3,3,3,3,3,3,3,3,3,3,3,3,3,3,3,3,3,3,3,3,3,3,3,3,3,
3,3,3,3,3,3,3,3,3,3,3,4),(183.336022710285,183.418369237534,183.500946924274,
183.583821518175,183.666843220968,183.750041231153,183.768111398642,183.842640868417,
183.917094196739,183.9914852864,184.065827999059,184.14013616408,184.214423587004,
184.288719132779,184.363023638853,184.43734960221,184.511709528832,184.586155211748,
184.66065006493,184.735247010616,184.766851134504,184.839990078184,184.913040995486,
184.986018819503,185.058938414014,185.131814588985,185.204662114563,185.277509611718,
185.350360760251,185.423228909348,185.496127419396,185.569112860954,185.642145673725,
185.715290097839,185.765590870366,185.841119159016,185.916561354331,185.991930362009,
186.067239039954,186.142500206338,186.220229006324,186.295439203632,186.370643428313,
186.445853238561,186.52108019353,186.596363083123,186.671679129978,186.747066039219,
186.764330606228,186.840922506793,186.917449208897,186.993920404951,187.070337265371,
187.146721304362,187.223081467929,187.263700474159,187.341819742201,187.419984045232,
187.498198121775,187.576503244015,187.654856670165,187.733295759485,187.763070342091,
187.845049121599,187.926955871758,188.010826956324,188.092492369716,188.177466289869,
188.262440210022,188.336051883564,188.40965824985,188.483272301184,188.556938593144,
188.630632120597,188.704407593094,188.761810077953,188.83712615777,188.912381635905,
188.987589440095,189.066503531416,189.141660684109,189.216812290113,189.291970005769,
189.367145488611,189.442379450268,189.517647220403,189.592990271303,189.61890217066),
 .UNSPECIFIED.);
#3550=B_SPLINE_CURVE_WITH_KNOTS('',3,(#222593,#222594,#222595,#222596,#222597,
#222598,#222599,#222600,#222601,#222602,#222603,#222604,#222605,#222606,
#222607,#222608,#222609,#222610,#222611,#222612,#222613,#222614,#222615,
#222616,#222617,#222618,#222619,#222620,#222621,#222622,#222623,#222624,
#222625,#222626,#222627,#222628,#222629,#222630,#222631,#222632,#222633,
#222634,#222635,#222636,#222637,#222638,#222639,#222640,#222641,#222642,
#222643,#222644,#222645,#222646,#222647,#222648,#222649,#222650,#222651,
#222652,#222653,#222654,#222655,#222656,#222657,#222658,#222659,#222660,
#222661,#222662,#222663,#222664,#222665,#222666,#222667,#222668,#222669,
#222670,#222671,#222672,#222673,#222674,#222675,#222676,#222677,#222678,
#222679,#222680,#222681,#222682,#222683,#222684,#222685,#222686,#222687,
#222688,#222689,#222690,#222691,#222692,#222693,#222694,#222695,#222696,
#222697,#222698,#222699,#222700,#222701,#222702,#222703,#222704,#222705,
#222706,#222707,#222708,#222709,#222710,#222711,#222712,#222713,#222714,
#222715,#222716,#222717,#222718,#222719,#222720,#222721,#222722,#222723,
#222724,#222725,#222726,#222727,#222728,#222729,#222730,#222731,#222732,
#222733,#222734,#222735,#222736,#222737,#222738,#222739,#222740,#222741,
#222742,#222743,#222744,#222745,#222746,#222747,#222748,#222749,#222750,
#222751,#222752,#222753,#222754,#222755,#222756,#222757,#222758,#222759,
#222760,#222761,#222762,#222763,#222764,#222765,#222766,#222767,#222768,
#222769,#222770,#222771,#222772,#222773,#222774,#222775,#222776,#222777,
#222778,#222779,#222780,#222781,#222782,#222783,#222784,#222785,#222786,
#222787,#222788,#222789,#222790,#222791,#222792,#222793,#222794,#222795,
#222796,#222797,#222798,#222799,#222800,#222801,#222802,#222803,#222804,
#222805,#222806,#222807,#222808,#222809,#222810,#222811,#222812,#222813,
#222814,#222815,#222816,#222817,#222818,#222819,#222820,#222821,#222822,
#222823,#222824,#222825,#222826,#222827,#222828,#222829,#222830,#222831,
#222832,#222833,#222834,#222835,#222836,#222837,#222838,#222839,#222840,
#222841,#222842,#222843,#222844,#222845,#222846,#222847,#222848,#222849,
#222850,#222851,#222852,#222853,#222854,#222855,#222856,#222857,#222858,
#222859,#222860,#222861,#222862,#222863,#222864,#222865,#222866,#222867,
#222868,#222869,#222870,#222871,#222872,#222873,#222874,#222875,#222876,
#222877,#222878,#222879,#222880,#222881,#222882,#222883,#222884,#222885,
#222886,#222887,#222888,#222889,#222890,#222891,#222892,#222893,#222894,
#222895,#222896,#222897,#222898,#222899,#222900,#222901,#222902,#222903,
#222904,#222905,#222906,#222907,#222908,#222909,#222910,#222911,#222912,
#222913,#222914,#222915,#222916,#222917,#222918,#222919,#222920,#222921,
#222922,#222923,#222924,#222925,#222926,#222927,#222928,#222929,#222930,
#222931,#222932,#222933,#222934,#222935,#222936,#222937,#222938,#222939,
#222940,#222941,#222942,#222943,#222944,#222945,#222946,#222947,#222948,
#222949,#222950,#222951,#222952,#222953,#222954,#222955,#222956,#222957,
#222958,#222959,#222960,#222961,#222962,#222963,#222964,#222965,#222966,
#222967,#222968,#222969,#222970,#222971,#222972,#222973,#222974,#222975,
#222976,#222977,#222978,#222979,#222980,#222981,#222982,#222983,#222984,
#222985,#222986,#222987,#222988,#222989,#222990,#222991,#222992,#222993,
#222994,#222995,#222996,#222997,#222998,#222999,#223000,#223001,#223002,
#223003,#223004,#223005,#223006,#223007,#223008,#223009,#223010,#223011,
#223012,#223013,#223014,#223015,#223016,#223017,#223018,#223019,#223020,
#223021,#223022,#223023,#223024,#223025,#223026,#223027,#223028,#223029,
#223030,#223031,#223032,#223033,#223034,#223035,#223036,#223037,#223038,
#223039,#223040,#223041,#223042,#223043,#223044,#223045,#223046,#223047,
#223048,#223049,#223050,#223051,#223052,#223053,#223054,#223055,#223056,
#223057,#223058,#223059,#223060,#223061,#223062,#223063,#223064,#223065,
#223066,#223067,#223068,#223069,#223070,#223071,#223072,#223073,#223074,
#223075,#223076,#223077,#223078,#223079,#223080,#223081,#223082,#223083,
#223084,#223085,#223086,#223087,#223088,#223089,#223090,#223091,#223092,
#223093,#223094,#223095,#223096,#223097,#223098,#223099,#223100,#223101,
#223102,#223103,#223104,#223105,#223106,#223107,#223108,#223109,#223110,
#223111,#223112,#223113,#223114,#223115,#223116,#223117,#223118,#223119,
#223120,#223121,#223122,#223123,#223124,#223125,#223126,#223127,#223128,
#223129,#223130,#223131,#223132,#223133,#223134),.UNSPECIFIED.,.F.,.F.,
(4,2,2,2,2,2,2,2,2,2,2,2,2,2,2,2,2,2,2,2,2,2,2,2,2,2,2,2,2,2,2,2,2,2,2,
2,2,2,2,2,2,2,2,2,2,2,2,2,2,2,2,2,2,2,2,2,2,2,2,2,2,2,2,2,2,2,2,2,2,2,2,
2,2,2,2,2,2,2,2,2,2,2,2,2,2,2,2,2,2,2,2,2,2,2,2,2,2,2,2,2,2,2,2,2,2,2,2,
2,2,2,2,2,2,2,2,2,2,2,2,2,2,2,2,2,2,2,2,2,2,2,2,2,2,2,2,2,2,2,2,2,2,2,2,
2,2,2,2,2,2,2,2,2,2,2,2,2,2,2,2,2,2,2,2,2,2,2,2,2,2,2,2,2,2,2,2,2,2,2,2,
2,2,2,2,2,2,2,2,2,2,2,2,2,2,2,2,2,2,2,2,2,2,2,2,2,2,2,2,2,2,2,2,2,2,2,2,
2,2,2,2,2,2,2,2,2,2,2,2,2,2,2,2,2,2,2,2,2,2,2,2,2,2,2,2,2,2,2,2,2,2,2,2,
2,2,2,2,2,2,2,2,2,2,2,2,2,2,2,2,2,2,2,4),(0.00141478209296347,0.116359404994446,
0.120713596378298,0.123214540612478,0.124937161336518,0.126623797141894,
0.128174337153862,0.130160235713197,0.133408934317356,0.150951991650534,
0.155749334295669,0.272937339542111,0.298978788255001,0.321770711377344,
0.373371119871339,0.473387650117704,0.481487790296529,0.486559257208962,
0.491316542452597,0.49477628650431,0.498478450251031,0.503759688630404,
0.514873934986964,0.704474471907343,0.773461894469543,0.837295790827264,
0.857270300442468,0.865073774911546,0.870679413777046,0.872621998411138,
0.874523090099118,0.876306419379916,0.878640993518927,0.882561907340408,
0.906034300954475,0.92741173681054,0.98542029462302,1.07896996220131,1.0912915984963,
1.10580264940794,1.12324718155251,1.18374223683944,1.23415143619826,1.2610063247466,
1.2657386548023,1.26825351019186,1.27032248806344,1.27272390408731,1.27682541294864,
1.29193252202704,1.50928071719468,1.60323321708623,1.64914433952348,1.6758190985247,
1.68908655310731,1.69157661288434,1.69291822518187,1.69402096091606,1.69531990823265,
1.69758797984725,1.70662127054167,1.84562906207161,1.99180643756179,2.02136389862685,
2.08005241041187,2.09060325162782,2.09398519473297,2.09614101616721,2.09815177665687,
2.10076760202711,2.1051294183366,2.11465336865836,2.292862221828,2.3977452646824,
2.44254255592615,2.47225966332362,2.48673261002166,2.48932521246531,2.49073025657572,
2.49188960883048,2.49308054306052,2.49530111103813,2.50268360430771,2.61449783213889,
2.7566490473711,2.89395538917891,2.90503701291405,2.90867091643284,2.91100878839675,
2.91320465382772,2.91608342247698,2.92243975105969,2.97355239232443,3.16934045245947,
3.24744999612144,3.27781382061395,3.30484355193634,3.30949127761645,3.31195107996309,
3.31397015828103,3.31600574299151,3.31974731734248,3.33181692527709,3.34186054006806,
3.34415719894622,3.4563422381925,3.63615425134901,3.74346699886949,3.75751928689668,
3.76484696221741,3.77026154518949,3.77615064600599,3.78655948072165,3.81795239455225,
3.98709659398994,4.04062311540851,4.06610994909314,4.07170786820321,4.07508129434783,
4.07813676821402,4.08205623412285,4.09014136897172,4.19101267416699,4.20490129226199,
4.3239442090558,4.35380498803724,4.37607020609286,4.38592139102362,4.39328217418404,
4.40019654021417,4.40982546353891,4.43558488579211,4.60938192688126,4.74921468486974,
4.8032303827859,4.82707226094502,4.83123819953745,4.83345169580967,4.8350963443329,
4.83688866530264,4.8400499951728,4.8492586136554,4.978535670744,5.22735475449493,
5.24420123961521,5.24869788283818,5.25131508635557,5.253539201544,5.25624796656749,
5.26128571005427,5.28848866018707,5.34178805470377,5.44519511585523,5.64808449119481,
5.65992105371258,5.6630140562037,5.66480781563575,5.6661890288924,5.66797909911986,
5.67113967557324,5.68513168809714,5.89233576998291,6.01287253798258,6.02408704939539,
6.02877483801351,6.03267928157106,6.0366829260164,6.0425381396563,6.05780290066231,
6.12536105281249,6.22081382715594,6.37722499988755,6.3920553984691,6.4069658588054,
6.41031449931962,6.41249742674544,6.41425639358635,6.41625762668003,6.41966626074085,
6.43306718102309,6.58931404627895,6.74184465204506,6.797563147668,6.80324253650551,
6.80601751036979,6.80800268087551,6.81009680096605,6.81284658402001,6.81873791247382,
6.89618879935492,7.04940887811756,7.21756355456425,7.22814829856036,7.23036541799864,
7.23177967345,7.23289843764632,7.23414906003042,7.23625205251837,7.24437958209808,
7.30285732956871,7.39807710413337,7.51015359261545,7.55692041408943,7.62447342919497,
7.63079653751478,7.63334877150556,7.63522348075787,7.63724733996519,7.63998498760219,
7.64299607044376,7.64810472380772,7.77661672313094,7.8610655066267,7.98791079850766,
8.02415904802625,8.02738635517798,8.02895612160769,8.03007940539563,8.03114582313132,
8.03263687473307,8.035639404262,8.05965302495922,8.12792990748607,8.26577714132999,
8.36364883022773,8.43834150360216,8.445243363526,8.44802604776885,8.45006898643234,
8.45227351423497,8.45525394017297,8.46199005889707,8.58455271122478,8.67493242463407,
8.83445073387878,8.84560930882574,8.84923788364449,8.85124750205198,8.85326589689574,
8.85575948249289,8.86057839100535,8.89201458938135,8.93912520555978,8.99940659501446,
9.04418114539806,9.2686714225183,9.29097838796148,9.29912743532482,9.30489584624313,
9.31082684438023,9.3152613209626,9.32229933418327,9.33286062879409,9.35205256135841,
9.39623637984588,9.59476159566194,9.60691808190879,9.61096430385776,9.61383759255424,
9.61655847052943,9.61948173177422,9.62321636905001,9.62901963608366,9.68950152708124,
9.88048070961918,9.91187820042959,9.92332779106643,9.93010636852422,9.93696233355684,
9.94394595622972,9.95697286124426),.UNSPECIFIED.);
#3551=B_SPLINE_CURVE_WITH_KNOTS('',3,(#223136,#223137,#223138,#223139,#223140,
#223141,#223142,#223143,#223144,#223145,#223146,#223147,#223148,#223149,
#223150,#223151,#223152,#223153),.UNSPECIFIED.,.F.,.F.,(4,2,2,2,2,2,2,2,
4),(202.185578535891,203.020495447786,203.855412359681,204.690329271575,
205.52524618347,206.360163095365,207.19508000726,208.029996919155,208.46876384307),
 .UNSPECIFIED.);
#3552=B_SPLINE_CURVE_WITH_KNOTS('',3,(#223155,#223156,#223157,#223158,#223159,
#223160,#223161,#223162,#223163,#223164,#223165,#223166,#223167,#223168,
#223169,#223170,#223171,#223172,#223173,#223174,#223175,#223176,#223177,
#223178,#223179,#223180,#223181,#223182,#223183,#223184,#223185,#223186,
#223187,#223188,#223189,#223190,#223191,#223192,#223193,#223194,#223195,
#223196,#223197,#223198,#223199,#223200,#223201,#223202,#223203,#223204,
#223205,#223206,#223207,#223208,#223209,#223210,#223211,#223212,#223213,
#223214,#223215,#223216,#223217,#223218,#223219,#223220,#223221,#223222,
#223223,#223224,#223225,#223226,#223227,#223228,#223229,#223230,#223231,
#223232,#223233,#223234,#223235,#223236,#223237,#223238,#223239,#223240,
#223241,#223242,#223243,#223244,#223245,#223246,#223247,#223248,#223249,
#223250,#223251,#223252,#223253,#223254,#223255,#223256,#223257,#223258,
#223259,#223260,#223261,#223262,#223263,#223264,#223265,#223266,#223267,
#223268,#223269,#223270,#223271,#223272,#223273,#223274,#223275,#223276,
#223277,#223278,#223279,#223280,#223281,#223282,#223283,#223284,#223285,
#223286,#223287,#223288,#223289,#223290,#223291,#223292,#223293,#223294,
#223295,#223296,#223297,#223298,#223299,#223300,#223301,#223302,#223303,
#223304,#223305,#223306,#223307,#223308,#223309,#223310,#223311,#223312,
#223313,#223314,#223315,#223316,#223317,#223318,#223319,#223320,#223321,
#223322,#223323,#223324,#223325,#223326,#223327,#223328,#223329,#223330,
#223331,#223332,#223333,#223334,#223335,#223336,#223337,#223338,#223339,
#223340,#223341,#223342,#223343,#223344,#223345,#223346,#223347,#223348,
#223349,#223350,#223351,#223352,#223353,#223354,#223355,#223356,#223357,
#223358,#223359,#223360,#223361,#223362,#223363,#223364,#223365,#223366,
#223367,#223368,#223369,#223370,#223371,#223372,#223373,#223374,#223375,
#223376,#223377,#223378,#223379,#223380,#223381,#223382,#223383,#223384,
#223385,#223386,#223387,#223388,#223389,#223390,#223391,#223392,#223393,
#223394,#223395,#223396,#223397,#223398,#223399,#223400,#223401,#223402,
#223403,#223404,#223405,#223406,#223407,#223408,#223409,#223410,#223411,
#223412,#223413,#223414,#223415,#223416,#223417,#223418,#223419,#223420,
#223421,#223422,#223423,#223424,#223425,#223426,#223427,#223428,#223429,
#223430,#223431,#223432,#223433,#223434,#223435,#223436,#223437,#223438,
#223439,#223440,#223441,#223442,#223443,#223444,#223445,#223446,#223447,
#223448,#223449,#223450,#223451,#223452,#223453,#223454,#223455,#223456,
#223457,#223458,#223459,#223460,#223461,#223462,#223463,#223464,#223465,
#223466,#223467,#223468,#223469,#223470,#223471,#223472,#223473,#223474,
#223475,#223476,#223477,#223478,#223479,#223480,#223481,#223482,#223483,
#223484,#223485,#223486,#223487,#223488,#223489,#223490,#223491,#223492,
#223493,#223494,#223495,#223496,#223497,#223498,#223499,#223500,#223501,
#223502,#223503,#223504,#223505,#223506,#223507,#223508,#223509,#223510,
#223511,#223512,#223513,#223514,#223515,#223516,#223517,#223518,#223519,
#223520,#223521,#223522,#223523,#223524,#223525,#223526,#223527,#223528,
#223529,#223530,#223531,#223532,#223533,#223534,#223535,#223536,#223537,
#223538,#223539,#223540,#223541,#223542,#223543,#223544,#223545,#223546,
#223547,#223548,#223549,#223550,#223551,#223552,#223553,#223554,#223555,
#223556,#223557,#223558,#223559,#223560,#223561,#223562,#223563,#223564,
#223565,#223566,#223567,#223568,#223569,#223570,#223571,#223572,#223573,
#223574,#223575,#223576,#223577,#223578,#223579,#223580,#223581,#223582,
#223583,#223584,#223585,#223586,#223587,#223588,#223589,#223590,#223591,
#223592,#223593,#223594,#223595,#223596,#223597,#223598,#223599,#223600,
#223601,#223602,#223603,#223604,#223605,#223606,#223607,#223608,#223609,
#223610,#223611,#223612,#223613,#223614,#223615,#223616,#223617,#223618,
#223619,#223620,#223621,#223622,#223623,#223624,#223625,#223626,#223627,
#223628,#223629,#223630,#223631,#223632,#223633,#223634,#223635,#223636,
#223637,#223638,#223639,#223640,#223641,#223642,#223643,#223644,#223645,
#223646,#223647,#223648,#223649,#223650,#223651,#223652,#223653,#223654,
#223655,#223656,#223657,#223658,#223659,#223660,#223661,#223662,#223663,
#223664),.UNSPECIFIED.,.F.,.F.,(4,2,2,2,2,2,2,2,2,2,2,2,2,2,2,2,2,2,2,2,
2,2,2,2,2,2,2,2,2,2,2,2,2,2,2,2,2,2,2,2,2,2,2,2,2,2,2,2,2,2,2,2,2,2,2,2,
2,2,2,2,2,2,2,2,2,2,2,2,2,2,2,2,2,2,2,2,2,2,2,2,2,2,2,2,2,2,2,2,2,2,2,2,
2,2,2,2,2,2,2,2,2,2,2,2,2,2,2,2,2,2,2,2,2,2,2,2,2,2,2,2,2,2,2,2,2,2,2,2,
2,2,2,2,2,2,2,2,2,2,2,2,2,2,2,2,2,2,2,2,2,2,2,2,2,2,2,2,2,2,2,2,2,2,2,2,
2,2,2,2,2,2,2,2,2,2,2,2,2,2,2,2,2,2,2,2,2,2,2,2,2,2,2,2,2,2,2,2,2,2,2,2,
2,2,2,2,2,2,2,2,2,2,2,2,2,2,2,2,2,2,2,2,2,2,2,2,2,2,2,2,2,2,2,2,2,2,2,2,
2,2,2,2,2,2,2,2,2,2,2,2,2,2,2,2,2,2,4),(0.00133830262631356,0.139438357579086,
0.200909927955577,0.209508844580474,0.211752834325512,0.213080352109106,
0.21425700926626,0.215748706974759,0.218098192436531,0.229507013707793,
0.421993595380599,0.451620266910188,0.480376448296373,0.564544135124727,
0.602832587721176,0.606901427897204,0.610432288970518,0.612716015638118,
0.614869745106133,0.617705946905205,0.624020649056565,0.676613099641912,
0.792716358974852,0.863680718094834,0.944020370796353,0.99289578010674,
1.00250355589665,1.00485610951166,1.00623714079598,1.0074604759438,1.00899088934706,
1.01136000470524,1.0221962463077,1.20354130757576,1.30998710672542,1.38605329671361,
1.39215352513267,1.39506367492406,1.39727253011517,1.39936098582232,1.40285072718565,
1.41191520827557,1.54771635385412,1.63867471557651,1.72911277505056,1.78088275114964,
1.78876314347224,1.79098132633146,1.79232785980166,1.79353937140027,1.79508039105697,
1.7982538373683,1.81927056726594,1.96200762844306,2.04847660565329,2.14113543824455,
2.17773569801643,2.18287239840428,2.1854935870463,2.1873835799262,2.18938865687908,
2.19278630229899,2.20186958155214,2.33722773467721,2.50060575595169,2.57149882734751,
2.58060493690987,2.58286362986976,2.58417822291274,2.58532648014708,2.58674195305811,
2.58891753397617,2.59889492988857,2.75135851960496,2.88939193510352,2.96216521301957,
2.99425031221139,2.99916571891074,3.00170106364452,3.00355333098142,3.00554124911303,
3.00896688569999,3.01845745509103,3.16296825385149,3.32543755771256,3.34898711237156,
3.39147184743647,3.39970383932617,3.40244844803796,3.40422617717617,3.40590456287852,
3.40811769542958,3.41187806073602,3.43562639104619,3.54773631740017,3.6676714469246,
3.77225498147016,3.78226586073498,3.78694540533719,3.79051851051431,3.79391491178562,
3.79868197694032,3.80851603030731,3.97441210778706,4.119683924084,4.14888688815871,
4.15269904518385,4.15460964287051,4.1559831629307,4.15743660377674,4.159478642271,
4.16368645322822,4.22050801050266,4.41190400161341,4.55663191296641,4.56336107757395,
4.5663979885925,4.56866838544094,4.57078979759241,4.57370655964312,4.58108207041647,
4.67058351988751,4.89358917796121,4.92474876578906,4.95159199142561,4.97821944055346,
4.98204503443158,4.98438633471492,4.98621324155,4.98819933261065,4.99137447244364,
5.00179405488996,5.0699426278857,5.20808369035609,5.38527053225892,5.41042425222849,
5.41983366614312,5.4265826832077,5.43375681758525,5.44333431888808,5.46484765121972,
5.57996216820587,5.65479128536492,5.68869329771623,5.73185275959319,5.73849672794218,
5.74245231441446,5.74548616777338,5.74873600157766,5.75390634089256,5.77397816222956,
5.9814355572245,6.03130896745828,6.04346455190079,6.05046246516573,6.05584844879478,
6.06285039165623,6.07537423077362,6.14409384998325,6.3143969172455,6.43792305260728,
6.49673122735505,6.50220387745475,6.50488943595653,6.50681843702397,6.50886097308644,
6.51155774593098,6.51739639911708,6.67750525198442,6.75865006920376,6.89476115433202,
6.90322521459539,6.90626100808863,6.90837198088078,6.91032816189779,6.91293558776614,
6.91750399557843,6.92334613241918,7.03760266100932,7.14477910103911,7.31377547487298,
7.32453049265749,7.3268329729917,7.32831102657186,7.32948635398314,7.33080664183205,
7.33301424739902,7.34160235404719,7.40612517014378,7.52037669269505,7.70645039252268,
7.71776743304887,7.72138315458545,7.72337090328877,7.7253562990838,7.72774439402465,
7.73223030956566,7.73783892352537,7.8511828877305,7.97573271879192,8.11408627778447,
8.12309130145391,8.12535733731279,8.1266560321319,8.1277591296147,8.12910190027674,
8.131596215513,8.14493282113219,8.17178604713191,8.21687010570135,8.32019641079246,
8.43758484663809,8.47763935982405,8.54000493457614,8.54587143447741,8.5486928051518,
8.55069064155522,8.55257070465912,8.55457441209143,8.55877803393305,8.5769646127124,
8.60965389586113,8.70652660861874,8.92702254732146,8.9398724682088,8.94335730855871,
8.94539640540007,8.94713553048431,8.94926158894222,8.95323946597728,8.97533210932884,
9.02327082979482,9.17751427222401,9.3061983178575,9.31830290047008,9.32364829341486,
9.32750853216207,9.33151186440182,9.33736322491477,9.35294285029365,9.4268301021248,
9.53506249341463,9.62862823160764,9.64585991443363,9.65710552521339,9.66278829823707,
9.68703810663649,9.69098875590284,9.69297352937588,9.69451972221765,9.69622400684683,
9.698999900928,9.70856667948123,9.77139261896573,9.95633438646292),
 .UNSPECIFIED.);
#3553=B_SPLINE_CURVE_WITH_KNOTS('',3,(#223666,#223667,#223668,#223669,#223670,
#223671,#223672,#223673,#223674,#223675,#223676,#223677,#223678,#223679,
#223680,#223681,#223682,#223683),.UNSPECIFIED.,.F.,.F.,(4,2,2,2,2,2,2,2,
4),(221.03513445743,221.870051369324,222.704968281219,223.539885193114,
224.374802105009,225.209719016904,226.044635928798,226.879552840693,227.318319764609),
 .UNSPECIFIED.);
#3554=B_SPLINE_CURVE_WITH_KNOTS('',3,(#223685,#223686,#223687,#223688,#223689,
#223690,#223691,#223692,#223693,#223694,#223695,#223696,#223697,#223698,
#223699,#223700,#223701,#223702,#223703,#223704,#223705,#223706,#223707,
#223708,#223709,#223710,#223711,#223712,#223713,#223714,#223715,#223716,
#223717,#223718,#223719,#223720,#223721,#223722,#223723,#223724,#223725,
#223726,#223727,#223728,#223729,#223730,#223731,#223732,#223733,#223734,
#223735,#223736,#223737,#223738,#223739,#223740,#223741,#223742,#223743,
#223744,#223745,#223746,#223747,#223748,#223749,#223750,#223751,#223752,
#223753,#223754,#223755,#223756,#223757,#223758,#223759,#223760,#223761,
#223762,#223763,#223764,#223765,#223766,#223767,#223768,#223769,#223770,
#223771,#223772,#223773,#223774,#223775,#223776,#223777,#223778,#223779,
#223780,#223781,#223782,#223783,#223784,#223785,#223786,#223787,#223788,
#223789,#223790,#223791,#223792,#223793,#223794,#223795,#223796,#223797,
#223798,#223799,#223800,#223801,#223802,#223803,#223804,#223805,#223806,
#223807,#223808,#223809,#223810,#223811,#223812,#223813,#223814,#223815,
#223816,#223817,#223818,#223819,#223820,#223821,#223822,#223823,#223824,
#223825,#223826,#223827,#223828,#223829,#223830,#223831,#223832,#223833,
#223834,#223835,#223836,#223837,#223838,#223839,#223840,#223841,#223842,
#223843,#223844,#223845,#223846,#223847,#223848,#223849,#223850,#223851,
#223852,#223853,#223854,#223855,#223856,#223857,#223858,#223859,#223860,
#223861,#223862,#223863,#223864,#223865,#223866,#223867,#223868,#223869,
#223870,#223871,#223872,#223873,#223874,#223875,#223876,#223877,#223878,
#223879,#223880,#223881,#223882,#223883,#223884,#223885,#223886,#223887,
#223888,#223889,#223890,#223891,#223892,#223893,#223894,#223895,#223896,
#223897,#223898,#223899,#223900,#223901,#223902,#223903,#223904,#223905,
#223906,#223907,#223908,#223909,#223910,#223911,#223912,#223913,#223914,
#223915,#223916,#223917,#223918,#223919,#223920,#223921,#223922,#223923,
#223924,#223925,#223926,#223927,#223928,#223929,#223930,#223931,#223932,
#223933,#223934,#223935,#223936,#223937,#223938,#223939,#223940,#223941,
#223942,#223943,#223944,#223945,#223946,#223947,#223948,#223949,#223950,
#223951,#223952,#223953,#223954,#223955,#223956,#223957,#223958,#223959,
#223960,#223961,#223962,#223963,#223964,#223965,#223966,#223967,#223968,
#223969,#223970,#223971,#223972,#223973,#223974,#223975,#223976,#223977,
#223978,#223979,#223980,#223981,#223982,#223983,#223984,#223985,#223986,
#223987,#223988,#223989,#223990,#223991,#223992,#223993,#223994,#223995,
#223996,#223997,#223998,#223999,#224000,#224001,#224002,#224003,#224004,
#224005,#224006,#224007,#224008,#224009,#224010,#224011,#224012,#224013,
#224014,#224015,#224016,#224017,#224018,#224019,#224020,#224021,#224022,
#224023,#224024,#224025,#224026,#224027,#224028,#224029,#224030,#224031,
#224032,#224033,#224034,#224035,#224036,#224037,#224038,#224039,#224040,
#224041,#224042,#224043,#224044,#224045,#224046,#224047,#224048,#224049,
#224050,#224051,#224052,#224053,#224054,#224055,#224056,#224057,#224058,
#224059,#224060,#224061,#224062,#224063,#224064,#224065,#224066,#224067,
#224068,#224069,#224070,#224071,#224072,#224073,#224074,#224075,#224076,
#224077,#224078,#224079,#224080,#224081,#224082,#224083,#224084,#224085,
#224086,#224087,#224088,#224089,#224090,#224091,#224092,#224093,#224094,
#224095,#224096,#224097,#224098,#224099,#224100,#224101,#224102,#224103,
#224104,#224105,#224106,#224107,#224108,#224109,#224110,#224111,#224112,
#224113,#224114,#224115,#224116,#224117,#224118,#224119,#224120,#224121,
#224122,#224123,#224124,#224125,#224126,#224127,#224128,#224129,#224130,
#224131,#224132,#224133,#224134,#224135,#224136,#224137,#224138,#224139,
#224140,#224141,#224142,#224143,#224144,#224145,#224146,#224147,#224148,
#224149,#224150,#224151,#224152,#224153,#224154,#224155,#224156,#224157,
#224158,#224159,#224160,#224161,#224162,#224163,#224164,#224165,#224166,
#224167,#224168,#224169,#224170,#224171,#224172,#224173,#224174,#224175,
#224176,#224177,#224178,#224179,#224180,#224181,#224182,#224183,#224184,
#224185,#224186,#224187,#224188,#224189,#224190,#224191,#224192,#224193,
#224194,#224195,#224196,#224197,#224198,#224199,#224200,#224201,#224202,
#224203,#224204,#224205,#224206,#224207,#224208,#224209,#224210,#224211,
#224212,#224213,#224214,#224215,#224216,#224217,#224218,#224219,#224220,
#224221,#224222),.UNSPECIFIED.,.F.,.F.,(4,2,2,2,2,2,2,2,2,2,2,2,2,2,2,2,
2,2,2,2,2,2,2,2,2,2,2,2,2,2,2,2,2,2,2,2,2,2,2,2,2,2,2,2,2,2,2,2,2,2,2,2,
2,2,2,2,2,2,2,2,2,2,2,2,2,2,2,2,2,2,2,2,2,2,2,2,2,2,2,2,2,2,2,2,2,2,2,2,
2,2,2,2,2,2,2,2,2,2,2,2,2,2,2,2,2,2,2,2,2,2,2,2,2,2,2,2,2,2,2,2,2,2,2,2,
2,2,2,2,2,2,2,2,2,2,2,2,2,2,2,2,2,2,2,2,2,2,2,2,2,2,2,2,2,2,2,2,2,2,2,2,
2,2,2,2,2,2,2,2,2,2,2,2,2,2,2,2,2,2,2,2,2,2,2,2,2,2,2,2,2,2,2,2,2,2,2,2,
2,2,2,2,2,2,2,2,2,2,2,2,2,2,2,2,2,2,2,2,2,2,2,2,2,2,2,2,2,2,2,2,2,2,2,2,
2,2,2,2,2,2,2,2,2,2,2,2,2,2,2,2,2,2,2,2,2,2,2,2,2,2,2,2,2,2,2,2,2,2,2,2,
4),(0.00178360762374811,0.0736416897494022,0.280704762209549,0.294847251336195,
0.298018590754599,0.299811024405146,0.301192311175473,0.302748746647271,
0.305638356977403,0.31513399396247,0.455386698910708,0.500470124117633,
0.53975750666081,0.552003339287543,0.617577443491403,0.702478195068584,
0.708871301398597,0.711855620784236,0.714128620099592,0.716283576240149,
0.719296309366565,0.725463656407434,0.786247841157901,0.909477002392962,
0.968821161715167,1.02765063337858,1.12112766540002,1.12678639674282,1.12929415694603,
1.13115110306628,1.13287419573746,1.1352251344067,1.14107732993314,1.24082199303932,
1.39233488144518,1.48237708782175,1.54803643164556,1.56237107849847,1.56933971001752,
1.57644308820018,1.58461391499729,1.59857291468339,1.65332873119535,1.73312865494947,
1.83842567941408,1.87710508084618,1.88375186659346,1.88678289825031,1.88985952749663,
1.89275838744855,1.89679012052627,1.90852613144818,2.0643159495406,2.16143619777806,
2.18252216858226,2.19114626542794,2.19720987110186,2.20336684917722,2.21226410157583,
2.23457056351268,2.45090867448738,2.53144339999366,2.60206623812774,2.64296605667699,
2.64808616527274,2.65064380431516,2.65247956552519,2.65441984414856,2.65714235344626,
2.6643365673102,2.76574706790368,2.87912583703883,2.97911274856601,3.04192368600478,
3.0487579700802,3.05175610291892,3.05396369446428,3.05600237630447,3.05876841272881,
3.06557451953596,3.13631678757094,3.19054509817067,3.36545170144217,3.42221009471864,
3.45203128295713,3.4687124366621,3.47146286301705,3.47290177434407,3.47396120438062,
3.47510605069817,3.47675459188173,3.48145031775249,3.55916435810003,3.57179704511197,
3.5718481661994,3.57195307728899,3.57216179615365,3.57255335310267,3.57322000969604,
3.57421922007048,3.57554008060686,3.57712951241453,3.57893770370976,3.58096143035843,
3.71064831303396,3.78977211014492,3.8575104584985,3.86389324574107,3.86666455148945,
3.86869394590888,3.87056020058093,3.87308030169292,3.87922155834318,3.93972948997708,
4.14486254416908,4.20490079137044,4.24866398478748,4.26683150647065,4.26949809266037,
4.27086654396646,4.27198121352722,4.27326317744398,4.27542433269413,4.28310280982966,
4.4051648529001,4.57048717128833,4.67360405628189,4.6886572772091,4.6926100711883,
4.69495436119641,4.69702927609223,4.69962307313635,4.70363322164583,4.721932836118,
4.97980010703783,5.07962937050696,5.08622954481,5.08865289916885,5.09035601560706,
5.09194812364498,5.09413575088398,5.09840537651871,5.12743622900781,5.20275215386603,
5.3923091299888,5.45382923546852,5.46424974522926,5.4692295743262,5.47307642985705,
5.47729018828258,5.48410946430728,5.50748062234046,5.73211654119411,5.82971214580383,
5.83520471469364,5.83728016654339,5.83875761614752,5.84015472376008,5.84209932536465,
5.84598634903332,5.88032486338937,5.91637986209933,6.07590018220587,6.23590983347248,
6.24595720324807,6.24966355772437,6.25183656845789,6.25387566667094,6.25668925849661,
6.26222351088608,6.30128005557024,6.39663853102738,6.47831245960531,6.56882542353529,
6.65873728826974,6.66510252912432,6.66753909467498,6.66928457521318,6.67094337565561,
6.67326612782538,6.6779585529885,6.71744729032768,6.79209341809599,6.90977659843109,
7.02932697906653,7.08700850453278,7.10124953606111,7.10951043017779,7.11604987782794,
7.12478871562823,7.14027018361526,7.23233614079705,7.34555775417832,7.41382540140005,
7.42179901554951,7.42570676631063,7.42858182150987,7.43140806069661,7.43608548496645,
7.45052510571772,7.55246393419507,7.69854678042963,7.72044328951425,7.7285645046275,
7.73432868890056,7.74038743963821,7.74833780618792,7.76460761032734,7.91920597578543,
8.14824602837285,8.15749081604834,8.17237111205729,8.18446240003284,8.18820665725569,
8.19024281711461,8.19226190773564,8.19467181496988,8.19913722572664,8.20464093928975,
8.21612682960537,8.24632908749532,8.33565772522918,8.53046241093476,8.58188516983021,
8.58817007197953,8.59081921520617,8.59303018631877,8.59529988927096,8.59861765181704,
8.60739464823482,8.724561640462,8.87406841694435,8.914689766971,8.99114143558169,
9.00762108396818,9.0102825434955,9.01185219694736,9.01304377176556,9.01430678338724,
9.01558831328976,9.01741767249102,9.03134090334122,9.05987685738208,9.11420116947001,
9.15958271476645,9.38623529217457,9.40082711705873,9.40476995133339,9.40707442666774,
9.40905742910072,9.41146469538596,9.41598526871393,9.44139210831433,9.48883454267792,
9.58786856279916,9.62624751959209,9.64524310642237,9.66586810206775,9.74998235635441,
9.7589094337966,9.80434768099741,9.80801623936946,9.80945788783498,9.81051103350733,
9.81164639673706,9.81317896332834,9.81486699567909,9.81773313255874,9.9564473454049),
 .UNSPECIFIED.);
#3555=B_SPLINE_CURVE_WITH_KNOTS('',3,(#224224,#224225,#224226,#224227,#224228,
#224229,#224230,#224231,#224232,#224233,#224234,#224235,#224236,#224237,
#224238,#224239,#224240,#224241,#224242,#224243,#224244,#224245,#224246,
#224247,#224248,#224249,#224250,#224251,#224252,#224253,#224254,#224255,
#224256,#224257,#224258,#224259,#224260,#224261,#224262,#224263,#224264,
#224265,#224266,#224267,#224268,#224269,#224270,#224271,#224272,#224273,
#224274,#224275,#224276,#224277,#224278,#224279,#224280,#224281,#224282,
#224283,#224284,#224285,#224286,#224287,#224288,#224289,#224290,#224291,
#224292,#224293,#224294,#224295,#224296,#224297,#224298,#224299,#224300,
#224301,#224302,#224303,#224304,#224305,#224306,#224307,#224308,#224309,
#224310,#224311,#224312,#224313,#224314,#224315,#224316,#224317,#224318,
#224319,#224320,#224321,#224322,#224323,#224324,#224325,#224326,#224327,
#224328,#224329,#224330,#224331,#224332,#224333,#224334,#224335,#224336,
#224337,#224338,#224339,#224340,#224341,#224342,#224343,#224344,#224345,
#224346,#224347,#224348,#224349,#224350,#224351,#224352,#224353,#224354,
#224355,#224356,#224357,#224358,#224359,#224360,#224361,#224362,#224363,
#224364,#224365,#224366,#224367,#224368,#224369,#224370,#224371,#224372,
#224373,#224374,#224375,#224376,#224377,#224378,#224379,#224380,#224381,
#224382,#224383,#224384,#224385,#224386,#224387,#224388,#224389,#224390,
#224391,#224392,#224393,#224394,#224395,#224396,#224397,#224398,#224399,
#224400,#224401,#224402,#224403,#224404,#224405,#224406,#224407,#224408,
#224409,#224410,#224411,#224412,#224413,#224414,#224415,#224416,#224417,
#224418,#224419,#224420,#224421,#224422,#224423,#224424,#224425,#224426,
#224427,#224428,#224429,#224430,#224431,#224432,#224433,#224434,#224435,
#224436,#224437,#224438,#224439,#224440,#224441,#224442,#224443,#224444,
#224445,#224446,#224447,#224448,#224449,#224450,#224451,#224452,#224453,
#224454,#224455,#224456,#224457,#224458,#224459,#224460,#224461,#224462,
#224463,#224464,#224465,#224466,#224467,#224468,#224469,#224470,#224471,
#224472,#224473,#224474,#224475,#224476,#224477,#224478,#224479,#224480,
#224481,#224482),.UNSPECIFIED.,.F.,.F.,(4,3,3,3,3,3,3,3,3,3,3,3,3,3,3,3,
3,3,3,3,3,3,3,3,3,3,3,3,3,3,3,3,3,3,3,3,3,3,3,3,3,3,3,3,3,3,3,3,3,3,3,3,
3,3,3,3,3,3,3,3,3,3,3,3,3,3,3,3,3,3,3,3,3,3,3,3,3,3,3,3,3,3,3,3,3,3,4),
(239.884690378968,239.957555113344,240.03035368128,240.103101051101,240.177247962562,
240.249945830814,240.322640540092,240.39534554821,240.470578246854,240.54337728036,
240.619826811573,240.696276342786,240.77727032217,240.858147360236,240.942522072856,
241.023080466785,241.103515008765,241.183774426348,241.195646210717,241.270050513933,
241.344471584734,241.418921696184,241.493453731457,241.568030171724,241.642711118493,
241.695016078648,241.771587622015,241.848091514626,241.924538709216,242.000940118241,
242.077306621218,242.15436277038,242.230700160461,242.307037031759,242.383383239976,
242.46097638361,242.53739549535,242.615575654931,242.693755814511,242.767532905335,
242.841247682769,242.914913217055,242.988543362142,243.062151985947,243.135764803752,
243.193125682442,243.274559213523,243.356128208519,243.440220043982,243.522062750477,
243.607279150425,243.692495550373,243.77092849387,243.849291677751,243.927589943029,
244.005809208886,244.083978500391,244.162089825479,244.191865418304,244.268227889387,
244.344607215469,244.42101298111,244.497487653202,244.57399970093,244.650594030156,
244.691235286235,244.766612665172,244.841928498572,244.917195608182,244.992426783265,
245.067634788409,245.14542731762,245.220645493803,245.295880369381,245.371143512926,
245.44644650627,245.521838702226,245.597283601575,245.672826962675,245.689975022097,
245.767187134031,245.844261924242,245.925165364718,246.001941919313,246.078621149182,
246.155182952082,246.167875686148),.UNSPECIFIED.);
#3556=B_SPLINE_CURVE_WITH_KNOTS('',3,(#224484,#224485,#224486,#224487,#224488,
#224489,#224490,#224491,#224492,#224493,#224494,#224495,#224496,#224497,
#224498,#224499,#224500,#224501,#224502,#224503,#224504,#224505,#224506,
#224507,#224508,#224509,#224510,#224511,#224512,#224513,#224514,#224515,
#224516,#224517,#224518,#224519,#224520,#224521,#224522,#224523,#224524,
#224525,#224526,#224527,#224528,#224529,#224530,#224531,#224532,#224533,
#224534,#224535,#224536,#224537,#224538,#224539,#224540,#224541,#224542,
#224543,#224544,#224545,#224546,#224547,#224548,#224549,#224550,#224551,
#224552,#224553,#224554,#224555,#224556,#224557,#224558,#224559,#224560,
#224561,#224562,#224563,#224564,#224565,#224566,#224567,#224568,#224569,
#224570,#224571,#224572,#224573,#224574,#224575,#224576,#224577,#224578,
#224579,#224580,#224581,#224582,#224583,#224584,#224585,#224586,#224587,
#224588,#224589,#224590,#224591,#224592,#224593,#224594,#224595,#224596,
#224597,#224598,#224599,#224600,#224601,#224602,#224603,#224604,#224605,
#224606,#224607,#224608,#224609,#224610,#224611,#224612,#224613,#224614,
#224615,#224616,#224617,#224618,#224619,#224620,#224621,#224622,#224623,
#224624,#224625,#224626,#224627,#224628,#224629,#224630,#224631,#224632,
#224633,#224634,#224635,#224636,#224637,#224638,#224639,#224640,#224641,
#224642,#224643,#224644,#224645,#224646,#224647,#224648,#224649,#224650,
#224651,#224652,#224653,#224654,#224655,#224656,#224657,#224658,#224659,
#224660,#224661,#224662,#224663,#224664,#224665,#224666,#224667,#224668,
#224669,#224670,#224671,#224672,#224673,#224674,#224675,#224676,#224677,
#224678,#224679,#224680,#224681,#224682,#224683,#224684,#224685,#224686,
#224687,#224688,#224689,#224690,#224691,#224692,#224693,#224694,#224695,
#224696,#224697,#224698,#224699,#224700,#224701,#224702,#224703,#224704,
#224705,#224706,#224707,#224708,#224709,#224710,#224711,#224712,#224713,
#224714,#224715,#224716,#224717,#224718,#224719,#224720,#224721,#224722,
#224723,#224724,#224725,#224726,#224727,#224728,#224729,#224730,#224731,
#224732,#224733,#224734,#224735,#224736,#224737,#224738,#224739,#224740,
#224741,#224742,#224743,#224744,#224745,#224746,#224747,#224748,#224749,
#224750,#224751,#224752,#224753,#224754,#224755,#224756,#224757,#224758,
#224759,#224760,#224761,#224762,#224763,#224764,#224765,#224766,#224767,
#224768,#224769,#224770,#224771,#224772,#224773,#224774,#224775,#224776,
#224777,#224778,#224779,#224780,#224781,#224782,#224783,#224784,#224785,
#224786,#224787,#224788,#224789,#224790,#224791,#224792,#224793,#224794,
#224795,#224796,#224797,#224798,#224799,#224800,#224801,#224802,#224803,
#224804,#224805,#224806,#224807,#224808,#224809,#224810,#224811,#224812,
#224813,#224814,#224815,#224816,#224817,#224818,#224819,#224820,#224821,
#224822,#224823,#224824,#224825,#224826,#224827,#224828,#224829,#224830,
#224831,#224832,#224833,#224834,#224835,#224836,#224837,#224838,#224839,
#224840,#224841,#224842,#224843,#224844,#224845,#224846,#224847,#224848,
#224849,#224850,#224851,#224852,#224853,#224854,#224855,#224856,#224857,
#224858,#224859,#224860,#224861,#224862,#224863,#224864,#224865,#224866,
#224867,#224868,#224869,#224870,#224871,#224872,#224873,#224874,#224875,
#224876,#224877,#224878,#224879,#224880,#224881,#224882,#224883,#224884,
#224885,#224886,#224887,#224888,#224889,#224890,#224891,#224892,#224893,
#224894,#224895,#224896,#224897,#224898,#224899,#224900,#224901,#224902,
#224903,#224904,#224905,#224906,#224907,#224908,#224909,#224910,#224911,
#224912,#224913,#224914,#224915,#224916,#224917,#224918,#224919,#224920,
#224921,#224922,#224923,#224924,#224925,#224926,#224927,#224928,#224929,
#224930,#224931,#224932,#224933,#224934,#224935,#224936,#224937,#224938,
#224939,#224940,#224941,#224942,#224943,#224944,#224945,#224946,#224947,
#224948,#224949,#224950,#224951,#224952,#224953,#224954,#224955,#224956,
#224957,#224958,#224959,#224960,#224961,#224962,#224963,#224964,#224965,
#224966,#224967,#224968,#224969,#224970,#224971,#224972,#224973,#224974,
#224975,#224976,#224977,#224978,#224979,#224980,#224981,#224982,#224983,
#224984,#224985,#224986,#224987,#224988,#224989,#224990,#224991,#224992,
#224993,#224994,#224995,#224996,#224997,#224998,#224999,#225000,#225001,
#225002,#225003,#225004,#225005,#225006,#225007,#225008,#225009,#225010,
#225011,#225012,#225013,#225014,#225015,#225016,#225017),.UNSPECIFIED.,
 .F.,.F.,(4,2,2,2,2,2,2,2,2,2,2,2,2,2,2,2,2,2,2,2,2,2,2,2,2,2,2,2,2,2,2,
2,2,2,2,2,2,2,2,2,2,2,2,2,2,2,2,2,2,2,2,2,2,2,2,2,2,2,2,2,2,2,2,2,2,2,2,
2,2,2,2,2,2,2,2,2,2,2,2,2,2,2,2,2,2,2,2,2,2,2,2,2,2,2,2,2,2,2,2,2,2,2,2,
2,2,2,2,2,2,2,2,2,2,2,2,2,2,2,2,2,2,2,2,2,2,2,2,2,2,2,2,2,2,2,2,2,2,2,2,
2,2,2,2,2,2,2,2,2,2,2,2,2,2,2,2,2,2,2,2,2,2,2,2,2,2,2,2,2,2,2,2,2,2,2,2,
2,2,2,2,2,2,2,2,2,2,2,2,2,2,2,2,2,2,2,2,2,2,2,2,2,2,2,2,2,2,2,2,2,2,2,2,
2,2,2,2,2,2,2,2,2,2,2,2,2,2,2,2,2,2,2,2,2,2,2,2,2,2,2,2,2,2,2,2,2,2,2,2,
2,2,2,2,2,2,2,2,2,2,2,2,2,2,2,2,2,2,2,4),(0.00147305716892635,0.00749381998220008,
0.00989642461442405,0.0118079829048873,0.0137693260591038,0.0157355795135307,
0.0192465931573194,0.0297741239825986,0.0873493969891357,0.309696769649157,
0.386917603875351,0.411215935545746,0.41406333181997,0.415467841926669,
0.416480171622895,0.417554622416341,0.419069926507322,0.423112408404172,
0.484956706463286,0.494114742432427,0.515694312418917,0.731820880505203,
0.795121819518333,0.819069490393267,0.82856580696502,0.835511048725812,
0.838441313161028,0.840389133113309,0.842509999797709,0.845062003771217,
0.851412094911848,0.908480833484355,1.01255981481909,1.07729625381323,1.09665701093856,
1.15800091991536,1.20518863666577,1.22785370565823,1.23186240982777,1.23399511384717,
1.23575109661907,1.23752561776291,1.24079921845053,1.25143549274712,1.44446835282154,
1.52631919617496,1.59140646865762,1.60633110121011,1.61213071029591,1.61612296278743,
1.61999114752965,1.6247405785079,1.63588042157662,1.75650378644571,1.96383091052599,
1.97757903204481,1.9807217713994,1.98250785869409,1.98388888945621,1.98568650492903,
1.98879629180428,2.00082420528186,2.19385017145956,2.37693435446593,2.38535666134309,
2.39175036815653,2.39472265470329,2.39686584859117,2.39898135547327,2.4018438854827,
2.40741769515225,2.44979529423293,2.71343498761884,2.73079416994145,2.79736966063391,
2.80854519227524,2.81181812812695,2.81383515324019,2.81567037544692,2.81803395408874,
2.82276617905866,2.8529980196032,2.8612867076133,2.86643381522325,2.98856451763317,
3.1253986752823,3.22601978175105,3.24358587827009,3.25253770714906,3.25909387800418,
3.2661827112549,3.27864194095808,3.31591120605247,3.36710649550511,3.50600031282143,
3.55980969685452,3.56715564594322,3.57092583504954,3.57396604147693,3.57698479251259,
3.58249521420504,3.60296082659404,3.81093646320781,3.85994105138886,3.87160176412624,
3.87842203111497,3.884427704769,3.89192636976483,3.90360007035288,3.97143062851463,
3.97495143564316,3.97649115815609,4.04749999433727,4.06453889821016,4.23757604590462,
4.30596485869173,4.32785746101088,4.33223244725983,4.3346335189519,4.33645174296798,
4.33876671198754,4.34264894769786,4.35627818914582,4.59536721964481,4.69232564877964,
4.72834126061973,4.73361316043832,4.73630940619206,4.73826990626417,4.74036522290009,
4.74395416352845,4.75376908552651,4.90099425833841,4.98010012222836,5.1432563160117,
5.15325930909398,5.15550211296467,5.15696161288984,5.15813521677076,5.15946756770922,
5.16172910941596,5.17098096162955,5.24955585341429,5.42261552657406,5.46667333789819,
5.54137372597943,5.54785422847531,5.55043319534066,5.5523145168499,5.55433317357092,
5.55704228381609,5.56308101046833,5.70276588390827,5.73979259404873,5.77866701934748,
5.92017758878054,5.92576743604786,5.95009656844959,5.95294779902459,5.95437691929121,
5.95542707054886,5.95656490125618,5.95811088801615,5.96163614965713,6.08759608074564,
6.21357425203831,6.36308707052553,6.37341486535841,6.37698732961625,6.37902046657422,
6.38089018312365,6.38341217754772,6.38817720967175,6.41570960466292,6.4475385025929,
6.54687493552076,6.65192631687319,6.76096093250478,6.76886610722654,6.77193070183781,
6.77366200021271,6.77524670633711,6.77732982332109,6.78116610887155,6.78596506843429,
6.88663246451514,7.07183470096642,7.1368856175419,7.14748150659527,7.15244180554368,
7.15629671311951,7.1604781225499,7.16715520691697,7.18921223266523,7.3206039620109,
7.5078200116614,7.51713309276275,7.51999759696788,7.52154940649921,7.52308437729133,
7.52491028987963,7.52817254726477,7.53223476950029,7.6723361719209,7.81595939317523,
7.86455457435632,7.92357175312076,7.93028064328713,7.93306510614329,7.93537081646518,
7.93771924807057,7.94111852466097,7.94992391280861,8.0591076782085,8.0887611135404,
8.13812776786223,8.28657640163204,8.34325019165643,8.34861018147624,8.35103600423687,
8.35288627887708,8.35459858201271,8.3573808967227,8.36455599852038,8.37507745287341,
8.40518381527544,8.53002490562667,8.74637300487212,8.77406955171921,8.78624194839587,
8.79327693428413,8.80058211049047,8.81005414500892,8.82028986324185,8.88235743277589,
8.93346645511187,8.97046170487788,9.02146462883256,9.09666097922066,9.10471071642131,
9.10863262926514,9.11162336737462,9.11491326618468,9.12009970791608,9.13990783198821,
9.17654704045082,9.29281063685616,9.35066906214817,9.39724906810497,9.40911411238741,
9.41604832099134,9.42204197529525,9.42938193625996,9.44349784483151,9.51429789004961,
9.64979844535283,9.76391586292631,9.77979063864637,9.86249121300546,9.86826121530637,
9.87102118310009,9.8729717211139,9.87492256942972,9.87688418705653,9.87939211661189,
9.88325415979244,9.9567376273315),.UNSPECIFIED.);
#3557=B_SPLINE_CURVE_WITH_KNOTS('',3,(#225019,#225020,#225021,#225022,#225023,
#225024,#225025,#225026,#225027,#225028,#225029,#225030),.UNSPECIFIED.,
 .F.,.F.,(4,1,1,1,1,1,1,1,1,4),(258.73438144831,259.672331324168,260.67107106003,
261.669810795892,262.169180663823,262.668550531754,263.667290267616,264.166660135548,
264.666030003479,265.017431607686),.UNSPECIFIED.);
#3558=B_SPLINE_CURVE_WITH_KNOTS('',3,(#225032,#225033,#225034,#225035,#225036,
#225037,#225038,#225039,#225040,#225041,#225042,#225043,#225044,#225045,
#225046,#225047,#225048,#225049,#225050,#225051,#225052,#225053,#225054,
#225055,#225056,#225057,#225058,#225059,#225060,#225061,#225062,#225063,
#225064,#225065,#225066,#225067,#225068,#225069,#225070,#225071,#225072,
#225073,#225074,#225075,#225076,#225077,#225078,#225079,#225080,#225081,
#225082,#225083,#225084,#225085,#225086,#225087,#225088,#225089,#225090,
#225091,#225092,#225093,#225094,#225095,#225096,#225097,#225098,#225099,
#225100,#225101,#225102,#225103,#225104,#225105,#225106,#225107,#225108,
#225109,#225110,#225111,#225112,#225113,#225114,#225115,#225116,#225117,
#225118,#225119,#225120,#225121,#225122,#225123,#225124,#225125,#225126,
#225127,#225128,#225129,#225130,#225131,#225132,#225133,#225134,#225135,
#225136,#225137,#225138,#225139,#225140,#225141,#225142,#225143,#225144,
#225145,#225146,#225147,#225148,#225149,#225150,#225151,#225152,#225153,
#225154,#225155,#225156,#225157,#225158,#225159,#225160,#225161,#225162,
#225163,#225164,#225165,#225166,#225167,#225168,#225169,#225170,#225171,
#225172,#225173,#225174,#225175,#225176,#225177,#225178,#225179,#225180,
#225181,#225182,#225183,#225184,#225185,#225186,#225187,#225188,#225189,
#225190,#225191,#225192,#225193,#225194,#225195,#225196,#225197,#225198,
#225199,#225200,#225201,#225202,#225203,#225204,#225205,#225206,#225207,
#225208,#225209,#225210,#225211,#225212,#225213,#225214,#225215,#225216,
#225217,#225218,#225219,#225220,#225221,#225222,#225223,#225224,#225225,
#225226,#225227,#225228,#225229,#225230,#225231,#225232,#225233,#225234,
#225235,#225236,#225237,#225238,#225239,#225240,#225241,#225242,#225243,
#225244,#225245,#225246,#225247,#225248,#225249,#225250,#225251,#225252,
#225253,#225254,#225255,#225256,#225257,#225258,#225259,#225260,#225261,
#225262,#225263,#225264,#225265,#225266,#225267,#225268,#225269,#225270,
#225271,#225272,#225273,#225274,#225275,#225276,#225277,#225278,#225279,
#225280,#225281,#225282,#225283,#225284,#225285,#225286,#225287,#225288,
#225289,#225290,#225291,#225292,#225293,#225294,#225295,#225296,#225297,
#225298,#225299,#225300,#225301,#225302,#225303,#225304,#225305,#225306,
#225307,#225308,#225309,#225310,#225311,#225312,#225313,#225314,#225315,
#225316,#225317,#225318,#225319,#225320,#225321,#225322,#225323,#225324,
#225325,#225326,#225327,#225328,#225329,#225330,#225331,#225332,#225333,
#225334,#225335,#225336,#225337,#225338,#225339,#225340,#225341,#225342,
#225343,#225344,#225345,#225346,#225347,#225348,#225349,#225350,#225351,
#225352,#225353,#225354,#225355,#225356,#225357,#225358,#225359,#225360,
#225361,#225362,#225363,#225364,#225365,#225366,#225367,#225368,#225369,
#225370,#225371,#225372,#225373,#225374,#225375,#225376,#225377,#225378,
#225379,#225380,#225381,#225382,#225383,#225384,#225385,#225386,#225387,
#225388,#225389,#225390,#225391,#225392,#225393,#225394,#225395,#225396,
#225397,#225398,#225399,#225400,#225401,#225402,#225403,#225404,#225405,
#225406,#225407,#225408,#225409,#225410,#225411,#225412,#225413,#225414,
#225415,#225416,#225417,#225418,#225419,#225420,#225421,#225422,#225423,
#225424,#225425,#225426,#225427,#225428,#225429,#225430,#225431,#225432,
#225433,#225434,#225435,#225436,#225437,#225438,#225439,#225440,#225441,
#225442,#225443,#225444,#225445,#225446,#225447,#225448,#225449,#225450,
#225451,#225452,#225453,#225454,#225455,#225456,#225457,#225458,#225459,
#225460,#225461,#225462,#225463,#225464,#225465,#225466,#225467,#225468,
#225469,#225470,#225471,#225472,#225473,#225474,#225475,#225476,#225477,
#225478,#225479,#225480,#225481,#225482,#225483,#225484,#225485,#225486,
#225487,#225488,#225489,#225490,#225491,#225492,#225493,#225494,#225495,
#225496,#225497,#225498,#225499,#225500,#225501,#225502,#225503,#225504,
#225505,#225506,#225507,#225508,#225509,#225510,#225511,#225512,#225513,
#225514,#225515,#225516,#225517,#225518,#225519,#225520,#225521,#225522,
#225523,#225524,#225525,#225526,#225527,#225528,#225529,#225530,#225531,
#225532,#225533,#225534,#225535,#225536,#225537,#225538,#225539,#225540,
#225541,#225542,#225543,#225544,#225545,#225546,#225547,#225548,#225549,
#225550,#225551,#225552,#225553,#225554,#225555,#225556,#225557,#225558,
#225559),.UNSPECIFIED.,.F.,.F.,(4,2,2,2,2,2,2,2,2,2,2,2,2,2,2,2,2,2,2,2,
2,2,2,2,2,2,2,2,2,2,2,2,2,2,2,2,2,2,2,2,2,2,2,2,2,2,2,2,2,2,2,2,2,2,2,2,
2,2,2,2,2,2,2,2,2,2,2,2,2,2,2,2,2,2,2,2,2,2,2,2,2,2,2,2,2,2,2,2,2,2,2,2,
2,2,2,2,2,2,2,2,2,2,2,2,2,2,2,2,2,2,2,2,2,2,2,2,2,2,2,2,2,2,2,2,2,2,2,2,
2,2,2,2,2,2,2,2,2,2,2,2,2,2,2,2,2,2,2,2,2,2,2,2,2,2,2,2,2,2,2,2,2,2,2,2,
2,2,2,2,2,2,2,2,2,2,2,2,2,2,2,2,2,2,2,2,2,2,2,2,2,2,2,2,2,2,2,2,2,2,2,2,
2,2,2,2,2,2,2,2,2,2,2,2,2,2,2,2,2,2,2,2,2,2,2,2,2,2,2,2,2,2,2,2,2,2,2,2,
2,2,2,2,2,2,2,2,2,2,2,2,2,2,2,2,2,2,2,2,2,2,2,2,2,2,2,4),(0.0013984589909669,
0.00758538319000157,0.0138316523058583,0.0196994110499808,0.0254599733433377,
0.0312029810325234,0.0408521959009723,0.0670506220258798,0.263875818637476,
0.374604171535812,0.442494887563076,0.470980336443651,0.475686080779563,
0.478158061972327,0.480177753916977,0.482204380610581,0.485908081914892,
0.497628898150731,0.670987232608517,0.724939834278448,0.803424167889865,
0.849056130185995,0.864568053748669,0.871496288178267,0.876953491396784,
0.879688091340448,0.881654135300919,0.883734616898646,0.886658491409639,
0.892692402676658,0.954517790180003,1.06719782345678,1.15138318962781,1.18514845399419,
1.23231646350036,1.28885223140284,1.29709014176535,1.29930269250406,1.30062416518764,
1.30179943662341,1.30327593644542,1.30557097117994,1.31695230561336,1.50171553573889,
1.5938543621018,1.65834335694585,1.67763285556883,1.68561494092747,1.68976246383864,
1.69237257390772,1.69482033988358,1.6966161003335,1.6985505366644,1.70190228222598,
1.71129664884711,1.84910727268763,1.99739640916572,2.02100485290848,2.0565939400234,
2.08994215418236,2.0957540899652,2.09761686394535,2.09881621982331,2.09995044159275,
2.10144848376419,2.10480041403386,2.13297363986997,2.2876359039831,2.38723418769212,
2.47826436330779,2.51407056879355,2.51916574942751,2.52175708196898,2.5236354376741,
2.52563740670042,2.5290524710947,2.53831181011983,2.68028656066205,2.8324264657307,
2.90092423575469,2.91214135413812,2.91534425345094,2.91729956497148,2.91906631924886,
2.92132438200619,2.92578812394697,2.95256148843368,3.01423206727539,3.26243012592556,
3.27844658624767,3.29057289505769,3.29588173518521,3.29977948537614,3.30337471127242,
3.30825234064485,3.31780649178716,3.40149477966164,3.53814658106887,3.59989758903079,
3.65270955818973,3.66126772315916,3.66393161015268,3.66561063506772,3.66716358391967,
3.66916538212632,3.67345173202999,3.70998647186018,3.7721878154103,3.94430896203305,
4.06623184297491,4.07382353364534,4.0770250111134,4.07933455863342,4.08143461370161,
4.08423514208219,4.09131604185056,4.16017456317236,4.21543042597559,4.41500376306745,
4.4521538777401,4.48846673739912,4.49302679587756,4.49532275048454,4.49697849173306,
4.49873536850344,4.50171302672694,4.50969788929422,4.5558996031632,4.55818672904746,
4.56651708872552,4.57426148976264,4.77405762967652,4.86244585520452,4.89816258982957,
4.9225221813698,4.93269101177473,4.94010362094912,4.94693270702372,4.95622585494011,
4.97958641694583,5.0863155888876,5.15991929287492,5.24062255944352,5.24887205316262,
5.25282366209976,5.25588313616447,5.25923978573685,5.26475455410025,5.28896928931034,
5.33840611258749,5.49964326902273,5.54206554987833,5.553707258246,5.56052332500533,
5.56647212405472,5.57394869997153,5.58873393812068,5.71364833666406,5.9061894145442,
6.00679675291165,6.01261567146818,6.01538767008321,6.0173416800407,6.01917446491608,
6.02170233049056,6.02667548361257,6.06271202118362,6.09128764979767,6.15084395491074,
6.30478092038589,6.35053978392625,6.40815910863949,6.4140684345446,6.4169608418462,
6.41903241393073,6.42121989791487,6.42409603483496,6.43027284727676,6.51402358647735,
6.63579271745738,6.80402699030117,6.82831240965539,6.8355042153803,6.83770194046944,
6.83888820738784,6.84005890868061,6.84143348485369,6.8439713904554,6.84711217147657,
6.95303621399563,7.05646877155635,7.16537518155188,7.22353235432673,7.22910956974834,
7.23180208113871,7.23371339844825,7.23551589336713,7.23801707150799,7.2429867141531,
7.27998503378046,7.3348989053676,7.53134472478755,7.60492069071673,7.63156229589308,
7.63448822126048,7.63593585331661,7.63699054844077,7.63812500419528,7.63965183604271,
7.64300335547336,7.67947348396097,7.75067837410735,7.82415842626353,8.0390830623178,
8.05400031891449,8.05808222761089,8.06047905128405,8.06254827147825,8.06506867161196,
8.06982713453443,8.09722967526423,8.13885817957425,8.27389320604298,8.43497693338631,
8.44942197315286,8.45273607831524,8.45491005719968,8.45666809466609,8.45863456403046,
8.46194762489439,8.46595644578898,8.47398697322504,8.49476788188291,8.53902296438352,
8.76260942456012,8.81939643524981,8.82955370676513,8.83447962426361,8.83831846655862,
8.84255749072362,8.84949445072087,8.87403410273132,9.09894629367027,9.17057566260111,
9.19692712812516,9.20102682623861,9.20301373803425,9.2045597691785,9.20599530795815,
9.20845855989933,9.2152745407914,9.22522897971901,9.2552425534656,9.29861907247562,
9.59372018011532,9.60981212948134,9.61423054017918,9.61682876017148,9.61907428775765,
9.62181258414712,9.62699222677798,9.65710591683204,9.70170682036863,9.95757013430097),
 .UNSPECIFIED.);
#3559=B_SPLINE_CURVE_WITH_KNOTS('',3,(#225561,#225562,#225563,#225564,#225565,
#225566,#225567,#225568,#225569,#225570,#225571,#225572,#225573,#225574,
#225575,#225576,#225577,#225578,#225579,#225580,#225581,#225582,#225583,
#225584,#225585,#225586,#225587,#225588,#225589,#225590,#225591,#225592,
#225593,#225594,#225595,#225596,#225597,#225598,#225599,#225600,#225601,
#225602,#225603,#225604,#225605,#225606,#225607,#225608,#225609,#225610,
#225611,#225612,#225613,#225614,#225615,#225616,#225617,#225618,#225619,
#225620,#225621,#225622,#225623,#225624,#225625,#225626,#225627,#225628,
#225629,#225630,#225631,#225632,#225633,#225634,#225635,#225636,#225637,
#225638,#225639,#225640,#225641,#225642,#225643,#225644,#225645,#225646,
#225647,#225648,#225649,#225650,#225651,#225652,#225653,#225654,#225655,
#225656,#225657,#225658,#225659,#225660,#225661,#225662,#225663,#225664,
#225665,#225666,#225667,#225668,#225669,#225670,#225671,#225672,#225673,
#225674,#225675,#225676,#225677,#225678,#225679,#225680,#225681,#225682,
#225683,#225684,#225685,#225686,#225687,#225688,#225689,#225690,#225691,
#225692,#225693,#225694,#225695,#225696,#225697,#225698,#225699,#225700,
#225701,#225702,#225703,#225704,#225705,#225706,#225707,#225708,#225709,
#225710,#225711,#225712,#225713,#225714,#225715,#225716,#225717,#225718,
#225719,#225720,#225721,#225722,#225723,#225724,#225725,#225726,#225727,
#225728,#225729,#225730,#225731,#225732,#225733,#225734,#225735,#225736,
#225737,#225738,#225739,#225740,#225741,#225742,#225743,#225744,#225745,
#225746,#225747,#225748,#225749,#225750,#225751,#225752,#225753,#225754,
#225755,#225756,#225757,#225758,#225759,#225760,#225761,#225762,#225763,
#225764,#225765,#225766,#225767,#225768,#225769,#225770,#225771,#225772,
#225773,#225774,#225775,#225776,#225777,#225778,#225779,#225780,#225781,
#225782,#225783,#225784,#225785,#225786,#225787,#225788,#225789,#225790,
#225791,#225792,#225793,#225794,#225795,#225796,#225797,#225798,#225799,
#225800,#225801,#225802,#225803,#225804,#225805,#225806,#225807,#225808,
#225809,#225810,#225811,#225812,#225813,#225814,#225815,#225816,#225817,
#225818,#225819,#225820,#225821,#225822,#225823,#225824,#225825,#225826,
#225827,#225828,#225829,#225830,#225831,#225832,#225833,#225834,#225835,
#225836,#225837,#225838,#225839,#225840,#225841,#225842,#225843,#225844,
#225845,#225846,#225847,#225848,#225849,#225850,#225851,#225852,#225853,
#225854,#225855,#225856,#225857,#225858,#225859,#225860,#225861,#225862,
#225863,#225864,#225865,#225866,#225867,#225868,#225869,#225870,#225871,
#225872,#225873,#225874,#225875,#225876,#225877,#225878,#225879,#225880,
#225881,#225882,#225883,#225884,#225885,#225886,#225887,#225888,#225889,
#225890,#225891,#225892,#225893,#225894,#225895,#225896,#225897,#225898,
#225899,#225900,#225901,#225902,#225903,#225904,#225905,#225906,#225907,
#225908,#225909,#225910,#225911,#225912,#225913,#225914,#225915,#225916,
#225917,#225918,#225919,#225920,#225921,#225922,#225923,#225924,#225925,
#225926,#225927,#225928,#225929,#225930,#225931,#225932,#225933,#225934,
#225935,#225936,#225937,#225938,#225939,#225940,#225941,#225942,#225943,
#225944,#225945,#225946,#225947,#225948,#225949,#225950,#225951,#225952,
#225953,#225954,#225955,#225956,#225957,#225958,#225959,#225960,#225961,
#225962,#225963,#225964,#225965,#225966,#225967,#225968,#225969,#225970,
#225971,#225972,#225973,#225974,#225975,#225976,#225977,#225978,#225979,
#225980,#225981,#225982,#225983,#225984,#225985,#225986,#225987,#225988,
#225989,#225990,#225991,#225992,#225993,#225994,#225995,#225996,#225997,
#225998,#225999,#226000,#226001,#226002,#226003,#226004,#226005,#226006,
#226007,#226008,#226009,#226010,#226011,#226012,#226013,#226014,#226015,
#226016,#226017,#226018,#226019,#226020,#226021,#226022,#226023,#226024,
#226025,#226026,#226027,#226028,#226029,#226030,#226031,#226032,#226033,
#226034,#226035,#226036,#226037,#226038,#226039,#226040,#226041,#226042,
#226043,#226044,#226045,#226046,#226047,#226048,#226049,#226050,#226051,
#226052,#226053,#226054,#226055,#226056,#226057,#226058,#226059,#226060,
#226061,#226062,#226063,#226064,#226065,#226066,#226067,#226068,#226069,
#226070,#226071,#226072,#226073,#226074,#226075,#226076,#226077,#226078,
#226079,#226080,#226081,#226082,#226083,#226084),.UNSPECIFIED.,.F.,.F.,
(4,2,2,2,2,2,2,2,2,2,2,2,2,2,2,2,2,2,2,2,2,2,2,2,2,2,2,2,2,2,2,2,2,2,2,
2,2,2,2,2,2,2,2,2,2,2,2,2,2,2,2,2,2,2,2,2,2,2,2,2,2,2,2,2,2,2,2,2,2,2,2,
2,2,2,2,2,2,2,2,2,2,2,2,2,2,2,2,2,2,2,2,2,2,2,2,2,2,2,2,2,2,2,2,2,2,2,2,
2,2,2,2,2,2,2,2,2,2,2,2,2,2,2,2,2,2,2,2,2,2,2,2,2,2,2,2,2,2,2,2,2,2,2,2,
2,2,2,2,2,2,2,2,2,2,2,2,2,2,2,2,2,2,2,2,2,2,2,2,2,2,2,2,2,2,2,2,2,2,2,2,
2,2,2,2,2,2,2,2,2,2,2,2,2,2,2,2,2,2,2,2,2,2,2,2,2,2,2,2,2,2,2,2,2,2,2,2,
2,2,2,2,2,2,2,2,2,2,2,2,2,2,2,2,2,2,2,2,2,2,2,2,2,2,2,2,2,2,2,2,2,2,2,2,
2,2,2,2,2,2,2,2,2,2,4),(0.00178286918103071,0.0702116732403354,0.0739134554827725,
0.0762686171690966,0.0780700941729444,0.0798031318675091,0.0815216676358921,
0.0838550823887649,0.0896065993021719,0.164469550269398,0.178374533877773,
0.32160563258876,0.386827762891506,0.471904890444151,0.492986723116284,
0.504735745040343,0.515147997854299,0.522603509386662,0.529380986753213,
0.538466808477913,0.560604650320051,0.72824374638507,0.822365739799538,
0.831373276795891,0.83546871079109,0.838387196001289,0.841558656577101,
0.846304169102604,0.86079626188838,0.92306555897299,1.08366895181813,1.12580905683544,
1.13698457916237,1.14369764165037,1.14971967740729,1.15738911520198,1.16963031667308,
1.25324542117658,1.25487205590743,1.39735445259342,1.47469279260515,1.55911341679864,
1.58100622837593,1.58961063169148,1.59398013506102,1.59762491862314,1.59984586309468,
1.60187285632001,1.60443498701174,1.6094090575242,1.6369315135227,1.8156866689287,
1.87671167317494,1.91310114619797,1.96632370158965,1.99343841542587,1.99833378850852,
2.00095017198125,2.00290087211242,2.00534253579087,2.0094424247477,2.02309515423683,
2.22704446612452,2.30613662411913,2.373741475614,2.40300492833247,2.41736952844954,
2.42000225318346,2.42142741260923,2.42248509982681,2.42363625727691,2.42530804519999,
2.43016758672025,2.51068593651509,2.70447576402168,2.80682032781053,2.81269252436261,
2.81537023123019,2.8173832629407,2.81927227527447,2.82188213036766,2.82854786113356,
2.91191490271624,3.01271061770623,3.12311267126745,3.18301569140295,3.21124211130723,
3.21481530627825,3.21758566695507,3.21898720138829,3.21999875576205,3.22107363425176,
3.22259160035302,3.22665321282433,3.28975829054167,3.44758266392114,3.55216454587476,
3.62484020195874,3.63714335469069,3.64082044972755,3.64310237917082,3.64518882801826,
3.64784534149745,3.65215436380811,3.66370874320673,3.86275202736945,4.01883048364631,
4.03229557406914,4.03570901908868,4.03771092228346,4.03946916457513,4.04164948561655,
4.04499095415936,4.05684111953118,4.22391385832158,4.32492680588544,4.39384547204995,
4.40929249818887,4.4151757713194,4.41918410156414,4.42308195796013,4.42774849343317,
4.43929718819992,4.58447487048618,4.71058063202622,4.75772221719597,4.77958681927027,
4.78318388134995,4.78506764999755,4.7866033255218,4.78837005230441,4.79134980813085,
4.80200481725375,4.97779453670051,5.17919466977863,5.19193290207189,5.19601480620525,
5.19826197228476,5.20050861069068,5.20326969184945,5.2085579321487,5.24113649814398,
5.31216611815138,5.51390710740312,5.60617790989111,5.61201333075414,5.61435999222778,
5.61608108423327,5.61793680196753,5.62044239385927,5.62609476488107,5.73810651998382,
5.83440217112809,5.92774913980307,6.00090088418838,6.03741721456688,6.04956461018117,
6.05659241272413,6.06389520351191,6.07337240929874,6.09359147351263,6.19529800053409,
6.26635008247157,6.35988397980786,6.36806909588673,6.37200663194041,6.37506265450251,
6.37842301211415,6.38396335201921,6.40860049569881,6.45939283193589,6.56747742286012,
6.61312086246876,6.61454182808589,6.63883833883263,6.66484242091535,6.67451670989531,
6.68025971480296,6.68632245567479,6.69432221923568,6.71185458909553,6.95204534382295,
7.11855733567308,7.12223529097698,7.13100900399951,7.13429529143143,7.13623889121713,
7.13807372463758,7.14062309868737,7.14570585888688,7.18611676571545,7.20738929120618,
7.26066915850748,7.40385925154798,7.46892479873277,7.52673788303649,7.53264978817835,
7.53554193863534,7.5376126280315,7.53979854117012,7.54267154541657,7.54842206898336,
7.58748227248819,7.6863002975352,7.77193864881608,7.91578203645863,7.95128191182783,
7.95498001168649,7.95644115954674,7.95753591908568,7.95873883296929,7.96040438186014,
7.96437843887609,8.06121820142061,8.21491708697904,8.33897543486416,8.34687856333327,
8.34968353266834,8.35162496278071,8.35341694022077,8.35584397420615,8.36005641699285,
8.38237386617808,8.42543011028978,8.52690141301026,8.73814164392687,8.75049573626578,
8.75280294918174,8.7542336798369,8.7553531958431,8.75659362495449,8.75862812913511,
8.76576542221671,8.81155263273582,8.87000187257926,8.99840624358182,9.03326004324483,
9.15513213718595,9.17116561220399,9.17535803919379,9.17777971444962,9.17963975728071,
9.18204404358492,9.18627184663985,9.20371922922874,9.2335846971396,9.31254852452438,
9.3700428151602,9.55479697246631,9.56697239860403,9.57038454765662,9.5724055450048,
9.57416101670328,9.57631295710055,9.58041811658988,9.60531436375194,9.66071275428514,
9.92178683662287,9.94215160107944,9.9484448831181,9.95135769407405,9.95208945193033),
 .UNSPECIFIED.);
#3560=B_SPLINE_CURVE_WITH_KNOTS('',3,(#226086,#226087,#226088,#226089,#226090,
#226091,#226092,#226093,#226094,#226095,#226096,#226097,#226098,#226099,
#226100,#226101,#226102,#226103,#226104,#226105,#226106,#226107,#226108,
#226109,#226110,#226111,#226112,#226113,#226114,#226115,#226116,#226117,
#226118,#226119,#226120,#226121,#226122,#226123,#226124,#226125,#226126,
#226127,#226128,#226129,#226130,#226131,#226132,#226133,#226134,#226135,
#226136,#226137,#226138,#226139,#226140,#226141,#226142,#226143,#226144,
#226145,#226146,#226147,#226148,#226149,#226150,#226151,#226152,#226153,
#226154,#226155,#226156,#226157,#226158,#226159,#226160,#226161,#226162,
#226163,#226164,#226165,#226166,#226167,#226168,#226169,#226170,#226171,
#226172,#226173,#226174,#226175,#226176,#226177,#226178,#226179,#226180,
#226181,#226182,#226183,#226184,#226185,#226186,#226187,#226188,#226189,
#226190,#226191,#226192,#226193,#226194,#226195,#226196,#226197,#226198,
#226199,#226200,#226201,#226202,#226203,#226204,#226205,#226206,#226207,
#226208,#226209,#226210,#226211,#226212,#226213,#226214,#226215,#226216,
#226217,#226218,#226219,#226220,#226221,#226222,#226223,#226224,#226225,
#226226,#226227,#226228,#226229,#226230,#226231,#226232,#226233,#226234,
#226235,#226236,#226237,#226238,#226239,#226240,#226241,#226242,#226243,
#226244,#226245,#226246,#226247,#226248,#226249,#226250,#226251,#226252,
#226253,#226254,#226255,#226256,#226257,#226258,#226259,#226260,#226261,
#226262,#226263,#226264,#226265,#226266,#226267,#226268,#226269,#226270,
#226271,#226272,#226273,#226274,#226275,#226276,#226277,#226278,#226279,
#226280,#226281,#226282,#226283,#226284,#226285,#226286,#226287,#226288,
#226289,#226290,#226291,#226292,#226293,#226294,#226295,#226296,#226297,
#226298,#226299,#226300,#226301,#226302,#226303,#226304,#226305,#226306,
#226307,#226308,#226309,#226310,#226311,#226312,#226313,#226314,#226315,
#226316,#226317,#226318,#226319,#226320,#226321,#226322,#226323,#226324,
#226325,#226326,#226327,#226328,#226329,#226330,#226331,#226332,#226333,
#226334,#226335,#226336,#226337,#226338,#226339,#226340,#226341,#226342,
#226343,#226344,#226345,#226346,#226347,#226348,#226349,#226350,#226351,
#226352,#226353,#226354,#226355,#226356,#226357,#226358,#226359,#226360,
#226361,#226362,#226363,#226364,#226365,#226366,#226367,#226368,#226369,
#226370,#226371,#226372,#226373,#226374,#226375,#226376,#226377,#226378,
#226379,#226380,#226381,#226382,#226383,#226384,#226385,#226386,#226387,
#226388,#226389,#226390,#226391,#226392,#226393,#226394,#226395,#226396,
#226397,#226398,#226399,#226400,#226401,#226402,#226403,#226404,#226405,
#226406,#226407,#226408,#226409,#226410,#226411,#226412,#226413,#226414,
#226415,#226416,#226417,#226418,#226419,#226420,#226421,#226422,#226423,
#226424,#226425,#226426,#226427,#226428,#226429,#226430,#226431,#226432,
#226433,#226434,#226435,#226436,#226437,#226438,#226439,#226440,#226441,
#226442,#226443,#226444,#226445,#226446,#226447,#226448,#226449,#226450,
#226451,#226452,#226453,#226454,#226455,#226456,#226457,#226458,#226459,
#226460,#226461,#226462,#226463,#226464,#226465,#226466,#226467,#226468,
#226469,#226470,#226471,#226472,#226473,#226474,#226475,#226476,#226477,
#226478,#226479,#226480,#226481,#226482,#226483,#226484,#226485,#226486,
#226487,#226488,#226489,#226490,#226491,#226492,#226493,#226494,#226495,
#226496,#226497,#226498,#226499,#226500,#226501,#226502,#226503,#226504,
#226505,#226506,#226507,#226508,#226509,#226510,#226511,#226512,#226513,
#226514,#226515,#226516,#226517,#226518,#226519,#226520,#226521,#226522,
#226523,#226524,#226525,#226526,#226527,#226528,#226529,#226530,#226531,
#226532,#226533,#226534,#226535,#226536,#226537,#226538,#226539,#226540,
#226541,#226542,#226543,#226544,#226545,#226546,#226547,#226548,#226549,
#226550,#226551,#226552,#226553,#226554,#226555,#226556,#226557,#226558,
#226559,#226560,#226561,#226562,#226563,#226564,#226565,#226566,#226567,
#226568,#226569,#226570,#226571,#226572,#226573,#226574,#226575,#226576,
#226577,#226578,#226579,#226580,#226581,#226582,#226583,#226584,#226585,
#226586,#226587,#226588,#226589,#226590,#226591,#226592,#226593,#226594,
#226595,#226596,#226597,#226598,#226599,#226600,#226601,#226602,#226603,
#226604,#226605,#226606,#226607,#226608,#226609,#226610,#226611,#226612,
#226613,#226614,#226615,#226616,#226617,#226618,#226619),.UNSPECIFIED.,
 .F.,.F.,(4,2,2,2,2,2,2,2,2,2,2,2,2,2,2,2,2,2,2,2,2,2,2,2,2,2,2,2,2,2,2,
2,2,2,2,2,2,2,2,2,2,2,2,2,2,2,2,2,2,2,2,2,2,2,2,2,2,2,2,2,2,2,2,2,2,2,2,
2,2,2,2,2,2,2,2,2,2,2,2,2,2,2,2,2,2,2,2,2,2,2,2,2,2,2,2,2,2,2,2,2,2,2,2,
2,2,2,2,2,2,2,2,2,2,2,2,2,2,2,2,2,2,2,2,2,2,2,2,2,2,2,2,2,2,2,2,2,2,2,2,
2,2,2,2,2,2,2,2,2,2,2,2,2,2,2,2,2,2,2,2,2,2,2,2,2,2,2,2,2,2,2,2,2,2,2,2,
2,2,2,2,2,2,2,2,2,2,2,2,2,2,2,2,2,2,2,2,2,2,2,2,2,2,2,2,2,2,2,2,2,2,2,2,
2,2,2,2,2,2,2,2,2,2,2,2,2,2,2,2,2,2,2,2,2,2,2,2,2,2,2,2,2,2,2,2,2,2,2,2,
2,2,2,2,2,2,2,2,2,2,2,2,2,2,2,2,2,2,2,4),(0.00234020634155756,0.0027510816593974,
0.00551666244128114,0.00960651587262544,0.015988039053587,0.034709088262484,
0.0487890063522092,0.298800863107575,0.344565586174986,0.365421925911194,
0.368975910792349,0.37085125084883,0.372387305170986,0.374162580527031,
0.377176090405291,0.388159462689479,0.572357328461512,0.596799345510092,
0.648110740262354,0.731805891957862,0.774921877363855,0.780612143318704,
0.78345762638049,0.785501125101516,0.787661491073668,0.791303999476934,
0.80094218796162,0.946683184463535,0.973280832551976,1.05209220156824,1.0788670978043,
1.11860737335751,1.18527413803429,1.19645764841932,1.19973138775093,1.20174856430344,
1.20358369678438,1.20594684048276,1.20974273635202,1.22976469973963,1.4196872550323,
1.58620370649975,1.62426033872084,1.63621069661681,1.64303996562399,1.64936279581738,
1.65808096700916,1.67443605317583,1.79797767843293,1.87897483675758,1.926105216938,
1.95020944640804,1.95613923727781,1.95963150463417,1.9626687341535,1.96640041163289,
1.97390276119606,2.04999442128266,2.15757843334392,2.23620418547095,2.25503206188746,
2.26327588537184,2.26869624063672,2.2747953808667,2.28359753911647,2.30532834570571,
2.5676610715653,2.67852344161176,2.71503694047112,2.72003333407314,2.72256580956398,
2.72439813298371,2.72634841073006,2.729670863345,2.73865032547288,2.83976376572276,
2.9551196832462,3.05433574594742,3.09547300106072,3.11732491861376,3.1206393505533,
3.12364584529936,3.12585505198356,3.12789202681393,3.13065087876145,3.13741510773507,
3.20645352418863,3.25260723367752,3.4387062212664,3.49512619324314,3.5258289055587,
3.5408214416601,3.54349361777068,3.54491600232031,3.5460872255496,3.54727012421086,
3.54945174029345,3.5567892729209,3.67653313056764,3.81568535251143,3.87129584491105,
3.92478241940949,3.93471742191485,3.93802319206267,3.94016244725309,3.94218066509392,
3.9448393924993,3.95076245520002,3.99990826628503,4.22359519879862,4.28373841163122,
4.32227091207181,4.33908595569833,4.34170184654556,4.34306010170982,4.34417431215424,
4.34546442504321,4.34766006975108,4.35566255940737,4.47654171720973,4.64038946849911,
4.75667794043611,4.76321816704555,4.76608841835433,4.76820219842565,4.77015453181233,
4.77280381456673,4.77932423148728,4.84748642893328,4.87037140727346,4.8788673160922,
4.98139134278997,5.14531532735059,5.15665336676671,5.16001447698011,5.1620052242881,
5.16374892828331,5.16593969809426,5.17022485130362,5.19970443713107,5.27726514978158,
5.44431443312162,5.52431215092603,5.53553307700073,5.5406149550474,5.54448974281139,
5.54862003062171,5.55506312165651,5.57507980679941,5.68661065923917,5.89651443824823,
5.90569785796369,5.90854715407342,5.91009615043434,5.91147849042039,5.9132828273197,
5.91650832437957,5.93174749687171,5.96149087625891,5.9922912685522,6.11077851938026,
6.23715942429661,6.23927010688217,6.24793280342784,6.31190386383668,6.31815557364956,
6.32118908665647,6.32334959657339,6.32539296555707,6.32823784484381,6.33392535460176,
6.37796842523448,6.47450432278688,6.56816988174891,6.72501553541103,6.73532904805074,
6.73857161284296,6.74057147259473,6.7423623258137,6.74464164425599,6.74912177160998,
6.78099553177467,6.87147850064111,6.95099692710767,7.13967902450119,7.16577493780009,
7.17544117848804,7.18236514832674,7.18972046648128,7.19953733853387,7.22160814647065,
7.3945903814351,7.48542570592058,7.49347161362858,7.49739272407579,7.50046569330726,
7.50377792092347,7.5090728477986,7.53023393725348,7.73913262105028,7.78620643959158,
7.79811272042643,7.80505675117524,7.81105029350359,7.81837926069913,7.83243985840723,
7.93996851827831,8.04576189461681,8.18657821314542,8.25188675567935,8.25796481255288,
8.26072294080131,8.26275174612017,8.26463997345015,8.26762458904398,8.27509840482735,
8.36834042332271,8.59722044716719,8.65326895592211,8.65978641275396,8.66243275510679,
8.66464292865305,8.66691339757199,8.67023519796964,8.67903966178091,8.79618114460997,
8.82774313442611,8.85243375918805,8.87282024726062,8.89016240359095,8.90519918130994,
8.91841622666362,8.95818791685082,9.04711978092511,9.05480762654373,9.07014273108751,
9.0799142995929,9.08213772613291,9.08359105855612,9.08469443705782,9.085979975628,
9.08808227811472,9.09557441444737,9.1081063990997,9.12993190802072,9.17381503759162,
9.45608280641075,9.47227975825498,9.47601290693852,9.47846407155866,9.48044920279866,
9.48271851362884,9.48660984712489,9.50222223923292,9.66609898221339,9.80467429081347,
9.8120493494853,9.87572038823951,9.87971391329847,9.88120808578717,9.88227448145145,
9.88335046319597,9.88444533578335,9.8858612038,9.88807395688612,9.90387815808587,
9.95827008045819),.UNSPECIFIED.);
#3561=B_SPLINE_CURVE_WITH_KNOTS('',3,(#226621,#226622,#226623,#226624,#226625,
#226626,#226627,#226628,#226629,#226630,#226631,#226632,#226633,#226634,
#226635,#226636,#226637,#226638,#226639,#226640,#226641,#226642,#226643,
#226644,#226645,#226646,#226647,#226648,#226649,#226650,#226651,#226652,
#226653,#226654,#226655,#226656,#226657,#226658,#226659,#226660,#226661,
#226662,#226663,#226664,#226665,#226666,#226667,#226668,#226669,#226670,
#226671,#226672,#226673,#226674,#226675,#226676,#226677,#226678,#226679,
#226680,#226681,#226682,#226683,#226684,#226685,#226686,#226687,#226688,
#226689,#226690,#226691,#226692,#226693,#226694,#226695,#226696,#226697,
#226698,#226699,#226700,#226701,#226702,#226703,#226704,#226705,#226706,
#226707,#226708,#226709,#226710,#226711,#226712,#226713,#226714,#226715,
#226716,#226717,#226718,#226719,#226720,#226721,#226722,#226723,#226724,
#226725,#226726,#226727,#226728,#226729,#226730,#226731,#226732,#226733,
#226734,#226735,#226736,#226737,#226738,#226739,#226740,#226741,#226742,
#226743,#226744,#226745,#226746,#226747,#226748,#226749,#226750,#226751,
#226752,#226753,#226754,#226755,#226756,#226757,#226758,#226759,#226760,
#226761,#226762,#226763,#226764,#226765,#226766,#226767,#226768,#226769,
#226770,#226771,#226772,#226773,#226774,#226775,#226776,#226777,#226778,
#226779,#226780,#226781,#226782,#226783,#226784,#226785,#226786,#226787,
#226788,#226789,#226790,#226791,#226792,#226793,#226794,#226795,#226796,
#226797,#226798,#226799,#226800,#226801,#226802,#226803,#226804,#226805,
#226806,#226807,#226808,#226809,#226810,#226811,#226812,#226813,#226814,
#226815,#226816,#226817,#226818,#226819,#226820,#226821,#226822,#226823,
#226824,#226825,#226826,#226827,#226828,#226829,#226830,#226831,#226832,
#226833,#226834,#226835,#226836,#226837,#226838,#226839,#226840,#226841,
#226842,#226843,#226844,#226845,#226846,#226847,#226848,#226849,#226850,
#226851,#226852,#226853,#226854,#226855,#226856,#226857,#226858,#226859,
#226860,#226861,#226862,#226863,#226864,#226865,#226866,#226867,#226868,
#226869,#226870,#226871,#226872,#226873,#226874,#226875,#226876,#226877,
#226878,#226879),.UNSPECIFIED.,.F.,.F.,(4,3,3,3,3,3,3,3,3,3,3,3,3,3,3,3,
3,3,3,3,3,3,3,3,3,3,3,3,3,3,3,3,3,3,3,3,3,3,3,3,3,3,3,3,3,3,3,3,3,3,3,3,
3,3,3,3,3,3,3,3,3,3,3,3,3,3,3,3,3,3,3,3,3,3,3,3,3,3,3,3,3,3,3,3,3,3,4),
(302.716543450764,302.789903215031,302.863182747746,302.936396853066,303.009560278126,
303.085475206124,303.158589582007,303.23170097055,303.304822643183,303.377967876696,
303.451183102599,303.524439931745,303.597783837003,303.616879702104,303.697873681488,
303.778750719554,303.863125432175,303.943683826104,304.024118368083,304.104377785666,
304.116249570035,304.190653873251,304.265074944053,304.339525055503,304.414057090776,
304.488633531045,304.563314477813,304.615619437966,304.692190981333,304.768694873943,
304.845142068533,304.921543477559,304.997909980536,305.074966129697,305.151303519778,
305.227640391075,305.303986599292,305.381579742926,305.457998854666,305.536179014247,
305.614359173828,305.688136264652,305.761851042085,305.835516576372,305.909146721459,
305.982755345264,306.056368163069,306.113729041759,306.19516257284,306.276731567837,
306.3608234033,306.442666109795,306.527882509743,306.61309890969,306.691531853187,
306.769895037067,306.848193302346,306.926412568203,307.004581859708,307.082693184795,
307.112468777621,307.188831248704,307.265210574786,307.341616340427,307.418091012518,
307.494603060247,307.571197389472,307.611838645552,307.68721602449,307.762531857889,
307.8377989675,307.913030142583,307.988238147729,308.066030676939,308.141248853122,
308.2164837287,308.291746872247,308.367049865591,308.442442061547,308.517886960896,
308.593430321996,308.610578381415,308.691791755436,308.772652942617,308.853304139261,
308.933615080475,308.999728757943),.UNSPECIFIED.);
#3562=B_SPLINE_CURVE_WITH_KNOTS('',3,(#226881,#226882,#226883,#226884,#226885,
#226886,#226887,#226888,#226889,#226890,#226891,#226892,#226893,#226894,
#226895,#226896,#226897,#226898),.UNSPECIFIED.,.F.,.F.,(4,2,2,2,2,2,2,2,
4),(308.999728757943,309.834645669838,310.669562581733,311.504479493628,
312.339396405523,313.174313317418,314.009230229313,314.844147141208,315.282914065123),
 .UNSPECIFIED.);
#3563=B_SPLINE_CURVE_WITH_KNOTS('',3,(#226900,#226901,#226902,#226903,#226904,
#226905,#226906,#226907,#226908,#226909,#226910,#226911,#226912),
 .UNSPECIFIED.,.F.,.F.,(4,1,1,1,1,1,1,1,1,1,4),(315.282914065123,315.60175653245,
316.600496268312,317.599236004174,318.098605872105,318.597975740036,319.596715475899,
320.09608534383,320.595455211761,321.094825079692,321.566099372303),
 .UNSPECIFIED.);
#3564=B_SPLINE_CURVE_WITH_KNOTS('',3,(#226914,#226915,#226916,#226917,#226918,
#226919,#226920,#226921,#226922,#226923,#226924,#226925,#226926,#226927),
 .UNSPECIFIED.,.F.,.F.,(4,2,1,1,1,1,1,1,1,1,4),(321.566099372303,321.594194947623,
322.592934683485,323.591674419347,324.59041415521,325.089784023141,325.589153891072,
326.587893626934,327.087263494865,327.586633362796,327.849284679482),
 .UNSPECIFIED.);
#3565=B_SPLINE_CURVE_WITH_KNOTS('',3,(#226929,#226930,#226931,#226932,#226933,
#226934,#226935,#226936,#226937,#226938,#226939,#226940,#226941,#226942,
#226943,#226944,#226945,#226946,#226947,#226948,#226949,#226950,#226951,
#226952,#226953,#226954,#226955,#226956,#226957,#226958,#226959,#226960,
#226961,#226962,#226963,#226964,#226965,#226966,#226967,#226968,#226969,
#226970,#226971,#226972,#226973,#226974,#226975,#226976,#226977,#226978,
#226979,#226980,#226981,#226982,#226983,#226984,#226985,#226986,#226987,
#226988,#226989,#226990,#226991,#226992,#226993,#226994,#226995,#226996,
#226997,#226998,#226999,#227000,#227001,#227002,#227003,#227004,#227005,
#227006,#227007,#227008,#227009,#227010,#227011,#227012,#227013,#227014,
#227015,#227016,#227017,#227018,#227019,#227020,#227021,#227022,#227023,
#227024,#227025,#227026,#227027,#227028,#227029,#227030,#227031,#227032,
#227033,#227034,#227035,#227036,#227037,#227038,#227039,#227040,#227041,
#227042,#227043,#227044,#227045,#227046,#227047,#227048,#227049,#227050,
#227051,#227052,#227053,#227054,#227055,#227056,#227057,#227058,#227059,
#227060,#227061,#227062,#227063,#227064,#227065,#227066,#227067,#227068,
#227069,#227070,#227071,#227072,#227073,#227074,#227075,#227076,#227077,
#227078,#227079,#227080,#227081,#227082,#227083,#227084,#227085,#227086,
#227087,#227088,#227089,#227090,#227091,#227092,#227093,#227094,#227095,
#227096,#227097,#227098,#227099,#227100,#227101,#227102,#227103,#227104,
#227105,#227106,#227107,#227108,#227109,#227110,#227111,#227112,#227113,
#227114,#227115,#227116,#227117,#227118,#227119,#227120,#227121,#227122,
#227123,#227124,#227125,#227126,#227127,#227128,#227129,#227130,#227131,
#227132,#227133,#227134,#227135,#227136,#227137,#227138,#227139,#227140,
#227141,#227142,#227143,#227144,#227145,#227146,#227147,#227148,#227149,
#227150,#227151,#227152,#227153,#227154,#227155,#227156,#227157,#227158,
#227159,#227160,#227161,#227162,#227163,#227164,#227165,#227166,#227167,
#227168,#227169,#227170,#227171,#227172,#227173,#227174,#227175,#227176,
#227177,#227178,#227179,#227180,#227181,#227182,#227183,#227184,#227185,
#227186,#227187,#227188,#227189,#227190,#227191,#227192,#227193,#227194,
#227195,#227196,#227197,#227198,#227199,#227200,#227201,#227202,#227203,
#227204,#227205,#227206,#227207,#227208,#227209,#227210,#227211,#227212,
#227213,#227214,#227215,#227216,#227217,#227218,#227219,#227220,#227221,
#227222,#227223,#227224,#227225,#227226,#227227,#227228,#227229,#227230,
#227231,#227232,#227233,#227234,#227235,#227236,#227237,#227238,#227239,
#227240,#227241,#227242,#227243,#227244,#227245,#227246,#227247,#227248,
#227249,#227250,#227251,#227252,#227253,#227254,#227255,#227256,#227257,
#227258,#227259,#227260,#227261,#227262,#227263,#227264,#227265,#227266,
#227267,#227268,#227269,#227270,#227271,#227272,#227273,#227274,#227275,
#227276,#227277,#227278,#227279,#227280,#227281,#227282,#227283,#227284,
#227285,#227286,#227287,#227288,#227289,#227290,#227291,#227292,#227293,
#227294,#227295,#227296,#227297,#227298,#227299,#227300,#227301,#227302,
#227303,#227304,#227305,#227306,#227307,#227308,#227309,#227310,#227311,
#227312,#227313,#227314,#227315,#227316,#227317,#227318,#227319,#227320,
#227321,#227322,#227323,#227324,#227325,#227326,#227327,#227328,#227329,
#227330,#227331,#227332,#227333,#227334,#227335,#227336,#227337,#227338,
#227339,#227340,#227341,#227342,#227343,#227344,#227345,#227346,#227347,
#227348,#227349,#227350,#227351,#227352,#227353,#227354,#227355,#227356,
#227357,#227358,#227359,#227360,#227361,#227362,#227363,#227364,#227365,
#227366,#227367,#227368,#227369,#227370,#227371,#227372,#227373,#227374,
#227375,#227376,#227377,#227378,#227379,#227380,#227381,#227382,#227383,
#227384,#227385,#227386,#227387,#227388,#227389,#227390,#227391,#227392,
#227393,#227394,#227395,#227396,#227397,#227398,#227399,#227400,#227401,
#227402,#227403,#227404,#227405,#227406,#227407,#227408,#227409,#227410,
#227411,#227412,#227413,#227414,#227415,#227416,#227417,#227418,#227419,
#227420,#227421,#227422,#227423,#227424,#227425,#227426,#227427,#227428,
#227429,#227430,#227431,#227432,#227433,#227434,#227435,#227436,#227437,
#227438,#227439,#227440,#227441,#227442,#227443,#227444,#227445,#227446,
#227447,#227448,#227449,#227450,#227451,#227452),.UNSPECIFIED.,.F.,.F.,
(4,2,2,2,2,2,2,2,2,2,2,2,2,2,2,2,2,2,2,2,2,2,2,2,2,2,2,2,2,2,2,2,2,2,2,
2,2,2,2,2,2,2,2,2,2,2,2,2,2,2,2,2,2,2,2,2,2,2,2,2,2,2,2,2,2,2,2,2,2,2,2,
2,2,2,2,2,2,2,2,2,2,2,2,2,2,2,2,2,2,2,2,2,2,2,2,2,2,2,2,2,2,2,2,2,2,2,2,
2,2,2,2,2,2,2,2,2,2,2,2,2,2,2,2,2,2,2,2,2,2,2,2,2,2,2,2,2,2,2,2,2,2,2,2,
2,2,2,2,2,2,2,2,2,2,2,2,2,2,2,2,2,2,2,2,2,2,2,2,2,2,2,2,2,2,2,2,2,2,2,2,
2,2,2,2,2,2,2,2,2,2,2,2,2,2,2,2,2,2,2,2,2,2,2,2,2,2,2,2,2,2,2,2,2,2,2,2,
2,2,2,2,2,2,2,2,2,2,2,2,2,2,2,2,2,2,2,2,2,2,2,2,2,2,2,2,2,2,2,2,2,2,2,2,
2,2,2,2,2,2,2,2,2,2,4),(0.00141745760897423,0.067162311283536,0.0780209552792477,
0.0851854906335986,0.0909210426250336,0.0968707264688579,0.103770083128768,
0.115494274022767,0.16237726379872,0.206207364650622,0.456623595264774,
0.515771718959542,0.541705696762699,0.546296033793239,0.548743640484823,
0.550743266418886,0.552779534906327,0.556530540707647,0.568631379334648,
0.729403105854545,0.782206725727187,0.839959053698312,0.910649773391808,
0.942586920948702,0.947704008334611,0.950368297643282,0.952532398783485,
0.954693798396332,0.958610983339168,0.97076891749642,1.14727277420351,1.23861232553984,
1.25127341753228,1.29295222246926,1.35877106132461,1.36769669441332,1.3699717109283,
1.37130726202381,1.37248079233919,1.3739364354681,1.37616408280461,1.38660790323757,
1.55435250822876,1.62359624571914,1.70728969075542,1.7409323688155,1.7530317453309,
1.75866975621739,1.76321455138327,1.76562750368209,1.76741959033857,1.76937143843708,
1.7728092133636,1.78279952483596,1.93040389735508,2.09480521253811,2.15768215265109,
2.16610157981944,2.16823014245425,2.16948636191472,2.17060432891969,2.17200979688767,
2.17419824471008,2.18440272010436,2.34513614150874,2.43847169427428,2.54388013707765,
2.58478491107501,2.590038248084,2.5926623072679,2.59454558218568,2.59653539051702,
2.59988731414479,2.60873923020928,2.74252500115857,2.86549427911651,2.97956761389034,
2.98492186811423,2.9873216337073,2.98910911048775,2.99077506111053,2.99305918913317,
2.99760158217403,3.03701411894509,3.22612515087694,3.33766817538262,3.35837177010574,
3.36501771431343,3.36919256894291,3.37305095147414,3.37802797119256,3.38873979701807,
3.4757667471831,3.60055926291225,3.702950785543,3.73007942154706,3.7338748728155,
3.73580055193312,3.73719431648433,3.73867797233158,3.74077693905783,3.74641995038451,
3.83459759229004,4.01592119297889,4.13803885224389,4.14501723412619,4.14811057371096,
4.15040092801254,4.15252510392066,4.15542110210616,4.162617729655,4.24217153457634,
4.4358174930071,4.49556434090439,4.53838244230649,4.56023523738886,4.56430251842368,
4.56649519939402,4.56813896253032,4.57020752468113,4.57371001678128,4.5856709199006,
4.59159097026156,4.59331528643355,4.76381405634778,4.88682837056718,4.98028744093667,
4.99556685502615,5.00495325654838,5.0122489791179,5.02032685882555,5.03369440147927,
5.08517552972484,5.18151594937427,5.30495942465799,5.31769911541664,5.32255699349876,
5.32546419180189,5.32853934239581,5.33259872032313,5.34214047037631,5.35572723109848,
5.39412830013317,5.52175314488656,5.56710689104154,5.61258119114196,5.62435653636009,
5.63127137982623,5.63726839234622,5.6446380237003,5.65889228698797,5.770932609268,
5.87746043311761,6.02576122481904,6.07851227678507,6.08445768173807,6.08714766808781,
6.08919904876443,6.0913832968761,6.09477985555712,6.10516305429029,6.15876632597075,
6.24280588310666,6.46947438593558,6.48346970680589,6.48761000085326,6.49006121147773,
6.49201149376827,6.49461691240164,6.49945868165752,6.52550465786664,6.57610237741566,
6.63504187202422,6.78934347291348,6.89954243926188,6.906839317458,6.90904993043202,
6.91023895192103,6.91140975623648,6.9128229400933,6.91545307037718,6.93107247920207,
6.93328937158055,6.97493539267457,7.12297310878393,7.23410455741389,7.29489494242167,
7.30104036424938,7.30356121067752,7.30542765906325,7.30745691844026,7.31022745077674,
7.31660585254173,7.37854628083601,7.41027894943964,7.5559193336004,7.69551565805991,
7.70455618857236,7.70682508324113,7.70812429905798,7.70922714750612,7.71056875669458,
7.71305839952144,7.7263145601904,7.75296164178759,7.80388452792607,7.91448178713277,
8.05145589969884,8.1211847484972,8.1277631866839,8.1304223377097,8.13237700972853,
8.13448857988451,8.13734730496074,8.14382485807563,8.26418415364691,8.40681007728003,
8.51264947398095,8.52188549783611,8.5249830537626,8.52672108417959,8.52846436419277,
8.53065237165202,8.53450719646242,8.55684285072358,8.60567549590081,8.73500394118451,
8.7944338573327,8.88825211858894,8.89875428431989,8.9038805227842,8.90754078777543,
8.91140082415158,8.91516033387907,8.92005701272533,8.94123735031426,8.97412411999817,
9.0572858725404,9.1244380607312,9.24036186541586,9.26775909043428,9.27190596608096,
9.27390233855925,9.27544973540007,9.27714746044654,9.2788859841696,9.28142499662682,
9.30442331369998,9.37414146134346,9.42320007992591,9.60208625751048,9.6104970471058,
9.67612638090174,9.68241991592185,9.6854634356422,9.68762640874013,9.68966831733391,
9.69250513700915,9.69815463790678,9.74091386502713,9.8504320272541,9.95730281891779),
 .UNSPECIFIED.);
#3566=B_SPLINE_CURVE_WITH_KNOTS('',3,(#227454,#227455,#227456,#227457,#227458,
#227459,#227460,#227461,#227462,#227463,#227464,#227465,#227466,#227467,
#227468,#227469,#227470,#227471),.UNSPECIFIED.,.F.,.F.,(4,2,2,2,2,2,2,2,
4),(340.415655293841,341.250572205736,342.085489117631,342.920406029526,
343.755322941421,344.590239853316,345.425156765211,346.260073677105,346.698657753416),
 .UNSPECIFIED.);
#3567=B_SPLINE_CURVE_WITH_KNOTS('',3,(#227473,#227474,#227475,#227476,#227477,
#227478,#227479,#227480,#227481,#227482,#227483,#227484,#227485,#227486,
#227487,#227488,#227489,#227490,#227491,#227492,#227493,#227494,#227495,
#227496,#227497,#227498,#227499,#227500,#227501,#227502,#227503,#227504,
#227505,#227506,#227507,#227508,#227509,#227510,#227511,#227512,#227513,
#227514,#227515,#227516,#227517,#227518,#227519,#227520,#227521,#227522,
#227523,#227524,#227525,#227526,#227527,#227528,#227529,#227530,#227531,
#227532,#227533,#227534,#227535,#227536,#227537,#227538,#227539,#227540,
#227541,#227542,#227543,#227544,#227545,#227546,#227547,#227548,#227549,
#227550,#227551,#227552,#227553,#227554,#227555,#227556,#227557,#227558,
#227559,#227560,#227561,#227562,#227563,#227564,#227565,#227566,#227567,
#227568,#227569,#227570,#227571,#227572,#227573,#227574,#227575,#227576,
#227577,#227578,#227579,#227580,#227581,#227582,#227583,#227584,#227585,
#227586,#227587,#227588,#227589,#227590,#227591,#227592,#227593,#227594,
#227595,#227596,#227597,#227598,#227599,#227600,#227601,#227602,#227603,
#227604,#227605,#227606,#227607,#227608,#227609,#227610,#227611,#227612,
#227613,#227614,#227615,#227616,#227617,#227618,#227619,#227620,#227621,
#227622,#227623,#227624,#227625,#227626,#227627,#227628,#227629,#227630,
#227631,#227632,#227633,#227634,#227635,#227636,#227637,#227638,#227639,
#227640,#227641,#227642,#227643,#227644,#227645,#227646,#227647,#227648,
#227649,#227650,#227651,#227652,#227653,#227654,#227655,#227656,#227657,
#227658,#227659,#227660,#227661,#227662,#227663,#227664,#227665,#227666,
#227667,#227668,#227669,#227670,#227671,#227672,#227673,#227674,#227675,
#227676,#227677,#227678,#227679,#227680,#227681,#227682,#227683,#227684,
#227685,#227686,#227687,#227688,#227689,#227690,#227691,#227692,#227693,
#227694,#227695,#227696,#227697,#227698,#227699,#227700,#227701,#227702,
#227703,#227704,#227705,#227706,#227707,#227708,#227709,#227710,#227711,
#227712,#227713,#227714,#227715,#227716,#227717,#227718,#227719,#227720,
#227721,#227722,#227723,#227724,#227725,#227726,#227727,#227728,#227729,
#227730,#227731,#227732,#227733,#227734),.UNSPECIFIED.,.F.,.F.,(4,3,3,3,
3,3,3,3,3,3,3,3,3,3,3,3,3,3,3,3,3,3,3,3,3,3,3,3,3,3,3,3,3,3,3,3,3,3,3,3,
3,3,3,3,3,3,3,3,3,3,3,3,3,3,3,3,3,3,3,3,3,3,3,3,3,3,3,3,3,3,3,3,3,3,3,3,
3,3,3,3,3,3,3,3,3,3,3,4),(346.698953041191,346.774312894999,346.849606692114,
346.924847356439,347.000047776703,347.075224878317,347.150390746122,347.22555702008,
347.300735338305,347.375965001418,347.451223462602,347.526553270498,347.56142808004,
347.635205170864,347.708919948298,347.782585482584,347.856215627671,347.929824251476,
348.003437069281,348.060797947971,348.142231479052,348.223800474049,348.307892309512,
348.389735016008,348.474951415955,348.560167815902,348.638600759399,348.716963943279,
348.795262208557,348.873481474414,348.951650765919,349.029762091005,349.059537683833,
349.135900154916,349.212279480999,349.288685246639,349.365159918731,349.441671966459,
349.518266295685,349.558907551764,349.634284930701,349.709600764101,349.784867873711,
349.860099048794,349.935307053938,350.013099583149,350.088317759332,350.163552634909,
350.238815778455,350.314118771799,350.389510967755,350.464955867104,350.540499228203,
350.557647287626,350.630791096602,350.703846109716,350.776827264111,350.849749426759,
350.922627410056,350.995475985878,351.068323386895,351.141173733045,351.214040373102,
351.286936666527,351.359918806511,351.432947707244,351.506087260815,351.556387023489,
351.630975642714,351.705478613094,351.779909870854,351.854283304733,351.928612765146,
352.002912072902,352.077205434053,352.151498983122,352.225805213731,352.300136623861,
352.374540666731,352.448986319046,352.523522877136,352.555126759351,352.63852443211,
352.724399776288,352.807379818993,352.89017442231,352.972685446835,352.982025808824),
 .UNSPECIFIED.);
#3568=B_SPLINE_CURVE_WITH_KNOTS('',3,(#227736,#227737,#227738,#227739,#227740,
#227741,#227742,#227743,#227744,#227745,#227746,#227747,#227748),
 .UNSPECIFIED.,.F.,.F.,(4,1,1,1,1,1,1,1,1,1,4),(352.9820259082,353.054496627282,
353.553866495213,354.552606231075,355.051976099006,355.551345966937,356.050715834868,
356.550085702799,357.548825438662,358.547565174524,359.26521121538),
 .UNSPECIFIED.);
#3569=B_SPLINE_CURVE_WITH_KNOTS('',3,(#227750,#227751,#227752,#227753,#227754,
#227755,#227756,#227757,#227758,#227759,#227760,#227761,#227762,#227763,
#227764,#227765,#227766,#227767,#227768,#227769,#227770,#227771,#227772,
#227773,#227774,#227775,#227776,#227777,#227778,#227779,#227780,#227781,
#227782,#227783,#227784,#227785,#227786,#227787,#227788,#227789,#227790,
#227791,#227792,#227793,#227794,#227795,#227796,#227797,#227798,#227799,
#227800,#227801,#227802,#227803,#227804,#227805,#227806,#227807,#227808,
#227809,#227810,#227811,#227812,#227813,#227814,#227815,#227816,#227817,
#227818,#227819,#227820,#227821,#227822,#227823,#227824,#227825,#227826,
#227827,#227828,#227829,#227830,#227831,#227832,#227833,#227834,#227835,
#227836,#227837,#227838,#227839,#227840,#227841,#227842,#227843,#227844,
#227845,#227846,#227847,#227848,#227849,#227850,#227851,#227852,#227853,
#227854,#227855,#227856,#227857,#227858,#227859,#227860,#227861,#227862,
#227863,#227864,#227865,#227866,#227867,#227868,#227869,#227870,#227871,
#227872,#227873,#227874,#227875,#227876,#227877,#227878,#227879,#227880,
#227881,#227882,#227883,#227884,#227885,#227886,#227887,#227888,#227889,
#227890,#227891,#227892,#227893,#227894,#227895,#227896,#227897,#227898,
#227899,#227900,#227901,#227902,#227903,#227904,#227905,#227906,#227907,
#227908,#227909,#227910,#227911,#227912,#227913,#227914,#227915,#227916,
#227917,#227918,#227919,#227920,#227921,#227922,#227923,#227924,#227925,
#227926,#227927,#227928,#227929,#227930,#227931,#227932,#227933,#227934,
#227935,#227936,#227937,#227938,#227939,#227940,#227941,#227942,#227943,
#227944,#227945,#227946,#227947,#227948,#227949,#227950,#227951,#227952,
#227953,#227954,#227955,#227956,#227957,#227958,#227959,#227960,#227961,
#227962,#227963,#227964,#227965,#227966,#227967,#227968,#227969,#227970,
#227971,#227972,#227973,#227974,#227975,#227976,#227977,#227978,#227979,
#227980,#227981,#227982,#227983,#227984,#227985,#227986,#227987,#227988,
#227989,#227990,#227991,#227992,#227993,#227994,#227995,#227996,#227997,
#227998,#227999,#228000,#228001,#228002,#228003,#228004,#228005,#228006,
#228007,#228008,#228009,#228010,#228011),.UNSPECIFIED.,.F.,.F.,(4,3,3,3,
3,3,3,3,3,3,3,3,3,3,3,3,3,3,3,3,3,3,3,3,3,3,3,3,3,3,3,3,3,3,3,3,3,3,3,3,
3,3,3,3,3,3,3,3,3,3,3,3,3,3,3,3,3,3,3,3,3,3,3,3,3,3,3,3,3,3,3,3,3,3,3,3,
3,3,3,3,3,3,3,3,3,3,3,4),(359.265211374834,359.351771246646,359.438775330765,
359.526288962694,359.546304910386,359.62729888977,359.708175927836,359.792550640457,
359.873109034386,359.953543576365,360.033802993948,360.045674778317,360.120079081534,
360.194500152335,360.268950263786,360.343482299059,360.418058739327,360.492739686096,
360.545044646248,360.621616189615,360.698120082225,360.774567276814,360.850968685839,
360.927335188816,361.004391337978,361.080728728059,361.157065599356,361.233411807572,
361.311004951207,361.387424062947,361.465604222528,361.54378438211,361.617561472934,
361.691276250369,361.764941784655,361.838571929742,361.912180553548,361.985793371353,
362.043154250042,362.124587781123,362.20615677612,362.290248611583,362.372091318079,
362.457307718026,362.542524117973,362.620957061469,362.699320245349,362.777618510626,
362.855837776482,362.934007067986,363.012118393073,363.041893985904,363.118256456988,
363.19463578307,363.271041548711,363.347516220803,363.424028268532,363.500622597758,
363.541263853835,363.616641232772,363.691957066172,363.767224175782,363.842455350865,
363.91766335601,363.995455885221,364.070674061403,364.145908936981,364.221172080526,
364.29647507387,364.371867269826,364.447312169175,364.522855530275,364.540003589697,
364.613147398672,364.686202411787,364.759183566181,364.832105728829,364.904983712125,
364.977832287947,365.050679688963,365.123530035113,365.19639667517,365.269292968596,
365.342275108579,365.415304009312,365.488443562883,365.538743325559,365.54839652256),
 .UNSPECIFIED.);
#3570=B_SPLINE_CURVE_WITH_KNOTS('',3,(#228013,#228014,#228015,#228016,#228017,
#228018,#228019,#228020,#228021,#228022,#228023,#228024,#228025),
 .UNSPECIFIED.,.F.,.F.,(4,1,1,1,1,1,1,1,1,1,4),(365.548397871087,366.537483061421,
367.036852929352,367.536222797283,368.534962533146,369.034332401077,369.533702269008,
370.033072136939,370.53244200487,371.531181740732,371.831581829739),
 .UNSPECIFIED.);
#3571=B_SPLINE_CURVE_WITH_KNOTS('',3,(#228027,#228028,#228029,#228030,#228031,
#228032,#228033,#228034,#228035,#228036,#228037,#228038,#228039,#228040,
#228041,#228042,#228043,#228044),.UNSPECIFIED.,.F.,.F.,(4,2,2,2,2,2,2,2,
4),(371.831581829739,372.666498741634,373.501415653529,374.336332565424,
375.171249477319,376.006166389214,376.841083301109,377.676000213004,378.114767136919),
 .UNSPECIFIED.);
#3572=B_SPLINE_CURVE_WITH_KNOTS('',3,(#228046,#228047,#228048,#228049,#228050,
#228051,#228052,#228053,#228054,#228055,#228056,#228057,#228058,#228059,
#228060,#228061,#228062,#228063,#228064,#228065,#228066,#228067,#228068,
#228069,#228070,#228071,#228072,#228073,#228074,#228075,#228076,#228077,
#228078,#228079,#228080,#228081,#228082,#228083,#228084,#228085,#228086,
#228087,#228088,#228089,#228090,#228091,#228092,#228093,#228094,#228095,
#228096,#228097,#228098,#228099,#228100,#228101,#228102,#228103,#228104,
#228105,#228106,#228107,#228108,#228109,#228110,#228111,#228112,#228113,
#228114,#228115,#228116,#228117,#228118,#228119,#228120,#228121,#228122,
#228123,#228124,#228125,#228126,#228127,#228128,#228129,#228130,#228131,
#228132,#228133,#228134,#228135,#228136,#228137,#228138,#228139,#228140,
#228141,#228142,#228143,#228144,#228145,#228146,#228147,#228148,#228149,
#228150,#228151,#228152,#228153,#228154,#228155,#228156,#228157,#228158,
#228159,#228160,#228161,#228162,#228163,#228164,#228165,#228166,#228167,
#228168,#228169,#228170,#228171,#228172,#228173,#228174,#228175,#228176,
#228177,#228178,#228179,#228180,#228181,#228182,#228183,#228184,#228185,
#228186,#228187,#228188,#228189,#228190,#228191,#228192,#228193,#228194,
#228195,#228196,#228197,#228198,#228199,#228200,#228201,#228202,#228203,
#228204,#228205,#228206,#228207,#228208,#228209,#228210,#228211,#228212,
#228213,#228214,#228215,#228216,#228217,#228218,#228219,#228220,#228221,
#228222,#228223,#228224,#228225,#228226,#228227,#228228,#228229,#228230,
#228231,#228232,#228233,#228234,#228235,#228236,#228237,#228238,#228239,
#228240,#228241,#228242,#228243,#228244,#228245,#228246,#228247,#228248,
#228249,#228250,#228251,#228252,#228253,#228254,#228255,#228256,#228257,
#228258,#228259,#228260,#228261,#228262,#228263,#228264,#228265,#228266,
#228267,#228268,#228269,#228270,#228271,#228272,#228273,#228274,#228275,
#228276,#228277,#228278,#228279,#228280,#228281,#228282,#228283,#228284,
#228285,#228286,#228287,#228288,#228289,#228290,#228291,#228292,#228293,
#228294,#228295,#228296,#228297,#228298,#228299,#228300,#228301,#228302,
#228303,#228304,#228305,#228306,#228307,#228308,#228309,#228310,#228311,
#228312,#228313,#228314,#228315,#228316,#228317,#228318,#228319,#228320,
#228321,#228322,#228323,#228324,#228325,#228326,#228327,#228328,#228329,
#228330,#228331,#228332,#228333,#228334,#228335,#228336,#228337,#228338,
#228339,#228340,#228341,#228342,#228343,#228344,#228345,#228346,#228347,
#228348,#228349,#228350,#228351,#228352,#228353,#228354,#228355,#228356,
#228357,#228358,#228359,#228360,#228361,#228362,#228363,#228364,#228365,
#228366,#228367,#228368,#228369,#228370,#228371,#228372,#228373,#228374,
#228375,#228376,#228377,#228378,#228379,#228380,#228381,#228382,#228383,
#228384,#228385,#228386,#228387,#228388,#228389,#228390,#228391,#228392,
#228393,#228394,#228395,#228396,#228397,#228398,#228399,#228400,#228401,
#228402,#228403,#228404,#228405,#228406,#228407,#228408,#228409,#228410,
#228411,#228412,#228413,#228414,#228415,#228416,#228417,#228418,#228419,
#228420,#228421,#228422,#228423,#228424,#228425,#228426,#228427,#228428,
#228429,#228430,#228431,#228432,#228433,#228434,#228435,#228436,#228437,
#228438,#228439,#228440,#228441,#228442,#228443,#228444,#228445,#228446,
#228447,#228448,#228449,#228450,#228451,#228452,#228453,#228454,#228455,
#228456,#228457,#228458,#228459,#228460,#228461,#228462,#228463,#228464,
#228465,#228466,#228467,#228468,#228469,#228470,#228471,#228472,#228473,
#228474,#228475,#228476,#228477,#228478,#228479,#228480,#228481,#228482,
#228483,#228484,#228485,#228486,#228487,#228488,#228489,#228490,#228491,
#228492,#228493,#228494,#228495,#228496,#228497,#228498,#228499,#228500,
#228501,#228502,#228503,#228504,#228505,#228506,#228507,#228508,#228509,
#228510,#228511,#228512,#228513,#228514,#228515,#228516,#228517,#228518,
#228519,#228520,#228521,#228522,#228523,#228524,#228525,#228526,#228527,
#228528,#228529,#228530,#228531,#228532,#228533,#228534,#228535,#228536,
#228537,#228538,#228539,#228540,#228541,#228542,#228543,#228544,#228545,
#228546,#228547,#228548,#228549,#228550,#228551,#228552,#228553,#228554,
#228555,#228556,#228557,#228558,#228559,#228560,#228561,#228562,#228563,
#228564,#228565,#228566,#228567,#228568,#228569,#228570,#228571,#228572,
#228573,#228574,#228575,#228576,#228577),.UNSPECIFIED.,.F.,.F.,(4,2,2,2,
2,2,2,2,2,2,2,2,2,2,2,2,2,2,2,2,2,2,2,2,2,2,2,2,2,2,2,2,2,2,2,2,2,2,2,2,
2,2,2,2,2,2,2,2,2,2,2,2,2,2,2,2,2,2,2,2,2,2,2,2,2,2,2,2,2,2,2,2,2,2,2,2,
2,2,2,2,2,2,2,2,2,2,2,2,2,2,2,2,2,2,2,2,2,2,2,2,2,2,2,2,2,2,2,2,2,2,2,2,
2,2,2,2,2,2,2,2,2,2,2,2,2,2,2,2,2,2,2,2,2,2,2,2,2,2,2,2,2,2,2,2,2,2,2,2,
2,2,2,2,2,2,2,2,2,2,2,2,2,2,2,2,2,2,2,2,2,2,2,2,2,2,2,2,2,2,2,2,2,2,2,2,
2,2,2,2,2,2,2,2,2,2,2,2,2,2,2,2,2,2,2,2,2,2,2,2,2,2,2,2,2,2,2,2,2,2,2,2,
2,2,2,2,2,2,2,2,2,2,2,2,2,2,2,2,2,2,2,2,2,2,2,2,2,2,2,2,2,2,2,2,2,2,2,2,
2,2,2,2,2,2,2,2,2,4),(0.00193034970426769,0.251769396345977,0.307891382236222,
0.316094863725038,0.318304129568899,0.319624845655523,0.320800202296045,
0.322277821764209,0.324576538969347,0.336011088366562,0.526210819881589,
0.627146546913494,0.679015458140233,0.697261508663907,0.704918787823994,
0.708942333462824,0.71236269399982,0.714508820411928,0.716422074763476,
0.71896165887763,0.724119115451281,0.754827416334772,0.855377445575457,
0.913468041963251,1.02182672019539,1.06417651461188,1.10754885551415,1.1143892613705,
1.1163676333868,1.11759151760635,1.11871635257558,1.12015632429706,1.12319993798314,
1.14340608252472,1.39324747618811,1.47245014954148,1.51280083785537,1.52686501275496,
1.5332437090269,1.53828118864638,1.54084079689098,1.54272164275102,1.54471464758234,
1.54752003513558,1.553324502198,1.61384341876806,1.74665762394975,1.85129426279119,
1.919846964539,1.93106700551334,1.93426960922784,1.93622449476669,1.93799070418438,
1.9402478494948,1.94470907225781,1.97145037102271,2.03268553921962,2.15004691225555,
2.22624741731643,2.29263519605128,2.30773765786598,2.31356555778627,2.31756287220201,
2.32144540522662,2.32614384381588,2.33715087961591,2.44894720632182,2.5774752340157,
2.67388587805365,2.68025247428209,2.68262848223882,2.68424450269457,2.68581142784186,
2.68767951432188,2.69224364650306,2.74067282460147,2.86836179220626,2.99440542087378,
3.07663044854312,3.0856210707495,3.09235955996217,3.09539870362877,3.0976899824399,
3.0998114797624,3.1026983944094,3.10984494589131,3.18724710976461,3.3234455339535,
3.43528251243566,3.48450070172673,3.50722820752353,3.51133755057011,3.51353887845412,
3.51535951598177,3.51720663445849,3.5206354633706,3.53196523777127,3.57280785946028,
3.70178657267434,3.83030678424797,3.92673972889401,3.94394864184916,3.95282829890369,
3.95937563719589,3.96753230187217,3.98126635160781,4.03067859941869,4.03852950046107,
4.07821319859314,4.1939951579044,4.25943941532161,4.26705086177669,4.27087517692903,
4.27363155463765,4.27655745285908,4.28069402265697,4.29331673539156,4.40451960396545,
4.55042695309604,4.5677947601653,4.57577536386716,4.58183807353924,4.58759456358594,
4.5956897185081,4.61758145167919,4.87590566985032,4.9788856913442,5.02579199541689,
5.03100494687026,5.0336272507417,5.03554120493761,5.03759635654019,5.04035902402382,
5.04654081505736,5.13814868412498,5.35684901036038,5.42593205335334,5.43267919995992,
5.43543473533897,5.43747058301688,5.43967985397271,5.44268886356742,5.44958518670571,
5.56854474825664,5.74935865021088,5.7825841352723,5.79748994768594,5.82805126021636,
5.84537470010864,5.85356447532792,5.85584884176459,5.85719941702674,5.85837099742916,
5.85980492261539,5.86253385625708,5.8806626475182,5.92398864901478,5.97913633837282,
6.14508326446712,6.19695932396676,6.24245218713914,6.24824589412459,6.25088032426205,
6.25289404541378,6.25504201828088,6.25838886946113,6.26865441706738,6.32486041346161,
6.37007819592485,6.51717304195755,6.57869895642406,6.5971396361932,6.62540158775356,
6.64983137868104,6.65268563856773,6.65411539495785,6.65516558565209,6.6563030623871,
6.65784786335825,6.6613673856847,6.78306040763654,6.91113060472586,7.06276880506085,
7.07308796367761,7.07665884709422,7.07869144382003,7.0805608844206,7.08308283750937,
7.08784887893496,7.11541533358484,7.14128200980715,7.23600266099889,7.3645336356411,
7.46206803261948,7.46911323842904,7.47160394636142,7.47332526822798,7.47491171580678,
7.47705711388727,7.48112806873204,7.50474857740392,7.55733803551137,7.7887734298149,
7.83801727121392,7.84675394090786,7.85187659955578,7.85575699457646,7.85931865811554,
7.86509484915785,7.88029003323125,7.90186502312458,7.97149602376957,8.09422951602577,
8.19207187906817,8.21474939099986,8.21861894205266,8.22058577526896,8.22212908958517,
8.22384158163449,8.22665672402663,8.23638169109511,8.25214869671166,8.30547477782331,
8.41041806471349,8.61388659578707,8.62734289951141,8.63151489439541,8.63378031166291,
8.63602531746479,8.6387555178748,8.64389753281159,8.67321829032837,8.72373655599779,
8.77479711312779,8.83908782135329,8.89667911150504,9.03614580348131,9.04600034025412,
9.04924834682371,9.05105731419524,9.05288065000309,9.05514287557664,9.0595444188461,
9.08863504615795,9.16146252377471,9.23946999706734,9.35493909019988,9.45736964677849,
9.47836148118326,9.48799961413974,9.49534889681019,9.50209872504978,9.50977756025845,
9.53034451817732,9.60822593396827,9.67004957467597,9.78815339424313,9.80113588441011,
9.80602918058808,9.80894172562362,9.81185242129976,9.8148046621534,9.81859783202482,
9.82469671079591,9.83705628883101,9.95375202500103),.UNSPECIFIED.);
#3573=B_SPLINE_CURVE_WITH_KNOTS('',3,(#228579,#228580,#228581,#228582,#228583,
#228584,#228585,#228586,#228587,#228588,#228589,#228590),.UNSPECIFIED.,
 .F.,.F.,(4,1,1,1,1,1,1,1,1,4),(390.681137751278,391.006606590045,391.505976457976,
392.504716193838,393.5034559297,394.502195665562,395.001565533494,395.500935401425,
396.499675137287,396.964023113174),.UNSPECIFIED.);
#3574=B_SPLINE_CURVE_WITH_KNOTS('',3,(#228592,#228593,#228594,#228595,#228596,
#228597,#228598,#228599,#228600,#228601,#228602,#228603,#228604,#228605,
#228606,#228607,#228608,#228609,#228610,#228611,#228612,#228613,#228614,
#228615,#228616,#228617,#228618,#228619,#228620,#228621,#228622,#228623,
#228624,#228625,#228626,#228627,#228628,#228629,#228630,#228631,#228632,
#228633,#228634,#228635,#228636,#228637,#228638,#228639,#228640,#228641,
#228642,#228643,#228644,#228645,#228646,#228647,#228648,#228649,#228650,
#228651,#228652,#228653,#228654,#228655,#228656,#228657,#228658,#228659,
#228660,#228661,#228662,#228663,#228664,#228665,#228666,#228667,#228668,
#228669,#228670,#228671,#228672,#228673,#228674,#228675,#228676,#228677,
#228678,#228679,#228680,#228681,#228682,#228683,#228684,#228685,#228686,
#228687,#228688,#228689,#228690,#228691,#228692,#228693,#228694,#228695,
#228696,#228697,#228698,#228699,#228700,#228701,#228702,#228703,#228704,
#228705,#228706,#228707,#228708,#228709,#228710,#228711,#228712,#228713,
#228714,#228715,#228716,#228717,#228718,#228719,#228720,#228721,#228722,
#228723,#228724,#228725,#228726,#228727,#228728,#228729,#228730,#228731,
#228732,#228733,#228734,#228735,#228736,#228737,#228738,#228739,#228740,
#228741,#228742,#228743,#228744,#228745,#228746,#228747,#228748,#228749,
#228750,#228751,#228752,#228753,#228754,#228755,#228756,#228757,#228758,
#228759,#228760,#228761,#228762,#228763,#228764,#228765,#228766,#228767,
#228768,#228769,#228770,#228771,#228772,#228773,#228774,#228775,#228776,
#228777,#228778,#228779,#228780,#228781,#228782,#228783,#228784,#228785,
#228786,#228787,#228788,#228789,#228790,#228791,#228792,#228793,#228794,
#228795,#228796,#228797,#228798,#228799,#228800,#228801,#228802,#228803,
#228804,#228805,#228806,#228807,#228808,#228809,#228810,#228811,#228812,
#228813,#228814,#228815,#228816,#228817,#228818,#228819,#228820,#228821,
#228822,#228823,#228824,#228825,#228826,#228827,#228828,#228829,#228830,
#228831,#228832,#228833,#228834,#228835,#228836,#228837,#228838,#228839,
#228840,#228841,#228842,#228843,#228844,#228845,#228846,#228847,#228848,
#228849,#228850,#228851,#228852,#228853,#228854,#228855,#228856,#228857,
#228858,#228859,#228860,#228861,#228862,#228863,#228864,#228865,#228866,
#228867,#228868,#228869,#228870,#228871,#228872,#228873,#228874,#228875,
#228876,#228877,#228878,#228879,#228880,#228881,#228882,#228883,#228884,
#228885,#228886,#228887,#228888,#228889,#228890,#228891,#228892,#228893,
#228894,#228895,#228896,#228897,#228898,#228899,#228900,#228901,#228902,
#228903,#228904,#228905,#228906,#228907,#228908,#228909,#228910,#228911,
#228912,#228913,#228914,#228915,#228916,#228917,#228918,#228919,#228920,
#228921,#228922,#228923,#228924,#228925,#228926,#228927,#228928,#228929,
#228930,#228931,#228932,#228933,#228934,#228935,#228936,#228937,#228938,
#228939,#228940,#228941,#228942,#228943,#228944,#228945,#228946,#228947,
#228948,#228949,#228950,#228951,#228952,#228953,#228954,#228955,#228956,
#228957,#228958,#228959,#228960,#228961,#228962,#228963,#228964,#228965,
#228966,#228967,#228968,#228969,#228970,#228971,#228972,#228973,#228974,
#228975,#228976,#228977,#228978,#228979,#228980,#228981,#228982,#228983,
#228984,#228985,#228986,#228987,#228988,#228989,#228990,#228991,#228992,
#228993,#228994,#228995,#228996,#228997,#228998,#228999,#229000,#229001,
#229002,#229003,#229004,#229005,#229006,#229007,#229008,#229009,#229010,
#229011,#229012,#229013,#229014,#229015,#229016,#229017,#229018,#229019,
#229020,#229021,#229022,#229023,#229024,#229025,#229026,#229027,#229028,
#229029,#229030,#229031,#229032,#229033,#229034,#229035,#229036,#229037,
#229038,#229039,#229040,#229041,#229042,#229043,#229044,#229045,#229046,
#229047,#229048,#229049,#229050,#229051,#229052,#229053,#229054,#229055,
#229056,#229057,#229058,#229059,#229060,#229061,#229062,#229063,#229064,
#229065,#229066,#229067,#229068,#229069,#229070,#229071),.UNSPECIFIED.,
 .F.,.F.,(4,2,2,2,2,2,2,2,2,2,2,2,2,2,2,2,2,2,2,2,2,2,2,2,2,2,2,2,2,2,2,
2,2,2,2,2,2,2,2,2,2,2,2,2,2,2,2,2,2,2,2,2,2,2,2,2,2,2,2,2,2,2,2,2,2,2,2,
2,2,2,2,2,2,2,2,2,2,2,2,2,2,2,2,2,2,2,2,2,2,2,2,2,2,2,2,2,2,2,2,2,2,2,2,
2,2,2,2,2,2,2,2,2,2,2,2,2,2,2,2,2,2,2,2,2,2,2,2,2,2,2,2,2,2,2,2,2,2,2,2,
2,2,2,2,2,2,2,2,2,2,2,2,2,2,2,2,2,2,2,2,2,2,2,2,2,2,2,2,2,2,2,2,2,2,2,2,
2,2,2,2,2,2,2,2,2,2,2,2,2,2,2,2,2,2,2,2,2,2,2,2,2,2,2,2,2,2,2,2,2,2,2,2,
2,2,2,2,2,2,2,2,2,2,2,2,2,2,2,2,2,2,2,2,2,2,2,2,2,2,2,2,4),(0.00169205085482047,
0.0516099663871825,0.0798090565293214,0.0891707982109067,0.096340521663136,
0.103370345146304,0.110316766529791,0.122039124148549,0.154045623255705,
0.199450145104775,0.353781929219954,0.403283886548112,0.409093062442713,
0.412849415832662,0.415805636931924,0.418561124198566,0.421491016970439,
0.425641897335404,0.438363213028286,0.554983080822192,0.638713628781982,
0.68090256455011,0.699476433871832,0.714050513036348,0.721456710782671,
0.727315814748324,0.734047324736872,0.745313900310716,0.785114221009155,
1.00357245087222,1.04761250334487,1.13942944891135,1.17198906773006,1.1768543131915,
1.17935968392888,1.18138158373093,1.18338972935964,1.18700192890167,1.19801217960724,
1.34975889907847,1.45789445194702,1.56823039798511,1.57681266588377,1.58010115173553,
1.58236505154398,1.58458147064734,1.58725038594849,1.59390271461916,1.65396136578439,
1.76932457583323,1.87446507875747,1.96820307840433,1.99687870674681,1.99999355308001,
2.00150729794154,2.00257739143659,2.00369324071564,2.00523466152933,2.00920649664411,
2.06822484936667,2.16043087939128,2.24455315911634,2.33601800746862,2.38259425680721,
2.38868310746353,2.39352068023074,2.3959951439471,2.3977944652624,2.39971754566394,
2.40301136705745,2.41201730801419,2.54599334559463,2.68860124462997,2.74644694630033,
2.78992843393922,2.796780015887,2.79875986784698,2.79998442182562,2.80110961256146,
2.80254968195062,2.80559215980666,2.82575592392835,2.94230832732665,3.04325453255975,
3.13297422592285,3.1877040790232,3.21579561287667,3.22058845230548,3.22311697265912,
3.22498809850428,3.22701940325989,3.22996143505291,3.2382979667065,3.36691408924803,
3.53002676926141,3.56006497810949,3.60519250149703,3.61396440857074,3.61688695375515,
3.61877959428914,3.62056630268876,3.62292214983633,3.62692545398737,3.65229271754626,
3.86288736341471,3.96882935111336,3.98889605681299,3.99546087660878,3.99961881417096,
4.00348508343925,4.00850549666663,4.01944267341708,4.11556215359659,4.24926291488605,
4.35883983892365,4.36375999285221,4.3659022883867,4.36747353595603,4.36891989842782,
4.37087516544998,4.37565165326645,4.44129639557311,4.53439098440493,4.6159743625376,
4.76440532157646,4.77399485349962,4.77763015256483,4.77978944611996,4.78183404615547,
4.78468444478042,4.79039692381932,4.83528978497999,4.90567479643752,5.02894123160039,
5.18197858425998,5.19177283842955,5.19500209179651,5.19680085854632,5.19861405584541,
5.20086391275691,5.20524199459982,5.23471931015002,5.31145832329827,5.4822875129227,
5.59765658539371,5.6200898725517,5.62920955406716,5.63667764823094,5.64425562432676,
5.65525977505159,5.68478217560014,5.70912829025556,5.79856907016586,5.93369004963465,
5.94669266683466,5.95147818627327,5.95465323394181,5.95765913623308,5.96173914461121,
5.97127653124005,5.98490766243149,6.18360091571373,6.24212040727959,6.25349825754496,
6.26078910284963,6.26659972486131,6.2731652238429,6.28431050105973,6.33098608008638,
6.42812006358124,6.63880564684559,6.65298822910695,6.68475963113383,6.70983956493742,
6.71423093404109,6.71688453325539,6.71893923076202,6.72098015170416,6.72429580549374,
6.72809487812411,6.73506101182642,6.78987042190301,6.88957101610736,6.96524381164446,
7.10296469311381,7.11207099643112,7.11553065717512,7.11758779122784,7.11953704145349,
7.12225667141412,7.12771491975124,7.17091031333986,7.23834425990563,7.33122250358557,
7.42268257061352,7.52922124307661,7.53627501946933,7.53843568540303,7.53960298146341,
7.54075560770922,7.54215143854955,7.54471007200515,7.55924933355297,7.58824594726097,
7.64636410566151,7.70209763132859,7.81776208415526,7.93142598930088,7.93850332430317,
7.94115271053839,7.9430305681646,7.9447991813057,7.94724964662972,7.95210507907004,
7.98766888158887,8.07638244655228,8.14951401847776,8.21967654325857,8.33350159578396,
8.3406609092546,8.34285561667671,8.34404942846161,8.34523388079835,8.34667583364257,
8.34821027262679,8.35479519898447,8.41406181631397,8.4537309150801,8.48980483970088,
8.65051319258309,8.66039397517519,8.7497739496824,8.75708535369838,8.75996830340157,
8.76206218250745,8.76430035290099,8.76728933837661,8.77389280438359,8.91007170909831,
9.06691452272662),.UNSPECIFIED.);
#3575=B_SPLINE_CURVE_WITH_KNOTS('',3,(#229075,#229076,#229077,#229078,#229079,
#229080,#229081,#229082,#229083,#229084,#229085,#229086,#229087,#229088,
#229089,#229090,#229091,#229092,#229093,#229094,#229095,#229096,#229097,
#229098,#229099,#229100,#229101,#229102,#229103,#229104,#229105,#229106,
#229107,#229108,#229109,#229110,#229111,#229112,#229113,#229114,#229115,
#229116,#229117,#229118,#229119,#229120,#229121,#229122,#229123,#229124,
#229125,#229126,#229127,#229128,#229129,#229130,#229131,#229132,#229133,
#229134,#229135,#229136,#229137,#229138,#229139,#229140,#229141,#229142,
#229143,#229144,#229145,#229146,#229147,#229148,#229149,#229150,#229151,
#229152,#229153,#229154,#229155,#229156,#229157,#229158,#229159,#229160,
#229161,#229162,#229163,#229164,#229165,#229166,#229167,#229168,#229169,
#229170,#229171,#229172,#229173,#229174,#229175,#229176,#229177,#229178,
#229179,#229180,#229181,#229182,#229183,#229184,#229185,#229186,#229187,
#229188,#229189,#229190,#229191,#229192,#229193,#229194,#229195,#229196,
#229197,#229198,#229199,#229200,#229201,#229202,#229203,#229204,#229205,
#229206,#229207,#229208,#229209,#229210,#229211,#229212,#229213,#229214,
#229215,#229216,#229217,#229218,#229219,#229220,#229221,#229222,#229223,
#229224,#229225,#229226,#229227,#229228,#229229,#229230,#229231,#229232,
#229233,#229234,#229235,#229236,#229237,#229238,#229239,#229240,#229241,
#229242,#229243,#229244,#229245,#229246),.UNSPECIFIED.,.F.,.F.,(4,3,3,3,
3,3,3,3,3,3,3,3,3,3,3,3,3,3,3,3,3,3,3,3,3,3,3,3,3,3,3,3,3,3,3,3,3,3,3,3,
3,3,3,3,3,3,3,3,3,3,3,3,3,3,3,3,3,4),(-410.482031439357,-410.40051557623,
-410.318975660214,-410.234897138017,-410.153354592523,-410.068008081974,
-409.982661571426,-409.908581990859,-409.834525645462,-409.760479759459,
-409.686410655311,-409.612330240246,-409.538194979741,-409.483291703495,
-409.39912997051,-409.314950786704,-409.230830079807,-409.14678551264,-409.062932700955,
-408.983921835564,-408.908993513659,-408.834071857824,-408.759144941605,
-408.684173917891,-408.609179509688,-408.534115640984,-408.484551967633,
-408.409077454774,-408.333661595445,-408.258291743711,-408.182955284671,
-408.107639626691,-408.029911202326,-407.954580371603,-407.879231192739,
-407.803852246168,-407.728432097994,-407.652921369643,-407.57735703147,
-407.501693797513,-407.485812231771,-407.412829970114,-407.339936403889,
-407.26711651233,-407.194355349297,-407.121638026441,-407.048949698084,
-406.976261565061,-406.90356994441,-406.830861420205,-406.758122564272,
-406.685296111268,-406.612422218906,-406.539435187989,-406.487072495908,
-406.38181871027,-406.280243949839,-406.216790079623),.UNSPECIFIED.);
#3576=B_SPLINE_CURVE_WITH_KNOTS('',3,(#229248,#229249,#229250,#229251,#229252,
#229253,#229254,#229255,#229256,#229257,#229258,#229259,#229260,#229261,
#229262,#229263,#229264,#229265),.UNSPECIFIED.,.F.,.F.,(4,2,2,2,2,2,2,2,
4),(-406.216790079623,-405.381873167729,-404.546956255834,-403.712039343939,
-402.877122432044,-402.042205520149,-401.207288608255,-400.37237169636,
-399.933604772444),.UNSPECIFIED.);
#3577=B_SPLINE_CURVE_WITH_KNOTS('',3,(#229267,#229268,#229269,#229270,#229271,
#229272,#229273,#229274,#229275,#229276,#229277,#229278,#229279,#229280,
#229281,#229282,#229283,#229284,#229285,#229286,#229287,#229288,#229289,
#229290,#229291,#229292,#229293,#229294,#229295,#229296,#229297,#229298,
#229299,#229300,#229301,#229302,#229303,#229304,#229305,#229306,#229307,
#229308,#229309,#229310,#229311,#229312,#229313,#229314,#229315,#229316,
#229317,#229318,#229319,#229320,#229321,#229322,#229323,#229324,#229325,
#229326,#229327,#229328,#229329,#229330,#229331,#229332,#229333,#229334,
#229335,#229336,#229337,#229338,#229339,#229340,#229341,#229342,#229343,
#229344,#229345,#229346,#229347,#229348,#229349,#229350,#229351,#229352,
#229353,#229354,#229355,#229356,#229357,#229358,#229359,#229360,#229361,
#229362,#229363,#229364,#229365,#229366,#229367,#229368,#229369,#229370,
#229371,#229372,#229373,#229374,#229375,#229376,#229377,#229378,#229379,
#229380,#229381,#229382,#229383,#229384,#229385,#229386,#229387,#229388,
#229389,#229390,#229391,#229392,#229393,#229394,#229395,#229396,#229397,
#229398,#229399,#229400,#229401,#229402,#229403,#229404,#229405,#229406,
#229407,#229408,#229409,#229410,#229411,#229412,#229413,#229414,#229415,
#229416,#229417,#229418,#229419,#229420,#229421,#229422,#229423,#229424,
#229425,#229426,#229427,#229428,#229429,#229430,#229431,#229432,#229433,
#229434,#229435,#229436,#229437,#229438,#229439,#229440,#229441,#229442,
#229443,#229444,#229445,#229446,#229447,#229448,#229449,#229450,#229451,
#229452,#229453,#229454,#229455,#229456,#229457,#229458,#229459,#229460,
#229461,#229462,#229463,#229464,#229465,#229466,#229467,#229468,#229469,
#229470,#229471,#229472,#229473,#229474,#229475,#229476,#229477,#229478,
#229479,#229480,#229481,#229482,#229483,#229484,#229485,#229486,#229487,
#229488,#229489,#229490,#229491,#229492,#229493,#229494,#229495,#229496,
#229497,#229498,#229499,#229500,#229501,#229502,#229503,#229504,#229505,
#229506,#229507,#229508,#229509,#229510,#229511,#229512,#229513,#229514,
#229515,#229516,#229517,#229518,#229519,#229520,#229521,#229522,#229523,
#229524,#229525,#229526,#229527,#229528,#229529,#229530,#229531,#229532,
#229533,#229534,#229535,#229536,#229537,#229538,#229539,#229540,#229541,
#229542,#229543,#229544,#229545,#229546,#229547,#229548,#229549,#229550,
#229551,#229552,#229553,#229554,#229555,#229556,#229557,#229558,#229559,
#229560,#229561,#229562,#229563,#229564,#229565,#229566,#229567,#229568,
#229569,#229570,#229571,#229572,#229573,#229574,#229575,#229576,#229577,
#229578,#229579,#229580,#229581,#229582,#229583,#229584,#229585,#229586,
#229587,#229588,#229589,#229590,#229591,#229592,#229593,#229594,#229595,
#229596,#229597,#229598,#229599,#229600,#229601,#229602,#229603,#229604,
#229605,#229606,#229607,#229608,#229609,#229610,#229611,#229612,#229613,
#229614,#229615,#229616,#229617,#229618,#229619,#229620,#229621,#229622,
#229623,#229624,#229625,#229626,#229627,#229628,#229629,#229630,#229631,
#229632,#229633,#229634,#229635,#229636,#229637,#229638,#229639,#229640,
#229641,#229642,#229643,#229644,#229645,#229646,#229647,#229648,#229649,
#229650,#229651,#229652,#229653,#229654,#229655,#229656,#229657,#229658,
#229659,#229660,#229661,#229662,#229663,#229664,#229665,#229666,#229667,
#229668,#229669,#229670,#229671,#229672,#229673,#229674,#229675,#229676,
#229677,#229678,#229679,#229680,#229681,#229682,#229683,#229684,#229685,
#229686,#229687,#229688,#229689,#229690,#229691,#229692,#229693,#229694,
#229695,#229696,#229697,#229698,#229699,#229700,#229701,#229702,#229703,
#229704,#229705,#229706,#229707,#229708,#229709,#229710,#229711,#229712,
#229713,#229714,#229715,#229716,#229717,#229718,#229719,#229720,#229721,
#229722,#229723,#229724,#229725,#229726,#229727,#229728,#229729,#229730,
#229731,#229732,#229733,#229734,#229735,#229736,#229737,#229738,#229739,
#229740,#229741,#229742,#229743,#229744,#229745,#229746,#229747,#229748,
#229749,#229750,#229751,#229752,#229753,#229754,#229755,#229756,#229757,
#229758,#229759,#229760,#229761,#229762,#229763,#229764,#229765,#229766,
#229767,#229768,#229769,#229770,#229771,#229772,#229773,#229774,#229775,
#229776,#229777,#229778,#229779,#229780,#229781,#229782,#229783,#229784,
#229785,#229786,#229787,#229788,#229789,#229790),.UNSPECIFIED.,.F.,.F.,
(4,2,2,2,2,2,2,2,2,2,2,2,2,2,2,2,2,2,2,2,2,2,2,2,2,2,2,2,2,2,2,2,2,2,2,
2,2,2,2,2,2,2,2,2,2,2,2,2,2,2,2,2,2,2,2,2,2,2,2,2,2,2,2,2,2,2,2,2,2,2,2,
2,2,2,2,2,2,2,2,2,2,2,2,2,2,2,2,2,2,2,2,2,2,2,2,2,2,2,2,2,2,2,2,2,2,2,2,
2,2,2,2,2,2,2,2,2,2,2,2,2,2,2,2,2,2,2,2,2,2,2,2,2,2,2,2,2,2,2,2,2,2,2,2,
2,2,2,2,2,2,2,2,2,2,2,2,2,2,2,2,2,2,2,2,2,2,2,2,2,2,2,2,2,2,2,2,2,2,2,2,
2,2,2,2,2,2,2,2,2,2,2,2,2,2,2,2,2,2,2,2,2,2,2,2,2,2,2,2,2,2,2,2,2,2,2,2,
2,2,2,2,2,2,2,2,2,2,2,2,2,2,2,2,2,2,2,2,2,2,2,2,2,2,2,2,2,2,2,2,2,2,2,2,
2,2,2,2,2,2,2,2,2,2,4),(0.0019992779279493,0.297228947054352,0.343206093336844,
0.3503282603909,0.352397935254475,0.353685501401623,0.3548647364931,0.356368710625501,
0.359526680001281,0.379983031318882,0.437800654898626,0.662665731018093,
0.715324353514643,0.748059636914255,0.760178068514997,0.768681673569802,
0.771949177383266,0.773969505821607,0.776163649489694,0.779054042805263,
0.785493405937425,0.839378339458817,0.921165257031632,0.973737674056047,
1.07403941840921,1.16448437909037,1.17121208842534,1.17406815400539,1.17613626449919,
1.17802306984809,1.18054909299143,1.18698989681943,1.29134835881228,1.32664915232754,
1.5997870143185,1.61836009401939,1.62653740906363,1.63261932489516,1.63891506645648,
1.64845069124845,1.67491640221799,1.85513197443603,1.90521009723151,1.92961637905726,
1.93513577982862,1.93848848843592,1.94153997204339,1.945475034328,1.95366711626696,
2.04401426136949,2.15307738077737,2.20282768142618,2.22468886393581,2.24207184232718,
2.25098865782536,2.25815829891227,2.26647546151626,2.28041334313099,2.33806240139658,
2.46055436802008,2.56649374416049,2.65783257485772,2.68983765934622,2.69431446185873,
2.69659007143058,2.69823903237573,2.69999636981616,2.7029953116031,2.71112778664773,
2.82658707030246,2.97984819749147,3.10018735797163,3.10637899983089,3.111348953454,
3.11402616316939,3.11626779025475,3.11886248164798,3.12327724801515,3.13937901070979,
3.39409515319172,3.45553455445926,3.51476141191506,3.52403085918468,3.52677149118404,
3.5284655787969,3.53001012201323,3.53200346106441,3.53614635902375,3.56357680677665,
3.57435733283979,3.58122904603894,3.58535026835805,3.58798373417945,3.74373595078643,
3.87546299879015,3.8873506421484,3.89259351518159,3.89647413767126,3.90007758010477,
3.90500423106867,3.91723138207572,4.08177131512006,4.20291119356008,4.24874216888675,
4.2701361636558,4.27407269269763,4.27618726296623,4.27792247886036,4.27996337786905,
4.28346682811556,4.29654384927286,4.53606304052704,4.59397590020799,4.64991898865479,
4.66525389452868,4.66922646203589,4.67157209062458,4.67364178030088,4.67622061745384,
4.68019127104281,4.69805679702972,4.98308190961803,5.08671613173766,5.09343687248634,
5.09551069425155,5.09663440683052,5.09774609515131,5.09909598980325,5.10167893502373,
5.11777829779163,5.1530080125434,5.21162561518377,5.40110282176406,5.48881648253929,
5.49555928488173,5.49817965419276,5.50006956882661,5.50207734004741,5.50473747379003,
5.51052916903007,5.60198522323136,5.70535856844502,5.75068322388203,5.80504227161934,
5.88711162687489,5.89211316909507,5.89380229969992,5.89495716783776,5.89601199595674,
5.89742402012768,5.90005588350536,5.91433289653597,5.94332463672421,5.99885041524903,
6.15764280351359,6.29966959544904,6.30942061895616,6.31299566695155,6.31508546967096,
6.31704247654236,6.31973651220617,6.32501318429958,6.36139058804319,6.45783807932016,
6.64126789772151,6.70721010371304,6.71317789432634,6.71586853547409,6.71791682725447,
6.72009390011982,6.72340330868569,6.73300407796326,6.78888707700809,6.91051973628635,
7.13545141826491,7.1577854348511,7.16593365678988,7.17169801146943,7.17774215403553,
7.18549655191127,7.20155886401366,7.22269298063199,7.27339432600211,7.37440708273428,
7.46791276261557,7.47534205621098,7.47905704995501,7.48208809077319,7.48536793971601,
7.49106782448146,7.49801744753919,7.5121595850515,7.55102878833044,7.68100662035085,
7.72011479218897,7.77224585818453,7.78621867100486,7.79441832452067,7.80160446698084,
7.810518651449,7.82767807427143,7.85054727836261,7.90668179587075,8.18684462456534,
8.19349108776987,8.20179636992428,8.23183535612473,8.23655325343509,8.23891140316971,
8.24074322508187,8.24275733182213,8.24481927279615,8.25129390476362,8.2602350460732,
8.28287732060411,8.31752193756336,8.41819280867382,8.4970593059251,8.64193316334752,
8.65158179498022,8.65522208733346,8.65737937709897,8.65941880359651,8.66225676051235,
8.66792519488908,8.71157596324893,8.82699719722926,8.9192282925171,8.96002475289104,
9.02690261667247,9.06363893165391,9.06749441673257,9.06946196239184,9.07090904721298,
9.07247303579576,9.07459116081652,9.07693165309151,9.09203175909149,9.12148023812957,
9.19951570275614,9.27169365400701,9.41823718439555,9.42978126939524,9.43444335739657,
9.4383364264765,9.44233870547363,9.44637124726198,9.45199548384072,9.48261243362604,
9.57513842185726,9.60500204001224,9.63839687086317,9.78932144734067,9.81185821182605,
9.81571034804602,9.81801999060946,9.81979676672897,9.82170336747785,9.8236421588566,
9.82643033046538,9.83123731522428,9.96237951771243),.UNSPECIFIED.);
#3578=B_SPLINE_CURVE_WITH_KNOTS('',3,(#229792,#229793,#229794,#229795,#229796,
#229797,#229798,#229799,#229800,#229801,#229802,#229803,#229804,#229805,
#229806,#229807,#229808,#229809,#229810,#229811,#229812,#229813,#229814,
#229815,#229816,#229817,#229818,#229819,#229820,#229821,#229822,#229823,
#229824,#229825,#229826,#229827,#229828,#229829,#229830,#229831,#229832,
#229833,#229834,#229835,#229836,#229837,#229838,#229839,#229840,#229841,
#229842,#229843,#229844,#229845,#229846,#229847,#229848,#229849,#229850,
#229851,#229852,#229853,#229854,#229855,#229856,#229857,#229858,#229859,
#229860,#229861,#229862,#229863,#229864,#229865,#229866,#229867,#229868,
#229869,#229870,#229871,#229872,#229873,#229874,#229875,#229876,#229877,
#229878,#229879,#229880,#229881,#229882,#229883,#229884,#229885,#229886,
#229887,#229888,#229889,#229890,#229891,#229892,#229893,#229894,#229895,
#229896,#229897,#229898,#229899,#229900,#229901,#229902,#229903,#229904,
#229905,#229906,#229907,#229908,#229909,#229910,#229911,#229912,#229913,
#229914,#229915,#229916,#229917,#229918,#229919,#229920,#229921,#229922,
#229923,#229924,#229925,#229926,#229927,#229928,#229929,#229930,#229931,
#229932,#229933,#229934,#229935,#229936,#229937,#229938,#229939,#229940,
#229941,#229942,#229943,#229944,#229945,#229946,#229947,#229948,#229949,
#229950,#229951,#229952,#229953,#229954,#229955,#229956,#229957,#229958,
#229959,#229960,#229961,#229962,#229963,#229964,#229965,#229966,#229967,
#229968,#229969,#229970,#229971,#229972,#229973,#229974,#229975,#229976,
#229977,#229978,#229979,#229980,#229981,#229982,#229983,#229984,#229985,
#229986,#229987,#229988,#229989,#229990,#229991,#229992,#229993,#229994,
#229995,#229996,#229997,#229998,#229999,#230000,#230001,#230002,#230003,
#230004,#230005,#230006,#230007,#230008,#230009,#230010,#230011,#230012,
#230013,#230014,#230015,#230016,#230017,#230018,#230019,#230020,#230021,
#230022,#230023,#230024,#230025,#230026,#230027,#230028,#230029,#230030,
#230031,#230032,#230033,#230034,#230035,#230036,#230037,#230038,#230039,
#230040,#230041,#230042,#230043,#230044,#230045,#230046,#230047,#230048,
#230049,#230050),.UNSPECIFIED.,.F.,.F.,(4,3,3,3,3,3,3,3,3,3,3,3,3,3,3,3,
3,3,3,3,3,3,3,3,3,3,3,3,3,3,3,3,3,3,3,3,3,3,3,3,3,3,3,3,3,3,3,3,3,3,3,3,
3,3,3,3,3,3,3,3,3,3,3,3,3,3,3,3,3,3,3,3,3,3,3,3,3,3,3,3,3,3,3,3,3,3,4),
(-387.367234158085,-387.293462939457,-387.219749263725,-387.146078733845,
-387.07243698482,-386.998797021076,-386.92515438306,-386.851496085639,-386.777809136646,
-386.704040445516,-386.630226409719,-386.556308537467,-386.512277778665,
-386.439138834976,-386.366087917664,-386.293110093637,-386.220190499117,
-386.147314324136,-386.07446679855,-386.001619301385,-385.928768152842,
-385.855900003737,-385.783001493679,-385.710016052112,-385.636983239331,
-385.563838815208,-385.513538042803,-385.438009754137,-385.362567558804,
-385.28719855111,-385.211889873148,-385.136628706748,-385.058899906772,
-384.983689709447,-384.908485484749,-384.833275674485,-384.758048719499,
-384.68276582989,-384.60744978302,-384.532062873763,-384.51479830694,-384.438206406543,
-384.361679704606,-384.285208508718,-384.208791648461,-384.13240760963,
-384.056047446221,-384.015428439009,-383.937309170526,-383.859144867048,
-383.780930790054,-383.702625667362,-383.624272240758,-383.545833150988,
-383.516058571078,-383.434079792495,-383.352173043258,-383.268301958231,
-383.18663654572,-383.101662624433,-383.016688703147,-382.94307702904,-382.869470662186,
-382.795856610283,-382.722190317753,-382.648496789728,-382.574721316661,
-382.517318835216,-382.44081811041,-382.364373343229,-382.287973623649,
-382.211608074043,-382.135265841853,-382.05817999904,-381.981838185664,
-381.905486098022,-381.829113873915,-381.751480180275,-381.675008503282,
-381.596793801318,-381.518579099354,-381.442494174995,-381.366503409665,
-381.290623633396,-381.214808144098,-381.139062747223,-381.084048850905),
 .UNSPECIFIED.);
#3579=B_SPLINE_CURVE_WITH_KNOTS('',3,(#230052,#230053,#230054,#230055,#230056,
#230057,#230058,#230059,#230060,#230061,#230062,#230063,#230064,#230065,
#230066,#230067,#230068,#230069,#230070,#230071,#230072,#230073,#230074,
#230075,#230076,#230077,#230078,#230079,#230080,#230081,#230082,#230083,
#230084,#230085,#230086,#230087,#230088,#230089,#230090,#230091,#230092,
#230093,#230094,#230095,#230096,#230097,#230098,#230099,#230100,#230101,
#230102,#230103,#230104,#230105,#230106,#230107,#230108,#230109,#230110,
#230111,#230112,#230113,#230114,#230115,#230116,#230117,#230118,#230119,
#230120,#230121,#230122,#230123,#230124,#230125,#230126,#230127,#230128,
#230129,#230130,#230131,#230132,#230133,#230134,#230135,#230136,#230137,
#230138,#230139,#230140,#230141,#230142,#230143,#230144,#230145,#230146,
#230147,#230148,#230149,#230150,#230151,#230152,#230153,#230154,#230155,
#230156,#230157,#230158,#230159,#230160,#230161,#230162,#230163,#230164,
#230165,#230166,#230167,#230168,#230169,#230170,#230171,#230172,#230173,
#230174,#230175,#230176,#230177,#230178,#230179,#230180,#230181,#230182,
#230183,#230184,#230185,#230186,#230187,#230188,#230189,#230190,#230191,
#230192,#230193,#230194,#230195,#230196,#230197,#230198,#230199,#230200,
#230201,#230202,#230203,#230204,#230205,#230206,#230207,#230208,#230209,
#230210,#230211,#230212,#230213,#230214,#230215,#230216,#230217,#230218,
#230219,#230220,#230221,#230222,#230223,#230224,#230225,#230226,#230227,
#230228,#230229,#230230,#230231,#230232,#230233,#230234,#230235,#230236,
#230237,#230238,#230239,#230240,#230241,#230242,#230243,#230244,#230245,
#230246,#230247,#230248,#230249,#230250,#230251,#230252,#230253,#230254,
#230255,#230256,#230257,#230258,#230259,#230260,#230261,#230262,#230263,
#230264,#230265,#230266,#230267,#230268,#230269,#230270,#230271,#230272,
#230273,#230274,#230275,#230276,#230277,#230278,#230279,#230280,#230281,
#230282,#230283,#230284,#230285,#230286,#230287,#230288,#230289,#230290,
#230291,#230292,#230293,#230294,#230295,#230296,#230297,#230298,#230299,
#230300,#230301,#230302,#230303,#230304,#230305,#230306,#230307,#230308,
#230309,#230310,#230311,#230312,#230313,#230314,#230315,#230316,#230317,
#230318,#230319,#230320,#230321,#230322,#230323,#230324,#230325,#230326,
#230327,#230328,#230329,#230330,#230331,#230332,#230333,#230334,#230335,
#230336,#230337,#230338,#230339,#230340,#230341,#230342,#230343,#230344,
#230345,#230346,#230347,#230348,#230349,#230350,#230351,#230352,#230353,
#230354,#230355,#230356,#230357,#230358,#230359,#230360,#230361,#230362,
#230363,#230364,#230365,#230366,#230367,#230368,#230369,#230370,#230371,
#230372,#230373,#230374,#230375,#230376,#230377,#230378,#230379,#230380,
#230381,#230382,#230383,#230384,#230385,#230386,#230387,#230388,#230389,
#230390,#230391,#230392,#230393,#230394,#230395,#230396,#230397,#230398,
#230399,#230400,#230401,#230402,#230403,#230404,#230405,#230406,#230407,
#230408,#230409,#230410,#230411,#230412,#230413,#230414,#230415,#230416,
#230417,#230418,#230419,#230420,#230421,#230422,#230423,#230424,#230425,
#230426,#230427,#230428,#230429,#230430,#230431,#230432,#230433,#230434,
#230435,#230436,#230437,#230438,#230439,#230440,#230441,#230442,#230443,
#230444,#230445,#230446,#230447,#230448,#230449,#230450,#230451,#230452,
#230453,#230454,#230455,#230456,#230457,#230458,#230459,#230460,#230461,
#230462,#230463,#230464,#230465,#230466,#230467,#230468,#230469,#230470,
#230471,#230472,#230473,#230474,#230475,#230476,#230477,#230478,#230479,
#230480,#230481,#230482,#230483,#230484,#230485,#230486,#230487,#230488,
#230489,#230490,#230491,#230492,#230493,#230494,#230495,#230496,#230497,
#230498,#230499,#230500,#230501,#230502,#230503,#230504,#230505,#230506,
#230507,#230508,#230509,#230510,#230511,#230512,#230513,#230514,#230515,
#230516,#230517,#230518,#230519,#230520,#230521,#230522,#230523,#230524,
#230525,#230526,#230527,#230528,#230529,#230530,#230531,#230532,#230533,
#230534,#230535,#230536,#230537,#230538,#230539,#230540,#230541,#230542,
#230543,#230544,#230545,#230546,#230547,#230548,#230549,#230550,#230551,
#230552,#230553,#230554,#230555,#230556,#230557,#230558,#230559,#230560,
#230561,#230562,#230563,#230564,#230565,#230566,#230567,#230568,#230569,
#230570,#230571,#230572,#230573,#230574,#230575,#230576,#230577,#230578,
#230579,#230580,#230581,#230582,#230583,#230584,#230585,#230586,#230587),
 .UNSPECIFIED.,.F.,.F.,(4,2,2,2,2,2,2,2,2,2,2,2,2,2,2,2,2,2,2,2,2,2,2,2,
2,2,2,2,2,2,2,2,2,2,2,2,2,2,2,2,2,2,2,2,2,2,2,2,2,2,2,2,2,2,2,2,2,2,2,2,
2,2,2,2,2,2,2,2,2,2,2,2,2,2,2,2,2,2,2,2,2,2,2,2,2,2,2,2,2,2,2,2,2,2,2,2,
2,2,2,2,2,2,2,2,2,2,2,2,2,2,2,2,2,2,2,2,2,2,2,2,2,2,2,2,2,2,2,2,2,2,2,2,
2,2,2,2,2,2,2,2,2,2,2,2,2,2,2,2,2,2,2,2,2,2,2,2,2,2,2,2,2,2,2,2,2,2,2,2,
2,2,2,2,2,2,2,2,2,2,2,2,2,2,2,2,2,2,2,2,2,2,2,2,2,2,2,2,2,2,2,2,2,2,2,2,
2,2,2,2,2,2,2,2,2,2,2,2,2,2,2,2,2,2,2,2,2,2,2,2,2,2,2,2,2,2,2,2,2,2,2,2,
2,2,2,2,2,2,2,2,2,2,2,2,2,2,2,2,2,2,2,2,2,2,2,2,2,2,2,4),(0.00136196530955085,
0.0236124556839763,0.0292659071113713,0.0333084640585915,0.03686252960954,
0.0406110068832381,0.0455738782555038,0.0562154239113908,0.0811176318447605,
0.331754615019365,0.386990162446628,0.411821203394026,0.415919343847642,
0.418067990451346,0.419820968232722,0.421839306700059,0.425247464787378,
0.437413270522316,0.618850537864965,0.675078510992058,0.751521043042145,
0.78695949380261,0.799638694305315,0.805533128507329,0.810278664031603,
0.812793239586447,0.814658691310162,0.816688399968935,0.820258021300029,
0.830598030662721,0.987769148384333,1.06460698171212,1.07436405361475,1.0856285243643,
1.11869579464937,1.17776687034043,1.22687328611878,1.23431620079812,1.23637958406761,
1.23762535416216,1.23874181795397,1.24015764158288,1.24241835223426,1.25409173095658,
1.45080428958484,1.51263164120352,1.58290728550593,1.61573032191407,1.62761190169168,
1.6331722370948,1.63762775506656,1.64003739605459,1.64182525262976,1.64377075150026,
1.64659637438564,1.65465439129887,1.78022263044505,1.9257462280367,1.94732001714936,
1.97689088139107,2.02499312575702,2.03231168265478,2.03440072306649,2.03569249340056,
2.03687034472446,2.03839035470773,2.0415478409083,2.06200134288342,2.21603159948904,
2.30008997083458,2.39102491668349,2.44033203172534,2.4468575824038,2.45205849979095,
2.45473623495933,2.45669059933914,2.4587862938115,2.46177763666948,2.46997709768255,
2.59804147266279,2.75498467654587,2.84632380395221,2.85306703717984,2.85592580350572,
2.8579944293996,2.85988071536277,2.86240457163804,2.86883176248918,2.95647887874079,
3.1553576752948,3.28668265609071,3.30169217464577,3.30920307279823,3.31462902464923,
3.32041336830083,3.33033597675164,3.35816721206757,3.39130941156882,3.53793166220926,
3.58693863800192,3.61100399089153,3.61650029836134,3.6198481238142,3.6229005346247,
3.62684437802611,3.63508246966176,3.71605282590116,3.78962674125273,3.89624006654166,
3.92007374651435,3.93017952969019,3.93756885727421,3.94439560498426,3.95372200436719,
3.97749884868377,4.18380905148408,4.30799040526486,4.36108159670524,4.3691519382429,
4.37504851788863,4.37759514899182,4.37945554635735,4.38116298809323,4.3834637948443,
4.38905029117079,4.4517122648304,4.64304984568877,4.71832975067706,4.77897813507876,
4.79021393804593,4.79394938264702,4.79636615937359,4.79864591963759,4.80164893488286,
4.80833883161805,4.86430167055103,4.97949568178559,5.19214041517499,5.20435864780263,
5.20748027517295,5.20927806586203,5.21065567300716,5.21243312294419,5.21554859833586,
5.22899736664495,5.35655949478621,5.46976260595272,5.55814447031661,5.56887165372405,
5.57384468777813,5.5776952059052,5.58185676427516,5.58847117190765,5.60900897955343,
5.71921882760491,5.90552851287311,5.92623721278161,5.95031689459131,5.95425040163329,
5.95658337968545,5.95836328899277,5.96025888333169,5.9632067183965,5.97220916524013,
6.13376393631706,6.33303116735921,6.34464228060622,6.34892983509415,6.35160610321291,
6.35368616361993,6.35597395612439,6.35968904765886,6.37238250886363,6.44881917279999,
6.53791359041877,6.72231983745179,6.77067658576297,6.77446759438621,6.7759399776664,
6.77700140471194,6.77801586706867,6.77941752830882,6.7823000244874,6.78604953950823,
6.81777620383178,6.89074502905239,7.15632948240258,7.17326913458454,7.17705951533461,
7.17952606945882,7.18150887834564,7.18375950397884,7.18757950328156,7.20242187076909,
7.25761702845799,7.31891429461854,7.51271221383867,7.56891525525163,7.57283425230113,
7.57436483136627,7.57547609651029,7.57666340132407,7.57821557579685,7.58156544577563,
7.58601102578738,7.62630965207514,7.68553923131124,7.6935001771149,7.9705581906164,
7.98820711490774,7.99226898591487,7.99493523144023,7.99709399981822,7.9995612759102,
8.00379099466473,8.02075594260699,8.19597357337795,8.26716439171727,8.38433310728232,
8.39243022026517,8.3952888759041,8.39726362528687,8.39924527104867,8.40173176557202,
8.40444550792262,8.40882277174437,8.41745632636344,8.5128419558117,8.68019757327686,
8.75336330516805,8.82955546336615,8.8414311107382,8.8489807385905,8.85497715618765,
8.86173355113897,8.87315396079692,8.91922952813686,9.00581296499531,9.08169880468175,
9.14752245751981,9.15478410073917,9.15845309383498,9.16134085574025,9.16473392303519,
9.17036390343075,9.19111094249666,9.22868379246932,9.34812426892164,9.42006510906791,
9.45516567168477,9.46727904885301,9.47428817319761,9.48084393399812,9.48990988194288,
9.50812860241058,9.61741479843833,9.68401792423951,9.87143384275936,9.88295728658906,
9.9104880277396,9.91467959153884,9.91713096380455,9.91894512436701,9.92064211511499,
9.92253831544743,9.92515013362575,9.92946269899985,9.95805478872874),
 .UNSPECIFIED.);
#3580=B_SPLINE_CURVE_WITH_KNOTS('',3,(#230589,#230590,#230591,#230592,#230593,
#230594,#230595,#230596,#230597,#230598,#230599,#230600,#230601,#230602,
#230603,#230604,#230605,#230606,#230607,#230608,#230609,#230610,#230611,
#230612,#230613,#230614,#230615,#230616,#230617,#230618,#230619,#230620,
#230621,#230622,#230623,#230624,#230625,#230626,#230627,#230628,#230629,
#230630,#230631,#230632,#230633,#230634,#230635,#230636,#230637,#230638,
#230639,#230640,#230641,#230642,#230643,#230644,#230645,#230646,#230647,
#230648,#230649,#230650,#230651,#230652,#230653,#230654,#230655,#230656,
#230657,#230658,#230659,#230660,#230661,#230662,#230663,#230664,#230665,
#230666,#230667,#230668,#230669,#230670,#230671,#230672,#230673,#230674,
#230675,#230676,#230677,#230678,#230679,#230680,#230681,#230682,#230683,
#230684,#230685,#230686,#230687,#230688,#230689,#230690,#230691,#230692,
#230693,#230694,#230695,#230696,#230697,#230698,#230699,#230700,#230701,
#230702,#230703,#230704,#230705,#230706,#230707,#230708,#230709,#230710,
#230711,#230712,#230713,#230714,#230715,#230716,#230717,#230718,#230719,
#230720,#230721,#230722,#230723,#230724,#230725,#230726,#230727,#230728,
#230729,#230730,#230731,#230732,#230733,#230734,#230735,#230736,#230737,
#230738,#230739,#230740,#230741,#230742,#230743,#230744,#230745,#230746,
#230747,#230748,#230749,#230750,#230751,#230752,#230753,#230754,#230755,
#230756,#230757,#230758,#230759,#230760,#230761,#230762,#230763,#230764,
#230765,#230766,#230767,#230768,#230769,#230770,#230771,#230772,#230773,
#230774,#230775,#230776,#230777,#230778,#230779,#230780,#230781,#230782,
#230783,#230784,#230785,#230786,#230787,#230788,#230789,#230790,#230791,
#230792,#230793,#230794,#230795,#230796,#230797,#230798,#230799,#230800,
#230801,#230802,#230803,#230804,#230805,#230806,#230807,#230808,#230809,
#230810,#230811,#230812,#230813,#230814,#230815,#230816,#230817,#230818,
#230819,#230820,#230821,#230822,#230823,#230824,#230825,#230826,#230827,
#230828,#230829,#230830,#230831,#230832,#230833,#230834,#230835,#230836,
#230837,#230838,#230839,#230840,#230841,#230842,#230843,#230844,#230845,
#230846,#230847,#230848,#230849,#230850,#230851,#230852,#230853,#230854,
#230855,#230856,#230857,#230858,#230859,#230860,#230861,#230862,#230863,
#230864,#230865,#230866,#230867,#230868,#230869,#230870,#230871,#230872,
#230873,#230874,#230875,#230876,#230877,#230878,#230879,#230880,#230881,
#230882,#230883,#230884,#230885,#230886,#230887,#230888,#230889,#230890,
#230891,#230892,#230893,#230894,#230895,#230896,#230897,#230898,#230899,
#230900,#230901,#230902,#230903,#230904,#230905,#230906,#230907,#230908,
#230909,#230910,#230911,#230912,#230913,#230914,#230915,#230916,#230917,
#230918,#230919,#230920,#230921,#230922,#230923,#230924,#230925,#230926,
#230927,#230928,#230929,#230930,#230931,#230932,#230933,#230934,#230935,
#230936,#230937,#230938,#230939,#230940,#230941,#230942,#230943,#230944,
#230945,#230946,#230947,#230948,#230949,#230950,#230951,#230952,#230953,
#230954,#230955,#230956,#230957,#230958,#230959,#230960,#230961,#230962,
#230963,#230964,#230965,#230966,#230967,#230968,#230969,#230970,#230971,
#230972,#230973,#230974,#230975,#230976,#230977,#230978,#230979,#230980,
#230981,#230982,#230983,#230984,#230985,#230986,#230987,#230988,#230989,
#230990,#230991,#230992,#230993,#230994,#230995,#230996,#230997,#230998,
#230999,#231000,#231001,#231002,#231003,#231004,#231005,#231006,#231007,
#231008,#231009,#231010,#231011,#231012,#231013,#231014,#231015,#231016,
#231017,#231018,#231019,#231020,#231021,#231022,#231023,#231024,#231025,
#231026,#231027,#231028,#231029,#231030,#231031,#231032,#231033,#231034,
#231035,#231036,#231037,#231038,#231039,#231040,#231041,#231042,#231043,
#231044,#231045,#231046,#231047,#231048,#231049,#231050,#231051,#231052,
#231053,#231054,#231055,#231056,#231057,#231058,#231059,#231060,#231061,
#231062,#231063,#231064,#231065,#231066,#231067,#231068,#231069,#231070,
#231071,#231072,#231073,#231074,#231075,#231076,#231077,#231078,#231079,
#231080,#231081,#231082,#231083,#231084,#231085,#231086,#231087,#231088,
#231089,#231090,#231091,#231092,#231093,#231094,#231095,#231096,#231097,
#231098,#231099,#231100,#231101,#231102),.UNSPECIFIED.,.F.,.F.,(4,2,2,2,
2,2,2,2,2,2,2,2,2,2,2,2,2,2,2,2,2,2,2,2,2,2,2,2,2,2,2,2,2,2,2,2,2,2,2,2,
2,2,2,2,2,2,2,2,2,2,2,2,2,2,2,2,2,2,2,2,2,2,2,2,2,2,2,2,2,2,2,2,2,2,2,2,
2,2,2,2,2,2,2,2,2,2,2,2,2,2,2,2,2,2,2,2,2,2,2,2,2,2,2,2,2,2,2,2,2,2,2,2,
2,2,2,2,2,2,2,2,2,2,2,2,2,2,2,2,2,2,2,2,2,2,2,2,2,2,2,2,2,2,2,2,2,2,2,2,
2,2,2,2,2,2,2,2,2,2,2,2,2,2,2,2,2,2,2,2,2,2,2,2,2,2,2,2,2,2,2,2,2,2,2,2,
2,2,2,2,2,2,2,2,2,2,2,2,2,2,2,2,2,2,2,2,2,2,2,2,2,2,2,2,2,2,2,2,2,2,2,2,
2,2,2,2,2,2,2,2,2,2,2,2,2,2,2,2,2,2,2,2,2,2,2,2,2,2,2,2,2,2,2,2,2,2,2,2,
4),(0.00195160114906104,0.236564753226539,0.335098581850809,0.341349135687907,
0.371066482143385,0.376219658527723,0.378948856434874,0.38118944845288,
0.383784799532088,0.388205161030339,0.404371930212253,0.665359609611313,
0.725025870907951,0.76793502568408,0.780676553610812,0.786183381855492,
0.789145668938059,0.79169772059083,0.7933345024209,0.794835394757625,0.796816015756153,
0.801005766199686,0.829563273344597,0.914924903629073,0.992305247446216,
1.1388234777171,1.15155728784486,1.15694717519968,1.16085261487765,1.16442084567994,
1.16921126430518,1.1809625016166,1.28496037894192,1.43771930148249,1.5062910684478,
1.5340595547071,1.5382753206524,1.54041869218177,1.54214016493648,1.54406633044912,
1.54719580108933,1.55719308137523,1.71076731761959,1.85052170758076,1.90154307399534,
1.92799922432744,1.93270483431189,1.93521076862615,1.93707518688884,1.93910906514032,
1.94270004339742,1.95319321398495,2.112470924865,2.20065729336001,2.29319376660234,
2.34863452435371,2.35659015448224,2.35869824394119,2.35976182573397,2.36076484505819,
2.36186170702233,2.36347530342251,2.36830670246239,2.44448922157615,2.64969227313868,
2.72428476963431,2.75516165586155,2.75991293289239,2.76236565755929,2.76432914529949,
2.76658296889377,2.77041742761224,2.78361358117687,2.98102972464616,3.10160093911351,
3.14775552386405,3.15246923897567,3.15488763139188,3.15695493810197,3.15821435612411,
3.15939037526977,3.16089613709275,3.16329452091367,3.1754174055144,3.37808115115149,
3.48507866512861,3.54071201146672,3.56987697388276,3.57486384442311,3.57749639958538,
3.57965319961953,3.58214645921628,3.58638082255285,3.60174548136215,3.86411377213341,
3.9675644317206,3.97563551736588,3.97870941021309,3.98082052597055,3.98288397233688,
3.98536646692756,3.99130331223031,4.04742376052928,4.19180128647086,4.29841063221591,
4.41085266647841,4.42509696251923,4.43245354526277,4.43843585520245,4.44532906634405,
4.45705585489681,4.50225922775368,4.50462396718772,4.71277304165758,4.73446683720325,
4.73979467280805,4.74310861046367,4.74617131004224,4.750121071576,4.75666154437867,
4.79633375072138,4.87116764325385,4.98086066249085,4.98324526279393,5.03510218389985,
5.04904785292532,5.05723937649996,5.06442310789975,5.07352169310156,5.09189884192763,
5.20324495223863,5.29946033092353,5.42534561773102,5.43381873306651,5.43916676054429,
5.44129494743573,5.444923396478,5.44812923292397,5.47727794521809,5.48096659548021,
5.48935523359825,5.49711748252184,5.50005618930305,5.50180265291852,5.50364017563343,
5.50604646685044,5.51117926205437,5.60703152194068,5.65322938854595,5.69923379864474,
5.83181448302771,5.90727697734319,5.91436915351803,5.91724339111729,5.9193589278411,
5.92164698764888,5.92474963189037,5.93180189113912,6.05417757569404,6.22436290625847,
6.2632633601556,6.32460772526371,6.32930883239099,6.33124751205842,6.33268688636149,
6.33425568919932,6.33640391338538,6.34137859048937,6.47708326990131,6.58813140664802,
6.68088685514166,6.6906372129087,6.69555956984243,6.69916115119682,6.70304037759745,
6.70827900432122,6.71407172541381,6.72395561189804,6.88919429061741,7.00315999926392,
7.04594902308813,7.07294386681487,7.07741187410535,7.07966792545691,7.08143108576343,
7.08338035349883,7.08656866245492,7.09768863143446,7.16515550970892,7.31735428283288,
7.46061729240305,7.46986953050109,7.4732790181967,7.47527689536756,7.47715087854513,
7.4797353415103,7.48481404437227,7.52038975389516,7.61146312801923,7.70978884005364,
7.88436282411656,7.89545187018429,7.89770241904568,7.89912525986586,7.90024272633313,
7.9014835297925,7.90354899742277,7.9113007217569,7.96493268655756,8.07410227886942,
8.1633819232011,8.28895534739201,8.29743218797857,8.30063948584882,8.30254251705441,
8.30434305262912,8.30685084125137,8.31158494177505,8.34429418175278,8.43727304185448,
8.50359607105898,8.68276785122259,8.6934972746029,8.69574253331132,8.69720183500901,
8.69837312675038,8.69970053238662,8.70194805627772,8.71060307247117,8.77262799719312,
8.88931169928874,8.93915506481872,9.10108606007421,9.11164154999792,9.11533508509668,
9.117448210463,9.11939837328633,9.12203929281573,9.12706373092504,9.15647196804778,
9.21916756444585,9.24932204092596,9.26897622435194,9.32650303437604,9.38529166836775,
9.50518047064267,9.51401274780402,9.51730809811315,9.51925011566599,9.52107965123076,
9.52361612295599,9.52864855077965,9.56666039541573,9.70423316355673,9.90844336539317,
9.94319584725104,9.95899229756381),.UNSPECIFIED.);
#3581=B_SPLINE_CURVE_WITH_KNOTS('',3,(#231104,#231105,#231106,#231107,#231108,
#231109,#231110,#231111,#231112,#231113,#231114,#231115,#231116,#231117,
#231118,#231119,#231120,#231121,#231122,#231123,#231124,#231125,#231126,
#231127,#231128,#231129,#231130,#231131,#231132,#231133,#231134,#231135,
#231136,#231137,#231138,#231139,#231140,#231141,#231142,#231143,#231144,
#231145,#231146,#231147,#231148,#231149,#231150,#231151,#231152,#231153,
#231154,#231155,#231156,#231157,#231158,#231159,#231160,#231161,#231162,
#231163,#231164,#231165,#231166,#231167,#231168,#231169,#231170,#231171,
#231172,#231173,#231174,#231175,#231176,#231177,#231178,#231179,#231180,
#231181,#231182,#231183,#231184,#231185,#231186,#231187,#231188,#231189,
#231190,#231191,#231192,#231193,#231194,#231195,#231196,#231197,#231198,
#231199,#231200,#231201,#231202,#231203,#231204,#231205,#231206,#231207,
#231208,#231209,#231210,#231211,#231212,#231213,#231214,#231215,#231216,
#231217,#231218,#231219,#231220,#231221,#231222,#231223,#231224,#231225,
#231226,#231227,#231228,#231229,#231230,#231231,#231232,#231233,#231234,
#231235,#231236,#231237,#231238,#231239,#231240,#231241,#231242,#231243,
#231244,#231245,#231246,#231247,#231248,#231249,#231250,#231251,#231252,
#231253,#231254,#231255,#231256,#231257,#231258,#231259,#231260,#231261,
#231262,#231263,#231264,#231265,#231266,#231267,#231268,#231269,#231270,
#231271,#231272,#231273,#231274,#231275,#231276,#231277,#231278,#231279,
#231280,#231281,#231282,#231283,#231284,#231285,#231286,#231287,#231288,
#231289,#231290,#231291,#231292,#231293,#231294,#231295,#231296,#231297,
#231298,#231299,#231300,#231301,#231302,#231303,#231304,#231305,#231306,
#231307,#231308,#231309,#231310,#231311,#231312,#231313,#231314,#231315,
#231316,#231317,#231318,#231319,#231320,#231321,#231322,#231323,#231324,
#231325,#231326,#231327,#231328,#231329,#231330,#231331,#231332,#231333,
#231334,#231335,#231336,#231337,#231338,#231339,#231340,#231341,#231342,
#231343,#231344,#231345,#231346,#231347,#231348,#231349,#231350,#231351,
#231352,#231353,#231354,#231355,#231356,#231357,#231358,#231359),
 .UNSPECIFIED.,.F.,.F.,(4,3,3,3,3,3,3,3,3,3,3,3,3,3,3,3,3,3,3,3,3,3,3,3,
3,3,3,3,3,3,3,3,3,3,3,3,3,3,3,3,3,3,3,3,3,3,3,3,3,3,3,3,3,3,3,3,3,3,3,3,
3,3,3,3,3,3,3,3,3,3,3,3,3,3,3,3,3,3,3,3,3,3,3,3,3,4),(-355.951307622187,
-355.872214267879,-355.791997192643,-355.712722085922,-355.63203402643,
-355.551345966937,-355.469367188351,-355.387460439111,-355.303589354085,
-355.221923941571,-355.136950020288,-355.051976099006,-354.9783644249,-354.904758058047,
-354.831144006145,-354.757477713616,-354.683784185592,-354.610008712527,
-354.552606231075,-354.476105506269,-354.399660739088,-354.323261019508,
-354.246895469902,-354.170553237711,-354.093467394898,-354.017125581522,
-353.940773493879,-353.864401269772,-353.786767576132,-353.710295899139,
-353.632081197176,-353.553866495213,-353.479184680524,-353.404582828373,
-353.330048544799,-353.255579987264,-353.181149771671,-353.10674485987,
-353.054496627282,-352.974199378859,-352.893756905955,-352.809099369304,
-352.728319222888,-352.647437711954,-352.566420911552,-352.555126759351,
-352.480597289582,-352.406143961265,-352.33175287161,-352.257410158957,
-352.183101993942,-352.108814571024,-352.034519025254,-351.960214519186,
-351.885888555835,-351.811528629219,-351.737082946309,-351.662588093133,
-351.587991147452,-351.556387023488,-351.483248079804,-351.410197162497,
-351.337219338475,-351.264299743959,-351.191423568983,-351.118576043401,
-351.045728546241,-350.972877397704,-350.900009248603,-350.82711073855,
-350.754125296988,-350.681092484212,-350.607948060094,-350.557647287626,
-350.482812503093,-350.408063623116,-350.333386917726,-350.258768704072,
-350.184198468804,-350.109654671839,-350.035124995162,-349.960597130254,
-349.886032136981,-349.811449289414,-349.73679721459,-349.668434343951),
 .UNSPECIFIED.);
#3582=B_SPLINE_CURVE_WITH_KNOTS('',3,(#231361,#231362,#231363,#231364,#231365,
#231366,#231367,#231368,#231369,#231370,#231371,#231372,#231373,#231374,
#231375,#231376,#231377,#231378,#231379,#231380,#231381,#231382,#231383,
#231384,#231385,#231386,#231387,#231388,#231389,#231390,#231391,#231392,
#231393,#231394,#231395,#231396,#231397,#231398,#231399,#231400,#231401,
#231402,#231403,#231404,#231405,#231406,#231407,#231408,#231409,#231410,
#231411,#231412,#231413,#231414,#231415,#231416,#231417,#231418,#231419,
#231420,#231421,#231422,#231423,#231424,#231425,#231426,#231427,#231428,
#231429,#231430,#231431,#231432,#231433,#231434,#231435,#231436,#231437,
#231438,#231439,#231440,#231441,#231442,#231443,#231444,#231445,#231446,
#231447,#231448,#231449,#231450,#231451,#231452,#231453,#231454,#231455,
#231456,#231457,#231458,#231459,#231460,#231461,#231462,#231463,#231464,
#231465,#231466,#231467,#231468,#231469,#231470,#231471,#231472,#231473,
#231474,#231475,#231476,#231477,#231478,#231479,#231480,#231481,#231482,
#231483,#231484,#231485,#231486,#231487,#231488,#231489,#231490,#231491,
#231492,#231493,#231494,#231495,#231496,#231497,#231498,#231499,#231500,
#231501,#231502,#231503,#231504,#231505,#231506,#231507,#231508,#231509,
#231510,#231511,#231512,#231513,#231514,#231515,#231516,#231517,#231518,
#231519,#231520,#231521,#231522,#231523,#231524,#231525,#231526,#231527,
#231528,#231529,#231530,#231531,#231532,#231533,#231534,#231535,#231536,
#231537,#231538,#231539,#231540,#231541,#231542,#231543,#231544,#231545,
#231546,#231547,#231548,#231549,#231550,#231551,#231552,#231553,#231554,
#231555,#231556,#231557,#231558,#231559,#231560,#231561,#231562,#231563,
#231564,#231565,#231566,#231567,#231568,#231569,#231570,#231571,#231572,
#231573,#231574,#231575,#231576,#231577,#231578,#231579,#231580,#231581,
#231582,#231583,#231584,#231585,#231586,#231587,#231588,#231589,#231590,
#231591,#231592,#231593,#231594,#231595,#231596,#231597,#231598,#231599,
#231600,#231601,#231602,#231603,#231604,#231605,#231606,#231607,#231608,
#231609,#231610,#231611,#231612,#231613,#231614,#231615,#231616,#231617,
#231618,#231619,#231620,#231621,#231622,#231623,#231624,#231625,#231626,
#231627,#231628,#231629,#231630,#231631,#231632,#231633,#231634,#231635,
#231636,#231637,#231638,#231639,#231640,#231641,#231642,#231643,#231644,
#231645,#231646,#231647,#231648,#231649,#231650,#231651,#231652,#231653,
#231654,#231655,#231656,#231657,#231658,#231659,#231660,#231661,#231662,
#231663,#231664,#231665,#231666,#231667,#231668,#231669,#231670,#231671,
#231672,#231673,#231674,#231675,#231676,#231677,#231678,#231679,#231680,
#231681,#231682,#231683,#231684,#231685,#231686,#231687,#231688,#231689,
#231690,#231691,#231692,#231693,#231694,#231695,#231696,#231697,#231698,
#231699,#231700,#231701,#231702,#231703,#231704,#231705,#231706,#231707,
#231708,#231709,#231710,#231711,#231712,#231713,#231714,#231715,#231716,
#231717,#231718,#231719,#231720,#231721,#231722,#231723,#231724,#231725,
#231726,#231727,#231728,#231729,#231730,#231731,#231732,#231733,#231734,
#231735,#231736,#231737,#231738,#231739,#231740,#231741,#231742,#231743,
#231744,#231745,#231746,#231747,#231748,#231749,#231750,#231751,#231752,
#231753,#231754,#231755,#231756,#231757,#231758,#231759,#231760,#231761,
#231762,#231763,#231764,#231765,#231766,#231767,#231768,#231769,#231770,
#231771,#231772,#231773,#231774,#231775,#231776,#231777,#231778,#231779,
#231780,#231781,#231782,#231783,#231784,#231785,#231786,#231787,#231788,
#231789,#231790,#231791,#231792,#231793,#231794,#231795,#231796,#231797,
#231798,#231799,#231800,#231801,#231802,#231803,#231804,#231805,#231806,
#231807,#231808,#231809,#231810,#231811,#231812,#231813,#231814,#231815,
#231816,#231817,#231818,#231819,#231820,#231821,#231822,#231823,#231824,
#231825,#231826,#231827,#231828,#231829,#231830,#231831,#231832,#231833,
#231834,#231835,#231836,#231837,#231838,#231839,#231840,#231841,#231842,
#231843,#231844,#231845,#231846,#231847,#231848,#231849,#231850,#231851,
#231852,#231853,#231854,#231855,#231856,#231857,#231858,#231859,#231860,
#231861,#231862,#231863,#231864,#231865,#231866,#231867,#231868,#231869,
#231870),.UNSPECIFIED.,.F.,.F.,(4,2,2,2,2,2,2,2,2,2,2,2,2,2,2,2,2,2,2,2,
2,2,2,2,2,2,2,2,2,2,2,2,2,2,2,2,2,2,2,2,2,2,2,2,2,2,2,2,2,2,2,2,2,2,2,2,
2,2,2,2,2,2,2,2,2,2,2,2,2,2,2,2,2,2,2,2,2,2,2,2,2,2,2,2,2,2,2,2,2,2,2,2,
2,2,2,2,2,2,2,2,2,2,2,2,2,2,2,2,2,2,2,2,2,2,2,2,2,2,2,2,2,2,2,2,2,2,2,2,
2,2,2,2,2,2,2,2,2,2,2,2,2,2,2,2,2,2,2,2,2,2,2,2,2,2,2,2,2,2,2,2,2,2,2,2,
2,2,2,2,2,2,2,2,2,2,2,2,2,2,2,2,2,2,2,2,2,2,2,2,2,2,2,2,2,2,2,2,2,2,2,2,
2,2,2,2,2,2,2,2,2,2,2,2,2,2,2,2,2,2,2,2,2,2,2,2,2,2,2,2,2,2,2,2,2,2,2,2,
2,2,2,2,2,2,2,2,2,2,2,2,2,2,2,2,2,2,4),(0.00112295043593974,0.107857761231311,
0.114052241037512,0.11753262099607,0.119876263535378,0.121786873765044,
0.123780062850454,0.126142361503766,0.130245616857605,0.146206662253084,
0.275373782427591,0.298248501714585,0.481116090907697,0.551258197698067,
0.561954403051901,0.569030521095548,0.575812313285773,0.58180525133378,
0.589315278962869,0.603815309583193,0.727213567684471,0.811149694425183,
0.867790479377148,0.878519070755276,0.882738884083325,0.885764054322842,
0.887785260694388,0.891662747752114,0.899521235632171,0.961118701627771,
0.991983501862881,1.09959451863446,1.15389657070839,1.18264477335284,1.19097144595685,
1.1990663375337,1.20633371589231,1.21562257141657,1.23061280904579,1.30388785569167,
1.39752278481727,1.5260173359784,1.59690886178953,1.62292528742539,1.63716266103208,
1.64075322826951,1.64250785486455,1.64415262475517,1.64592156107976,1.64845460840261,
1.65545593457385,1.7271548492867,1.75184942887734,1.90829040079901,1.93818210128818,
2.00678198508029,2.05092922827064,2.05660833427005,2.05944714554916,2.06148541949694,
2.06363986052975,2.06727140512236,2.07687513308396,2.22018732039301,2.29787265950914,
2.41440600941893,2.46123301989485,2.46930129331774,2.47190908974559,2.47358480724344,
2.47513370139148,2.47712916470635,2.48041827605827,2.49871540572181,2.68896916872065,
2.80850992496078,2.82928211024011,2.83553226289197,2.83975436237766,2.84358602778225,
2.84851409156694,2.85643707689237,2.89396366801267,3.13522414108122,3.20594768434382,
3.21301668193643,3.21825708861012,3.22062456065244,3.22241122187724,3.22406618882445,
3.22631931655624,3.23074323398895,3.26907822257239,3.48483465793414,3.606016289264,
3.61240072429383,3.61523788931165,3.61734126710108,3.61929386823524,3.62195869187147,
3.62859429587152,3.70126098194594,3.75450237641733,3.88486956360218,3.97351805365338,
4.01756102919334,4.03594836859251,4.03865911356981,4.04004520238173,4.04105265575698,
4.0421289104894,4.04398638815591,4.04925626816744,4.13321670647967,4.32706869089585,
4.43356477957858,4.43944980757982,4.44212594332586,4.44413474111292,4.44601756874773,
4.44861539316056,4.45523177561149,4.53708738527925,4.71795624852287,4.7730462506962,
4.82685711183819,4.83466889334435,4.83680424019092,4.83810597188383,4.8392807073837,
4.84077978189214,4.84315755514824,4.85499520050329,4.89548550671736,4.97743828454832,
5.14289378391396,5.24552568332095,5.25296970987121,5.25583947659063,5.25790154105346,
5.26008513331391,5.26296635075888,5.26919361511967,5.36041122273955,5.58784091811462,
5.64983572182749,5.6557462016845,5.65842500768345,5.66047005379632,5.66264924614495,
5.66604149439303,5.67644366504155,5.80844313803825,6.02920781335209,6.03212123698015,
6.03291018219741,6.03962697243758,6.09351236530757,6.1056440790818,6.11262479733669,
6.11859950671055,6.12584225110404,6.13952303010811,6.2330848856891,6.38093547007934,
6.41184455655155,6.41800078969678,6.4215134612741,6.42423651430679,6.42779226694364,
6.434158619028,6.46464776615813,6.68090148649987,6.71743753095939,6.7294823224904,
6.73657986852364,6.74311113862535,6.75197839879513,6.76919525900418,6.86613477588839,
6.9957181482243,7.12636138773892,7.16298460680583,7.17499715609568,7.17849922917028,
7.18056393430239,7.18220262904189,7.18438600597253,7.18842795298414,7.20994954403043,
7.2483432632449,7.38078843922027,7.57889553757676,7.59143892739234,7.5954897233255,
7.59772731538535,7.59996927580979,7.60267619458662,7.60779231263027,7.61420491967219,
7.73416011782752,7.87000006968885,7.99861036794204,8.0066985499553,8.0094043524844,
8.0109208253831,8.01244061825881,8.01434618235529,8.01806049937145,8.0430661105764,
8.10635300393819,8.28753627468491,8.3602344302799,8.37026869583972,8.37517339317417,
8.37894566852037,8.38308013039411,8.38957946152218,8.40926838715509,8.51212648697745,
8.7291806888181,8.7517013395258,8.75554979194496,8.75785709171259,8.75963198644352,
8.76153649070127,8.7645277982498,8.77389350866761,8.82409056768681,8.94394991238551,
9.00072061672186,9.08605060986792,9.14286500119761,9.14919479646023,9.15173921741696,
9.15385400417221,9.15579629143257,9.15871867891198,9.16560485203871,9.17502846607691,
9.1987526885668,9.26190345048189,9.47695637213122,9.50088516645802,9.50885250652798,
9.57084860559634,9.57488558648574,9.57639754210294,9.5774692007131,9.57847856087551,
9.57987837702897,9.58271392282284,9.60678763708164,9.68405601565054,9.95413096362147),
 .UNSPECIFIED.);
#3583=B_SPLINE_CURVE_WITH_KNOTS('',3,(#231872,#231873,#231874,#231875,#231876,
#231877,#231878,#231879,#231880,#231881,#231882,#231883,#231884,#231885,
#231886,#231887,#231888,#231889,#231890,#231891,#231892,#231893,#231894,
#231895,#231896,#231897,#231898,#231899,#231900,#231901,#231902,#231903,
#231904,#231905,#231906,#231907,#231908,#231909,#231910,#231911,#231912,
#231913,#231914,#231915,#231916,#231917,#231918,#231919,#231920,#231921,
#231922,#231923,#231924,#231925,#231926,#231927,#231928,#231929,#231930,
#231931,#231932,#231933,#231934,#231935,#231936,#231937,#231938,#231939,
#231940,#231941,#231942,#231943,#231944,#231945,#231946,#231947,#231948,
#231949,#231950,#231951,#231952,#231953,#231954,#231955,#231956,#231957,
#231958,#231959,#231960,#231961,#231962,#231963,#231964,#231965,#231966,
#231967,#231968,#231969,#231970,#231971,#231972,#231973,#231974,#231975,
#231976,#231977,#231978,#231979,#231980,#231981,#231982,#231983,#231984,
#231985,#231986,#231987,#231988,#231989,#231990,#231991,#231992,#231993,
#231994,#231995,#231996,#231997,#231998,#231999,#232000,#232001,#232002,
#232003,#232004,#232005,#232006,#232007,#232008,#232009,#232010,#232011,
#232012,#232013,#232014,#232015,#232016,#232017,#232018,#232019,#232020,
#232021,#232022,#232023,#232024,#232025,#232026,#232027,#232028,#232029,
#232030,#232031,#232032,#232033,#232034,#232035,#232036,#232037,#232038,
#232039,#232040,#232041,#232042,#232043,#232044,#232045,#232046,#232047,
#232048,#232049,#232050,#232051,#232052,#232053,#232054,#232055,#232056,
#232057,#232058,#232059,#232060,#232061,#232062,#232063,#232064,#232065,
#232066,#232067,#232068,#232069,#232070,#232071,#232072,#232073,#232074,
#232075,#232076,#232077,#232078,#232079,#232080,#232081,#232082,#232083,
#232084,#232085,#232086,#232087,#232088,#232089,#232090,#232091,#232092,
#232093,#232094,#232095,#232096,#232097,#232098,#232099,#232100,#232101,
#232102,#232103,#232104,#232105,#232106,#232107,#232108,#232109,#232110,
#232111,#232112,#232113,#232114,#232115,#232116,#232117,#232118,#232119,
#232120,#232121,#232122,#232123,#232124,#232125,#232126,#232127,#232128,
#232129,#232130,#232131,#232132,#232133,#232134,#232135,#232136,#232137,
#232138,#232139,#232140,#232141,#232142,#232143,#232144,#232145,#232146,
#232147,#232148,#232149,#232150,#232151,#232152,#232153,#232154,#232155,
#232156,#232157,#232158,#232159,#232160,#232161,#232162,#232163,#232164,
#232165,#232166,#232167,#232168,#232169,#232170,#232171,#232172,#232173,
#232174,#232175,#232176,#232177,#232178,#232179,#232180,#232181,#232182,
#232183,#232184,#232185,#232186,#232187,#232188,#232189,#232190,#232191,
#232192,#232193,#232194,#232195,#232196,#232197,#232198,#232199,#232200,
#232201,#232202,#232203,#232204,#232205,#232206,#232207,#232208,#232209,
#232210,#232211,#232212,#232213,#232214,#232215,#232216,#232217,#232218,
#232219,#232220,#232221,#232222,#232223,#232224,#232225,#232226,#232227,
#232228,#232229,#232230,#232231,#232232,#232233,#232234,#232235,#232236,
#232237,#232238,#232239,#232240,#232241,#232242,#232243,#232244,#232245,
#232246,#232247,#232248,#232249,#232250,#232251,#232252,#232253,#232254,
#232255,#232256,#232257,#232258,#232259,#232260,#232261,#232262,#232263,
#232264,#232265,#232266,#232267,#232268,#232269,#232270,#232271,#232272,
#232273,#232274,#232275,#232276,#232277,#232278,#232279,#232280,#232281,
#232282,#232283,#232284,#232285,#232286,#232287,#232288,#232289,#232290,
#232291,#232292,#232293,#232294,#232295,#232296,#232297,#232298,#232299,
#232300,#232301,#232302,#232303,#232304,#232305,#232306,#232307,#232308,
#232309,#232310,#232311,#232312,#232313,#232314,#232315,#232316,#232317,
#232318,#232319,#232320,#232321,#232322,#232323,#232324,#232325,#232326,
#232327,#232328,#232329,#232330,#232331,#232332,#232333,#232334,#232335,
#232336,#232337,#232338,#232339,#232340,#232341,#232342,#232343,#232344,
#232345,#232346,#232347,#232348,#232349,#232350,#232351,#232352,#232353,
#232354,#232355,#232356,#232357,#232358,#232359,#232360,#232361,#232362,
#232363,#232364,#232365,#232366,#232367,#232368,#232369,#232370,#232371,
#232372,#232373,#232374,#232375,#232376,#232377,#232378,#232379,#232380,
#232381,#232382,#232383,#232384,#232385,#232386,#232387,#232388,#232389,
#232390,#232391,#232392,#232393,#232394,#232395,#232396,#232397,#232398,
#232399,#232400,#232401,#232402,#232403,#232404,#232405,#232406,#232407,
#232408,#232409,#232410,#232411,#232412,#232413,#232414,#232415,#232416,
#232417,#232418,#232419,#232420,#232421,#232422,#232423,#232424,#232425,
#232426,#232427,#232428,#232429,#232430,#232431,#232432,#232433,#232434,
#232435),.UNSPECIFIED.,.F.,.F.,(4,2,2,2,2,2,2,2,2,2,2,2,2,2,2,2,2,2,2,2,
2,2,2,2,2,2,2,2,2,2,2,2,2,2,2,2,2,2,2,2,2,2,2,2,2,2,2,2,2,2,2,2,2,2,2,2,
2,2,2,2,2,2,2,2,2,2,2,2,2,2,2,2,2,2,2,2,2,2,2,2,2,2,2,2,2,2,2,2,2,2,2,2,
2,2,2,2,2,2,2,2,2,2,2,2,2,2,2,2,2,2,2,2,2,2,2,2,2,2,2,2,2,2,2,2,2,2,2,2,
2,2,2,2,2,2,2,2,2,2,2,2,2,2,2,2,2,2,2,2,2,2,2,2,2,2,2,2,2,2,2,2,2,2,2,2,
2,2,2,2,2,2,2,2,2,2,2,2,2,2,2,2,2,2,2,2,2,2,2,2,2,2,2,2,2,2,2,2,2,2,2,2,
2,2,2,2,2,2,2,2,2,2,2,2,2,2,2,2,2,2,2,2,2,2,2,2,2,2,2,2,2,2,2,2,2,2,2,2,
2,2,2,2,2,2,2,2,2,2,2,2,2,2,2,2,2,2,2,2,2,2,2,2,2,2,2,2,2,2,2,2,2,2,2,2,
2,2,2,2,2,2,2,2,2,4),(0.0032206418046776,0.0210815066455308,0.0247042507456413,
0.0270909668341338,0.0289948856039576,0.030956571544407,0.033214350708931,
0.0370668490571024,0.050425706038174,0.0620697250116354,0.353057957478074,
0.385273656061949,0.405409759524707,0.421049422028272,0.423676422408627,
0.425087103529002,0.426141876280886,0.427297560028865,0.428990064128685,
0.433907907077473,0.515931179852567,0.73650149141895,0.800117252920412,
0.824252461611661,0.833899344259589,0.840885907074259,0.8439551733344,0.845984027311522,
0.848190726433849,0.850836312029805,0.857119975050606,0.908794956654506,
1.01523386745463,1.07849304557427,1.09715152519909,1.15506181007503,1.22874672678773,
1.24123594825736,1.24486812448472,1.24710134196542,1.24912998606215,1.25173825949375,
1.25694708520209,1.29009327122796,1.49492160947072,1.62439221179749,1.68165307843147,
1.69366231132888,1.70054652176404,1.70652974236568,1.71368481878407,1.72457364687925,
1.76331773546716,1.77132589907341,1.81691928737767,1.92389715881651,1.97576795349413,
2.00073405597256,2.00629000915767,2.00964992742166,2.01269944769531,2.01662002904365,
2.02473876563319,2.12246582381584,2.22612994589353,2.27471633215386,2.30699490280657,
2.31835159170384,2.32598326567893,2.33336024675526,2.34346546601538,2.36696470916073,
2.40068737829753,2.47660581004675,2.63053530187008,2.74870457837365,2.76266715475535,
2.76619991018831,2.76827197933312,2.7700922094825,2.77235008735283,2.77580480011788,
2.79106481552979,3.03152603787664,3.11878106124968,3.17028949982466,3.17707609948838,
3.18243269440358,3.18519324082447,3.18722854893409,3.18939162628324,3.19244695733074,
3.19880297860454,3.26739163782652,3.42013159838122,3.52398098310493,3.55901338400802,
3.5928386585894,3.5967075923737,3.59864550039752,3.6000387254337,3.60151292431991,
3.60358520317242,3.60907664869178,3.61342172824158,3.61947896731472,3.62682603539969,
3.62892996612677,3.76689450369097,3.94803417659746,3.95867418631668,3.96368432408664,
3.96752724255743,3.9711963136118,3.97742221081651,3.9937553964033,4.03033585854662,
4.2383565476632,4.31164769041488,4.34025402838042,4.34450033823187,4.34667980305043,
4.34841863255329,4.35015418631263,4.35325262327839,4.36252836817173,4.50748641265443,
4.62861042566123,4.7017140133385,4.73377783731544,4.73872804177424,4.74128560384759,
4.74333410019072,4.74568674279962,4.74969242080386,4.76350594980729,4.96944792107184,
4.98269894529362,5.14102443446203,5.16146583148092,5.1645153245062,5.16595452310382,
5.16707719543242,5.16829715355923,5.17026541232617,5.17703635336674,5.21975295382772,
5.27732771800372,5.44132576940524,5.55696655520913,5.56465362800154,5.56742371587753,
5.56935380460868,5.57114531401955,5.57358695461421,5.57828453803244,5.60780233278795,
5.67303390219221,5.7386473075883,5.7959334123614,5.93580992220177,5.95915834182736,
5.96201723540035,5.96349428641046,5.96459182050953,5.96578879146311,5.96742916049262,
5.97123147063057,6.03429608349821,6.18486740598433,6.36544184241586,6.37793733696198,
6.38189171012615,6.38405704260124,6.38599866751159,6.38854623492465,6.39313825259284,
6.41503353879074,6.45619640237481,6.55842925719197,6.66059367903474,6.77163237177265,
6.78071813420437,6.7840521485203,6.78600158142916,6.78799101681612,6.79053907128206,
6.79333878228997,6.79792316627911,6.80712543683528,6.91514253963537,7.07405388093739,
7.08430748019835,7.21121244470401,7.22863055207428,7.23663913729507,7.24271621870402,
7.24918221776059,7.2592793271078,7.27108715926858,7.41103220822256,7.52897613667893,
7.54147668653348,7.54596300330288,7.54907122568415,7.55213369856453,7.55647370570668,
7.56690092774815,7.58165456246179,7.62305917260627,7.69306944835078,7.79580074871121,
7.84153941857464,7.85492986694404,7.86299948143802,7.86954336113563,7.87850707924674,
7.89620010989325,7.99645834816143,8.13318567781716,8.28191368613601,8.2836649203808,
8.28497876142606,8.29351949998282,8.3022314808724,8.30531407847945,8.3070888558898,
8.308858960583,8.31111149245552,8.31549247171402,8.32101189585491,8.33294845516719,
8.36637850472788,8.44503178625175,8.61744580600723,8.64896195620345,8.71307323156934,
8.71931714347526,8.72234488298367,8.7245003765125,8.72653826396476,8.72937433306842,
8.73503992202204,8.77871120401351,8.89525715032246,8.91541235140057,8.93235780893388,
8.94690265630715,8.95956117281509,8.97068929231293,9.06712488805322,9.12964381189146,
9.13436217075744,9.13630347640733,9.13774314035973,9.13920704466464,9.14073816984089,
9.14429134384458,9.16554268333411,9.21218503153921,9.2614649244329,9.39844391353661,
9.4859834721567,9.49668735608423,9.50165514882539,9.50550397493303,9.50966606207296,
9.51628637525377,9.53687817624927,9.64758675553711,9.79655125727371,9.80873977005857,
9.85039853072301,9.87763383153486,9.88211261691432,9.88437049508769,9.88613333962904,
9.88777133884977,9.88967301624833,9.89237281830234,9.8969677328629,9.95836513107871),
 .UNSPECIFIED.);
#3584=B_SPLINE_CURVE_WITH_KNOTS('',3,(#232437,#232438,#232439,#232440,#232441,
#232442,#232443,#232444,#232445,#232446,#232447,#232448,#232449,#232450,
#232451,#232452,#232453,#232454,#232455,#232456,#232457,#232458,#232459,
#232460,#232461,#232462,#232463,#232464,#232465,#232466,#232467,#232468,
#232469,#232470,#232471,#232472,#232473,#232474,#232475,#232476,#232477,
#232478,#232479,#232480,#232481,#232482,#232483,#232484,#232485,#232486,
#232487,#232488,#232489,#232490,#232491,#232492,#232493,#232494,#232495,
#232496,#232497,#232498,#232499,#232500,#232501,#232502,#232503,#232504,
#232505,#232506,#232507,#232508,#232509,#232510,#232511,#232512,#232513,
#232514,#232515,#232516,#232517,#232518,#232519,#232520,#232521,#232522,
#232523,#232524,#232525,#232526,#232527,#232528,#232529,#232530,#232531,
#232532,#232533,#232534,#232535,#232536,#232537,#232538,#232539,#232540,
#232541,#232542,#232543,#232544,#232545,#232546,#232547,#232548,#232549,
#232550,#232551,#232552,#232553,#232554,#232555,#232556,#232557,#232558,
#232559,#232560,#232561,#232562,#232563,#232564,#232565,#232566,#232567,
#232568,#232569,#232570,#232571,#232572,#232573,#232574,#232575,#232576,
#232577,#232578,#232579,#232580,#232581,#232582,#232583,#232584,#232585,
#232586,#232587,#232588,#232589,#232590,#232591,#232592,#232593,#232594,
#232595,#232596,#232597,#232598,#232599,#232600,#232601,#232602,#232603,
#232604,#232605,#232606,#232607,#232608,#232609,#232610,#232611,#232612,
#232613,#232614,#232615,#232616,#232617,#232618,#232619,#232620,#232621,
#232622,#232623,#232624,#232625,#232626,#232627,#232628,#232629,#232630,
#232631,#232632,#232633,#232634,#232635,#232636,#232637,#232638,#232639,
#232640,#232641,#232642,#232643,#232644,#232645,#232646,#232647,#232648,
#232649,#232650,#232651,#232652,#232653,#232654,#232655,#232656,#232657,
#232658,#232659,#232660,#232661,#232662,#232663,#232664,#232665,#232666,
#232667,#232668,#232669,#232670,#232671,#232672,#232673,#232674,#232675,
#232676,#232677,#232678,#232679,#232680,#232681,#232682,#232683,#232684,
#232685,#232686,#232687,#232688,#232689,#232690,#232691,#232692,#232693,
#232694,#232695),.UNSPECIFIED.,.F.,.F.,(4,3,3,3,3,3,3,3,3,3,3,3,3,3,3,3,
3,3,3,3,3,3,3,3,3,3,3,3,3,3,3,3,3,3,3,3,3,3,3,3,3,3,3,3,3,3,3,3,3,3,3,3,
3,3,3,3,3,3,3,3,3,3,3,3,3,3,3,3,3,3,3,3,3,3,3,3,3,3,3,3,3,3,3,3,3,3,4),
(-324.535381086289,-324.461322539534,-324.387335999405,-324.313407189673,
-324.239521874744,-324.165665849949,-324.091812204043,-324.017956628568,
-323.944086283212,-323.870188321613,-323.796208072316,-323.722183693228,
-323.648051467166,-323.591674419347,-323.518535475663,-323.445484558356,
-323.372506734333,-323.299587139818,-323.226710964842,-323.15386343926,
-323.0810159421,-323.008164793562,-322.935296644461,-322.862398134409,-322.789412692846,
-322.71637988007,-322.643235455953,-322.592934683485,-322.517406394818,
-322.441964199485,-322.36659519179,-322.291286513827,-322.216025347427,
-322.138296547451,-322.063086350126,-321.987882125428,-321.912672315163,
-321.837445360177,-321.762162470567,-321.686846423697,-321.61145951444,
-321.594194947623,-321.517603047222,-321.441076345282,-321.36460514939,
-321.288188289129,-321.211804250295,-321.135444086883,-321.094825079692,
-321.016705811213,-320.938541507739,-320.860327430751,-320.782022308062,
-320.703668881464,-320.625229791698,-320.595455211761,-320.513476433175,
-320.431569683936,-320.347698598909,-320.266033186396,-320.181059265113,
-320.09608534383,-320.022473669723,-319.948867302869,-319.875253250966,
-319.801586958436,-319.727893430411,-319.654117957344,-319.596715475898,
-319.520214751092,-319.443769983911,-319.367370264331,-319.291004714725,
-319.214662482534,-319.137576639722,-319.061234826346,-318.984882738703,
-318.908510514596,-318.830876820956,-318.754405143963,-318.676190441999,
-318.597975740036,-318.518993131618,-318.440204240229,-318.361532828754,
-318.283021502504,-318.252195779109),.UNSPECIFIED.);
#3585=B_SPLINE_CURVE_WITH_KNOTS('',3,(#232697,#232698,#232699,#232700,#232701,
#232702,#232703,#232704,#232705,#232706,#232707,#232708,#232709,#232710,
#232711,#232712,#232713,#232714,#232715,#232716,#232717,#232718,#232719,
#232720,#232721,#232722,#232723,#232724,#232725,#232726,#232727,#232728,
#232729,#232730,#232731,#232732,#232733,#232734,#232735,#232736,#232737,
#232738,#232739,#232740,#232741,#232742,#232743,#232744,#232745,#232746,
#232747,#232748,#232749,#232750,#232751,#232752,#232753,#232754,#232755,
#232756,#232757,#232758,#232759,#232760,#232761,#232762,#232763,#232764,
#232765,#232766,#232767,#232768,#232769,#232770,#232771,#232772,#232773,
#232774,#232775,#232776,#232777,#232778,#232779,#232780,#232781,#232782,
#232783,#232784,#232785,#232786,#232787,#232788,#232789,#232790,#232791,
#232792,#232793,#232794,#232795,#232796,#232797,#232798,#232799,#232800,
#232801,#232802,#232803,#232804,#232805,#232806,#232807,#232808,#232809,
#232810,#232811,#232812,#232813,#232814,#232815,#232816,#232817,#232818,
#232819,#232820,#232821,#232822,#232823,#232824,#232825,#232826,#232827,
#232828,#232829,#232830,#232831,#232832,#232833,#232834,#232835,#232836,
#232837,#232838,#232839,#232840,#232841,#232842,#232843,#232844,#232845,
#232846,#232847,#232848,#232849,#232850,#232851,#232852,#232853,#232854,
#232855,#232856,#232857,#232858,#232859,#232860,#232861,#232862,#232863,
#232864,#232865,#232866,#232867,#232868,#232869,#232870,#232871,#232872,
#232873,#232874,#232875,#232876,#232877,#232878,#232879,#232880,#232881,
#232882,#232883,#232884,#232885,#232886,#232887,#232888,#232889,#232890,
#232891,#232892,#232893,#232894,#232895,#232896,#232897,#232898,#232899,
#232900,#232901,#232902,#232903,#232904,#232905,#232906,#232907,#232908,
#232909,#232910,#232911,#232912,#232913,#232914,#232915,#232916,#232917,
#232918,#232919,#232920,#232921,#232922,#232923,#232924,#232925,#232926,
#232927,#232928,#232929,#232930,#232931,#232932,#232933,#232934,#232935,
#232936,#232937,#232938,#232939,#232940,#232941,#232942,#232943,#232944,
#232945,#232946,#232947,#232948,#232949,#232950,#232951,#232952,#232953,
#232954,#232955,#232956,#232957,#232958,#232959,#232960,#232961,#232962,
#232963,#232964,#232965,#232966,#232967,#232968,#232969,#232970,#232971,
#232972,#232973,#232974,#232975,#232976,#232977,#232978,#232979,#232980,
#232981,#232982,#232983,#232984,#232985,#232986,#232987,#232988,#232989,
#232990,#232991,#232992,#232993,#232994,#232995,#232996,#232997,#232998,
#232999,#233000,#233001,#233002,#233003,#233004,#233005,#233006,#233007,
#233008,#233009,#233010,#233011,#233012,#233013,#233014,#233015,#233016,
#233017,#233018,#233019,#233020,#233021,#233022,#233023,#233024,#233025,
#233026,#233027,#233028,#233029,#233030,#233031,#233032,#233033,#233034,
#233035,#233036,#233037,#233038,#233039,#233040,#233041,#233042,#233043,
#233044,#233045,#233046,#233047,#233048,#233049,#233050,#233051,#233052,
#233053,#233054,#233055,#233056,#233057,#233058,#233059,#233060,#233061,
#233062,#233063,#233064,#233065,#233066,#233067,#233068,#233069,#233070,
#233071,#233072,#233073,#233074,#233075,#233076,#233077,#233078,#233079,
#233080,#233081,#233082,#233083,#233084,#233085,#233086,#233087,#233088,
#233089,#233090,#233091,#233092,#233093,#233094,#233095,#233096,#233097,
#233098,#233099,#233100,#233101,#233102,#233103,#233104,#233105,#233106,
#233107,#233108,#233109,#233110,#233111,#233112,#233113,#233114,#233115,
#233116,#233117,#233118,#233119,#233120,#233121,#233122,#233123,#233124,
#233125,#233126,#233127,#233128,#233129,#233130,#233131,#233132,#233133,
#233134,#233135,#233136,#233137,#233138,#233139,#233140,#233141,#233142,
#233143,#233144,#233145,#233146,#233147,#233148,#233149,#233150,#233151,
#233152,#233153,#233154,#233155,#233156,#233157,#233158,#233159,#233160,
#233161,#233162,#233163,#233164,#233165,#233166,#233167,#233168,#233169,
#233170,#233171,#233172,#233173,#233174,#233175,#233176,#233177,#233178,
#233179,#233180,#233181,#233182,#233183,#233184,#233185,#233186,#233187,
#233188,#233189,#233190,#233191,#233192,#233193,#233194,#233195,#233196,
#233197,#233198),.UNSPECIFIED.,.F.,.F.,(4,2,2,2,2,2,2,2,2,2,2,2,2,2,2,2,
2,2,2,2,2,2,2,2,2,2,2,2,2,2,2,2,2,2,2,2,2,2,2,2,2,2,2,2,2,2,2,2,2,2,2,2,
2,2,2,2,2,2,2,2,2,2,2,2,2,2,2,2,2,2,2,2,2,2,2,2,2,2,2,2,2,2,2,2,2,2,2,2,
2,2,2,2,2,2,2,2,2,2,2,2,2,2,2,2,2,2,2,2,2,2,2,2,2,2,2,2,2,2,2,2,2,2,2,2,
2,2,2,2,2,2,2,2,2,2,2,2,2,2,2,2,2,2,2,2,2,2,2,2,2,2,2,2,2,2,2,2,2,2,2,2,
2,2,2,2,2,2,2,2,2,2,2,2,2,2,2,2,2,2,2,2,2,2,2,2,2,2,2,2,2,2,2,2,2,2,2,2,
2,2,2,2,2,2,2,2,2,2,2,2,2,2,2,2,2,2,2,2,2,2,2,2,2,2,2,2,2,2,2,2,2,2,2,2,
2,2,2,2,2,2,2,2,2,2,2,2,2,2,2,2,2,2,4),(0.00121348254971357,0.0844218198558422,
0.0938908223239574,0.0995313570605865,0.103568722924125,0.107122786700612,
0.110982982662361,0.116020140960127,0.127045063186039,0.202337357354917,
0.223548934817849,0.41236865835311,0.45999701856791,0.481978766425379,0.485944302503179,
0.488064681781256,0.489645790598398,0.49162592270192,0.494952698098768,
0.506037432433198,0.664169816120028,0.703088453675587,0.740702436756285,
0.873118102024691,0.879345226483091,0.882154392177681,0.884253945898625,
0.886215218605446,0.888910923892993,0.89572233686709,0.976101250752053,
0.995824217702251,1.07690379222896,1.16463032242153,1.19717713056531,1.24822317687767,
1.29674388054704,1.30413339346925,1.3061914227682,1.30743595353808,1.30855258424657,
1.30997039499775,1.31223788006559,1.32401417485332,1.5147928207457,1.61981545740611,
1.67543314668045,1.7027385224526,1.70736475114492,1.70979125675229,1.71158089231656,
1.71351789017113,1.71689768993709,1.72651793240158,1.86784129999972,1.9934495171053,
2.04361259485488,2.09218373487637,2.10171270357673,2.10399199124184,2.10532632758646,
2.10649652235821,2.10794508851437,2.11015868318238,2.11985027955127,2.1631622147198,
2.29159962793086,2.43201702828084,2.51511024396737,2.52126904679386,2.52413803445429,
2.52632060264184,2.52838790489381,2.53185090819893,2.54089181687515,2.67737341746246,
2.8106270386984,2.86104786617758,2.89671188749953,2.91960222083244,2.92403151039003,
2.92644104182935,2.92843475022784,2.93079920729671,2.93491007149538,2.95094460912242,
2.96234391471357,3.1473631002315,3.35333733438873,3.37040884544617,3.37831617020363,
3.38435726405786,3.39092492367593,3.40148312175346,3.43419333811076,3.55957373021619,
3.66762151305439,3.67753608564849,3.68500610339691,3.68872712527851,3.69146762592415,
3.69443200852598,3.69871470392511,3.7108461594919,3.84368802674237,3.97746397191585,
3.99393622541746,4.00266612862714,4.00919111258611,4.01742321659748,4.03158679962271,
4.08882938149597,4.20846239901833,4.35636008293556,4.43222836102517,4.43958541959908,
4.44506498827798,4.44753647773335,4.44938407780453,4.45111000103136,4.45348249100253,
4.45948207722142,4.52180264480049,4.73219138048668,4.85463960363688,4.86165294335743,
4.86474824260393,4.86703472227711,4.86915151742863,4.87203163315172,4.87915931552144,
4.9562021062755,4.97915154849782,5.2164716270247,5.27196792397129,5.27619282034345,
5.27825313742188,5.2797241668528,5.2811180557192,5.28306300437236,5.28696581014438,
5.31794020020128,5.37693092113321,5.52774652357561,5.62780566875286,5.63881662368138,
5.64384260131559,5.6477013461789,5.65183958277373,5.65834876045442,5.67809379822284,
5.78139445040959,5.99765580472344,6.02062611636122,6.02450058699412,6.02681624756777,
6.02859331986864,6.0304960005705,6.03347577957996,6.04273725223415,6.09201848481516,
6.12393150813305,6.21285647196616,6.40411712068135,6.41426258337349,6.41877916301148,
6.42149502674862,6.42358711170371,6.42583451083396,6.42936935642802,6.44047140390451,
6.61494864815417,6.7980135238467,6.84099059839442,6.84466713048314,6.84612022645114,
6.84717652714774,6.84830635187796,6.84978949672812,6.85308692451535,6.85752214496301,
6.89956960595399,6.9653520553536,7.22669244407188,7.2434030572105,7.24717452648218,
7.24963511532834,7.25161734319513,7.25387187510414,7.25770966595411,7.27275648340527,
7.38230629116713,7.5857184956636,7.60453891713797,7.63970880731287,7.64290495321987,
7.64446553837621,7.64558474774064,7.6466493550247,7.64811107488101,7.65100963953831,
7.65472859020836,7.81070683397365,7.89530111916282,8.04959797527249,8.05965722849809,
8.06327786963883,8.06537617756431,8.06732962022545,8.07000093913175,8.07517143403037,
8.10869624201312,8.18539530231802,8.30659516009491,8.44729962888903,8.46069265125458,
8.46451083249091,8.46677694187205,8.46875075720316,8.47114132612438,8.4756432653729,
8.49997497170848,8.5537482984691,8.6693217340446,8.79155088950859,8.8161934538348,
8.89872537445595,8.91088729507275,8.91852372787577,8.92452995178897,8.93123572432224,
8.94242321553105,8.9856041182205,9.20142749733787,9.22097401063266,9.22625472040813,
9.22954080256217,9.23228094579009,9.2360213794865,9.24325038851341,9.29347785845239,
9.38529183628633,9.51708001320053,9.5320192117991,9.54132473617372,9.54859554383567,
9.55668236514666,9.57017550939193,9.6266678921445,9.71456334555599,9.9583219418317),
 .UNSPECIFIED.);
#3586=B_SPLINE_CURVE_WITH_KNOTS('',3,(#233200,#233201,#233202,#233203,#233204,
#233205,#233206,#233207,#233208,#233209,#233210,#233211,#233212,#233213,
#233214,#233215,#233216,#233217,#233218,#233219,#233220,#233221,#233222,
#233223,#233224,#233225,#233226,#233227,#233228,#233229,#233230,#233231,
#233232,#233233,#233234,#233235,#233236,#233237,#233238,#233239,#233240,
#233241,#233242,#233243,#233244,#233245,#233246,#233247,#233248,#233249,
#233250,#233251,#233252,#233253,#233254,#233255,#233256,#233257,#233258,
#233259,#233260,#233261,#233262,#233263,#233264,#233265,#233266,#233267,
#233268,#233269,#233270,#233271,#233272,#233273,#233274,#233275,#233276,
#233277,#233278,#233279,#233280,#233281,#233282,#233283,#233284,#233285,
#233286,#233287,#233288,#233289,#233290,#233291,#233292,#233293,#233294,
#233295,#233296,#233297,#233298,#233299,#233300,#233301,#233302,#233303,
#233304,#233305,#233306,#233307,#233308,#233309,#233310,#233311,#233312,
#233313,#233314,#233315,#233316,#233317,#233318,#233319,#233320,#233321,
#233322,#233323,#233324,#233325,#233326,#233327,#233328,#233329,#233330,
#233331,#233332,#233333,#233334,#233335,#233336,#233337,#233338,#233339,
#233340,#233341,#233342,#233343,#233344,#233345,#233346,#233347,#233348,
#233349,#233350,#233351,#233352,#233353,#233354,#233355,#233356,#233357,
#233358,#233359,#233360,#233361,#233362,#233363,#233364,#233365,#233366,
#233367,#233368,#233369,#233370,#233371,#233372,#233373,#233374,#233375,
#233376,#233377,#233378,#233379,#233380,#233381,#233382,#233383,#233384,
#233385,#233386,#233387,#233388,#233389,#233390,#233391,#233392,#233393,
#233394,#233395,#233396,#233397,#233398,#233399,#233400,#233401,#233402,
#233403,#233404,#233405,#233406,#233407,#233408,#233409,#233410,#233411,
#233412,#233413,#233414,#233415,#233416,#233417,#233418,#233419,#233420,
#233421,#233422,#233423,#233424,#233425,#233426,#233427,#233428,#233429,
#233430,#233431,#233432,#233433,#233434,#233435,#233436,#233437,#233438,
#233439,#233440,#233441,#233442,#233443,#233444,#233445,#233446,#233447,
#233448,#233449,#233450,#233451,#233452,#233453,#233454,#233455,#233456,
#233457,#233458,#233459,#233460,#233461,#233462,#233463,#233464,#233465,
#233466,#233467,#233468,#233469,#233470,#233471,#233472,#233473,#233474,
#233475,#233476,#233477,#233478,#233479,#233480,#233481,#233482,#233483,
#233484,#233485,#233486,#233487,#233488,#233489,#233490,#233491,#233492,
#233493,#233494,#233495,#233496,#233497,#233498,#233499,#233500,#233501,
#233502,#233503,#233504,#233505,#233506,#233507,#233508,#233509,#233510,
#233511,#233512,#233513,#233514,#233515,#233516,#233517,#233518,#233519,
#233520,#233521,#233522,#233523,#233524,#233525,#233526,#233527,#233528,
#233529,#233530,#233531,#233532,#233533,#233534,#233535,#233536,#233537,
#233538,#233539,#233540,#233541,#233542,#233543,#233544,#233545,#233546,
#233547,#233548,#233549,#233550,#233551,#233552,#233553,#233554,#233555,
#233556,#233557,#233558,#233559,#233560,#233561,#233562,#233563,#233564,
#233565,#233566,#233567,#233568,#233569,#233570,#233571,#233572,#233573,
#233574,#233575,#233576,#233577,#233578,#233579,#233580,#233581,#233582,
#233583,#233584,#233585,#233586,#233587,#233588,#233589,#233590,#233591,
#233592,#233593,#233594,#233595,#233596,#233597,#233598,#233599,#233600,
#233601,#233602,#233603,#233604,#233605,#233606,#233607,#233608,#233609,
#233610,#233611,#233612,#233613,#233614,#233615,#233616,#233617,#233618,
#233619,#233620,#233621,#233622,#233623,#233624,#233625,#233626,#233627,
#233628,#233629,#233630,#233631,#233632,#233633,#233634,#233635,#233636,
#233637,#233638,#233639,#233640,#233641,#233642,#233643,#233644,#233645,
#233646,#233647,#233648,#233649,#233650,#233651,#233652,#233653,#233654,
#233655,#233656,#233657,#233658,#233659,#233660,#233661,#233662,#233663,
#233664,#233665,#233666,#233667,#233668,#233669,#233670,#233671,#233672,
#233673,#233674,#233675,#233676,#233677,#233678,#233679,#233680,#233681,
#233682,#233683,#233684,#233685,#233686,#233687,#233688,#233689,#233690,
#233691,#233692,#233693,#233694,#233695,#233696,#233697,#233698,#233699,
#233700,#233701,#233702,#233703,#233704,#233705,#233706,#233707,#233708,
#233709,#233710,#233711,#233712,#233713,#233714,#233715,#233716,#233717,
#233718,#233719,#233720,#233721,#233722,#233723,#233724,#233725,#233726,
#233727,#233728,#233729),.UNSPECIFIED.,.F.,.F.,(4,2,2,2,2,2,2,2,2,2,2,2,
2,2,2,2,2,2,2,2,2,2,2,2,2,2,2,2,2,2,2,2,2,2,2,2,2,2,2,2,2,2,2,2,2,2,2,2,
2,2,2,2,2,2,2,2,2,2,2,2,2,2,2,2,2,2,2,2,2,2,2,2,2,2,2,2,2,2,2,2,2,2,2,2,
2,2,2,2,2,2,2,2,2,2,2,2,2,2,2,2,2,2,2,2,2,2,2,2,2,2,2,2,2,2,2,2,2,2,2,2,
2,2,2,2,2,2,2,2,2,2,2,2,2,2,2,2,2,2,2,2,2,2,2,2,2,2,2,2,2,2,2,2,2,2,2,2,
2,2,2,2,2,2,2,2,2,2,2,2,2,2,2,2,2,2,2,2,2,2,2,2,2,2,2,2,2,2,2,2,2,2,2,2,
2,2,2,2,2,2,2,2,2,2,2,2,2,2,2,2,2,2,2,2,2,2,2,2,2,2,2,2,2,2,2,2,2,2,2,2,
2,2,2,2,2,2,2,2,2,2,2,2,2,2,2,2,2,2,2,2,2,2,2,2,2,2,2,2,2,2,2,2,2,2,2,2,
4),(0.00198884727365615,0.0171463707040567,0.0256750116657391,0.0285743152075191,
0.0305866372870217,0.0322993945240548,0.0340195300615396,0.0362724063238345,
0.0397113804947701,0.0547865144684803,0.0645103343802238,0.339946689773468,
0.438496089949156,0.445648012664128,0.448767624582792,0.451057800839298,
0.453167975412984,0.456023790731331,0.463015146236112,0.534410202560947,
0.663414367777973,0.781945904415294,0.816553468401073,0.843738551184968,
0.853013901187956,0.85737159961459,0.859872133056049,0.861592841285253,
0.863249291791709,0.864758552761795,0.866733820356451,0.870789238402392,
0.89632099829748,0.999804598008103,1.07998952121405,1.21001057913817,1.22185351716905,
1.22708650650142,1.23096366351171,1.23456663790031,1.23949692087691,1.24926504030501,
1.32028598747467,1.36023160900097,1.48807763203879,1.60040933539202,1.60692629772314,
1.60952169020636,1.61131058988051,1.61309256735427,1.61559167289823,1.62141855944166,
1.69726813511767,1.80495645909475,1.81444926508167,1.82472222017144,1.83592778297765,
1.86583974181973,1.94738375994934,1.98016180636644,1.99842068553729,2.00263008699332,
2.00502771032156,2.00688439860489,2.00930426391325,2.01349991396267,2.02961421801231,
2.2751727379974,2.37781057022431,2.41991444269915,2.42439616841689,2.42773598930991,
2.42924167604163,2.43037581271755,2.43142478027466,2.43285578139489,2.43572132969231,
2.46062740154547,2.4872096705856,2.50739463983733,2.69427950051916,2.81104590060132,
2.82645764099631,2.83032669765709,2.83258813120023,2.83456946622926,2.83701993548203,
2.84075936335307,2.85708823751138,3.11896859020952,3.22101295715412,3.224122329879,
3.22663225561638,3.22800275638513,3.22905757435155,3.23021203204805,3.23225973071354,
3.23830593948605,3.26140641444881,3.50785970597717,3.63168381495137,3.64273248754689,
3.64635703997747,3.64868926688715,3.65088009198266,3.65375262778956,3.66009670594612,
3.7111551285214,3.90697201860214,4.04084444490444,4.0465966752032,4.04927525244862,
4.05131321204736,4.05324474820864,4.05648195626984,4.0649647837136,4.06738218615224,
4.08362869955827,4.27695943649482,4.4767814234358,4.49374047659829,4.50162583718784,
4.50766270131223,4.51342676625764,4.52324848705835,4.5503816094235,4.72584019635343,
4.80151275330677,4.80854801537686,4.81219114061619,4.81521704842281,4.81876577335425,
4.82493202384562,4.84942811029881,4.98058111098711,5.10032363114756,5.11532613117836,
5.12464987561789,5.13192191358108,5.13999675390767,5.15343804759686,5.2093274977759,
5.29726575778849,5.50169861115414,5.51417552653281,5.55316339279786,5.56592534514112,
5.56946716002764,5.57156148416652,5.57337924684139,5.57560598448812,5.57984974886658,
5.6058721421834,5.63549664847498,5.69924491139167,5.75326929445897,5.83321316984002,
5.97387554835989,5.98333153742395,5.98693941643972,5.9890891201945,5.99135574236815,
5.99433029162459,6.0006971050468,6.08447378271113,6.19173283708081,6.35057534276617,
6.35276396250618,6.39487236110566,6.39928948434063,6.40131295177347,6.40286612313846,
6.40452909361055,6.40713335771399,6.41522597832415,6.53779729423936,6.66650677623621,
6.75076037147215,6.76137828678529,6.76632962933164,6.77017575196176,6.77394659486115,
6.7801561052831,6.78738276233063,6.80064288660128,6.90528395347411,7.11882343087342,
7.14275321813219,7.14667747078748,7.14900735035899,7.15078628566553,7.15268218683037,
7.15563325837464,7.16466650933385,7.21202251169895,7.26047709391965,7.38658358420473,
7.52995863424854,7.53920387679239,7.54261147842525,7.54460844175146,7.54648169127216,
7.54906533578278,7.55414311384868,7.58973821287799,7.68074153179939,7.78113081675769,
7.93081272570395,7.96301871081334,7.96614438211233,7.96765291296083,7.96872372892792,
7.96973357871389,7.97113614977494,7.973985159641,7.99860481526616,8.07535028583002,
8.21109717850274,8.35600223288823,8.36595202447255,8.36937830018627,8.37132423484702,
8.37311126671674,8.37551797012166,8.38005280963434,8.40542663700932,8.44020910999858,
8.5124599738622,8.57647449677435,8.73229627854706,8.76081629940044,8.76417665051739,
8.76571616156273,8.76690033082439,8.76817048983073,8.77016390757077,8.77638447316304,
8.81210312745829,8.84027971198559,8.92017256287157,8.99311816982852,9.16843772328873,
9.179908002401,9.18372764738194,9.18586543128531,9.18780977047556,9.19040065179808,
9.1951942912154,9.22051898846983,9.27020543496659,9.31009548091169,9.33439906163638,
9.35107034385852,9.40167657937295,9.56852906458665,9.5813534354853,9.58518418670587,
9.58746115849259,9.58927774551977,9.59171256628152,9.59626289846381,9.62157075763454,
9.67863810718868,9.78800941450442,9.95698214585812),.UNSPECIFIED.);
#3587=B_SPLINE_CURVE_WITH_KNOTS('',3,(#233731,#233732,#233733,#233734,#233735,
#233736,#233737,#233738,#233739,#233740,#233741,#233742,#233743,#233744,
#233745,#233746,#233747,#233748,#233749,#233750,#233751,#233752,#233753,
#233754,#233755,#233756,#233757,#233758,#233759,#233760,#233761,#233762,
#233763,#233764,#233765,#233766,#233767,#233768,#233769,#233770,#233771,
#233772,#233773,#233774,#233775,#233776,#233777,#233778,#233779,#233780,
#233781,#233782,#233783,#233784,#233785,#233786,#233787,#233788,#233789,
#233790,#233791,#233792,#233793,#233794,#233795,#233796,#233797,#233798,
#233799,#233800,#233801,#233802,#233803,#233804,#233805,#233806,#233807,
#233808,#233809,#233810,#233811,#233812,#233813,#233814,#233815,#233816,
#233817,#233818,#233819,#233820,#233821,#233822,#233823,#233824,#233825,
#233826,#233827,#233828,#233829,#233830,#233831,#233832,#233833,#233834,
#233835,#233836,#233837,#233838,#233839,#233840,#233841,#233842,#233843,
#233844,#233845,#233846,#233847,#233848,#233849,#233850,#233851,#233852,
#233853,#233854,#233855,#233856,#233857,#233858,#233859,#233860,#233861,
#233862,#233863,#233864,#233865,#233866,#233867,#233868,#233869,#233870,
#233871,#233872,#233873,#233874,#233875,#233876,#233877,#233878,#233879,
#233880,#233881,#233882,#233883,#233884,#233885,#233886,#233887,#233888,
#233889,#233890,#233891,#233892,#233893,#233894,#233895,#233896,#233897,
#233898,#233899,#233900,#233901,#233902,#233903,#233904,#233905,#233906,
#233907,#233908,#233909,#233910,#233911,#233912,#233913,#233914,#233915,
#233916,#233917,#233918,#233919,#233920,#233921,#233922,#233923,#233924,
#233925,#233926,#233927,#233928,#233929,#233930,#233931,#233932,#233933,
#233934,#233935,#233936,#233937,#233938,#233939,#233940,#233941,#233942,
#233943,#233944,#233945,#233946,#233947,#233948,#233949,#233950,#233951,
#233952,#233953,#233954,#233955,#233956,#233957,#233958,#233959,#233960,
#233961,#233962,#233963,#233964,#233965,#233966,#233967,#233968,#233969,
#233970,#233971,#233972,#233973,#233974,#233975,#233976,#233977,#233978,
#233979,#233980,#233981,#233982,#233983,#233984,#233985,#233986,#233987,
#233988,#233989,#233990,#233991,#233992,#233993,#233994,#233995,#233996,
#233997,#233998,#233999,#234000,#234001,#234002,#234003,#234004,#234005,
#234006,#234007,#234008,#234009,#234010,#234011,#234012,#234013,#234014,
#234015,#234016,#234017,#234018,#234019,#234020,#234021,#234022,#234023,
#234024,#234025,#234026,#234027,#234028,#234029,#234030,#234031,#234032,
#234033,#234034,#234035,#234036,#234037,#234038,#234039,#234040,#234041,
#234042,#234043,#234044,#234045,#234046,#234047,#234048,#234049,#234050,
#234051,#234052,#234053,#234054,#234055,#234056,#234057,#234058,#234059,
#234060,#234061,#234062,#234063,#234064,#234065,#234066,#234067,#234068,
#234069,#234070,#234071,#234072,#234073,#234074,#234075,#234076,#234077,
#234078,#234079,#234080,#234081,#234082,#234083,#234084,#234085,#234086,
#234087,#234088,#234089,#234090,#234091,#234092,#234093,#234094,#234095,
#234096,#234097,#234098,#234099,#234100,#234101,#234102,#234103,#234104,
#234105,#234106,#234107,#234108,#234109,#234110,#234111,#234112,#234113,
#234114,#234115,#234116,#234117,#234118,#234119,#234120,#234121,#234122,
#234123,#234124,#234125,#234126,#234127,#234128,#234129,#234130,#234131,
#234132,#234133,#234134,#234135,#234136,#234137,#234138,#234139,#234140,
#234141,#234142,#234143,#234144,#234145,#234146,#234147,#234148,#234149,
#234150,#234151,#234152,#234153,#234154,#234155,#234156,#234157,#234158,
#234159,#234160,#234161,#234162,#234163,#234164,#234165,#234166,#234167,
#234168,#234169,#234170,#234171,#234172,#234173,#234174,#234175,#234176,
#234177,#234178,#234179,#234180,#234181,#234182,#234183,#234184,#234185,
#234186,#234187,#234188,#234189,#234190,#234191,#234192,#234193,#234194,
#234195,#234196,#234197,#234198,#234199,#234200,#234201,#234202,#234203,
#234204,#234205,#234206,#234207,#234208,#234209,#234210,#234211,#234212,
#234213,#234214,#234215,#234216,#234217,#234218,#234219,#234220,#234221,
#234222,#234223,#234224,#234225,#234226,#234227,#234228,#234229,#234230,
#234231,#234232,#234233,#234234,#234235,#234236,#234237,#234238,#234239,
#234240,#234241,#234242,#234243,#234244,#234245,#234246,#234247,#234248,
#234249,#234250,#234251,#234252,#234253,#234254,#234255,#234256,#234257,
#234258,#234259,#234260,#234261,#234262,#234263,#234264,#234265,#234266,
#234267,#234268,#234269,#234270),.UNSPECIFIED.,.F.,.F.,(4,2,2,2,2,2,2,2,
2,2,2,2,2,2,2,2,2,2,2,2,2,2,2,2,2,2,2,2,2,2,2,2,2,2,2,2,2,2,2,2,2,2,2,2,
2,2,2,2,2,2,2,2,2,2,2,2,2,2,2,2,2,2,2,2,2,2,2,2,2,2,2,2,2,2,2,2,2,2,2,2,
2,2,2,2,2,2,2,2,2,2,2,2,2,2,2,2,2,2,2,2,2,2,2,2,2,2,2,2,2,2,2,2,2,2,2,2,
2,2,2,2,2,2,2,2,2,2,2,2,2,2,2,2,2,2,2,2,2,2,2,2,2,2,2,2,2,2,2,2,2,2,2,2,
2,2,2,2,2,2,2,2,2,2,2,2,2,2,2,2,2,2,2,2,2,2,2,2,2,2,2,2,2,2,2,2,2,2,2,2,
2,2,2,2,2,2,2,2,2,2,2,2,2,2,2,2,2,2,2,2,2,2,2,2,2,2,2,2,2,2,2,2,2,2,2,2,
2,2,2,2,2,2,2,2,2,2,2,2,2,2,2,2,2,2,2,2,2,2,2,2,2,2,2,2,2,2,2,2,2,2,2,2,
2,2,2,2,2,2,2,2,2,4),(0.00205360525305213,0.0593773831792553,0.0709500426668551,
0.078387278285601,0.0842101463919144,0.0900833689727588,0.0967768172356078,
0.107906200022069,0.145521832312656,0.183512161887853,0.331647921885141,
0.380309783067713,0.386610574941088,0.390475557176331,0.393449185361408,
0.396513321521263,0.399420247524142,0.404301921621275,0.417240578218173,
0.537201828279952,0.635946020232279,0.670160334207074,0.686942760904269,
0.697107784863918,0.70639267951786,0.713552708210863,0.720528995699381,
0.730433139607536,0.758236895515654,0.966234212694743,1.01196019163004,
1.07540724372314,1.12473622823872,1.14713744478909,1.15122571308088,1.15341944632182,
1.15521863703423,1.15705682449771,1.16045990331156,1.17156797294044,1.32805796697757,
1.40356860481657,1.4937897370052,1.55412833393993,1.56532848468822,1.56905961121908,
1.57147559582088,1.57375605124961,1.57676208927215,1.58346749925563,1.63989676132955,
1.76949086823613,1.87701698099182,1.97723449858227,1.98163453464158,1.9836772509676,
1.98522828585988,1.98669558037854,1.98874187253823,1.99407399428787,2.09022757991063,
2.31426091890442,2.33083116572251,2.33926705995999,2.34447590037582,2.34904311461777,
2.35281533125918,2.35646991147333,2.3615953388166,2.37211816715402,2.46745545288722,
2.5284496864162,2.6460567307181,2.70100867185602,2.72565193418798,2.72974133771406,
2.73188788440267,2.73364041348433,2.73539782756739,2.73860491692891,2.74870976159622,
2.76637992867256,2.784918640935,2.82649458631348,2.85496790901447,2.98881103843157,
3.08335170830491,3.11857882984537,3.12364332606152,3.12622421688244,3.12809703732692,
3.13009503490561,3.13350821274674,3.14278858630628,3.27745952538948,3.43163516002308,
3.54546352338192,3.54896410693957,3.55050330045609,3.55163770428469,3.55268580471725,
3.55411384607153,3.5569680805554,3.5815431018535,3.60872192624215,3.77629372366884,
3.94407473016478,3.95016500657277,3.95287931387753,3.9548946862876,3.95676781534534,
3.9593275971224,3.96571887143421,4.03693816836897,4.17164512195338,4.27806269168589,
4.32522137383842,4.34434074334756,4.34709905676227,4.34853695790378,4.34970606435603,
4.35087475178229,4.35299452002735,4.35958585464541,4.46691401580334,4.65500045602485,
4.72757700092795,4.7601521669558,4.76528444894179,4.76794721403573,4.77010533766783,
4.77225691637946,4.77614527253955,4.78813940258596,4.97925228940441,5.15242881733038,
5.164390961761,5.1681183727177,5.1701461628033,5.17214017817843,5.17458482360079,
5.17918130914651,5.20544650410065,5.26579687621784,5.44815445466409,5.56141184189628,
5.60540178023497,5.61701461854046,5.62381041672618,5.62920234273582,5.63640900534867,
5.64991971182084,5.7376414434567,5.85141717861117,5.92048737470507,5.92791808783788,
5.93163108123368,5.93465938434876,5.93814835399665,5.94421169093895,5.97019259428511,
6.2022969742365,6.23056432947623,6.24170856281142,6.24853279283878,6.25591319113084,
6.26598870398649,6.28987618720666,6.51211520319966,6.65871075563774,6.68407446407058,
6.68816276990672,6.6905837778307,6.69242926316786,6.69439338345106,6.69744550481796,
6.70675527511992,6.75558513419176,6.78733789871383,7.08599480269894,7.10202595954001,
7.10643092943572,7.1090219341054,7.11126164476541,7.11399337028287,7.11916214303216,
7.14925243638016,7.19748962008518,7.35580622802623,7.50835243907473,7.51771672213975,
7.52052779970833,7.52222904553766,7.52373140904439,7.52484952617282,7.52751956766254,
7.53617325522243,7.59008738779717,7.65238041551183,7.77511719782402,7.87042876030836,
7.88132075575424,7.88632264737826,7.89017554013963,7.89431993812796,7.90086509899404,
7.92089791876676,8.02672945398436,8.0744434782342,8.23913441652531,8.26258080509861,
8.26682324146756,8.26900355767995,8.27072786402079,8.27236472539724,8.27522732987946,
8.28357721238536,8.32536162479298,8.34057933791867,8.39991510481678,8.57260632285271,
8.6530124525068,8.6597895352244,8.66247818182678,8.66443660328259,8.6665352689038,
8.66934713098162,8.67559609546932,8.81153970653139,8.83747737210576,8.85839597324602,
8.87589268648235,8.89084831779175,8.90381590562649,8.91517429517758,8.92520088161523,
9.0109191707375,9.02032151786773,9.08151202355462,9.08553477902998,9.08704417909839,
9.08811492807227,9.08912416099025,9.09019815694449,9.09249645058799,9.10329677071956,
9.12382449830058,9.18563346055924,9.41119241550355,9.41965029178766,9.48058705346492,
9.48672574858062,9.48924076892925,9.49110177736394,9.49312402626457,9.49588299084781,
9.50222599674433,9.61700966967578,9.81664443196399,9.82402160762228,9.87924801352412,
9.88314845096017,9.88467527486454,9.88578497181194,9.88690754280314,9.88806219203879,
9.88956622787327,9.89193273604794,9.9010358693165,9.95458350454511),
 .UNSPECIFIED.);
#3588=B_SPLINE_CURVE_WITH_KNOTS('',3,(#234272,#234273,#234274,#234275,#234276,
#234277,#234278,#234279,#234280,#234281,#234282,#234283,#234284,#234285,
#234286,#234287,#234288,#234289,#234290,#234291,#234292,#234293,#234294,
#234295,#234296,#234297,#234298,#234299,#234300,#234301,#234302,#234303,
#234304,#234305,#234306,#234307,#234308,#234309,#234310,#234311,#234312,
#234313,#234314,#234315,#234316,#234317,#234318,#234319,#234320,#234321,
#234322,#234323,#234324,#234325,#234326,#234327,#234328,#234329,#234330,
#234331,#234332,#234333,#234334,#234335,#234336,#234337,#234338,#234339,
#234340,#234341,#234342,#234343,#234344,#234345,#234346,#234347,#234348,
#234349,#234350,#234351,#234352,#234353,#234354,#234355,#234356,#234357,
#234358,#234359,#234360,#234361,#234362,#234363,#234364,#234365,#234366,
#234367,#234368,#234369,#234370,#234371,#234372,#234373,#234374,#234375,
#234376,#234377,#234378,#234379,#234380,#234381,#234382,#234383,#234384,
#234385,#234386,#234387,#234388,#234389,#234390,#234391,#234392,#234393,
#234394,#234395,#234396,#234397,#234398,#234399,#234400,#234401,#234402,
#234403,#234404,#234405,#234406,#234407,#234408,#234409,#234410,#234411,
#234412,#234413,#234414,#234415,#234416,#234417,#234418,#234419,#234420,
#234421,#234422,#234423,#234424,#234425,#234426,#234427,#234428,#234429,
#234430,#234431,#234432,#234433,#234434,#234435,#234436,#234437,#234438,
#234439,#234440,#234441,#234442,#234443,#234444,#234445,#234446,#234447,
#234448,#234449,#234450,#234451,#234452,#234453,#234454,#234455,#234456,
#234457,#234458,#234459,#234460,#234461,#234462,#234463,#234464,#234465,
#234466,#234467,#234468,#234469,#234470,#234471,#234472,#234473,#234474,
#234475,#234476,#234477,#234478,#234479,#234480,#234481,#234482,#234483,
#234484,#234485,#234486,#234487,#234488,#234489,#234490,#234491,#234492,
#234493,#234494,#234495,#234496,#234497,#234498,#234499,#234500,#234501,
#234502,#234503,#234504,#234505,#234506,#234507,#234508,#234509,#234510,
#234511,#234512,#234513,#234514,#234515,#234516,#234517,#234518,#234519,
#234520,#234521,#234522,#234523,#234524,#234525,#234526,#234527,#234528,
#234529,#234530,#234531,#234532,#234533,#234534,#234535,#234536,#234537,
#234538,#234539,#234540,#234541,#234542,#234543,#234544,#234545,#234546,
#234547,#234548,#234549,#234550,#234551,#234552,#234553,#234554,#234555,
#234556,#234557,#234558,#234559,#234560,#234561,#234562,#234563,#234564,
#234565,#234566,#234567,#234568,#234569,#234570,#234571,#234572,#234573,
#234574,#234575,#234576,#234577,#234578,#234579,#234580,#234581,#234582,
#234583,#234584,#234585,#234586,#234587,#234588,#234589,#234590,#234591,
#234592,#234593,#234594,#234595,#234596,#234597,#234598,#234599,#234600,
#234601,#234602,#234603,#234604,#234605,#234606,#234607,#234608,#234609,
#234610,#234611,#234612,#234613,#234614,#234615,#234616,#234617,#234618,
#234619,#234620,#234621,#234622,#234623,#234624,#234625,#234626,#234627,
#234628,#234629,#234630,#234631,#234632,#234633,#234634,#234635,#234636,
#234637,#234638,#234639,#234640,#234641,#234642,#234643,#234644,#234645,
#234646,#234647,#234648,#234649,#234650,#234651,#234652,#234653,#234654,
#234655,#234656,#234657,#234658,#234659,#234660,#234661,#234662,#234663,
#234664,#234665,#234666,#234667,#234668,#234669,#234670,#234671,#234672,
#234673,#234674,#234675,#234676,#234677,#234678,#234679,#234680,#234681,
#234682,#234683,#234684,#234685,#234686,#234687,#234688,#234689,#234690,
#234691,#234692,#234693,#234694,#234695,#234696,#234697,#234698,#234699,
#234700,#234701,#234702,#234703,#234704,#234705,#234706,#234707,#234708,
#234709,#234710,#234711,#234712,#234713,#234714,#234715,#234716,#234717,
#234718,#234719,#234720,#234721,#234722,#234723,#234724,#234725,#234726,
#234727,#234728,#234729,#234730,#234731,#234732,#234733,#234734,#234735,
#234736,#234737,#234738,#234739,#234740,#234741,#234742,#234743,#234744,
#234745,#234746,#234747,#234748,#234749,#234750,#234751,#234752,#234753,
#234754,#234755,#234756,#234757,#234758,#234759,#234760,#234761,#234762,
#234763,#234764,#234765,#234766,#234767,#234768,#234769,#234770,#234771,
#234772,#234773,#234774,#234775,#234776,#234777,#234778,#234779,#234780,
#234781,#234782,#234783,#234784,#234785,#234786,#234787,#234788,#234789,
#234790,#234791,#234792,#234793,#234794,#234795,#234796,#234797,#234798,
#234799,#234800,#234801,#234802,#234803,#234804,#234805,#234806,#234807,
#234808,#234809,#234810,#234811,#234812,#234813,#234814,#234815,#234816,
#234817,#234818,#234819,#234820,#234821,#234822,#234823,#234824,#234825,
#234826,#234827,#234828,#234829,#234830,#234831,#234832,#234833,#234834,
#234835,#234836,#234837,#234838,#234839,#234840,#234841,#234842,#234843,
#234844,#234845,#234846,#234847,#234848,#234849,#234850,#234851,#234852,
#234853,#234854,#234855,#234856,#234857,#234858,#234859,#234860,#234861,
#234862,#234863,#234864,#234865,#234866,#234867,#234868,#234869,#234870,
#234871,#234872,#234873,#234874,#234875,#234876,#234877),.UNSPECIFIED.,
 .F.,.F.,(4,2,2,2,2,2,2,2,2,2,2,2,2,2,2,2,2,2,2,2,2,2,2,2,2,2,2,2,2,2,2,
2,2,2,2,2,2,2,2,2,2,2,2,2,2,2,2,2,2,2,2,2,2,2,2,2,2,2,2,2,2,2,2,2,2,2,2,
2,2,2,2,2,2,2,2,2,2,2,2,2,2,2,2,2,2,2,2,2,2,2,2,2,2,2,2,2,2,2,2,2,2,2,2,
2,2,2,2,2,2,2,2,2,2,2,2,2,2,2,2,2,2,2,2,2,2,2,2,2,2,2,2,2,2,2,2,2,2,2,2,
2,2,2,2,2,2,2,2,2,2,2,2,2,2,2,2,2,2,2,2,2,2,2,2,2,2,2,2,2,2,2,2,2,2,2,2,
2,2,2,2,2,2,2,2,2,2,2,2,2,2,2,2,2,2,2,2,2,2,2,2,2,2,2,2,2,2,2,2,2,2,2,2,
2,2,2,2,2,2,2,2,2,2,2,2,2,2,2,2,2,2,2,2,2,2,2,2,2,2,2,2,2,2,2,2,2,2,2,2,
2,2,2,2,2,2,2,2,2,2,2,2,2,2,2,2,2,2,2,2,2,2,2,2,2,2,2,2,2,2,2,2,2,2,2,2,
2,2,2,2,2,2,2,2,2,2,2,2,2,2,2,2,2,2,2,4),(0.00298799696991318,0.284548765783284,
0.324998927055044,0.346725222155488,0.351305191664363,0.353849462103799,
0.355790169769175,0.358278477046583,0.362493946379329,0.377687442785345,
0.66059392337514,0.692141903033456,0.74376107945835,0.751799365416695,0.754868007480455,
0.756748203307425,0.75875736883098,0.761424396136439,0.767062140285104,
0.813045040613457,0.851696620085529,0.966681559443179,1.18248503247399,
1.19970929428457,1.20764425203756,1.21368870322025,1.21943727358696,1.22753303494866,
1.24933838462884,1.39644278402009,1.49756032582151,1.50718066805563,1.51447769270129,
1.51816799080709,1.52119605835027,1.52461057865531,1.528486301843,1.54176519756824,
1.64990297845833,1.76907429410024,1.81353878448344,1.82626300613302,1.83418715327372,
1.84150036838553,1.85097416731601,1.87191821243426,1.91125857047846,2.00269496746611,
2.15544490963139,2.21564526546191,2.26959544567536,2.27454803620845,2.27691910327582,
2.27871753272058,2.28066213035479,2.28368242512681,2.29237227960743,2.41431295984751,
2.52924991619505,2.64228407850674,2.68569748934479,2.69135654976542,2.69419162031758,
2.69622968291942,2.69838618730555,2.70141668921914,2.70767060469526,2.77212923676101,
3.00228363882309,3.10122818216294,3.10573712412653,3.10780052101499,3.10932669216269,
3.11094032735715,3.11337516754345,3.11995516740608,3.12909479836546,3.13647279354061,
3.32450255266738,3.45563082949889,3.46750153588689,3.47274025719392,3.47661910396445,
3.48022182328744,3.48514892266501,3.49738398487739,3.65955108685084,3.78189312907216,
3.82847781518075,3.85011695632573,3.85406506303475,3.85618166033255,3.85791637276539,
3.85995415785783,3.8634461258874,3.87641739633784,4.11471652493715,4.17295090954306,
4.21998032789621,4.24401684337691,4.24859622282434,4.25107487411233,4.25311851524632,
4.25553322655929,4.25970597316534,4.27558213461076,4.56266753812426,4.62094811823215,
4.66614181437333,4.67321956954466,4.67524610460064,4.67648363998103,4.67760182436175,
4.67903262957894,4.68202531574454,4.70216719251704,4.87116396568071,4.98214133931871,
5.06837894972334,5.07509185703591,5.07770673777867,5.07959479344217,5.08160253718232,
5.08426594247148,5.09007785230583,5.18458896375922,5.36353426498577,5.46450593290116,
5.47120978641427,5.47331677306128,5.47448291547406,5.47565289450548,5.47709636506131,
5.47987739632411,5.49738898961177,5.53660580707938,5.60359509018789,5.68135984876374,
5.72282644617998,5.77733392846139,5.78255071137604,5.79752027473821,5.8826017497064,
5.88972222839802,5.89253898445213,5.89458793407069,5.89678101119802,5.89971480069819,
5.90621649758936,6.04659169101303,6.1880630934402,6.22382424185533,6.28644160115385,
6.29236817336843,6.29505089337251,6.29709753693096,6.29927708753388,6.30266713472379,
6.31304151492471,6.44373525924046,6.66293617186134,6.72930784022965,6.74195126360323,
6.74896039003915,6.75474814701651,6.76168794798178,6.77393682564694,6.83220505472201,
6.963394911328,7.0086240185794,7.04809320969585,7.05412042887509,7.0579068482803,
7.06094252491028,7.06438300306789,7.07010359180137,7.09075113572629,7.12870279050102,
7.25112988858497,7.29508607544355,7.30174672313976,7.35156376228543,7.36504335588487,
7.37309971220848,7.3801985505715,7.38913573684223,7.40668576792219,7.50750554505508,
7.64480123736787,7.76762089597334,7.77480722676958,7.80973069737468,7.81471279126246,
7.81706468222407,7.81890038753219,7.82089693743581,7.82409069312295,7.83458325074647,
7.89411208133,8.0649478922328,8.21990728815591,8.2297296047366,8.23339632818336,
8.23555827492464,8.23759491135854,8.24041759155522,8.24601435703751,8.28654843353863,
8.38716979905904,8.45819940578936,8.63253257031194,8.6438349884074,8.64687495326056,
8.64865401811518,8.65017146464981,8.65202655136355,8.65549716417568,8.67472986534528,
8.71597425739663,8.74999292881849,8.77587831713415,8.83529161266237,8.99640837878672,
9.00768371203758,9.01284299678956,9.01666126575537,9.01685702865119,9.01688451776892,
9.01691093381246,9.01693631941594,9.01696071608408,9.01698416361527,9.01700670017908,
9.01702836231571,9.01704918504256,9.01706920194387,9.01708844520265,9.01710229598491,
9.01711601142003,9.01712959720982,9.01714305477671,9.0171563855366,9.01716959082916,
9.01718267195316,9.01719563028769,9.01720846710627,9.0172211837034,9.01723378135626,
9.01724626132437,9.0172586248577,9.01727087321867,9.01728300759856,9.01729502927146,
9.01730693938076,9.01731873917141,9.01733042971497,9.01734201220508,9.0173534878348,
9.01736485761211,9.01737612271136,9.01738728428401,9.01739834328824,9.01740930083484,
9.01742015799366,9.01743091585589,9.01744157542675,9.01745213774419,9.01746260383416,
9.01747297469172,9.01748325129263,9.01749343469561,9.01750352578474,9.01751352550644,
9.01752343481792,9.01753325468627,9.02173162943359,9.02879505359289,9.05298730611816,
9.22099259945438,9.31932129227878,9.3622738721429,9.38969638335723,9.39418775108313,
9.39644971286767,9.3982146578637,9.40016301155353,9.40334330437531,9.4143720901834,
9.48073396554205,9.55247242503873,9.58468629245607,9.60168085315791,9.6213175865944,
9.77629978667344,9.78656475456521,9.79012509040459,9.79215399775925,9.79402142642433,
9.79654271237396,9.79922118703221,9.80344490315052,9.83479378676887,9.96256522287139),
 .UNSPECIFIED.);
#3589=B_SPLINE_CURVE_WITH_KNOTS('',3,(#234879,#234880,#234881,#234882,#234883,
#234884,#234885,#234886,#234887,#234888,#234889,#234890,#234891,#234892,
#234893,#234894,#234895,#234896,#234897,#234898,#234899,#234900,#234901,
#234902,#234903,#234904,#234905,#234906,#234907,#234908,#234909,#234910,
#234911,#234912,#234913,#234914,#234915,#234916,#234917,#234918,#234919,
#234920,#234921,#234922,#234923,#234924,#234925,#234926,#234927,#234928,
#234929,#234930,#234931,#234932,#234933,#234934,#234935,#234936,#234937,
#234938,#234939,#234940,#234941,#234942,#234943,#234944,#234945,#234946,
#234947,#234948,#234949,#234950,#234951,#234952,#234953,#234954,#234955,
#234956,#234957,#234958,#234959,#234960,#234961,#234962,#234963,#234964,
#234965,#234966,#234967,#234968,#234969,#234970,#234971,#234972,#234973,
#234974,#234975,#234976,#234977,#234978,#234979,#234980,#234981,#234982,
#234983,#234984,#234985,#234986,#234987,#234988,#234989,#234990,#234991,
#234992,#234993,#234994,#234995,#234996,#234997,#234998,#234999,#235000,
#235001,#235002,#235003,#235004,#235005,#235006,#235007,#235008,#235009,
#235010,#235011,#235012,#235013,#235014,#235015,#235016,#235017,#235018,
#235019,#235020,#235021,#235022,#235023,#235024,#235025,#235026,#235027,
#235028,#235029,#235030,#235031,#235032,#235033,#235034,#235035,#235036,
#235037,#235038,#235039,#235040,#235041,#235042,#235043,#235044,#235045,
#235046,#235047,#235048,#235049,#235050,#235051,#235052,#235053,#235054,
#235055,#235056,#235057,#235058,#235059,#235060,#235061,#235062,#235063,
#235064,#235065,#235066,#235067,#235068,#235069,#235070,#235071,#235072,
#235073,#235074,#235075,#235076,#235077,#235078,#235079,#235080,#235081,
#235082,#235083,#235084,#235085,#235086,#235087,#235088,#235089,#235090,
#235091,#235092,#235093,#235094,#235095,#235096,#235097,#235098,#235099,
#235100,#235101,#235102,#235103,#235104,#235105,#235106,#235107,#235108,
#235109,#235110,#235111,#235112,#235113,#235114,#235115,#235116,#235117,
#235118,#235119,#235120,#235121,#235122,#235123,#235124,#235125,#235126,
#235127,#235128,#235129,#235130,#235131,#235132,#235133,#235134),
 .UNSPECIFIED.,.F.,.F.,(4,3,3,3,3,3,3,3,3,3,3,3,3,3,3,3,3,3,3,3,3,3,3,3,
3,3,3,3,3,3,3,3,3,3,3,3,3,3,3,3,3,3,3,3,3,3,3,3,3,3,3,3,3,3,3,3,3,3,3,3,
3,3,3,3,3,3,3,3,3,3,3,3,3,3,3,3,3,3,3,3,3,3,3,3,3,4),(-267.986713186487,
-267.895065432478,-267.802448421134,-267.708773505748,-267.662249211065,
-267.589110267381,-267.516059350074,-267.443081526052,-267.370161931536,
-267.29728575656,-267.224438230978,-267.151590733819,-267.078739585281,
-267.00587143618,-266.932972926128,-266.859987484565,-266.786954671789,
-266.713810247672,-266.663509475203,-266.587981186536,-266.512538991203,
-266.437169983508,-266.361861305545,-266.286600139145,-266.208871339169,
-266.133661141844,-266.058456917146,-265.983247106881,-265.908020151895,
-265.832737262285,-265.757421215414,-265.682034306157,-265.664769739341,
-265.588177838941,-265.511651137,-265.435179941109,-265.358763080849,-265.282379042015,
-265.206018878603,-265.16539987141,-265.087280602929,-265.009116299454,
-264.930902222464,-264.852597099774,-264.774243673173,-264.695804583406,
-264.666030003478,-264.584051224892,-264.502144475652,-264.418273390626,
-264.336607978112,-264.251634056829,-264.166660135547,-264.093048461441,
-264.019442094588,-263.945828042687,-263.872161750158,-263.798468222134,
-263.724692749069,-263.667290267616,-263.59078954281,-263.514344775629,
-263.437945056048,-263.361579506442,-263.285237274251,-263.208151431439,
-263.131809618062,-263.05545753042,-262.979085306312,-262.901451612672,
-262.824979935679,-262.746765233717,-262.668550531754,-262.593868717066,
-262.519266864914,-262.444732581341,-262.370264023807,-262.295833808213,
-262.221428896414,-262.169180663823,-262.090168152782,-262.011043352256,
-261.931733613374,-261.852330853427,-261.772764020692,-261.703528014493),
 .UNSPECIFIED.);
#3590=B_SPLINE_CURVE_WITH_KNOTS('',3,(#235136,#235137,#235138,#235139,#235140,
#235141,#235142,#235143,#235144,#235145,#235146,#235147,#235148,#235149),
 .UNSPECIFIED.,.F.,.F.,(4,2,1,1,1,1,1,1,1,1,4),(-261.703527798163,-261.669810795892,
-260.67107106003,-259.672331324168,-258.673591588305,-258.174221720374,
-257.674851852443,-257.175481984512,-256.676112116581,-255.677372380719,
-255.420342707314),.UNSPECIFIED.);
#3591=B_SPLINE_CURVE_WITH_KNOTS('',3,(#235151,#235152,#235153,#235154,#235155,
#235156,#235157,#235158,#235159,#235160,#235161,#235162,#235163,#235164,
#235165,#235166,#235167,#235168),.UNSPECIFIED.,.F.,.F.,(4,2,2,2,2,2,2,2,
4),(-255.420342707314,-254.585425795419,-253.750508883524,-252.915591971629,
-252.080675059734,-251.245758147839,-250.410841235945,-249.57592432405,
-249.137157400134),.UNSPECIFIED.);
#3592=B_SPLINE_CURVE_WITH_KNOTS('',3,(#235170,#235171,#235172,#235173,#235174,
#235175,#235176,#235177,#235178,#235179,#235180,#235181,#235182,#235183,
#235184,#235185,#235186,#235187),.UNSPECIFIED.,.F.,.F.,(4,2,2,2,2,2,2,2,
4),(-249.137157400134,-248.302240488239,-247.467323576345,-246.63240666445,
-245.797489752555,-244.96257284066,-244.127655928765,-243.29273901687,-242.853972092955),
 .UNSPECIFIED.);
#3593=B_SPLINE_CURVE_WITH_KNOTS('',3,(#235189,#235190,#235191,#235192,#235193,
#235194,#235195,#235196,#235197,#235198,#235199,#235200,#235201,#235202,
#235203,#235204,#235205,#235206),.UNSPECIFIED.,.F.,.F.,(4,2,2,2,2,2,2,2,
4),(-242.853972092955,-242.01905518106,-241.184138269165,-240.34922135727,
-239.514304445375,-238.67938753348,-237.844470621585,-237.009553709691,
-236.570786785775),.UNSPECIFIED.);
#3594=B_SPLINE_CURVE_WITH_KNOTS('',3,(#235208,#235209,#235210,#235211,#235212,
#235213,#235214,#235215,#235216,#235217,#235218,#235219,#235220,#235221,
#235222,#235223,#235224,#235225),.UNSPECIFIED.,.F.,.F.,(4,2,2,2,2,2,2,2,
4),(-236.570786785775,-235.73586987388,-234.900952961985,-234.066036050091,
-233.231119138196,-232.396202226301,-231.561285314406,-230.726368402511,
-230.287602016329),.UNSPECIFIED.);
#3595=B_SPLINE_CURVE_WITH_KNOTS('',3,(#235227,#235228,#235229,#235230,#235231,
#235232,#235233,#235234,#235235,#235236,#235237,#235238,#235239,#235240,
#235241,#235242,#235243,#235244,#235245,#235246,#235247,#235248,#235249,
#235250,#235251,#235252,#235253,#235254,#235255,#235256,#235257,#235258,
#235259,#235260,#235261,#235262,#235263,#235264,#235265,#235266,#235267,
#235268,#235269,#235270,#235271,#235272,#235273,#235274,#235275,#235276,
#235277,#235278,#235279,#235280,#235281,#235282,#235283,#235284,#235285,
#235286,#235287,#235288,#235289,#235290,#235291,#235292,#235293,#235294,
#235295,#235296,#235297,#235298,#235299,#235300,#235301,#235302,#235303,
#235304,#235305,#235306,#235307,#235308,#235309,#235310,#235311,#235312,
#235313,#235314,#235315,#235316,#235317,#235318,#235319,#235320,#235321,
#235322,#235323,#235324,#235325,#235326,#235327,#235328,#235329,#235330,
#235331,#235332,#235333,#235334,#235335,#235336,#235337,#235338,#235339,
#235340,#235341,#235342,#235343,#235344,#235345,#235346,#235347,#235348,
#235349,#235350,#235351,#235352,#235353,#235354,#235355,#235356,#235357,
#235358,#235359,#235360,#235361,#235362,#235363,#235364,#235365,#235366,
#235367,#235368,#235369,#235370,#235371,#235372,#235373,#235374,#235375,
#235376,#235377,#235378,#235379,#235380,#235381,#235382,#235383,#235384,
#235385,#235386,#235387,#235388,#235389,#235390,#235391,#235392,#235393,
#235394,#235395,#235396,#235397,#235398,#235399,#235400,#235401,#235402,
#235403,#235404,#235405,#235406,#235407,#235408,#235409,#235410,#235411,
#235412,#235413,#235414,#235415,#235416,#235417,#235418,#235419,#235420,
#235421,#235422,#235423,#235424,#235425,#235426,#235427,#235428,#235429,
#235430,#235431,#235432,#235433,#235434,#235435,#235436,#235437,#235438,
#235439,#235440,#235441,#235442,#235443,#235444,#235445,#235446,#235447,
#235448,#235449,#235450,#235451,#235452,#235453,#235454,#235455,#235456,
#235457,#235458,#235459,#235460,#235461,#235462,#235463,#235464,#235465,
#235466,#235467,#235468,#235469,#235470,#235471,#235472,#235473,#235474,
#235475,#235476,#235477,#235478,#235479,#235480,#235481,#235482,#235483,
#235484,#235485,#235486,#235487,#235488,#235489,#235490,#235491,#235492,
#235493,#235494,#235495,#235496,#235497,#235498,#235499,#235500,#235501,
#235502,#235503,#235504,#235505,#235506,#235507,#235508,#235509,#235510,
#235511,#235512,#235513,#235514,#235515,#235516,#235517,#235518,#235519,
#235520,#235521,#235522,#235523,#235524,#235525,#235526,#235527,#235528,
#235529,#235530,#235531,#235532,#235533,#235534,#235535,#235536,#235537,
#235538,#235539,#235540,#235541,#235542,#235543,#235544,#235545,#235546,
#235547,#235548,#235549,#235550,#235551,#235552,#235553,#235554,#235555,
#235556,#235557,#235558,#235559,#235560,#235561,#235562,#235563,#235564,
#235565,#235566,#235567,#235568,#235569,#235570,#235571,#235572,#235573,
#235574,#235575,#235576,#235577,#235578,#235579,#235580,#235581,#235582,
#235583,#235584,#235585,#235586,#235587,#235588,#235589,#235590,#235591,
#235592,#235593,#235594,#235595,#235596,#235597,#235598,#235599,#235600,
#235601,#235602,#235603,#235604,#235605,#235606,#235607,#235608,#235609,
#235610,#235611,#235612,#235613,#235614,#235615,#235616,#235617,#235618,
#235619,#235620,#235621,#235622,#235623,#235624,#235625,#235626,#235627,
#235628,#235629,#235630,#235631,#235632,#235633,#235634,#235635,#235636,
#235637,#235638,#235639,#235640,#235641,#235642,#235643,#235644,#235645,
#235646,#235647,#235648,#235649,#235650,#235651,#235652,#235653,#235654,
#235655,#235656,#235657,#235658,#235659,#235660,#235661,#235662,#235663,
#235664,#235665,#235666,#235667,#235668,#235669,#235670,#235671,#235672,
#235673,#235674,#235675,#235676,#235677,#235678,#235679,#235680,#235681,
#235682,#235683,#235684,#235685,#235686,#235687,#235688,#235689,#235690,
#235691,#235692,#235693,#235694,#235695,#235696,#235697,#235698,#235699,
#235700,#235701,#235702,#235703,#235704,#235705,#235706,#235707,#235708,
#235709,#235710,#235711,#235712,#235713,#235714,#235715,#235716,#235717,
#235718,#235719,#235720,#235721,#235722,#235723,#235724,#235725,#235726,
#235727,#235728,#235729,#235730,#235731,#235732,#235733,#235734,#235735,
#235736,#235737,#235738,#235739,#235740,#235741,#235742,#235743,#235744,
#235745,#235746,#235747,#235748,#235749,#235750,#235751,#235752,#235753,
#235754),.UNSPECIFIED.,.F.,.F.,(4,2,2,2,2,2,2,2,2,2,2,2,2,2,2,2,2,2,2,2,
2,2,2,2,2,2,2,2,2,2,2,2,2,2,2,2,2,2,2,2,2,2,2,2,2,2,2,2,2,2,2,2,2,2,2,2,
2,2,2,2,2,2,2,2,2,2,2,2,2,2,2,2,2,2,2,2,2,2,2,2,2,2,2,2,2,2,2,2,2,2,2,2,
2,2,2,2,2,2,2,2,2,2,2,2,2,2,2,2,2,2,2,2,2,2,2,2,2,2,2,2,2,2,2,2,2,2,2,2,
2,2,2,2,2,2,2,2,2,2,2,2,2,2,2,2,2,2,2,2,2,2,2,2,2,2,2,2,2,2,2,2,2,2,2,2,
2,2,2,2,2,2,2,2,2,2,2,2,2,2,2,2,2,2,2,2,2,2,2,2,2,2,2,2,2,2,2,2,2,2,2,2,
2,2,2,2,2,2,2,2,2,2,2,2,2,2,2,2,2,2,2,2,2,2,2,2,2,2,2,2,2,2,2,2,2,2,2,2,
2,2,2,2,2,2,2,2,2,2,2,2,2,2,2,2,2,2,2,2,2,2,2,2,2,2,2,4),(0.00169204175923553,
0.128820729549866,0.140683025697351,0.148239355435246,0.154099751533378,
0.159924582078469,0.165707733094985,0.175623411871471,0.203402886356974,
0.263964772043401,0.302904995997001,0.40067121699731,0.448936386886242,
0.458962870963235,0.462230108879606,0.46505189696762,0.468101290201929,
0.4720210615819,0.480135792335445,0.547890937157175,0.584005929628486,0.678993742421287,
0.729124166352655,0.751100998364294,0.768396438538095,0.777259485312679,
0.784349980201744,0.792546544477399,0.806545531812426,0.862443329299604,
1.05576876431122,1.12858114708919,1.18912499742063,1.21670182157923,1.22104091711757,
1.22328782371271,1.22510716381907,1.22691905878811,1.23019139750927,1.24025612684883,
1.38650270824074,1.48438440875138,1.59010145705835,1.63193953570891,1.63755223969695,
1.64037795327922,1.64241478874154,1.64457509822983,1.647619307508,1.65392866794775,
1.72056071707936,1.72798325846529,1.83832078293851,1.91810726604842,1.9938072517963,
2.00811599113056,2.03504711049864,2.04911690525961,2.05233998483585,2.05414124676916,
2.0555204334066,2.05706506452728,2.05990392965606,2.06903323549553,2.2694105348947,
2.38950596251023,2.40329786963805,2.4138757783152,2.41885878175748,2.42249017097881,
2.42609434920214,2.43102647218762,2.44079878655823,2.51187178886177,2.55180317775188,
2.68459742272682,2.76524027888333,2.79529881490304,2.79961307049101,2.80180679976827,
2.80339658996465,2.805090871918,2.80749110791666,2.81396474196005,2.89957851414183,
3.02964073147012,3.12935166732212,3.16144850191309,3.18924472845449,3.19401451073827,
3.19653421577097,3.19840018891676,3.20042725333625,3.20398378810365,3.21423167167558,
3.36141446846769,3.51863597739258,3.57398848603187,3.61202332116103,3.61838305501683,
3.62033162805872,3.62155169738221,3.62267442709653,3.62411604503934,3.6272487747198,
3.65080155909433,3.75795219330761,3.91884444431871,4.01486876972315,4.02069258082322,
4.02335823456778,4.02536634283641,4.027253780909,4.02986628694234,4.03656467908008,
4.12247782165953,4.3118803869199,4.39221401883121,4.41487996418079,4.41774571437491,
4.41920619622363,4.42026667955683,4.42139854218053,4.42333276780259,4.42859603003401,
4.51319801795877,4.69466099315154,4.79137056726509,4.83066288951878,4.83603576457255,
4.8387492661589,4.84070860666857,4.84278985202896,4.84572781629199,4.85358660094087,
4.97971560591509,5.22203897867044,5.23532474586461,5.23920967770097,5.24149947805944,
5.2434986370988,5.24600236257967,5.25087576676225,5.28389372599522,5.37147028218351,
5.44957751348197,5.59368552850528,5.67368575373751,5.68572240553988,5.69332205030121,
5.69932544446027,5.70605532303809,5.71734813236724,5.76178475147623,5.84356915572153,
5.98565499882068,5.99744099848249,6.0014733544957,6.00436836048662,6.00743696770192,
6.01149238485903,6.02031287945392,6.10682909705381,6.27746254598682,6.3030915218253,
6.31273421121391,6.31964289014398,6.32697732741801,6.33675018470292,6.35880962872048,
6.54833670380946,6.74727039439894,6.74998377749953,6.75857061786715,6.76157403299604,
6.76351437709716,6.76526586662232,6.76762039591887,6.77248700424533,6.82837164971718,
6.86031354783463,7.15807473009532,7.17413169191457,7.1785411150683,7.18113416937885,
7.18337530307501,7.18610832659734,7.1912782385094,7.22134050042427,7.26688401961591,
7.38764540583095,7.49218527626971,7.54778505620299,7.58744352305227,7.59171346905189,
7.59352115934466,7.59507465946784,7.59652145567753,7.59872843975061,7.60404536907063,
7.61142088518676,7.69569447150197,7.85616488913764,7.94322063727004,7.95391394755627,
7.95887997287957,7.96272876548692,7.96689214700736,7.97351737711832,7.99414433217313,
8.10515945361295,8.29427107004716,8.33066535288816,8.33810378391215,8.34087396869458,
8.3424528111761,8.34416494034495,8.34636985810621,8.35073968853788,8.38373367652693,
8.41328961371291,8.47258339069487,8.6430064111253,8.72588262336472,8.73271165494646,
8.73540978983135,8.73737122634909,8.73946946073971,8.74227442225615,8.74848222362601,
8.87346131447097,8.90295973531925,8.92832892186743,8.94926142702981,8.96706624758196,
8.98250506767304,8.99607309430263,9.04305659958386,9.12973743231144,9.1557935455754,
9.15906608125554,9.16054714558957,9.16167610861934,9.16271540183624,9.16389057355239,
9.16719897728497,9.1716457970705,9.18253256765766,9.21969436889805,9.27912567786901,
9.54063424822291,9.55730314222564,9.56107039710376,9.56352925890164,9.5655107761421,
9.56776523854358,9.57160472181438,9.5866803364728,9.69681320649013,9.92869023299713,
9.93814457512901,9.95463105348814,9.95744203340321,9.958588076165),
 .UNSPECIFIED.);
#3596=B_SPLINE_CURVE_WITH_KNOTS('',3,(#235756,#235757,#235758,#235759,#235760,
#235761,#235762,#235763,#235764,#235765,#235766,#235767,#235768),
 .UNSPECIFIED.,.F.,.F.,(4,1,1,1,1,1,1,1,1,1,4),(-217.721230864236,-216.726522682094,
-216.227152814163,-215.727782946231,-215.2284130783,-214.729043210369,-213.730303474507,
-213.230933606576,-212.731563738645,-211.732824002783,-211.438045557057),
 .UNSPECIFIED.);
#3597=B_SPLINE_CURVE_WITH_KNOTS('',3,(#235770,#235771,#235772,#235773,#235774,
#235775,#235776,#235777,#235778,#235779,#235780,#235781,#235782,#235783,
#235784,#235785,#235786,#235787),.UNSPECIFIED.,.F.,.F.,(4,2,2,2,2,2,2,2,
4),(-211.438045557057,-210.603128645162,-209.768211733267,-208.933294821372,
-208.098377909477,-207.263460997582,-206.428544085688,-205.593627173793,
-205.154860249877),.UNSPECIFIED.);
#3598=B_SPLINE_CURVE_WITH_KNOTS('',3,(#235789,#235790,#235791,#235792,#235793,
#235794,#235795,#235796,#235797,#235798,#235799,#235800,#235801),
 .UNSPECIFIED.,.F.,.F.,(4,1,1,1,1,1,1,1,1,1,4),(-205.154860249877,-204.741645851748,
-204.242275983816,-203.742906115885,-202.744166380023,-202.244796512092,
-201.745426644161,-201.24605677623,-200.746686908299,-199.747947172437,
-198.872317216215),.UNSPECIFIED.);
#3599=B_SPLINE_CURVE_WITH_KNOTS('',3,(#235803,#235804,#235805,#235806,#235807,
#235808,#235809,#235810,#235811,#235812,#235813,#235814,#235815,#235816,
#235817,#235818,#235819,#235820,#235821,#235822,#235823,#235824,#235825,
#235826,#235827,#235828,#235829,#235830,#235831,#235832,#235833,#235834,
#235835,#235836,#235837,#235838,#235839,#235840,#235841,#235842,#235843,
#235844,#235845,#235846,#235847,#235848,#235849,#235850,#235851,#235852,
#235853,#235854,#235855,#235856,#235857,#235858,#235859,#235860,#235861,
#235862,#235863,#235864,#235865,#235866,#235867,#235868,#235869,#235870,
#235871,#235872,#235873,#235874,#235875,#235876,#235877,#235878,#235879,
#235880,#235881,#235882,#235883,#235884,#235885,#235886,#235887,#235888,
#235889,#235890,#235891,#235892,#235893,#235894,#235895,#235896,#235897,
#235898,#235899,#235900,#235901,#235902,#235903,#235904,#235905,#235906,
#235907,#235908,#235909,#235910,#235911,#235912,#235913,#235914,#235915,
#235916,#235917,#235918,#235919,#235920,#235921,#235922,#235923,#235924,
#235925,#235926,#235927,#235928,#235929,#235930,#235931,#235932,#235933,
#235934,#235935,#235936,#235937,#235938,#235939,#235940,#235941,#235942,
#235943,#235944,#235945,#235946,#235947,#235948,#235949,#235950,#235951,
#235952,#235953,#235954,#235955,#235956,#235957,#235958,#235959,#235960,
#235961,#235962,#235963,#235964,#235965,#235966,#235967,#235968,#235969,
#235970,#235971,#235972,#235973,#235974,#235975,#235976,#235977,#235978,
#235979,#235980,#235981,#235982,#235983,#235984,#235985,#235986,#235987,
#235988,#235989,#235990,#235991,#235992,#235993,#235994,#235995,#235996,
#235997,#235998,#235999,#236000,#236001,#236002,#236003,#236004,#236005,
#236006,#236007,#236008,#236009,#236010,#236011,#236012,#236013,#236014,
#236015,#236016,#236017,#236018,#236019,#236020,#236021,#236022,#236023,
#236024,#236025,#236026,#236027,#236028,#236029,#236030,#236031,#236032,
#236033,#236034,#236035,#236036,#236037,#236038,#236039,#236040,#236041,
#236042,#236043,#236044,#236045,#236046,#236047,#236048,#236049,#236050,
#236051,#236052,#236053,#236054,#236055,#236056,#236057,#236058,#236059,
#236060,#236061,#236062,#236063,#236064,#236065,#236066,#236067,#236068,
#236069,#236070,#236071,#236072,#236073,#236074,#236075,#236076,#236077,
#236078,#236079,#236080,#236081,#236082,#236083,#236084,#236085,#236086,
#236087,#236088,#236089,#236090,#236091,#236092,#236093,#236094,#236095,
#236096,#236097,#236098,#236099,#236100,#236101,#236102,#236103,#236104,
#236105,#236106,#236107,#236108,#236109,#236110,#236111,#236112,#236113,
#236114,#236115,#236116,#236117,#236118,#236119,#236120,#236121,#236122,
#236123,#236124,#236125,#236126,#236127,#236128,#236129,#236130,#236131,
#236132,#236133,#236134,#236135,#236136,#236137,#236138,#236139,#236140,
#236141,#236142,#236143,#236144,#236145,#236146,#236147,#236148,#236149,
#236150,#236151,#236152,#236153,#236154,#236155,#236156,#236157,#236158,
#236159,#236160,#236161,#236162,#236163,#236164,#236165,#236166,#236167,
#236168,#236169,#236170,#236171,#236172,#236173,#236174,#236175,#236176,
#236177,#236178,#236179,#236180,#236181,#236182,#236183,#236184,#236185,
#236186,#236187,#236188,#236189,#236190,#236191,#236192,#236193,#236194,
#236195,#236196,#236197,#236198,#236199,#236200,#236201,#236202,#236203,
#236204,#236205,#236206,#236207,#236208,#236209,#236210,#236211,#236212,
#236213,#236214,#236215,#236216,#236217,#236218,#236219,#236220,#236221,
#236222,#236223,#236224,#236225,#236226,#236227,#236228,#236229,#236230,
#236231,#236232,#236233,#236234,#236235,#236236,#236237,#236238,#236239,
#236240,#236241,#236242,#236243,#236244,#236245,#236246,#236247,#236248,
#236249,#236250,#236251,#236252,#236253,#236254,#236255,#236256,#236257,
#236258,#236259,#236260,#236261,#236262,#236263,#236264,#236265,#236266,
#236267,#236268,#236269,#236270,#236271,#236272,#236273,#236274,#236275,
#236276,#236277,#236278,#236279,#236280,#236281,#236282,#236283,#236284,
#236285,#236286,#236287,#236288,#236289,#236290,#236291,#236292,#236293,
#236294,#236295,#236296,#236297,#236298,#236299,#236300,#236301,#236302,
#236303,#236304,#236305,#236306,#236307,#236308,#236309,#236310,#236311,
#236312,#236313,#236314),.UNSPECIFIED.,.F.,.F.,(4,2,2,2,2,2,2,2,2,2,2,2,
2,2,2,2,2,2,2,2,2,2,2,2,2,2,2,2,2,2,2,2,2,2,2,2,2,2,2,2,2,2,2,2,2,2,2,2,
2,2,2,2,2,2,2,2,2,2,2,2,2,2,2,2,2,2,2,2,2,2,2,2,2,2,2,2,2,2,2,2,2,2,2,2,
2,2,2,2,2,2,2,2,2,2,2,2,2,2,2,2,2,2,2,2,2,2,2,2,2,2,2,2,2,2,2,2,2,2,2,2,
2,2,2,2,2,2,2,2,2,2,2,2,2,2,2,2,2,2,2,2,2,2,2,2,2,2,2,2,2,2,2,2,2,2,2,2,
2,2,2,2,2,2,2,2,2,2,2,2,2,2,2,2,2,2,2,2,2,2,2,2,2,2,2,2,2,2,2,2,2,2,2,2,
2,2,2,2,2,2,2,2,2,2,2,2,2,2,2,2,2,2,2,2,2,2,2,2,2,2,2,2,2,2,2,2,2,2,2,2,
2,2,2,2,2,2,2,2,2,2,2,2,2,2,2,2,2,2,2,2,2,2,2,2,2,2,2,4),(0.00191394602328637,
0.0944684754693169,0.0968787543811911,0.0983665318117488,0.0994814529629017,
0.100615559975077,0.101664719732112,0.103090817090912,0.105887054240193,
0.12763755181692,0.173614383098775,0.17623185663861,0.193988745972456,0.201991997469711,
0.388809479155954,0.47888957738054,0.515488743238011,0.520600192581283,
0.523190882670798,0.525065193613106,0.527059499253994,0.530453206829348,
0.539607289044027,0.677360939269346,0.7531359649222,0.90944661516137,0.9151363597031,
0.917592281779398,0.919353568118223,0.921167383202567,0.923815197944702,
0.930498814302529,1.05802998502632,1.1640079236285,1.26878048960929,1.28869166797053,
1.29522135334016,1.29936283769931,1.30321780059319,1.30822916199294,1.31916900526404,
1.41650018840158,1.52664256844806,1.65582814407429,1.66257437105731,1.66500177368406,
1.66659914332189,1.66813226846972,1.67019231135599,1.67463451426253,1.72186110719343,
1.72725618031526,1.85890588313987,1.86822966012696,1.87826647274652,2.06808767085959,
2.07493643224757,2.07800103869861,2.08028159700849,2.08240491975219,2.08531250857926,
2.09260349276629,2.17717654891765,2.39425704232891,2.48671387608953,2.4929571512927,
2.49556329862019,2.49740115479434,2.49926630033228,2.50194414333719,2.50847537381707,
2.64116885546442,2.79842118967124,2.90781414322716,2.92603832800423,2.93510416525806,
2.94165874948799,2.94866558159823,2.96077233530204,2.99583534854256,3.04933207070088,
3.18906711428707,3.24256420034153,3.24988582910731,3.2536445606738,3.25638604252864,
3.25974654629061,3.26531076330751,3.28640744456579,3.50096403718671,3.54353952171919,
3.55467284200496,3.56136498471022,3.56737092888208,3.5750233776465,3.58724403358075,
3.67089698022099,3.67229479695662,3.69652306667407,3.73224316255104,3.90006502780105,
3.99828908783521,4.01150396856832,4.01520806888163,4.0174565765314,4.01948041085218,
4.02205670610179,4.02728895523267,4.05904036458754,4.31149141491449,4.40807605909275,
4.41497567782393,4.41797987270617,4.4201832066768,4.42221182842074,4.4249549063649,
4.43165841026875,4.49894569756243,4.73629255702961,4.79177956105173,4.82979520809024,
4.83625982116579,4.83828178316545,4.83955792139589,4.84073921720697,4.842263121934,
4.84554111627787,4.8717099444164,4.97796292638631,5.17124535684743,5.22414262022017,
5.22956778117636,5.23221889861133,5.23411550747943,5.23591615060921,5.23843400958516,
5.24350742287998,5.28456962391348,5.39337520753743,5.62013413645552,5.63289458858313,
5.63522372982776,5.63664390185122,5.63776289188969,5.63899187619111,5.64098328075268,
5.647738916276,5.6896753863514,5.74704872772061,5.79449560458504,5.98324166854546,
6.04997186947067,6.05646035763179,6.05909913621516,6.06104463750869,6.0631518844749,
6.06601465780526,6.07254389980024,6.19222131088364,6.43637942348593,6.44972212081554,
6.45324982083382,6.45529507648987,6.45686966735421,6.45891015731025,6.46251251544456,
6.47847045918395,6.70231210933929,6.74753686779607,6.81828248311108,6.82079214391801,
6.82447663327616,6.83123142445203,6.83560875042149,6.83941382748229,6.84408867267543,
6.85306472269427,6.91199682482521,6.98738355365248,7.17263047638213,7.19669960705479,
7.20063259858052,7.20260991379666,7.20415097122904,7.20585027845178,7.20861959596037,
7.21817817962904,7.28104625864239,7.39422308208374,7.53039313982771,7.60419540394855,
7.61124294065932,7.61410775528786,7.61621950505469,7.61835784101097,7.62131220791434,
7.62457555280662,7.63001528465736,7.74539429994104,7.87017344689481,8.01845555064868,
8.02791098626311,8.03109972669997,8.03289373647992,8.03469665518467,8.03696485644724,
8.04141233842279,8.07262492204533,8.15960006128387,8.21796695152772,8.28532783371875,
8.34142091704411,8.40023665798033,8.43938515023859,8.46039441767353,8.46987493623481,
8.47718428717912,8.48509528725677,8.49777872530006,8.54189264333745,8.66107099817978,
8.76937339949178,8.78263913865442,8.78756893471798,8.79048344157793,8.79354019513237,
8.79753191479276,8.80667652505242,8.81954730929483,8.83966168945805,8.94515289856989,
9.03216271589456,9.0774422303577,9.08917558159987,9.09606649866031,9.10204307168555,
9.10938782529794,9.12359396995231,9.23533418761744,9.34172038092684,9.48797904483556,
9.51998810048555,9.53574774787381,9.54678259175826,9.55038573202943,9.55238917562775,
9.55420350498837,9.55661002644198,9.56103172804729,9.58383993125126,9.62028933910265,
9.75430381301949,9.94182413716274,9.94912265785832,9.95188999567882,9.95197847831517),
 .UNSPECIFIED.);
#3600=B_SPLINE_CURVE_WITH_KNOTS('',3,(#236316,#236317,#236318,#236319,#236320,
#236321,#236322,#236323,#236324,#236325,#236326,#236327,#236328,#236329,
#236330,#236331,#236332,#236333,#236334,#236335,#236336,#236337,#236338,
#236339,#236340,#236341,#236342,#236343,#236344,#236345,#236346,#236347,
#236348,#236349,#236350,#236351,#236352,#236353,#236354,#236355,#236356,
#236357,#236358,#236359,#236360,#236361,#236362,#236363,#236364,#236365,
#236366,#236367,#236368,#236369,#236370,#236371,#236372,#236373,#236374,
#236375,#236376,#236377,#236378,#236379,#236380,#236381,#236382,#236383,
#236384,#236385,#236386,#236387,#236388,#236389,#236390,#236391,#236392,
#236393,#236394,#236395,#236396,#236397,#236398,#236399,#236400,#236401,
#236402,#236403,#236404,#236405,#236406,#236407,#236408,#236409,#236410,
#236411,#236412,#236413,#236414,#236415,#236416,#236417,#236418,#236419,
#236420,#236421,#236422,#236423,#236424,#236425,#236426,#236427,#236428,
#236429,#236430,#236431,#236432,#236433,#236434,#236435,#236436,#236437,
#236438,#236439,#236440,#236441,#236442,#236443,#236444,#236445,#236446,
#236447,#236448,#236449,#236450,#236451,#236452,#236453,#236454,#236455,
#236456,#236457,#236458,#236459,#236460,#236461,#236462,#236463,#236464,
#236465,#236466,#236467,#236468,#236469,#236470,#236471,#236472,#236473,
#236474,#236475,#236476,#236477,#236478,#236479,#236480,#236481,#236482,
#236483,#236484,#236485,#236486,#236487,#236488,#236489,#236490,#236491,
#236492,#236493,#236494,#236495,#236496,#236497,#236498,#236499,#236500,
#236501,#236502,#236503,#236504,#236505,#236506,#236507,#236508,#236509,
#236510,#236511,#236512,#236513,#236514,#236515,#236516,#236517,#236518,
#236519,#236520,#236521,#236522,#236523,#236524,#236525,#236526,#236527,
#236528,#236529,#236530,#236531,#236532,#236533,#236534,#236535,#236536,
#236537,#236538,#236539,#236540,#236541,#236542,#236543,#236544,#236545,
#236546,#236547,#236548,#236549,#236550,#236551,#236552,#236553,#236554,
#236555,#236556,#236557,#236558,#236559,#236560,#236561,#236562,#236563,
#236564,#236565,#236566,#236567,#236568,#236569,#236570,#236571,#236572,
#236573,#236574,#236575,#236576,#236577,#236578,#236579,#236580,#236581,
#236582,#236583,#236584,#236585,#236586,#236587,#236588,#236589,#236590,
#236591,#236592,#236593,#236594,#236595,#236596,#236597,#236598,#236599,
#236600,#236601,#236602,#236603,#236604,#236605,#236606,#236607,#236608,
#236609,#236610,#236611,#236612,#236613,#236614,#236615,#236616,#236617,
#236618,#236619,#236620,#236621,#236622,#236623,#236624,#236625,#236626,
#236627,#236628,#236629,#236630,#236631,#236632,#236633,#236634,#236635,
#236636,#236637,#236638,#236639,#236640,#236641,#236642,#236643,#236644,
#236645,#236646,#236647,#236648,#236649,#236650,#236651,#236652,#236653,
#236654,#236655,#236656,#236657,#236658,#236659,#236660,#236661,#236662,
#236663,#236664,#236665,#236666,#236667,#236668,#236669,#236670,#236671,
#236672,#236673,#236674,#236675,#236676,#236677,#236678,#236679,#236680,
#236681,#236682,#236683,#236684,#236685,#236686,#236687,#236688,#236689,
#236690,#236691,#236692,#236693,#236694,#236695,#236696,#236697,#236698,
#236699,#236700,#236701,#236702,#236703,#236704,#236705,#236706,#236707,
#236708,#236709,#236710,#236711,#236712,#236713,#236714,#236715,#236716,
#236717,#236718,#236719,#236720,#236721,#236722,#236723,#236724,#236725,
#236726,#236727,#236728,#236729,#236730,#236731,#236732,#236733,#236734,
#236735,#236736,#236737,#236738,#236739,#236740,#236741,#236742,#236743,
#236744,#236745,#236746,#236747,#236748,#236749,#236750,#236751,#236752,
#236753,#236754,#236755,#236756,#236757,#236758,#236759,#236760,#236761,
#236762,#236763,#236764,#236765,#236766,#236767,#236768,#236769,#236770,
#236771,#236772,#236773,#236774,#236775,#236776,#236777,#236778,#236779,
#236780,#236781,#236782,#236783,#236784,#236785,#236786,#236787,#236788,
#236789,#236790,#236791,#236792,#236793,#236794,#236795,#236796,#236797,
#236798,#236799,#236800,#236801,#236802,#236803,#236804,#236805,#236806,
#236807,#236808,#236809,#236810,#236811,#236812,#236813,#236814,#236815,
#236816,#236817,#236818,#236819,#236820,#236821,#236822,#236823,#236824,
#236825,#236826,#236827,#236828,#236829,#236830,#236831,#236832,#236833,
#236834,#236835,#236836,#236837,#236838,#236839,#236840,#236841,#236842,
#236843,#236844,#236845,#236846,#236847,#236848,#236849,#236850,#236851),
 .UNSPECIFIED.,.F.,.F.,(4,2,2,2,2,2,2,2,2,2,2,2,2,2,2,2,2,2,2,2,2,2,2,2,
2,2,2,2,2,2,2,2,2,2,2,2,2,2,2,2,2,2,2,2,2,2,2,2,2,2,2,2,2,2,2,2,2,2,2,2,
2,2,2,2,2,2,2,2,2,2,2,2,2,2,2,2,2,2,2,2,2,2,2,2,2,2,2,2,2,2,2,2,2,2,2,2,
2,2,2,2,2,2,2,2,2,2,2,2,2,2,2,2,2,2,2,2,2,2,2,2,2,2,2,2,2,2,2,2,2,2,2,2,
2,2,2,2,2,2,2,2,2,2,2,2,2,2,2,2,2,2,2,2,2,2,2,2,2,2,2,2,2,2,2,2,2,2,2,2,
2,2,2,2,2,2,2,2,2,2,2,2,2,2,2,2,2,2,2,2,2,2,2,2,2,2,2,2,2,2,2,2,2,2,2,2,
2,2,2,2,2,2,2,2,2,2,2,2,2,2,2,2,2,2,2,2,2,2,2,2,2,2,2,2,2,2,2,2,2,2,2,2,
2,2,2,2,2,2,2,2,2,2,2,2,2,2,2,2,2,2,2,2,2,2,2,2,2,2,2,4),(0.00339948482433297,
0.00455387327914176,0.00664996712160906,0.00873724952909339,0.0121709021781368,
0.0214685783812223,0.135307833821441,0.314182684490307,0.353627606970092,
0.419655465577952,0.42338951960139,0.425017653679891,0.426212325674946,
0.427312396922012,0.42879988447454,0.432460253131873,0.475177802971346,
0.714150741962386,0.809465072885502,0.816427375995736,0.819294158830642,
0.8211561069453,0.823158041344754,0.825927199254051,0.832221943478852,0.899169337230051,
0.953950646209046,1.0316465729292,1.06073320793195,1.12383170898784,1.18641361564054,
1.20839122098479,1.21420268843468,1.22055901103832,1.22248176157527,1.22369166755149,
1.22481705384346,1.22627654792165,1.22870111687558,1.24250521349936,1.49320134560417,
1.59815341710021,1.62519463167248,1.63558829475165,1.64067998302065,1.64372058023638,
1.64642918211452,1.64849292367045,1.65044114577943,1.65308949870639,1.65963092718299,
1.72928979630668,1.8748814370295,1.88449478561483,1.90851723324041,1.9368652742486,
1.98371305418456,2.02876788713024,2.03752331401305,2.04043890103097,2.04232663972898,
2.04410843317757,2.04645737595751,2.05044797667661,2.07570506531668,2.31290595027982,
2.39588274065368,2.4131551307623,2.41931173633497,2.42337112885412,2.42721933887109,
2.4323420122959,2.44346155433415,2.56457920699647,2.77132998387571,2.7850154786549,
2.788147280369,2.78992769532024,2.79130459612038,2.79309719544224,2.79619919424374,
2.80820442811209,3.00036542393493,3.10911235752052,3.18387398114573,3.19235306518527,
3.19683164100235,3.19969238903921,3.20235615643741,3.2045515636765,3.20713767022418,
3.2115212344762,3.22734602892659,3.48484718086632,3.54586704482024,3.60503996033402,
3.61549323086494,3.61868094259353,3.62067511073813,3.62250957416612,3.62486118362018,
3.62984762871348,3.66496249138946,3.81066625069469,3.93773126464987,4.03333530711437,
4.05043489394663,4.05927749241149,4.06580499482296,4.07394629437169,4.08767649875489,
4.13730063433213,4.14453138502757,4.33868139139739,4.36812197195588,4.3744218540239,
4.37796260732031,4.38098763802104,4.38463695972295,4.39148420262095,4.43794992964713,
4.47341912094612,4.57773625520793,4.63410204604303,4.65684022046811,4.67410962621323,
4.68205892720294,4.68810342082402,4.69384667174326,4.70192970705974,4.72383430911374,
4.98043653009428,5.07306595565444,5.13145371522956,5.13691219763676,5.13959223446717,
5.14151792584327,5.14355755994882,5.14625151499181,5.15208802552767,5.29876817117258,
5.52255160090704,5.53646301250632,5.54058638021093,5.54302940697211,5.54497419972363,
5.54757358691066,5.55240828907908,5.57850914157836,5.62919703557433,5.73237414372841,
5.77357598384598,5.81877303674438,5.93807333948164,5.95795685134136,5.96108610969121,
5.96260003528448,5.96377654538478,5.96507024593164,5.96716997594589,5.97460594262434,
6.12801696243354,6.19382477862986,6.34258553306811,6.35228112607749,6.35567063568027,
6.35760888796711,6.35939701072369,6.36181743138727,6.36641863258125,6.39373414244521,
6.44924464588058,6.60652997609976,6.74810102696531,6.75699148042267,6.75924234210572,
6.7605352809782,6.7616350542402,6.76297566634959,6.7654715243006,6.77894044147464,
6.80615055495681,6.85895994488177,6.98639084190845,7.09404343482521,7.17308281239266,
7.17986195381161,7.18255119101633,7.18450997547661,7.18660895510604,7.18942096964188,
7.19566923139514,7.33550696751887,7.48979875668508,7.53349611221558,7.57034088976368,
7.57549970457562,7.57765762229547,7.57945218726998,7.58128714669426,7.58390255074102,
7.59053882180874,7.71666253032761,7.87975650779436,7.94217139571655,7.95261903061846,
7.95754280623525,7.96138444121906,7.96556664780587,7.97214482226862,7.99355206650326,
8.02691021788937,8.09098127821539,8.21834836765874,8.31740099175191,8.32305608362912,
8.32515381340454,8.32663465380853,8.32802493142828,8.32994421681633,8.33364882798252,
8.3383076883155,8.34845993152279,8.37930991719329,8.43980061647463,8.50192482997755,
8.58010934834867,8.72405182152072,8.73367410871813,8.73730809197383,8.73946267492432,
8.74150022302738,8.74433665155944,8.75000598526771,8.79384511977416,8.91776982214926,
8.94710239846476,9.02559809895208,9.14452052881674,9.15205892038015,9.15496340560512,
9.15670153875358,9.15835648129549,9.16067888481514,9.16319386113808,9.17573134821778,
9.19747221331567,9.28844273291446,9.37170794198734,9.55559744081383,9.58153997804678,
9.59117084718496,9.59807315161972,9.60540858640614,9.61256505958894,9.62197872987209,
9.63695150711152,9.72650206571606,9.86572588617263,9.88743509752931,9.90541988793216,
9.910985433902,9.91402747613791,9.91702868902569,9.91991051144495,9.92348634666446,
9.92899640776304,9.95507935882116),.UNSPECIFIED.);
#3601=B_SPLINE_CURVE_WITH_KNOTS('',3,(#236853,#236854,#236855,#236856,#236857,
#236858,#236859,#236860,#236861,#236862,#236863,#236864),.UNSPECIFIED.,
 .F.,.F.,(4,1,1,1,1,1,1,1,1,4),(-173.738933713979,-173.281344172089,-172.781974304158,
-171.783234568295,-170.784494832433,-169.785755096571,-169.28638522864,
-168.787015360709,-167.788275624847,-167.4557484068),.UNSPECIFIED.);
#3602=B_SPLINE_CURVE_WITH_KNOTS('',3,(#236866,#236867,#236868,#236869,#236870,
#236871,#236872,#236873,#236874,#236875,#236876,#236877,#236878,#236879,
#236880,#236881,#236882,#236883),.UNSPECIFIED.,.F.,.F.,(4,2,2,2,2,2,2,2,
4),(-167.4557484068,-166.620831494905,-165.78591458301,-164.950997671115,
-164.11608075922,-163.281163847326,-162.446246935431,-161.611330023536,
-161.17256309962),.UNSPECIFIED.);
#3603=B_SPLINE_CURVE_WITH_KNOTS('',3,(#236885,#236886,#236887,#236888,#236889,
#236890,#236891,#236892,#236893,#236894,#236895,#236896,#236897,#236898,
#236899,#236900,#236901,#236902,#236903,#236904,#236905,#236906,#236907,
#236908,#236909,#236910,#236911,#236912,#236913,#236914,#236915,#236916,
#236917,#236918,#236919,#236920,#236921,#236922,#236923,#236924,#236925,
#236926,#236927,#236928,#236929,#236930,#236931,#236932,#236933,#236934,
#236935,#236936,#236937,#236938,#236939,#236940,#236941,#236942,#236943,
#236944,#236945,#236946,#236947,#236948,#236949,#236950,#236951,#236952,
#236953,#236954,#236955,#236956,#236957,#236958,#236959,#236960,#236961,
#236962,#236963,#236964,#236965,#236966,#236967,#236968,#236969,#236970,
#236971,#236972,#236973,#236974,#236975,#236976,#236977,#236978,#236979,
#236980,#236981,#236982,#236983,#236984,#236985,#236986,#236987,#236988,
#236989,#236990,#236991,#236992,#236993,#236994,#236995,#236996,#236997,
#236998,#236999,#237000,#237001,#237002,#237003,#237004,#237005,#237006,
#237007,#237008,#237009,#237010,#237011,#237012,#237013,#237014,#237015,
#237016,#237017,#237018,#237019,#237020,#237021,#237022,#237023,#237024,
#237025,#237026,#237027,#237028,#237029,#237030,#237031,#237032,#237033,
#237034,#237035,#237036,#237037,#237038,#237039,#237040,#237041,#237042,
#237043,#237044,#237045,#237046,#237047,#237048,#237049,#237050,#237051,
#237052,#237053,#237054,#237055,#237056,#237057,#237058,#237059,#237060,
#237061,#237062,#237063,#237064,#237065,#237066,#237067,#237068,#237069,
#237070,#237071,#237072,#237073,#237074,#237075,#237076,#237077,#237078,
#237079,#237080,#237081,#237082,#237083,#237084,#237085,#237086,#237087,
#237088,#237089,#237090,#237091,#237092,#237093,#237094,#237095,#237096,
#237097,#237098,#237099,#237100,#237101,#237102,#237103,#237104,#237105,
#237106,#237107,#237108,#237109,#237110,#237111,#237112,#237113,#237114,
#237115,#237116,#237117,#237118,#237119,#237120,#237121,#237122,#237123,
#237124,#237125,#237126,#237127,#237128,#237129,#237130,#237131,#237132,
#237133,#237134,#237135,#237136,#237137,#237138,#237139,#237140,#237141,
#237142,#237143,#237144,#237145,#237146),.UNSPECIFIED.,.F.,.F.,(4,3,3,3,
3,3,3,3,3,3,3,3,3,3,3,3,3,3,3,3,3,3,3,3,3,3,3,3,3,3,3,3,3,3,3,3,3,3,3,3,
3,3,3,3,3,3,3,3,3,3,3,3,3,3,3,3,3,3,3,3,3,3,3,3,3,3,3,3,3,3,3,3,3,3,3,3,
3,3,3,3,3,3,3,3,3,3,3,4),(-161.17256309962,-161.086963947609,-161.000905088157,
-160.91465001931,-160.828218360044,-160.797097473811,-160.723320382987,
-160.649605605553,-160.575940071267,-160.502309926181,-160.428701302376,
-160.355088484571,-160.29772760588,-160.216294074799,-160.134725079803,
-160.050633244339,-159.968790537844,-159.883574137897,-159.798357737949,
-159.719924794452,-159.641561610572,-159.563263345294,-159.485044079437,
-159.406874787932,-159.328763462845,-159.298987870018,-159.222625398935,
-159.146246072852,-159.069840307211,-158.99336563512,-158.916853587391,
-158.840259258165,-158.799618002087,-158.72424062315,-158.64892478975,-158.57365768014,
-158.498426505057,-158.423218499912,-158.345425970701,-158.270207794519,
-158.194972918941,-158.119709775396,-158.044406782052,-157.969014586096,
-157.893569686747,-157.818026325647,-157.800878266225,-157.727734457249,
-157.654679444135,-157.58169828974,-157.508776127093,-157.435898143796,
-157.363049567974,-157.290202166957,-157.217351820808,-157.14448518075,
-157.071588887325,-156.998606747341,-156.925577846609,-156.852438293037,
-156.802138530363,-156.727549911139,-156.653046940759,-156.578615682998,
-156.50424224912,-156.429912788706,-156.355613480951,-156.2813201198,-156.207026570731,
-156.132720340123,-156.058388929992,-155.983984887122,-155.909539234808,
-155.835002676717,-155.803398794501,-155.722404815116,-155.641527777048,
-155.557153064428,-155.476594670498,-155.396160128518,-155.315900710935,
-155.304028926569,-155.231802226745,-155.159571043702,-155.08729105622,
-155.014985614552,-154.942600493689,-154.889377792441),.UNSPECIFIED.);
#3604=B_SPLINE_CURVE_WITH_KNOTS('',3,(#237148,#237149,#237150,#237151,#237152,
#237153,#237154,#237155,#237156,#237157,#237158,#237159,#237160,#237161),
 .UNSPECIFIED.,.F.,.F.,(4,2,1,1,1,1,1,1,1,1,4),(-154.889377792441,-154.804659058638,
-153.805919322776,-153.306549454845,-152.807179586914,-152.307809718983,
-151.808439851052,-150.80970011519,-149.810960379327,-148.812220643465,
-148.606192485261),.UNSPECIFIED.);
#3605=B_SPLINE_CURVE_WITH_KNOTS('',3,(#237163,#237164,#237165,#237166,#237167,
#237168,#237169,#237170,#237171,#237172,#237173,#237174,#237175),
 .UNSPECIFIED.,.F.,.F.,(4,1,1,1,1,1,1,1,1,1,4),(-148.606192485261,-148.312850775534,
-147.813480907603,-146.814741171741,-146.31537130381,-145.816001435879,
-145.316631567948,-144.817261700017,-143.818521964154,-142.819782228292,
-142.323011474765),.UNSPECIFIED.);
#3606=B_SPLINE_CURVE_WITH_KNOTS('',3,(#237177,#237178,#237179,#237180,#237181,
#237182,#237183,#237184,#237185,#237186,#237187,#237188,#237189,#237190,
#237191,#237192,#237193,#237194,#237195,#237196,#237197,#237198,#237199,
#237200,#237201,#237202,#237203,#237204,#237205,#237206,#237207,#237208,
#237209,#237210,#237211,#237212,#237213,#237214,#237215,#237216,#237217,
#237218,#237219,#237220,#237221,#237222,#237223,#237224,#237225,#237226,
#237227,#237228,#237229,#237230,#237231,#237232,#237233,#237234,#237235,
#237236,#237237,#237238,#237239,#237240,#237241,#237242,#237243,#237244,
#237245,#237246,#237247,#237248,#237249,#237250,#237251,#237252,#237253,
#237254,#237255,#237256,#237257,#237258,#237259,#237260,#237261,#237262,
#237263,#237264,#237265,#237266,#237267,#237268,#237269,#237270,#237271,
#237272,#237273,#237274,#237275,#237276,#237277,#237278,#237279,#237280,
#237281,#237282,#237283,#237284,#237285,#237286,#237287,#237288,#237289,
#237290,#237291,#237292,#237293,#237294,#237295,#237296,#237297,#237298,
#237299,#237300,#237301,#237302,#237303,#237304,#237305,#237306,#237307,
#237308,#237309,#237310,#237311,#237312,#237313,#237314,#237315,#237316,
#237317,#237318,#237319,#237320,#237321,#237322,#237323,#237324,#237325,
#237326,#237327,#237328,#237329,#237330,#237331,#237332,#237333,#237334,
#237335,#237336,#237337,#237338,#237339,#237340,#237341,#237342,#237343,
#237344,#237345,#237346,#237347,#237348,#237349,#237350,#237351,#237352,
#237353,#237354,#237355,#237356,#237357,#237358,#237359,#237360,#237361,
#237362,#237363,#237364,#237365,#237366,#237367,#237368,#237369,#237370,
#237371,#237372,#237373,#237374,#237375,#237376,#237377,#237378,#237379,
#237380,#237381,#237382,#237383,#237384,#237385,#237386,#237387,#237388,
#237389,#237390,#237391,#237392,#237393,#237394,#237395,#237396,#237397,
#237398,#237399,#237400,#237401,#237402,#237403,#237404,#237405,#237406,
#237407,#237408,#237409,#237410,#237411,#237412,#237413,#237414,#237415,
#237416,#237417,#237418,#237419,#237420,#237421,#237422,#237423,#237424,
#237425,#237426,#237427,#237428,#237429,#237430,#237431,#237432,#237433,
#237434,#237435,#237436,#237437,#237438,#237439,#237440,#237441,#237442,
#237443,#237444,#237445,#237446,#237447,#237448,#237449,#237450,#237451,
#237452,#237453,#237454,#237455,#237456,#237457,#237458,#237459,#237460,
#237461,#237462,#237463,#237464,#237465,#237466,#237467,#237468,#237469,
#237470,#237471,#237472,#237473,#237474,#237475,#237476,#237477,#237478,
#237479,#237480,#237481,#237482,#237483,#237484,#237485,#237486,#237487,
#237488,#237489,#237490,#237491,#237492,#237493,#237494,#237495,#237496,
#237497,#237498,#237499,#237500,#237501,#237502,#237503,#237504,#237505,
#237506,#237507,#237508,#237509,#237510,#237511,#237512,#237513,#237514,
#237515,#237516,#237517,#237518,#237519,#237520,#237521,#237522,#237523,
#237524,#237525,#237526,#237527,#237528,#237529,#237530,#237531,#237532,
#237533,#237534,#237535,#237536,#237537,#237538,#237539,#237540,#237541,
#237542,#237543,#237544,#237545,#237546,#237547,#237548,#237549,#237550,
#237551,#237552,#237553,#237554,#237555,#237556,#237557,#237558,#237559,
#237560,#237561,#237562,#237563,#237564,#237565,#237566,#237567,#237568,
#237569,#237570,#237571,#237572,#237573,#237574,#237575,#237576,#237577,
#237578,#237579,#237580,#237581,#237582,#237583,#237584,#237585,#237586,
#237587,#237588,#237589,#237590,#237591,#237592,#237593,#237594,#237595,
#237596,#237597,#237598,#237599,#237600,#237601,#237602,#237603,#237604,
#237605,#237606,#237607,#237608,#237609,#237610,#237611,#237612,#237613,
#237614,#237615,#237616,#237617,#237618,#237619,#237620,#237621,#237622,
#237623,#237624,#237625,#237626,#237627,#237628,#237629,#237630,#237631,
#237632,#237633,#237634,#237635,#237636,#237637,#237638,#237639,#237640,
#237641,#237642,#237643,#237644,#237645,#237646,#237647,#237648,#237649,
#237650,#237651,#237652,#237653,#237654,#237655,#237656,#237657,#237658,
#237659,#237660,#237661,#237662,#237663,#237664,#237665,#237666,#237667,
#237668,#237669,#237670,#237671,#237672,#237673,#237674,#237675,#237676,
#237677,#237678,#237679,#237680,#237681,#237682,#237683,#237684,#237685,
#237686,#237687,#237688,#237689,#237690,#237691,#237692,#237693,#237694,
#237695,#237696,#237697,#237698,#237699,#237700,#237701,#237702,#237703,
#237704),.UNSPECIFIED.,.F.,.F.,(4,2,2,2,2,2,2,2,2,2,2,2,2,2,2,2,2,2,2,2,
2,2,2,2,2,2,2,2,2,2,2,2,2,2,2,2,2,2,2,2,2,2,2,2,2,2,2,2,2,2,2,2,2,2,2,2,
2,2,2,2,2,2,2,2,2,2,2,2,2,2,2,2,2,2,2,2,2,2,2,2,2,2,2,2,2,2,2,2,2,2,2,2,
2,2,2,2,2,2,2,2,2,2,2,2,2,2,2,2,2,2,2,2,2,2,2,2,2,2,2,2,2,2,2,2,2,2,2,2,
2,2,2,2,2,2,2,2,2,2,2,2,2,2,2,2,2,2,2,2,2,2,2,2,2,2,2,2,2,2,2,2,2,2,2,2,
2,2,2,2,2,2,2,2,2,2,2,2,2,2,2,2,2,2,2,2,2,2,2,2,2,2,2,2,2,2,2,2,2,2,2,2,
2,2,2,2,2,2,2,2,2,2,2,2,2,2,2,2,2,2,2,2,2,2,2,2,2,2,2,2,2,2,2,2,2,2,2,2,
2,2,2,2,2,2,2,2,2,2,2,2,2,2,2,2,2,2,2,2,2,2,2,2,2,2,2,4),(0.0021989709022817,
0.0174738004725367,0.0266728755051898,0.0299382247501041,0.0322134910204027,
0.0341521217674839,0.0360942225102894,0.0386454182923098,0.0425298197095983,
0.0593724824131793,0.0713825199188557,0.347097866130202,0.368030873495306,
0.415799838349878,0.4248840106627,0.427842081983253,0.429739993881052,0.431519050973966,
0.433846547561474,0.437761180144164,0.461486819034567,0.664991788550958,
0.778735926505257,0.799669477603781,0.806335194698198,0.810508145377708,
0.81435498729063,0.819232439769835,0.828320947708939,0.885068479635379,
1.0805050027113,1.13853363449481,1.17135912758122,1.17531027967798,1.17726509952547,
1.17866054829179,1.18012818425219,1.18217562692914,1.18751470151173,1.27391376687694,
1.48849605253348,1.54189020753851,1.56832628035386,1.57873831866527,1.58394503756975,
1.58711228818103,1.58999789805207,1.59221915989653,1.59437129957261,1.59798919177949,
1.60750353409201,1.76031121766192,1.80896726801298,1.82385355094814,1.84502469574128,
1.868941032755,1.94823196004474,1.97737628860025,2.00160931358989,2.0057809029104,
2.00799278732535,2.00963505208825,2.01142336245892,2.0145720214624,2.02374636291436,
2.06763821673483,2.16449978428803,2.31389660910018,2.42013999978783,2.43812779283363,
2.44715128100224,2.45370419203812,2.46073650583,2.47295762087248,2.50882860657318,
2.62186693306429,2.73434336006735,2.75731589412689,2.76314506974697,2.76658354771801,
2.76930668750305,2.77295163022944,2.7797670796623,2.82513029934676,2.97263428312689,
3.02492738605399,3.05759168321795,3.06776254529853,3.07424598824688,3.0803185391646,
3.08829070033247,3.10618911176577,3.23578322706014,3.26269325353364,3.42237870678029,
3.49281121943322,3.52214049901602,3.52687410283799,3.52934873690492,3.53136451293,
3.5336823032336,3.53758955315858,3.55149730201945,3.78888827893873,3.90640055085566,
3.92492608801512,3.92928222306655,3.93177816618775,3.93371808020571,3.93625659422768,
3.94068369022375,3.95797752250563,4.22572829481897,4.28997352849309,4.34160438303979,
4.34941165000115,4.3515796492766,4.35288939424111,4.35406372663174,4.35555187563319,
4.35788993530852,4.36999889449647,4.62186277568004,4.73789099874759,4.74416639418397,
4.74691487771793,4.74893678386463,4.75080264529649,4.75333208479401,4.75954490870874,
4.82311051877275,4.90635095761544,4.98335325688672,5.13758966274805,5.14745750765565,
5.14958862503011,5.15096544073365,5.15207830464268,5.15334886035637,5.15552310436134,
5.16417522289751,5.22935264471346,5.38943195538701,5.49567112458791,5.56437151347006,
5.57091331971715,5.57356262390711,5.57551184801385,5.57761924885999,5.58047536034238,
5.58695991826877,5.70701839025305,5.78223496458913,5.85756767548642,5.95843458726013,
5.96562440013223,5.96841324242663,5.97008746599995,5.97168493076239,5.97393193038925,
5.9785086244463,6.01875108526842,6.09571659667715,6.22558332806175,6.33099790155063,
6.3417463338379,6.34692924796671,6.35059940071529,6.35444236212084,6.35945076597468,
6.37008032567029,6.38381590989211,6.50305248595167,6.61033121327096,6.68899932446522,
6.6911439401827,6.69846682299931,6.70786823658444,6.71406355422338,6.71643746471502,
6.71803706399938,6.71956934880039,6.72167313368793,6.72640120639067,6.83881363264207,
7.04473471356267,7.11920234201839,7.12627043538521,7.12914008036274,7.13125411132866,
7.13354234508795,7.13664841839845,7.14372219769389,7.26609364661515,7.44406763241697,
7.5384124957183,7.54450139382672,7.54710177529751,7.54895192314209,7.55080436873359,
7.55348766333007,7.56019521650181,7.67766519208207,7.75680515859896,7.94751727124192,
7.97358688586004,7.98323481317064,7.99014324066107,7.99747961903742,8.00726669782614,
8.02924906752106,8.04568397594722,8.09814082665305,8.25654388848295,8.29478093100519,
8.30119871952584,8.30511084035366,8.30817615833971,8.31148049848513,8.31676268781673,
8.33786466406911,8.54600766504765,8.54929210693049,8.59426347079943,8.60597363108527,
8.61286233817759,8.61884395812064,8.62620380444695,8.64046760361987,8.75340891515095,
8.92470453324758,9.03948258503262,9.04930177842657,9.05439046548154,9.06428347330626,
9.06766430407698,9.06982713677481,9.0717737907459,9.07436189944925,9.07965057076832,
9.13153347095929,9.161839032087,9.45082576697285,9.46514098011268,9.4693102371038,
9.47176348756786,9.47390240231286,9.47657653534121,9.48176433342541,9.51577736270638,
9.61169624415625,9.82139515579529,9.82891527249432,9.8444090272567,9.87642326666226,
9.88782640812077,9.8901731141985,9.89166265333087,9.89283630844183,9.89393097241329,
9.89520994627623,9.89703664572866,9.90018424157577,9.95940165500043),
 .UNSPECIFIED.);
#3607=B_SPLINE_CURVE_WITH_KNOTS('',3,(#237706,#237707,#237708,#237709,#237710,
#237711,#237712,#237713,#237714,#237715,#237716,#237717,#237718,#237719,
#237720,#237721,#237722,#237723,#237724,#237725,#237726,#237727,#237728,
#237729,#237730,#237731,#237732,#237733,#237734,#237735,#237736,#237737,
#237738,#237739,#237740,#237741,#237742,#237743,#237744,#237745,#237746,
#237747,#237748,#237749,#237750,#237751,#237752,#237753,#237754,#237755,
#237756,#237757,#237758,#237759,#237760,#237761,#237762,#237763,#237764,
#237765,#237766,#237767,#237768,#237769,#237770,#237771,#237772,#237773,
#237774,#237775,#237776,#237777,#237778,#237779,#237780,#237781,#237782,
#237783,#237784,#237785,#237786,#237787,#237788,#237789,#237790,#237791,
#237792,#237793,#237794,#237795,#237796,#237797,#237798,#237799,#237800,
#237801,#237802,#237803,#237804,#237805,#237806,#237807,#237808,#237809,
#237810,#237811,#237812,#237813,#237814,#237815,#237816,#237817,#237818,
#237819,#237820,#237821,#237822,#237823,#237824,#237825,#237826,#237827,
#237828,#237829,#237830,#237831,#237832,#237833,#237834,#237835,#237836,
#237837,#237838,#237839,#237840,#237841,#237842,#237843,#237844,#237845,
#237846,#237847,#237848,#237849,#237850,#237851,#237852,#237853,#237854,
#237855,#237856,#237857,#237858,#237859,#237860,#237861,#237862,#237863,
#237864,#237865,#237866,#237867,#237868,#237869,#237870,#237871,#237872,
#237873,#237874,#237875,#237876,#237877,#237878,#237879,#237880,#237881,
#237882,#237883,#237884,#237885,#237886,#237887,#237888,#237889,#237890,
#237891,#237892,#237893,#237894,#237895,#237896,#237897,#237898,#237899,
#237900,#237901,#237902,#237903,#237904,#237905,#237906,#237907,#237908,
#237909,#237910,#237911,#237912,#237913,#237914,#237915,#237916,#237917,
#237918,#237919,#237920,#237921,#237922,#237923,#237924,#237925,#237926,
#237927,#237928,#237929,#237930,#237931,#237932,#237933,#237934,#237935,
#237936,#237937,#237938,#237939,#237940,#237941,#237942,#237943,#237944,
#237945,#237946,#237947,#237948,#237949,#237950,#237951,#237952,#237953,
#237954,#237955,#237956,#237957,#237958,#237959,#237960,#237961,#237962,
#237963,#237964,#237965,#237966,#237967,#237968,#237969,#237970,#237971,
#237972,#237973,#237974,#237975,#237976,#237977,#237978,#237979,#237980,
#237981,#237982,#237983,#237984,#237985,#237986,#237987,#237988,#237989,
#237990,#237991,#237992,#237993,#237994,#237995,#237996,#237997,#237998,
#237999,#238000,#238001,#238002,#238003,#238004,#238005,#238006,#238007,
#238008,#238009,#238010,#238011,#238012,#238013,#238014,#238015,#238016,
#238017,#238018,#238019,#238020,#238021,#238022,#238023,#238024,#238025,
#238026,#238027,#238028,#238029,#238030,#238031,#238032,#238033,#238034,
#238035,#238036,#238037,#238038,#238039,#238040,#238041,#238042,#238043,
#238044,#238045,#238046,#238047,#238048,#238049,#238050,#238051,#238052,
#238053,#238054,#238055,#238056,#238057,#238058,#238059,#238060,#238061,
#238062,#238063,#238064,#238065,#238066,#238067,#238068,#238069,#238070,
#238071,#238072,#238073,#238074,#238075,#238076,#238077,#238078,#238079,
#238080,#238081,#238082,#238083,#238084,#238085,#238086,#238087,#238088,
#238089,#238090,#238091,#238092,#238093,#238094,#238095,#238096,#238097,
#238098,#238099,#238100,#238101,#238102,#238103,#238104,#238105,#238106,
#238107,#238108,#238109,#238110,#238111,#238112,#238113,#238114,#238115,
#238116,#238117,#238118,#238119,#238120,#238121,#238122,#238123,#238124,
#238125,#238126,#238127,#238128,#238129,#238130,#238131,#238132,#238133,
#238134,#238135,#238136,#238137,#238138,#238139,#238140,#238141,#238142,
#238143,#238144,#238145,#238146,#238147,#238148,#238149,#238150,#238151,
#238152,#238153,#238154,#238155,#238156,#238157,#238158,#238159,#238160,
#238161,#238162,#238163,#238164,#238165,#238166,#238167,#238168,#238169,
#238170,#238171,#238172,#238173,#238174,#238175,#238176,#238177,#238178,
#238179,#238180,#238181,#238182,#238183,#238184,#238185,#238186,#238187,
#238188,#238189,#238190,#238191,#238192,#238193,#238194,#238195,#238196,
#238197,#238198,#238199,#238200,#238201,#238202,#238203,#238204,#238205,
#238206,#238207,#238208,#238209,#238210,#238211,#238212,#238213,#238214,
#238215,#238216,#238217,#238218,#238219,#238220,#238221,#238222,#238223,
#238224,#238225,#238226,#238227),.UNSPECIFIED.,.F.,.F.,(4,2,2,2,2,2,2,2,
2,2,2,2,2,2,2,2,2,2,2,2,2,2,2,2,2,2,2,2,2,2,2,2,2,2,2,2,2,2,2,2,2,2,2,2,
2,2,2,2,2,2,2,2,2,2,2,2,2,2,2,2,2,2,2,2,2,2,2,2,2,2,2,2,2,2,2,2,2,2,2,2,
2,2,2,2,2,2,2,2,2,2,2,2,2,2,2,2,2,2,2,2,2,2,2,2,2,2,2,2,2,2,2,2,2,2,2,2,
2,2,2,2,2,2,2,2,2,2,2,2,2,2,2,2,2,2,2,2,2,2,2,2,2,2,2,2,2,2,2,2,2,2,2,2,
2,2,2,2,2,2,2,2,2,2,2,2,2,2,2,2,2,2,2,2,2,2,2,2,2,2,2,2,2,2,2,2,2,2,2,2,
2,2,2,2,2,2,2,2,2,2,2,2,2,2,2,2,2,2,2,2,2,2,2,2,2,2,2,2,2,2,2,2,2,2,2,2,
2,2,2,2,2,2,2,2,2,2,2,2,2,2,2,2,2,2,2,2,2,2,2,2,2,2,2,2,2,2,2,2,2,2,2,2,
4),(0.00299195565914869,0.204304804266415,0.320244810562324,0.326542787206419,
0.329294687620281,0.331316600490947,0.333180703415817,0.335705074651995,
0.34189213052287,0.404553223481172,0.411592970530418,0.636928067218467,
0.674866396373037,0.728274714773573,0.731687948662123,0.732873622492273,
0.733912975580605,0.735038047081858,0.736494562585654,0.739635667112466,
0.762236700674419,0.806638273444298,0.869735799451805,0.91887819108263,
1.02262490578281,1.11641133873917,1.14926879989619,1.15424935112239,1.15681302471986,
1.15886177128647,1.16090992805181,1.16457281483211,1.17559656731536,1.34926890633361,
1.46912408925914,1.49973481648366,1.53975517059341,1.54788366995576,1.55071756100016,
1.55235466775212,1.55408252452801,1.55628243085285,1.56061205819994,1.58560172998946,
1.66252762168121,1.79568348466412,1.90226210779061,1.92238455881232,1.92894392654275,
1.93309306340189,1.93694741598128,1.94194703248927,1.95281741083261,2.04698630083693,
2.21071082270353,2.28518518395986,2.29562800539406,2.29848758286372,2.2999467967776,
2.30136522088102,2.30309272570482,2.30601238542521,2.31635510723129,2.47928496179845,
2.62718255999014,2.69509861694944,2.70716634289075,2.71100439381433,2.71344376059045,
2.71571406445084,2.71866068503036,2.72355965343022,2.75169282693605,3.04145885928254,
3.07215039366537,3.11771733149536,3.12663957863907,3.12964350296555,3.13156610184395,
3.13337316435036,3.13574480587359,3.14066074606192,3.17648501260328,3.18151930501821,
3.18343929898297,3.18942585848539,3.31437803155712,3.44601130397284,3.54401305514848,
3.56132449412585,3.57021313896487,3.57674923932828,3.58486885880461,3.59848440236222,
3.64683823566358,3.74302040705679,3.8539846184391,3.87964297138532,3.88568451176497,
3.88916977206863,3.8922000838631,3.89592219022888,3.90339785463276,3.97654938184403,
4.08913883278223,4.14540363197154,4.16811808311313,4.18537536277887,4.1933253522458,
4.19937296409566,4.20512111748317,4.21484449495481,4.24159794094126,4.45351757539433,
4.55123789040861,4.61707546128271,4.6449395881812,4.64961039396671,4.65207151252482,
4.65389151514154,4.65615187015555,4.65990548931065,4.6720731238729,4.93219920390064,
4.9822409057344,5.04390151203434,5.049909093815,5.05282270517774,5.0548972157326,
5.05685876769572,5.05958892498399,5.06504405211841,5.10708895782481,5.17148858104234,
5.38383565645856,5.46715989685606,5.47224009107114,5.47414590115759,5.47527209333453,
5.47633441526766,5.47780871336862,5.48074296883495,5.50618455166452,5.58375004322157,
5.76076495864503,5.8586879061462,5.86559558604784,5.86824256080507,5.87013907252819,
5.87214230079071,5.87477704441215,5.88043824110462,5.95700090597055,6.01606562736595,
6.16564617843788,6.20207302889519,6.26669839135053,6.2707014702226,6.272195380661,
6.27326040581108,6.27427264350614,6.27568974477782,6.27855000631779,6.30173179414512,
6.38026173374556,6.5231089037454,6.66045998095707,6.68852872213931,6.69316443745879,
6.69591560048796,6.69801338715346,6.70024605382043,6.70371473257594,6.7142784953503,
6.77214132597164,6.82731308083084,6.99953481505245,7.03955011865145,7.08358112310091,
7.08861547926961,7.09092686011959,7.09270333393783,7.09460772762128,7.09753502127016,
7.10629747161386,7.15748911108523,7.21600591603339,7.3424301977461,7.36685990934665,
7.37535349354944,7.45410193372041,7.46525987960156,7.47032297712433,7.4741878668301,
7.47831184533427,7.48462591674326,7.50378758916066,7.60845244672014,7.75106830074242,
7.83131352684389,7.83650839589159,7.83853242610142,7.83999396334239,7.84154835255648,
7.84361147349523,7.8478751366821,7.88960619378119,7.93361538749365,8.03018348146863,
8.16687972144069,8.16897151929548,8.17729834377345,8.24152544979838,8.24777404933818,
8.25080347503001,8.25295989749751,8.25499844048672,8.25783506763205,8.26350047360152,
8.3071104767254,8.42184149937684,8.53106033194356,8.58667991039619,8.66114829700223,
8.66668485039674,8.66895620704304,8.67065650039618,8.67252363375266,8.67510603784243,
8.68093741241986,8.76275052773776,8.9334985521694,8.99432166999402,9.08041593852909,
9.09935036586209,9.10855623680853,9.1158165916179,9.12257464338248,9.1305186875639,
9.15441069112099,9.18778239639276,9.28245288027419,9.38920598611402,9.41767991291176,
9.42359865913288,9.42740270733699,9.43026453163843,9.43308749145909,9.43802689747503,
9.45453695458353,9.48325429475277,9.55419608272797,9.69982830507318,9.72174693294451,
9.72986082076731,9.73561480151826,9.74165822659727,9.74757750191515,9.75531173530273,
9.76760694038484,9.96019807358396),.UNSPECIFIED.);
#3608=B_SPLINE_CURVE_WITH_KNOTS('',3,(#238229,#238230,#238231,#238232,#238233,
#238234,#238235,#238236,#238237,#238238,#238239,#238240),.UNSPECIFIED.,
 .F.,.F.,(4,1,1,1,1,1,1,1,1,4),(-117.190265949363,-116.852549095875,-115.853809360013,
-114.855069624151,-113.856329888289,-113.356960020358,-112.857590152427,
-111.858850416564,-111.359480548633,-110.907173562223),.UNSPECIFIED.);
#3609=B_SPLINE_CURVE_WITH_KNOTS('',3,(#238242,#238243,#238244,#238245,#238246,
#238247,#238248,#238249,#238250,#238251,#238252,#238253,#238254,#238255,
#238256,#238257,#238258,#238259,#238260,#238261,#238262,#238263,#238264,
#238265,#238266,#238267,#238268,#238269,#238270,#238271,#238272,#238273,
#238274,#238275,#238276,#238277,#238278,#238279,#238280,#238281,#238282,
#238283,#238284,#238285,#238286,#238287,#238288,#238289,#238290,#238291,
#238292,#238293,#238294,#238295,#238296,#238297,#238298,#238299,#238300,
#238301,#238302,#238303,#238304,#238305,#238306,#238307,#238308,#238309,
#238310,#238311,#238312,#238313,#238314,#238315,#238316,#238317,#238318,
#238319,#238320,#238321,#238322,#238323,#238324,#238325,#238326,#238327,
#238328,#238329,#238330,#238331,#238332,#238333,#238334,#238335,#238336,
#238337,#238338,#238339,#238340,#238341,#238342,#238343,#238344,#238345,
#238346,#238347,#238348,#238349,#238350,#238351,#238352,#238353,#238354,
#238355,#238356,#238357,#238358,#238359,#238360,#238361,#238362,#238363,
#238364,#238365,#238366,#238367,#238368,#238369,#238370,#238371,#238372,
#238373,#238374,#238375,#238376,#238377,#238378,#238379,#238380,#238381,
#238382,#238383,#238384,#238385,#238386,#238387,#238388,#238389,#238390,
#238391,#238392,#238393,#238394,#238395,#238396,#238397,#238398,#238399,
#238400,#238401,#238402,#238403,#238404,#238405,#238406,#238407,#238408,
#238409,#238410,#238411,#238412,#238413,#238414,#238415,#238416,#238417,
#238418,#238419,#238420,#238421,#238422,#238423,#238424,#238425,#238426,
#238427,#238428,#238429,#238430,#238431,#238432,#238433,#238434,#238435,
#238436,#238437,#238438,#238439,#238440,#238441,#238442,#238443,#238444,
#238445,#238446,#238447,#238448,#238449,#238450,#238451,#238452,#238453,
#238454,#238455,#238456,#238457,#238458,#238459,#238460,#238461,#238462,
#238463,#238464,#238465,#238466,#238467,#238468,#238469,#238470,#238471,
#238472,#238473,#238474,#238475,#238476,#238477,#238478,#238479,#238480,
#238481,#238482,#238483,#238484,#238485,#238486,#238487,#238488,#238489,
#238490,#238491,#238492,#238493,#238494,#238495,#238496,#238497,#238498,
#238499,#238500,#238501,#238502,#238503,#238504,#238505,#238506,#238507,
#238508,#238509,#238510,#238511,#238512,#238513,#238514,#238515,#238516,
#238517,#238518,#238519,#238520,#238521,#238522,#238523,#238524,#238525,
#238526,#238527,#238528,#238529,#238530,#238531,#238532,#238533,#238534,
#238535,#238536,#238537,#238538,#238539,#238540,#238541,#238542,#238543,
#238544,#238545,#238546,#238547,#238548,#238549,#238550,#238551,#238552,
#238553,#238554,#238555,#238556,#238557,#238558,#238559,#238560,#238561,
#238562,#238563,#238564,#238565,#238566,#238567,#238568,#238569,#238570,
#238571,#238572,#238573,#238574,#238575,#238576,#238577,#238578,#238579,
#238580,#238581,#238582,#238583,#238584,#238585,#238586,#238587,#238588,
#238589,#238590,#238591,#238592,#238593,#238594,#238595,#238596,#238597,
#238598,#238599,#238600,#238601,#238602,#238603,#238604,#238605,#238606,
#238607,#238608,#238609,#238610,#238611,#238612,#238613,#238614,#238615,
#238616,#238617,#238618,#238619,#238620,#238621,#238622,#238623,#238624,
#238625,#238626,#238627,#238628,#238629,#238630,#238631,#238632,#238633,
#238634,#238635,#238636,#238637,#238638,#238639,#238640,#238641,#238642,
#238643,#238644,#238645,#238646,#238647,#238648,#238649,#238650,#238651,
#238652,#238653,#238654,#238655,#238656,#238657,#238658,#238659,#238660,
#238661,#238662,#238663,#238664,#238665,#238666,#238667,#238668,#238669,
#238670,#238671,#238672,#238673,#238674,#238675,#238676,#238677,#238678,
#238679,#238680,#238681,#238682,#238683,#238684,#238685,#238686,#238687,
#238688,#238689,#238690,#238691,#238692,#238693,#238694,#238695,#238696,
#238697,#238698,#238699,#238700,#238701,#238702,#238703,#238704,#238705,
#238706,#238707,#238708,#238709,#238710,#238711,#238712,#238713,#238714,
#238715,#238716,#238717,#238718,#238719,#238720,#238721,#238722,#238723,
#238724,#238725,#238726,#238727,#238728,#238729,#238730,#238731,#238732,
#238733,#238734,#238735,#238736,#238737,#238738,#238739,#238740,#238741,
#238742,#238743,#238744,#238745,#238746,#238747,#238748,#238749,#238750,
#238751,#238752,#238753,#238754,#238755,#238756,#238757,#238758,#238759,
#238760,#238761,#238762,#238763,#238764,#238765,#238766,#238767,#238768,
#238769,#238770,#238771,#238772,#238773),.UNSPECIFIED.,.F.,.F.,(4,2,2,2,
2,2,2,2,2,2,2,2,2,2,2,2,2,2,2,2,2,2,2,2,2,2,2,2,2,2,2,2,2,2,2,2,2,2,2,2,
2,2,2,2,2,2,2,2,2,2,2,2,2,2,2,2,2,2,2,2,2,2,2,2,2,2,2,2,2,2,2,2,2,2,2,2,
2,2,2,2,2,2,2,2,2,2,2,2,2,2,2,2,2,2,2,2,2,2,2,2,2,2,2,2,2,2,2,2,2,2,2,2,
2,2,2,2,2,2,2,2,2,2,2,2,2,2,2,2,2,2,2,2,2,2,2,2,2,2,2,2,2,2,2,2,2,2,2,2,
2,2,2,2,2,2,2,2,2,2,2,2,2,2,2,2,2,2,2,2,2,2,2,2,2,2,2,2,2,2,2,2,2,2,2,2,
2,2,2,2,2,2,2,2,2,2,2,2,2,2,2,2,2,2,2,2,2,2,2,2,2,2,2,2,2,2,2,2,2,2,2,2,
2,2,2,2,2,2,2,2,2,2,2,2,2,2,2,2,2,2,2,2,2,2,2,2,2,2,2,2,2,2,2,2,2,2,2,2,
2,2,2,2,2,2,2,2,2,4),(0.00169228455310972,0.0208076269905666,0.0253450676512967,
0.028578787775409,0.0314337004501233,0.0344443448113954,0.038454885536899,
0.0472928164606967,0.0676712750305325,0.222564681765073,0.313584499892351,
0.323952755739825,0.330905989705942,0.337640572908688,0.343642230693239,
0.351231648228265,0.3632360314278,0.442557054241769,0.455688197628108,0.586744997765805,
0.690920919657209,0.758036552953802,0.776820279838839,0.788331717801715,
0.790967179565189,0.793431903208939,0.795252200090675,0.797225314918757,
0.800077186140425,0.808129421379954,0.920323387521312,1.00928009993188,
1.03197721228674,1.07611124159112,1.15343357722061,1.18712921290333,1.19230671378435,
1.19497966880917,1.19693349108771,1.19903142785402,1.20264945607814,1.21268970641155,
1.35854381573034,1.43676116437018,1.55776425527931,1.59433205669564,1.61139695277517,
1.61415929065484,1.61559878379946,1.61676842347332,1.61810957967311,1.62036069398205,
1.62865214230122,1.76175622680944,1.87950054449306,1.93305524260216,1.97954626927877,
2.00334533803057,2.00777689856845,2.01016203636926,2.01212151155541,2.01412670253363,
2.01784484117802,2.03003463628287,2.20610779653977,2.31332088712653,2.4083246153947,
2.41183163265305,2.41335669410116,2.41448827944028,2.41554171415283,2.41698384425655,
2.41984225800678,2.44327430915916,2.56101213228956,2.71742644390102,2.82484555380525,
2.83310698266921,2.83625776692704,2.83842203236919,2.84053709857879,2.84307946885111,
2.84939172199921,2.90553149848208,2.94267724921543,2.9474590867901,3.01941150883196,
3.14739623827848,3.20002360362122,3.2167685300442,3.22383622191268,3.22917713514963,
3.23156450679453,3.23335512552312,3.23500704905952,3.23724595120155,3.2416207474191,
3.27612070593001,3.41987860763695,3.52016687370595,3.58886499066643,3.60427151014516,
3.61014193184447,3.61414277597609,3.61803429467319,3.62269433790107,3.63423239363179,
3.78394630907534,3.90780218299441,3.95387866748268,3.97487437816231,3.97842863793518,
3.98030141090392,3.98183396814278,3.98360363767069,3.98660389098188,3.99749576972629,
4.23922173720676,4.34334398942954,4.38479330531526,4.39039362823808,4.39321661640452,
4.39525288334908,4.3974138877732,4.40046121041333,4.40859415404207,4.53508409308175,
4.7280846798277,4.78147015467643,4.80481267547004,4.80894458182232,4.81114795898351,
4.81296503373147,4.81480403383221,4.81820463144641,4.82933357975924,4.83068598413479,
4.93244088232358,4.97959955842857,5.2115747076536,5.23720597040815,5.24680704476339,
5.25370468666267,5.26105045543184,5.27088604405945,5.29313366319661,5.48935994625193,
5.55700391340357,5.56511838418575,5.56903859757746,5.57208859002595,5.57544979738637,
5.58100989282558,5.60602751137852,5.65806073355562,5.81309836040524,5.85793712897173,
5.86963851818398,5.87652674884228,5.88251081746369,5.88987733632125,5.9041658123057,
6.01761112622703,6.12439057893242,6.27537940762288,6.32397338177412,6.32980036219826,
6.33246470724888,6.33450816038374,6.33669527817769,6.34011969931916,6.35076906884506,
6.40666787173508,6.48385107286157,6.66964267094354,6.72478816321071,6.73113790592886,
6.73405765829006,6.73622044784171,6.73804013832393,6.74111495239306,6.74840795149835,
6.8668242706869,6.99071742597146,7.14196370014696,7.1516794128272,7.15389525291374,
7.15534464068133,7.15651506553866,7.15784919170866,7.16012695650551,7.16963249840598,
7.21817697075377,7.33881573120204,7.53193293115088,7.54449433845744,7.54818121967568,
7.55039306320065,7.55233415854644,7.55475191927114,7.5593361462241,7.58622963422652,
7.6377810628483,7.69746167566451,7.93676797303654,7.9498855680596,7.95223786817523,
7.95366549810445,7.95478635074989,7.95601335864582,7.95799267409618,7.96462642168007,
8.0053286665715,8.06381251433966,8.12397765349998,8.14629453413927,8.17093619392347,
8.17899959373945,8.21661780854425,8.36294588747713,8.37257863718179,8.3759768179475,
8.37817903062541,8.38022574589198,8.3828842390018,8.38850258874395,8.44665309134468,
8.54610240447915,8.65619970976153,8.722040668501,8.76462846072826,8.76913501639208,
8.771409862585,8.77307097752536,8.77485496533041,8.77725130282303,8.78260350901246,
8.8665284594664,9.09788295166691,9.13877535851554,9.14768687169815,9.15244662830048,
9.15626185421358,9.16058702776937,9.16793282344946,9.19703446173512,9.42066559124138,
9.51279039668691,9.51816002007446,9.52021292130714,9.52168233687259,9.52307842345449,
9.52503216348626,9.52897642995906,9.56674891862977,9.61277441818467,9.90812336478384,
9.9220811786498,9.9301983200311,9.93324339390951,9.93540400980293,9.93757600224356,
9.9397668989649,9.94258125256913,9.9495742293905,9.95986201202622),
 .UNSPECIFIED.);
#3610=B_SPLINE_CURVE_WITH_KNOTS('',3,(#238775,#238776,#238777,#238778,#238779,
#238780,#238781,#238782,#238783,#238784,#238785,#238786,#238787,#238788,
#238789,#238790,#238791,#238792,#238793,#238794,#238795,#238796,#238797,
#238798,#238799,#238800,#238801,#238802,#238803,#238804,#238805,#238806,
#238807,#238808,#238809,#238810,#238811,#238812,#238813,#238814,#238815,
#238816,#238817,#238818,#238819,#238820,#238821,#238822,#238823,#238824,
#238825,#238826,#238827,#238828,#238829,#238830,#238831,#238832,#238833,
#238834,#238835,#238836,#238837,#238838,#238839,#238840,#238841,#238842,
#238843,#238844,#238845,#238846,#238847,#238848,#238849,#238850,#238851,
#238852,#238853,#238854,#238855,#238856,#238857,#238858,#238859,#238860,
#238861,#238862,#238863,#238864,#238865,#238866,#238867,#238868,#238869,
#238870,#238871,#238872,#238873,#238874,#238875,#238876,#238877,#238878,
#238879,#238880,#238881,#238882,#238883,#238884,#238885,#238886,#238887,
#238888,#238889,#238890,#238891,#238892,#238893,#238894,#238895,#238896,
#238897,#238898,#238899,#238900,#238901,#238902,#238903,#238904,#238905,
#238906,#238907,#238908,#238909,#238910,#238911,#238912,#238913,#238914,
#238915,#238916,#238917,#238918,#238919,#238920,#238921,#238922,#238923,
#238924,#238925,#238926,#238927,#238928,#238929,#238930,#238931,#238932,
#238933,#238934,#238935,#238936,#238937,#238938,#238939,#238940,#238941,
#238942,#238943,#238944,#238945,#238946,#238947,#238948,#238949,#238950,
#238951,#238952,#238953,#238954,#238955,#238956,#238957,#238958,#238959,
#238960,#238961,#238962,#238963,#238964,#238965,#238966,#238967,#238968,
#238969,#238970,#238971,#238972,#238973,#238974,#238975,#238976,#238977,
#238978,#238979,#238980,#238981,#238982,#238983,#238984,#238985,#238986,
#238987,#238988,#238989,#238990,#238991,#238992,#238993,#238994,#238995,
#238996,#238997,#238998,#238999,#239000,#239001,#239002,#239003,#239004,
#239005,#239006,#239007,#239008,#239009,#239010,#239011,#239012,#239013,
#239014,#239015,#239016,#239017,#239018,#239019,#239020,#239021,#239022,
#239023,#239024,#239025,#239026,#239027,#239028,#239029,#239030,#239031,
#239032,#239033,#239034,#239035,#239036),.UNSPECIFIED.,.F.,.F.,(4,3,3,3,
3,3,3,3,3,3,3,3,3,3,3,3,3,3,3,3,3,3,3,3,3,3,3,3,3,3,3,3,3,3,3,3,3,3,3,3,
3,3,3,3,3,3,3,3,3,3,3,3,3,3,3,3,3,3,3,3,3,3,3,3,3,3,3,3,3,3,3,3,3,3,3,3,
3,3,3,3,3,3,3,3,3,3,3,4),(-98.3406346348103,-98.2595400399228,-98.1783170760883,
-98.0969160050002,-98.0154335325594,-97.9338358821689,-97.8764941144939,
-97.8027170236699,-97.7290022462361,-97.6553367119498,-97.5817065668627,
-97.5080979430576,-97.4344851252523,-97.3771242465628,-97.2956907154816,
-97.2141217204853,-97.1300298850219,-97.0481871785268,-96.9629707785793,
-96.8777543786317,-96.7993214351354,-96.7209582512547,-96.6426599859769,
-96.56444072012,-96.4862714286153,-96.4081601035283,-96.3783845107007,-96.3020220396171,
-96.2256427135349,-96.1492369478946,-96.0727622758028,-95.9962502280743,
-95.919655898848,-95.8790146427695,-95.803637263832,-95.7283214304325,-95.6530543208225,
-95.5778231457396,-95.5026151405947,-95.4248226113838,-95.3496044352015,
-95.2743695596237,-95.1991064160779,-95.1238034227342,-95.0484112267784,
-94.9729663274293,-94.8974229663296,-94.8802749069074,-94.8071310979317,
-94.7340760848174,-94.6610949304227,-94.5881727677748,-94.5152947844789,
-94.4424462086562,-94.3695988076401,-94.2967484614904,-94.2238818214328,
-94.1509855280076,-94.0780033880236,-94.0049744872913,-93.93183493372,-93.8815351710452,
-93.8069465518206,-93.7324435814405,-93.6580123236801,-93.5836388898013,
-93.5093094293879,-93.4350101216312,-93.3607167604803,-93.2864232114111,
-93.212116980803,-93.1377855706714,-93.063381527802,-92.9889358754876,-92.9143993173973,
-92.882795435183,-92.8018014557991,-92.7209244177331,-92.6365497051128,
-92.5559913111839,-92.4755567692027,-92.3952973516194,-92.3834255672519,
-92.3127120478732,-92.2419793657373,-92.1712373965128,-92.100443561887,
-92.0575247206449),.UNSPECIFIED.);
#3611=B_SPLINE_CURVE_WITH_KNOTS('',3,(#239038,#239039,#239040,#239041,#239042,
#239043,#239044,#239045,#239046,#239047,#239048,#239049,#239050,#239051,
#239052,#239053,#239054,#239055,#239056,#239057,#239058,#239059,#239060,
#239061,#239062,#239063,#239064,#239065,#239066,#239067,#239068,#239069,
#239070,#239071,#239072,#239073,#239074,#239075,#239076,#239077,#239078,
#239079,#239080,#239081,#239082,#239083,#239084,#239085,#239086,#239087,
#239088,#239089,#239090,#239091,#239092,#239093,#239094,#239095,#239096,
#239097,#239098,#239099,#239100,#239101,#239102,#239103,#239104,#239105,
#239106,#239107,#239108,#239109,#239110,#239111,#239112,#239113,#239114,
#239115,#239116,#239117,#239118,#239119,#239120,#239121,#239122,#239123,
#239124,#239125,#239126,#239127,#239128,#239129,#239130,#239131,#239132,
#239133,#239134,#239135,#239136,#239137,#239138,#239139,#239140,#239141,
#239142,#239143,#239144,#239145,#239146,#239147,#239148,#239149,#239150,
#239151,#239152,#239153,#239154,#239155,#239156,#239157,#239158,#239159,
#239160,#239161,#239162,#239163,#239164,#239165,#239166,#239167,#239168,
#239169,#239170,#239171,#239172,#239173,#239174,#239175,#239176,#239177,
#239178,#239179,#239180,#239181,#239182,#239183,#239184,#239185,#239186,
#239187,#239188,#239189,#239190,#239191,#239192,#239193,#239194,#239195,
#239196,#239197,#239198,#239199,#239200,#239201,#239202,#239203,#239204,
#239205,#239206,#239207,#239208,#239209,#239210,#239211,#239212,#239213,
#239214,#239215,#239216,#239217,#239218,#239219,#239220,#239221,#239222,
#239223,#239224,#239225,#239226,#239227,#239228,#239229,#239230,#239231,
#239232,#239233,#239234,#239235,#239236,#239237,#239238,#239239,#239240,
#239241,#239242,#239243,#239244,#239245,#239246,#239247,#239248,#239249,
#239250,#239251,#239252,#239253,#239254,#239255,#239256,#239257,#239258,
#239259,#239260,#239261,#239262,#239263,#239264,#239265,#239266,#239267,
#239268,#239269,#239270,#239271,#239272,#239273,#239274,#239275,#239276,
#239277,#239278,#239279,#239280,#239281,#239282,#239283,#239284,#239285,
#239286,#239287,#239288,#239289,#239290,#239291,#239292,#239293,#239294,
#239295,#239296,#239297,#239298,#239299,#239300,#239301,#239302,#239303,
#239304,#239305,#239306,#239307,#239308,#239309,#239310,#239311,#239312,
#239313,#239314,#239315,#239316,#239317,#239318,#239319,#239320,#239321,
#239322,#239323,#239324,#239325,#239326,#239327,#239328,#239329,#239330,
#239331,#239332,#239333,#239334,#239335,#239336,#239337,#239338,#239339,
#239340,#239341,#239342,#239343,#239344,#239345,#239346,#239347,#239348,
#239349,#239350,#239351,#239352,#239353,#239354,#239355,#239356,#239357,
#239358,#239359,#239360,#239361,#239362,#239363,#239364,#239365,#239366,
#239367,#239368,#239369,#239370,#239371,#239372,#239373,#239374,#239375,
#239376,#239377,#239378,#239379,#239380,#239381,#239382,#239383,#239384,
#239385,#239386,#239387,#239388,#239389,#239390,#239391,#239392,#239393,
#239394,#239395,#239396,#239397,#239398,#239399,#239400,#239401,#239402,
#239403,#239404,#239405,#239406,#239407,#239408,#239409,#239410,#239411,
#239412,#239413,#239414,#239415,#239416,#239417,#239418,#239419,#239420,
#239421,#239422,#239423,#239424,#239425,#239426,#239427,#239428,#239429,
#239430,#239431,#239432,#239433,#239434,#239435,#239436,#239437,#239438,
#239439,#239440,#239441,#239442,#239443,#239444,#239445,#239446,#239447,
#239448,#239449,#239450,#239451,#239452,#239453,#239454,#239455,#239456,
#239457,#239458,#239459,#239460,#239461,#239462,#239463,#239464,#239465,
#239466,#239467,#239468,#239469,#239470,#239471,#239472,#239473,#239474,
#239475,#239476,#239477,#239478,#239479,#239480,#239481,#239482,#239483,
#239484,#239485,#239486,#239487,#239488,#239489,#239490,#239491,#239492,
#239493,#239494,#239495,#239496,#239497,#239498,#239499,#239500,#239501,
#239502,#239503,#239504,#239505,#239506,#239507,#239508,#239509,#239510,
#239511,#239512,#239513,#239514,#239515,#239516,#239517,#239518,#239519,
#239520,#239521,#239522,#239523,#239524,#239525,#239526,#239527,#239528,
#239529,#239530,#239531,#239532,#239533,#239534,#239535,#239536,#239537,
#239538,#239539,#239540,#239541,#239542,#239543,#239544,#239545,#239546,
#239547,#239548,#239549,#239550,#239551,#239552,#239553,#239554,#239555,
#239556,#239557,#239558,#239559,#239560,#239561,#239562,#239563,#239564,
#239565,#239566,#239567,#239568,#239569),.UNSPECIFIED.,.F.,.F.,(4,2,2,2,
2,2,2,2,2,2,2,2,2,2,2,2,2,2,2,2,2,2,2,2,2,2,2,2,2,2,2,2,2,2,2,2,2,2,2,2,
2,2,2,2,2,2,2,2,2,2,2,2,2,2,2,2,2,2,2,2,2,2,2,2,2,2,2,2,2,2,2,2,2,2,2,2,
2,2,2,2,2,2,2,2,2,2,2,2,2,2,2,2,2,2,2,2,2,2,2,2,2,2,2,2,2,2,2,2,2,2,2,2,
2,2,2,2,2,2,2,2,2,2,2,2,2,2,2,2,2,2,2,2,2,2,2,2,2,2,2,2,2,2,2,2,2,2,2,2,
2,2,2,2,2,2,2,2,2,2,2,2,2,2,2,2,2,2,2,2,2,2,2,2,2,2,2,2,2,2,2,2,2,2,2,2,
2,2,2,2,2,2,2,2,2,2,2,2,2,2,2,2,2,2,2,2,2,2,2,2,2,2,2,2,2,2,2,2,2,2,2,2,
2,2,2,2,2,2,2,2,2,2,2,2,2,2,2,2,2,2,2,2,2,2,2,2,2,2,2,2,2,2,2,2,2,2,2,2,
2,2,2,2,2,2,2,2,2,4),(0.00168853654697166,0.103339731779065,0.116709103368618,
0.119909819402091,0.121921927725409,0.123450686793796,0.125005944841013,
0.12646436286641,0.128477680641417,0.132515065212291,0.177689730312591,
0.228623367850564,0.249036582934583,0.268445607615176,0.303450819898069,
0.374741801445695,0.484928277307592,0.527814364491861,0.533458032260693,
0.536289952263605,0.538327552940703,0.540485236988003,0.543520125587614,
0.549791950905152,0.61495115622597,0.831600933000776,0.906641884417419,
0.933284008908887,0.948747815085201,0.952405588095498,0.954155556065803,
0.955805456194687,0.957564232907861,0.960565088326756,0.96872739470707,
1.01488825339754,1.02098415546149,1.10356382417768,1.3277152707527,1.37527288312188,
1.38490143914292,1.39382965514626,1.40037061669404,1.40846560719594,1.42196674955635,
1.46898226310315,1.58285488841581,1.64103889779607,1.68191669357966,1.70389993752507,
1.70964361566064,1.7125441444328,1.71549165590169,1.71859027738407,1.72424135909924,
1.74799894038754,1.93308197397957,1.99880602126494,2.01127147313891,2.01853235860103,
2.02451028080824,2.03148133259751,2.04356235634708,2.09646940527705,2.10398228705012,
2.10490186330515,2.10587811737234,2.10854866602033,2.3290771378131,2.46349727660132,
2.47181110792954,2.47491926149835,2.47681356345735,2.47885612828041,2.48151546511217,
2.48731761399358,2.54145516429396,2.7652313972412,2.8377069473607,2.87007967974646,
2.87520429309674,2.87786585918399,2.8800244111254,2.88217749645447,2.88607186763164,
2.89810235538176,3.08116099681484,3.19950167804142,3.24734514166295,3.2788950104216,
3.29439130645193,3.29708304165713,3.29850744990815,3.29956309069247,3.30071056266545,
3.30237447278133,3.30719192326801,3.38260961457423,3.55985410753927,3.65239015410068,
3.68556094803072,3.69039635096814,3.69286646711469,3.69466131221872,3.69657836676933,
3.6998587646696,3.70880991178198,3.84228172598022,3.98236506457672,4.05625028332767,
4.08053406073973,4.09280075552887,4.09519521565728,4.09650557507375,4.09750598523813,
4.09862346252664,4.10066859228941,4.10716399529996,4.2100660153807,4.41703773010512,
4.51076886249678,4.51679478019851,4.5195658435748,4.52165877740946,4.52362998002922,
4.52636489079275,4.53189764305847,4.58282917182821,4.63692616519046,4.82942715706796,
4.89896505390662,4.91025439857647,4.91345940811302,4.91541200134376,4.9171736932817,
4.91942168872401,4.92385406422193,4.95016294717397,4.97897029083771,5.036575624393,
5.12685406664593,5.16867720942107,5.27631099976005,5.28829590462778,5.29304485042576,
5.29695758346708,5.30093033201643,5.30666871558552,5.32155851700503,5.39021514263851,
5.48803571729544,5.65017830051696,5.65875447732786,5.66152321278846,5.66305339979902,
5.66457194136063,5.66645483831327,5.67005879372544,5.69379770098295,5.72471854317786,
5.76343072559383,5.97135389644435,5.99512276541605,6.064694695965,6.07163974256652,
6.07448754261534,6.07659580077471,6.0788877827083,6.08201681604806,6.08922084850348,
6.19287285235846,6.34176514002606,6.47990495044213,6.48870401131937,6.49180150205578,
6.49357792703083,6.49522056462194,6.49745034302472,6.50171003325252,6.5278425942545,
6.58887115706061,6.6913161784719,6.89253921815124,6.91862129425685,6.92914893333392,
6.93593619220506,6.94335382702288,6.9536284980989,6.97849892936106,7.09448146098816,
7.17109372123003,7.2383000085443,7.24640418032512,7.25032117506468,7.25336944989762,
7.25672956132128,7.26228993755151,7.28734330302029,7.33950737510419,7.50053846524446,
7.54002157104421,7.55016741781575,7.55707834179827,7.56245209498876,7.56931978872469,
7.58125956322892,7.637273796907,7.76266390317901,7.98173145793878,7.99701380263632,
8.00066057287301,8.00949775476811,8.01279011218912,8.01473234487359,8.01656264501494,
8.01910058157145,8.02414191891868,8.06313402520017,8.08316012605268,8.2061315746236,
8.35853773941729,8.40601511165231,8.41160863972868,8.41441819759993,8.41646443728593,
8.41853123151786,8.42133640741034,8.42721010458581,8.43487546995718,8.452623324503,
8.50440190469988,8.57372475598848,8.81842456013667,8.83201697021729,8.83451051409028,
8.83602848572844,8.83720922687333,8.83848890813283,8.84052533983301,8.8473323555643,
8.89005019233614,8.93182688192965,9.0390439423254,9.09698435937286,9.20580204566911,
9.22396924230918,9.22785583344512,9.23035189577089,9.23224036131919,9.23439597264157,
9.23785350294356,9.24194676519544,9.24979245494232,9.26864661996942,9.32277930518578,
9.42944215632464,9.61843082928927,9.63014555805185,9.63240842327018,9.63382458804416,
9.63494069532217,9.6361854288512,9.63824561408103,9.64566164813229,9.69449048739954,
9.95574806259247),.UNSPECIFIED.);
#3612=B_SPLINE_CURVE_WITH_KNOTS('',3,(#239571,#239572,#239573,#239574,#239575,
#239576,#239577,#239578,#239579,#239580,#239581,#239582,#239583,#239584,
#239585,#239586,#239587,#239588,#239589,#239590,#239591,#239592,#239593,
#239594,#239595,#239596,#239597,#239598,#239599,#239600,#239601,#239602,
#239603,#239604,#239605,#239606,#239607,#239608,#239609,#239610,#239611,
#239612,#239613,#239614,#239615,#239616,#239617,#239618,#239619,#239620,
#239621,#239622,#239623,#239624,#239625,#239626,#239627,#239628,#239629,
#239630,#239631,#239632,#239633,#239634,#239635,#239636,#239637,#239638,
#239639,#239640,#239641,#239642,#239643,#239644,#239645,#239646,#239647,
#239648,#239649,#239650,#239651,#239652,#239653,#239654,#239655,#239656,
#239657,#239658,#239659,#239660,#239661,#239662,#239663,#239664,#239665,
#239666,#239667,#239668,#239669,#239670,#239671,#239672,#239673,#239674,
#239675,#239676,#239677,#239678,#239679,#239680,#239681,#239682,#239683,
#239684,#239685,#239686,#239687,#239688,#239689,#239690,#239691,#239692,
#239693,#239694,#239695,#239696,#239697,#239698,#239699,#239700,#239701,
#239702,#239703,#239704,#239705,#239706,#239707,#239708,#239709,#239710,
#239711,#239712,#239713,#239714,#239715,#239716,#239717,#239718,#239719,
#239720,#239721,#239722,#239723,#239724,#239725,#239726,#239727,#239728,
#239729,#239730,#239731,#239732,#239733,#239734,#239735,#239736,#239737,
#239738,#239739,#239740,#239741,#239742,#239743,#239744,#239745,#239746,
#239747,#239748,#239749,#239750,#239751,#239752,#239753,#239754,#239755,
#239756,#239757,#239758,#239759,#239760,#239761,#239762,#239763,#239764,
#239765,#239766,#239767,#239768,#239769,#239770,#239771,#239772,#239773,
#239774,#239775,#239776,#239777,#239778,#239779,#239780,#239781,#239782,
#239783,#239784,#239785,#239786,#239787,#239788,#239789,#239790,#239791,
#239792,#239793,#239794,#239795,#239796,#239797,#239798,#239799,#239800,
#239801,#239802,#239803,#239804,#239805,#239806,#239807,#239808,#239809,
#239810,#239811,#239812,#239813,#239814,#239815,#239816,#239817,#239818,
#239819,#239820,#239821,#239822,#239823,#239824,#239825,#239826,#239827,
#239828,#239829),.UNSPECIFIED.,.F.,.F.,(4,3,3,3,3,3,3,3,3,3,3,3,3,3,3,3,
3,3,3,3,3,3,3,3,3,3,3,3,3,3,3,3,3,3,3,3,3,3,3,3,3,3,3,3,3,3,3,3,3,3,3,3,
3,3,3,3,3,3,3,3,3,3,3,3,3,3,3,3,3,3,3,3,3,3,3,3,3,3,3,3,3,3,3,3,3,3,4),
(-79.4911541062857,-79.4169417776376,-79.3427292477536,-79.2685040476418,
-79.1942537038747,-79.119923121499,-79.0455512581999,-78.9710699178442,
-78.9004391331125,-78.8194451537285,-78.738568115662,-78.6541934030418,
-78.5736350091126,-78.4932004671337,-78.412941049551,-78.4010692651813,
-78.3266649619649,-78.252243891163,-78.177793779712,-78.103261744439,-78.0286853041711,
-77.9540043574025,-77.9016993972503,-77.8251278538832,-77.7486239612732,
-77.6721767666834,-77.5957753576583,-77.5194088546811,-77.4423527055195,
-77.3660153154383,-77.2896784441415,-77.2133322359245,-77.1357390922904,
-77.0593199805502,-76.9811398209692,-76.9029596613881,-76.8291825705641,
-76.7554677931303,-76.6818022588445,-76.6081721137573,-76.5345634899521,
-76.4609506721469,-76.403589793457,-76.3221562623758,-76.2405872673796,
-76.1564954319162,-76.074652725421,-75.9894363254734,-75.9042199255259,
-75.8257869820293,-75.7474237981485,-75.6691255328703,-75.5909062670135,
-75.5127369755081,-75.434625650421,-75.4048500575948,-75.3284875865113,
-75.2521082604288,-75.1757024947876,-75.0992278226961,-75.0227157749675,
-74.9461214457415,-74.9054801896637,-74.8301028107262,-74.7547869773266,
-74.6795198677163,-74.6042886926334,-74.5290806874893,-74.4512881582783,
-74.3760699820961,-74.3008351065181,-74.2255719629728,-74.1502689696294,
-74.0748767736736,-73.9994318743241,-73.9238885132244,-73.9067404538015,
-73.8341485820666,-73.7616487829755,-73.6892437432365,-73.616893345192,
-73.5445839604959,-73.4723019987726,-73.4000210509366,-73.3277420649391,
-73.2554289082589,-73.2079687991061),.UNSPECIFIED.);
#3613=B_SPLINE_CURVE_WITH_KNOTS('',3,(#239831,#239832,#239833,#239834,#239835,
#239836,#239837,#239838,#239839,#239840,#239841,#239842,#239843),
 .UNSPECIFIED.,.F.,.F.,(4,1,1,1,1,1,1,1,1,1,4),(-73.2079630106607,-72.9080007179394,
-71.9092609820772,-71.4098911141461,-70.910521246215,-69.9117815103528,
-69.4124116424217,-68.9130417744906,-68.4136719065595,-67.9143020386284,
-66.9247834919266),.UNSPECIFIED.);
#3614=B_SPLINE_CURVE_WITH_KNOTS('',3,(#239845,#239846,#239847,#239848,#239849,
#239850,#239851,#239852,#239853,#239854,#239855,#239856,#239857,#239858,
#239859,#239860,#239861,#239862,#239863,#239864,#239865,#239866,#239867,
#239868,#239869,#239870,#239871,#239872,#239873,#239874,#239875,#239876,
#239877,#239878,#239879,#239880,#239881,#239882,#239883,#239884,#239885,
#239886,#239887,#239888,#239889,#239890,#239891,#239892,#239893,#239894,
#239895,#239896,#239897,#239898,#239899,#239900,#239901,#239902,#239903,
#239904,#239905,#239906,#239907,#239908,#239909,#239910,#239911,#239912,
#239913,#239914,#239915,#239916,#239917,#239918,#239919,#239920,#239921,
#239922,#239923,#239924,#239925,#239926,#239927,#239928,#239929,#239930,
#239931,#239932,#239933,#239934,#239935,#239936,#239937,#239938,#239939,
#239940,#239941,#239942,#239943,#239944,#239945,#239946,#239947,#239948,
#239949,#239950,#239951,#239952,#239953,#239954,#239955,#239956,#239957,
#239958,#239959,#239960,#239961,#239962,#239963,#239964,#239965,#239966,
#239967,#239968,#239969,#239970,#239971,#239972,#239973,#239974,#239975,
#239976,#239977,#239978,#239979,#239980,#239981,#239982,#239983,#239984,
#239985,#239986,#239987,#239988,#239989,#239990,#239991,#239992,#239993,
#239994,#239995,#239996,#239997,#239998,#239999,#240000,#240001,#240002,
#240003,#240004,#240005,#240006,#240007,#240008,#240009,#240010,#240011,
#240012,#240013,#240014,#240015,#240016,#240017,#240018,#240019,#240020,
#240021,#240022,#240023,#240024,#240025,#240026,#240027,#240028,#240029,
#240030,#240031,#240032,#240033,#240034,#240035,#240036,#240037,#240038,
#240039,#240040,#240041,#240042,#240043,#240044,#240045,#240046,#240047,
#240048,#240049,#240050,#240051,#240052,#240053,#240054,#240055,#240056,
#240057,#240058,#240059,#240060,#240061,#240062,#240063,#240064,#240065,
#240066,#240067,#240068,#240069,#240070,#240071,#240072,#240073,#240074,
#240075,#240076,#240077,#240078,#240079,#240080,#240081,#240082,#240083,
#240084,#240085,#240086,#240087,#240088,#240089,#240090,#240091,#240092,
#240093,#240094,#240095,#240096,#240097,#240098,#240099,#240100,#240101,
#240102,#240103,#240104,#240105,#240106,#240107,#240108,#240109,#240110,
#240111,#240112,#240113,#240114,#240115,#240116,#240117,#240118,#240119,
#240120,#240121,#240122,#240123,#240124,#240125,#240126,#240127,#240128,
#240129,#240130,#240131,#240132,#240133,#240134,#240135,#240136,#240137,
#240138,#240139,#240140,#240141,#240142,#240143,#240144,#240145,#240146,
#240147,#240148,#240149,#240150,#240151,#240152,#240153,#240154,#240155,
#240156,#240157,#240158,#240159,#240160,#240161,#240162,#240163,#240164,
#240165,#240166,#240167,#240168,#240169,#240170,#240171,#240172,#240173,
#240174,#240175,#240176,#240177,#240178,#240179,#240180,#240181,#240182,
#240183,#240184,#240185,#240186,#240187,#240188,#240189,#240190,#240191,
#240192,#240193,#240194,#240195,#240196,#240197,#240198,#240199,#240200,
#240201,#240202,#240203,#240204,#240205,#240206,#240207,#240208,#240209,
#240210,#240211,#240212,#240213,#240214,#240215,#240216,#240217,#240218,
#240219,#240220,#240221,#240222,#240223,#240224,#240225,#240226,#240227,
#240228,#240229,#240230,#240231,#240232,#240233,#240234,#240235,#240236,
#240237,#240238,#240239,#240240,#240241,#240242,#240243,#240244,#240245,
#240246,#240247,#240248,#240249,#240250,#240251,#240252,#240253,#240254,
#240255,#240256,#240257,#240258,#240259,#240260,#240261,#240262,#240263,
#240264,#240265,#240266,#240267,#240268,#240269,#240270,#240271,#240272,
#240273,#240274,#240275,#240276,#240277,#240278,#240279,#240280,#240281,
#240282,#240283,#240284,#240285,#240286,#240287,#240288,#240289,#240290,
#240291,#240292,#240293,#240294,#240295,#240296,#240297,#240298,#240299,
#240300,#240301,#240302,#240303,#240304,#240305,#240306,#240307,#240308,
#240309,#240310,#240311,#240312,#240313,#240314,#240315,#240316,#240317,
#240318,#240319,#240320,#240321,#240322,#240323,#240324,#240325,#240326,
#240327,#240328,#240329,#240330,#240331,#240332,#240333,#240334,#240335,
#240336,#240337,#240338,#240339,#240340,#240341,#240342,#240343,#240344,
#240345,#240346,#240347,#240348,#240349,#240350,#240351,#240352,#240353,
#240354,#240355,#240356,#240357,#240358,#240359,#240360,#240361,#240362,
#240363,#240364,#240365,#240366,#240367,#240368,#240369,#240370,#240371,
#240372,#240373,#240374,#240375,#240376,#240377,#240378,#240379,#240380),
 .UNSPECIFIED.,.F.,.F.,(4,2,2,2,2,2,2,2,2,2,2,2,2,2,2,2,2,2,2,2,2,2,2,2,
2,2,2,2,2,2,2,2,2,2,2,2,2,2,2,2,2,2,2,2,2,2,2,2,2,2,2,2,2,2,2,2,2,2,2,2,
2,2,2,2,2,2,2,2,2,2,2,2,2,2,2,2,2,2,2,2,2,2,2,2,2,2,2,2,2,2,2,2,2,2,2,2,
2,2,2,2,2,2,2,2,2,2,2,2,2,2,2,2,2,2,2,2,2,2,2,2,2,2,2,2,2,2,2,2,2,2,2,2,
2,2,2,2,2,2,2,2,2,2,2,2,2,2,2,2,2,2,2,2,2,2,2,2,2,2,2,2,2,2,2,2,2,2,2,2,
2,2,2,2,2,2,2,2,2,2,2,2,2,2,2,2,2,2,2,2,2,2,2,2,2,2,2,2,2,2,2,2,2,2,2,2,
2,2,2,2,2,2,2,2,2,2,2,2,2,2,2,2,2,2,2,2,2,2,2,2,2,2,2,2,2,2,2,2,2,2,2,2,
2,2,2,2,2,2,2,2,2,2,2,2,2,2,2,2,2,2,2,2,2,2,2,2,2,2,2,4),(0.00169193791497629,
0.00269170506770563,0.00382150025259507,0.00497529633340349,0.00612871498677458,
0.00781404984112232,0.0127998102560316,0.0992952071431597,0.241006483008384,
0.322626394132003,0.377792672142896,0.392612611969002,0.396430301496517,
0.398680227178473,0.40066282537986,0.403129648395394,0.406921427368932,
0.423882088545111,0.720344176276257,0.761999575993357,0.786495003610549,
0.794610060402936,0.798187028584304,0.800148816717977,0.801850918525245,
0.802890651810846,0.804020129466061,0.805502025233649,0.808777036101699,
0.834874903823989,0.920904233879457,0.967500913020852,0.980912714031539,
0.996157536723248,1.01371285205981,1.03430642778889,1.05917268435567,1.1462898639267,
1.19419078706825,1.21892152272548,1.22353968531524,1.22602709661673,1.22807158792978,
1.2304798192881,1.23462312763094,1.25019882037846,1.50776471703766,1.61170323614546,
1.61806083577225,1.62063131590095,1.62244712727404,1.62408777752376,1.62653484005037,
1.63208333747967,1.69733399475308,1.71453434540894,1.77072893152393,1.82607377245994,
1.86883958206715,1.97233102078528,1.99209917900411,1.99861236331483,2.00275211594448,
2.00661155462139,2.01163740824028,2.02223697865391,2.11094795066746,2.2521701178907,
2.31149739673316,2.34706474246649,2.36436910993395,2.36773658355138,2.36956942002404,
2.37094074793797,2.37263899443585,2.37543340819382,2.38464280408234,2.52136993519002,
2.66382753941995,2.69168124697717,2.74567494986017,2.77453042838392,2.77964388032204,
2.78236530897271,2.7846064282369,2.78721020996672,2.79166387605688,2.80814413952905,
3.0723007112816,3.19249748446832,3.19770148117874,3.20012160946691,3.20192793370995,
3.20385213158838,3.20678705274988,3.21490666489957,3.26058563038,3.45696833731933,
3.60858174425896,3.62933295423243,3.6388758473337,3.64617743203437,3.6531596255548,
3.66512330126049,3.69907632554344,3.72244135797862,3.9207261316018,3.94939208378295,
3.95564501118944,3.95917706738549,3.96220477585861,3.96586978785082,3.97278949746997,
4.02143038678407,4.16594232237504,4.21793371071668,4.25046108114024,4.26061642479772,
4.26709636139357,4.27317011279584,4.28115037057796,4.29909527338847,4.42922029695093,
4.45532200989663,4.6151098573033,4.68561020734812,4.71496503238116,4.71969958685053,
4.72217437990107,4.72419011427012,4.72650766679617,4.73041406749951,4.7443145311256,
4.9817770008264,5.11136280130468,5.11975512578225,5.12277618835428,5.12488027268926,
5.12683269665446,5.12949280737777,5.13460835220472,5.166719266993,5.23760724695966,
5.43608360217353,5.51880128110111,5.54007577545144,5.54327138229398,5.54478268616827,
5.54596300416593,5.54724703090316,5.54930075443546,5.55626618434596,5.60059970139283,
5.71391934567529,5.76770393658139,5.83765198534363,5.86655691376328,5.92976267005913,
5.93596224009174,5.93848959361659,5.9403551204055,5.94237782829179,5.94512950614628,
5.95142129764205,6.06660831633939,6.21447673287528,6.33258252053735,6.33996131170891,
6.34208622879112,6.3432143380281,6.34421423220962,6.34550979973154,6.34779606258712,
6.35786515280854,6.50209947308295,6.63022997193524,6.68385855991787,6.75636680479173,
6.76300222428483,6.76566786760625,6.76762152277431,6.76972646836974,6.77256650816992,
6.77896061103927,6.90010161075822,7.04944354150552,7.11024052719992,7.13157422536459,
7.15503633824202,7.15895189951689,7.16128266915803,7.16306272759256,7.16495997673894,
7.16791350023821,7.17629680272853,7.22445722843781,7.27171794556602,7.38298996736577,
7.52272654605282,7.53492211562209,7.53984331999971,7.54344558705204,7.5470762183348,
7.55207062557926,7.56270376977997,7.57658146530835,7.6979480214644,7.89693516338263,
7.90608691397582,7.90892907885227,7.91047472319245,7.91185436953749,7.91365560717128,
7.91687678948814,7.93211474533385,7.96186624535493,7.98775288882021,8.11227883685769,
8.29696385425935,8.31608660193267,8.32037354804583,8.32316558670998,8.32541176434123,
8.32796330222301,8.33229917487821,8.34921812148471,8.47198196962048,8.57770487934709,
8.72604339770952,8.73626234349374,8.73955529783358,8.7413717060368,8.74300872228565,
8.74516883785471,8.74909927208373,8.76861747392223,8.84327724321625,8.8922336851052,
9.10085744071271,9.15955384252156,9.17374138775755,9.18206044321826,9.18921735449683,
9.19795299470797,9.21462684093077,9.23562578246183,9.2825854315289,9.37911520275485,
9.44521762658215,9.48781279647693,9.49448894292639,9.49847904204394,9.50154865086394,
9.50436835791005,9.50757441393806,9.51205835446919,9.55249840557096,9.66752902267458,
9.70622078553479,9.78400107516521,9.7965135759874,9.80418665527794,9.81021515008504,
9.81583977894261,9.82236785490708,9.83171345803354,9.86860524257916,9.96114864333145),
 .UNSPECIFIED.);
#3615=B_SPLINE_CURVE_WITH_KNOTS('',3,(#240382,#240383,#240384,#240385,#240386,
#240387,#240388,#240389,#240390,#240391,#240392,#240393,#240394,#240395,
#240396,#240397,#240398,#240399),.UNSPECIFIED.,.F.,.F.,(4,2,2,2,2,2,2,2,
4),(-54.3584128775674,-53.5234959656725,-52.6885790537777,-51.8536621418828,
-51.018745229988,-50.1838283180931,-49.3489114061983,-48.5139944943034,
-48.0752275703878),.UNSPECIFIED.);
#3616=B_SPLINE_CURVE_WITH_KNOTS('',3,(#240401,#240402,#240403,#240404,#240405,
#240406,#240407,#240408,#240409,#240410,#240411,#240412,#240413,#240414,
#240415,#240416,#240417,#240418,#240419,#240420,#240421,#240422,#240423,
#240424,#240425,#240426,#240427,#240428,#240429,#240430,#240431,#240432,
#240433,#240434,#240435,#240436,#240437,#240438,#240439,#240440,#240441,
#240442,#240443,#240444,#240445,#240446,#240447,#240448,#240449,#240450,
#240451,#240452,#240453,#240454,#240455,#240456,#240457,#240458,#240459,
#240460,#240461,#240462,#240463,#240464,#240465,#240466,#240467,#240468,
#240469,#240470,#240471,#240472,#240473,#240474,#240475,#240476,#240477,
#240478,#240479,#240480,#240481,#240482,#240483,#240484,#240485,#240486,
#240487,#240488,#240489,#240490,#240491,#240492,#240493,#240494,#240495,
#240496,#240497,#240498,#240499,#240500,#240501,#240502,#240503,#240504,
#240505,#240506,#240507,#240508,#240509,#240510,#240511,#240512,#240513,
#240514,#240515,#240516,#240517,#240518,#240519,#240520,#240521,#240522,
#240523,#240524,#240525,#240526,#240527,#240528,#240529,#240530,#240531,
#240532,#240533,#240534,#240535,#240536,#240537,#240538,#240539,#240540,
#240541,#240542,#240543,#240544,#240545,#240546,#240547,#240548,#240549,
#240550,#240551,#240552,#240553,#240554,#240555,#240556,#240557,#240558,
#240559,#240560,#240561,#240562,#240563,#240564,#240565,#240566,#240567,
#240568,#240569,#240570,#240571,#240572,#240573,#240574,#240575,#240576,
#240577,#240578,#240579,#240580,#240581,#240582,#240583,#240584,#240585,
#240586,#240587,#240588,#240589,#240590,#240591,#240592,#240593,#240594,
#240595,#240596,#240597,#240598,#240599,#240600,#240601,#240602,#240603,
#240604,#240605,#240606,#240607,#240608,#240609,#240610,#240611,#240612,
#240613,#240614,#240615,#240616,#240617,#240618,#240619,#240620,#240621,
#240622,#240623,#240624,#240625,#240626,#240627,#240628,#240629,#240630,
#240631,#240632,#240633,#240634,#240635,#240636,#240637,#240638,#240639,
#240640,#240641,#240642,#240643,#240644,#240645,#240646,#240647,#240648,
#240649,#240650,#240651,#240652,#240653,#240654,#240655,#240656,#240657,
#240658,#240659,#240660,#240661,#240662,#240663,#240664,#240665,#240666,
#240667,#240668,#240669,#240670,#240671,#240672,#240673,#240674,#240675,
#240676,#240677,#240678,#240679,#240680,#240681,#240682,#240683,#240684,
#240685,#240686,#240687,#240688,#240689,#240690,#240691,#240692,#240693,
#240694,#240695,#240696,#240697,#240698,#240699,#240700,#240701,#240702,
#240703,#240704,#240705,#240706,#240707,#240708,#240709,#240710,#240711,
#240712,#240713,#240714,#240715,#240716,#240717,#240718,#240719,#240720,
#240721,#240722,#240723,#240724,#240725,#240726,#240727,#240728,#240729,
#240730,#240731,#240732,#240733,#240734,#240735,#240736,#240737,#240738,
#240739,#240740,#240741,#240742,#240743,#240744,#240745,#240746,#240747,
#240748,#240749,#240750,#240751,#240752,#240753,#240754,#240755,#240756,
#240757,#240758,#240759,#240760,#240761,#240762,#240763,#240764,#240765,
#240766,#240767,#240768,#240769,#240770,#240771,#240772,#240773,#240774,
#240775,#240776,#240777,#240778,#240779,#240780,#240781,#240782,#240783,
#240784,#240785,#240786,#240787,#240788,#240789,#240790,#240791,#240792,
#240793,#240794,#240795,#240796,#240797,#240798,#240799,#240800,#240801,
#240802,#240803,#240804,#240805,#240806,#240807,#240808,#240809,#240810,
#240811,#240812,#240813,#240814,#240815,#240816,#240817,#240818,#240819,
#240820,#240821,#240822,#240823,#240824,#240825,#240826,#240827,#240828,
#240829,#240830,#240831,#240832,#240833,#240834,#240835,#240836,#240837,
#240838,#240839,#240840,#240841,#240842,#240843,#240844,#240845,#240846,
#240847,#240848,#240849,#240850,#240851,#240852,#240853,#240854,#240855,
#240856,#240857,#240858,#240859,#240860,#240861,#240862,#240863,#240864,
#240865,#240866,#240867,#240868,#240869,#240870,#240871,#240872,#240873,
#240874,#240875,#240876,#240877,#240878,#240879,#240880,#240881,#240882,
#240883,#240884,#240885,#240886,#240887,#240888,#240889,#240890,#240891,
#240892,#240893,#240894,#240895,#240896,#240897,#240898,#240899,#240900,
#240901,#240902,#240903,#240904,#240905,#240906,#240907,#240908,#240909,
#240910,#240911,#240912,#240913,#240914,#240915,#240916,#240917,#240918,
#240919,#240920,#240921,#240922,#240923,#240924,#240925,#240926,#240927,
#240928,#240929,#240930,#240931,#240932,#240933,#240934),.UNSPECIFIED.,
 .F.,.F.,(4,2,2,2,2,2,2,2,2,2,2,2,2,2,2,2,2,2,2,2,2,2,2,2,2,2,2,2,2,2,2,
2,2,2,2,2,2,2,2,2,2,2,2,2,2,2,2,2,2,2,2,2,2,2,2,2,2,2,2,2,2,2,2,2,2,2,2,
2,2,2,2,2,2,2,2,2,2,2,2,2,2,2,2,2,2,2,2,2,2,2,2,2,2,2,2,2,2,2,2,2,2,2,2,
2,2,2,2,2,2,2,2,2,2,2,2,2,2,2,2,2,2,2,2,2,2,2,2,2,2,2,2,2,2,2,2,2,2,2,2,
2,2,2,2,2,2,2,2,2,2,2,2,2,2,2,2,2,2,2,2,2,2,2,2,2,2,2,2,2,2,2,2,2,2,2,2,
2,2,2,2,2,2,2,2,2,2,2,2,2,2,2,2,2,2,2,2,2,2,2,2,2,2,2,2,2,2,2,2,2,2,2,2,
2,2,2,2,2,2,2,2,2,2,2,2,2,2,2,2,2,2,2,2,2,2,2,2,2,2,2,2,2,2,2,2,2,2,2,2,
2,2,2,2,2,2,2,2,2,2,2,2,2,2,2,2,2,2,2,4),(0.00146851476906278,0.0692655499922215,
0.089400024040553,0.0944724269859721,0.0979216631136692,0.10079614387533,
0.103826040131627,0.107544923500693,0.115003199896438,0.186094811208884,
0.224090798072318,0.247835106160534,0.308925425060645,0.385911850393577,
0.395396505367879,0.401983996719065,0.40758372284573,0.413584498335929,
0.421163537381088,0.43313302811207,0.511650111852883,0.533885271508265,
0.550653768842362,0.610088844507437,0.695342960668452,0.763872207393003,
0.828673286310461,0.846988381638754,0.858255087048304,0.860883916315355,
0.863343919807208,0.865358432888645,0.867383740437143,0.871096100778068,
0.882928927181664,1.00570375849612,1.0949202422572,1.10725360276171,1.12203587807812,
1.14024040144564,1.17665250669679,1.22959135477994,1.2574577685711,1.26238349373266,
1.26500332067486,1.26695109340906,1.26938195387707,1.27344676632077,1.28684307039591,
1.48953822268046,1.59429653067734,1.64722436496261,1.67001914779108,1.68193156982673,
1.68442587582703,1.68580788963179,1.68686010553232,1.68820667708916,1.69048067620084,
1.699007592445,1.83320636878154,1.91433248206823,2.00116412607974,2.04758138321328,
2.07327093689801,2.07779856366154,2.08020438118668,2.08199201583473,2.08393984632913,
2.08737273939037,2.09736311776734,2.25035853958936,2.34086219951431,2.42334381656648,
2.47124487084906,2.48045694180497,2.48264705455828,2.48391445301725,2.48502773023013,
2.48640815062321,2.48852180057692,2.49783469281014,2.64027236954451,2.78661456731993,
2.89790777159325,2.90405032128404,2.90684380022263,2.9089408203341,2.91090649083658,
2.91361889860019,2.9205288124644,3.00746342268466,3.08094752984613,3.21696487836916,
3.28628447779599,3.29366639353152,3.2992417040133,3.30167813007679,3.30346861096541,
3.30512016524016,3.30735819810807,3.3117302047703,3.34616255928018,3.48102229500202,
3.66470672226491,3.67616166560683,3.68133677937927,3.68520523450572,3.68882296825786,
3.69380834510445,3.70380937046665,3.80930176243178,3.95469563085087,4.01412049204915,
4.04445109559307,4.04833620637309,4.05027756287007,4.05167092904741,4.05314329642527,
4.05520855719195,4.05945341164996,4.11624426606879,4.35259196524155,4.45173974255662,
4.45942928899073,4.46264309909995,4.46495101407759,4.46704243310408,4.4698209430599,
4.47651653444533,4.53544696527002,4.58686524887046,4.78434186162305,4.81647525970919,
4.86725545082275,4.8767945511091,4.87987594964872,4.88184718000565,4.88369104798299,
4.88609800726606,4.89118138658488,4.93073369506005,4.93397829819044,4.9424219841965,
4.94746081248866,4.96182761578438,4.97931403108478,5.13232177972035,5.19767445793448,
5.29017099030379,5.30814170620958,5.31726645604533,5.32404357307894,5.33147412144347,
5.34181122439952,5.36705810810029,5.48654600837033,5.62010697718058,5.63243770025018,
5.63674947375852,5.63972184210742,5.64246037319347,5.64616461509851,5.65353944431,
5.65891213165663,5.75702947264751,5.81745184643111,5.8900276791472,5.92842317402104,
5.93963986723146,5.94635255651402,5.95175639700145,5.95908673606465,5.97320283754696,
6.08260894230299,6.18869458790093,6.33186130138922,6.39275686151867,6.39886911788521,
6.40158565431815,6.40363759916557,6.40580370646485,6.40913420829052,6.41903724095087,
6.58242591113428,6.64124548791066,6.78932858486455,6.79899146336551,6.80248121211969,
6.80476739780165,6.80690958549081,6.80971868068372,6.81575512173777,6.88803267113628,
6.94634842367095,7.15777823880518,7.21826760452027,7.22242266133639,7.2239985759794,
7.22512208375423,7.22618560398163,7.22766751009316,7.23063917424668,7.25778159710836,
7.3405378102815,7.42141909464429,7.60213831654654,7.61198270719985,7.61667453197753,
7.61911681233593,7.62106469069747,7.62292166189652,7.62620201937552,7.63597445512227,
7.68802905016287,7.74398652575734,7.86691034088456,7.99386296446121,8.01799387513124,
8.02083409728693,8.02225893514415,8.02330653245235,8.024442106603,8.0259859358551,
8.02951019481616,8.16114626072756,8.26532140583614,8.43049623128637,8.44129483081343,
8.44485577421308,8.44709601763168,8.44913169165893,8.45170803553229,8.45692585819034,
8.49696761798772,8.60010556517228,8.67224933983917,8.82674969048819,8.83676331148724,
8.83995907297507,8.8417143463864,8.84346735621258,8.84561833100048,8.84972792404426,
8.87483099212183,8.93025937475379,9.16046590934478,9.20700970330384,9.21578324258158,
9.22077446923018,9.22462722643471,9.22878029181728,9.2353563898159,9.25659352010707,
9.37988075886679,9.56244294581531,9.56877658684074,9.57689514520887,9.58298516814561,
9.5873987079952,9.5894219755417,9.59097540622986,9.59263928113368,9.59524623506897,
9.60335540458085,9.65004831824916,9.95823180089409),.UNSPECIFIED.);
#3617=B_SPLINE_CURVE_WITH_KNOTS('',3,(#240936,#240937,#240938,#240939,#240940,
#240941,#240942,#240943,#240944,#240945,#240946,#240947,#240948,#240949,
#240950,#240951,#240952,#240953),.UNSPECIFIED.,.F.,.F.,(4,2,2,2,2,2,2,2,
4),(-35.5088569560286,-34.6739400441337,-33.8390231322389,-33.004106220344,
-32.1691893084491,-31.3342723965543,-30.4993554846594,-29.6644385727646,
-29.225671648849),.UNSPECIFIED.);
#3618=B_SPLINE_CURVE_WITH_KNOTS('',3,(#240955,#240956,#240957,#240958,#240959,
#240960,#240961,#240962,#240963,#240964,#240965,#240966,#240967),
 .UNSPECIFIED.,.F.,.F.,(4,1,1,1,1,1,1,1,1,1,4),(-29.225671648849,-28.9634523400033,
-27.9647126041411,-27.46534273621,-26.9659728682789,-26.4666030003479,-25.9672331324168,
-24.9684933965546,-23.9697536606924,-22.9710139248302,-22.9424868718849),
 .UNSPECIFIED.);
#3619=B_SPLINE_CURVE_WITH_KNOTS('',3,(#240969,#240970,#240971,#240972,#240973,
#240974,#240975,#240976,#240977,#240978,#240979,#240980,#240981,#240982,
#240983,#240984,#240985,#240986,#240987,#240988,#240989,#240990,#240991,
#240992,#240993,#240994,#240995,#240996,#240997,#240998,#240999,#241000,
#241001,#241002,#241003,#241004,#241005,#241006,#241007,#241008,#241009,
#241010,#241011,#241012,#241013,#241014,#241015,#241016,#241017,#241018,
#241019,#241020,#241021,#241022,#241023,#241024,#241025,#241026,#241027,
#241028,#241029,#241030,#241031,#241032,#241033,#241034,#241035,#241036,
#241037,#241038,#241039,#241040,#241041,#241042,#241043,#241044,#241045,
#241046,#241047,#241048,#241049,#241050,#241051,#241052,#241053,#241054,
#241055,#241056,#241057,#241058,#241059,#241060,#241061,#241062,#241063,
#241064,#241065,#241066,#241067,#241068,#241069,#241070,#241071,#241072,
#241073,#241074,#241075,#241076,#241077,#241078,#241079,#241080,#241081,
#241082,#241083,#241084,#241085,#241086,#241087,#241088,#241089,#241090,
#241091,#241092,#241093,#241094,#241095,#241096,#241097,#241098,#241099,
#241100,#241101,#241102,#241103,#241104,#241105,#241106,#241107,#241108,
#241109,#241110,#241111,#241112,#241113,#241114,#241115,#241116,#241117,
#241118,#241119,#241120,#241121,#241122,#241123,#241124,#241125,#241126,
#241127,#241128,#241129,#241130,#241131,#241132,#241133,#241134,#241135,
#241136,#241137,#241138,#241139,#241140,#241141,#241142,#241143,#241144,
#241145,#241146,#241147,#241148,#241149,#241150,#241151,#241152,#241153,
#241154,#241155,#241156,#241157,#241158,#241159,#241160,#241161,#241162,
#241163,#241164,#241165,#241166,#241167,#241168,#241169,#241170,#241171,
#241172,#241173,#241174,#241175,#241176,#241177,#241178,#241179,#241180,
#241181,#241182,#241183,#241184,#241185,#241186,#241187,#241188,#241189,
#241190,#241191,#241192,#241193,#241194,#241195,#241196,#241197,#241198,
#241199,#241200,#241201,#241202,#241203,#241204,#241205,#241206,#241207,
#241208,#241209,#241210,#241211,#241212,#241213,#241214,#241215,#241216,
#241217,#241218,#241219,#241220,#241221,#241222,#241223,#241224),
 .UNSPECIFIED.,.F.,.F.,(4,3,3,3,3,3,3,3,3,3,3,3,3,3,3,3,3,3,3,3,3,3,3,3,
3,3,3,3,3,3,3,3,3,3,3,3,3,3,3,3,3,3,3,3,3,3,3,3,3,3,3,3,3,3,3,3,3,3,3,3,
3,3,3,3,3,3,3,3,3,3,3,3,3,3,3,3,3,3,3,3,3,3,3,3,3,4),(-22.9424863416694,
-22.8626944275539,-22.7830199127632,-22.7035200632596,-22.6241260056474,
-22.544893840185,-22.4716440568991,-22.3972397536512,-22.3228186828177,
-22.2483685713348,-22.1738365360289,-22.0992600957276,-22.0245791489254,
-21.972274188968,-21.8957026457029,-21.8191987531952,-21.7427515587079,
-21.6663501497856,-21.5899836469113,-21.5129274976856,-21.4365901077061,
-21.3602532365099,-21.2839070283929,-21.2063138845711,-21.1298947729273,
-21.0517146130165,-20.9735344531058,-20.8997573618599,-20.826042584007,
-20.752377049305,-20.6787469038082,-20.6051382795967,-20.5315254613912,
-20.4741645851747,-20.3927310551976,-20.311162061333,-20.2270702253107,
-20.1452275199713,-20.0600111186075,-19.9747947172437,-19.8963617729823,
-19.8179985883438,-19.7397003223178,-19.6614810557322,-19.5833117635119,
-19.5052004377325,-19.4754248493126,-19.3990623781506,-19.322683051983,
-19.2462772862505,-19.169802614058,-19.0932905662234,-19.0166962368841,
-18.9760549813815,-18.9006776035735,-18.8253617713139,-18.7500946628522,
-18.6748634889253,-18.5996554849425,-18.5218629550146,-18.4466447799998,
-18.3714099055896,-18.2961467632106,-18.2208437710307,-18.1454515762295,
-18.0700066780304,-17.994463318066,-17.9773152455193,-17.904171434713,-17.831116419771,
-17.7581352635524,-17.6852130990856,-17.6123351139755,-17.5394865363451,
-17.466639133535,-17.393788785599,-17.3209221437638,-17.2480258485698,-17.1750437068389,
-17.1020148043683,-17.0288752490888,-16.9785755096571,-16.884308028905,
-16.7907763237038,-16.6987671708473,-16.6593011630521),.UNSPECIFIED.);
#3620=B_SPLINE_CURVE_WITH_KNOTS('',3,(#241226,#241227,#241228,#241229,#241230,
#241231,#241232,#241233,#241234,#241235,#241236,#241237,#241238),
 .UNSPECIFIED.,.F.,.F.,(4,1,1,1,1,1,1,1,1,1,4),(-16.6593010344898,-15.9798357737949,
-15.4804659058638,-14.9810960379327,-13.9823563020706,-13.4829864341395,
-12.9836165662084,-12.4842466982773,-11.9848768303462,-10.986137094484,
-10.3761157273102),.UNSPECIFIED.);
#3621=B_SPLINE_CURVE_WITH_KNOTS('',3,(#241239,#241240,#241241,#241242,#241243,
#241244,#241245,#241246,#241247,#241248,#241249,#241250,#241251,#241252,
#241253,#241254,#241255,#241256,#241257,#241258,#241259,#241260,#241261,
#241262,#241263,#241264,#241265,#241266,#241267,#241268,#241269,#241270,
#241271,#241272,#241273,#241274,#241275,#241276,#241277,#241278,#241279,
#241280,#241281,#241282,#241283,#241284,#241285,#241286,#241287,#241288,
#241289,#241290,#241291,#241292,#241293,#241294,#241295,#241296,#241297,
#241298,#241299,#241300,#241301,#241302,#241303,#241304,#241305,#241306,
#241307,#241308,#241309,#241310,#241311,#241312,#241313,#241314,#241315,
#241316,#241317,#241318,#241319,#241320,#241321,#241322,#241323,#241324,
#241325,#241326,#241327,#241328,#241329,#241330,#241331,#241332,#241333,
#241334,#241335,#241336,#241337,#241338,#241339,#241340,#241341,#241342,
#241343,#241344,#241345,#241346,#241347,#241348,#241349,#241350,#241351,
#241352,#241353,#241354,#241355,#241356,#241357,#241358,#241359,#241360,
#241361,#241362,#241363,#241364,#241365,#241366,#241367,#241368,#241369,
#241370,#241371,#241372,#241373,#241374,#241375,#241376,#241377,#241378,
#241379,#241380,#241381,#241382,#241383,#241384,#241385,#241386,#241387,
#241388,#241389,#241390,#241391,#241392,#241393,#241394,#241395,#241396,
#241397,#241398,#241399,#241400,#241401,#241402,#241403,#241404,#241405,
#241406,#241407,#241408,#241409,#241410,#241411,#241412,#241413,#241414,
#241415,#241416,#241417,#241418,#241419,#241420,#241421,#241422,#241423,
#241424,#241425,#241426,#241427,#241428,#241429,#241430,#241431,#241432,
#241433,#241434,#241435,#241436,#241437,#241438,#241439,#241440,#241441,
#241442,#241443,#241444,#241445,#241446,#241447,#241448,#241449,#241450,
#241451,#241452,#241453,#241454,#241455,#241456,#241457,#241458,#241459,
#241460,#241461,#241462,#241463,#241464,#241465,#241466,#241467,#241468,
#241469,#241470,#241471,#241472,#241473,#241474,#241475,#241476,#241477,
#241478,#241479,#241480,#241481,#241482,#241483,#241484,#241485,#241486,
#241487,#241488,#241489,#241490,#241491,#241492,#241493,#241494,#241495,
#241496,#241497),.UNSPECIFIED.,.F.,.F.,(4,3,3,3,3,3,3,3,3,3,3,3,3,3,3,3,
3,3,3,3,3,3,3,3,3,3,3,3,3,3,3,3,3,3,3,3,3,3,3,3,3,3,3,3,3,3,3,3,3,3,3,3,
3,3,3,3,3,3,3,3,3,3,3,3,3,3,3,3,3,3,3,3,3,3,3,3,3,3,3,3,3,3,3,3,3,3,4),
(-10.3761155919908,-10.2949452678718,-10.2133195299643,-10.1314591778195,
-10.0492442106362,-9.98739735862183,-9.91280691640399,-9.83830212093258,
-9.76386903770048,-9.68949377967818,-9.61516249815242,-9.54086137401722,
-9.46656620911823,-9.3922708644428,-9.3179628479057,-9.24362966306445,-9.16922387076276,
-9.09477648114597,-9.02023821787867,-8.98865762275964,-8.90768234806484,
-8.82682378339225,-8.74243977625133,-8.66189879816705,-8.58148114198779,
-8.50123776391101,-8.48928775482855,-8.41486188710567,-8.34041906846526,
-8.26594704683611,-8.19139293979972,-8.11679432384346,-8.0420911626425,
-7.98991788689746,-7.91335494065555,-7.83685968219422,-7.76042114153417,
-7.68402838897576,-7.60767052774935,-7.53060898066009,-7.45428011123147,
-7.37795169077802,-7.30161384817896,-7.22400492389304,-7.14759387543904,
-7.06938601323716,-6.99117815103528,-6.91742310966251,-6.84373039576828,
-6.77008692443867,-6.6964787878574,-6.62289214969108,-6.54930120466727,
-6.49180828310419,-6.41019566437374,-6.32844180433781,-6.24444095704664,
-6.16240671975315,-6.07742256746312,-5.9924384151731,-5.91439691633121,
-5.8364239239298,-5.75851331313484,-5.6806752626253,-5.60288259323826,-5.5251391570527,
-5.49306854724201,-5.41619341909099,-5.3392952721306,-5.26236564969255,
-5.1853627112488,-5.10832015885976,-5.03119535881957,-4.99369867931092,
-4.91974063918843,-4.84584806684379,-4.77200666060005,-4.69820215528429,
-4.6225431926378,-4.54875584762045,-4.47496019497449,-4.40114335197271,
-4.32409012750761,-4.25015428000783,-4.17616787206064,-4.10208725131818,
-4.09293045411233),.UNSPECIFIED.);
#3622=B_SPLINE_CURVE_WITH_KNOTS('',3,(#241500,#241501,#241502,#241503,#241504,
#241505,#241506,#241507,#241508,#241509,#241510,#241511,#241512,#241513,
#241514,#241515,#241516,#241517,#241518,#241519,#241520,#241521,#241522,
#241523,#241524,#241525,#241526,#241527,#241528,#241529,#241530,#241531,
#241532,#241533,#241534,#241535,#241536,#241537,#241538,#241539,#241540,
#241541,#241542,#241543,#241544,#241545,#241546,#241547,#241548,#241549,
#241550,#241551,#241552,#241553,#241554,#241555,#241556,#241557,#241558,
#241559,#241560,#241561,#241562,#241563,#241564,#241565,#241566,#241567,
#241568,#241569,#241570,#241571,#241572,#241573,#241574,#241575),
 .UNSPECIFIED.,.F.,.F.,(4,3,3,3,3,3,3,3,3,3,3,3,3,3,3,3,3,3,3,3,3,3,3,3,
3,4),(415.785312438574,415.867774042332,415.950234980212,416.03269527961,
416.115154967923,416.197614072545,416.280072620868,416.362530640282,416.444988158175,
416.531665331254,416.614132116863,416.696597229994,416.779060780301,416.861522877415,
416.943983630947,417.026443150489,417.108901545616,417.191358925887,417.273825311706,
417.35628851333,417.438748969279,417.521207117915,417.603672721927,417.686132600504,
417.768596712241,417.831822927442),.UNSPECIFIED.);
#3623=B_SPLINE_CURVE_WITH_KNOTS('',3,(#241577,#241578,#241579,#241580,#241581,
#241582,#241583,#241584,#241585,#241586,#241587,#241588,#241589,#241590,
#241591,#241592,#241593,#241594,#241595,#241596,#241597,#241598,#241599,
#241600,#241601,#241602,#241603,#241604,#241605,#241606,#241607,#241608,
#241609,#241610,#241611,#241612,#241613,#241614,#241615,#241616,#241617,
#241618,#241619,#241620,#241621,#241622,#241623,#241624,#241625,#241626,
#241627,#241628,#241629,#241630,#241631,#241632,#241633,#241634,#241635,
#241636,#241637,#241638,#241639,#241640,#241641,#241642,#241643,#241644,
#241645,#241646,#241647,#241648,#241649,#241650,#241651,#241652,#241653,
#241654,#241655,#241656,#241657,#241658,#241659,#241660,#241661,#241662,
#241663,#241664),.UNSPECIFIED.,.F.,.F.,(4,3,3,3,3,3,3,3,3,3,3,3,3,3,3,3,
3,3,3,3,3,3,3,3,3,3,3,3,3,4),(417.831822927442,417.936862277953,418.045946800198,
418.102105343728,418.177999062294,418.25379634993,418.329514096796,418.405169105709,
418.480778112549,418.558286483429,418.633868479123,418.709457603604,418.785068942452,
418.864012976737,418.939757279917,419.015558616832,419.091467379743,419.10084507959,
419.178871624819,419.256804913119,419.334660133074,419.412452418422,419.490194251559,
419.567908427544,419.645608569675,419.72330829071,419.801050685512,419.878814189843,
419.956654054945,420.022062012856),.UNSPECIFIED.);
#3624=B_SPLINE_CURVE_WITH_KNOTS('',3,(#241668,#241669,#241670,#241671,#241672,
#241673,#241674,#241675,#241676,#241677,#241678,#241679,#241680,#241681,
#241682,#241683,#241684,#241685,#241686,#241687,#241688,#241689,#241690,
#241691,#241692,#241693,#241694,#241695,#241696,#241697,#241698,#241699,
#241700,#241701,#241702,#241703,#241704),.UNSPECIFIED.,.F.,.F.,(4,3,3,3,
3,3,3,3,3,3,3,3,4),(417.832158352677,417.908872951564,417.985549119717,
418.062212442549,418.138866002223,418.215550066432,418.283790826053,418.368525197013,
418.453296162334,418.538099097117,418.622896862441,418.707669660275,418.783160693984),
 .UNSPECIFIED.);
#3625=B_SPLINE_CURVE_WITH_KNOTS('',3,(#241705,#241706,#241707,#241708,#241709,
#241710,#241711,#241712,#241713,#241714,#241715,#241716,#241717,#241718,
#241719,#241720,#241721,#241722,#241723,#241724,#241725,#241726,#241727,
#241728,#241729,#241730,#241731,#241732,#241733,#241734,#241735,#241736,
#241737,#241738,#241739,#241740,#241741,#241742,#241743,#241744,#241745,
#241746,#241747,#241748,#241749,#241750,#241751,#241752,#241753,#241754,
#241755,#241756,#241757,#241758,#241759,#241760,#241761,#241762,#241763,
#241764,#241765,#241766,#241767,#241768,#241769,#241770,#241771,#241772,
#241773,#241774,#241775,#241776,#241777,#241778,#241779,#241780),
 .UNSPECIFIED.,.F.,.F.,(4,3,3,3,3,3,3,3,3,3,3,3,3,3,3,3,3,3,3,3,3,3,3,3,
3,4),(415.785312438575,415.867774042333,415.950234980212,416.03269527961,
416.115154967923,416.197614072545,416.280072620869,416.362530640283,416.444988158176,
416.531665331255,416.614132116864,416.696597229995,416.779060780302,416.861522877416,
416.943983630948,417.02644315049,417.108901545617,417.191358925888,417.273825311707,
417.356288513331,417.43874896928,417.521207117916,417.603672721928,417.686132600505,
417.768596712242,417.831822927443),.UNSPECIFIED.);
#3626=B_SPLINE_CURVE_WITH_KNOTS('',3,(#241784,#241785,#241786,#241787,#241788,
#241789,#241790,#241791,#241792,#241793),.UNSPECIFIED.,.F.,.F.,(4,2,2,2,
4),(0.911640176190889,0.987592569311299,1.06354496243171,1.13953259867645,
1.21552023492119),.UNSPECIFIED.);
#3627=B_SPLINE_CURVE_WITH_KNOTS('',3,(#241795,#241796,#241797,#241798,#241799,
#241800,#241801,#241802,#241803,#241804,#241805,#241806,#241807,#241808,
#241809,#241810,#241811,#241812),.UNSPECIFIED.,.F.,.F.,(4,2,2,2,2,2,2,2,
4),(0.303880058730296,0.379832451850707,0.455784844971118,0.531772481215855,
0.607760117460592,0.68374775370533,0.759735389950067,0.835687783070478,
0.911640176190889),.UNSPECIFIED.);
#3628=B_SPLINE_CURVE_WITH_KNOTS('',3,(#241813,#241814,#241815,#241816,#241817,
#241818,#241819,#241820,#241821,#241822),.UNSPECIFIED.,.F.,.F.,(4,2,2,2,
4),(1.21552023492119,1.29150787116592,1.36749550741066,1.44344790053107,
1.51940029365148),.UNSPECIFIED.);
#3629=B_SPLINE_CURVE_WITH_KNOTS('',3,(#241826,#241827,#241828,#241829,#241830,
#241831,#241832,#241833,#241834,#241835),.UNSPECIFIED.,.F.,.F.,(4,2,2,2,
4),(0.911640176190889,0.9875925693113,1.06354496243171,1.13953259867645,
1.21552023492119),.UNSPECIFIED.);
#3630=B_SPLINE_CURVE_WITH_KNOTS('',3,(#241837,#241838,#241839,#241840,#241841,
#241842,#241843,#241844,#241845,#241846,#241847,#241848,#241849,#241850,
#241851,#241852,#241853,#241854),.UNSPECIFIED.,.F.,.F.,(4,2,2,2,2,2,2,2,
4),(0.303880058730296,0.379832451850707,0.455784844971118,0.531772481215856,
0.607760117460593,0.68374775370533,0.759735389950067,0.835687783070478,
0.911640176190889),.UNSPECIFIED.);
#3631=B_SPLINE_CURVE_WITH_KNOTS('',3,(#241855,#241856,#241857,#241858,#241859,
#241860,#241861,#241862,#241863,#241864),.UNSPECIFIED.,.F.,.F.,(4,2,2,2,
4),(1.21552023492119,1.29150787116592,1.36749550741066,1.44344790053107,
1.51940029365148),.UNSPECIFIED.);
#3632=B_SPLINE_CURVE_WITH_KNOTS('',3,(#244221,#244222,#244223,#244224,#244225,
#244226,#244227,#244228,#244229,#244230,#244231,#244232,#244233,#244234,
#244235,#244236,#244237,#244238,#244239,#244240,#244241,#244242,#244243,
#244244,#244245,#244246,#244247,#244248,#244249,#244250,#244251,#244252,
#244253,#244254,#244255,#244256,#244257,#244258,#244259,#244260,#244261,
#244262,#244263,#244264,#244265,#244266,#244267,#244268,#244269,#244270,
#244271,#244272,#244273,#244274,#244275,#244276,#244277,#244278,#244279,
#244280,#244281,#244282,#244283,#244284,#244285,#244286,#244287,#244288,
#244289,#244290,#244291,#244292,#244293,#244294,#244295,#244296,#244297,
#244298,#244299,#244300,#244301,#244302,#244303,#244304,#244305,#244306,
#244307,#244308,#244309,#244310,#244311,#244312,#244313,#244314,#244315,
#244316,#244317,#244318,#244319,#244320,#244321,#244322,#244323,#244324,
#244325,#244326,#244327,#244328,#244329,#244330,#244331,#244332),
 .UNSPECIFIED.,.F.,.F.,(4,3,3,3,3,3,3,3,3,3,3,3,3,3,3,3,3,3,3,3,3,3,3,3,
3,3,3,3,3,3,3,3,3,3,3,3,3,4),(0.,0.0614070448361033,0.123000388029202,0.185032164943811,
0.246804846791042,0.29762099995536,0.305065160573997,0.365696235832332,
0.426395934638525,0.449954325750456,0.510788416315891,0.571039794968828,
0.588887633948557,0.599629016443718,0.607143367867252,0.666657656805943,
0.725941079523381,0.784345238663423,0.825028657709657,0.870198948105793,
0.888116253859817,0.894842574301577,0.952699129950469,1.01087631965265,
1.06867337830243,1.12531084762339,1.15700566255158,1.16650423523313,1.1732896249373,
1.18639098087874,1.24342851224962,1.30047172399187,1.34989027008284,1.35816107472823,
1.41436027386202,1.46989172561496,1.52521609801738,1.53373699248706),
 .UNSPECIFIED.);
#3633=B_SPLINE_CURVE_WITH_KNOTS('',3,(#244333,#244334,#244335,#244336,#244337,
#244338,#244339,#244340,#244341,#244342,#244343,#244344,#244345,#244346,
#244347,#244348,#244349,#244350,#244351,#244352,#244353,#244354,#244355,
#244356,#244357,#244358,#244359,#244360,#244361,#244362,#244363,#244364,
#244365,#244366,#244367,#244368,#244369,#244370,#244371,#244372,#244373,
#244374,#244375,#244376,#244377,#244378,#244379,#244380,#244381,#244382,
#244383,#244384,#244385,#244386,#244387,#244388,#244389,#244390,#244391,
#244392,#244393,#244394,#244395,#244396,#244397,#244398,#244399,#244400,
#244401,#244402,#244403,#244404,#244405,#244406,#244407,#244408,#244409,
#244410,#244411,#244412,#244413,#244414,#244415,#244416,#244417,#244418,
#244419,#244420,#244421,#244422,#244423,#244424,#244425,#244426,#244427,
#244428,#244429,#244430,#244431,#244432,#244433,#244434,#244435,#244436,
#244437,#244438,#244439,#244440,#244441),.UNSPECIFIED.,.F.,.F.,(4,3,3,3,
3,3,3,3,3,3,3,3,3,3,3,3,3,3,3,3,3,3,3,3,3,3,3,3,3,3,3,3,3,3,3,3,4),(-1.53373699248736,
-1.48074492111914,-1.42597430957864,-1.38913925044945,-1.35382340313308,
-1.34128955619904,-1.284953556331,-1.22801001408438,-1.17965192531475,-1.16822998829084,
-1.15948917603948,-1.13129383654512,-1.07393261892752,-1.01569915500957,
-0.957333826688686,-0.899346117127988,-0.88926600173786,-0.882672214977545,
-0.823092924494319,-0.767660588719696,-0.7089616547114,-0.649590264476471,
-0.604729941843312,-0.595476697221127,-0.535516633819567,-0.474961154894728,
-0.414241537401714,-0.390466188696484,-0.329920792589955,-0.320304295415085,
-0.310066000769442,-0.297802242924248,-0.237064747296051,-0.175222188325058,
-0.113179732983841,-0.0515754651466952,0.),.UNSPECIFIED.);
#3634=B_SPLINE_CURVE_WITH_KNOTS('',3,(#246798,#246799,#246800,#246801,#246802,
#246803,#246804,#246805,#246806,#246807,#246808,#246809,#246810,#246811,
#246812,#246813,#246814,#246815,#246816,#246817,#246818,#246819,#246820,
#246821,#246822,#246823,#246824,#246825,#246826,#246827,#246828,#246829,
#246830,#246831,#246832,#246833,#246834,#246835,#246836,#246837,#246838,
#246839,#246840,#246841,#246842,#246843,#246844,#246845,#246846,#246847,
#246848,#246849,#246850,#246851,#246852,#246853,#246854,#246855,#246856,
#246857,#246858,#246859,#246860,#246861,#246862,#246863,#246864,#246865,
#246866,#246867,#246868,#246869,#246870,#246871,#246872,#246873,#246874,
#246875,#246876,#246877,#246878,#246879,#246880,#246881,#246882,#246883,
#246884,#246885,#246886,#246887,#246888,#246889,#246890,#246891,#246892,
#246893,#246894,#246895,#246896,#246897,#246898,#246899,#246900,#246901,
#246902,#246903,#246904,#246905,#246906,#246907,#246908,#246909),
 .UNSPECIFIED.,.F.,.F.,(4,3,3,3,3,3,3,3,3,3,3,3,3,3,3,3,3,3,3,3,3,3,3,3,
3,3,3,3,3,3,3,3,3,3,3,3,3,4),(0.,0.0528697059263613,0.107325934667311,0.162613932174076,
0.218756404443508,0.264210921238665,0.272319408785509,0.329151478442084,
0.385983548098659,0.401883732982838,0.459384745316969,0.517029025796296,
0.532644921841707,0.541940475471059,0.54873148511669,0.607427868628937,
0.666405972188839,0.72513755497834,0.764359179612553,0.822926923794845,
0.826792889734822,0.83378661030972,0.892090379582624,0.951786196051419,
1.01185326841918,1.07167856199159,1.10858072873138,1.11899067792923,1.12650652923598,
1.1400296903362,1.20015177784907,1.26114459016009,1.31842175654699,1.32779114489853,
1.38958900979801,1.45163430952323,1.51340906521101,1.52870610664523),
 .UNSPECIFIED.);
#3635=B_SPLINE_CURVE_WITH_KNOTS('',3,(#246910,#246911,#246912,#246913,#246914,
#246915,#246916,#246917,#246918,#246919,#246920,#246921,#246922,#246923,
#246924,#246925,#246926,#246927,#246928,#246929,#246930,#246931,#246932,
#246933,#246934,#246935,#246936,#246937,#246938,#246939,#246940,#246941,
#246942,#246943,#246944,#246945,#246946,#246947,#246948,#246949,#246950,
#246951,#246952,#246953,#246954,#246955,#246956,#246957,#246958,#246959,
#246960,#246961,#246962,#246963,#246964,#246965,#246966,#246967,#246968,
#246969,#246970,#246971,#246972,#246973,#246974,#246975,#246976,#246977,
#246978,#246979,#246980,#246981,#246982,#246983,#246984,#246985,#246986,
#246987,#246988,#246989,#246990,#246991,#246992,#246993,#246994,#246995,
#246996,#246997,#246998,#246999,#247000,#247001,#247002,#247003,#247004,
#247005,#247006,#247007,#247008,#247009,#247010,#247011,#247012,#247013,
#247014,#247015,#247016,#247017,#247018,#247019,#247020,#247021),
 .UNSPECIFIED.,.F.,.F.,(4,3,3,3,3,3,3,3,3,3,3,3,3,3,3,3,3,3,3,3,3,3,3,3,
3,3,3,3,3,3,3,3,3,3,3,3,3,4),(-1.52870610664522,-1.46751956777301,-1.4056757019945,
-1.34361550157725,-1.33048902574182,-1.32126641659285,-1.28497700231689,
-1.22375459820483,-1.16284546373868,-1.14061554159086,-1.12299841173653,
-1.11207164330468,-1.08095498548466,-1.02082441436179,-0.960638340272262,
-0.900842120772938,-0.852426264160289,-0.833346966102961,-0.821061892466914,
-0.762469470452377,-0.707178694322342,-0.648327099083374,-0.589945955835236,
-0.547705085953817,-0.537342986300492,-0.479826857793964,-0.422459929680001,
-0.365926586536747,-0.346773440319137,-0.303426760279258,-0.283727392684925,
-0.271794967690972,-0.261530163865359,-0.205492049525167,-0.149273616827515,
-0.0934113811589646,-0.0385977154833653,-1.01138585612593E-13),
 .UNSPECIFIED.);
#3636=B_SPLINE_CURVE_WITH_KNOTS('',3,(#247043,#247044,#247045,#247046,#247047,
#247048,#247049,#247050,#247051,#247052),.UNSPECIFIED.,.F.,.F.,(4,2,2,2,
4),(0.905379612473188,0.980827373439309,1.05627513440543,1.13172397551817,
1.20717281663092),.UNSPECIFIED.);
#3637=B_SPLINE_CURVE_WITH_KNOTS('',3,(#247054,#247055,#247056,#247057,#247058,
#247059,#247060,#247061,#247062,#247063,#247064,#247065,#247066,#247067,
#247068,#247069,#247070,#247071),.UNSPECIFIED.,.F.,.F.,(4,2,2,2,2,2,2,2,
4),(0.301793204157729,0.377240965123851,0.452688726089972,0.528137567202715,
0.603586408315459,0.679035249428202,0.754484090540945,0.829931851507066,
0.905379612473188),.UNSPECIFIED.);
#3638=B_SPLINE_CURVE_WITH_KNOTS('',3,(#247072,#247073,#247074,#247075,#247076,
#247077,#247078,#247079,#247080,#247081),.UNSPECIFIED.,.F.,.F.,(4,2,2,2,
4),(1.20717281663092,1.28262165774366,1.3580704988564,1.43351825982252,
1.50896602078865),.UNSPECIFIED.);
#3639=B_SPLINE_CURVE_WITH_KNOTS('',3,(#247084,#247085,#247086,#247087,#247088,
#247089,#247090,#247091,#247092,#247093,#247094,#247095,#247096,#247097,
#247098,#247099,#247100,#247101,#247102,#247103,#247104,#247105,#247106,
#247107,#247108,#247109,#247110,#247111,#247112,#247113,#247114,#247115,
#247116,#247117),.UNSPECIFIED.,.T.,.F.,(4,2,2,2,2,2,2,2,2,2,2,2,2,2,2,2,
4),(-1.21552023492118,-1.13953259867645,-1.06354496243171,-0.987592569311299,
-0.911640176190888,-0.835687783070478,-0.759735389950067,-0.683747753705329,
-0.607760117460592,-0.531772481215855,-0.455784844971118,-0.379832451850707,
-0.303880058730296,-0.227927665609885,-0.151975272489474,-0.0759876362447371,
0.),.UNSPECIFIED.);
#3640=B_SPLINE_CURVE_WITH_KNOTS('',3,(#247121,#247122,#247123,#247124,#247125,
#247126,#247127,#247128,#247129,#247130),.UNSPECIFIED.,.F.,.F.,(4,2,2,2,
4),(-0.303880058730296,-0.227927665609886,-0.151975272489475,-0.0759876362447375,
0.),.UNSPECIFIED.);
#3641=B_SPLINE_CURVE_WITH_KNOTS('',3,(#247132,#247133,#247134,#247135,#247136,
#247137,#247138,#247139,#247140,#247141,#247142,#247143,#247144,#247145,
#247146,#247147,#247148,#247149),.UNSPECIFIED.,.F.,.F.,(4,2,2,2,2,2,2,2,
4),(-0.911640176190889,-0.835687783070478,-0.759735389950067,-0.68374775370533,
-0.607760117460593,-0.531772481215855,-0.455784844971118,-0.379832451850707,
-0.303880058730296),.UNSPECIFIED.);
#3642=B_SPLINE_CURVE_WITH_KNOTS('',3,(#247150,#247151,#247152,#247153,#247154,
#247155,#247156,#247157,#247158,#247159),.UNSPECIFIED.,.F.,.F.,(4,2,2,2,
4),(0.,0.0759876362447371,0.151975272489474,0.227927665609885,0.303880058730296),
 .UNSPECIFIED.);
#3643=B_SPLINE_CURVE_WITH_KNOTS('',3,(#247163,#247164,#247165,#247166,#247167,
#247168,#247169,#247170,#247171,#247172),.UNSPECIFIED.,.F.,.F.,(4,2,2,2,
4),(0.905379612473188,0.980827373439309,1.05627513440543,1.13172397551817,
1.20717281663092),.UNSPECIFIED.);
#3644=B_SPLINE_CURVE_WITH_KNOTS('',3,(#247174,#247175,#247176,#247177,#247178,
#247179,#247180,#247181,#247182,#247183,#247184,#247185,#247186,#247187,
#247188,#247189,#247190,#247191),.UNSPECIFIED.,.F.,.F.,(4,2,2,2,2,2,2,2,
4),(0.301793204157729,0.377240965123851,0.452688726089972,0.528137567202715,
0.603586408315459,0.679035249428202,0.754484090540945,0.829931851507066,
0.905379612473188),.UNSPECIFIED.);
#3645=B_SPLINE_CURVE_WITH_KNOTS('',3,(#247192,#247193,#247194,#247195,#247196,
#247197,#247198,#247199,#247200,#247201),.UNSPECIFIED.,.F.,.F.,(4,2,2,2,
4),(1.20717281663092,1.28262165774366,1.3580704988564,1.43351825982252,
1.50896602078865),.UNSPECIFIED.);
#3646=B_SPLINE_CURVE_WITH_KNOTS('',3,(#247356,#247357,#247358,#247359,#247360,
#247361,#247362,#247363,#247364,#247365,#247366,#247367,#247368,#247369,
#247370,#247371,#247372,#247373,#247374,#247375,#247376,#247377,#247378,
#247379,#247380,#247381,#247382,#247383,#247384,#247385,#247386,#247387,
#247388,#247389,#247390,#247391,#247392,#247393,#247394,#247395,#247396,
#247397,#247398,#247399,#247400,#247401,#247402,#247403,#247404,#247405,
#247406,#247407,#247408,#247409,#247410,#247411,#247412,#247413,#247414,
#247415,#247416,#247417,#247418,#247419,#247420,#247421,#247422,#247423,
#247424,#247425,#247426,#247427,#247428,#247429,#247430,#247431,#247432,
#247433,#247434,#247435,#247436,#247437,#247438,#247439,#247440,#247441,
#247442,#247443,#247444,#247445,#247446,#247447,#247448,#247449,#247450,
#247451,#247452,#247453,#247454,#247455,#247456,#247457,#247458,#247459,
#247460,#247461,#247462,#247463,#247464,#247465,#247466,#247467,#247468,
#247469,#247470,#247471,#247472,#247473,#247474,#247475,#247476,#247477,
#247478,#247479,#247480,#247481,#247482,#247483,#247484,#247485,#247486,
#247487,#247488,#247489,#247490,#247491,#247492,#247493,#247494,#247495,
#247496,#247497,#247498,#247499,#247500,#247501,#247502,#247503,#247504,
#247505,#247506,#247507,#247508,#247509,#247510,#247511,#247512,#247513,
#247514,#247515,#247516,#247517,#247518,#247519,#247520,#247521,#247522,
#247523,#247524,#247525,#247526,#247527,#247528,#247529,#247530,#247531,
#247532,#247533,#247534,#247535,#247536,#247537,#247538,#247539,#247540,
#247541,#247542,#247543,#247544,#247545,#247546,#247547,#247548,#247549,
#247550,#247551,#247552,#247553,#247554,#247555,#247556,#247557,#247558,
#247559,#247560,#247561,#247562,#247563,#247564,#247565,#247566,#247567,
#247568,#247569,#247570,#247571,#247572,#247573,#247574,#247575,#247576,
#247577,#247578,#247579,#247580,#247581,#247582,#247583,#247584,#247585,
#247586,#247587,#247588,#247589,#247590,#247591,#247592,#247593,#247594,
#247595,#247596,#247597,#247598,#247599,#247600,#247601,#247602,#247603,
#247604,#247605,#247606,#247607,#247608,#247609,#247610,#247611,#247612,
#247613,#247614,#247615,#247616,#247617,#247618,#247619,#247620,#247621,
#247622,#247623,#247624,#247625,#247626,#247627,#247628,#247629),
 .UNSPECIFIED.,.F.,.F.,(4,3,3,3,3,3,3,3,3,3,3,3,3,3,3,3,3,3,3,3,3,3,3,3,
3,3,3,3,3,3,3,3,3,3,3,3,3,3,3,3,3,3,3,3,3,3,3,3,3,3,3,3,3,3,3,3,3,3,3,3,
3,3,3,3,3,3,3,3,3,3,3,3,3,3,3,3,3,3,3,3,3,3,3,3,3,3,3,3,3,3,3,4),(-2.02747957522558,
-1.99824474635933,-1.99629697858914,-1.96434886453735,-1.94771240967622,
-1.93464992018109,-1.92899254917003,-1.8963788881421,-1.86351124585845,
-1.84194255873285,-1.83673933906724,-1.80209590099024,-1.76903471505845,
-1.73643586541624,-1.71730072608774,-1.70954969143332,-1.70500834289113,
-1.69816558675924,-1.66796497076637,-1.66624311511707,-1.63347199808372,
-1.59881224827677,-1.58364860773623,-1.57740361260911,-1.57281360985668,
-1.53925479883535,-1.50531500590784,-1.47148480017328,-1.45673015640375,
-1.44483082316201,-1.44007092151362,-1.40580982079488,-1.37203186923789,
-1.35619399962815,-1.32417162930309,-1.32246375520252,-1.31137143543089,
-1.30408331014913,-1.27083606559476,-1.23645358594825,-1.20182786580053,
-1.17685917371408,-1.17113655759577,-1.16634083510167,-1.13153658048666,
-1.09665147006904,-1.06221352047721,-1.0321459247931,-1.02687330274833,
-1.00207832910898,-0.970106886116407,-0.968154570621599,-0.933428976642505,
-0.89821340097426,-0.889062877044913,-0.883889592269312,-0.848660796107921,
-0.81299245745828,-0.777358669907495,-0.759631620008249,-0.746573372525805,
-0.741724080509391,-0.705701740199829,-0.670225247749574,-0.635542270713525,
-0.611878481403642,-0.600013081478758,-0.594932488268286,-0.560071350862289,
-0.524344779833904,-0.48796845368674,-0.459087602195323,-0.453607297630247,
-0.448569183216579,-0.412045530179206,-0.375288304735632,-0.339100257750381,
-0.318555603751638,-0.303972630746695,-0.298673006997446,-0.261788714920118,
-0.256921641755406,-0.223059098039412,-0.220857509819622,-0.184147769510166,
-0.161129298321395,-0.154473005979913,-0.149382466658041,-0.11203684999353,
-0.0747139011585263,-0.0373569505792632,0.),.UNSPECIFIED.);
#3647=B_SPLINE_CURVE_WITH_KNOTS('',3,(#247637,#247638,#247639,#247640,#247641,
#247642,#247643,#247644,#247645,#247646,#247647,#247648,#247649,#247650,
#247651,#247652,#247653,#247654,#247655,#247656,#247657,#247658,#247659,
#247660,#247661,#247662,#247663,#247664,#247665,#247666,#247667,#247668,
#247669,#247670,#247671,#247672,#247673,#247674,#247675,#247676,#247677,
#247678,#247679,#247680,#247681,#247682,#247683,#247684,#247685),
 .UNSPECIFIED.,.F.,.F.,(4,3,3,3,3,3,3,3,3,3,3,3,3,3,3,3,4),(-0.379502319520468,
-0.350579328605622,-0.315279094551637,-0.279996782838352,-0.268904605244671,
-0.264656187206077,-0.230575220092214,-0.196553534542628,-0.163007386746561,
-0.142631463403241,-0.131301183629302,-0.126714514936786,-0.0943066959694338,
-0.0623519123392507,-0.0311759561696254,-0.00354365828344034,-6.47742434437623E-14),
 .UNSPECIFIED.);
#3648=B_SPLINE_CURVE_WITH_KNOTS('',3,(#247691,#247692,#247693,#247694,#247695,
#247696,#247697,#247698,#247699,#247700,#247701,#247702,#247703,#247704,
#247705,#247706,#247707,#247708,#247709,#247710,#247711,#247712,#247713,
#247714,#247715,#247716,#247717,#247718,#247719,#247720,#247721,#247722,
#247723,#247724,#247725,#247726,#247727,#247728,#247729,#247730,#247731,
#247732,#247733,#247734,#247735,#247736,#247737,#247738,#247739,#247740,
#247741,#247742,#247743,#247744,#247745,#247746,#247747,#247748,#247749,
#247750,#247751,#247752,#247753,#247754,#247755,#247756,#247757,#247758,
#247759,#247760,#247761,#247762,#247763,#247764,#247765,#247766,#247767,
#247768,#247769,#247770,#247771,#247772,#247773,#247774,#247775,#247776,
#247777,#247778,#247779,#247780,#247781,#247782,#247783,#247784,#247785,
#247786,#247787,#247788,#247789,#247790,#247791,#247792,#247793,#247794,
#247795,#247796,#247797,#247798,#247799,#247800,#247801,#247802,#247803,
#247804,#247805,#247806,#247807,#247808,#247809,#247810,#247811,#247812,
#247813,#247814,#247815,#247816,#247817,#247818,#247819,#247820,#247821,
#247822,#247823,#247824,#247825,#247826,#247827,#247828,#247829,#247830,
#247831,#247832,#247833,#247834,#247835,#247836,#247837,#247838,#247839,
#247840,#247841,#247842,#247843,#247844,#247845,#247846,#247847,#247848,
#247849,#247850,#247851,#247852,#247853,#247854,#247855,#247856,#247857,
#247858,#247859,#247860,#247861,#247862,#247863,#247864,#247865,#247866,
#247867,#247868),.UNSPECIFIED.,.F.,.F.,(4,3,3,3,3,3,3,3,3,3,3,3,3,3,3,3,
3,3,3,3,3,3,3,3,3,3,3,3,3,3,3,3,3,3,3,3,3,3,3,3,3,3,3,3,3,3,3,3,3,3,3,3,
3,3,3,3,3,3,3,4),(10.3763203563934,10.4685630468881,10.5606871195005,10.6530034956873,
10.7449811286153,10.8369328546413,10.9288843331454,11.0214677821077,11.1135450142217,
11.2063815716082,11.2992181289947,11.3925071972562,11.4856743835116,11.5787469958742,
11.671756411856,11.7647335460437,11.8577029439718,11.9506891380896,12.0437754407899,
12.136915160519,12.2302071912169,12.294046588707,12.3870547316618,12.4799363079774,
12.5727190398393,12.6654333606845,12.7581122928936,12.8507807367849,12.943463577407,
13.0362446719034,13.1290776878867,13.2220637037164,13.2888750484192,13.382032516625,
13.4750651584355,13.5680004849872,13.6608690716508,13.7537032475578,13.8465277306185,
13.9393672240905,14.0323049649879,14.125294863567,14.2184365482503,14.2837035081315,
14.3768524935008,14.4698769118861,14.5628042846802,14.6556653589909,14.7484922973377,
14.8413098275675,14.9341426631096,15.0270742465684,15.1200582578556,15.2131945567684,
15.2785319678437,15.3799288349245,15.480948245519,15.5817221848362,15.6821411676171,
15.7079632676789),.UNSPECIFIED.);
#3649=B_SPLINE_CURVE_WITH_KNOTS('',3,(#247871,#247872,#247873,#247874,#247875,
#247876,#247877,#247878,#247879,#247880,#247881,#247882,#247883,#247884,
#247885,#247886,#247887,#247888,#247889,#247890,#247891,#247892,#247893,
#247894,#247895,#247896,#247897,#247898,#247899,#247900,#247901,#247902,
#247903,#247904,#247905,#247906,#247907,#247908,#247909,#247910,#247911,
#247912,#247913,#247914,#247915,#247916,#247917,#247918,#247919,#247920,
#247921,#247922,#247923,#247924,#247925,#247926,#247927,#247928,#247929,
#247930,#247931,#247932,#247933,#247934,#247935,#247936,#247937,#247938,
#247939,#247940,#247941,#247942,#247943,#247944,#247945,#247946,#247947,
#247948,#247949,#247950,#247951,#247952,#247953,#247954,#247955,#247956,
#247957,#247958,#247959,#247960,#247961,#247962,#247963,#247964,#247965,
#247966,#247967,#247968,#247969,#247970,#247971,#247972,#247973,#247974,
#247975,#247976,#247977,#247978,#247979,#247980,#247981,#247982,#247983,
#247984,#247985,#247986,#247987,#247988,#247989,#247990,#247991,#247992,
#247993,#247994,#247995,#247996,#247997,#247998,#247999,#248000,#248001,
#248002,#248003,#248004,#248005,#248006),.UNSPECIFIED.,.F.,.F.,(4,3,3,3,
3,3,3,3,3,3,3,3,3,3,3,3,3,3,3,3,3,3,3,3,3,3,3,3,3,3,3,3,3,3,3,3,3,3,3,3,
3,3,3,3,3,4),(11.6152142277546,11.7105094858962,11.8057504942051,11.9009592767727,
11.9961843748489,12.0914240174434,12.1866982082662,12.2820269791461,12.3774952630653,
12.4730416608485,12.5687527374881,12.609327240686,12.7015323089428,12.7935998055635,
12.8855584723409,12.9774367511178,13.069272429844,13.1610912608687,13.2529189756459,
13.3448411934394,13.436811901971,13.5289383207552,13.6034402536173,13.6967164976112,
13.7898681174578,13.8829224520209,13.975909532746,14.0688618527508,14.1618039767653,
14.2547604544307,14.347813236206,14.4409173688033,14.5341703263431,14.5975532665487,
14.6908501826115,14.784025381243,14.8771061578232,14.9701238940431,15.0631094575167,
15.1560873828664,15.2490821917039,15.3421770033991,15.4353252969455,15.5286254390666,
15.59166627948,15.7079632679489),.UNSPECIFIED.);
#3650=B_SPLINE_CURVE_WITH_KNOTS('',3,(#248011,#248012,#248013,#248014,#248015,
#248016,#248017,#248018,#248019,#248020,#248021,#248022,#248023,#248024,
#248025,#248026,#248027,#248028,#248029,#248030,#248031,#248032,#248033,
#248034,#248035,#248036,#248037,#248038,#248039,#248040,#248041,#248042,
#248043,#248044,#248045,#248046,#248047,#248048,#248049,#248050,#248051,
#248052,#248053,#248054,#248055,#248056,#248057,#248058,#248059,#248060,
#248061,#248062,#248063,#248064,#248065,#248066,#248067,#248068,#248069,
#248070,#248071,#248072,#248073,#248074,#248075,#248076,#248077,#248078,
#248079,#248080,#248081,#248082,#248083,#248084,#248085,#248086,#248087,
#248088,#248089,#248090,#248091,#248092,#248093,#248094,#248095,#248096,
#248097,#248098,#248099,#248100,#248101,#248102,#248103,#248104,#248105,
#248106,#248107,#248108,#248109,#248110,#248111,#248112,#248113,#248114,
#248115,#248116,#248117,#248118,#248119,#248120,#248121,#248122,#248123,
#248124,#248125,#248126,#248127,#248128,#248129,#248130,#248131,#248132,
#248133,#248134,#248135,#248136,#248137,#248138,#248139,#248140,#248141,
#248142,#248143,#248144,#248145,#248146,#248147,#248148,#248149,#248150,
#248151,#248152,#248153,#248154,#248155,#248156,#248157,#248158,#248159,
#248160,#248161,#248162,#248163,#248164,#248165,#248166,#248167,#248168,
#248169,#248170,#248171,#248172,#248173,#248174,#248175,#248176,#248177,
#248178,#248179,#248180,#248181,#248182,#248183,#248184,#248185,#248186,
#248187,#248188,#248189,#248190,#248191,#248192,#248193,#248194,#248195,
#248196,#248197,#248198,#248199,#248200,#248201,#248202,#248203,#248204,
#248205,#248206,#248207,#248208,#248209,#248210,#248211,#248212,#248213,
#248214,#248215,#248216,#248217,#248218,#248219,#248220,#248221,#248222),
 .UNSPECIFIED.,.F.,.F.,(4,2,2,2,2,2,2,2,2,2,2,2,2,2,2,2,2,2,2,2,2,2,2,2,
2,2,2,2,2,2,2,2,2,2,2,2,2,2,2,2,2,2,2,2,2,2,2,2,2,2,2,2,2,2,2,2,2,2,2,2,
2,2,2,2,2,2,2,2,2,2,2,2,2,2,2,2,2,2,2,2,2,2,2,2,2,2,2,2,2,2,2,2,2,2,2,2,
2,2,2,2,2,2,2,2,2,4),(-2.03067141131433,-1.97483616077069,-1.96126379034493,
-1.9545729520835,-1.94924404260476,-1.94319645392332,-1.93277625310953,
-1.87740289985723,-1.82305026185814,-1.80032478632167,-1.7945208337889,
-1.79115358029843,-1.78812090026516,-1.78392753539794,-1.77381178780753,
-1.75897702158424,-1.7089001526612,-1.64844411523202,-1.63800185762131,
-1.63188981306857,-1.62656806293351,-1.61996968429409,-1.60687468288044,
-1.55774436938992,-1.5062960375289,-1.4794697209714,-1.47346806347462,-1.47002274413215,
-1.46701074783559,-1.46296765821994,-1.45374385803148,-1.44064312057713,
-1.40093987702096,-1.33175045168366,-1.31859465808437,-1.3118969602576,
-1.30656687157817,-1.30052251491307,-1.29011952281498,-1.2353637336783,
-1.18209964995384,-1.15782795374053,-1.15191601322357,-1.14852504088423,
-1.14549976297345,-1.14135560017372,-1.13153664036763,-1.11728774956787,
-1.07097628306266,-1.0108018768231,-0.997222669837635,-0.990530695708932,
-0.985201911922215,-0.979155583314236,-0.968740455130169,-0.913538364394459,
-0.85948627542512,-0.836326513585347,-0.830491039560349,-0.827117003020576,
-0.824086653374452,-0.819908246120698,-0.809883740708039,-0.79523042661246,
-0.74635779995978,-0.689476235577065,-0.675858091793467,-0.669157890249812,
-0.663827486230811,-0.657784576464042,-0.647388695842203,-0.592870630599238,
-0.540029374168084,-0.515159180350477,-0.509209357314793,-0.505809712305229,
-0.502784523415308,-0.498652144176125,-0.488915986734228,-0.474831487736167,
-0.429531130530253,-0.368212505709077,-0.354584366405084,-0.347880538645923,
-0.342547713937049,-0.336502488409553,-0.326103555440953,-0.313437790281824,
-0.286206819983695,-0.246066940785503,-0.22982085334851,-0.19472010318304,
-0.188368341713729,-0.184843822290316,-0.181847158005165,-0.177933589784178,
-0.169418797408968,-0.132209288608843,-0.0626984163688823,-0.0379054806914244,
-0.0292672891627416,-0.0236050312665482,-0.0185480379602508,-0.0132366222581118,
-0.00734349179396152,-0.000945049796771579),.UNSPECIFIED.);
#3651=B_SPLINE_CURVE_WITH_KNOTS('',3,(#248223,#248224,#248225,#248226,#248227,
#248228,#248229,#248230,#248231,#248232,#248233,#248234,#248235,#248236,
#248237,#248238,#248239,#248240,#248241,#248242,#248243,#248244,#248245,
#248246,#248247,#248248,#248249,#248250,#248251,#248252,#248253,#248254,
#248255,#248256,#248257,#248258,#248259,#248260,#248261,#248262,#248263,
#248264,#248265,#248266,#248267,#248268,#248269,#248270,#248271,#248272,
#248273,#248274,#248275,#248276,#248277,#248278,#248279,#248280,#248281,
#248282,#248283,#248284,#248285,#248286,#248287,#248288,#248289,#248290,
#248291,#248292,#248293,#248294,#248295,#248296,#248297,#248298,#248299,
#248300,#248301,#248302,#248303,#248304,#248305,#248306,#248307,#248308,
#248309,#248310,#248311,#248312,#248313,#248314,#248315,#248316,#248317,
#248318,#248319,#248320,#248321,#248322,#248323,#248324,#248325,#248326,
#248327,#248328,#248329,#248330,#248331,#248332,#248333,#248334,#248335,
#248336,#248337,#248338,#248339,#248340,#248341,#248342,#248343,#248344,
#248345,#248346,#248347,#248348,#248349,#248350,#248351,#248352,#248353,
#248354,#248355,#248356,#248357,#248358,#248359,#248360,#248361,#248362,
#248363,#248364,#248365,#248366,#248367,#248368,#248369,#248370,#248371,
#248372,#248373,#248374,#248375,#248376,#248377,#248378,#248379,#248380,
#248381,#248382,#248383,#248384,#248385,#248386,#248387,#248388,#248389,
#248390,#248391,#248392,#248393,#248394,#248395,#248396,#248397,#248398,
#248399,#248400,#248401,#248402,#248403,#248404,#248405,#248406,#248407,
#248408,#248409,#248410,#248411,#248412,#248413,#248414,#248415,#248416,
#248417,#248418,#248419,#248420,#248421,#248422,#248423,#248424,#248425,
#248426),.UNSPECIFIED.,.F.,.F.,(4,2,2,2,2,2,2,2,2,2,2,2,2,2,2,2,2,2,2,2,
2,2,2,2,2,2,2,2,2,2,2,2,2,2,2,2,2,2,2,2,2,2,2,2,2,2,2,2,2,2,2,2,2,2,2,2,
2,2,2,2,2,2,2,2,2,2,2,2,2,2,2,2,2,2,2,2,2,2,2,2,2,2,2,2,2,2,2,2,2,2,2,2,
2,2,2,2,2,2,2,2,2,4),(-4.06024336860817,-4.01103093763988,-3.96064562767585,
-3.94732081492831,-3.94061788480259,-3.935264494322,-3.92907883301094,-3.91855996553229,
-3.86473609846212,-3.82694857062176,-3.79988403095017,-3.78944272167838,
-3.78183318208697,-3.77815115892528,-3.77510947605076,-3.77150688488609,
-3.765014522366,-3.72747951411371,-3.64463736684358,-3.6274606957388,-3.62002097883177,
-3.61448358951176,-3.60857175650951,-3.59922385331445,-3.56936521439295,
-3.50038098158607,-3.47725865926583,-3.46333140306374,-3.45851718481015,
-3.45530992008311,-3.45242578797797,-3.44760990687348,-3.4346648612484,
-3.37315107853622,-3.32275563082252,-3.30657769464003,-3.29931747220349,
-3.29381689393851,-3.28785179805557,-3.27821603365067,-3.2460953895588,
-3.18377392033821,-3.14533094013184,-3.13889302885373,-3.13534271705904,
-3.13226981654794,-3.12824642799737,-3.11917154938555,-3.0675409065031,
-3.01860421874562,-2.99912151847835,-2.98455694764226,-2.9775926015785,
-2.97213596036157,-2.9660351025152,-2.95574364731131,-2.91315560025828,
-2.84809684012526,-2.83129167150733,-2.82016906103291,-2.81576275529667,
-2.81264460943735,-2.80924806003364,-2.8035231533907,-2.78254715361318,
-2.72720686048132,-2.67621104046059,-2.6627715404695,-2.65601592257644,
-2.65062146082266,-2.64438840593758,-2.63378554905489,-2.57707604629983,
-2.53584161241735,-2.51354582093467,-2.49996531294343,-2.4952061534296,
-2.49201814165426,-2.4887349503665,-2.48352632456309,-2.46758367680557,
-2.44867351299677,-2.39110641406612,-2.36332328365804,-2.3444113612538,
-2.33670506103856,-2.33113408528844,-2.32533441689205,-2.31646820370616,
-2.2909478684611,-2.2241291642873,-2.18578324295766,-2.17707113585314,-2.17306808095327,
-2.1700026845052,-2.16639021933042,-2.15984851911487,-2.12011471493321,
-2.07743418681169,-2.04509749541676,-2.0308601546849,-2.03077061808298),
 .UNSPECIFIED.);
#3652=B_SPLINE_CURVE_WITH_KNOTS('',3,(#248432,#248433,#248434,#248435),
 .UNSPECIFIED.,.F.,.F.,(4,4),(-0.0010441278808804,-0.000941427881473156),
 .UNSPECIFIED.);
#3653=B_SPLINE_CURVE_WITH_KNOTS('',3,(#248436,#248437,#248438,#248439,#248440,
#248441,#248442,#248443,#248444,#248445,#248446,#248447,#248448,#248449,
#248450,#248451,#248452,#248453,#248454,#248455,#248456,#248457,#248458,
#248459,#248460,#248461,#248462,#248463,#248464,#248465,#248466,#248467,
#248468,#248469,#248470,#248471,#248472,#248473,#248474,#248475,#248476,
#248477,#248478,#248479,#248480,#248481,#248482,#248483,#248484,#248485,
#248486,#248487,#248488,#248489,#248490,#248491,#248492,#248493,#248494,
#248495,#248496,#248497,#248498,#248499,#248500,#248501,#248502,#248503,
#248504,#248505,#248506,#248507,#248508,#248509,#248510,#248511,#248512,
#248513,#248514,#248515,#248516,#248517,#248518,#248519,#248520,#248521,
#248522,#248523,#248524,#248525,#248526,#248527,#248528,#248529,#248530,
#248531,#248532,#248533,#248534,#248535,#248536,#248537,#248538,#248539,
#248540,#248541,#248542,#248543,#248544,#248545,#248546,#248547,#248548,
#248549,#248550,#248551,#248552,#248553,#248554,#248555,#248556,#248557,
#248558,#248559,#248560,#248561,#248562,#248563,#248564,#248565,#248566,
#248567,#248568,#248569,#248570,#248571,#248572,#248573,#248574,#248575,
#248576,#248577,#248578,#248579,#248580,#248581,#248582,#248583,#248584,
#248585,#248586,#248587,#248588,#248589,#248590,#248591,#248592,#248593,
#248594,#248595,#248596,#248597,#248598,#248599,#248600,#248601,#248602,
#248603,#248604,#248605,#248606,#248607,#248608,#248609,#248610,#248611,
#248612,#248613,#248614,#248615,#248616,#248617,#248618,#248619,#248620,
#248621,#248622,#248623,#248624,#248625,#248626,#248627,#248628,#248629,
#248630,#248631,#248632,#248633,#248634,#248635,#248636,#248637,#248638,
#248639,#248640,#248641,#248642,#248643,#248644,#248645),.UNSPECIFIED.,
 .F.,.F.,(4,2,2,2,2,2,2,2,2,2,2,2,2,2,2,2,2,2,2,2,2,2,2,2,2,2,2,2,2,2,2,
2,2,2,2,2,2,2,2,2,2,2,2,2,2,2,2,2,2,2,2,2,2,2,2,2,2,2,2,2,2,2,2,2,2,2,2,
2,2,2,2,2,2,2,2,2,2,2,2,2,2,2,2,2,2,2,2,2,2,2,2,2,2,2,2,2,2,2,2,2,2,2,2,
2,4),(-4.06000788164972,-4.0490529277794,-4.0449969392343,-4.04198931254412,
-4.0391085131236,-4.03576120822483,-4.03004756816254,-4.00845705239628,
-3.95057220832007,-3.89738773129655,-3.88703658997922,-3.88100414033653,
-3.87567366802917,-3.868960948112,-3.85527264034345,-3.79734136389309,-3.74937474976475,
-3.73486201898847,-3.72490988315929,-3.72074368142778,-3.71771539811846,
-3.71433589767344,-3.70847476776611,-3.68494175028851,-3.62034744739797,
-3.57544766813393,-3.56544034148988,-3.5594818588834,-3.55413894643412,
-3.54730386680118,-3.53625234529564,-3.45604119929961,-3.40827534981182,
-3.40173300907305,-3.39820709497625,-3.3952093357214,-3.3913604164974,-3.38327876583815,
-3.31743613076699,-3.26404475569927,-3.24787839060404,-3.24071613607295,
-3.23532956044951,-3.22952866484843,-3.22025402320601,-3.18994975342525,
-3.12705909501232,-3.09004799435543,-3.08155205725997,-3.07763990307568,
-3.07464231721219,-3.0711151154941,-3.06474859461741,-3.02868648049119,
-3.01330103703042,-2.97267755409784,-2.94587933930806,-2.92751860680357,
-2.91999723969625,-2.91455162275291,-2.90887749047995,-2.90019837081972,
-2.87529825664998,-2.80771639459657,-2.77883145846871,-2.76799276510915,
-2.76000176277614,-2.75618425865536,-2.7534802590545,-2.75000509641622,
-2.74387094394008,-2.71442112058098,-2.66487400011064,-2.61207544008875,
-2.60173630994273,-2.59570607247023,-2.59037469025189,-2.58365698577204,
-2.57040160050305,-2.50348730762648,-2.46213296590742,-2.44872968238932,
-2.43934809470799,-2.43527796176851,-2.43226283502322,-2.42883322124811,
-2.42290025906192,-2.39717684288309,-2.34498340605783,-2.29082024311193,
-2.28043698799768,-2.27439725905009,-2.26906717127117,-2.26236404223516,
-2.2487280651821,-2.19013852699169,-2.14261465343102,-2.12110801857514,
-2.11561513428152,-2.11231610431234,-2.10929091289068,-2.10563518934698,
-2.09632790046346,-2.03095948049066,-2.03067141131433),.UNSPECIFIED.);
#3654=B_SPLINE_CURVE_WITH_KNOTS('',3,(#248646,#248647,#248648,#248649,#248650,
#248651,#248652,#248653,#248654,#248655,#248656,#248657,#248658,#248659,
#248660,#248661,#248662,#248663,#248664,#248665,#248666,#248667,#248668,
#248669,#248670,#248671,#248672,#248673,#248674,#248675,#248676,#248677,
#248678,#248679,#248680,#248681,#248682,#248683,#248684,#248685,#248686,
#248687,#248688,#248689,#248690,#248691,#248692,#248693,#248694,#248695,
#248696,#248697,#248698,#248699,#248700,#248701,#248702,#248703,#248704,
#248705,#248706,#248707,#248708,#248709,#248710,#248711,#248712,#248713,
#248714,#248715,#248716,#248717,#248718,#248719,#248720,#248721,#248722,
#248723,#248724,#248725,#248726,#248727,#248728,#248729,#248730,#248731,
#248732,#248733,#248734,#248735,#248736,#248737,#248738,#248739,#248740,
#248741,#248742,#248743,#248744,#248745,#248746,#248747,#248748,#248749,
#248750,#248751,#248752,#248753,#248754,#248755,#248756,#248757,#248758,
#248759,#248760,#248761,#248762,#248763,#248764,#248765,#248766,#248767,
#248768,#248769,#248770,#248771,#248772,#248773,#248774,#248775,#248776,
#248777,#248778,#248779,#248780,#248781,#248782,#248783,#248784,#248785,
#248786,#248787,#248788,#248789,#248790,#248791,#248792,#248793,#248794,
#248795,#248796,#248797,#248798,#248799,#248800,#248801,#248802,#248803,
#248804,#248805,#248806,#248807,#248808,#248809,#248810,#248811,#248812,
#248813,#248814,#248815,#248816,#248817,#248818,#248819,#248820,#248821,
#248822,#248823,#248824,#248825,#248826,#248827,#248828,#248829,#248830,
#248831,#248832,#248833,#248834,#248835,#248836,#248837,#248838,#248839,
#248840,#248841,#248842,#248843,#248844,#248845,#248846,#248847,#248848,
#248849,#248850,#248851,#248852,#248853,#248854,#248855,#248856,#248857,
#248858,#248859),.UNSPECIFIED.,.F.,.F.,(4,2,2,2,2,2,2,2,2,2,2,2,2,2,2,2,
2,2,2,2,2,2,2,2,2,2,2,2,2,2,2,2,2,2,2,2,2,2,2,2,2,2,2,2,2,2,2,2,2,2,2,2,
2,2,2,2,2,2,2,2,2,2,2,2,2,2,2,2,2,2,2,2,2,2,2,2,2,2,2,2,2,2,2,2,2,2,2,2,
2,2,2,2,2,2,2,2,2,2,2,2,2,2,2,2,2,2,4),(-2.03077061808298,-2.02055497819448,
-2.01386303777659,-2.00842532828469,-2.00213243245978,-1.99095608667018,
-1.92975997225102,-1.86395954660106,-1.8557293319733,-1.85181618094681,
-1.84875688259027,-1.84507566739787,-1.83801827904976,-1.82884566161254,
-1.80676468105038,-1.76530813189062,-1.70846287298297,-1.6978618494301,
-1.69163023327029,-1.68623730939664,-1.67948405694965,-1.66605114574467,
-1.6150922529632,-1.55982087497854,-1.53870033584592,-1.53296254066424,
-1.52956302728876,-1.52644289827209,-1.5220375466739,-1.5109407677984,-1.49419603380479,
-1.429686933506,-1.38662833180775,-1.37630269963784,-1.37019030724985,-1.36472854712188,
-1.35776465823026,-1.34322688969505,-1.32379474589797,-1.2687596457538,
-1.26052245996461,-1.21922338157848,-1.21265567901223,-1.20903697087285,
-1.20597159627351,-1.20197542502426,-1.19330310569111,-1.15534308323836,
-1.08958527540451,-1.06290592868058,-1.05391148214489,-1.04808444815133,
-1.04252802674135,-1.0349076162412,-1.016549384954,-0.989897764633018,-0.949224549136618,
-0.934233302568002,-0.897957045876173,-0.891496759073359,-0.887902004265296,
-0.884862730251556,-0.880849158009556,-0.872082002163689,-0.833214053748261,
-0.764905908432308,-0.741089653023172,-0.73244112623066,-0.727261538535745,
-0.721736249545464,-0.714304276331715,-0.697109032219287,-0.614187985446788,
-0.576830332333955,-0.570341550970263,-0.566740208648143,-0.563672321912328,
-0.559650370391542,-0.550838273879347,-0.511537765051561,-0.442001568670601,
-0.41949531311763,-0.411030856338562,-0.405885055828772,-0.400337725289012,
-0.392772447364188,-0.374762442562489,-0.348811754576788,-0.306785831119333,
-0.291464462354942,-0.255653646910567,-0.249205092313655,-0.245612831395585,
-0.242573027726789,-0.238555302358582,-0.230278547225392,-0.221678285298059,
-0.196433013886694,-0.143637614041602,-0.102019751448381,-0.0917804785727679,
-0.0856864194060444,-0.0802207649475341,-0.0732238710232165,-0.0656228449603274,
-0.0464796131870714,-0.00122941941383501),.UNSPECIFIED.);
#3655=B_SPLINE_CURVE_WITH_KNOTS('',3,(#248864,#248865,#248866,#248867,#248868,
#248869,#248870,#248871,#248872,#248873,#248874,#248875,#248876,#248877,
#248878,#248879,#248880,#248881,#248882,#248883,#248884,#248885,#248886,
#248887,#248888,#248889,#248890,#248891,#248892,#248893,#248894,#248895,
#248896,#248897,#248898,#248899,#248900,#248901,#248902,#248903,#248904,
#248905,#248906,#248907,#248908,#248909,#248910,#248911,#248912,#248913,
#248914,#248915,#248916,#248917,#248918,#248919,#248920,#248921,#248922,
#248923,#248924,#248925,#248926,#248927,#248928,#248929,#248930,#248931,
#248932,#248933,#248934,#248935,#248936,#248937,#248938,#248939,#248940,
#248941,#248942,#248943,#248944,#248945,#248946,#248947,#248948,#248949,
#248950,#248951,#248952,#248953,#248954,#248955,#248956,#248957,#248958,
#248959,#248960,#248961,#248962,#248963,#248964,#248965,#248966,#248967,
#248968,#248969,#248970,#248971,#248972,#248973,#248974,#248975,#248976,
#248977,#248978,#248979,#248980,#248981,#248982,#248983,#248984,#248985,
#248986,#248987,#248988,#248989,#248990,#248991,#248992,#248993,#248994,
#248995,#248996,#248997,#248998,#248999,#249000,#249001,#249002,#249003,
#249004,#249005,#249006,#249007,#249008,#249009,#249010,#249011,#249012,
#249013,#249014,#249015,#249016,#249017,#249018,#249019,#249020,#249021,
#249022,#249023,#249024,#249025,#249026,#249027,#249028,#249029,#249030,
#249031,#249032,#249033,#249034,#249035,#249036,#249037,#249038,#249039,
#249040,#249041,#249042,#249043,#249044,#249045,#249046,#249047,#249048,
#249049,#249050,#249051,#249052,#249053,#249054,#249055,#249056,#249057,
#249058,#249059,#249060,#249061,#249062,#249063,#249064,#249065,#249066,
#249067,#249068,#249069,#249070,#249071,#249072,#249073,#249074,#249075,
#249076,#249077,#249078,#249079,#249080,#249081,#249082,#249083,#249084,
#249085,#249086,#249087,#249088,#249089,#249090,#249091,#249092,#249093,
#249094,#249095,#249096,#249097,#249098,#249099,#249100,#249101,#249102,
#249103,#249104,#249105,#249106,#249107,#249108,#249109,#249110,#249111,
#249112,#249113,#249114,#249115,#249116,#249117,#249118,#249119,#249120,
#249121,#249122,#249123,#249124,#249125,#249126,#249127,#249128,#249129,
#249130,#249131,#249132,#249133),.UNSPECIFIED.,.F.,.F.,(4,2,2,2,2,2,2,2,
2,2,2,2,2,2,2,2,2,2,2,2,2,2,2,2,2,2,2,2,2,2,2,2,2,2,2,2,2,2,2,2,2,2,2,2,
2,2,2,2,2,2,2,2,2,2,2,2,2,2,2,2,2,2,2,2,2,2,2,2,2,2,2,2,2,2,2,2,2,2,2,2,
2,2,2,2,2,2,2,2,2,2,2,2,2,2,2,2,2,2,2,2,2,2,2,2,2,2,2,2,2,2,2,2,2,2,2,2,
2,2,2,2,2,2,2,2,2,2,2,2,2,2,2,2,2,2,4),(-2.03049264206931,-2.03028509209775,
-1.98875219490121,-1.92233554041634,-1.9150056198462,-1.91127243186873,
-1.90822889792823,-1.90496847502886,-1.89964943273837,-1.8802164542492,
-1.8407220076384,-1.77124689806472,-1.75810845416528,-1.75141546601951,
-1.74608716725735,-1.74004275566971,-1.72963437144085,-1.67461500588666,
-1.62087088884263,-1.59730235228608,-1.59143874872317,-1.5880588295639,
-1.58503086613491,-1.580866144922,-1.57092206009866,-1.55642651649832,-1.50855832268436,
-1.45055252814352,-1.43688012976825,-1.43017066320431,-1.42484070775506,
-1.41880664012084,-1.40844716940965,-1.35502090777339,-1.30423856273821,
-1.2764873914327,-1.27043833552235,-1.2669826848018,-1.26427582822313,-1.26043080914499,
-1.25229351986786,-1.20600348109814,-1.12725914149006,-1.11604488040571,
-1.10916252113611,-1.10381437563225,-1.09788246207519,-1.08799762548072,
-1.04539533043727,-0.983611048514379,-0.955209749741391,-0.949128074285096,
-0.945665074020801,-0.94295953996442,-0.939125610181733,-0.931046650042836,
-0.897785034127711,-0.837694352007401,-0.801306047639294,-0.791513762783684,
-0.785601674986457,-0.780248747260584,-0.773328260650355,-0.758526466873553,
-0.738520003470266,-0.679712632760192,-0.634659508142356,-0.628165958685232,
-0.624610692810223,-0.621616521564816,-0.617744008496053,-0.609460659659126,
-0.57439713558441,-0.512475341887416,-0.479530541052491,-0.469994403080385,
-0.464137451718634,-0.458769699658739,-0.451736555519746,-0.436308791976659,
-0.376238255739193,-0.316586119393395,-0.307971054437799,-0.304078960075506,
-0.301188401675312,-0.301123873795849,-0.301064179693311,-0.301008824114215,
-0.300957378105432,-0.300909468102858,-0.300864767136011,-0.300822987675755,
-0.300783875764898,-0.300747206180224,-0.300712778420836,-0.300680413357834,
-0.300649950409566,-0.3006212451624,-0.300594167364014,-0.300568599205255,
-0.300544433843571,-0.30052157413206,-0.300485514880745,-0.300449837416733,
-0.300414525371713,-0.300379562987406,-0.300344935070795,-0.300310626980818,
-0.300276624597331,-0.300242914278798,-0.300209482840455,-0.300176317528037,
-0.30014340600438,-0.300110736314592,-0.300078296869722,-0.300046076425722,
-0.300014064062174,-0.299982249171943,-0.299950621429795,-0.299919170791457,
-0.299887887475917,-0.299856761937967,-0.296027465083763,-0.29153099791895,
-0.283725619066497,-0.266253683265083,-0.193692098516056,-0.158540528277937,
-0.148825311640787,-0.142929767128729,-0.137572628360742,-0.130619378177436,
-0.115637592219247,-0.0953077315725876,-0.0010441278808804),
 .UNSPECIFIED.);
#3656=B_SPLINE_CURVE_WITH_KNOTS('',3,(#249135,#249136,#249137,#249138),
 .UNSPECIFIED.,.F.,.F.,(4,4),(-0.00122941941383501,-0.000938193424354277),
 .UNSPECIFIED.);
#3657=B_SPLINE_CURVE_WITH_KNOTS('',3,(#249139,#249140,#249141,#249142,#249143,
#249144,#249145,#249146,#249147,#249148,#249149,#249150,#249151,#249152,
#249153,#249154,#249155,#249156,#249157,#249158,#249159,#249160,#249161,
#249162,#249163,#249164,#249165,#249166,#249167,#249168,#249169,#249170,
#249171,#249172,#249173,#249174,#249175,#249176,#249177,#249178,#249179,
#249180,#249181,#249182,#249183,#249184,#249185,#249186,#249187,#249188,
#249189,#249190,#249191,#249192,#249193,#249194,#249195,#249196,#249197,
#249198,#249199,#249200,#249201,#249202,#249203,#249204,#249205,#249206,
#249207,#249208,#249209,#249210,#249211,#249212,#249213,#249214,#249215,
#249216,#249217,#249218,#249219,#249220,#249221,#249222,#249223,#249224,
#249225,#249226,#249227,#249228,#249229,#249230,#249231,#249232,#249233,
#249234,#249235,#249236,#249237,#249238,#249239,#249240,#249241,#249242,
#249243,#249244,#249245,#249246,#249247,#249248,#249249,#249250,#249251,
#249252,#249253,#249254,#249255,#249256,#249257,#249258,#249259,#249260,
#249261,#249262,#249263,#249264,#249265,#249266,#249267,#249268,#249269,
#249270,#249271,#249272,#249273,#249274,#249275,#249276,#249277,#249278,
#249279,#249280,#249281,#249282,#249283,#249284,#249285,#249286,#249287,
#249288,#249289,#249290,#249291,#249292,#249293,#249294,#249295,#249296,
#249297,#249298,#249299,#249300,#249301,#249302,#249303,#249304,#249305,
#249306,#249307,#249308,#249309,#249310,#249311,#249312,#249313,#249314,
#249315,#249316,#249317,#249318,#249319,#249320,#249321,#249322,#249323,
#249324,#249325,#249326,#249327,#249328,#249329,#249330,#249331,#249332,
#249333,#249334,#249335,#249336,#249337,#249338,#249339,#249340,#249341,
#249342,#249343,#249344,#249345,#249346,#249347,#249348,#249349,#249350,
#249351,#249352,#249353,#249354,#249355,#249356),.UNSPECIFIED.,.F.,.F.,
(4,2,2,2,2,2,2,2,2,2,2,2,2,2,2,2,2,2,2,2,2,2,2,2,2,2,2,2,2,2,2,2,2,2,2,
2,2,2,2,2,2,2,2,2,2,2,2,2,2,2,2,2,2,2,2,2,2,2,2,2,2,2,2,2,2,2,2,2,2,2,2,
2,2,2,2,2,2,2,2,2,2,2,2,2,2,2,2,2,2,2,2,2,2,2,2,2,2,2,2,2,2,2,2,2,2,2,2,
2,4),(-4.05980598877536,-4.00607694824287,-3.99262316888618,-3.98819389244878,
-3.98419843106118,-3.98113306609582,-3.97751367387623,-3.97094319247696,
-3.92930711700454,-3.88698963756487,-3.84933018664956,-3.83338570315429,
-3.82676395598467,-3.82656688810241,-3.82101619355601,-3.81587539147052,
-3.80743801250747,-3.78511797659816,-3.71506698191493,-3.67594244555395,
-3.6671486089494,-3.66312999380678,-3.66009004847685,-3.6564982027568,-3.65005182179954,
-3.61430656934356,-3.59931918298223,-3.5591584577112,-3.53190815441749,
-3.51325375846902,-3.50558646815111,-3.50002153283071,-3.49489904946328,
-3.48656362695737,-3.4649352795161,-3.3945191928488,-3.35490508492687,-3.34606080179038,
-3.34203287068172,-3.33896432985524,-3.33536678876337,-3.32889544246668,
-3.29220181534951,-3.20904506029438,-3.19156318726119,-3.1840836680527,
-3.17855051860901,-3.17338319225235,-3.16480186199284,-3.14147430196178,
-3.07266462457491,-3.03361265844576,-3.02482625938831,-3.02080898143384,
-3.0177415487464,-3.01413703310056,-3.00763397481958,-2.96969300776106,
-2.95759595440448,-2.91906459686975,-2.89047633493205,-2.87117647121552,
-2.86340987786898,-2.85782732523811,-2.85204364559089,-2.84325756130552,
-2.81841727248823,-2.75099216672519,-2.71242933902449,-2.70369341142794,
-2.69968524333211,-2.69661849251979,-2.69300735707348,-2.68647504482617,
-2.64729114378985,-2.63667200591327,-2.58183473035739,-2.56243895268676,
-2.54792014731511,-2.54095927695921,-2.53549723360981,-2.52938176642631,
-2.5190441890201,-2.47580374196751,-2.41139602287648,-2.39465753334207,
-2.38356424368313,-2.37915907781165,-2.37603874914964,-2.37263882131665,
-2.36689960775753,-2.34576350041702,-2.29052543613442,-2.23958511204373,
-2.22615325606372,-2.21939986273756,-2.21400650838632,-2.20777405399907,
-2.19717080610413,-2.14016681058464,-2.09843380492365,-2.07657693387381,
-2.06318069390806,-2.05844680709546,-2.05526477219033,-2.05197516342719,
-2.04673797527469,-2.03055789688724,-2.03039724048114),.UNSPECIFIED.);
#3658=B_SPLINE_CURVE_WITH_KNOTS('',3,(#249361,#249362,#249363,#249364,#249365,
#249366,#249367,#249368,#249369,#249370,#249371,#249372,#249373,#249374,
#249375,#249376,#249377,#249378,#249379,#249380,#249381,#249382,#249383,
#249384,#249385,#249386,#249387,#249388,#249389,#249390,#249391,#249392,
#249393,#249394,#249395,#249396,#249397,#249398,#249399,#249400,#249401,
#249402,#249403,#249404,#249405,#249406,#249407,#249408,#249409,#249410,
#249411,#249412,#249413,#249414,#249415,#249416,#249417,#249418,#249419,
#249420,#249421,#249422,#249423,#249424,#249425,#249426,#249427,#249428,
#249429,#249430,#249431,#249432,#249433,#249434,#249435,#249436,#249437,
#249438,#249439,#249440,#249441,#249442,#249443,#249444,#249445,#249446,
#249447,#249448,#249449,#249450,#249451,#249452,#249453,#249454,#249455,
#249456,#249457,#249458,#249459,#249460,#249461,#249462,#249463,#249464,
#249465,#249466,#249467,#249468,#249469,#249470,#249471,#249472,#249473,
#249474,#249475,#249476,#249477,#249478,#249479,#249480,#249481,#249482,
#249483,#249484,#249485,#249486,#249487,#249488,#249489,#249490,#249491,
#249492,#249493,#249494,#249495,#249496,#249497,#249498,#249499,#249500,
#249501,#249502,#249503,#249504,#249505,#249506,#249507,#249508,#249509,
#249510,#249511,#249512,#249513,#249514,#249515,#249516,#249517,#249518,
#249519,#249520,#249521,#249522,#249523,#249524,#249525,#249526,#249527,
#249528,#249529,#249530,#249531,#249532,#249533,#249534,#249535,#249536,
#249537,#249538,#249539,#249540,#249541,#249542,#249543,#249544,#249545,
#249546,#249547,#249548,#249549,#249550,#249551,#249552,#249553,#249554,
#249555,#249556,#249557,#249558,#249559,#249560,#249561,#249562,#249563,
#249564,#249565,#249566,#249567,#249568,#249569,#249570,#249571,#249572,
#249573,#249574,#249575,#249576),.UNSPECIFIED.,.F.,.F.,(4,2,2,2,2,2,2,2,
2,2,2,2,2,2,2,2,2,2,2,2,2,2,2,2,2,2,2,2,2,2,2,2,2,2,2,2,2,2,2,2,2,2,2,2,
2,2,2,2,2,2,2,2,2,2,2,2,2,2,2,2,2,2,2,2,2,2,2,2,2,2,2,2,2,2,2,2,2,2,2,2,
2,2,2,2,2,2,2,2,2,2,2,2,2,2,2,2,2,2,2,2,2,2,2,2,2,2,2,4),(-4.05954993223484,
-4.03036658012576,-4.01419262699979,-4.00699249478495,-4.00162895680077,
-3.99619715841623,-3.99050054573201,-3.98171219325065,-3.95584406383671,
-3.91403273066718,-3.85485065504541,-3.84330114932281,-3.83888578137858,
-3.83581573520925,-3.83253893153171,-3.82714535955158,-3.80890416335039,
-3.7317456495446,-3.70576206967119,-3.68780535047242,-3.68034835524555,
-3.67491473193295,-3.66922214860698,-3.66045211764536,-3.63474778210027,
-3.5610604622095,-3.53701802348523,-3.52278306230362,-3.51800671128323,
-3.51486456277623,-3.51206834900636,-3.5074748479715,-3.49562123656505,
-3.40600188302322,-3.38255741141337,-3.36589733553926,-3.35865211972301,
-3.35325363156675,-3.34818598108828,-3.33971239162828,-3.31635224500923,
-3.24738524241934,-3.21810866031752,-3.20717967433171,-3.19913833956825,
-3.1953117517077,-3.19260726036538,-3.18913975460874,-3.18303743350277,
-3.15419949137435,-3.10423333769317,-3.05123106355611,-3.04088709210085,
-3.03485668838411,-3.02952674852438,-3.02281299073591,-3.0095724076287,
-2.94236152114677,-2.9012386406383,-2.88787845967648,-2.87851995234048,
-2.87445436931095,-2.87144041807952,-2.86800965219237,-2.86206940361582,
-2.83620509408032,-2.78412689397127,-2.73825444409505,-2.72282544493743,
-2.71579257671991,-2.71042533747878,-2.70456923923268,-2.69503518639547,
-2.66210816528481,-2.60011382638448,-2.56504820208316,-2.55676522229272,
-2.5528929921763,-2.54989910955309,-2.54634423166144,-2.53985158079507,
-2.49465637908026,-2.46118071676765,-2.41319521535961,-2.40024513492375,
-2.39367620166703,-2.38835757318798,-2.38222630339106,-2.37169434992307,
-2.31339905265122,-2.27119761953275,-2.25027629054823,-2.23733446527528,
-2.23272381567628,-2.22961608560992,-2.22640054770862,-2.22128527680501,
-2.20555801949651,-2.18417559509424,-2.16802161501854,-2.1281766541877,
-2.10055041396245,-2.08178712661103,-2.07420436149142,-2.0687484915808,
-2.06309369451128,-2.05450376131022,-2.03049264206931),.UNSPECIFIED.);
#3659=B_SPLINE_CURVE_WITH_KNOTS('',3,(#249578,#249579,#249580,#249581,#249582,
#249583,#249584,#249585,#249586,#249587,#249588,#249589,#249590,#249591,
#249592,#249593,#249594,#249595,#249596,#249597,#249598,#249599,#249600,
#249601,#249602,#249603,#249604,#249605,#249606,#249607,#249608,#249609,
#249610,#249611,#249612,#249613,#249614,#249615,#249616,#249617,#249618,
#249619,#249620,#249621,#249622,#249623,#249624,#249625,#249626,#249627,
#249628,#249629,#249630,#249631,#249632,#249633,#249634,#249635,#249636,
#249637,#249638,#249639,#249640,#249641,#249642,#249643,#249644,#249645,
#249646,#249647,#249648,#249649,#249650,#249651,#249652,#249653,#249654,
#249655,#249656,#249657,#249658,#249659,#249660,#249661,#249662,#249663,
#249664,#249665,#249666,#249667,#249668,#249669,#249670,#249671,#249672,
#249673,#249674,#249675,#249676,#249677,#249678,#249679,#249680,#249681,
#249682,#249683,#249684,#249685,#249686,#249687,#249688,#249689,#249690,
#249691,#249692,#249693,#249694,#249695,#249696,#249697,#249698,#249699,
#249700,#249701,#249702,#249703,#249704,#249705,#249706,#249707,#249708,
#249709,#249710,#249711,#249712,#249713,#249714,#249715,#249716,#249717,
#249718,#249719,#249720,#249721,#249722,#249723,#249724,#249725,#249726,
#249727,#249728,#249729,#249730,#249731,#249732,#249733,#249734,#249735,
#249736,#249737,#249738,#249739,#249740,#249741,#249742,#249743,#249744,
#249745,#249746,#249747,#249748,#249749,#249750,#249751,#249752,#249753,
#249754,#249755,#249756,#249757,#249758,#249759,#249760,#249761,#249762,
#249763,#249764,#249765,#249766,#249767,#249768,#249769,#249770,#249771,
#249772,#249773,#249774,#249775,#249776,#249777,#249778,#249779,#249780,
#249781,#249782,#249783,#249784,#249785,#249786,#249787),.UNSPECIFIED.,
 .F.,.F.,(4,2,2,2,2,2,2,2,2,2,2,2,2,2,2,2,2,2,2,2,2,2,2,2,2,2,2,2,2,2,2,
2,2,2,2,2,2,2,2,2,2,2,2,2,2,2,2,2,2,2,2,2,2,2,2,2,2,2,2,2,2,2,2,2,2,2,2,
2,2,2,2,2,2,2,2,2,2,2,2,2,2,2,2,2,2,2,2,2,2,2,2,2,2,2,2,2,2,2,2,2,2,2,2,
2,4),(-2.03039724048114,-2.00074720145003,-1.92955318715566,-1.90877531220974,
-1.9005693611473,-1.89547004600393,-1.88988559509671,-1.88210828687461,
-1.86273783696658,-1.83399757922457,-1.80792591584767,-1.74910430934334,
-1.74031283091048,-1.73633725382342,-1.73326727718626,-1.72968033876686,
-1.72307513175734,-1.67748815478831,-1.60074575991067,-1.5866040858316,
-1.57960239709298,-1.57447553018519,-1.56891448228211,-1.56126842276891,
-1.54274868794605,-1.51576955837716,-1.47550725754844,-1.46020926457178,
-1.42435803464802,-1.4179085105867,-1.41431605879151,-1.41127632709393,
-1.40725899701873,-1.39847161994737,-1.35940923906924,-1.29055053678822,
-1.26732534227102,-1.25875861906537,-1.25359414387355,-1.24805953717539,
-1.24057010554252,-1.22302703982024,-1.19800073084897,-1.15511790842254,
-1.14566430713688,-1.10348248273422,-1.09690688970201,-1.09328640627237,
-1.09022120327229,-1.08622741373684,-1.07756814365768,-1.03973191826394,
-0.974318161318125,-0.94724249695607,-0.93820557911344,-0.932369533309311,
-0.92681778025944,-0.919224918735237,-0.901040637390619,-0.874740023720986,
-0.833425054458958,-0.818296125792496,-0.782198550243678,-0.775742876228114,
-0.772149138589994,-0.769109736992565,-0.765094687434443,-0.756319259193837,
-0.717370734785041,-0.648833846917342,-0.625266130947525,-0.616651890874911,
-0.611478751113957,-0.605949821022574,-0.598494462199108,-0.581157523267402,
-0.498111001494814,-0.461066589618979,-0.454585969209858,-0.450986495855608,
-0.447918412873352,-0.44389388786784,-0.435067518805084,-0.395627296426434,
-0.325692929561808,-0.303608986675095,-0.295206201158356,-0.290071687656267,
-0.284780187635255,-0.284571792168612,-0.2843685221861,-0.277709813699694,
-0.269679867835412,-0.255927836998914,-0.225289734371868,-0.167052378029449,
-0.13932200039344,-0.133189449986556,-0.129668282391417,-0.126586247529304,
-0.122435349254635,-0.112896430227072,-0.0992675105548785,-0.0569890199881752,
-0.000938351556276533),.UNSPECIFIED.);
#3660=B_SPLINE_CURVE_WITH_KNOTS('',3,(#249788,#249789,#249790,#249791),
 .UNSPECIFIED.,.F.,.F.,(4,4),(-4.05918925078444,-4.05903826007612),
 .UNSPECIFIED.);
#3661=B_SPLINE_CURVE_WITH_KNOTS('',3,(#249797,#249798,#249799,#249800,#249801,
#249802,#249803,#249804,#249805,#249806,#249807,#249808,#249809,#249810,
#249811,#249812,#249813,#249814,#249815,#249816,#249817,#249818,#249819,
#249820,#249821,#249822,#249823,#249824,#249825,#249826,#249827,#249828,
#249829,#249830,#249831,#249832,#249833,#249834,#249835,#249836,#249837,
#249838,#249839,#249840,#249841,#249842,#249843,#249844,#249845,#249846,
#249847,#249848,#249849,#249850,#249851,#249852,#249853,#249854,#249855,
#249856,#249857,#249858,#249859,#249860,#249861,#249862,#249863,#249864,
#249865,#249866,#249867,#249868,#249869,#249870,#249871,#249872,#249873,
#249874,#249875,#249876,#249877,#249878,#249879,#249880,#249881,#249882,
#249883,#249884,#249885,#249886,#249887,#249888,#249889,#249890,#249891,
#249892,#249893,#249894,#249895,#249896,#249897,#249898,#249899,#249900,
#249901,#249902,#249903,#249904,#249905,#249906,#249907,#249908,#249909,
#249910,#249911,#249912,#249913,#249914,#249915,#249916,#249917,#249918,
#249919,#249920,#249921,#249922,#249923,#249924,#249925,#249926,#249927,
#249928,#249929,#249930,#249931,#249932,#249933,#249934,#249935,#249936,
#249937,#249938,#249939,#249940,#249941,#249942,#249943,#249944,#249945,
#249946,#249947,#249948,#249949,#249950,#249951,#249952,#249953,#249954,
#249955,#249956,#249957,#249958,#249959,#249960,#249961,#249962,#249963,
#249964,#249965,#249966,#249967,#249968,#249969,#249970,#249971,#249972,
#249973,#249974,#249975,#249976,#249977,#249978,#249979,#249980,#249981,
#249982,#249983,#249984,#249985,#249986,#249987,#249988,#249989,#249990,
#249991,#249992,#249993,#249994,#249995,#249996,#249997,#249998,#249999,
#250000),.UNSPECIFIED.,.F.,.F.,(4,2,2,2,2,2,2,2,2,2,2,2,2,2,2,2,2,2,2,2,
2,2,2,2,2,2,2,2,2,2,2,2,2,2,2,2,2,2,2,2,2,2,2,2,2,2,2,2,2,2,2,2,2,2,2,2,
2,2,2,2,2,2,2,2,2,2,2,2,2,2,2,2,2,2,2,2,2,2,2,2,2,2,2,2,2,2,2,2,2,2,2,2,
2,2,2,2,2,2,2,2,2,4),(-2.03058182286514,-2.03057883788715,-2.02734955910508,
-2.02424962838836,-2.0196817282572,-2.00706295052508,-1.92652991392495,
-1.88424374243307,-1.87409887347353,-1.86810999671337,-1.86277140426693,
-1.85598513505474,-1.84191311198418,-1.82319953202033,-1.77160036950882,
-1.72068441842592,-1.71181442524786,-1.70781394313925,-1.70479849962751,
-1.70136904563078,-1.69527965431392,-1.66382948213334,-1.6219633310418,
-1.56370323797362,-1.55324667243251,-1.54713124246375,-1.54180953841587,
-1.53521509085457,-1.52214110235948,-1.47318239345337,-1.42211194256197,
-1.394745771292,-1.38871553467375,-1.38526368448638,-1.38255540671093,-1.37870262487658,
-1.37052694392871,-1.33642960942612,-1.33479820517616,-1.27242439971672,
-1.2403371997795,-1.23083284168761,-1.22498193714512,-1.21961087693604,
-1.21256048135147,-1.19704038290564,-1.11290404198645,-1.07403761799863,
-1.06760091513295,-1.06405761398891,-1.06106114262109,-1.05716963570628,
-1.04878820037972,-1.01284740879893,-0.92521322875506,-0.912206363931,-0.905539362378852,
-0.900211937743628,-0.894147196728197,-0.883648945741923,-0.825307225790441,
-0.765904447006784,-0.750026394419319,-0.744891955008563,-0.741671477271295,
-0.73856534074901,-0.733966560722513,-0.721120601361326,-0.700427160583973,
-0.65805882884072,-0.599442475378507,-0.58899180375374,-0.582877392065725,
-0.577555115409264,-0.570958069949591,-0.557872491131587,-0.508825287905069,
-0.457565922127511,-0.430458798873896,-0.424441750222474,-0.420992721558942,
-0.418283655092944,-0.41442582696834,-0.406224355672079,-0.371902409167053,
-0.286343269570671,-0.272142474163376,-0.264434349407393,-0.259008946664582,
-0.254013730620893,-0.247231869556841,-0.229823697111821,-0.204727606379191,
-0.157924025102434,-0.113591846603902,-0.10465810026743,-0.10070885090533,
-0.0976999811722273,-0.0942401188870639,-0.0880095632349312,-0.0530658769367188,
-0.000941250914017463),.UNSPECIFIED.);
#3662=B_SPLINE_CURVE_WITH_KNOTS('',3,(#250001,#250002,#250003,#250004),
 .UNSPECIFIED.,.F.,.F.,(4,4),(-4.05981130541024,-4.05954993223484),
 .UNSPECIFIED.);
#3663=B_SPLINE_CURVE_WITH_KNOTS('',3,(#250005,#250006,#250007,#250008,#250009,
#250010,#250011,#250012,#250013,#250014,#250015,#250016,#250017,#250018,
#250019,#250020,#250021,#250022,#250023,#250024,#250025,#250026,#250027,
#250028,#250029,#250030,#250031,#250032,#250033,#250034,#250035,#250036,
#250037,#250038,#250039,#250040,#250041,#250042,#250043,#250044,#250045,
#250046,#250047,#250048,#250049,#250050,#250051,#250052,#250053,#250054,
#250055,#250056,#250057,#250058,#250059,#250060,#250061,#250062,#250063,
#250064,#250065,#250066,#250067,#250068,#250069,#250070,#250071,#250072,
#250073,#250074,#250075,#250076,#250077,#250078,#250079,#250080,#250081,
#250082,#250083,#250084,#250085,#250086,#250087,#250088,#250089,#250090,
#250091,#250092,#250093,#250094,#250095,#250096,#250097,#250098,#250099,
#250100,#250101,#250102,#250103,#250104,#250105,#250106,#250107,#250108,
#250109,#250110,#250111,#250112,#250113,#250114,#250115,#250116,#250117,
#250118,#250119,#250120,#250121,#250122,#250123,#250124,#250125,#250126,
#250127,#250128,#250129,#250130,#250131,#250132,#250133,#250134,#250135,
#250136,#250137,#250138,#250139,#250140,#250141,#250142,#250143,#250144,
#250145,#250146,#250147,#250148,#250149,#250150,#250151,#250152,#250153,
#250154,#250155,#250156,#250157,#250158,#250159,#250160,#250161,#250162,
#250163,#250164,#250165,#250166,#250167,#250168,#250169,#250170,#250171,
#250172,#250173,#250174,#250175,#250176,#250177,#250178,#250179,#250180,
#250181,#250182,#250183,#250184,#250185,#250186,#250187,#250188,#250189,
#250190,#250191,#250192,#250193,#250194,#250195,#250196,#250197,#250198,
#250199,#250200,#250201,#250202,#250203,#250204,#250205,#250206,#250207,
#250208,#250209,#250210,#250211,#250212,#250213,#250214,#250215,#250216,
#250217,#250218,#250219,#250220),.UNSPECIFIED.,.F.,.F.,(4,2,2,2,2,2,2,2,
2,2,2,2,2,2,2,2,2,2,2,2,2,2,2,2,2,2,2,2,2,2,2,2,2,2,2,2,2,2,2,2,2,2,2,2,
2,2,2,2,2,2,2,2,2,2,2,2,2,2,2,2,2,2,2,2,2,2,2,2,2,2,2,2,2,2,2,2,2,2,2,2,
2,2,2,2,2,2,2,2,2,2,2,2,2,2,2,2,2,2,2,2,2,2,2,2,2,2,2,4),(-4.05903826007612,
-4.04597790593254,-4.03596969919603,-4.03061706022468,-4.02538357229182,
-4.01946089423376,-4.0100089105106,-3.97890101285379,-3.91973109898298,
-3.88072795593345,-3.87194922368865,-3.86793467907121,-3.86489657033458,
-3.86130540175457,-3.85485682694083,-3.81891217513851,-3.80373650436185,
-3.7634255595225,-3.73654524591903,-3.71807505689601,-3.71043917246118,
-3.70488197880268,-3.69975617936139,-3.69139158091948,-3.669549036397,-3.59938693653689,
-3.55986933777879,-3.55103751200743,-3.54701315832674,-3.54394641282536,
-3.54034988069102,-3.53387781926496,-3.49704153653491,-3.48258636613612,
-3.43782139527663,-3.41365940731507,-3.39656053812398,-3.38914644784391,
-3.38362569345179,-3.37844401436517,-3.36977686191264,-3.34580905418622,
-3.27763206358795,-3.23880993600112,-3.23004943670116,-3.22603797690813,
-3.22299989564504,-3.21940598813428,-3.21294613441084,-3.17658908037883,
-3.16172415219348,-3.12107990492158,-3.09445994343133,-3.07611756811528,
-3.06850134013622,-3.06294709424354,-3.05712154920507,-3.04812779651883,
-3.02143747181968,-2.9556777918362,-2.91771689366382,-2.90904618163467,
-2.90505108407026,-2.90198670201232,-2.89836930683124,-2.89180440882497,
-2.85050153536521,-2.84026365344427,-2.79751355728265,-2.77241609077581,
-2.7548368125169,-2.74734299397284,-2.74180906074834,-2.73664797669383,
-2.72809347598532,-2.70494362640618,-2.63600083403551,-2.59690735574113,
-2.5881183752321,-2.58410148739711,-2.58106263162405,-2.57747181151553,
-2.57102668232514,-2.53525606673819,-2.51996684847196,-2.47992193149385,
-2.43910914034588,-2.42919496588705,-2.42317208171714,-2.41769231191204,
-2.41068539927334,-2.39604491955083,-2.31833134451679,-2.27240273667403,
-2.26579265937188,-2.26220532119914,-2.25913641303872,-2.2551640576646,
-2.24638662646662,-2.18847539947846,-2.14205726266983,-2.12433071740527,
-2.11077447323354,-2.10399815802401,-2.09860448757189,-2.09239161765776,
-2.08187029123698,-2.03033138896571),.UNSPECIFIED.);
#3664=B_SPLINE_CURVE_WITH_KNOTS('',3,(#250226,#250227,#250228,#250229),
 .UNSPECIFIED.,.F.,.F.,(4,4),(-0.00120239128176678,-0.000939850288917991),
 .UNSPECIFIED.);
#3665=B_SPLINE_CURVE_WITH_KNOTS('',3,(#250230,#250231,#250232,#250233,#250234,
#250235,#250236,#250237,#250238,#250239,#250240,#250241,#250242,#250243,
#250244,#250245,#250246,#250247,#250248,#250249,#250250,#250251,#250252,
#250253,#250254,#250255,#250256,#250257,#250258,#250259,#250260,#250261,
#250262,#250263,#250264,#250265,#250266,#250267,#250268,#250269,#250270,
#250271,#250272,#250273,#250274,#250275,#250276,#250277,#250278,#250279,
#250280,#250281,#250282,#250283,#250284,#250285,#250286,#250287,#250288,
#250289,#250290,#250291,#250292,#250293,#250294,#250295,#250296,#250297,
#250298,#250299,#250300,#250301,#250302,#250303,#250304,#250305,#250306,
#250307,#250308,#250309,#250310,#250311,#250312,#250313,#250314,#250315,
#250316,#250317,#250318,#250319,#250320,#250321,#250322,#250323,#250324,
#250325,#250326,#250327,#250328,#250329,#250330,#250331,#250332,#250333,
#250334,#250335,#250336,#250337,#250338,#250339,#250340,#250341,#250342,
#250343,#250344,#250345,#250346,#250347,#250348,#250349,#250350,#250351,
#250352,#250353,#250354,#250355,#250356,#250357,#250358,#250359,#250360,
#250361,#250362,#250363,#250364,#250365,#250366,#250367,#250368,#250369,
#250370,#250371,#250372,#250373,#250374,#250375,#250376,#250377,#250378,
#250379,#250380,#250381,#250382,#250383,#250384,#250385,#250386,#250387,
#250388,#250389,#250390,#250391,#250392,#250393,#250394,#250395,#250396,
#250397,#250398,#250399,#250400,#250401,#250402,#250403,#250404,#250405,
#250406,#250407,#250408,#250409,#250410,#250411,#250412,#250413,#250414,
#250415,#250416,#250417,#250418,#250419,#250420,#250421,#250422,#250423,
#250424,#250425,#250426,#250427,#250428,#250429,#250430,#250431,#250432,
#250433,#250434,#250435,#250436,#250437),.UNSPECIFIED.,.F.,.F.,(4,2,2,2,
2,2,2,2,2,2,2,2,2,2,2,2,2,2,2,2,2,2,2,2,2,2,2,2,2,2,2,2,2,2,2,2,2,2,2,2,
2,2,2,2,2,2,2,2,2,2,2,2,2,2,2,2,2,2,2,2,2,2,2,2,2,2,2,2,2,2,2,2,2,2,2,2,
2,2,2,2,2,2,2,2,2,2,2,2,2,2,2,2,2,2,2,2,2,2,2,2,2,2,2,4),(-4.05986983129597,
-3.99181327440633,-3.97381836660338,-3.9621811725854,-3.95775289382385,
-3.95468043230858,-3.95140805248172,-3.9460346986115,-3.92799029834988,
-3.90940947514947,-3.89329789548272,-3.84212150885882,-3.82101482597013,
-3.80571472003521,-3.79927328357972,-3.79910183904098,-3.79892374102063,
-3.79352547522316,-3.78845576058314,-3.77997325987689,-3.75655264393949,
-3.68044103212314,-3.64742986514537,-3.63937985161934,-3.63555127889657,
-3.63284623469308,-3.62937920582057,-3.62328033491758,-3.59452732199759,
-3.53308176206738,-3.49057192432417,-3.48069218534804,-3.47476107857106,
-3.46941223143004,-3.46252696897282,-3.45130358759924,-3.37257162566693,
-3.32622125425776,-3.31807599117137,-3.31422925167252,-3.31152201093935,
-3.30806695226786,-3.30202139916676,-3.27434008220855,-3.22354124241745,
-3.17471672227241,-3.16165999075327,-3.15506943292488,-3.14974858276697,
-3.14363161622601,-3.13316619249863,-3.07580251468088,-3.03392111546468,
-3.0120986782409,-2.99877292745343,-2.99411114289614,-2.99099266179133,
-2.98817604992191,-2.98424765940126,-2.97611561910698,-2.92556713508906,
-2.87379319925098,-2.85504803476284,-2.84095720685412,-2.83416797320819,
-2.82882968284655,-2.82284389100876,-2.81271106153646,-2.77061734359409,
-2.68992108935853,-2.68127722570045,-2.67456505107889,-2.67100327749087,
-2.66800916930287,-2.66414387156366,-2.65590116776557,-2.59063071069953,
-2.53678030992871,-2.52058908646574,-2.5134221389193,-2.50803443852083,
-2.50223462437102,-2.49296674228541,-2.46271973351095,-2.39976947629276,
-2.36273551909781,-2.35423669176454,-2.35032377485134,-2.34732585853618,
-2.34379856546825,-2.33743258685057,-2.30141371420175,-2.28598536984817,
-2.24462880482309,-2.20488724970749,-2.19517231321176,-2.18927608202312,
-2.18391776994754,-2.17707776635535,-2.16575725333272,-2.08787415652705,
-2.0536225374624,-2.03575359151365,-2.03058182286514),.UNSPECIFIED.);
#3666=B_SPLINE_CURVE_WITH_KNOTS('',3,(#250439,#250440,#250441,#250442,#250443,
#250444,#250445,#250446,#250447,#250448,#250449,#250450,#250451,#250452,
#250453,#250454,#250455,#250456,#250457,#250458,#250459,#250460,#250461,
#250462,#250463,#250464,#250465,#250466,#250467,#250468,#250469,#250470,
#250471,#250472,#250473,#250474,#250475,#250476,#250477,#250478,#250479,
#250480,#250481,#250482,#250483,#250484,#250485,#250486,#250487,#250488,
#250489,#250490,#250491,#250492,#250493,#250494,#250495,#250496,#250497,
#250498,#250499,#250500,#250501,#250502,#250503,#250504,#250505,#250506,
#250507,#250508,#250509,#250510,#250511,#250512,#250513,#250514,#250515,
#250516,#250517,#250518,#250519,#250520,#250521,#250522,#250523,#250524,
#250525,#250526,#250527,#250528,#250529,#250530,#250531,#250532,#250533,
#250534,#250535,#250536,#250537,#250538,#250539,#250540,#250541,#250542,
#250543,#250544,#250545,#250546,#250547,#250548,#250549,#250550,#250551,
#250552,#250553,#250554,#250555,#250556,#250557,#250558,#250559,#250560,
#250561,#250562,#250563,#250564,#250565,#250566,#250567,#250568,#250569,
#250570,#250571,#250572,#250573,#250574,#250575,#250576,#250577,#250578,
#250579,#250580,#250581,#250582,#250583,#250584,#250585,#250586,#250587,
#250588,#250589,#250590,#250591,#250592,#250593,#250594,#250595,#250596,
#250597,#250598,#250599,#250600,#250601,#250602,#250603,#250604,#250605,
#250606,#250607,#250608,#250609,#250610,#250611,#250612,#250613,#250614,
#250615,#250616,#250617,#250618,#250619,#250620,#250621,#250622,#250623,
#250624,#250625,#250626,#250627,#250628,#250629,#250630,#250631,#250632,
#250633,#250634,#250635,#250636,#250637,#250638,#250639,#250640,#250641,
#250642,#250643,#250644,#250645,#250646),.UNSPECIFIED.,.F.,.F.,(4,2,2,2,
2,2,2,2,2,2,2,2,2,2,2,2,2,2,2,2,2,2,2,2,2,2,2,2,2,2,2,2,2,2,2,2,2,2,2,2,
2,2,2,2,2,2,2,2,2,2,2,2,2,2,2,2,2,2,2,2,2,2,2,2,2,2,2,2,2,2,2,2,2,2,2,2,
2,2,2,2,2,2,2,2,2,2,2,2,2,2,2,2,2,2,2,2,2,2,2,2,2,2,2,4),(-2.03033138896571,
-2.03004475095578,-1.95484454428,-1.94601038089878,-1.94202760776874,-1.93895741764169,
-1.93537663409036,-1.92879841290792,-1.8846143032805,-1.81171614604089,
-1.79268949781134,-1.78476170987519,-1.77920647951301,-1.77347948396448,
-1.7649627804795,-1.74009358124814,-1.69826083666401,-1.63289842784909,
-1.62462343667328,-1.62070171262031,-1.61764202451515,-1.61396800297792,
-1.60694417349348,-1.59782753623496,-1.57595030953848,-1.53429232050904,
-1.47734666840118,-1.46674781319756,-1.46051730470633,-1.45512524866261,
-1.44837297732227,-1.43494172115453,-1.38398918534725,-1.32872975590806,
-1.30759407527396,-1.30185565666621,-1.29845641745498,-1.29533686327393,
-1.29093303090463,-1.27984412963497,-1.26311514491643,-1.19874296522546,
-1.15554767863535,-1.1452146479462,-1.13910101718287,-1.13364007682602,
-1.12667987756694,-1.11215982968773,-1.09275832860198,-1.03788722598818,
-1.02758849370523,-0.988098826979995,-0.981560793837528,-0.977948841660985,
-0.974882904176124,-0.970877810412923,-0.962155910267061,-0.923719655786981,
-0.856625978313642,-0.831482876241476,-0.822660986141599,-0.816870578928996,
-0.811293956695655,-0.803556039818518,-0.784438908085983,-0.75622722174661,
-0.695409069765793,-0.666413251311307,-0.660218404506081,-0.656683408920067,
-0.653913933282333,-0.649971841764152,-0.641589488048009,-0.606302982244557,
-0.544006199202803,-0.512038662238862,-0.502420107102914,-0.496460052925732,
-0.490960389662207,-0.483695906419145,-0.467485579927382,-0.416390175078096,
-0.353805927807226,-0.342090273559588,-0.337461308658229,-0.334331800474152,
-0.331021305907723,-0.325687262211454,-0.30689904523175,-0.269892876830737,
-0.197168796855664,-0.18530800974726,-0.178235859933491,-0.172746236021974,
-0.166754120374895,-0.156986342178952,-0.118456738247924,-0.0392440781129341,
-0.0223793449285437,-0.0170639986491465,-0.013757500959231,-0.0108711009658924,
-0.00772048351218813,-0.000937009717170368),.UNSPECIFIED.);
#3667=B_SPLINE_CURVE_WITH_KNOTS('',3,(#250647,#250648,#250649,#250650),
 .UNSPECIFIED.,.F.,.F.,(4,4),(-4.06006436020849,-4.05997090679314),
 .UNSPECIFIED.);
#3668=B_SPLINE_CURVE_WITH_KNOTS('',3,(#250655,#250656,#250657,#250658,#250659,
#250660,#250661,#250662,#250663,#250664,#250665,#250666,#250667,#250668,
#250669,#250670,#250671,#250672,#250673,#250674,#250675,#250676,#250677,
#250678,#250679,#250680,#250681,#250682,#250683,#250684,#250685,#250686,
#250687,#250688,#250689,#250690,#250691,#250692,#250693,#250694,#250695,
#250696,#250697,#250698,#250699,#250700,#250701,#250702,#250703,#250704,
#250705,#250706,#250707,#250708,#250709,#250710,#250711,#250712,#250713,
#250714,#250715,#250716,#250717,#250718,#250719,#250720,#250721,#250722,
#250723,#250724,#250725,#250726,#250727,#250728,#250729,#250730,#250731,
#250732,#250733,#250734,#250735,#250736,#250737,#250738,#250739,#250740,
#250741,#250742,#250743,#250744,#250745,#250746,#250747,#250748,#250749,
#250750,#250751,#250752,#250753,#250754,#250755,#250756,#250757,#250758,
#250759,#250760,#250761,#250762,#250763,#250764,#250765,#250766,#250767,
#250768,#250769,#250770,#250771,#250772,#250773,#250774,#250775,#250776,
#250777,#250778,#250779,#250780,#250781,#250782,#250783,#250784,#250785,
#250786,#250787,#250788,#250789,#250790,#250791,#250792,#250793,#250794,
#250795,#250796,#250797,#250798,#250799,#250800,#250801,#250802,#250803,
#250804,#250805,#250806,#250807,#250808,#250809,#250810,#250811,#250812,
#250813,#250814,#250815,#250816,#250817,#250818,#250819,#250820,#250821,
#250822,#250823,#250824,#250825,#250826,#250827,#250828,#250829,#250830,
#250831,#250832,#250833,#250834,#250835,#250836,#250837,#250838,#250839,
#250840,#250841,#250842,#250843,#250844,#250845,#250846,#250847,#250848,
#250849,#250850,#250851,#250852,#250853,#250854),.UNSPECIFIED.,.F.,.F.,
(4,2,2,2,2,2,2,2,2,2,2,2,2,2,2,2,2,2,2,2,2,2,2,2,2,2,2,2,2,2,2,2,2,2,2,
2,2,2,2,2,2,2,2,2,2,2,2,2,2,2,2,2,2,2,2,2,2,2,2,2,2,2,2,2,2,2,2,2,2,2,2,
2,2,2,2,2,2,2,2,2,2,2,2,2,2,2,2,2,2,2,2,2,2,2,2,2,2,2,2,4),(-2.03106147693124,
-2.00135992172458,-1.99213232428103,-1.98634111809768,-1.98095012196117,
-1.97376177043868,-1.95744594529994,-1.9021958880149,-1.83867193668762,
-1.83027464040683,-1.82642168933958,-1.82342321020104,-1.81989931713118,
-1.81336799840513,-1.76637047091445,-1.68518531261994,-1.67425504855372,
-1.6674548948778,-1.66211510973925,-1.65613502393256,-1.64603002272997,
-1.59914584237983,-1.54056139226403,-1.51350426281483,-1.50749041072096,
-1.50404236158618,-1.50133352220733,-1.49747530862163,-1.48927028776032,
-1.45491224318001,-1.3937104958698,-1.35937728697544,-1.34974719630998,
-1.3438693372301,-1.3385063130127,-1.33151387965844,-1.31631860837556,-1.23166592646812,
-1.192835566198,-1.18639987277859,-1.18285687532182,-1.17986049743235,-1.17596890052114,
-1.16758650831909,-1.13163542957096,-1.04402649750223,-1.03101499033604,
-1.02434717787059,-1.01901986369826,-1.01295606600793,-1.00246155857587,
-0.944265486605784,-0.885123604310577,-0.868916151471909,-0.863743230656771,
-0.860514390684492,-0.857414254977698,-0.852845128538774,-0.840217016180446,
-0.75966812682607,-0.717409466946983,-0.707266345854092,-0.701277911584229,
-0.695939353344808,-0.689152635575111,-0.675077842874266,-0.656359318764803,
-0.604733883981113,-0.553860813128715,-0.544987711052228,-0.540986689889558,
-0.537971217104552,-0.534542170901426,-0.528454495061337,-0.497040858222865,
-0.455148512029609,-0.396740512103912,-0.38635845080893,-0.380259808636969,
-0.37493653904309,-0.368319119861507,-0.355127391117024,-0.305216354839862,
-0.252123495642277,-0.227608386494145,-0.221680648527473,-0.218286264343582,
-0.215261657679254,-0.211123763955944,-0.201344435291602,-0.187173611779952,
-0.128413363064338,-0.0891715966497953,-0.0700127803815348,-0.0621605980149476,
-0.0567084908522559,-0.0517050497910303,-0.0462407742051427,-0.0387693217578128,
-0.00120239128176678),.UNSPECIFIED.);
#3669=B_SPLINE_CURVE_WITH_KNOTS('',3,(#250855,#250856,#250857,#250858,#250859,
#250860,#250861,#250862,#250863,#250864,#250865,#250866,#250867,#250868,
#250869,#250870,#250871,#250872,#250873,#250874,#250875,#250876,#250877,
#250878,#250879,#250880,#250881,#250882,#250883,#250884,#250885,#250886,
#250887,#250888,#250889,#250890,#250891,#250892,#250893,#250894,#250895,
#250896,#250897,#250898,#250899,#250900,#250901,#250902,#250903,#250904,
#250905,#250906,#250907,#250908,#250909,#250910,#250911,#250912,#250913,
#250914,#250915,#250916,#250917,#250918,#250919,#250920,#250921,#250922,
#250923,#250924,#250925,#250926,#250927,#250928,#250929,#250930,#250931,
#250932,#250933,#250934,#250935,#250936,#250937,#250938,#250939,#250940,
#250941,#250942,#250943,#250944,#250945,#250946,#250947,#250948,#250949,
#250950,#250951,#250952,#250953,#250954,#250955,#250956,#250957,#250958,
#250959,#250960,#250961,#250962,#250963,#250964,#250965,#250966,#250967,
#250968,#250969,#250970,#250971,#250972,#250973,#250974,#250975,#250976,
#250977,#250978,#250979,#250980,#250981,#250982,#250983,#250984,#250985,
#250986,#250987,#250988,#250989,#250990,#250991,#250992,#250993,#250994,
#250995,#250996,#250997,#250998,#250999,#251000,#251001,#251002,#251003,
#251004,#251005,#251006,#251007,#251008,#251009,#251010,#251011,#251012,
#251013,#251014,#251015,#251016,#251017,#251018,#251019,#251020,#251021,
#251022,#251023,#251024,#251025,#251026,#251027,#251028,#251029,#251030,
#251031,#251032,#251033,#251034,#251035,#251036,#251037,#251038,#251039,
#251040,#251041,#251042,#251043,#251044,#251045,#251046,#251047,#251048,
#251049,#251050,#251051,#251052,#251053,#251054,#251055,#251056,#251057,
#251058,#251059,#251060,#251061,#251062,#251063,#251064,#251065,#251066,
#251067,#251068,#251069,#251070,#251071,#251072,#251073,#251074,#251075,
#251076,#251077,#251078,#251079,#251080,#251081,#251082,#251083,#251084,
#251085,#251086,#251087,#251088,#251089,#251090),.UNSPECIFIED.,.F.,.F.,
(4,2,2,2,2,2,2,2,2,2,2,2,2,2,2,2,2,2,2,2,2,2,2,2,2,2,2,2,2,2,2,2,2,2,2,
2,2,2,2,2,2,2,2,2,2,2,2,2,2,2,2,2,2,2,2,2,2,2,2,2,2,2,2,2,2,2,2,2,2,2,2,
2,2,2,2,2,2,2,2,2,2,2,2,2,2,2,2,2,2,2,2,2,2,2,2,2,2,2,2,2,2,2,2,2,2,2,2,
2,2,2,2,2,2,2,2,2,2,4),(-4.05997090679314,-4.01824280524362,-3.98687820213071,
-3.93567680536283,-3.92221607379754,-3.91545857828971,-3.9100667041386,
-3.90384125480551,-3.89326288243562,-3.83379071636708,-3.79039717101627,
-3.77117286398523,-3.7628048578411,-3.75806037807277,-3.75403284670643,
-3.75399524448692,-3.75395761696416,-3.75391995276596,-3.75388224034229,
-3.75384446795469,-3.75380662366009,-3.75378647922505,-3.75376589425216,
-3.75374484599186,-3.7537233102051,-3.75370126101515,-3.75367867075903,
-3.75365550983221,-3.75363174651384,-3.7536073467604,-3.7535822739617,-3.75059286505521,
-3.7470433830799,-3.74078279001646,-3.71079648955641,-3.65141336595605,
-3.62306408252607,-3.60388024650983,-3.59613295659654,-3.59055530968897,
-3.58476885748337,-3.57596298369627,-3.55094764193656,-3.48371062514029,
-3.44521975611649,-3.43649296022556,-3.43248729823112,-3.42942170645355,
-3.42581103830104,-3.41927747384724,-3.37994071568165,-3.33766468344431,
-3.29242302373853,-3.27971694565728,-3.27310866655302,-3.2682024023488,
-3.26203632357425,-3.25145635106178,-3.20282122787205,-3.12413374002489,
-3.11541562818334,-3.11141132827631,-3.1083455959236,-3.10473336208792,
-3.09819368643935,-3.05858209371425,-3.04847588473183,-3.01012868331876,
-2.98129042974709,-2.96187292823813,-2.95408952134713,-2.94850478413205,
-2.9427274692977,-2.93396807540726,-2.90932289779428,-2.84173855942869,
-2.80312206711941,-2.79438150030537,-2.79037296617171,-2.78730672768343,
-2.78369713235045,-2.77716979624726,-2.73816263352102,-2.72570333766245,
-2.68378172487325,-2.65809912475973,-2.64022262190217,-2.6326793675314,
-2.62713618021893,-2.62128392945349,-2.61216965207654,-2.58437009485361,
-2.50441818312249,-2.486278178061,-2.47452505500896,-2.4700206488298,-2.46688314408606,
-2.46352171999791,-2.45795646743631,-2.43872975858396,-2.3821312035586,
-2.33046750641607,-2.3169495053076,-2.3101798968261,-2.30478592652532,-2.29856646011958,
-2.28801874964022,-2.23447937724356,-2.19680162310392,-2.15729804585081,
-2.15082868883574,-2.14727082617008,-2.14419638797228,-2.14017778601563,
-2.1311439958556,-2.08103734388464,-2.03096923846931,-2.03076530206895),
 .UNSPECIFIED.);
#3670=B_SPLINE_CURVE_WITH_KNOTS('',3,(#251095,#251096,#251097,#251098,#251099,
#251100,#251101,#251102,#251103,#251104,#251105,#251106,#251107,#251108,
#251109,#251110,#251111,#251112,#251113,#251114,#251115,#251116,#251117,
#251118,#251119,#251120,#251121,#251122,#251123,#251124,#251125,#251126,
#251127,#251128,#251129,#251130,#251131,#251132,#251133,#251134,#251135,
#251136,#251137,#251138,#251139,#251140,#251141,#251142,#251143,#251144,
#251145,#251146,#251147,#251148,#251149,#251150,#251151,#251152,#251153,
#251154,#251155,#251156,#251157,#251158,#251159,#251160,#251161,#251162,
#251163,#251164,#251165,#251166,#251167,#251168,#251169,#251170,#251171,
#251172,#251173,#251174,#251175,#251176,#251177,#251178,#251179,#251180,
#251181,#251182,#251183,#251184,#251185,#251186,#251187,#251188,#251189,
#251190,#251191,#251192,#251193,#251194,#251195,#251196,#251197,#251198,
#251199,#251200,#251201,#251202,#251203,#251204,#251205,#251206,#251207,
#251208,#251209,#251210,#251211,#251212,#251213,#251214,#251215,#251216,
#251217,#251218,#251219,#251220,#251221,#251222,#251223,#251224,#251225,
#251226,#251227,#251228,#251229,#251230,#251231,#251232,#251233,#251234,
#251235,#251236,#251237,#251238,#251239,#251240,#251241,#251242,#251243,
#251244,#251245,#251246,#251247,#251248,#251249,#251250,#251251,#251252,
#251253,#251254,#251255,#251256,#251257,#251258,#251259,#251260,#251261,
#251262,#251263,#251264,#251265,#251266,#251267,#251268,#251269,#251270,
#251271,#251272,#251273,#251274,#251275,#251276,#251277,#251278,#251279,
#251280,#251281,#251282,#251283,#251284,#251285,#251286,#251287,#251288,
#251289,#251290,#251291,#251292,#251293,#251294,#251295,#251296,#251297,
#251298,#251299,#251300,#251301,#251302,#251303,#251304,#251305,#251306,
#251307,#251308,#251309,#251310,#251311,#251312,#251313,#251314,#251315,
#251316,#251317,#251318,#251319,#251320,#251321,#251322,#251323,#251324,
#251325,#251326,#251327,#251328,#251329,#251330,#251331,#251332,#251333,
#251334,#251335,#251336,#251337,#251338,#251339,#251340),.UNSPECIFIED.,
 .F.,.F.,(4,2,2,2,2,2,2,2,2,2,2,2,2,2,2,2,2,2,2,2,2,2,2,2,2,2,2,2,2,2,2,
2,2,2,2,2,2,2,2,2,2,2,2,2,2,2,2,2,2,2,2,2,2,2,2,2,2,2,2,2,2,2,2,2,2,2,2,
2,2,2,2,2,2,2,2,2,2,2,2,2,2,2,2,2,2,2,2,2,2,2,2,2,2,2,2,2,2,2,2,2,2,2,2,
2,2,2,2,2,2,2,2,2,2,2,2,2,2,2,2,2,2,2,4),(-4.06053628618758,-4.02160247291763,
-3.99254683092489,-3.94078145176954,-3.92468553480843,-3.91753559308151,
-3.91215105573062,-3.90634545210276,-3.89704809315843,-3.86653684379152,
-3.78910608080314,-3.77122073374161,-3.76329128620407,-3.7587466357091,
-3.75487015269569,-3.75483572564846,-3.75480121917029,-3.75476662258901,
-3.75473192502075,-3.754697115353,-3.75466218222167,-3.75462711399698,-3.75459189877042,
-3.75455652431483,-3.75452097807844,-3.75448524716045,-3.75444931828298,
-3.75441317776608,-3.75437681150701,-3.75435519816047,-3.75433274655183,
-3.75430940496138,-3.75428511718236,-3.75425982198671,-3.75423345255093,
-3.75420593578835,-3.75417719158038,-3.75294776784094,-3.7500168695276,
-3.74634417547087,-3.73758276643462,-3.69013558696533,-3.64883285407783,
-3.62241490918712,-3.60424142541614,-3.59674922343819,-3.59130860400187,
-3.585625339043,-3.57690335952019,-3.55163669929627,-3.4843768107486,-3.44225958124779,
-3.43581928664967,-3.43231475839618,-3.42931372430127,-3.42543356403228,
-3.41719368116728,-3.35301731613637,-3.29682186137098,-3.2815835430287,
-3.27458350148761,-3.26921953700484,-3.26334549319698,-3.25373284769265,
-3.21965731681177,-3.15825003951293,-3.12348786216106,-3.11544659629313,
-3.11161938113049,-3.10891418459862,-3.10544540928693,-3.09934004856297,
-3.07046652620577,-3.02050594871814,-2.96749872286672,-2.95715219177907,
-2.95112017528144,-2.94578873786866,-2.93907299711668,-2.92582818514412,
-2.858612474182,-2.81746821286857,-2.8041025137039,-2.79474045861759,-2.79067357942079,
-2.78765876631303,-2.78422713260338,-2.77828561980348,-2.75242075918696,
-2.70032330346211,-2.65089668712429,-2.63776444477846,-2.63115872055616,
-2.62583636273981,-2.61972945265415,-2.60931038224313,-2.55538901087016,
-2.51760177539952,-2.48137900891173,-2.47296769060748,-2.46907098140614,
-2.46607449701136,-2.46253587019646,-2.45611883001515,-2.41804728966191,
-2.37429494020325,-2.33316458200083,-2.3177041657883,-2.31066454265426,
-2.30529515955346,-2.29943967706842,-2.28991335248799,-2.25711112030618,
-2.19502710042522,-2.15988190638871,-2.15158886887443,-2.14771411582957,
-2.14471929685586,-2.14116451478505,-2.134674937849,-2.09148426352191,-2.03126909524015,
-2.03106147693124),.UNSPECIFIED.);
#3671=B_SPLINE_CURVE_WITH_KNOTS('',3,(#251341,#251342,#251343,#251344,#251345,
#251346,#251347,#251348,#251349,#251350,#251351,#251352,#251353,#251354,
#251355,#251356,#251357,#251358,#251359,#251360,#251361,#251362,#251363,
#251364,#251365,#251366,#251367,#251368,#251369,#251370,#251371,#251372,
#251373,#251374,#251375,#251376,#251377,#251378,#251379,#251380,#251381,
#251382,#251383,#251384,#251385,#251386,#251387,#251388,#251389,#251390,
#251391,#251392,#251393,#251394,#251395,#251396,#251397,#251398,#251399,
#251400,#251401,#251402,#251403,#251404,#251405,#251406,#251407,#251408,
#251409,#251410,#251411,#251412,#251413,#251414,#251415,#251416,#251417,
#251418,#251419,#251420,#251421,#251422,#251423,#251424,#251425,#251426,
#251427,#251428,#251429,#251430,#251431,#251432,#251433,#251434,#251435,
#251436,#251437,#251438,#251439,#251440,#251441,#251442,#251443,#251444,
#251445,#251446,#251447,#251448,#251449,#251450,#251451,#251452,#251453,
#251454,#251455,#251456,#251457,#251458,#251459,#251460,#251461,#251462,
#251463,#251464,#251465,#251466,#251467,#251468,#251469,#251470,#251471,
#251472,#251473,#251474,#251475,#251476,#251477,#251478,#251479,#251480,
#251481,#251482,#251483,#251484,#251485,#251486,#251487,#251488,#251489,
#251490,#251491,#251492,#251493,#251494,#251495,#251496,#251497,#251498,
#251499,#251500,#251501,#251502,#251503,#251504,#251505,#251506,#251507,
#251508,#251509,#251510,#251511,#251512,#251513,#251514,#251515,#251516,
#251517,#251518,#251519,#251520,#251521,#251522,#251523,#251524,#251525,
#251526,#251527,#251528,#251529,#251530,#251531,#251532,#251533,#251534,
#251535,#251536,#251537,#251538,#251539,#251540,#251541,#251542,#251543,
#251544,#251545,#251546,#251547,#251548,#251549,#251550,#251551,#251552,
#251553,#251554),.UNSPECIFIED.,.F.,.F.,(4,2,2,2,2,2,2,2,2,2,2,2,2,2,2,2,
2,2,2,2,2,2,2,2,2,2,2,2,2,2,2,2,2,2,2,2,2,2,2,2,2,2,2,2,2,2,2,2,2,2,2,2,
2,2,2,2,2,2,2,2,2,2,2,2,2,2,2,2,2,2,2,2,2,2,2,2,2,2,2,2,2,2,2,2,2,2,2,2,
2,2,2,2,2,2,2,2,2,2,2,2,2,2,2,2,2,2,4),(-2.03076530206895,-2.00184929588146,
-1.99258929123149,-1.98670572754556,-1.98117633945776,-1.97371943523126,
-1.95637448636026,-1.87331725589928,-1.83628719771598,-1.82980668022375,
-1.82620712525286,-1.82313888050872,-1.81911402297132,-1.81028647188528,
-1.77083697219452,-1.70087529691708,-1.67881462779443,-1.67041501911654,
-1.66528090856498,-1.65972482221062,-1.65210891533437,-1.63378221316232,
-1.60719539209839,-1.56650157569052,-1.55188859119328,-1.51515420245962,
-1.50868151336268,-1.5050837720035,-1.50201538732481,-1.49798814456081,
-1.48914706762221,-1.44956375975893,-1.37921568115567,-1.35756336950096,
-1.34922455609283,-1.34410157751239,-1.33853730561561,-1.33087318092118,
-1.31223862523505,-1.28502532630068,-1.24507245639649,-1.22970943597816,
-1.19399821820182,-1.18755220669189,-1.18396049483954,-1.18092058176281,
-1.1769019610738,-1.16810778724459,-1.12898041849121,-1.05993755001622,
-1.03690774624279,-1.02836846217224,-1.02320898308664,-1.01767101111008,
-1.01016152930244,-0.992496209942183,-0.967229510164724,-0.92459077779838,
-0.912442463860844,-0.873056484973561,-0.866519986760633,-0.862908153379994,
-0.859841837981553,-0.855835627967705,-0.84710899334885,-0.808632034232486,
-0.741428228832295,-0.716398485270796,-0.70758956561908,-0.701801466671953,
-0.696222485495031,-0.688473767196113,-0.669289100914378,-0.640937633221003,
-0.58120570412414,-0.551414956244729,-0.54517950726272,-0.541635124093891,
-0.538866951905071,-0.53493798638522,-0.526626545469866,-0.491976675198403,
-0.430338647544821,-0.397089734202491,-0.38740132175486,-0.381425856999087,
-0.375930390633862,-0.368698565405506,-0.352678299055561,-0.307504527255256,
-0.255236804070178,-0.229874200022828,-0.223812117060306,-0.220341881036696,
-0.217246816139825,-0.21299982827083,-0.202892974719206,-0.188158233440947,
-0.134975612643627,-0.0937919592940926,-0.0729182784888145,-0.0646976557608329,
-0.0595958187794864,-0.0540138417708553,-0.0484812902795008,-0.0409878253526347,
-0.00120365178948661),.UNSPECIFIED.);
#3672=B_SPLINE_CURVE_WITH_KNOTS('',3,(#251560,#251561,#251562,#251563,#251564,
#251565,#251566,#251567,#251568,#251569,#251570,#251571,#251572,#251573,
#251574,#251575,#251576,#251577,#251578,#251579,#251580,#251581,#251582,
#251583,#251584,#251585,#251586,#251587,#251588,#251589,#251590,#251591,
#251592,#251593,#251594,#251595,#251596,#251597,#251598,#251599,#251600,
#251601,#251602,#251603,#251604,#251605,#251606,#251607,#251608,#251609,
#251610,#251611,#251612,#251613,#251614,#251615,#251616,#251617,#251618,
#251619,#251620,#251621,#251622,#251623,#251624,#251625,#251626,#251627,
#251628,#251629,#251630,#251631,#251632,#251633,#251634,#251635,#251636,
#251637,#251638,#251639,#251640,#251641,#251642,#251643,#251644,#251645,
#251646,#251647,#251648,#251649,#251650,#251651,#251652,#251653,#251654,
#251655,#251656,#251657,#251658,#251659,#251660,#251661,#251662,#251663,
#251664,#251665,#251666,#251667,#251668,#251669,#251670,#251671,#251672,
#251673,#251674,#251675,#251676,#251677,#251678,#251679,#251680,#251681,
#251682,#251683,#251684,#251685,#251686,#251687,#251688,#251689,#251690,
#251691,#251692,#251693,#251694,#251695,#251696,#251697,#251698,#251699,
#251700,#251701,#251702,#251703,#251704,#251705,#251706,#251707,#251708,
#251709,#251710,#251711,#251712,#251713,#251714,#251715,#251716,#251717,
#251718,#251719,#251720,#251721,#251722,#251723,#251724,#251725,#251726,
#251727,#251728,#251729,#251730,#251731,#251732,#251733,#251734,#251735,
#251736,#251737,#251738,#251739,#251740,#251741,#251742,#251743,#251744,
#251745,#251746,#251747,#251748,#251749,#251750,#251751,#251752,#251753,
#251754,#251755,#251756,#251757,#251758,#251759,#251760,#251761,#251762,
#251763,#251764,#251765,#251766,#251767,#251768,#251769,#251770,#251771),
 .UNSPECIFIED.,.F.,.F.,(4,2,2,2,2,2,2,2,2,2,2,2,2,2,2,2,2,2,2,2,2,2,2,2,
2,2,2,2,2,2,2,2,2,2,2,2,2,2,2,2,2,2,2,2,2,2,2,2,2,2,2,2,2,2,2,2,2,2,2,2,
2,2,2,2,2,2,2,2,2,2,2,2,2,2,2,2,2,2,2,2,2,2,2,2,2,2,2,2,2,2,2,2,2,2,2,2,
2,2,2,2,2,2,2,2,2,4),(-2.03033861750309,-2.03004890790123,-1.97725081667204,
-1.95233290066491,-1.94638146170912,-1.94298227338569,-1.93995968753833,
-1.93583311881427,-1.92611879437715,-1.91207401587518,-1.86700227208894,
-1.80523064461586,-1.79167148688881,-1.78498347339538,-1.77965514151353,
-1.77360641467977,-1.76317965540511,-1.70755274188579,-1.65276286404174,
-1.63066459086127,-1.62490887902268,-1.62155231165956,-1.61851625743412,
-1.61430025160995,-1.60404417042071,-1.58892856999398,-1.53692741944389,
-1.47892155205336,-1.46846374162645,-1.46234850852207,-1.45702753090137,
-1.45043470166669,-1.43736636858799,-1.38844594465325,-1.33745235432084,
-1.30999013023625,-1.30395549116173,-1.30050290674528,-1.29779518352488,
-1.29394466635748,-1.28577944189796,-1.25176934640795,-1.25037174513555,
-1.18830152261266,-1.15561157943863,-1.14609847045106,-1.14024615927711,
-1.13487642244268,-1.12783158130633,-1.11233983627481,-1.04825006012616,
-0.993049229854669,-0.98419737340668,-0.9802627974761,-0.977255923398685,
-0.97378746893247,-0.967515912823084,-0.931390358403826,-0.871366329964801,
-0.834827211812955,-0.825025294135688,-0.819110637173888,-0.813757444881677,
-0.806839532021044,-0.792054850474799,-0.772079883573775,-0.713470265297573,
-0.668144925532808,-0.661649560864759,-0.658093619007614,-0.655099081845828,
-0.651226357692079,-0.642943488258302,-0.607889369135181,-0.545973991822587,
-0.512998893886362,-0.503459139491535,-0.497600916532352,-0.492232620730419,
-0.485199668798438,-0.46977612463057,-0.402480440426757,-0.350486227358892,
-0.341558546899066,-0.337610477554837,-0.334601871076583,-0.331141559895353,
-0.324908444431098,-0.317048802723645,-0.299397739084804,-0.224787816605238,
-0.19164212908942,-0.182086975423961,-0.176225481514923,-0.170858231737986,
-0.163832526640007,-0.148449489014628,-0.103627271110006,-0.0398122519758747,
-0.0229961981578295,-0.0177548958133785,-0.0145111855666649,-0.0116827105219521,
-0.00861350243500196,-0.00485913010226856,-0.000939989750838741),
 .UNSPECIFIED.);
#3673=B_SPLINE_CURVE_WITH_KNOTS('',3,(#251772,#251773,#251774,#251775),
 .UNSPECIFIED.,.F.,.F.,(4,4),(-4.06063413645091,-4.06053628618758),
 .UNSPECIFIED.);
#3674=B_SPLINE_CURVE_WITH_KNOTS('',3,(#251777,#251778,#251779,#251780),
 .UNSPECIFIED.,.F.,.F.,(4,4),(-0.00120365178948661,-0.000936875117553324),
 .UNSPECIFIED.);
#3675=B_SPLINE_CURVE_WITH_KNOTS('',3,(#251781,#251782,#251783,#251784,#251785,
#251786,#251787,#251788,#251789,#251790,#251791,#251792,#251793,#251794,
#251795,#251796,#251797,#251798,#251799,#251800,#251801,#251802,#251803,
#251804,#251805,#251806,#251807,#251808,#251809,#251810,#251811,#251812,
#251813,#251814,#251815,#251816,#251817,#251818,#251819,#251820,#251821,
#251822,#251823,#251824,#251825,#251826,#251827,#251828,#251829,#251830,
#251831,#251832,#251833,#251834,#251835,#251836,#251837,#251838,#251839,
#251840,#251841,#251842,#251843,#251844,#251845,#251846,#251847,#251848,
#251849,#251850,#251851,#251852,#251853,#251854,#251855,#251856,#251857,
#251858,#251859,#251860,#251861,#251862,#251863,#251864,#251865,#251866,
#251867,#251868,#251869,#251870,#251871,#251872,#251873,#251874,#251875,
#251876,#251877,#251878,#251879,#251880,#251881,#251882,#251883,#251884,
#251885,#251886,#251887,#251888,#251889,#251890,#251891,#251892,#251893,
#251894,#251895,#251896,#251897,#251898,#251899,#251900,#251901,#251902,
#251903,#251904,#251905,#251906,#251907,#251908,#251909,#251910,#251911,
#251912,#251913,#251914,#251915,#251916,#251917,#251918,#251919,#251920,
#251921,#251922,#251923,#251924,#251925,#251926,#251927,#251928,#251929,
#251930,#251931,#251932,#251933,#251934,#251935,#251936,#251937,#251938,
#251939,#251940,#251941,#251942,#251943,#251944,#251945,#251946,#251947,
#251948,#251949,#251950,#251951,#251952,#251953,#251954,#251955,#251956,
#251957,#251958,#251959,#251960,#251961,#251962,#251963,#251964,#251965,
#251966,#251967,#251968,#251969,#251970,#251971,#251972,#251973,#251974,
#251975,#251976,#251977,#251978,#251979,#251980,#251981,#251982,#251983,
#251984,#251985,#251986,#251987,#251988,#251989,#251990,#251991,#251992,
#251993,#251994),.UNSPECIFIED.,.F.,.F.,(4,2,2,2,2,2,2,2,2,2,2,2,2,2,2,2,
2,2,2,2,2,2,2,2,2,2,2,2,2,2,2,2,2,2,2,2,2,2,2,2,2,2,2,2,2,2,2,2,2,2,2,2,
2,2,2,2,2,2,2,2,2,2,2,2,2,2,2,2,2,2,2,2,2,2,2,2,2,2,2,2,2,2,2,2,2,2,2,2,
2,2,2,2,2,2,2,2,2,2,2,2,2,2,2,2,2,2,4),(-4.0599101953197,-4.00818357316239,
-3.96848897714484,-3.96201432955781,-3.95845532602245,-3.95538107042525,
-3.95136419111971,-3.94234021348775,-3.89717804213648,-3.84622964427985,
-3.82426867843098,-3.80844400713818,-3.80187225425212,-3.80168047385455,
-3.80148213101809,-3.80127617050302,-3.80106138751048,-3.79557221084531,
-3.78957591183097,-3.77979061913736,-3.74508986309689,-3.67242665755617,
-3.65487630702403,-3.6433978906777,-3.63893423301607,-3.63580391938678,
-3.63242722551226,-3.62679307065948,-3.60683947182472,-3.55076296493494,
-3.49937562309541,-3.48589036399379,-3.47912688421341,-3.47373312016505,
-3.46750869606673,-3.45693990121842,-3.40237029577803,-3.34793162685712,
-3.33240903194856,-3.32190862337254,-3.31759725465209,-3.31449246914492,
-3.31105274047838,-3.3051308486166,-3.28188038301354,-3.22816291101631,
-3.1821667155189,-3.16612570560703,-3.15889020164693,-3.15339412819943,
-3.14742013006937,-3.13773892965905,-3.10509942446152,-3.04309570937919,
-3.00505178392451,-2.99862448983653,-2.9950754315408,-2.99199906495436,
-2.98796579128925,-2.97884994529758,-2.93043268046179,-2.88612384596614,
-2.86232604214216,-2.84541401282776,-2.83802888568189,-2.83251040561381,
-2.82731687151801,-2.81859609520331,-2.79425091077692,-2.72637372076309,
-2.68765019412936,-2.67889749283997,-2.67488622334734,-2.67181916350439,
-2.66821010365552,-2.66168724177889,-2.62293329508153,-2.61022219244065,
-2.56832925760348,-2.54260605300121,-2.52470807088446,-2.51716035829978,
-2.51161551293607,-2.50646466546695,-2.49797487877086,-2.47529728885201,
-2.40586981792854,-2.3665992951441,-2.35778985391995,-2.35376809743213,
-2.35069994637586,-2.34709777315226,-2.34060632564289,-2.3031502477248,
-2.22029973512685,-2.20315539231148,-2.19573135357903,-2.19020677283707,
-2.18431006848756,-2.17499034084613,-2.14530686814059,-2.07570090638503,
-2.05243480010754,-2.03845346521758,-2.03364385250762,-2.03044625802384,
-2.03042678336567),.UNSPECIFIED.);
#3676=B_SPLINE_CURVE_WITH_KNOTS('',3,(#251999,#252000,#252001,#252002,#252003,
#252004,#252005,#252006,#252007,#252008,#252009,#252010,#252011,#252012,
#252013,#252014,#252015,#252016,#252017,#252018,#252019,#252020,#252021,
#252022,#252023,#252024,#252025,#252026,#252027,#252028,#252029,#252030,
#252031,#252032,#252033,#252034,#252035,#252036,#252037,#252038,#252039,
#252040,#252041,#252042,#252043,#252044,#252045,#252046,#252047,#252048,
#252049,#252050,#252051,#252052,#252053,#252054,#252055,#252056,#252057,
#252058,#252059,#252060,#252061,#252062,#252063,#252064,#252065,#252066,
#252067,#252068,#252069,#252070,#252071,#252072,#252073,#252074,#252075,
#252076,#252077,#252078,#252079,#252080,#252081,#252082,#252083,#252084,
#252085,#252086,#252087,#252088,#252089,#252090,#252091,#252092,#252093,
#252094,#252095,#252096,#252097,#252098,#252099,#252100,#252101,#252102,
#252103,#252104,#252105,#252106,#252107,#252108,#252109,#252110,#252111,
#252112,#252113,#252114,#252115,#252116,#252117,#252118,#252119,#252120,
#252121,#252122,#252123,#252124,#252125,#252126,#252127,#252128,#252129,
#252130,#252131,#252132,#252133,#252134,#252135,#252136,#252137,#252138,
#252139,#252140,#252141,#252142,#252143,#252144,#252145,#252146,#252147,
#252148,#252149,#252150,#252151,#252152,#252153,#252154,#252155,#252156,
#252157,#252158,#252159,#252160,#252161,#252162,#252163,#252164,#252165,
#252166,#252167,#252168,#252169,#252170,#252171,#252172,#252173,#252174,
#252175,#252176,#252177,#252178,#252179,#252180,#252181,#252182,#252183,
#252184,#252185,#252186,#252187,#252188,#252189,#252190,#252191,#252192,
#252193,#252194,#252195,#252196,#252197,#252198,#252199,#252200,#252201,
#252202,#252203,#252204,#252205,#252206,#252207,#252208),.UNSPECIFIED.,
 .F.,.F.,(4,2,2,2,2,2,2,2,2,2,2,2,2,2,2,2,2,2,2,2,2,2,2,2,2,2,2,2,2,2,2,
2,2,2,2,2,2,2,2,2,2,2,2,2,2,2,2,2,2,2,2,2,2,2,2,2,2,2,2,2,2,2,2,2,2,2,2,
2,2,2,2,2,2,2,2,2,2,2,2,2,2,2,2,2,2,2,2,2,2,2,2,2,2,2,2,2,2,2,2,2,2,2,2,
2,4),(-4.05973564480636,-4.04895947790271,-4.0401996181676,-4.03494287370566,
-4.02984221445363,-4.02408797733691,-4.01502963392216,-3.98662498898566,
-3.91606292588892,-3.88075592232649,-3.87451271351252,-3.87105049960473,
-3.86804268648183,-3.86409885109718,-3.85519352795782,-3.80194757114214,
-3.76071477880727,-3.73757296729003,-3.72107073082661,-3.71385122584619,
-3.70845589758762,-3.70267799484809,-3.69351053999885,-3.66414748249112,
-3.60043996107158,-3.56313425657547,-3.55460687359398,-3.55068891719227,
-3.54769079323628,-3.54416756471351,-3.53781894825693,-3.50277854541742,
-3.48715005152721,-3.41477399173373,-3.39927276359096,-3.39222642535054,
-3.38685663215876,-3.38100531866879,-3.37149626296092,-3.33884974262725,
-3.27668657388353,-3.2414624056373,-3.23316111798039,-3.22928509610191,
-3.22629049860871,-3.22273741019866,-3.21625435554874,-3.17432317272511,
-3.11313447998543,-3.09274612496387,-3.07773039038647,-3.07077077691878,
-3.06541255190526,-3.05951962503591,-3.04981764551578,-3.01486792364621,
-2.95021733255777,-2.92754371839915,-2.91386344192486,-2.90915599912745,
-2.90602806947897,-2.90321976458621,-2.89856160549191,-2.88626966783993,
-2.79716247480215,-2.77374822616665,-2.75710342367256,-2.74986023312093,
-2.74446154544535,-2.73939247289678,-2.73091354072414,-2.70751918734115,
-2.63857280271443,-2.60930087306103,-2.59837246371469,-2.59033122126131,
-2.58650437219777,-2.58379957522817,-2.58033150873631,-2.57422782863558,
-2.54627516752496,-2.49572519841999,-2.44242335787306,-2.43206848472008,
-2.42603528544164,-2.42070500237664,-2.41399366075304,-2.40076721530869,
-2.33314605476252,-2.29230350270686,-2.27899342472995,-2.26966085701216,
-2.26559946195761,-2.26258574704101,-2.25915196628226,-2.25319957139567,
-2.22713745340132,-2.17519092797079,-2.1258391842483,-2.11271731757875,
-2.10611425967868,-2.10079285651173,-2.09468573206507,-2.08426306240254,
-2.03033861750309),.UNSPECIFIED.);
#3677=B_SPLINE_CURVE_WITH_KNOTS('',3,(#252210,#252211,#252212,#252213,#252214,
#252215,#252216,#252217,#252218,#252219,#252220,#252221,#252222,#252223,
#252224,#252225,#252226,#252227,#252228,#252229,#252230,#252231,#252232,
#252233,#252234,#252235,#252236,#252237,#252238,#252239,#252240,#252241,
#252242,#252243,#252244,#252245,#252246,#252247,#252248,#252249,#252250,
#252251,#252252,#252253,#252254,#252255,#252256,#252257,#252258,#252259,
#252260,#252261,#252262,#252263,#252264,#252265,#252266,#252267,#252268,
#252269,#252270,#252271,#252272,#252273,#252274,#252275,#252276,#252277,
#252278,#252279,#252280,#252281,#252282,#252283,#252284,#252285,#252286,
#252287,#252288,#252289,#252290,#252291,#252292,#252293,#252294,#252295,
#252296,#252297,#252298,#252299,#252300,#252301,#252302,#252303,#252304,
#252305,#252306,#252307,#252308,#252309,#252310,#252311,#252312,#252313,
#252314,#252315,#252316,#252317,#252318,#252319,#252320,#252321,#252322,
#252323,#252324,#252325,#252326,#252327,#252328,#252329,#252330,#252331,
#252332,#252333,#252334,#252335,#252336,#252337,#252338,#252339,#252340,
#252341,#252342,#252343,#252344,#252345,#252346,#252347,#252348,#252349,
#252350,#252351,#252352,#252353,#252354,#252355,#252356,#252357,#252358,
#252359,#252360,#252361,#252362,#252363,#252364,#252365,#252366,#252367,
#252368,#252369,#252370,#252371,#252372,#252373,#252374,#252375,#252376,
#252377,#252378,#252379,#252380,#252381,#252382,#252383,#252384,#252385,
#252386,#252387,#252388,#252389,#252390,#252391,#252392,#252393,#252394,
#252395,#252396,#252397,#252398,#252399,#252400,#252401,#252402,#252403,
#252404,#252405,#252406,#252407,#252408,#252409,#252410,#252411,#252412,
#252413,#252414,#252415,#252416,#252417),.UNSPECIFIED.,.F.,.F.,(4,2,2,2,
2,2,2,2,2,2,2,2,2,2,2,2,2,2,2,2,2,2,2,2,2,2,2,2,2,2,2,2,2,2,2,2,2,2,2,2,
2,2,2,2,2,2,2,2,2,2,2,2,2,2,2,2,2,2,2,2,2,2,2,2,2,2,2,2,2,2,2,2,2,2,2,2,
2,2,2,2,2,2,2,2,2,2,2,2,2,2,2,2,2,2,2,2,2,2,2,2,2,2,2,4),(-2.03042678336567,
-2.0271766588524,-2.02203124980944,-2.0051458401705,-1.97410420040719,-1.8983471496252,
-1.88194887337186,-1.87527230136595,-1.86971819800052,-1.86398637017759,
-1.85545094609828,-1.83043654458003,-1.78821497586018,-1.72349046635426,
-1.71596304215994,-1.71213856459357,-1.70902427697767,-1.70568624623425,
-1.70022852577767,-1.68007541875722,-1.63825152741114,-1.5725631157043,
-1.55917563529424,-1.55234271647675,-1.54689320264598,-1.540698152456,-1.5299883956653,
-1.4683449077896,-1.40204814226571,-1.39386969266444,-1.38996566352539,
-1.38690615867673,-1.38321588183987,-1.37611615019736,-1.32466139905582,
-1.25050211353124,-1.23875638341914,-1.23171607523815,-1.22623002787951,
-1.2202204108632,-1.21037483196101,-1.17069668646326,-1.1297146466336,-1.11587137626313,
-1.0782767140547,-1.07178171329455,-1.06817893057478,-1.06511112774005,
-1.06109101375384,-1.05228949017911,-1.01309364175023,-0.94385817082773,
-0.92102801903239,-0.912516790358778,-0.907362255448577,-0.901820484742364,
-0.894289602703367,-0.87649425666982,-0.850971087847861,-0.808827028893174,
-0.797495569084699,-0.757256865535598,-0.750703862772229,-0.747088223416008,
-0.744022157884542,-0.740020796105065,-0.731321409729111,-0.693107749684921,
-0.626644615330917,-0.600769395450082,-0.59186221652949,-0.586053248380764,
-0.580486091914029,-0.572805790259274,-0.554067797396065,-0.526642613777348,
-0.486669839395028,-0.471872491107209,-0.435976748210515,-0.429525873433119,
-0.425933042778938,-0.422893238264779,-0.418876134260448,-0.410090469243235,
-0.37104633952984,-0.302257086552059,-0.278958774535814,-0.270381610934319,
-0.265215074810287,-0.259681442734589,-0.259485331154416,-0.252978685183491,
-0.237566609476168,-0.216356965085827,-0.164580847592149,-0.156574339676578,
-0.11506810328143,-0.108497881713489,-0.104878488866221,-0.101812992052141,
-0.0978172403445724,-0.0891479295199449,-0.0512186982902751,-0.000938329146361453),
 .UNSPECIFIED.);
#3678=B_SPLINE_CURVE_WITH_KNOTS('',3,(#252418,#252419,#252420,#252421),
 .UNSPECIFIED.,.F.,.F.,(4,4),(-4.0607596339126,-4.06051280328589),
 .UNSPECIFIED.);
#3679=B_SPLINE_CURVE_WITH_KNOTS('',3,(#252427,#252428,#252429,#252430,#252431,
#252432,#252433,#252434,#252435,#252436,#252437,#252438,#252439,#252440,
#252441,#252442,#252443,#252444,#252445,#252446,#252447,#252448,#252449,
#252450,#252451,#252452,#252453,#252454,#252455,#252456,#252457,#252458,
#252459,#252460,#252461,#252462,#252463,#252464,#252465,#252466,#252467,
#252468,#252469,#252470,#252471,#252472,#252473,#252474,#252475,#252476,
#252477,#252478,#252479,#252480,#252481,#252482,#252483,#252484,#252485,
#252486,#252487,#252488,#252489,#252490,#252491,#252492,#252493,#252494,
#252495,#252496,#252497,#252498,#252499,#252500,#252501,#252502,#252503,
#252504,#252505,#252506,#252507,#252508,#252509,#252510,#252511,#252512,
#252513,#252514,#252515,#252516,#252517,#252518,#252519,#252520,#252521,
#252522,#252523,#252524,#252525,#252526,#252527,#252528,#252529,#252530,
#252531,#252532,#252533,#252534,#252535,#252536,#252537,#252538,#252539,
#252540,#252541,#252542,#252543,#252544,#252545,#252546,#252547,#252548,
#252549,#252550,#252551,#252552,#252553,#252554,#252555,#252556,#252557,
#252558,#252559,#252560,#252561,#252562,#252563,#252564,#252565,#252566,
#252567,#252568,#252569,#252570,#252571,#252572,#252573,#252574,#252575,
#252576,#252577,#252578,#252579,#252580,#252581,#252582,#252583,#252584,
#252585,#252586,#252587,#252588,#252589,#252590,#252591,#252592,#252593,
#252594,#252595,#252596,#252597,#252598,#252599,#252600,#252601,#252602,
#252603,#252604,#252605,#252606,#252607,#252608,#252609,#252610,#252611,
#252612,#252613,#252614,#252615,#252616,#252617,#252618,#252619,#252620,
#252621,#252622,#252623,#252624,#252625,#252626,#252627,#252628,#252629,
#252630,#252631,#252632,#252633,#252634,#252635,#252636),.UNSPECIFIED.,
 .F.,.F.,(4,2,2,2,2,2,2,2,2,2,2,2,2,2,2,2,2,2,2,2,2,2,2,2,2,2,2,2,2,2,2,
2,2,2,2,2,2,2,2,2,2,2,2,2,2,2,2,2,2,2,2,2,2,2,2,2,2,2,2,2,2,2,2,2,2,2,2,
2,2,2,2,2,2,2,2,2,2,2,2,2,2,2,2,2,2,2,2,2,2,2,2,2,2,2,2,2,2,2,2,2,2,2,2,
2,4),(-2.03032387244298,-1.985810352188,-1.92354028603898,-1.90998856667296,
-1.90330182203253,-1.8979734141344,-1.89192343591164,-1.88149153535254,
-1.82569392074198,-1.77061721719319,-1.74891965200316,-1.74319588344627,
-1.73984622431255,-1.73680753612006,-1.7325755580415,-1.7222209776748,-1.70690750334284,
-1.65350623116215,-1.59730564184874,-1.58680678975198,-1.58068220046311,
-1.57536184162547,-1.56878108118556,-1.55577502540947,-1.50735400480745,
-1.45747415578814,-1.42843560360286,-1.4223220933579,-1.41885158443418,
-1.4161467978325,-1.41232251572522,-1.40429607663505,-1.33816476365675,
-1.2809630757481,-1.26734742409785,-1.26064828923641,-1.25531865135497,
-1.24927651969447,-1.23888175498732,-1.18436757511404,-1.1315368358298,
-1.10665560378847,-1.10070616779897,-1.0973072172321,-1.0942841922768,-1.09015614018212,
-1.08043438714862,-1.06637559166544,-1.02122315479132,-0.959546581143472,
-0.945984702377664,-0.939295782185956,-0.933966925025547,-0.927917813081183,
-0.917490930616126,-0.861889115931241,-0.807145595013794,-0.784972499816132,
-0.779210543216743,-0.775852412722177,-0.772816509082223,-0.768602873731845,
-0.758362927624136,-0.743280187726051,-0.691512814550863,-0.633198624710415,
-0.622743016026284,-0.616627923709213,-0.611306380242599,-0.604711959246729,
-0.591637435762296,-0.542672612896766,-0.491586934217922,-0.464245534626607,
-0.458216737563347,-0.454765281665521,-0.452057040883249,-0.448203956006191,
-0.44002626839897,-0.405910018304364,-0.347346149265129,-0.310495490934644,
-0.300656135244878,-0.294733106429359,-0.289638493607166,-0.289413176345763,
-0.289197912242156,-0.288991140798167,-0.288791522621203,-0.288597893934967,
-0.288409231141944,-0.281854747281621,-0.274014556102258,-0.260610926794667,
-0.230924903372333,-0.168249844613081,-0.142728446000465,-0.13679928309122,
-0.133370386324583,-0.13035474928407,-0.126282497862192,-0.116889819551263,
-0.103467134916947,-0.0620033227178036,-0.000941319676076269),
 .UNSPECIFIED.);
#3680=B_SPLINE_CURVE_WITH_KNOTS('',3,(#252637,#252638,#252639,#252640),
 .UNSPECIFIED.,.F.,.F.,(4,4),(-4.05986998617981,-4.05973564480636),
 .UNSPECIFIED.);
#3681=B_SPLINE_CURVE_WITH_KNOTS('',3,(#252641,#252642,#252643,#252644,#252645,
#252646,#252647,#252648,#252649,#252650,#252651,#252652,#252653,#252654,
#252655,#252656,#252657,#252658,#252659,#252660,#252661,#252662,#252663,
#252664,#252665,#252666,#252667,#252668,#252669,#252670,#252671,#252672,
#252673,#252674,#252675,#252676,#252677,#252678,#252679,#252680,#252681,
#252682,#252683,#252684,#252685,#252686,#252687,#252688,#252689,#252690,
#252691,#252692,#252693,#252694,#252695,#252696,#252697,#252698,#252699,
#252700,#252701,#252702,#252703,#252704,#252705,#252706,#252707,#252708,
#252709,#252710,#252711,#252712,#252713,#252714,#252715,#252716,#252717,
#252718,#252719,#252720,#252721,#252722,#252723,#252724,#252725,#252726,
#252727,#252728,#252729,#252730,#252731,#252732,#252733,#252734,#252735,
#252736,#252737,#252738,#252739,#252740,#252741,#252742,#252743,#252744,
#252745,#252746,#252747,#252748,#252749,#252750,#252751,#252752,#252753,
#252754,#252755,#252756,#252757,#252758,#252759,#252760,#252761,#252762,
#252763,#252764,#252765,#252766,#252767,#252768,#252769,#252770,#252771,
#252772,#252773,#252774,#252775,#252776,#252777,#252778,#252779,#252780,
#252781,#252782,#252783,#252784,#252785,#252786,#252787,#252788,#252789,
#252790,#252791,#252792,#252793,#252794,#252795,#252796,#252797,#252798,
#252799,#252800,#252801,#252802,#252803,#252804,#252805,#252806,#252807,
#252808,#252809,#252810,#252811,#252812,#252813,#252814,#252815,#252816,
#252817,#252818,#252819,#252820,#252821,#252822,#252823,#252824,#252825,
#252826,#252827,#252828,#252829,#252830,#252831,#252832,#252833,#252834,
#252835,#252836,#252837,#252838,#252839,#252840,#252841,#252842,#252843,
#252844,#252845,#252846,#252847,#252848,#252849,#252850,#252851,#252852,
#252853,#252854),.UNSPECIFIED.,.F.,.F.,(4,2,2,2,2,2,2,2,2,2,2,2,2,2,2,2,
2,2,2,2,2,2,2,2,2,2,2,2,2,2,2,2,2,2,2,2,2,2,2,2,2,2,2,2,2,2,2,2,2,2,2,2,
2,2,2,2,2,2,2,2,2,2,2,2,2,2,2,2,2,2,2,2,2,2,2,2,2,2,2,2,2,2,2,2,2,2,2,2,
2,2,2,2,2,2,2,2,2,2,2,2,2,2,2,2,2,2,4),(-4.06051280328589,-4.03349125568929,
-4.01797158672048,-4.01142748395604,-4.00620981613182,-4.0007717472446,
-3.99447020809177,-3.98355486818143,-3.94287798577048,-3.86239817469966,
-3.84984294219378,-3.84522336059247,-3.84206413072108,-3.83874119466294,
-3.83335134071936,-3.81582217360265,-3.73852180782294,-3.71233298024723,
-3.6942027536992,-3.68661855630653,-3.68106827117857,-3.67592736286728,
-3.6674886887581,-3.6451584869305,-3.57541814088679,-3.53604066839924,-3.5272210190726,
-3.52319778988702,-3.52012993408766,-3.51652978031027,-3.51004584196845,
-3.47284742515918,-3.45869316300082,-3.41789830071261,-3.3914337616427,
-3.37316622438791,-3.36555993514114,-3.36000566748489,-3.35417355568086,
-3.34515625505989,-3.3182694035266,-3.25264379989367,-3.21472527649837,
-3.20605714684187,-3.2020615546724,-3.1989960283176,-3.19537637525836,-3.18880524111753,
-3.14713488154956,-3.13723108008066,-3.0944370688264,-3.06935563307476,
-3.05178256520013,-3.04428789401309,-3.03875207945414,-3.03358834981565,
-3.02502736287699,-3.0018466361948,-2.9328960461705,-2.8937938222999,-2.88500201710137,
-2.88098363879058,-2.8779435680964,-2.87435120757464,-2.86790307356932,
-2.83210261136269,-2.81681513458398,-2.77672309287494,-2.74964031211071,
-2.73106756802185,-2.7234127576404,-2.71784974674643,-2.71272409566563,
-2.70437229440999,-2.68263635170562,-2.612317957888,-2.57273690714379,-2.56389572095591,
-2.55986821272448,-2.5567995561936,-2.55320136360772,-2.54672765371147,
-2.50995534786278,-2.49541633557083,-2.45390009997454,-2.42781272325173,
-2.4097320755428,-2.4021548468511,-2.39660487459141,-2.3914608972026,-2.38300941636734,
-2.36059842024774,-2.29091604761021,-2.25155574557122,-2.24273688908833,
-2.23871331543739,-2.23564488271078,-2.23204368132547,-2.22555699918416,
-2.18829553169727,-2.10536409910089,-2.08812972904022,-2.08069053433702,
-2.07516337189089,-2.06927202045497,-2.0599781067523,-2.03077402217095),
 .UNSPECIFIED.);
#3682=B_SPLINE_CURVE_WITH_KNOTS('',3,(#252860,#252861,#252862,#252863),
 .UNSPECIFIED.,.F.,.F.,(4,4),(-0.00122902991741216,-0.000941425455351654),
 .UNSPECIFIED.);
#3683=B_SPLINE_CURVE_WITH_KNOTS('',3,(#252864,#252865,#252866,#252867,#252868,
#252869,#252870,#252871,#252872,#252873,#252874,#252875,#252876,#252877,
#252878,#252879,#252880,#252881,#252882,#252883,#252884,#252885,#252886,
#252887,#252888,#252889,#252890,#252891,#252892,#252893,#252894,#252895,
#252896,#252897,#252898,#252899,#252900,#252901,#252902,#252903,#252904,
#252905,#252906,#252907,#252908,#252909,#252910,#252911,#252912,#252913,
#252914,#252915,#252916,#252917,#252918,#252919,#252920,#252921,#252922,
#252923,#252924,#252925,#252926,#252927,#252928,#252929,#252930,#252931,
#252932,#252933,#252934,#252935,#252936,#252937,#252938,#252939,#252940,
#252941,#252942,#252943,#252944,#252945,#252946,#252947,#252948,#252949,
#252950,#252951,#252952,#252953,#252954,#252955,#252956,#252957,#252958,
#252959,#252960,#252961,#252962,#252963,#252964,#252965,#252966,#252967,
#252968,#252969,#252970,#252971,#252972,#252973,#252974,#252975,#252976,
#252977,#252978,#252979,#252980,#252981,#252982,#252983,#252984,#252985,
#252986,#252987,#252988,#252989,#252990,#252991,#252992,#252993,#252994,
#252995,#252996,#252997,#252998,#252999,#253000,#253001,#253002,#253003,
#253004,#253005,#253006,#253007,#253008,#253009,#253010,#253011,#253012,
#253013,#253014,#253015,#253016,#253017,#253018,#253019,#253020,#253021,
#253022,#253023,#253024,#253025,#253026,#253027,#253028,#253029,#253030,
#253031,#253032,#253033,#253034,#253035,#253036,#253037,#253038,#253039,
#253040,#253041,#253042,#253043,#253044,#253045,#253046,#253047,#253048,
#253049,#253050,#253051,#253052,#253053,#253054,#253055,#253056,#253057,
#253058,#253059,#253060,#253061,#253062,#253063,#253064,#253065,#253066,
#253067,#253068,#253069,#253070,#253071,#253072,#253073,#253074,#253075),
 .UNSPECIFIED.,.F.,.F.,(4,2,2,2,2,2,2,2,2,2,2,2,2,2,2,2,2,2,2,2,2,2,2,2,
2,2,2,2,2,2,2,2,2,2,2,2,2,2,2,2,2,2,2,2,2,2,2,2,2,2,2,2,2,2,2,2,2,2,2,2,
2,2,2,2,2,2,2,2,2,2,2,2,2,2,2,2,2,2,2,2,2,2,2,2,2,2,2,2,2,2,2,2,2,2,2,2,
2,2,2,2,2,2,2,2,2,4),(-4.05943251925004,-4.01250822828506,-3.99869180488384,
-3.99431174770842,-3.99036929249612,-3.98739604133786,-3.98390133402738,
-3.97767895338795,-3.94666864821514,-3.91381217739116,-3.86853671793411,
-3.84258318432119,-3.83468588315656,-3.82890593503146,-3.82351208450195,
-3.81642464002805,-3.80024123070016,-3.72023387395155,-3.69145300066394,
-3.68063901099352,-3.67266207567129,-3.6688474473133,-3.66614394447111,
-3.66266726220235,-3.65652563605165,-3.62696882539559,-3.5662552977107,
-3.52388031345365,-3.51400818717552,-3.50807871213459,-3.50272948635832,
-3.49584114035094,-3.48460717483407,-3.4059691569951,-3.37216683792621,
-3.35444193777202,-3.3492818534785,-3.34605614430662,-3.34299124926135,
-3.33917602137439,-3.33151435548724,-3.26989190052413,-3.21166273216861,
-3.19623443672209,-3.189200932372,-3.18383282620497,-3.17797540741489,-3.16843835097828,
-3.135491160719,-3.07349378708838,-3.03842960767292,-3.03014601281479,-3.02627325645761,
-3.02327885567791,-3.01972322998573,-3.01322889528417,-2.96789483302572,
-2.90934516297389,-2.8893826137384,-2.87460369712268,-2.8676869804542,-2.86233406007126,
-2.85641904047069,-2.84661498570669,-2.81004558422709,-2.74996973025211,
-2.71679557872491,-2.70872644586684,-2.70489411555978,-2.70218852576888,
-2.69872373791196,-2.69263527019818,-2.66409989525194,-2.61390539088448,
-2.56078224175002,-2.55043257266201,-2.54440019526658,-2.53906931699561,
-2.53235545667524,-2.51911822540249,-2.45173970619264,-2.41071836577752,
-2.39737538857587,-2.38802541442379,-2.38396082180492,-2.38094650606853,
-2.37751406816091,-2.37156827607295,-2.34562464238657,-2.29358874690308,
-2.24419313259982,-2.23106529814149,-2.22446076464558,-2.21918777663066,
-2.21309862063046,-2.20275723842207,-2.1534136935319,-2.09409657721453,
-2.07800990117234,-2.06727669991833,-2.06298478229787,-2.05993625966779,
-2.05661209101579,-2.05100447384093,-2.03050942068758,-2.03032387244298),
 .UNSPECIFIED.);
#3684=B_SPLINE_CURVE_WITH_KNOTS('',3,(#253076,#253077,#253078,#253079,#253080,
#253081,#253082,#253083,#253084,#253085,#253086,#253087,#253088,#253089,
#253090,#253091,#253092,#253093,#253094,#253095,#253096,#253097,#253098,
#253099,#253100,#253101,#253102,#253103,#253104,#253105,#253106,#253107,
#253108,#253109,#253110,#253111,#253112,#253113,#253114,#253115,#253116,
#253117,#253118,#253119,#253120,#253121,#253122,#253123,#253124,#253125,
#253126,#253127,#253128,#253129,#253130,#253131,#253132,#253133,#253134,
#253135,#253136,#253137,#253138,#253139,#253140,#253141,#253142,#253143,
#253144,#253145,#253146,#253147,#253148,#253149,#253150,#253151,#253152,
#253153,#253154,#253155,#253156,#253157,#253158,#253159,#253160,#253161,
#253162,#253163,#253164,#253165,#253166,#253167,#253168,#253169,#253170,
#253171,#253172,#253173,#253174,#253175,#253176,#253177,#253178,#253179,
#253180,#253181,#253182,#253183,#253184,#253185,#253186,#253187,#253188,
#253189,#253190,#253191,#253192,#253193,#253194,#253195,#253196,#253197,
#253198,#253199,#253200,#253201,#253202,#253203,#253204,#253205,#253206,
#253207,#253208,#253209,#253210,#253211,#253212,#253213,#253214,#253215,
#253216,#253217,#253218,#253219,#253220,#253221,#253222,#253223,#253224,
#253225,#253226,#253227,#253228,#253229,#253230,#253231,#253232,#253233,
#253234,#253235,#253236,#253237,#253238,#253239,#253240,#253241,#253242,
#253243,#253244,#253245,#253246,#253247,#253248,#253249,#253250,#253251,
#253252,#253253,#253254,#253255,#253256,#253257,#253258,#253259,#253260,
#253261,#253262,#253263,#253264,#253265,#253266,#253267,#253268,#253269,
#253270,#253271,#253272,#253273,#253274,#253275,#253276,#253277,#253278,
#253279,#253280,#253281,#253282,#253283,#253284,#253285,#253286,#253287,
#253288,#253289,#253290,#253291,#253292,#253293,#253294,#253295,#253296,
#253297,#253298,#253299,#253300,#253301,#253302,#253303,#253304,#253305,
#253306,#253307,#253308,#253309,#253310,#253311,#253312,#253313,#253314,
#253315,#253316,#253317,#253318,#253319,#253320,#253321,#253322,#253323,
#253324,#253325,#253326,#253327,#253328,#253329,#253330,#253331,#253332,
#253333,#253334,#253335,#253336,#253337,#253338,#253339,#253340,#253341,
#253342,#253343,#253344,#253345,#253346,#253347,#253348,#253349,#253350,
#253351,#253352,#253353,#253354,#253355,#253356,#253357,#253358,#253359,
#253360,#253361),.UNSPECIFIED.,.F.,.F.,(4,2,2,2,2,2,2,2,2,2,2,2,2,2,2,2,
2,2,2,2,2,2,2,2,2,2,2,2,2,2,2,2,2,2,2,2,2,2,2,2,2,2,2,2,2,2,2,2,2,2,2,2,
2,2,2,2,2,2,2,2,2,2,2,2,2,2,2,2,2,2,2,2,2,2,2,2,2,2,2,2,2,2,2,2,2,2,2,2,
2,2,2,2,2,2,2,2,2,2,2,2,2,2,2,2,2,2,2,2,2,2,2,2,2,2,2,2,2,2,2,2,2,2,2,2,
2,2,2,2,2,2,2,2,2,2,2,2,2,2,2,2,2,2,4),(-2.03077402217095,-2.03054329316223,
-1.97950585915411,-1.93073468173083,-1.92164973112131,-1.91762170578921,
-1.91454578935731,-1.91099296232783,-1.90454882531797,-1.86593920117148,
-1.77779666055522,-1.76604576490879,-1.75900419718089,-1.75351822575622,
-1.74750976437705,-1.73766855481353,-1.69805145397977,-1.65673369875796,
-1.64160362689499,-1.60550368697605,-1.59904757017494,-1.59545358493151,
-1.59241397319969,-1.58839864511556,-1.57962260455279,-1.54067133170504,
-1.47212954737459,-1.44856037273098,-1.43994556085159,-1.4347720679502,
-1.42924275314098,-1.42178686272413,-1.40444862657257,-1.32139627239894,
-1.28434952425307,-1.27786846171124,-1.2742687408577,-1.27120044555993,
-1.26717564031127,-1.25834865026321,-1.21890559621116,-1.14896332429741,
-1.12688025601084,-1.11847724295872,-1.11334243874796,-1.10778667194497,
-1.10017314680449,-1.08186211223756,-1.05530717594241,-1.01457391612522,
-1.00004092705399,-0.963213367338413,-0.956738149084022,-0.953139798652997,
-0.950071424547374,-0.946044887688408,-0.937207968424374,-0.897666354508307,
-0.827439310204909,-0.805658349468258,-0.797300224416531,-0.792173679241101,
-0.786611982132833,-0.778963205191546,-0.76042741658232,-0.733416031009266,
-0.693192610916315,-0.677879780903844,-0.642051895967409,-0.635602743905788,
-0.632010284501868,-0.628970404021135,-0.624952692052985,-0.616163779156102,
-0.577088448558739,-0.508194685334339,-0.485003014050021,-0.476440777667917,
-0.471276981678272,-0.465741576980334,-0.45824835991361,-0.440683342348332,
-0.415614311212734,-0.37277173621231,-0.324923390426804,-0.315880989057198,
-0.311860761365656,-0.308896579504256,-0.308834430346243,-0.308789475798928,
-0.308720948683653,-0.308656605274084,-0.308596018595368,-0.308538820093903,
-0.308484689679083,-0.308433347778783,-0.308384548947327,-0.308338076656965,
-0.308293739044644,-0.308251365395575,-0.308210803230603,-0.308171915865701,
-0.308134580350116,-0.308098685760015,-0.308064131705786,-0.308030827072463,
-0.30799868895484,-0.307967641715317,-0.307937616183952,-0.307908548967409,
-0.307880381834737,-0.30785306118997,-0.307826537601013,-0.307800765381932,
-0.30777570225921,-0.307751309031958,-0.307727549284388,-0.307704389134684,
-0.307681797019091,-0.307659743486991,-0.3076382010022,-0.307617143810173,
-0.307596547766604,-0.307576390229745,-0.307538527833294,-0.307500736275751,
-0.307463003621433,-0.307425318134875,-0.307387668267892,-0.303382625934521,
-0.298671112517162,-0.290390078420425,-0.271467109705538,-0.229540664352217,
-0.168239170202113,-0.157611171051473,-0.151373578930371,-0.145929509675019,
-0.139159569306342,-0.125640660345811,-0.0739691429210548,-0.0428284470474373,
-0.000993735616496565),.UNSPECIFIED.);
#3685=B_SPLINE_CURVE_WITH_KNOTS('',3,(#253366,#253367,#253368,#253369,#253370,
#253371,#253372,#253373,#253374,#253375,#253376,#253377,#253378,#253379,
#253380,#253381,#253382,#253383,#253384,#253385,#253386,#253387,#253388,
#253389,#253390,#253391,#253392,#253393,#253394,#253395,#253396,#253397,
#253398,#253399,#253400,#253401,#253402,#253403,#253404,#253405,#253406,
#253407,#253408,#253409,#253410,#253411,#253412,#253413,#253414,#253415,
#253416,#253417,#253418,#253419,#253420,#253421,#253422,#253423,#253424,
#253425,#253426,#253427,#253428,#253429,#253430,#253431,#253432,#253433,
#253434,#253435,#253436,#253437,#253438,#253439,#253440,#253441,#253442,
#253443,#253444,#253445,#253446,#253447,#253448,#253449,#253450,#253451,
#253452,#253453,#253454,#253455,#253456,#253457,#253458,#253459,#253460,
#253461,#253462,#253463,#253464,#253465,#253466,#253467,#253468,#253469,
#253470,#253471,#253472,#253473,#253474,#253475,#253476,#253477,#253478,
#253479,#253480,#253481,#253482,#253483,#253484,#253485,#253486,#253487,
#253488,#253489,#253490,#253491,#253492,#253493,#253494,#253495,#253496,
#253497,#253498,#253499,#253500,#253501,#253502,#253503,#253504,#253505,
#253506,#253507,#253508,#253509,#253510,#253511,#253512,#253513,#253514,
#253515,#253516,#253517,#253518,#253519,#253520,#253521,#253522,#253523,
#253524,#253525,#253526,#253527,#253528,#253529,#253530,#253531,#253532,
#253533,#253534,#253535,#253536,#253537,#253538,#253539,#253540,#253541,
#253542,#253543,#253544,#253545,#253546,#253547,#253548,#253549,#253550,
#253551,#253552,#253553,#253554,#253555,#253556,#253557,#253558,#253559,
#253560,#253561,#253562,#253563,#253564,#253565,#253566,#253567,#253568,
#253569,#253570,#253571),.UNSPECIFIED.,.F.,.F.,(4,2,2,2,2,2,2,2,2,2,2,2,
2,2,2,2,2,2,2,2,2,2,2,2,2,2,2,2,2,2,2,2,2,2,2,2,2,2,2,2,2,2,2,2,2,2,2,2,
2,2,2,2,2,2,2,2,2,2,2,2,2,2,2,2,2,2,2,2,2,2,2,2,2,2,2,2,2,2,2,2,2,2,2,2,
2,2,2,2,2,2,2,2,2,2,2,2,2,2,2,2,2,2,4),(-2.03071434728601,-2.02406353587364,
-2.01908685646972,-2.01362036552204,-2.00598027294809,-1.98684159483128,
-1.95843052180122,-1.89658083920336,-1.89528978875892,-1.86831400199091,
-1.8623051670069,-1.85885859650199,-1.85615003054387,-1.85229105765456,
-1.84408001077536,-1.80966252041393,-1.74840407813406,-1.71419939256671,
-1.70457929248984,-1.69870419392353,-1.69334152724426,-1.68634644716821,
-1.67113260672148,-1.61240722870165,-1.55091232302111,-1.5432430068348,
-1.53942597866863,-1.53636067767775,-1.53313574560849,-1.5279791761728,
-1.51028871772211,-1.47659588702326,-1.39783732428557,-1.38662317591827,
-1.37974055820503,-1.37439201637046,-1.3684594627284,-1.35857307600554,
-1.31595351180966,-1.25412522186513,-1.22577419175953,-1.21969463139117,
-1.21623193311996,-1.21352608969297,-1.20969099567397,-1.20160678144858,
-1.16830230027922,-1.10816681240579,-1.07185565381104,-1.06206729328405,
-1.05615578902976,-1.05080225455898,-1.04387937690591,-1.02906606648274,
-1.0090394273269,-0.950114599950162,-0.905204604022645,-0.898711062141302,
-0.895155656839439,-0.89216127447609,-0.888288370641051,-0.880003777188907,
-0.844931766851071,-0.782999404528137,-0.750063418814445,-0.740527639791859,
-0.734670505290375,-0.729302321317867,-0.722268227158778,-0.706836768310102,
-0.662882551525829,-0.587324587877297,-0.579408214725877,-0.575531178003882,
-0.572727493736941,-0.569593497403912,-0.564857878698352,-0.55095592115304,
-0.527744458004199,-0.45850658474406,-0.428180345289793,-0.418902371277761,
-0.413100484883986,-0.407713718237056,-0.400552308899267,-0.384392958971016,
-0.331219995956714,-0.264939614330755,-0.256841801552086,-0.25300381065856,
-0.250011517639456,-0.246428651366949,-0.240067262257872,-0.19709964013155,
-0.1506644438478,-0.108485130216251,-0.0983466391663633,-0.092359187068013,
-0.0870204334487193,-0.0802320040166418,-0.0728770014022373,-0.053460858918564,
-0.00122902991741216),.UNSPECIFIED.);
#3686=B_SPLINE_CURVE_WITH_KNOTS('',3,(#253573,#253574,#253575,#253576),
 .UNSPECIFIED.,.F.,.F.,(4,4),(-0.000993735616496565,-0.000938146623603337),
 .UNSPECIFIED.);
#3687=B_SPLINE_CURVE_WITH_KNOTS('',3,(#253577,#253578,#253579,#253580,#253581,
#253582,#253583,#253584,#253585,#253586,#253587,#253588,#253589,#253590,
#253591,#253592,#253593,#253594,#253595,#253596,#253597,#253598,#253599,
#253600,#253601,#253602,#253603,#253604,#253605,#253606,#253607,#253608,
#253609,#253610,#253611,#253612,#253613,#253614,#253615,#253616,#253617,
#253618,#253619,#253620,#253621,#253622,#253623,#253624,#253625,#253626,
#253627,#253628,#253629,#253630,#253631,#253632,#253633,#253634,#253635,
#253636,#253637,#253638,#253639,#253640,#253641,#253642,#253643,#253644,
#253645,#253646,#253647,#253648,#253649,#253650,#253651,#253652,#253653,
#253654,#253655,#253656,#253657,#253658,#253659,#253660,#253661,#253662,
#253663,#253664,#253665,#253666,#253667,#253668,#253669,#253670,#253671,
#253672,#253673,#253674,#253675,#253676,#253677,#253678,#253679,#253680,
#253681,#253682,#253683,#253684,#253685,#253686,#253687,#253688,#253689,
#253690,#253691,#253692,#253693,#253694,#253695,#253696,#253697,#253698,
#253699,#253700,#253701,#253702,#253703,#253704,#253705,#253706,#253707,
#253708,#253709,#253710,#253711,#253712,#253713,#253714,#253715,#253716,
#253717,#253718,#253719,#253720,#253721,#253722,#253723,#253724,#253725,
#253726,#253727,#253728,#253729,#253730,#253731,#253732,#253733,#253734,
#253735,#253736,#253737,#253738,#253739,#253740,#253741,#253742,#253743,
#253744,#253745,#253746,#253747,#253748,#253749,#253750,#253751,#253752,
#253753,#253754,#253755,#253756,#253757,#253758,#253759,#253760,#253761,
#253762,#253763,#253764,#253765,#253766,#253767,#253768,#253769,#253770,
#253771,#253772,#253773,#253774,#253775,#253776,#253777,#253778,#253779,
#253780,#253781,#253782,#253783,#253784),.UNSPECIFIED.,.F.,.F.,(4,2,2,2,
2,2,2,2,2,2,2,2,2,2,2,2,2,2,2,2,2,2,2,2,2,2,2,2,2,2,2,2,2,2,2,2,2,2,2,2,
2,2,2,2,2,2,2,2,2,2,2,2,2,2,2,2,2,2,2,2,2,2,2,2,2,2,2,2,2,2,2,2,2,2,2,2,
2,2,2,2,2,2,2,2,2,2,2,2,2,2,2,2,2,2,2,2,2,2,2,2,2,2,2,4),(-4.0605796293872,
-4.05409653814727,-4.05094574927176,-4.04805958206979,-4.04475364936424,
-4.03944020767741,-4.02258933328322,-3.96312384572504,-3.91146372269416,
-3.89794667649816,-3.89117755144233,-3.88578396873489,-3.87956495193356,
-3.86901801060594,-3.81548323498542,-3.77780937643852,-3.73830672729257,
-3.7318377827319,-3.72828016492804,-3.72520595107168,-3.72118765843364,
-3.71215462673145,-3.66472314858551,-3.62396546582613,-3.59747481512421,
-3.57919480194637,-3.57158696240612,-3.5660328166401,-3.56089772232263,
-3.55249020429396,-3.5303715943021,-3.46043424058787,-3.42098855318837,
-3.41216208958356,-3.40813770658865,-3.40506983786599,-3.40147068841176,
-3.3949909237573,-3.3579464086148,-3.27495018129301,-3.25762678725453,-3.25017394098637,
-3.2446456298785,-3.23947215267957,-3.2308552501926,-3.20726693857718,-3.13871064020466,
-3.09974982394642,-3.09097343904006,-3.0869582952316,-3.08389140175189,
-3.08028623487374,-3.07377900089017,-3.03563950788253,-3.02378990676986,
-2.98525145487083,-2.95665356403366,-2.93734984990228,-2.92958330183846,
-2.92400130200861,-2.91821864982873,-2.90943502643838,-2.884608077925,-2.8171822791253,
-2.77862105721687,-2.76988590975396,-2.76587819919882,-2.762811845006,-2.75920123468644,
-2.75267000458885,-2.713502205214,-2.7028713199414,-2.66429069312906,-2.63562296125547,
-2.61628571449468,-2.6085138464603,-2.60293068291467,-2.59714914719821,
-2.58837180865543,-2.56359502834578,-2.49611955358164,-2.45753996298766,
-2.44880265565485,-2.44479442018048,-2.44172785734091,-2.43811721072124,
-2.43158646864904,-2.39245684384723,-2.34981146838474,-2.30057356491377,
-2.29022508293843,-2.28410754981459,-2.27864633148644,-2.27169017715562,
-2.26049701804941,-2.18099474896332,-2.1330416947955,-2.12639875716953,
-2.12280375566951,-2.11973482762843,-2.11577064317526,-2.1070425078828,
-2.03134880387602,-2.03107347865865),.UNSPECIFIED.);
#3688=B_SPLINE_CURVE_WITH_KNOTS('',3,(#253789,#253790,#253791,#253792,#253793,
#253794,#253795,#253796,#253797,#253798,#253799,#253800,#253801,#253802,
#253803,#253804,#253805,#253806,#253807,#253808,#253809,#253810,#253811,
#253812,#253813,#253814,#253815,#253816,#253817,#253818,#253819,#253820,
#253821,#253822,#253823,#253824,#253825,#253826,#253827,#253828,#253829,
#253830,#253831,#253832,#253833,#253834,#253835,#253836,#253837,#253838,
#253839,#253840,#253841,#253842,#253843,#253844,#253845,#253846,#253847,
#253848,#253849,#253850,#253851,#253852,#253853,#253854,#253855,#253856,
#253857,#253858,#253859,#253860,#253861,#253862,#253863,#253864,#253865,
#253866,#253867,#253868,#253869,#253870,#253871,#253872,#253873,#253874,
#253875,#253876,#253877,#253878,#253879,#253880,#253881,#253882,#253883,
#253884,#253885,#253886,#253887,#253888,#253889,#253890,#253891,#253892,
#253893,#253894,#253895,#253896,#253897,#253898,#253899,#253900,#253901,
#253902,#253903,#253904,#253905,#253906,#253907,#253908,#253909,#253910,
#253911,#253912,#253913,#253914,#253915,#253916,#253917,#253918,#253919,
#253920,#253921,#253922,#253923,#253924,#253925,#253926,#253927,#253928,
#253929,#253930,#253931,#253932,#253933,#253934,#253935,#253936,#253937,
#253938,#253939,#253940,#253941,#253942,#253943,#253944,#253945,#253946,
#253947,#253948,#253949,#253950,#253951,#253952,#253953,#253954,#253955,
#253956,#253957,#253958,#253959,#253960,#253961,#253962,#253963,#253964,
#253965,#253966,#253967,#253968,#253969,#253970,#253971,#253972,#253973,
#253974,#253975,#253976,#253977,#253978,#253979,#253980,#253981,#253982,
#253983,#253984,#253985,#253986,#253987,#253988,#253989,#253990,#253991,
#253992,#253993,#253994,#253995,#253996,#253997,#253998,#253999,#254000,
#254001,#254002,#254003,#254004,#254005,#254006,#254007,#254008,#254009,
#254010,#254011,#254012,#254013,#254014,#254015,#254016),.UNSPECIFIED.,
 .F.,.F.,(4,2,2,2,2,2,2,2,2,2,2,2,2,2,2,2,2,2,2,2,2,2,2,2,2,2,2,2,2,2,2,
2,2,2,2,2,2,2,2,2,2,2,2,2,2,2,2,2,2,2,2,2,2,2,2,2,2,2,2,2,2,2,2,2,2,2,2,
2,2,2,2,2,2,2,2,2,2,2,2,2,2,2,2,2,2,2,2,2,2,2,2,2,2,2,2,2,2,2,2,2,2,2,2,
2,2,2,2,2,2,2,2,2,2,4),(-4.06010073944462,-4.00327381972928,-3.96354321613332,
-3.95382913717875,-3.94793261272819,-3.94257345686202,-3.93573155962147,
-3.92440621706684,-3.84644538263637,-3.81217588003557,-3.80014661742054,
-3.79165397931317,-3.78785687065285,-3.78782741753919,-3.78779774106567,
-3.78776783213994,-3.78773768139857,-3.78770727920272,-3.78767661562042,
-3.78764568041245,-3.78761446301772,-3.78758295253458,-3.78755113770363,
-3.78751900689269,-3.78748654807848,-3.78745374882245,-3.78446082116079,
-3.78091495024047,-3.77445452154205,-3.73152093672186,-3.67108319396295,
-3.65081826413086,-3.6358742218668,-3.62893220238744,-3.62358128586204,
-3.6176902729464,-3.60797748721511,-3.57278083568718,-3.51198929032935,
-3.4780773912706,-3.46992745463897,-3.46608259880066,-3.46337725259315,
-3.4599244489104,-3.45388855361422,-3.42639083462642,-3.375467653324,-3.32658438507309,
-3.31351883544498,-3.30692550601872,-3.30160314019417,-3.29548516284331,
-3.28501958727846,-3.22786620357478,-3.18631516943313,-3.16420952710604,
-3.1507647081687,-3.14608612238395,-3.14296317251842,-3.14014902650046,
-3.1354598512689,-3.12294655100966,-3.03412819164323,-3.01073693376364,
-2.99410510255792,-2.98686475848883,-2.98146714681414,-2.97569927442377,
-2.96657460111911,-2.93760591624089,-2.86688601835713,-2.83238166636915,
-2.82616880991931,-2.82271365554672,-2.81970550700989,-2.81575297569686,
-2.80679421059303,-2.75557752525019,-2.70425262343495,-2.68559656333056,
-2.67155765210389,-2.66477944844609,-2.6594437432434,-2.65345450536128,
-2.64330020421297,-2.60080367279707,-2.52038715406851,-2.50783714237644,
-2.50327974661355,-2.50018274011633,-2.49695169062712,-2.49176663044955,
-2.4754470752176,-2.41644688862484,-2.36654683849256,-2.35099536903007,
-2.34394025165896,-2.33856932025821,-2.3327221861508,-2.32323217569013,
-2.29129199238619,-2.22878774728127,-2.1932389719582,-2.18490191505006,
-2.18101919654915,-2.17802413799751,-2.17447613384317,-2.16801536993754,
-2.127813068444,-2.11636009937467,-2.07437677528396,-2.04861021427306,-2.03076150463163,
-2.03071434728601),.UNSPECIFIED.);
#3689=B_SPLINE_CURVE_WITH_KNOTS('',3,(#254017,#254018,#254019,#254020,#254021,
#254022,#254023,#254024,#254025,#254026,#254027,#254028,#254029,#254030,
#254031,#254032,#254033,#254034,#254035,#254036,#254037,#254038,#254039,
#254040,#254041,#254042,#254043,#254044,#254045,#254046,#254047,#254048,
#254049,#254050,#254051,#254052,#254053,#254054,#254055,#254056,#254057,
#254058,#254059,#254060,#254061,#254062,#254063,#254064,#254065,#254066,
#254067,#254068,#254069,#254070,#254071,#254072,#254073,#254074,#254075,
#254076,#254077,#254078,#254079,#254080,#254081,#254082,#254083,#254084,
#254085,#254086,#254087,#254088,#254089,#254090,#254091,#254092,#254093,
#254094,#254095,#254096,#254097,#254098,#254099,#254100,#254101,#254102,
#254103,#254104,#254105,#254106,#254107,#254108,#254109,#254110,#254111,
#254112,#254113,#254114,#254115,#254116,#254117,#254118,#254119,#254120,
#254121,#254122,#254123,#254124,#254125,#254126,#254127,#254128,#254129,
#254130,#254131,#254132,#254133,#254134,#254135,#254136,#254137,#254138,
#254139,#254140,#254141,#254142,#254143,#254144,#254145,#254146,#254147,
#254148,#254149,#254150,#254151,#254152,#254153,#254154,#254155,#254156,
#254157,#254158,#254159,#254160,#254161,#254162,#254163,#254164,#254165,
#254166,#254167,#254168,#254169,#254170,#254171,#254172,#254173,#254174,
#254175,#254176,#254177,#254178,#254179,#254180,#254181,#254182,#254183,
#254184,#254185,#254186,#254187,#254188,#254189,#254190,#254191,#254192,
#254193,#254194,#254195,#254196,#254197,#254198,#254199,#254200,#254201,
#254202,#254203,#254204,#254205,#254206,#254207,#254208,#254209,#254210,
#254211,#254212,#254213,#254214),.UNSPECIFIED.,.F.,.F.,(4,2,2,2,2,2,2,2,
2,2,2,2,2,2,2,2,2,2,2,2,2,2,2,2,2,2,2,2,2,2,2,2,2,2,2,2,2,2,2,2,2,2,2,2,
2,2,2,2,2,2,2,2,2,2,2,2,2,2,2,2,2,2,2,2,2,2,2,2,2,2,2,2,2,2,2,2,2,2,2,2,
2,2,2,2,2,2,2,2,2,2,2,2,2,2,2,2,2,2,4),(-2.03107347865865,-1.97987140276865,
-1.96935418936223,-1.96314124982904,-1.95774600484078,-1.95096573060103,
-1.93739473676935,-1.91964251984052,-1.87311767327197,-1.81524548508242,
-1.80647004637097,-1.80249736955979,-1.79942770421053,-1.7958388269116,
-1.78922439505932,-1.74309306716707,-1.6647820322584,-1.6504859861263,-1.64356723128021,
-1.63810996876968,-1.63197024785478,-1.62151806627189,-1.56961476231467,
-1.49396957897866,-1.48522263387823,-1.48125497303931,-1.47818557264391,
-1.47459253849214,-1.46795984212665,-1.42069163022611,-1.3403609399169,
-1.32927419322384,-1.3223489672679,-1.3168906606756,-1.31075401261354,-1.30031762959146,
-1.24886537199474,-1.23445353129113,-1.17245050089247,-1.16475124987323,
-1.16088437433675,-1.15775942943671,-1.15444086660573,-1.14906999593193,
-1.12988481612895,-1.09153056410051,-1.02085667034282,-1.00769791181744,
-1.00091296824315,-0.995468306777088,-0.989242551512734,-0.978385278680229,
-0.910769964633354,-0.851601209292436,-0.842842660399556,-0.838873334059304,
-0.835804313932795,-0.832213870076595,-0.82559113737444,-0.778929064482799,
-0.697753264600984,-0.686766790816478,-0.6798713303275,-0.674416387165562,
-0.668262339198706,-0.657743213899477,-0.603856541579402,-0.551966623724773,
-0.526073966225798,-0.519980961073066,-0.516503654286094,-0.51340870629343,
-0.509171369945661,-0.49913246482896,-0.484533614802463,-0.43641812230889,
-0.379164040841241,-0.365641442919304,-0.358779333173023,-0.353325360989467,
-0.347145290395334,-0.336512593794242,-0.278706986746644,-0.22010626409411,
-0.203474162443042,-0.198183901363649,-0.19488245296827,-0.191711808758821,
-0.18702436267922,-0.173953674365784,-0.152858000224886,-0.0816886554492921,
-0.050513571115412,-0.0410564845528834,-0.0351342931714837,-0.0299017612655023,
-0.0245521852369908,-0.0144938878548919,-0.0009418500334415),
 .UNSPECIFIED.);
#3690=B_SPLINE_CURVE_WITH_KNOTS('',3,(#254218,#254219,#254220,#254221,#254222,
#254223,#254224,#254225,#254226,#254227,#254228,#254229,#254230,#254231,
#254232,#254233,#254234,#254235,#254236,#254237,#254238,#254239,#254240,
#254241,#254242,#254243,#254244,#254245,#254246,#254247,#254248,#254249,
#254250,#254251,#254252,#254253,#254254,#254255,#254256,#254257,#254258,
#254259,#254260,#254261,#254262,#254263,#254264,#254265,#254266,#254267,
#254268,#254269,#254270,#254271,#254272,#254273,#254274,#254275,#254276,
#254277,#254278,#254279,#254280,#254281,#254282,#254283,#254284,#254285,
#254286,#254287,#254288,#254289,#254290,#254291,#254292,#254293,#254294,
#254295,#254296,#254297,#254298,#254299,#254300,#254301,#254302,#254303,
#254304,#254305,#254306,#254307,#254308,#254309,#254310,#254311,#254312,
#254313,#254314,#254315,#254316,#254317,#254318,#254319,#254320,#254321,
#254322,#254323,#254324,#254325,#254326,#254327,#254328,#254329,#254330,
#254331,#254332,#254333,#254334,#254335,#254336,#254337,#254338,#254339,
#254340,#254341,#254342,#254343,#254344,#254345,#254346,#254347,#254348,
#254349,#254350,#254351,#254352,#254353,#254354,#254355,#254356,#254357,
#254358,#254359,#254360,#254361,#254362,#254363,#254364,#254365,#254366,
#254367,#254368,#254369,#254370,#254371,#254372,#254373,#254374,#254375,
#254376,#254377,#254378,#254379,#254380,#254381,#254382,#254383,#254384,
#254385,#254386,#254387,#254388,#254389,#254390,#254391,#254392,#254393,
#254394,#254395,#254396,#254397,#254398,#254399,#254400,#254401,#254402,
#254403,#254404,#254405,#254406,#254407,#254408,#254409,#254410,#254411,
#254412,#254413,#254414,#254415,#254416,#254417,#254418,#254419),
 .UNSPECIFIED.,.F.,.F.,(4,3,3,3,3,3,3,3,3,3,3,3,3,3,3,3,3,3,3,3,3,3,3,3,
3,3,3,3,3,3,3,3,3,3,3,3,3,3,3,3,3,3,3,3,3,3,3,3,3,3,3,3,3,3,3,3,3,3,3,3,
3,3,3,3,3,3,3,4),(103.672557568463,103.818264882234,103.911421475433,104.004453418626,
104.097388222185,104.190256550746,104.283090631506,104.375915182229,104.468754906163,
104.561693127135,104.654683645779,104.747826170789,104.813093341946,104.906094866231,
104.998971156067,105.091749927756,105.184462290313,105.277140494718,105.369809440183,
105.462494011671,105.555278725024,105.648116417002,105.741108778493,105.807921801659,
105.901228431653,105.994409634355,106.087492733004,106.180507314493,106.273486338418,
106.366454353206,106.459435891529,106.552512528404,106.645639768258,106.738914907065,
106.802750261371,106.896007663259,106.989142157043,107.082181088458,107.175155441427,
107.268096669001,107.36102934722,107.453978038381,107.547025821459,107.640126395497,
107.733378630147,107.797578721083,107.889714279306,107.981724267907,108.073637374533,
108.165488259454,108.257307641196,108.349121268857,108.440954881136,108.53290045036,
108.62490406731,108.717079415847,108.792407180795,108.88812029801,108.983691451607,
109.08413447522,109.17946841731,109.274736986051,109.369960264623,109.465158289751,
109.560375980784,109.655603167526,109.750891777179,109.787235640508),
 .UNSPECIFIED.);
#3691=B_SPLINE_CURVE_WITH_KNOTS('',3,(#254420,#254421,#254422,#254423,#254424,
#254425,#254426,#254427,#254428,#254429,#254430,#254431,#254432,#254433,
#254434,#254435,#254436,#254437,#254438,#254439,#254440,#254441,#254442,
#254443,#254444,#254445,#254446,#254447,#254448,#254449,#254450,#254451,
#254452,#254453,#254454,#254455,#254456,#254457,#254458,#254459,#254460,
#254461,#254462,#254463,#254464,#254465,#254466,#254467,#254468,#254469,
#254470,#254471,#254472,#254473,#254474,#254475,#254476,#254477,#254478,
#254479,#254480,#254481,#254482,#254483,#254484,#254485,#254486,#254487,
#254488,#254489,#254490,#254491,#254492,#254493,#254494,#254495,#254496,
#254497,#254498,#254499,#254500,#254501,#254502,#254503,#254504,#254505,
#254506,#254507,#254508,#254509,#254510,#254511,#254512,#254513,#254514,
#254515,#254516,#254517,#254518,#254519,#254520,#254521,#254522,#254523,
#254524,#254525,#254526,#254527,#254528,#254529,#254530,#254531,#254532,
#254533,#254534,#254535,#254536,#254537,#254538,#254539,#254540,#254541,
#254542,#254543,#254544,#254545,#254546,#254547,#254548,#254549,#254550,
#254551,#254552,#254553,#254554,#254555,#254556,#254557,#254558,#254559,
#254560,#254561,#254562,#254563,#254564,#254565,#254566,#254567,#254568,
#254569,#254570,#254571,#254572,#254573,#254574,#254575,#254576,#254577,
#254578,#254579,#254580,#254581,#254582,#254583,#254584,#254585,#254586,
#254587,#254588,#254589,#254590,#254591,#254592,#254593,#254594,#254595,
#254596,#254597,#254598,#254599,#254600,#254601,#254602,#254603,#254604,
#254605,#254606,#254607,#254608,#254609,#254610,#254611,#254612,#254613,
#254614,#254615,#254616,#254617,#254618,#254619,#254620,#254621,#254622,
#254623,#254624,#254625,#254626,#254627),.UNSPECIFIED.,.F.,.F.,(4,3,3,3,
3,3,3,3,3,3,3,3,3,3,3,3,3,3,3,3,3,3,3,3,3,3,3,3,3,3,3,3,3,3,3,3,3,3,3,3,
3,3,3,3,3,3,3,3,3,3,3,3,3,3,3,3,3,3,3,3,3,3,3,3,3,3,3,3,3,4),(103.672557568638,
103.775261298986,103.878304277879,103.981841562232,104.067724430369,104.160884025681,
104.253918755596,104.346856130719,104.439726668314,104.532562751129,104.625389096472,
104.71823040696,104.811169702776,104.904161123854,104.997303785972,105.061837443301,
105.155002762704,105.24804360184,105.340987457664,105.433864999584,105.526708405513,
105.619542381756,105.712391620173,105.805339248105,105.89833923927,105.991490764735,
106.055950456232,106.148960347062,106.241845173368,106.334632639107,106.427353861026,
106.520041040157,106.612719065257,106.705412810912,106.79820660008,106.891053440063,
106.984054484014,107.050063469163,107.143377911911,107.236567096213,107.329658332532,
107.422681216068,107.51566865497,107.608645186738,107.701635333198,107.794720482451,
107.887856302815,107.98113957308,108.044176482095,108.137443386498,108.230587553017,
108.323636312462,108.416620648389,108.509571966454,108.602514829852,108.695473788108,
108.78853171488,108.881642489695,108.974904434524,109.038289495026,109.129533207633,
109.220652399344,109.31253870885,109.403501420215,109.494435465899,109.585367240415,
109.677961149161,109.769019124106,109.862380999752,109.955742875397),
 .UNSPECIFIED.);
#3692=B_SPLINE_CURVE_WITH_KNOTS('',3,(#254631,#254632,#254633,#254634,#254635,
#254636),.UNSPECIFIED.,.F.,.F.,(4,1,1,4),(-4.09274904019424,-3.97645205172536,
-2.98233903879402,-2.06157629883971),.UNSPECIFIED.);
#3693=B_SPLINE_CURVE_WITH_KNOTS('',3,(#254640,#254641,#254642,#254643,#254644),
 .UNSPECIFIED.,.F.,.F.,(4,1,4),(0.,0.994828459712242,1.11004521091125),
 .UNSPECIFIED.);
#3694=B_SPLINE_CURVE_WITH_KNOTS('',3,(#254646,#254647,#254648,#254649,#254650,
#254651,#254652,#254653,#254654,#254655,#254656,#254657,#254658,#254659,
#254660,#254661,#254662,#254663,#254664,#254665,#254666,#254667,#254668,
#254669,#254670,#254671,#254672,#254673,#254674,#254675,#254676,#254677,
#254678,#254679,#254680,#254681,#254682,#254683,#254684,#254685,#254686,
#254687,#254688,#254689,#254690,#254691,#254692,#254693,#254694,#254695,
#254696,#254697,#254698,#254699,#254700,#254701,#254702,#254703,#254704,
#254705,#254706,#254707,#254708,#254709,#254710,#254711,#254712,#254713,
#254714,#254715,#254716,#254717,#254718,#254719,#254720,#254721,#254722,
#254723,#254724,#254725,#254726,#254727,#254728,#254729,#254730,#254731,
#254732,#254733,#254734,#254735,#254736,#254737,#254738,#254739,#254740,
#254741,#254742,#254743,#254744,#254745,#254746,#254747,#254748,#254749,
#254750,#254751,#254752,#254753,#254754,#254755,#254756,#254757,#254758,
#254759,#254760,#254761,#254762,#254763,#254764,#254765,#254766,#254767,
#254768,#254769,#254770,#254771,#254772,#254773,#254774,#254775,#254776,
#254777,#254778,#254779,#254780,#254781,#254782,#254783,#254784,#254785,
#254786,#254787,#254788,#254789,#254790,#254791,#254792,#254793,#254794,
#254795,#254796,#254797,#254798,#254799,#254800,#254801,#254802,#254803,
#254804,#254805,#254806,#254807,#254808,#254809,#254810,#254811,#254812,
#254813,#254814,#254815,#254816,#254817,#254818,#254819,#254820,#254821,
#254822,#254823,#254824,#254825,#254826,#254827,#254828,#254829,#254830,
#254831,#254832,#254833,#254834,#254835,#254836,#254837,#254838,#254839,
#254840,#254841,#254842,#254843,#254844,#254845,#254846,#254847,#254848,
#254849,#254850,#254851,#254852,#254853,#254854,#254855,#254856,#254857,
#254858,#254859,#254860,#254861,#254862,#254863,#254864,#254865,#254866,
#254867,#254868,#254869,#254870,#254871,#254872,#254873,#254874),
 .UNSPECIFIED.,.F.,.F.,(4,3,3,3,3,3,3,3,3,3,3,3,3,3,3,3,3,3,3,3,3,3,3,3,
3,3,3,3,3,3,3,3,3,3,3,3,3,3,3,3,3,3,3,3,3,3,3,3,3,3,3,3,3,3,3,3,3,3,3,3,
3,3,3,3,3,3,3,3,3,3,3,3,3,3,3,3,4),(1.11004521091125,1.19658618195254,1.28302206104525,
1.37135141834266,1.45765852628216,1.54394367013426,1.63022970115781,1.72008650572448,
1.8064919221077,1.89295545020592,1.97954245262436,1.9896569194245,2.07839354757622,
2.16701659509698,2.25554962299147,2.34666659250964,2.43509828185352,2.5235164115662,
2.61194213703314,2.70039661379871,2.78894866238135,2.87755943927535,2.96629553894112,
2.98448537913676,3.0732431575045,3.16189000871733,3.2504494542818,3.3415575023527,
3.43002198667484,3.51847523453205,3.60693837515941,3.70003224108181,3.78862983616903,
3.87728906280227,3.96607484431248,3.97931383884901,4.06780433717442,4.15617965886143,
4.24446368224824,4.33567350928737,4.42385463612318,4.51202206901021,4.6001972411382,
4.6884015861779,4.77670539429878,4.86506874564576,4.95356048372003,4.97414229856127,
5.0627748690265,5.15129384270911,5.23972291607954,5.33087889635379,5.41920764213421,
5.50752339531487,5.59584743246272,5.68420103088712,5.77265392246731,5.86116643802116,
5.94980632727041,5.96897075827352,6.05759525793551,6.14610639539864,6.23452787596184,
6.32568679371483,6.41400860712589,6.50231768646847,6.59063531702913,6.67898278504305,
6.76742998783123,6.85593706670144,6.94457192822607,6.96379921798578,7.06027097853904,
7.15639479474065,7.25229694340983,7.34786388506623,7.39323051792991),
 .UNSPECIFIED.);
#3695=B_SPLINE_CURVE_WITH_KNOTS('',3,(#254876,#254877,#254878,#254879,#254880,
#254881,#254882,#254883,#254884,#254885,#254886,#254887,#254888,#254889,
#254890,#254891,#254892,#254893,#254894,#254895,#254896,#254897,#254898,
#254899,#254900,#254901,#254902,#254903,#254904,#254905,#254906,#254907,
#254908,#254909,#254910,#254911,#254912,#254913,#254914,#254915,#254916,
#254917,#254918,#254919,#254920,#254921,#254922,#254923,#254924,#254925,
#254926,#254927,#254928,#254929,#254930,#254931,#254932,#254933,#254934,
#254935,#254936,#254937,#254938,#254939,#254940,#254941,#254942,#254943,
#254944,#254945,#254946,#254947,#254948,#254949,#254950,#254951,#254952,
#254953,#254954,#254955,#254956,#254957,#254958,#254959,#254960,#254961,
#254962,#254963,#254964,#254965,#254966,#254967,#254968,#254969,#254970,
#254971,#254972,#254973,#254974,#254975,#254976,#254977,#254978,#254979,
#254980,#254981,#254982,#254983,#254984,#254985,#254986,#254987,#254988,
#254989,#254990,#254991,#254992,#254993,#254994,#254995,#254996,#254997,
#254998,#254999,#255000,#255001,#255002,#255003,#255004,#255005,#255006,
#255007,#255008,#255009,#255010,#255011,#255012,#255013,#255014,#255015,
#255016,#255017,#255018,#255019,#255020,#255021,#255022,#255023,#255024,
#255025,#255026,#255027,#255028,#255029,#255030,#255031,#255032,#255033,
#255034,#255035,#255036,#255037,#255038,#255039,#255040,#255041,#255042,
#255043,#255044,#255045,#255046,#255047,#255048,#255049,#255050,#255051,
#255052,#255053,#255054,#255055,#255056,#255057,#255058,#255059,#255060,
#255061,#255062,#255063,#255064,#255065,#255066,#255067,#255068,#255069,
#255070,#255071,#255072,#255073,#255074,#255075,#255076,#255077,#255078,
#255079,#255080,#255081,#255082,#255083,#255084,#255085,#255086,#255087,
#255088,#255089,#255090,#255091,#255092,#255093,#255094,#255095,#255096,
#255097,#255098,#255099,#255100,#255101,#255102,#255103,#255104),
 .UNSPECIFIED.,.F.,.F.,(4,3,3,3,3,3,3,3,3,3,3,3,3,3,3,3,3,3,3,3,3,3,3,3,
3,3,3,3,3,3,3,3,3,3,3,3,3,3,3,3,3,3,3,3,3,3,3,3,3,3,3,3,3,3,3,3,3,3,3,3,
3,3,3,3,3,3,3,3,3,3,3,3,3,3,3,3,4),(7.39323051809083,7.48347022309097,7.57375978939412,
7.66411673584461,7.75462047802957,7.84520966702015,7.93595807272466,7.95862767769803,
8.04723962034107,8.13573789041722,8.22414621052771,8.31530995138803,8.40361795631955,
8.49191300997709,8.58021641201351,8.66854946288955,8.75698204080424,8.84547435567409,
8.93409436213729,8.95345613741028,9.04206509863056,9.13056039468739,9.2189657518448,
9.31013060750452,9.39843569670434,9.48672785736798,9.57502839244658,9.6633586057217,
9.75178840399521,9.84027796987582,9.92889529292322,9.94828459712254,10.0368893664816,
10.1253803957387,10.2137814167579,10.3049478717675,10.3932484794336,10.4815361122486,
10.5698320779018,10.6581576848853,10.7465828452453,10.8350677491512,10.9236804104514,
10.9431130568348,11.0317210210924,11.120215285819,11.2086195786997,11.2997848209307,
11.3880887702342,11.4763797648196,11.5646791087858,11.6530081070455,11.7414366608764,
11.829924963588,11.9185410057114,11.937941516547,12.0265488062092,12.1150423936802,
12.2034460074971,12.2946115035923,12.3829147737558,12.4712050903673,12.5595037582774,
12.6478320831516,12.7362599709608,12.8247476111719,12.9133630009563,12.9327699762593,
13.0203928491707,13.1078750269985,13.1952767025933,13.2826202103428,13.3699278286532,
13.4572453849245,13.5445677094498,13.63195244959,13.6764158252704),
 .UNSPECIFIED.);
#3696=B_SPLINE_CURVE_WITH_KNOTS('',3,(#255106,#255107,#255108,#255109,#255110,
#255111,#255112,#255113,#255114,#255115,#255116,#255117,#255118,#255119,
#255120,#255121,#255122,#255123,#255124,#255125,#255126,#255127,#255128,
#255129,#255130,#255131,#255132,#255133,#255134,#255135,#255136,#255137,
#255138,#255139,#255140,#255141,#255142,#255143,#255144,#255145,#255146,
#255147,#255148,#255149,#255150,#255151,#255152,#255153,#255154,#255155,
#255156,#255157,#255158,#255159,#255160,#255161,#255162,#255163,#255164,
#255165,#255166,#255167,#255168,#255169,#255170,#255171,#255172,#255173,
#255174,#255175,#255176,#255177,#255178,#255179,#255180,#255181,#255182,
#255183,#255184,#255185,#255186,#255187,#255188,#255189,#255190,#255191,
#255192,#255193,#255194,#255195,#255196,#255197,#255198,#255199,#255200,
#255201,#255202,#255203,#255204,#255205,#255206,#255207,#255208,#255209,
#255210,#255211,#255212,#255213,#255214,#255215,#255216,#255217,#255218,
#255219,#255220,#255221,#255222,#255223,#255224,#255225,#255226,#255227,
#255228,#255229,#255230,#255231,#255232,#255233,#255234,#255235,#255236,
#255237,#255238,#255239,#255240,#255241,#255242,#255243,#255244,#255245,
#255246,#255247,#255248,#255249,#255250,#255251,#255252,#255253,#255254,
#255255,#255256,#255257,#255258,#255259,#255260,#255261,#255262,#255263,
#255264,#255265,#255266,#255267,#255268,#255269,#255270,#255271,#255272,
#255273,#255274,#255275,#255276,#255277,#255278,#255279,#255280,#255281,
#255282,#255283,#255284,#255285,#255286,#255287,#255288,#255289,#255290,
#255291,#255292,#255293,#255294,#255295,#255296,#255297,#255298,#255299,
#255300,#255301,#255302,#255303,#255304,#255305,#255306,#255307,#255308,
#255309,#255310,#255311,#255312,#255313,#255314,#255315,#255316,#255317,
#255318,#255319,#255320,#255321,#255322,#255323,#255324,#255325,#255326,
#255327,#255328,#255329,#255330,#255331,#255332,#255333,#255334),
 .UNSPECIFIED.,.F.,.F.,(4,3,3,3,3,3,3,3,3,3,3,3,3,3,3,3,3,3,3,3,3,3,3,3,
3,3,3,3,3,3,3,3,3,3,3,3,3,3,3,3,3,3,3,3,3,3,3,3,3,3,3,3,3,3,3,3,3,3,3,3,
3,3,3,3,3,3,3,3,3,3,3,3,3,3,3,3,4),(13.676415825492,13.7891574344351,13.9043053450487,
13.9275984359716,14.016205699341,14.1046992571262,14.1931028379146,14.2842683451358,
14.372571574107,14.4608618465555,14.5491604673653,14.6374887422324,14.7259165759653,
14.8144041596502,14.9030194897623,14.9224268956838,15.0110340298656,15.0995274575668,
15.1879309075392,15.2790964635213,15.3673995607014,15.4556897012271,15.5439881901263,
15.6323163332399,15.7207440361164,15.8092314893145,15.8978466904685,15.9172553553961,
16.0058624376068,16.0943558121718,16.1827592079139,16.2739247838132,16.3622278243749,
16.4505179074917,16.5388163382506,16.6271444225509,16.7155720659096,16.804059459106,
16.8926746000073,16.9120838151083,17.0006909620515,17.0891844022555,17.1775878644579,
17.2687534157532,17.3570565243985,17.4453466760841,17.5336451758243,17.6219733294457,
17.7104010422817,17.7988885051298,17.8875037154091,17.9069122748205,17.9955193991191,
18.0840128164805,18.1724162556715,18.2635818155292,18.3518849008906,18.4401750292317,
18.5284735055923,18.6168016358241,18.7052293253736,18.7937167649678,18.8823319522173,
18.9017407345328,18.9903478540733,19.0788412665423,19.1672447007132,19.2584102624047,
19.3467133424586,19.4350034653947,19.5233019362577,19.6116300609052,19.7000577447692,
19.7885451786117,19.8771603600567,19.896569194245,19.95960113245),
 .UNSPECIFIED.);
#3697=B_SPLINE_CURVE_WITH_KNOTS('',3,(#255336,#255337,#255338,#255339,#255340,
#255341,#255342,#255343,#255344,#255345,#255346,#255347,#255348,#255349,
#255350,#255351,#255352,#255353,#255354,#255355,#255356,#255357,#255358,
#255359,#255360,#255361,#255362,#255363,#255364,#255365,#255366,#255367,
#255368,#255369,#255370,#255371,#255372,#255373,#255374,#255375,#255376,
#255377,#255378,#255379,#255380,#255381,#255382,#255383,#255384,#255385,
#255386,#255387,#255388,#255389,#255390,#255391,#255392,#255393,#255394,
#255395,#255396,#255397,#255398,#255399,#255400,#255401,#255402,#255403,
#255404,#255405,#255406,#255407,#255408,#255409,#255410,#255411,#255412,
#255413,#255414,#255415,#255416,#255417,#255418,#255419,#255420,#255421,
#255422,#255423,#255424,#255425,#255426,#255427,#255428,#255429,#255430,
#255431,#255432,#255433,#255434,#255435,#255436,#255437,#255438,#255439,
#255440,#255441,#255442,#255443,#255444,#255445,#255446,#255447,#255448,
#255449,#255450,#255451,#255452,#255453,#255454,#255455,#255456,#255457,
#255458,#255459,#255460,#255461,#255462,#255463,#255464,#255465,#255466,
#255467,#255468,#255469,#255470,#255471,#255472,#255473,#255474,#255475,
#255476,#255477,#255478,#255479,#255480,#255481,#255482,#255483,#255484,
#255485,#255486,#255487,#255488,#255489,#255490,#255491,#255492,#255493,
#255494,#255495,#255496,#255497,#255498,#255499,#255500,#255501,#255502,
#255503,#255504,#255505,#255506,#255507,#255508,#255509,#255510,#255511,
#255512,#255513,#255514,#255515,#255516,#255517,#255518,#255519,#255520,
#255521,#255522,#255523,#255524,#255525,#255526,#255527,#255528,#255529,
#255530,#255531,#255532,#255533,#255534,#255535,#255536,#255537,#255538,
#255539,#255540,#255541,#255542,#255543,#255544,#255545,#255546,#255547,
#255548,#255549,#255550,#255551,#255552,#255553,#255554,#255555,#255556,
#255557,#255558,#255559,#255560,#255561),.UNSPECIFIED.,.F.,.F.,(4,3,3,3,
3,3,3,3,3,3,3,3,3,3,3,3,3,3,3,3,3,3,3,3,3,3,3,3,3,3,3,3,3,3,3,3,3,3,3,3,
3,3,3,3,3,3,3,3,3,3,3,3,3,3,3,3,3,3,3,3,3,3,3,3,3,3,3,3,3,3,3,3,3,3,3,4),
(19.9596011326339,20.0473762095346,20.1350428488705,20.2226256406632,20.3101531325818,
20.3976527830734,20.4851466858016,20.5726569253986,20.6602579030711,20.7479081347566,
20.8356943412198,20.8913976539573,20.9800047786225,21.0684981963089,21.1569016357831,
21.2480671955189,21.3363702810569,21.4246604095348,21.5129588859916,21.6012870162792,
21.6897147058233,21.7782021453768,21.8668173325332,21.8862261136696,21.9748332380488,
22.0633266554348,22.151730094595,22.2428956544434,22.3311987396352,22.4194888677553,
22.5077873438435,22.596115473751,22.6845431629013,22.773030602052,22.8616457887963,
22.8810545733818,22.9696616989445,23.0581551175325,23.1465585579113,23.2377241173092,
23.3260272037533,23.4143173331362,23.5026158104959,23.5909439416836,23.6793716321186,
23.7678590725585,23.856474260589,23.8758830330941,23.9644901580618,24.0529835760482,
24.1413870158199,24.2325525754432,24.3208556612698,24.4091457900321,24.4974442667698,
24.5857723973327,24.6742000871445,24.7626875269612,24.8513027143727,24.8707114928063,
24.9593186177899,25.0478120357911,25.1362154755763,25.227381035194,25.3156841210307,
25.4039742498019,25.4922727265469,25.5806008571162,25.6690285469324,25.7575159867526,
25.8461311741657,25.8655399525186,25.9654106279957,26.0649637746012,26.1639285591376,
26.2427864394061),.UNSPECIFIED.);
#3698=B_SPLINE_CURVE_WITH_KNOTS('',3,(#255563,#255564,#255565,#255566,#255567,
#255568,#255569,#255570,#255571,#255572,#255573,#255574,#255575,#255576,
#255577,#255578,#255579,#255580,#255581,#255582,#255583,#255584,#255585,
#255586,#255587,#255588,#255589,#255590,#255591,#255592,#255593,#255594,
#255595,#255596,#255597,#255598,#255599,#255600,#255601,#255602,#255603,
#255604,#255605,#255606,#255607,#255608,#255609,#255610,#255611,#255612,
#255613,#255614,#255615,#255616,#255617,#255618,#255619,#255620,#255621,
#255622,#255623,#255624,#255625,#255626,#255627,#255628,#255629,#255630,
#255631,#255632,#255633,#255634,#255635,#255636,#255637,#255638,#255639,
#255640,#255641,#255642,#255643,#255644,#255645,#255646,#255647,#255648,
#255649,#255650,#255651,#255652,#255653,#255654,#255655,#255656,#255657,
#255658,#255659,#255660,#255661,#255662,#255663,#255664,#255665,#255666,
#255667,#255668,#255669,#255670,#255671,#255672,#255673,#255674,#255675,
#255676,#255677,#255678,#255679,#255680,#255681,#255682,#255683,#255684,
#255685,#255686,#255687,#255688,#255689,#255690,#255691,#255692,#255693,
#255694,#255695,#255696,#255697,#255698,#255699,#255700,#255701,#255702,
#255703,#255704,#255705,#255706,#255707,#255708,#255709,#255710,#255711,
#255712,#255713,#255714,#255715,#255716,#255717,#255718,#255719,#255720,
#255721,#255722,#255723,#255724,#255725,#255726,#255727,#255728,#255729,
#255730,#255731,#255732,#255733,#255734,#255735,#255736,#255737,#255738,
#255739,#255740,#255741,#255742,#255743,#255744,#255745,#255746,#255747,
#255748,#255749,#255750,#255751,#255752,#255753,#255754,#255755,#255756,
#255757,#255758,#255759,#255760,#255761,#255762,#255763,#255764,#255765,
#255766,#255767,#255768,#255769,#255770,#255771,#255772,#255773,#255774,
#255775,#255776,#255777,#255778,#255779,#255780,#255781,#255782,#255783,
#255784,#255785,#255786,#255787,#255788),.UNSPECIFIED.,.F.,.F.,(4,3,3,3,
3,3,3,3,3,3,3,3,3,3,3,3,3,3,3,3,3,3,3,3,3,3,3,3,3,3,3,3,3,3,3,3,3,3,3,3,
3,3,3,3,3,3,3,3,3,3,3,3,3,3,3,3,3,3,3,3,3,3,3,3,3,3,3,3,3,3,3,3,3,3,3,4),
(26.2427864396296,26.3318193218316,26.4208635005913,26.5099390761185,26.5991295140694,
26.6883785209592,26.7777899169144,26.8603684122308,26.9489755372762,27.0374689553405,
27.1258723951899,27.217037954784,27.305341040688,27.3936311695276,27.4819296463415,
27.5702577769808,27.6586854668681,27.7471729067595,27.8357880942444,27.8551968719431,
27.9438039969987,28.032297415073,28.1207008549323,28.2118664145227,28.3001695004365,
28.3884596292859,28.4767581061098,28.5650862367584,28.6535139266547,28.7420013665553,
28.830616554049,28.8500253316553,28.9386324567299,29.0271258748237,29.1155293147029,
29.206694874286,29.2949979602201,29.3832880890899,29.4715865659343,29.5599146966042,
29.6483423865216,29.7368298264431,29.825445013958,29.8448537913676,29.9334609164285,
30.0219543345085,30.1103577743733,30.2015233339616,30.2898264198815,30.3781165487372,
30.4664150255671,30.5547431562226,30.6431708461254,30.7316582860327,30.8202734735329,
30.8396822510798,30.9282893761434,31.016782794226,31.1051862340936,31.1963517936809,
31.2846548796033,31.3729450084614,31.4612434852935,31.5495716159513,31.6379993058566,
31.7264867457661,31.8151019332689,31.8345107107921,31.9226441977953,32.0106702726248,
32.0986108681665,32.1864878426814,32.2743354198353,32.3621629675877,32.4500259983624,
32.5259717468092),.UNSPECIFIED.);
#3699=B_SPLINE_CURVE_WITH_KNOTS('',3,(#255790,#255791,#255792,#255793,#255794,
#255795,#255796,#255797,#255798,#255799,#255800,#255801,#255802,#255803,
#255804,#255805,#255806,#255807,#255808,#255809,#255810,#255811,#255812,
#255813,#255814,#255815,#255816,#255817,#255818,#255819,#255820,#255821,
#255822,#255823,#255824,#255825,#255826,#255827,#255828,#255829,#255830,
#255831,#255832,#255833,#255834,#255835,#255836,#255837,#255838,#255839,
#255840,#255841,#255842,#255843,#255844,#255845,#255846,#255847,#255848,
#255849,#255850,#255851,#255852,#255853,#255854,#255855,#255856,#255857,
#255858,#255859,#255860,#255861,#255862,#255863,#255864,#255865,#255866,
#255867,#255868,#255869,#255870,#255871,#255872,#255873,#255874,#255875,
#255876,#255877,#255878,#255879,#255880,#255881,#255882,#255883,#255884,
#255885,#255886,#255887,#255888,#255889,#255890,#255891,#255892,#255893,
#255894,#255895,#255896,#255897,#255898,#255899,#255900,#255901,#255902,
#255903,#255904,#255905,#255906,#255907,#255908,#255909,#255910,#255911,
#255912,#255913,#255914,#255915,#255916,#255917,#255918,#255919,#255920,
#255921,#255922,#255923,#255924,#255925,#255926,#255927,#255928,#255929,
#255930,#255931,#255932,#255933,#255934,#255935,#255936,#255937,#255938,
#255939,#255940,#255941,#255942,#255943,#255944,#255945,#255946,#255947,
#255948,#255949,#255950,#255951,#255952,#255953,#255954,#255955,#255956,
#255957,#255958,#255959,#255960,#255961,#255962,#255963,#255964,#255965,
#255966,#255967,#255968,#255969,#255970,#255971,#255972,#255973,#255974,
#255975,#255976,#255977,#255978,#255979,#255980,#255981,#255982,#255983,
#255984,#255985,#255986,#255987,#255988,#255989,#255990,#255991,#255992,
#255993,#255994,#255995,#255996,#255997,#255998,#255999,#256000,#256001,
#256002,#256003,#256004,#256005,#256006,#256007,#256008,#256009,#256010,
#256011,#256012,#256013,#256014,#256015,#256016,#256017,#256018),
 .UNSPECIFIED.,.F.,.F.,(4,3,3,3,3,3,3,3,3,3,3,3,3,3,3,3,3,3,3,3,3,3,3,3,
3,3,3,3,3,3,3,3,3,3,3,3,3,3,3,3,3,3,3,3,3,3,3,3,3,3,3,3,3,3,3,3,3,3,3,3,
3,3,3,3,3,3,3,3,3,3,3,3,3,3,3,3,4),(32.5259717469845,32.6316063770899,32.7385526087099,
32.8293391705043,32.9179462955682,33.0064397136512,33.0948431535192,33.1860087131064,
33.2743117990292,33.3626019278877,33.4509004047208,33.5392285353792,33.6276562252851,
33.716143665195,33.8047588526984,33.8241676302166,33.9127747552809,34.0012681733644,
34.089671613233,34.18083717282,34.2691402587434,34.3574303876023,34.4457288644357,
34.5340569950947,34.622484685001,34.7109721249114,34.7995873124152,34.8189960899289,
34.9076032149935,34.9960966330771,35.0845000729459,35.1756656325328,35.2639687184563,
35.3522588473155,35.4405573241492,35.5288854548083,35.6173131447149,35.7058005846256,
35.7944157721296,35.8138245496411,35.9024316747054,35.9909250927888,36.0793285326574,
36.1704940922444,36.2587971781677,36.3470873070266,36.43538578386,36.5237139145189,
36.6121416044252,36.7006290443357,36.7892442318394,36.8086530093534,36.8972601344178,
36.9857535525013,37.07415699237,37.1653225519569,37.2536256378803,37.3419157667393,
37.4302142435728,37.5185423742318,37.6069700641382,37.6954575040487,37.7840726915525,
37.8034814690656,37.89208859413,37.9805820122135,38.0689854520821,38.1601510116691,
38.2484540975925,38.3367442264515,38.4250427032849,38.5133708339439,38.6017985238503,
38.690285963761,38.7789011512648,38.7983099287779,38.8091570539888),
 .UNSPECIFIED.);
#3700=B_SPLINE_CURVE_WITH_KNOTS('',3,(#256020,#256021,#256022,#256023,#256024,
#256025,#256026,#256027,#256028,#256029,#256030,#256031,#256032,#256033,
#256034,#256035,#256036,#256037,#256038,#256039,#256040,#256041,#256042,
#256043,#256044,#256045,#256046,#256047,#256048,#256049,#256050,#256051,
#256052,#256053,#256054,#256055,#256056,#256057,#256058,#256059,#256060,
#256061,#256062,#256063,#256064,#256065,#256066,#256067,#256068,#256069,
#256070,#256071,#256072,#256073,#256074,#256075,#256076,#256077,#256078,
#256079,#256080,#256081,#256082,#256083,#256084,#256085,#256086,#256087,
#256088,#256089,#256090,#256091,#256092,#256093,#256094,#256095,#256096,
#256097,#256098,#256099,#256100,#256101,#256102,#256103,#256104,#256105,
#256106,#256107,#256108,#256109,#256110,#256111,#256112,#256113,#256114,
#256115,#256116,#256117,#256118,#256119,#256120,#256121,#256122,#256123,
#256124,#256125,#256126,#256127,#256128,#256129,#256130,#256131,#256132,
#256133,#256134,#256135,#256136,#256137,#256138,#256139,#256140,#256141,
#256142,#256143,#256144,#256145,#256146,#256147,#256148,#256149,#256150,
#256151,#256152,#256153,#256154,#256155,#256156,#256157,#256158,#256159,
#256160,#256161,#256162,#256163,#256164,#256165,#256166,#256167,#256168,
#256169,#256170,#256171,#256172,#256173,#256174,#256175,#256176,#256177,
#256178,#256179,#256180,#256181,#256182,#256183,#256184,#256185,#256186,
#256187,#256188,#256189,#256190,#256191,#256192,#256193,#256194,#256195,
#256196,#256197,#256198,#256199,#256200,#256201,#256202,#256203,#256204,
#256205,#256206,#256207,#256208,#256209,#256210,#256211,#256212,#256213,
#256214,#256215,#256216,#256217,#256218,#256219,#256220,#256221,#256222,
#256223,#256224,#256225,#256226,#256227,#256228,#256229,#256230,#256231,
#256232,#256233,#256234,#256235,#256236,#256237,#256238,#256239,#256240,
#256241,#256242,#256243,#256244,#256245),.UNSPECIFIED.,.F.,.F.,(4,3,3,3,
3,3,3,3,3,3,3,3,3,3,3,3,3,3,3,3,3,3,3,3,3,3,3,3,3,3,3,3,3,3,3,3,3,3,3,3,
3,3,3,3,3,3,3,3,3,3,3,3,3,3,3,3,3,3,3,3,3,3,3,3,3,3,3,3,3,3,3,3,3,3,3,4),
(38.8091570541465,38.897595286393,38.9859200585766,39.0741553025263,39.1640281882718,
39.2521650539386,39.3402896600519,39.4284234933862,39.5196022171622,39.6078681861544,
39.7005032873222,39.7931383884901,39.8817455135546,39.9702389316381,40.0586423715069,
40.1498079310938,40.2381110170172,40.3264011458762,40.4146996227097,40.5030277533687,
40.5914554432752,40.6799428831856,40.7685580706896,40.7879668482024,40.8765739732668,
40.9650673913502,41.0534708312188,41.1446363908058,41.2329394767291,41.3212296055882,
41.4095280824215,41.4978562130806,41.5862839029871,41.6747713428978,41.7633865304015,
41.7827953079146,41.871402432979,41.9598958510626,42.0482992909313,42.1394648505183,
42.2277679364417,42.3160580653006,42.4043565421341,42.492684672793,42.5811123626994,
42.6695998026096,42.7582149901136,42.7776237676269,42.8662308926912,42.9547243107747,
43.0431277506435,43.1342933102305,43.2225963961537,43.3108865250126,43.3991850018458,
43.4875131325044,43.5759408224108,43.6644282623213,43.7530434498251,43.7724522273391,
43.8610593524037,43.9495527704867,44.0379562103554,44.1291217699424,44.2174248558657,
44.3057149847247,44.3940134615584,44.4823415922176,44.5707692821241,44.6592567220348,
44.7478719095386,44.7672806870514,44.8719117025869,44.9760047942364,45.0791547761021,
45.0923423609627),.UNSPECIFIED.);
#3701=B_SPLINE_CURVE_WITH_KNOTS('',3,(#256247,#256248,#256249,#256250,#256251,
#256252,#256253,#256254,#256255,#256256,#256257,#256258,#256259,#256260,
#256261,#256262,#256263,#256264,#256265,#256266,#256267,#256268,#256269,
#256270,#256271,#256272,#256273,#256274,#256275,#256276,#256277,#256278,
#256279,#256280,#256281,#256282,#256283,#256284,#256285,#256286,#256287,
#256288,#256289,#256290,#256291,#256292,#256293,#256294,#256295,#256296,
#256297,#256298,#256299,#256300,#256301,#256302,#256303,#256304,#256305,
#256306,#256307,#256308,#256309,#256310,#256311,#256312,#256313,#256314,
#256315,#256316,#256317,#256318,#256319,#256320,#256321,#256322,#256323,
#256324,#256325,#256326,#256327,#256328,#256329,#256330,#256331,#256332,
#256333,#256334,#256335,#256336,#256337,#256338,#256339,#256340,#256341,
#256342,#256343,#256344,#256345,#256346,#256347,#256348,#256349,#256350,
#256351,#256352,#256353,#256354,#256355,#256356,#256357,#256358,#256359,
#256360,#256361,#256362,#256363,#256364,#256365,#256366,#256367,#256368,
#256369,#256370,#256371,#256372,#256373,#256374,#256375,#256376,#256377,
#256378,#256379,#256380,#256381,#256382,#256383,#256384,#256385,#256386,
#256387,#256388,#256389,#256390,#256391,#256392,#256393,#256394,#256395,
#256396,#256397,#256398,#256399,#256400,#256401,#256402,#256403,#256404,
#256405,#256406,#256407,#256408,#256409,#256410,#256411,#256412,#256413,
#256414,#256415,#256416,#256417,#256418,#256419,#256420,#256421,#256422,
#256423,#256424,#256425,#256426,#256427,#256428,#256429,#256430,#256431,
#256432,#256433,#256434,#256435,#256436,#256437,#256438,#256439,#256440,
#256441,#256442,#256443,#256444,#256445,#256446,#256447,#256448,#256449,
#256450,#256451,#256452,#256453,#256454,#256455,#256456,#256457,#256458,
#256459,#256460,#256461,#256462,#256463,#256464,#256465,#256466,#256467,
#256468,#256469,#256470,#256471,#256472,#256473,#256474,#256475),
 .UNSPECIFIED.,.F.,.F.,(4,3,3,3,3,3,3,3,3,3,3,3,3,3,3,3,3,3,3,3,3,3,3,3,
3,3,3,3,3,3,3,3,3,3,3,3,3,3,3,3,3,3,3,3,3,3,3,3,3,3,3,3,3,3,3,3,3,3,3,3,
3,3,3,3,3,3,3,3,3,3,3,3,3,3,3,3,4),(45.0923423611684,45.1804874726743,45.268615113927,
45.3567467014704,45.4449036496255,45.533162152123,45.621476590854,45.7099331199093,
45.7621091467636,45.8507162718281,45.9392096899116,46.0276131297802,46.1187786893672,
46.2070817752906,46.2953719041496,46.3836703809832,46.4719985116424,46.5604262015488,
46.6489136414594,46.7375288289634,46.7569376064759,46.8455447315403,46.9340381496237,
47.0224415894924,47.1136071490793,47.2019102350027,47.2902003638616,47.378498840695,
47.4668269713538,47.5552546612603,47.6437421011705,47.7323572886743,47.7517660661881,
47.8403731912525,47.928866609336,48.0172700492049,48.1084356087918,48.1967386947152,
48.2850288235743,48.3733273004076,48.4616554310666,48.550083120973,48.6385705608837,
48.7271857483876,48.7465945259004,48.8352016509647,48.923695069048,49.0120985089169,
49.1032640685039,49.1915671544272,49.279857283286,49.3681557601194,49.4564838907784,
49.5449115806848,49.6333990205953,49.7220142080992,49.7414229856126,49.8300301106771,
49.9185235287605,50.0069269686287,50.0980925282157,50.186395614139,50.2746857429981,
50.3629842198315,50.4513123504906,50.5397400403971,50.6282274803076,50.7168426678114,
50.7362514453249,50.8252260157582,50.9140857907327,51.0028517450659,51.0960207258864,
51.1846602000951,51.2732715330894,51.3618844535853,51.3755276683479),
 .UNSPECIFIED.);
#3702=B_SPLINE_CURVE_WITH_KNOTS('',3,(#256477,#256478,#256479,#256480,#256481,
#256482,#256483,#256484,#256485,#256486,#256487,#256488,#256489,#256490,
#256491,#256492,#256493,#256494,#256495,#256496,#256497,#256498,#256499,
#256500,#256501,#256502,#256503,#256504,#256505,#256506,#256507,#256508,
#256509,#256510,#256511,#256512,#256513,#256514,#256515,#256516,#256517,
#256518,#256519,#256520,#256521,#256522,#256523,#256524,#256525,#256526,
#256527,#256528,#256529,#256530,#256531,#256532,#256533,#256534,#256535,
#256536,#256537,#256538,#256539,#256540,#256541,#256542,#256543,#256544,
#256545,#256546,#256547,#256548,#256549,#256550,#256551,#256552,#256553,
#256554,#256555,#256556,#256557,#256558,#256559,#256560,#256561,#256562,
#256563,#256564,#256565,#256566,#256567,#256568,#256569,#256570,#256571,
#256572,#256573,#256574,#256575,#256576,#256577,#256578,#256579,#256580,
#256581,#256582,#256583,#256584,#256585,#256586,#256587,#256588,#256589,
#256590,#256591,#256592,#256593,#256594,#256595,#256596,#256597,#256598,
#256599,#256600,#256601,#256602,#256603,#256604,#256605,#256606,#256607,
#256608,#256609,#256610,#256611,#256612,#256613,#256614,#256615,#256616,
#256617,#256618,#256619,#256620,#256621,#256622,#256623,#256624,#256625,
#256626,#256627,#256628,#256629,#256630,#256631,#256632,#256633,#256634,
#256635,#256636,#256637,#256638,#256639,#256640,#256641,#256642,#256643,
#256644,#256645,#256646,#256647,#256648,#256649,#256650,#256651,#256652,
#256653,#256654,#256655,#256656,#256657,#256658,#256659,#256660,#256661,
#256662,#256663,#256664,#256665,#256666,#256667,#256668,#256669,#256670,
#256671,#256672,#256673,#256674,#256675,#256676,#256677,#256678,#256679,
#256680,#256681,#256682,#256683,#256684,#256685,#256686,#256687,#256688,
#256689,#256690,#256691,#256692,#256693,#256694,#256695,#256696,#256697,
#256698,#256699,#256700,#256701,#256702),.UNSPECIFIED.,.F.,.F.,(4,3,3,3,
3,3,3,3,3,3,3,3,3,3,3,3,3,3,3,3,3,3,3,3,3,3,3,3,3,3,3,3,3,3,3,3,3,3,3,3,
3,3,3,3,3,3,3,3,3,3,3,3,3,3,3,3,3,3,3,3,3,3,3,3,3,3,3,3,3,3,3,3,3,3,3,4),
(51.3755276685726,51.476178803125,51.5773060586414,51.6790268227341,51.7310799050371,
51.8196870301015,51.908180448185,51.9965838880539,52.0877494476408,52.1760525335642,
52.2643426624233,52.3526411392568,52.4409692699155,52.5293969598219,52.6178843997324,
52.7064995872363,52.7259083647494,52.8145154898138,52.9030089078973,52.991412347766,
53.0825779073529,53.1708809932763,53.2591711221353,53.3474695989688,53.4357977296278,
53.5242254195342,53.6127128594447,53.7013280469485,53.7207368244617,53.8093439495261,
53.8978373676095,53.9862408074781,54.0774063670651,54.1657094529885,54.2539995818474,
54.3422980586809,54.4306261893398,54.5190538792462,54.6075413191567,54.6961565066605,
54.7155652841739,54.8041724092383,54.8926658273218,54.9810692671905,55.0722348267774,
55.1605379127008,55.2488280415598,55.3371265183933,55.4254546490523,55.5138823389587,
55.6023697788692,55.6909849663731,55.7103937438862,55.7990008689506,55.8874942870341,
55.9758977269028,56.0670632864898,56.1553663724132,56.2436565012722,56.3319549781056,
56.4202831087644,56.5087107986708,56.5971982385813,56.6858134260852,56.7052222035984,
56.7932537350039,56.8811719603503,56.9690012602387,57.0567678288438,57.1445015213368,
57.2322242343352,57.3199578511882,57.4077779743433,57.495642164388,57.5836458244834,
57.6587129753877),.UNSPECIFIED.);
#3703=B_SPLINE_CURVE_WITH_KNOTS('',3,(#256704,#256705,#256706,#256707,#256708,
#256709,#256710,#256711,#256712,#256713,#256714,#256715,#256716,#256717,
#256718,#256719,#256720,#256721,#256722,#256723,#256724,#256725,#256726,
#256727,#256728,#256729,#256730,#256731,#256732,#256733,#256734,#256735,
#256736,#256737,#256738,#256739,#256740,#256741,#256742,#256743,#256744,
#256745,#256746,#256747,#256748,#256749,#256750,#256751,#256752,#256753,
#256754,#256755,#256756,#256757,#256758,#256759,#256760,#256761,#256762,
#256763,#256764,#256765,#256766,#256767,#256768,#256769,#256770,#256771,
#256772,#256773,#256774,#256775,#256776,#256777,#256778,#256779,#256780,
#256781,#256782,#256783,#256784,#256785,#256786,#256787,#256788,#256789,
#256790,#256791,#256792,#256793,#256794,#256795,#256796,#256797,#256798,
#256799,#256800,#256801,#256802,#256803,#256804,#256805,#256806,#256807,
#256808,#256809,#256810,#256811,#256812,#256813,#256814,#256815,#256816,
#256817,#256818,#256819,#256820,#256821,#256822,#256823,#256824,#256825,
#256826,#256827,#256828,#256829,#256830,#256831,#256832,#256833,#256834,
#256835,#256836,#256837,#256838,#256839,#256840,#256841,#256842,#256843,
#256844,#256845,#256846,#256847,#256848,#256849,#256850,#256851,#256852,
#256853,#256854,#256855,#256856,#256857,#256858,#256859,#256860,#256861,
#256862,#256863,#256864,#256865,#256866,#256867,#256868,#256869,#256870,
#256871,#256872,#256873,#256874,#256875,#256876,#256877,#256878,#256879,
#256880,#256881,#256882,#256883,#256884,#256885,#256886,#256887,#256888,
#256889,#256890,#256891,#256892,#256893,#256894,#256895,#256896,#256897,
#256898,#256899,#256900,#256901,#256902,#256903,#256904,#256905,#256906,
#256907,#256908,#256909,#256910,#256911,#256912,#256913,#256914,#256915,
#256916,#256917,#256918,#256919,#256920,#256921,#256922,#256923,#256924,
#256925,#256926,#256927,#256928,#256929,#256930,#256931,#256932),
 .UNSPECIFIED.,.F.,.F.,(4,3,3,3,3,3,3,3,3,3,3,3,3,3,3,3,3,3,3,3,3,3,3,3,
3,3,3,3,3,3,3,3,3,3,3,3,3,3,3,3,3,3,3,3,3,3,3,3,3,3,3,3,3,3,3,3,3,3,3,3,
3,3,3,3,3,3,3,3,3,3,3,3,3,3,3,3,4),(57.6587129755275,57.7000506633107,57.7886577883743,
57.8771512064569,57.9655546463247,58.056720205912,58.1450232918345,58.2333134206926,
58.3216118975252,58.4099400281833,58.4983677180889,58.5868551579985,58.6754703455015,
58.6948791230229,58.7834862480875,58.8719796661712,58.9603831060401,59.051548665627,
59.1398517515505,59.2281418804097,59.3164403572433,59.4047684879024,59.493196177809,
59.5816836177198,59.6702988052238,59.6897075827352,59.7783147077997,59.8668081258832,
59.9552115657519,60.0463771253389,60.1346802112623,60.2229703401214,60.3112688169549,
60.399596947614,60.4880246375204,60.576512077431,60.665127264935,60.6845360424474,
60.7731431675117,60.8616365855951,60.9500400254637,61.0412055850507,61.129508670974,
61.2177987998329,61.3060972766663,61.3944254073251,61.4828530972315,61.5713405371419,
61.6599557246456,61.6793645021597,61.7679716272241,61.8564650453076,61.9448684851763,
62.0360340447632,62.1243371306866,62.2126272595456,62.3009257363791,62.3892538670381,
62.4776815569445,62.5661689968551,62.654784184359,62.6741929618719,62.7628000869363,
62.8512935050199,62.9396969448887,63.0308625044756,63.1191655903991,63.2074557192581,
63.2957541960915,63.3840823267506,63.4725100166571,63.5609974565676,63.6496126440714,
63.6690214215842,63.7804659467197,63.8901245517755,63.9418982824832),
 .UNSPECIFIED.);
#3704=B_SPLINE_CURVE_WITH_KNOTS('',3,(#256934,#256935,#256936,#256937,#256938,
#256939,#256940,#256941,#256942,#256943,#256944,#256945,#256946,#256947,
#256948,#256949,#256950,#256951,#256952,#256953,#256954,#256955,#256956,
#256957,#256958,#256959,#256960,#256961,#256962,#256963,#256964,#256965,
#256966,#256967,#256968,#256969,#256970,#256971,#256972,#256973,#256974,
#256975,#256976,#256977,#256978,#256979,#256980,#256981,#256982,#256983,
#256984,#256985,#256986,#256987,#256988,#256989,#256990,#256991,#256992,
#256993,#256994,#256995,#256996,#256997,#256998,#256999,#257000,#257001,
#257002,#257003,#257004,#257005,#257006,#257007,#257008,#257009,#257010,
#257011,#257012,#257013,#257014,#257015,#257016,#257017,#257018,#257019,
#257020,#257021,#257022,#257023,#257024,#257025,#257026,#257027,#257028,
#257029,#257030,#257031,#257032,#257033,#257034,#257035,#257036,#257037,
#257038,#257039,#257040,#257041,#257042,#257043,#257044,#257045,#257046,
#257047,#257048,#257049,#257050,#257051,#257052,#257053,#257054,#257055,
#257056,#257057,#257058,#257059,#257060,#257061,#257062,#257063,#257064,
#257065,#257066,#257067,#257068,#257069,#257070,#257071,#257072,#257073,
#257074,#257075,#257076,#257077,#257078,#257079,#257080,#257081,#257082,
#257083,#257084,#257085,#257086,#257087,#257088,#257089,#257090,#257091,
#257092,#257093,#257094,#257095,#257096,#257097,#257098,#257099,#257100,
#257101,#257102,#257103,#257104,#257105,#257106,#257107,#257108,#257109,
#257110,#257111,#257112,#257113,#257114,#257115,#257116,#257117,#257118,
#257119,#257120,#257121,#257122,#257123,#257124,#257125,#257126,#257127,
#257128,#257129,#257130,#257131,#257132,#257133,#257134,#257135,#257136,
#257137,#257138,#257139,#257140,#257141,#257142,#257143,#257144,#257145,
#257146,#257147,#257148,#257149,#257150,#257151,#257152,#257153,#257154,
#257155,#257156,#257157,#257158,#257159,#257160,#257161,#257162),
 .UNSPECIFIED.,.F.,.F.,(4,3,3,3,3,3,3,3,3,3,3,3,3,3,3,3,3,3,3,3,3,3,3,3,
3,3,3,3,3,3,3,3,3,3,3,3,3,3,3,3,3,3,3,3,3,3,3,3,3,3,3,3,3,3,3,3,3,3,3,3,
3,3,3,3,3,3,3,3,3,3,3,3,3,3,3,3,4),(63.9418982827071,64.0321422325308,64.1196536355069,
64.2071478195229,64.2946468554795,64.3821728137796,64.4697961122042,64.5574781053708,
64.6452874718245,64.6638498812965,64.7524570063608,64.840950424444,64.9293538643125,
65.0205194238995,65.1088225098228,65.1971126386817,65.2854111155151,65.3737392461739,
65.4621669360803,65.5506543759904,65.6392695634944,65.6586783410087,65.7472854660733,
65.8357788841568,65.9241823240256,66.0153478836125,66.103650969536,66.1919410983952,
66.2802395752289,66.3685677058882,66.4569953957948,66.5454828357052,66.6340980232092,
66.6535068007209,66.7421139257853,66.8306073438688,66.9190107837375,67.0101763433245,
67.0984794292477,67.1867695581066,67.2750680349402,67.3633961655994,67.4518238555058,
67.5403112954164,67.62892648292,67.6483352604332,67.7369423854971,67.8254358035799,
67.9138392434483,68.0050048030354,68.0933078889583,68.1815980178167,68.2698964946495,
68.3582246253081,68.446652315214,68.535139755124,68.6237549426273,68.6431637201455,
68.7317708452113,68.8202642632963,68.9086677031662,68.9998332627526,69.0881363486775,
69.176426477538,69.2647249543729,69.3530530850333,69.4414807749412,69.5299682148529,
69.6185834023578,69.6379921798577,69.7281401915285,69.8181614902726,69.9080751538865,
69.9978824824515,70.0876273877454,70.1773265093766,70.2250835898867),
 .UNSPECIFIED.);
#3705=B_SPLINE_CURVE_WITH_KNOTS('',3,(#257164,#257165,#257166,#257167,#257168,
#257169,#257170,#257171,#257172,#257173,#257174,#257175,#257176,#257177,
#257178,#257179,#257180,#257181,#257182,#257183,#257184,#257185,#257186,
#257187,#257188,#257189,#257190,#257191,#257192,#257193,#257194,#257195,
#257196,#257197,#257198,#257199,#257200,#257201,#257202,#257203,#257204,
#257205,#257206,#257207,#257208,#257209,#257210,#257211,#257212,#257213,
#257214,#257215,#257216,#257217,#257218,#257219,#257220,#257221,#257222,
#257223,#257224,#257225,#257226,#257227,#257228,#257229,#257230,#257231,
#257232,#257233,#257234,#257235,#257236,#257237,#257238,#257239,#257240,
#257241,#257242,#257243,#257244,#257245,#257246,#257247,#257248,#257249,
#257250,#257251,#257252,#257253,#257254,#257255,#257256,#257257,#257258,
#257259,#257260,#257261,#257262,#257263,#257264,#257265,#257266,#257267,
#257268,#257269,#257270,#257271,#257272,#257273,#257274,#257275,#257276,
#257277,#257278,#257279,#257280,#257281,#257282,#257283,#257284,#257285,
#257286,#257287,#257288,#257289,#257290,#257291,#257292,#257293,#257294,
#257295,#257296,#257297,#257298,#257299,#257300,#257301,#257302,#257303,
#257304,#257305,#257306,#257307,#257308,#257309,#257310,#257311,#257312,
#257313,#257314,#257315,#257316,#257317,#257318,#257319,#257320,#257321,
#257322,#257323,#257324,#257325,#257326,#257327,#257328,#257329,#257330,
#257331,#257332,#257333,#257334,#257335,#257336,#257337,#257338,#257339,
#257340,#257341,#257342,#257343,#257344,#257345,#257346,#257347,#257348,
#257349,#257350,#257351,#257352,#257353,#257354,#257355,#257356,#257357,
#257358,#257359,#257360,#257361,#257362,#257363,#257364,#257365,#257366,
#257367,#257368,#257369,#257370,#257371,#257372,#257373,#257374,#257375,
#257376,#257377,#257378,#257379,#257380,#257381,#257382,#257383,#257384,
#257385,#257386,#257387,#257388,#257389,#257390,#257391,#257392),
 .UNSPECIFIED.,.F.,.F.,(4,3,3,3,3,3,3,3,3,3,3,3,3,3,3,3,3,3,3,3,3,3,3,3,
3,3,3,3,3,3,3,3,3,3,3,3,3,3,3,3,3,3,3,3,3,3,3,3,3,3,3,3,3,3,3,3,3,3,3,3,
3,3,3,3,3,3,3,3,3,3,3,3,3,3,3,3,4),(70.2250835900812,70.3218443516428,70.4190899158864,
70.5165901278083,70.6144198067222,70.6328206395699,70.7214277646309,70.809921182711,
70.8983246225762,70.9894901821644,71.0777932680843,71.1660833969398,71.2543818737698,
71.3427100044253,71.4311376943283,71.5196251342353,71.6082403217358,71.6276490992822,
71.7162562243575,71.8047496424519,71.8931530823314,71.9843186419143,72.0726217278485,
72.1609118567182,72.2492103335624,72.3375384642319,72.4259661541488,72.5144535940698,
72.6030687815839,72.6224775589944,72.7110846840487,72.7995781021221,72.8879815419807,
72.9791471015715,73.0674501874851,73.1557403163344,73.2440387931583,73.3323669238078,
73.420794613705,73.5092820536064,73.5978972411014,73.6173060187067,73.7059131437523,
73.7944065618168,73.8828100016663,73.9739755612604,74.0622786471644,74.150568776004,
74.2388672528181,74.3271953834575,74.4156230733446,74.5041105132358,74.5927257007206,
74.612134478419,74.7007416035599,74.7892350217199,74.8776384616652,74.9688040212234,
75.0571071072231,75.1453972361581,75.2336957130672,75.3220238438014,75.4104515337821,
75.4989389737664,75.5875541613426,75.6069629381312,75.6945092421715,75.7819426777027,
75.8727334550957,75.9600150315868,76.047266012454,76.1345086911532,76.2217653498227,
76.3091023023828,76.39648710581,76.4839876343942,76.5082688968469),
 .UNSPECIFIED.);
#3706=B_SPLINE_CURVE_WITH_KNOTS('',3,(#257394,#257395,#257396,#257397,#257398,
#257399,#257400,#257401,#257402,#257403,#257404,#257405,#257406,#257407,
#257408,#257409,#257410,#257411,#257412,#257413,#257414,#257415,#257416,
#257417,#257418,#257419,#257420,#257421,#257422,#257423,#257424,#257425,
#257426,#257427,#257428,#257429,#257430,#257431,#257432,#257433,#257434,
#257435,#257436,#257437,#257438,#257439,#257440,#257441,#257442,#257443,
#257444,#257445,#257446,#257447,#257448,#257449,#257450,#257451,#257452,
#257453,#257454,#257455,#257456,#257457,#257458,#257459,#257460,#257461,
#257462,#257463,#257464,#257465,#257466,#257467,#257468,#257469,#257470,
#257471,#257472,#257473,#257474,#257475,#257476,#257477,#257478,#257479,
#257480,#257481,#257482,#257483,#257484,#257485,#257486,#257487,#257488,
#257489,#257490,#257491,#257492,#257493,#257494,#257495,#257496,#257497,
#257498,#257499,#257500,#257501,#257502,#257503,#257504,#257505,#257506,
#257507,#257508,#257509,#257510,#257511,#257512,#257513,#257514,#257515,
#257516,#257517,#257518,#257519,#257520,#257521,#257522,#257523,#257524,
#257525,#257526,#257527,#257528,#257529,#257530,#257531,#257532,#257533,
#257534,#257535,#257536,#257537,#257538,#257539,#257540,#257541,#257542,
#257543,#257544,#257545,#257546,#257547,#257548,#257549,#257550,#257551,
#257552,#257553,#257554,#257555,#257556,#257557,#257558,#257559,#257560,
#257561,#257562,#257563,#257564,#257565,#257566,#257567,#257568,#257569,
#257570,#257571,#257572,#257573,#257574,#257575,#257576,#257577,#257578,
#257579,#257580,#257581,#257582,#257583,#257584,#257585,#257586,#257587,
#257588,#257589,#257590,#257591,#257592,#257593,#257594,#257595,#257596,
#257597,#257598,#257599,#257600,#257601,#257602,#257603,#257604,#257605,
#257606,#257607,#257608,#257609,#257610,#257611,#257612,#257613,#257614,
#257615,#257616,#257617,#257618,#257619),.UNSPECIFIED.,.F.,.F.,(4,3,3,3,
3,3,3,3,3,3,3,3,3,3,3,3,3,3,3,3,3,3,3,3,3,3,3,3,3,3,3,3,3,3,3,3,3,3,3,3,
3,3,3,3,3,3,3,3,3,3,3,3,3,3,3,3,3,3,3,3,3,3,3,3,3,3,3,3,3,3,3,3,3,3,3,4),
(76.5082688970663,76.6017913978435,76.6903985228155,76.7788919408056,76.8672953805797,
76.9584609402017,77.0467640260285,77.1350541547905,77.2233526315264,77.3116807620876,
77.4001084518961,77.4885958917088,77.5772110791153,77.5966198575557,77.6852269831444,
77.7737204017533,77.8621238421481,77.9532894015381,78.041592487986,78.1298826173679,
78.2181810947223,78.3065092258995,78.3949369163176,78.4834243567367,78.5720395447406,
78.591448317268,78.6800554415763,78.7685488589052,78.8569522980218,78.9481178578916,
79.0364209430736,79.1247110711964,79.2130095472997,79.3013376772352,79.3897653664317,
79.4782528056393,79.5668679924559,79.5862767769802,79.6748839016983,79.7633773194274,
79.8517807589342,79.942946318654,80.0312494041995,80.1195395326753,80.2078380091207,
80.2961661393873,80.3845938288969,80.4730812684075,80.5616964555102,80.5811052366925,
80.6697123652559,80.7582057868492,80.8466092302344,80.9377747885057,81.0260778779398,
81.1143680103014,81.2026664906256,81.2909946247595,81.3794223181006,81.4679097614261,
81.5565249522907,81.5759336964047,81.6645408154376,81.7530342274963,81.8414376613538,
81.9326032231992,82.0209063031824,82.1091964261374,82.1974948971095,82.2858230219558,
82.3742507061504,82.4627381404012,82.5513533223634,82.570762156117,82.6912110363831,
82.7914542042459),.UNSPECIFIED.);
#3707=B_SPLINE_CURVE_WITH_KNOTS('',3,(#257621,#257622,#257623,#257624,#257625,
#257626,#257627,#257628,#257629,#257630,#257631,#257632,#257633,#257634,
#257635,#257636,#257637,#257638,#257639,#257640,#257641,#257642,#257643,
#257644,#257645,#257646,#257647,#257648,#257649,#257650,#257651,#257652,
#257653,#257654,#257655,#257656,#257657,#257658,#257659,#257660,#257661,
#257662,#257663,#257664,#257665,#257666,#257667,#257668,#257669,#257670,
#257671,#257672,#257673,#257674,#257675,#257676,#257677,#257678,#257679,
#257680,#257681,#257682,#257683,#257684,#257685,#257686,#257687,#257688,
#257689,#257690,#257691,#257692,#257693,#257694,#257695,#257696,#257697,
#257698,#257699,#257700,#257701,#257702,#257703,#257704,#257705,#257706,
#257707,#257708,#257709,#257710,#257711,#257712,#257713,#257714,#257715,
#257716,#257717,#257718,#257719,#257720,#257721,#257722,#257723,#257724,
#257725,#257726,#257727,#257728,#257729,#257730,#257731,#257732,#257733,
#257734,#257735,#257736,#257737,#257738,#257739,#257740,#257741,#257742,
#257743,#257744,#257745,#257746,#257747,#257748,#257749,#257750,#257751,
#257752,#257753,#257754,#257755,#257756,#257757,#257758,#257759,#257760,
#257761,#257762,#257763,#257764,#257765,#257766,#257767,#257768,#257769,
#257770,#257771,#257772,#257773,#257774,#257775,#257776,#257777,#257778,
#257779,#257780,#257781,#257782,#257783,#257784,#257785,#257786,#257787,
#257788,#257789,#257790,#257791,#257792,#257793,#257794,#257795,#257796,
#257797,#257798,#257799,#257800,#257801,#257802,#257803,#257804,#257805,
#257806,#257807,#257808,#257809,#257810,#257811,#257812,#257813,#257814,
#257815,#257816,#257817,#257818,#257819,#257820,#257821,#257822,#257823,
#257824,#257825,#257826,#257827,#257828,#257829,#257830,#257831,#257832,
#257833,#257834,#257835,#257836,#257837,#257838,#257839,#257840,#257841,
#257842,#257843,#257844,#257845,#257846),.UNSPECIFIED.,.F.,.F.,(4,3,3,3,
3,3,3,3,3,3,3,3,3,3,3,3,3,3,3,3,3,3,3,3,3,3,3,3,3,3,3,3,3,3,3,3,3,3,3,3,
3,3,3,3,3,3,3,3,3,3,3,3,3,3,3,3,3,3,3,3,3,3,3,3,3,3,3,3,3,3,3,3,3,3,3,4),
(82.7914542044676,82.8786912064162,82.9658605008993,83.0529939686767,83.1401140002044,
83.2272429704705,83.3144574461672,83.4017150705519,83.4891135083265,83.5655906158292,
83.6541977635751,83.7426912044279,83.8310946671256,83.9222602181776,84.0105633269349,
84.0988534785905,84.1871519781585,84.2754801314657,84.3639078437791,84.4523953059819,
84.5410105154437,84.5604190755415,84.6490261542103,84.7375195259123,84.8259229194677,
84.9170884964409,85.0053915365081,85.0936816197577,85.1819800512769,85.2703081369651,
85.3587357826303,85.4472231786738,85.5358383231833,85.5552475352537,85.643854673882,
85.732348105177,85.8207515578944,85.9119171125283,86.0002202103292,86.0885103506881,
86.176808838633,86.2651369800039,86.3535646799847,86.442052129609,86.5306673262334,
86.550075994966,86.6386832620597,86.7271768228551,86.8155804059424,86.9067459120344,
86.9950491415257,87.0833394138348,87.1716380338451,87.2599663072531,87.3483941385609,
87.4368817192527,87.5254970455713,87.5449044546782,87.6335112335058,87.7220043052216,
87.8104073989971,87.9015730884213,87.9898758310873,88.0781656183221,88.1664637555268,
88.2547915489157,88.3432189067063,88.4317060171204,88.5203208814088,88.5397329143905,
88.6314471618556,88.7230153488038,88.8144085406912,88.9056990092786,88.9968741033722,
89.0746395114255),.UNSPECIFIED.);
#3708=B_SPLINE_CURVE_WITH_KNOTS('',3,(#257848,#257849,#257850,#257851,#257852,
#257853,#257854,#257855,#257856,#257857,#257858,#257859,#257860,#257861,
#257862,#257863,#257864,#257865,#257866,#257867,#257868,#257869,#257870,
#257871,#257872,#257873,#257874,#257875,#257876,#257877,#257878,#257879,
#257880,#257881,#257882,#257883,#257884,#257885,#257886,#257887,#257888,
#257889,#257890,#257891,#257892,#257893,#257894,#257895,#257896,#257897,
#257898,#257899,#257900,#257901,#257902,#257903,#257904,#257905,#257906,
#257907,#257908,#257909,#257910,#257911,#257912,#257913,#257914,#257915,
#257916,#257917,#257918,#257919,#257920,#257921,#257922,#257923,#257924,
#257925,#257926,#257927,#257928,#257929,#257930,#257931,#257932,#257933,
#257934,#257935,#257936,#257937,#257938,#257939,#257940,#257941,#257942,
#257943,#257944,#257945,#257946,#257947,#257948,#257949,#257950,#257951,
#257952,#257953,#257954,#257955,#257956,#257957,#257958,#257959,#257960,
#257961,#257962,#257963,#257964,#257965,#257966,#257967,#257968,#257969,
#257970,#257971,#257972,#257973,#257974,#257975,#257976,#257977,#257978,
#257979,#257980,#257981,#257982,#257983,#257984,#257985,#257986,#257987,
#257988,#257989,#257990,#257991,#257992,#257993,#257994,#257995,#257996,
#257997,#257998,#257999,#258000,#258001,#258002,#258003,#258004,#258005,
#258006,#258007,#258008,#258009,#258010,#258011,#258012,#258013,#258014,
#258015,#258016,#258017,#258018,#258019,#258020,#258021,#258022,#258023,
#258024,#258025,#258026,#258027,#258028,#258029,#258030,#258031,#258032,
#258033,#258034,#258035,#258036,#258037,#258038,#258039,#258040,#258041,
#258042,#258043,#258044,#258045,#258046,#258047,#258048,#258049,#258050,
#258051,#258052,#258053,#258054,#258055,#258056,#258057,#258058,#258059,
#258060,#258061,#258062,#258063,#258064,#258065,#258066,#258067,#258068,
#258069,#258070,#258071,#258072,#258073),.UNSPECIFIED.,.F.,.F.,(4,3,3,3,
3,3,3,3,3,3,3,3,3,3,3,3,3,3,3,3,3,3,3,3,3,3,3,3,3,3,3,3,3,3,3,3,3,3,3,3,
3,3,3,3,3,3,3,3,3,3,3,3,3,3,3,3,3,3,3,3,3,3,3,3,3,3,3,3,3,3,3,3,3,3,3,4),
(89.0746395116165,89.1686632146834,89.2630023574553,89.3575003593515,89.4522779338305,
89.5345613741027,89.6231693503936,89.711663624846,89.8000679251546,89.8912331637371,
89.979537114721,90.0678281088546,90.1561274502379,90.2444564437819,90.3328849897766,
90.4213732828159,90.5099893126814,90.529389833815,90.6179944436426,90.7064853439579,
90.794886266498,90.8860527698766,90.9743533552645,91.0626409940622,91.1509369939529,
91.2392626634439,91.3276879276889,91.4161729598151,91.5047857836245,91.5242182935272,
91.6128275436993,91.7013230732993,91.7897286088216,91.8808933768739,91.9691985064186,
92.0574906562365,92.1457911292899,92.2341212293331,92.3225508394298,92.4110401730542,
92.4996572017433,92.5190467532395,92.6076586787778,92.6961569350293,92.7845652445817,
92.8757289906279,92.9640369931715,93.0523320474714,93.1406354531799,93.2289685107595,
93.3174010998141,93.4058934284332,93.4945134523218,93.5138752129518,93.6024645262058,
93.6909401039031,93.7793256959558,93.8704979430443,93.9587832740915,94.0470557126769,
94.1353365826214,94.2236472086369,94.3120576318395,94.4005279235777,94.489126264354,
94.508703672664,94.5960456223258,94.6832745648956,94.7704058542892,94.8574831823146,
94.9445290257256,95.0315658284712,95.1186578056599,95.2057776856793,95.2930068060975,
95.3578248184193),.UNSPECIFIED.);
#3709=B_SPLINE_CURVE_WITH_KNOTS('',3,(#258074,#258075,#258076,#258077,#258078,
#258079,#258080,#258081,#258082,#258083,#258084,#258085,#258086,#258087,
#258088,#258089),.UNSPECIFIED.,.F.,.F.,(4,3,3,3,3,4),(95.3578248186051,
95.5035321323763,95.6067616768316,95.7095307827672,95.8114768751005,95.8411954015946),
 .UNSPECIFIED.);
#3710=B_SPLINE_CURVE_WITH_KNOTS('',3,(#258093,#258094,#258095,#258096,#258097,
#258098,#258099,#258100,#258101,#258102,#258103,#258104,#258105,#258106,
#258107,#258108,#258109,#258110,#258111,#258112,#258113,#258114,#258115,
#258116,#258117,#258118,#258119,#258120,#258121,#258122,#258123,#258124,
#258125,#258126,#258127,#258128,#258129,#258130,#258131,#258132,#258133,
#258134,#258135,#258136,#258137,#258138,#258139,#258140,#258141,#258142,
#258143,#258144,#258145,#258146,#258147,#258148,#258149,#258150,#258151,
#258152,#258153,#258154,#258155,#258156,#258157,#258158,#258159,#258160,
#258161,#258162,#258163,#258164,#258165,#258166,#258167,#258168,#258169,
#258170,#258171,#258172,#258173,#258174,#258175,#258176,#258177,#258178,
#258179,#258180,#258181,#258182,#258183,#258184,#258185,#258186,#258187,
#258188,#258189,#258190,#258191,#258192,#258193,#258194,#258195,#258196,
#258197,#258198,#258199,#258200,#258201,#258202,#258203,#258204,#258205,
#258206,#258207,#258208,#258209,#258210,#258211,#258212,#258213,#258214,
#258215,#258216,#258217,#258218,#258219,#258220,#258221,#258222,#258223,
#258224,#258225,#258226,#258227,#258228,#258229,#258230,#258231,#258232,
#258233,#258234,#258235,#258236,#258237,#258238,#258239,#258240,#258241,
#258242,#258243,#258244,#258245,#258246,#258247,#258248,#258249,#258250,
#258251,#258252,#258253,#258254,#258255,#258256,#258257,#258258,#258259,
#258260,#258261,#258262,#258263,#258264,#258265,#258266,#258267,#258268,
#258269,#258270,#258271,#258272,#258273,#258274,#258275,#258276,#258277,
#258278,#258279,#258280,#258281,#258282,#258283,#258284,#258285,#258286,
#258287,#258288,#258289,#258290,#258291,#258292,#258293,#258294,#258295,
#258296,#258297,#258298,#258299,#258300,#258301,#258302,#258303),
 .UNSPECIFIED.,.F.,.F.,(4,3,3,3,3,3,3,3,3,3,3,3,3,3,3,3,3,3,3,3,3,3,3,3,
3,3,3,3,3,3,3,3,3,3,3,3,3,3,3,3,3,3,3,3,3,3,3,3,3,3,3,3,3,3,3,3,3,3,3,3,
3,3,3,3,3,3,3,3,3,3,4),(-97.9023967967897,-97.8098768245286,-97.7131764352143,
-97.6202556022436,-97.5271946252469,-97.4339194033831,-97.4230752672713,
-97.3343296902634,-97.2456975231773,-97.1571552179489,-97.0661310974978,
-96.9776898140414,-96.8892620118076,-96.800826546421,-96.7078604734008,
-96.6192962152005,-96.5306722242695,-96.4419244412054,-96.42896225434,-96.3401970093587,
-96.2515425422849,-96.1629753425841,-96.0719595799372,-95.9834870676489,
-95.8950257250841,-95.8065544323462,-95.7136281346118,-95.6250225631976,
-95.5363553665576,-95.447561935756,-95.4348492414086,-95.3463507655028,
-95.2579673164513,-95.1696750265485,-95.0785576767896,-94.9903680015801,
-94.9021919521721,-94.8140081043174,-94.7257950332546,-94.6374826197777,
-94.5491106283321,-94.4606106255198,-94.4407362284773,-94.352095377284,
-94.2635679649133,-94.175130306476,-94.0840669201097,-93.9957292952466,
-93.9074045909461,-93.8190715404506,-93.7307088762241,-93.6422470377735,
-93.5537255403015,-93.4650770429167,-93.446623215546,-93.3579908217227,
-93.2694716376156,-93.181041968962,-93.0899754981686,-93.0016452127027,
-92.9133275920912,-92.8250013603883,-92.7366452406657,-92.6481895061684,
-92.5596738613995,-92.4710308067318,-92.4525102026146,-92.3537185416299,
-92.25549727205,-92.1564204153629,-92.0573435586757),.UNSPECIFIED.);
#3711=B_SPLINE_CURVE_WITH_KNOTS('',3,(#258305,#258306,#258307,#258308,#258309,
#258310,#258311,#258312,#258313,#258314),.UNSPECIFIED.,.F.,.F.,(4,1,1,1,
1,1,1,4),(-92.0573433407085,-91.4583971896833,-90.4642841767519,-89.4701711638206,
-88.4760581508893,-87.4819451379579,-86.4878321250266,-85.7741580335289),
 .UNSPECIFIED.);
#3712=B_SPLINE_CURVE_WITH_KNOTS('',3,(#258316,#258317,#258318,#258319,#258320,
#258321,#258322,#258323,#258324,#258325,#258326),.UNSPECIFIED.,.F.,.F.,
(4,1,1,1,1,1,1,1,4),(-85.7741580335289,-85.4937191120952,-84.4996060991639,
-83.5054930862326,-82.5113800733012,-81.5172670603699,-80.5231540474386,
-79.5290410345072,-79.4909727263493),.UNSPECIFIED.);
#3713=B_SPLINE_CURVE_WITH_KNOTS('',3,(#258328,#258329,#258330,#258331,#258332,
#258333,#258334,#258335,#258336,#258337),.UNSPECIFIED.,.F.,.F.,(4,1,1,1,
1,1,1,4),(-79.4909727263493,-78.5349280215759,-77.5408150086445,-76.5467019957132,
-75.5525889827818,-74.5584759698505,-73.5643629569192,-73.2077947719134),
 .UNSPECIFIED.);
#3714=B_SPLINE_CURVE_WITH_KNOTS('',3,(#258339,#258340,#258341,#258342,#258343,
#258344,#258345,#258346,#258347,#258348,#258349,#258350,#258351,#258352,
#258353,#258354,#258355,#258356,#258357,#258358,#258359,#258360,#258361,
#258362,#258363,#258364,#258365,#258366,#258367,#258368,#258369,#258370,
#258371,#258372,#258373,#258374,#258375,#258376,#258377,#258378,#258379,
#258380,#258381,#258382,#258383,#258384,#258385,#258386,#258387,#258388,
#258389,#258390,#258391,#258392,#258393,#258394,#258395,#258396,#258397,
#258398,#258399,#258400,#258401,#258402,#258403,#258404,#258405,#258406,
#258407,#258408,#258409,#258410,#258411,#258412,#258413,#258414,#258415,
#258416,#258417,#258418,#258419,#258420,#258421,#258422,#258423,#258424,
#258425,#258426,#258427,#258428,#258429,#258430,#258431,#258432,#258433,
#258434,#258435,#258436,#258437,#258438,#258439,#258440,#258441,#258442,
#258443,#258444,#258445,#258446,#258447,#258448,#258449,#258450,#258451,
#258452,#258453,#258454,#258455,#258456,#258457,#258458,#258459,#258460,
#258461,#258462,#258463,#258464,#258465,#258466,#258467,#258468,#258469,
#258470,#258471,#258472,#258473,#258474,#258475,#258476,#258477,#258478,
#258479,#258480,#258481,#258482,#258483,#258484,#258485,#258486,#258487,
#258488,#258489,#258490,#258491,#258492,#258493,#258494,#258495,#258496,
#258497,#258498,#258499,#258500,#258501,#258502,#258503,#258504,#258505,
#258506,#258507,#258508,#258509,#258510,#258511,#258512,#258513,#258514,
#258515,#258516,#258517,#258518,#258519,#258520,#258521,#258522,#258523,
#258524,#258525,#258526,#258527,#258528,#258529,#258530,#258531,#258532,
#258533,#258534,#258535,#258536,#258537,#258538,#258539,#258540,#258541,
#258542,#258543,#258544,#258545,#258546,#258547,#258548,#258549,#258550,
#258551,#258552,#258553,#258554,#258555,#258556,#258557,#258558,#258559,
#258560,#258561,#258562,#258563,#258564,#258565,#258566,#258567),
 .UNSPECIFIED.,.F.,.F.,(4,3,3,3,3,3,3,3,3,3,3,3,3,3,3,3,3,3,3,3,3,3,3,3,
3,3,3,3,3,3,3,3,3,3,3,3,3,3,3,3,3,3,3,3,3,3,3,3,3,3,3,3,3,3,3,3,3,3,3,3,
3,3,3,3,3,3,3,3,3,3,3,3,3,3,3,3,4),(-73.2077874191697,-73.1191307791567,
-73.0304750182465,-72.9417994239236,-72.8489120539397,-72.7600798965587,
-72.6711787100487,-72.5821422240396,-72.5702499439878,-72.4816347896643,
-72.3931331886022,-72.3047214231813,-72.2136483616657,-72.1253366635817,
-72.0370378526932,-71.9487306333893,-71.8603937092123,-71.7719573456623,
-71.6834611976276,-71.5948376755639,-71.5761369310565,-71.4875217767217,
-71.3990201756487,-71.3106084102167,-71.2195353487053,-71.1312236506104,
-71.042924839711,-70.9546176203965,-70.8662806962091,-70.7778443326487,
-70.6893481846037,-70.6007246625301,-70.5820239181251,-70.4934087637716,
-70.4049071626793,-70.3164953972278,-70.2254223357235,-70.1371106376086,
-70.0488118266889,-69.9605046073539,-69.8721676831462,-69.7837313195652,
-69.6952351714996,-69.6066116494054,-69.5879109051938,-69.4992957508541,
-69.4107941497758,-69.3223823843386,-69.2313093228291,-69.1429976247286,
-69.0546988138235,-68.9663915945029,-68.8780546703097,-68.7896183067433,
-68.7011221586918,-68.6124986366122,-68.5937978922625,-68.50518273792,-68.416681136839,
-68.328269371399,-68.2371963098905,-68.1488846117874,-68.0605858008793,
-67.9722785815559,-67.88394165736,-67.7955052937909,-67.7070091457367,-67.6183856236545,
-67.5996848793311,-67.5113193348893,-67.4230629416262,-67.3348940028069,
-67.2467908959305,-67.1587233843022,-67.0706780149519,-66.9826080226754,
-66.9246021119901),.UNSPECIFIED.);
#3715=B_SPLINE_CURVE_WITH_KNOTS('',3,(#258569,#258570,#258571,#258572,#258573,
#258574,#258575,#258576,#258577,#258578,#258579,#258580,#258581,#258582,
#258583,#258584,#258585,#258586,#258587,#258588,#258589,#258590,#258591,
#258592,#258593,#258594,#258595,#258596,#258597,#258598,#258599,#258600,
#258601,#258602,#258603,#258604,#258605,#258606,#258607,#258608,#258609,
#258610,#258611,#258612,#258613,#258614,#258615,#258616,#258617,#258618,
#258619,#258620,#258621,#258622,#258623,#258624,#258625,#258626,#258627,
#258628,#258629,#258630,#258631,#258632,#258633,#258634,#258635,#258636,
#258637,#258638,#258639,#258640,#258641,#258642,#258643,#258644,#258645,
#258646,#258647,#258648,#258649,#258650,#258651,#258652,#258653,#258654,
#258655,#258656,#258657,#258658,#258659,#258660,#258661,#258662,#258663,
#258664,#258665,#258666,#258667,#258668,#258669,#258670,#258671,#258672,
#258673,#258674,#258675,#258676,#258677,#258678,#258679,#258680,#258681,
#258682,#258683,#258684,#258685,#258686,#258687,#258688,#258689,#258690,
#258691,#258692,#258693,#258694,#258695,#258696,#258697,#258698,#258699,
#258700,#258701,#258702,#258703,#258704,#258705,#258706,#258707,#258708,
#258709,#258710,#258711,#258712,#258713,#258714,#258715,#258716,#258717,
#258718,#258719,#258720,#258721,#258722,#258723,#258724,#258725,#258726,
#258727,#258728,#258729,#258730,#258731,#258732,#258733,#258734,#258735,
#258736,#258737,#258738,#258739,#258740,#258741,#258742,#258743,#258744,
#258745,#258746,#258747,#258748,#258749,#258750,#258751,#258752,#258753,
#258754,#258755,#258756,#258757,#258758,#258759,#258760,#258761,#258762,
#258763,#258764,#258765,#258766,#258767,#258768,#258769,#258770,#258771,
#258772,#258773,#258774,#258775,#258776,#258777,#258778,#258779,#258780,
#258781,#258782,#258783,#258784,#258785,#258786,#258787,#258788,#258789,
#258790,#258791,#258792,#258793,#258794),.UNSPECIFIED.,.F.,.F.,(4,3,3,3,
3,3,3,3,3,3,3,3,3,3,3,3,3,3,3,3,3,3,3,3,3,3,3,3,3,3,3,3,3,3,3,3,3,3,3,3,
3,3,3,3,3,3,3,3,3,3,3,3,3,3,3,3,3,3,3,3,3,3,3,3,3,3,3,3,3,3,3,3,3,3,3,4),
(-66.9246021117923,-66.8206773626048,-66.7131246145023,-66.6055718663998,
-66.5169567120572,-66.4284551109757,-66.3400433455352,-66.2489702840269,
-66.1606585859232,-66.0723597750149,-65.9840525556914,-65.8957156314953,
-65.8072792679258,-65.7187831198716,-65.6301595977888,-65.6114588534684,
-65.5228436991252,-65.4343420980434,-65.3459303326026,-65.2548572710944,
-65.1665455729903,-65.0782467620815,-64.9899395427575,-64.9016026185607,
-64.8131662549907,-64.7246701069361,-64.6360465848529,-64.6173458405371,
-64.5287306861937,-64.4402290851117,-64.3518173196705,-64.2607442581624,
-64.1724325600581,-64.0841337491491,-63.9958265298249,-63.9074896056279,
-63.8190532420577,-63.7305570940027,-63.6419335719193,-63.6232328276058,
-63.5346176732626,-63.4461160721808,-63.3577043067398,-63.2666312452317,
-63.1783195471276,-63.0900207362188,-63.0017135168948,-62.913376592698,
-62.824940229128,-62.7364440810733,-62.6478205589901,-62.6291198146744,
-62.5405046603312,-62.4520030592493,-62.3635912938083,-62.2725182323002,
-62.184206534196,-62.0959077232872,-62.0076005039631,-61.9192635797663,
-61.8308272161963,-61.7423310681415,-61.6537075460582,-61.6350068017431,
-61.5464000329724,-61.4579068136205,-61.3695034155933,-61.2784925892747,
-61.190189177838,-61.1018986244542,-61.0135996241492,-60.9252708710678,
-60.8368426762851,-60.7483546362475,-60.6597393331835,-60.6414168050444),
 .UNSPECIFIED.);
#3716=B_SPLINE_CURVE_WITH_KNOTS('',3,(#258796,#258797,#258798,#258799,#258800,
#258801,#258802,#258803,#258804,#258805,#258806,#258807,#258808,#258809,
#258810,#258811,#258812,#258813,#258814,#258815,#258816,#258817,#258818,
#258819,#258820,#258821,#258822,#258823,#258824,#258825,#258826,#258827,
#258828,#258829,#258830,#258831,#258832,#258833,#258834,#258835,#258836,
#258837,#258838,#258839,#258840,#258841,#258842,#258843,#258844,#258845,
#258846,#258847,#258848,#258849,#258850,#258851,#258852,#258853,#258854,
#258855,#258856,#258857,#258858,#258859,#258860,#258861,#258862,#258863,
#258864,#258865,#258866,#258867,#258868,#258869,#258870,#258871,#258872,
#258873,#258874,#258875,#258876,#258877,#258878,#258879,#258880,#258881,
#258882,#258883,#258884,#258885,#258886,#258887,#258888,#258889,#258890,
#258891,#258892,#258893,#258894,#258895,#258896,#258897,#258898,#258899,
#258900,#258901,#258902,#258903,#258904,#258905,#258906,#258907,#258908,
#258909,#258910,#258911,#258912,#258913,#258914,#258915,#258916,#258917,
#258918,#258919,#258920,#258921,#258922,#258923,#258924,#258925,#258926,
#258927,#258928,#258929,#258930,#258931,#258932,#258933,#258934,#258935,
#258936,#258937,#258938,#258939,#258940,#258941,#258942,#258943,#258944,
#258945,#258946,#258947,#258948,#258949,#258950,#258951,#258952,#258953,
#258954,#258955,#258956,#258957,#258958,#258959,#258960,#258961,#258962,
#258963,#258964,#258965,#258966,#258967,#258968,#258969,#258970,#258971,
#258972,#258973,#258974,#258975,#258976,#258977,#258978,#258979,#258980,
#258981,#258982,#258983,#258984,#258985,#258986,#258987,#258988,#258989,
#258990,#258991,#258992,#258993,#258994,#258995,#258996,#258997,#258998,
#258999,#259000,#259001,#259002,#259003,#259004,#259005,#259006,#259007,
#259008,#259009,#259010,#259011,#259012,#259013,#259014,#259015,#259016,
#259017,#259018,#259019,#259020,#259021),.UNSPECIFIED.,.F.,.F.,(4,3,3,3,
3,3,3,3,3,3,3,3,3,3,3,3,3,3,3,3,3,3,3,3,3,3,3,3,3,3,3,3,3,3,3,3,3,3,3,3,
3,3,3,3,3,3,3,3,3,3,3,3,3,3,3,3,3,3,3,3,3,3,3,3,3,3,3,3,3,3,3,3,3,3,3,4),
(-60.6414168048005,-60.5527932377506,-60.4642832273796,-60.375863066609,
-60.2847277802679,-60.1964077670923,-60.1081006701652,-60.0197852033004,
-59.9314400794989,-59.8429955189631,-59.7544912348454,-59.6658594661403,
-59.6467807758804,-59.5581656215372,-59.4696640204554,-59.3812522550144,
-59.2901791935062,-59.2018674954021,-59.1135686844933,-59.0252614651692,
-58.9369245409723,-58.8484881774023,-58.7599920293476,-58.6713685072643,
-58.6526677629491,-58.5640526086058,-58.4755510075239,-58.3871392420829,
-58.2960661805748,-58.2077544824706,-58.1194556715617,-58.0311484522376,
-57.9428115280407,-57.8543751644707,-57.7658790164159,-57.6772554943325,
-57.6585547500177,-57.5699395956745,-57.4814379945926,-57.3930262291516,
-57.3019531676434,-57.2136414695393,-57.1253426586305,-57.0370354393064,
-56.9486985151095,-56.8602621515395,-56.7717660034847,-56.6831424814014,
-56.6644417370864,-56.5758265827432,-56.4873249816614,-56.3989132162204,
-56.3078401547122,-56.2195284566081,-56.1312296456993,-56.0429224263752,
-55.9545855021785,-55.8661491386085,-55.7776529905539,-55.6890294684706,
-55.6703287241551,-55.5817135698118,-55.4932119687299,-55.4048002032889,
-55.3137271417808,-55.2254154436766,-55.1371166327677,-55.0488094134437,
-54.9604724892468,-54.8720361256767,-54.7835399776221,-54.6949164555388,
-54.6762157112237,-54.5708557136836,-54.4645436057556,-54.3582314978275),
 .UNSPECIFIED.);
#3717=B_SPLINE_CURVE_WITH_KNOTS('',3,(#259023,#259024,#259025,#259026,#259027,
#259028,#259029,#259030,#259031,#259032,#259033,#259034,#259035,#259036,
#259037,#259038,#259039,#259040,#259041,#259042,#259043,#259044,#259045,
#259046,#259047,#259048,#259049,#259050,#259051,#259052,#259053,#259054,
#259055,#259056,#259057,#259058,#259059,#259060,#259061,#259062,#259063,
#259064,#259065,#259066,#259067,#259068,#259069,#259070,#259071,#259072,
#259073,#259074,#259075,#259076,#259077,#259078,#259079,#259080,#259081,
#259082,#259083,#259084,#259085,#259086,#259087,#259088,#259089,#259090,
#259091,#259092,#259093,#259094,#259095,#259096,#259097,#259098,#259099,
#259100,#259101,#259102,#259103,#259104,#259105,#259106,#259107,#259108,
#259109,#259110,#259111,#259112,#259113,#259114,#259115,#259116,#259117,
#259118,#259119,#259120,#259121,#259122,#259123,#259124,#259125,#259126,
#259127,#259128,#259129,#259130,#259131,#259132,#259133,#259134,#259135,
#259136,#259137,#259138,#259139,#259140,#259141,#259142,#259143,#259144,
#259145,#259146,#259147,#259148,#259149,#259150,#259151,#259152,#259153,
#259154,#259155,#259156,#259157,#259158,#259159,#259160,#259161,#259162,
#259163,#259164,#259165,#259166,#259167,#259168,#259169,#259170,#259171,
#259172,#259173,#259174,#259175,#259176,#259177,#259178,#259179,#259180,
#259181,#259182,#259183,#259184,#259185,#259186,#259187,#259188,#259189,
#259190,#259191,#259192,#259193,#259194,#259195,#259196,#259197,#259198,
#259199,#259200,#259201,#259202,#259203,#259204,#259205,#259206,#259207,
#259208,#259209,#259210,#259211,#259212,#259213,#259214,#259215,#259216,
#259217,#259218,#259219,#259220,#259221,#259222,#259223,#259224,#259225,
#259226,#259227,#259228,#259229,#259230,#259231,#259232,#259233,#259234,
#259235,#259236,#259237,#259238,#259239,#259240,#259241,#259242,#259243,
#259244,#259245,#259246,#259247,#259248,#259249,#259250,#259251),
 .UNSPECIFIED.,.F.,.F.,(4,3,3,3,3,3,3,3,3,3,3,3,3,3,3,3,3,3,3,3,3,3,3,3,
3,3,3,3,3,3,3,3,3,3,3,3,3,3,3,3,3,3,3,3,3,3,3,3,3,3,3,3,3,3,3,3,3,3,3,3,
3,3,3,3,3,3,3,3,3,3,3,3,3,3,3,3,4),(-54.358231497631,-54.2701712613679,
-54.1821317164641,-54.094091339317,-54.0060286107654,-53.9178668301822,
-53.8296515905965,-53.7412933384214,-53.6821026982924,-53.5934875439491,
-53.5049859428671,-53.416574177426,-53.3255011159179,-53.2371894178138,
-53.148890606905,-53.0605833875811,-52.9722464633841,-52.8838100998141,
-52.7953139517594,-52.7066904296761,-52.687989685361,-52.5993745310178,
-52.5108729299358,-52.4224611644946,-52.3313881029865,-52.2430764048823,
-52.1547775939733,-52.0664703746491,-51.9781334504521,-51.8896970868823,
-51.8012009388273,-51.712577416744,-51.6938766724297,-51.6052615180865,
-51.5167599170046,-51.4283481515637,-51.3372750900555,-51.2489633919514,
-51.1606645810424,-51.0723573617186,-50.9840204375214,-50.8955840739514,
-50.8070879258966,-50.7184644038133,-50.6997636594984,-50.6111485051552,
-50.5226469040735,-50.4342351386325,-50.3431620771243,-50.2548503790201,
-50.1665515681111,-50.0782443487871,-49.98990742459,-49.90147106102,-49.8129749129652,
-49.7243513908818,-49.705650646567,-49.6170354922239,-49.528533891142,-49.4401221257014,
-49.3490490641932,-49.2607373660889,-49.1724385551802,-49.0841313358561,
-48.9957944116597,-48.9073580480896,-48.818861900035,-48.7302383779515,
-48.7115376336357,-48.622510573146,-48.5335985669592,-48.4447807108149,
-48.352347080724,-48.2636567565059,-48.1749951783338,-48.0863334765725,
-48.0750461904514),.UNSPECIFIED.);
#3718=B_SPLINE_CURVE_WITH_KNOTS('',3,(#259253,#259254,#259255,#259256,#259257,
#259258,#259259,#259260,#259261,#259262,#259263,#259264,#259265,#259266,
#259267,#259268,#259269,#259270,#259271,#259272,#259273,#259274,#259275,
#259276,#259277,#259278,#259279,#259280,#259281,#259282,#259283,#259284,
#259285,#259286,#259287,#259288,#259289,#259290,#259291,#259292,#259293,
#259294,#259295,#259296,#259297,#259298,#259299,#259300,#259301,#259302,
#259303,#259304,#259305,#259306,#259307,#259308,#259309,#259310,#259311,
#259312,#259313,#259314,#259315,#259316,#259317,#259318,#259319,#259320,
#259321,#259322,#259323,#259324,#259325,#259326,#259327,#259328,#259329,
#259330,#259331,#259332,#259333,#259334,#259335,#259336,#259337,#259338,
#259339,#259340,#259341,#259342,#259343,#259344,#259345,#259346,#259347,
#259348,#259349,#259350,#259351,#259352,#259353,#259354,#259355,#259356,
#259357,#259358,#259359,#259360,#259361,#259362,#259363,#259364,#259365,
#259366,#259367,#259368,#259369,#259370,#259371,#259372,#259373,#259374,
#259375,#259376,#259377,#259378,#259379,#259380,#259381,#259382,#259383,
#259384,#259385,#259386,#259387,#259388,#259389,#259390,#259391,#259392,
#259393,#259394,#259395,#259396,#259397,#259398,#259399,#259400,#259401,
#259402,#259403,#259404,#259405,#259406,#259407,#259408,#259409,#259410,
#259411,#259412,#259413,#259414,#259415,#259416,#259417,#259418,#259419,
#259420,#259421,#259422,#259423,#259424,#259425,#259426,#259427,#259428,
#259429,#259430,#259431,#259432,#259433,#259434,#259435,#259436,#259437,
#259438,#259439,#259440,#259441,#259442,#259443,#259444,#259445,#259446,
#259447,#259448,#259449,#259450,#259451,#259452,#259453,#259454,#259455,
#259456,#259457,#259458,#259459,#259460,#259461,#259462,#259463,#259464,
#259465,#259466,#259467,#259468,#259469,#259470,#259471,#259472,#259473,
#259474,#259475,#259476,#259477,#259478),.UNSPECIFIED.,.F.,.F.,(4,3,3,3,
3,3,3,3,3,3,3,3,3,3,3,3,3,3,3,3,3,3,3,3,3,3,3,3,3,3,3,3,3,3,3,3,3,3,3,3,
3,3,3,3,3,3,3,3,3,3,3,3,3,3,3,3,3,3,3,3,3,3,3,3,3,3,3,3,3,3,3,3,3,3,3,4),
(-48.075046190225,-47.9745922065697,-47.8736760615069,-47.7721776295322,
-47.7174246207043,-47.6288094663611,-47.5403078652793,-47.4518960998384,
-47.3608230383303,-47.2725113402262,-47.1842125293174,-47.0959053099934,
-47.0075683857966,-46.9191320222266,-46.830635874172,-46.7420123520887,
-46.723311607773,-46.6346964534298,-46.5461948523479,-46.4577830869068,
-46.3667100253987,-46.2783983272945,-46.1900995163857,-46.1017922970616,
-46.0134553728647,-45.9250190092947,-45.8365228612399,-45.7478993391567,
-45.7291985948417,-45.6405834404984,-45.5520818394165,-45.4636700739755,
-45.3725970124673,-45.2842853143631,-45.1959865034543,-45.1076792841302,
-45.0193423599333,-44.9309059963632,-44.8424098483084,-44.7537863262251,
-44.7350855819103,-44.6464704275671,-44.5579688264852,-44.4695570610442,
-44.378483999536,-44.2901723014319,-44.2018734905231,-44.1135662711991,
-44.0252293470023,-43.9367929834323,-43.8482968353776,-43.7596733132943,
-43.740972568979,-43.6523574146358,-43.5638558135539,-43.4754440481129,
-43.3843709866047,-43.2960592885005,-43.2077604775917,-43.1194532582676,
-43.0311163340706,-42.9426799705006,-42.8541838224459,-42.7655603003626,
-42.7468595560476,-42.6587931162129,-42.5708398586021,-42.4829754395242,
-42.3951736725909,-42.3074047672152,-42.2196468586651,-42.1318780954865,
-42.0440227241161,-41.9561233914437,-41.8680841239335,-41.7918608832718),
 .UNSPECIFIED.);
#3719=B_SPLINE_CURVE_WITH_KNOTS('',3,(#259480,#259481,#259482,#259483,#259484,
#259485,#259486,#259487,#259488,#259489,#259490),.UNSPECIFIED.,.F.,.F.,
(4,1,1,1,1,1,1,1,4),(-41.7918608832718,-41.7527465431163,-40.758633530185,
-39.7645205172536,-38.7704075043223,-37.7762944913909,-36.7821814784596,
-35.7880684655282,-35.5086755760922),.UNSPECIFIED.);
#3720=B_SPLINE_CURVE_WITH_KNOTS('',3,(#259492,#259493,#259494,#259495,#259496,
#259497,#259498,#259499,#259500,#259501),.UNSPECIFIED.,.F.,.F.,(4,1,1,1,
1,1,1,4),(-35.5086755760922,-34.7939554525969,-33.7998424396656,-32.8057294267342,
-31.8116164138029,-30.8175034008716,-29.8233903879402,-29.2254902689126),
 .UNSPECIFIED.);
#3721=B_SPLINE_CURVE_WITH_KNOTS('',3,(#259503,#259504,#259505,#259506,#259507,
#259508,#259509,#259510,#259511,#259512),.UNSPECIFIED.,.F.,.F.,(4,1,1,1,
1,1,1,4),(-29.2254902689126,-28.8292773750089,-27.8351643620775,-26.8410513491462,
-25.8469383362148,-24.8528253232835,-23.8587123103522,-22.942304961733),
 .UNSPECIFIED.);
#3722=B_SPLINE_CURVE_WITH_KNOTS('',3,(#259514,#259515,#259516,#259517,#259518,
#259519,#259520,#259521,#259522,#259523,#259524),.UNSPECIFIED.,.F.,.F.,
(4,1,1,1,1,1,1,1,4),(-22.942304961733,-22.8645992974208,-21.8704862844895,
-20.8763732715581,-19.8822602586268,-18.8881472456955,-17.8940342327641,
-16.8999212198328,-16.6591196545534),.UNSPECIFIED.);
#3723=B_SPLINE_CURVE_WITH_KNOTS('',3,(#259526,#259527,#259528,#259529,#259530,
#259531,#259532,#259533,#259534,#259535),.UNSPECIFIED.,.F.,.F.,(4,1,1,1,
1,1,1,4),(-16.6591196545534,-15.9058082069014,-14.9116951939701,-13.9175821810388,
-12.9234691681074,-11.9293561551761,-10.9352431422447,-10.3759343473738),
 .UNSPECIFIED.);
#3724=B_SPLINE_CURVE_WITH_KNOTS('',3,(#259536,#259537,#259538,#259539,#259540,
#259541,#259542,#259543,#259544,#259545),.UNSPECIFIED.,.F.,.F.,(4,1,1,1,
1,1,1,4),(-10.3759343473738,-9.9411301293134,-8.94701711638206,-7.95290410345072,
-6.95879109051938,-5.96467807758804,-4.9705650646567,-4.09274904019424),
 .UNSPECIFIED.);
#3725=B_SPLINE_CURVE_WITH_KNOTS('',3,(#259547,#259548,#259549,#259550,#259551,
#259552,#259553,#259554,#259555,#259556,#259557,#259558,#259559,#259560,
#259561,#259562,#259563,#259564,#259565,#259566,#259567,#259568,#259569,
#259570,#259571,#259572,#259573,#259574,#259575,#259576,#259577,#259578,
#259579,#259580,#259581,#259582,#259583),.UNSPECIFIED.,.F.,.F.,(4,3,3,3,
3,3,3,3,3,3,3,3,4),(109.955742875643,110.032402507957,110.128120593318,
110.223696942156,110.324049264497,110.419388953009,110.514663397292,110.609892664551,
110.705096775639,110.800320560765,110.895553903767,110.990848473115,111.026515520889),
 .UNSPECIFIED.);
#3726=B_SPLINE_CURVE_WITH_KNOTS('',3,(#259585,#259586,#259587,#259588,#259589,
#259590,#259591,#259592,#259593,#259594,#259595,#259596,#259597,#259598,
#259599,#259600,#259601,#259602,#259603,#259604,#259605,#259606,#259607,
#259608,#259609),.UNSPECIFIED.,.F.,.F.,(4,3,3,3,3,3,3,3,4),(-0.549622632142507,
-0.513017594085634,-0.477058007630391,-0.4417375777789,-0.426178763214292,
-0.417876160218151,-0.412493643783751,-0.408624068330263,-0.379508346512894),
 .UNSPECIFIED.);
#3727=B_SPLINE_CURVE_WITH_KNOTS('',3,(#260022,#260023,#260024,#260025,#260026,
#260027,#260028,#260029,#260030,#260031,#260032,#260033,#260034,#260035,
#260036,#260037,#260038,#260039,#260040,#260041,#260042,#260043,#260044,
#260045,#260046,#260047,#260048,#260049,#260050,#260051,#260052,#260053,
#260054,#260055,#260056,#260057,#260058,#260059,#260060,#260061,#260062,
#260063,#260064,#260065,#260066,#260067,#260068,#260069,#260070,#260071,
#260072,#260073,#260074,#260075,#260076,#260077,#260078,#260079,#260080,
#260081,#260082,#260083,#260084,#260085,#260086,#260087,#260088,#260089,
#260090,#260091,#260092,#260093,#260094,#260095,#260096,#260097,#260098,
#260099,#260100,#260101,#260102,#260103,#260104,#260105,#260106,#260107,
#260108,#260109,#260110,#260111,#260112,#260113,#260114,#260115),
 .UNSPECIFIED.,.F.,.F.,(4,3,3,3,3,3,3,3,3,3,3,3,3,3,3,3,3,3,3,3,3,3,3,3,
3,3,3,3,3,3,3,4),(-0.741270768406358,-0.712628874131324,-0.676115879403475,
-0.645170516354468,-0.634510439317648,-0.598376433025019,-0.562201275520222,
-0.552334427207448,-0.544010451928663,-0.537620481368847,-0.502220944134419,
-0.467072958588553,-0.432961270314914,-0.409685081650182,-0.401126444594882,
-0.393612449446962,-0.360002546520967,-0.339856515655984,-0.305586608063842,
-0.281392336058492,-0.269295200055818,-0.261473488331155,-0.257198064053143,
-0.223773286179016,-0.190288603318019,-0.157388277993465,-0.128292725468663,
-0.123232979734184,-0.0910310892017754,-0.0592806646549281,-0.0285050479878524,
0.),.UNSPECIFIED.);
#3728=B_SPLINE_CURVE_WITH_KNOTS('',3,(#260536,#260537,#260538,#260539,#260540,
#260541,#260542,#260543,#260544,#260545,#260546,#260547,#260548,#260549,
#260550,#260551,#260552,#260553,#260554,#260555,#260556,#260557,#260558,
#260559,#260560,#260561,#260562,#260563,#260564,#260565,#260566,#260567,
#260568,#260569,#260570,#260571,#260572,#260573,#260574,#260575,#260576,
#260577,#260578,#260579,#260580,#260581,#260582,#260583,#260584,#260585,
#260586,#260587,#260588,#260589,#260590,#260591,#260592,#260593,#260594,
#260595,#260596,#260597,#260598,#260599,#260600,#260601,#260602,#260603,
#260604,#260605,#260606,#260607,#260608,#260609,#260610,#260611,#260612,
#260613,#260614,#260615,#260616,#260617,#260618,#260619,#260620,#260621,
#260622,#260623,#260624,#260625,#260626),.UNSPECIFIED.,.F.,.F.,(4,3,3,3,
3,3,3,3,3,3,3,3,3,3,3,3,3,3,3,3,3,3,3,3,3,3,3,3,3,3,4),(-0.744397949170608,
-0.721015353144527,-0.689663353689886,-0.660791961248297,-0.655129677496236,
-0.623063100944602,-0.590176459395623,-0.57188783490759,-0.566327003320675,
-0.532731534257962,-0.498780580187938,-0.465742657817175,-0.449223696631794,
-0.440358610599788,-0.433480268257869,-0.432704735446413,-0.397791832207206,
-0.377365240725741,-0.343711753671548,-0.309316447784973,-0.297483911038414,
-0.292610347577743,-0.25715627413548,-0.221728826073117,-0.185872338321595,
-0.15079405380869,-0.145699899549763,-0.108961750383309,-0.0721608531336355,
-0.036054100646489,-9.78674087907486E-15),.UNSPECIFIED.);
#3729=B_SPLINE_CURVE_WITH_KNOTS('',3,(#260681,#260682,#260683,#260684,#260685,
#260686,#260687,#260688,#260689,#260690,#260691,#260692,#260693,#260694,
#260695,#260696,#260697,#260698,#260699,#260700,#260701,#260702,#260703,
#260704,#260705,#260706,#260707,#260708,#260709,#260710,#260711,#260712,
#260713,#260714,#260715,#260716,#260717,#260718,#260719,#260720,#260721,
#260722,#260723,#260724,#260725,#260726,#260727,#260728,#260729,#260730,
#260731,#260732,#260733,#260734,#260735,#260736,#260737,#260738,#260739,
#260740,#260741,#260742,#260743,#260744,#260745,#260746,#260747,#260748,
#260749,#260750,#260751,#260752,#260753,#260754,#260755,#260756,#260757,
#260758,#260759,#260760,#260761,#260762,#260763,#260764,#260765,#260766,
#260767,#260768,#260769,#260770,#260771,#260772,#260773,#260774,#260775,
#260776,#260777,#260778,#260779,#260780,#260781,#260782,#260783,#260784,
#260785,#260786,#260787,#260788,#260789,#260790,#260791,#260792,#260793,
#260794,#260795,#260796,#260797,#260798,#260799,#260800,#260801,#260802,
#260803,#260804,#260805,#260806,#260807,#260808,#260809,#260810,#260811,
#260812,#260813,#260814,#260815,#260816,#260817,#260818,#260819,#260820,
#260821,#260822,#260823,#260824,#260825,#260826,#260827,#260828,#260829,
#260830,#260831,#260832,#260833,#260834,#260835,#260836,#260837,#260838,
#260839,#260840,#260841,#260842,#260843,#260844,#260845,#260846,#260847,
#260848,#260849,#260850,#260851,#260852,#260853,#260854,#260855,#260856,
#260857,#260858,#260859,#260860,#260861,#260862,#260863,#260864,#260865,
#260866,#260867,#260868,#260869,#260870,#260871,#260872,#260873,#260874,
#260875,#260876,#260877,#260878,#260879,#260880,#260881,#260882,#260883,
#260884,#260885,#260886,#260887,#260888,#260889,#260890,#260891,#260892,
#260893,#260894,#260895,#260896,#260897,#260898,#260899,#260900,#260901,
#260902,#260903,#260904,#260905,#260906,#260907,#260908,#260909,#260910,
#260911,#260912,#260913,#260914,#260915,#260916,#260917,#260918),
 .UNSPECIFIED.,.F.,.F.,(4,3,3,3,3,3,3,3,3,3,3,3,3,3,3,3,3,3,3,3,3,3,3,3,
3,3,3,3,3,3,3,3,3,3,3,3,3,3,3,3,3,3,3,3,3,3,3,3,3,3,3,3,3,3,3,3,3,3,3,3,
3,3,3,3,3,3,3,3,3,3,3,3,3,3,3,3,3,3,3,4),(-0.996917990983662,-0.97987983316105,
-0.978871413435325,-0.961116856180621,-0.951587145757447,-0.947910386874838,
-0.928982261184871,-0.90990005817218,-0.905014559890978,-0.901598586961351,
-0.882292182793549,-0.863107350127392,-0.849971152762544,-0.842038908785025,
-0.838710948675444,-0.836834955397696,-0.818300729608859,-0.798949153300391,
-0.782788097020223,-0.778225005840288,-0.774303315136981,-0.754735795630886,
-0.734928220216909,-0.718611340927443,-0.712743439168397,-0.709092797998921,
-0.689172521999581,-0.669660703059046,-0.64998645040343,-0.645862963244773,
-0.642554076823802,-0.622791476319913,-0.60262246477522,-0.589248643053048,
-0.580502223935803,-0.577010713467821,-0.556520757801954,-0.536095573597444,
-0.515863732297644,-0.510831775808524,-0.506523713187674,-0.495631890997843,
-0.476757208574652,-0.475757192304605,-0.455615109588419,-0.446506125233596,
-0.440748198417535,-0.437135126114829,-0.416450924878763,-0.395477580104861,
-0.375263317722426,-0.368809689737484,-0.365367048241743,-0.34417333376397,
-0.323355482063595,-0.314620530575122,-0.30288119489851,-0.297338412534419,
-0.29378483272482,-0.272901128535689,-0.251582427725212,-0.235983519228227,
-0.228246846789718,-0.224656212168728,-0.221044939969769,-0.1994931133928,
-0.177920926015553,-0.15673512369944,-0.15170307566897,-0.148203038640002,
-0.12679115974933,-0.106630188425335,-0.105503598453981,-0.0837818265101803,
-0.0759343988619359,-0.0724446243915576,-0.0506399122259315,-0.028541324462408,
-0.00653824277564539,0.),.UNSPECIFIED.);
#3730=B_SPLINE_CURVE_WITH_KNOTS('',3,(#260926,#260927,#260928,#260929,#260930,
#260931,#260932,#260933,#260934,#260935,#260936,#260937,#260938,#260939,
#260940,#260941,#260942,#260943,#260944,#260945,#260946,#260947,#260948,
#260949,#260950,#260951,#260952,#260953,#260954,#260955,#260956,#260957,
#260958,#260959),.UNSPECIFIED.,.F.,.F.,(4,3,3,3,3,3,3,3,3,3,3,4),(-0.135495685711106,
-0.130764870569518,-0.110890150910476,-0.0911021965626242,-0.0717094166696496,
-0.0636025318400057,-0.0603549952613959,-0.0416129334602128,-0.0231970346481039,
-0.00669672064089262,-0.00531383823267436,0.),.UNSPECIFIED.);
#3731=B_SPLINE_CURVE_WITH_KNOTS('',3,(#260965,#260966,#260967,#260968,#260969,
#260970,#260971,#260972,#260973,#260974,#260975,#260976,#260977,#260978,
#260979,#260980,#260981,#260982,#260983,#260984,#260985,#260986,#260987,
#260988,#260989,#260990,#260991,#260992,#260993,#260994,#260995,#260996,
#260997,#260998,#260999,#261000,#261001,#261002,#261003,#261004,#261005,
#261006,#261007,#261008,#261009,#261010,#261011,#261012,#261013,#261014,
#261015,#261016,#261017,#261018,#261019,#261020,#261021,#261022,#261023,
#261024,#261025,#261026,#261027,#261028,#261029,#261030,#261031,#261032,
#261033,#261034,#261035,#261036,#261037),.UNSPECIFIED.,.F.,.F.,(4,3,3,3,
3,3,3,3,3,3,3,3,3,3,3,3,3,3,3,3,3,3,3,3,4),(10.3761005036881,10.4920608060658,
10.6025246039385,10.7128890189401,10.8231984893798,10.9334973658563,11.0439020613945,
11.154368831279,11.2650249188774,11.3037829227095,11.4156702736963,11.527365113134,
11.6389525957845,11.7504752987031,11.8619757060865,11.973579669562,12.0852315334915,
12.1971014732273,12.3015149226994,12.4130322909134,12.5243820781322,12.6356109379018,
12.746764643097,12.8579360623938,12.962846328138),.UNSPECIFIED.);
#3732=B_SPLINE_CURVE_WITH_KNOTS('',3,(#261040,#261041,#261042,#261043,#261044,
#261045,#261046,#261047,#261048,#261049,#261050,#261051,#261052,#261053,
#261054,#261055,#261056,#261057,#261058,#261059,#261060,#261061,#261062,
#261063,#261064,#261065,#261066,#261067,#261068,#261069,#261070,#261071,
#261072,#261073,#261074,#261075,#261076,#261077,#261078,#261079),
 .UNSPECIFIED.,.F.,.F.,(4,3,3,3,3,3,3,3,3,3,3,3,3,4),(11.6154215191107,
11.7297387352054,11.8440009194378,11.9582350805506,12.072475803645,12.1867576725813,
12.3012123412273,12.4157557152712,12.5305425716753,12.6127553697675,12.7232745471891,
12.8336234769681,12.9438241005833,12.9641212388815),.UNSPECIFIED.);
#3733=B_SPLINE_CURVE_WITH_KNOTS('',3,(#261085,#261086,#261087,#261088,#261089,
#261090,#261091,#261092,#261093,#261094,#261095,#261096,#261097,#261098,
#261099,#261100,#261101,#261102,#261103,#261104,#261105,#261106,#261107,
#261108,#261109,#261110,#261111,#261112,#261113,#261114,#261115,#261116,
#261117,#261118,#261119,#261120,#261121,#261122,#261123,#261124,#261125,
#261126,#261127,#261128,#261129,#261130,#261131,#261132,#261133,#261134,
#261135,#261136,#261137,#261138,#261139,#261140,#261141,#261142,#261143,
#261144,#261145,#261146,#261147,#261148,#261149,#261150,#261151,#261152,
#261153,#261154,#261155,#261156,#261157,#261158,#261159,#261160,#261161,
#261162,#261163,#261164,#261165,#261166,#261167,#261168,#261169,#261170,
#261171,#261172,#261173,#261174,#261175,#261176,#261177,#261178,#261179,
#261180,#261181,#261182,#261183,#261184,#261185,#261186,#261187,#261188,
#261189,#261190,#261191,#261192,#261193,#261194,#261195,#261196,#261197,
#261198,#261199,#261200,#261201,#261202,#261203,#261204,#261205,#261206,
#261207,#261208),.UNSPECIFIED.,.F.,.F.,(4,2,2,2,2,2,2,2,2,2,2,2,2,2,2,2,
2,2,2,2,2,2,2,2,2,2,2,2,2,2,2,2,2,2,2,2,2,2,2,2,2,2,2,2,2,2,2,2,2,2,2,2,
2,2,2,2,2,2,2,2,2,4),(-0.552947915177876,-0.544185360780231,-0.51218218436496,
-0.488189034423349,-0.484648122800509,-0.482446896583355,-0.480732351908997,
-0.47883597676679,-0.475714314137584,-0.464114614355967,-0.419003879019557,
-0.40715830506582,-0.405160537844409,-0.403927534603725,-0.402969700281705,
-0.401860730166516,-0.399880616425001,-0.390353475498068,-0.346512915273737,
-0.331676450249068,-0.328199494079562,-0.326204152709283,-0.324517345195867,
-0.322466289877511,-0.318632060010591,-0.29260268614785,-0.266934087854077,
-0.262655616377667,-0.251362376908043,-0.249392698891025,-0.248167981037694,
-0.247210488374884,-0.246094706241731,-0.244085508640898,-0.234068401248511,
-0.183577356834065,-0.182068791615472,-0.17451174617764,-0.171740812681764,
-0.17010252972066,-0.16841328938821,-0.166217870318622,-0.163797452958358,
-0.159779510990715,-0.15150417860358,-0.106352984611612,-0.095541494497319,
-0.0935956104315449,-0.0923781161284116,-0.0914219328422961,-0.0903032256914169,
-0.088274674515791,-0.0778537337230705,-0.0308276129186543,-0.0202923165647704,
-0.0170438453819075,-0.0149325205532303,-0.013328725997535,-0.0117302233231597,
-0.00985101753289302,-0.00596234470578328,-0.000462250202742447),
 .UNSPECIFIED.);
#3734=B_SPLINE_CURVE_WITH_KNOTS('',3,(#261209,#261210,#261211,#261212,#261213,
#261214,#261215,#261216,#261217,#261218,#261219,#261220,#261221,#261222,
#261223,#261224,#261225,#261226,#261227,#261228,#261229,#261230,#261231,
#261232,#261233,#261234,#261235,#261236,#261237,#261238,#261239,#261240,
#261241,#261242,#261243,#261244,#261245,#261246,#261247,#261248,#261249,
#261250,#261251,#261252,#261253,#261254,#261255,#261256,#261257,#261258,
#261259,#261260,#261261,#261262,#261263,#261264,#261265,#261266,#261267,
#261268,#261269,#261270,#261271,#261272,#261273,#261274,#261275,#261276,
#261277,#261278,#261279,#261280,#261281,#261282,#261283,#261284),
 .UNSPECIFIED.,.F.,.F.,(4,3,3,3,3,3,3,3,3,3,3,3,3,3,3,3,3,3,3,3,3,3,3,3,
3,4),(12.962846328138,13.0741156623616,13.1866812925254,13.2992469226893,
13.4109725593946,13.5224995862497,13.6339156712123,13.7452636982314,13.8565864540708,
13.9680095127458,14.0794784018147,14.1911642428179,14.2969789226792,14.4086941947502,
14.5202114955061,14.6316182494718,14.7429573571259,14.8542716222304,14.9656869401723,
15.0771484850974,15.18882776068,15.2947109226691,15.4175521494668,15.5400015244941,
15.6618361688977,15.7079632676234),.UNSPECIFIED.);
#3735=B_SPLINE_CURVE_WITH_KNOTS('',3,(#261286,#261287,#261288,#261289,#261290,
#261291,#261292,#261293,#261294,#261295,#261296,#261297,#261298,#261299,
#261300,#261301,#261302,#261303,#261304,#261305,#261306,#261307,#261308,
#261309,#261310,#261311,#261312,#261313,#261314,#261315,#261316,#261317,
#261318,#261319,#261320,#261321,#261322,#261323,#261324,#261325,#261326,
#261327,#261328,#261329,#261330,#261331,#261332,#261333,#261334,#261335,
#261336,#261337,#261338,#261339,#261340,#261341,#261342,#261343,#261344,
#261345,#261346,#261347,#261348,#261349,#261350,#261351,#261352,#261353,
#261354,#261355,#261356,#261357,#261358,#261359,#261360,#261361),
 .UNSPECIFIED.,.F.,.F.,(4,3,3,3,3,3,3,3,3,3,3,3,3,3,3,3,3,3,3,3,3,3,3,3,
3,4),(12.9641212388815,13.074229711549,13.1843101652664,13.2944889695355,
13.4047143343461,13.5151543602736,13.6100892204243,13.7219600539943,13.8336321466415,
13.9451931128889,14.0566855716135,14.1681520443355,14.2797163578875,14.3913254608342,
14.5031474993986,14.607423071081,14.7193156410109,14.8310158640507,14.9426088321047,
15.0541371117456,15.1656431768019,15.2772527477869,15.3889102779343,15.5007855451298,
15.6047569217378,15.707963267949),.UNSPECIFIED.);
#3736=B_SPLINE_CURVE_WITH_KNOTS('',3,(#261362,#261363,#261364,#261365,#261366,
#261367,#261368,#261369,#261370,#261371,#261372,#261373,#261374,#261375,
#261376,#261377,#261378,#261379,#261380,#261381,#261382,#261383,#261384,
#261385,#261386,#261387,#261388,#261389,#261390,#261391,#261392,#261393,
#261394,#261395,#261396,#261397,#261398,#261399,#261400,#261401,#261402,
#261403,#261404,#261405,#261406,#261407,#261408,#261409,#261410,#261411,
#261412,#261413,#261414,#261415,#261416,#261417,#261418,#261419,#261420,
#261421,#261422,#261423,#261424,#261425,#261426,#261427,#261428,#261429,
#261430,#261431,#261432,#261433,#261434,#261435,#261436,#261437,#261438,
#261439,#261440,#261441,#261442,#261443,#261444,#261445,#261446,#261447,
#261448,#261449,#261450,#261451,#261452,#261453,#261454,#261455,#261456,
#261457,#261458,#261459,#261460,#261461,#261462,#261463,#261464,#261465,
#261466,#261467,#261468,#261469,#261470,#261471,#261472,#261473,#261474,
#261475,#261476,#261477,#261478,#261479,#261480,#261481),.UNSPECIFIED.,
 .F.,.F.,(4,2,2,2,2,2,2,2,2,2,2,2,2,2,2,2,2,2,2,2,2,2,2,2,2,2,2,2,2,2,2,
2,2,2,2,2,2,2,2,2,2,2,2,2,2,2,2,2,2,2,2,2,2,2,2,2,2,2,2,4),(-1.96129963604252,
-1.93322459695046,-1.9090261506906,-1.90355760708412,-1.90118796758417,
-1.89944226607523,-1.89782450274418,-1.8956133373866,-1.89003323316185,
-1.85580303280489,-1.83565344211002,-1.82866187122417,-1.82566758490452,
-1.82402199023137,-1.82259561103283,-1.8216157956448,-1.82071142512442,
-1.81924560135888,-1.81562210787264,-1.78588026363565,-1.75093023406771,
-1.74691431796691,-1.7448073864601,-1.74307878105252,-1.74107020406526,
-1.73761082759208,-1.72345599400789,-1.67867418663412,-1.66971364432886,
-1.66774729959421,-1.66663025038523,-1.66565665950387,-1.66441033784986,
-1.66235120010726,-1.64943925171088,-1.61610925304974,-1.59705654272514,
-1.59220344036914,-1.58993377696539,-1.58819243396338,-1.58652684445777,
-1.5836832771723,-1.57576054590822,-1.52429907328513,-1.514215372696,-1.5121873348502,
-1.51106001936016,-1.51009182085771,-1.50885150676948,-1.50685253641527,
-1.4952331432125,-1.45022036797864,-1.44246532139049,-1.43684770883712,
-1.43444311549047,-1.43268245335169,-1.43105831068808,-1.4288498238886,
-1.42333489991376,-1.40933590033974),.UNSPECIFIED.);
#3737=B_SPLINE_CURVE_WITH_KNOTS('',3,(#261486,#261487,#261488,#261489,#261490,
#261491,#261492,#261493,#261494,#261495,#261496,#261497,#261498,#261499,
#261500,#261501,#261502,#261503,#261504,#261505,#261506,#261507,#261508,
#261509,#261510,#261511,#261512,#261513,#261514,#261515,#261516,#261517,
#261518,#261519,#261520,#261521,#261522,#261523,#261524,#261525,#261526,
#261527,#261528,#261529,#261530,#261531,#261532,#261533,#261534,#261535,
#261536,#261537,#261538,#261539,#261540,#261541,#261542,#261543,#261544,
#261545,#261546,#261547,#261548,#261549,#261550,#261551,#261552,#261553,
#261554,#261555,#261556,#261557,#261558,#261559,#261560,#261561,#261562,
#261563,#261564,#261565,#261566,#261567,#261568,#261569,#261570,#261571,
#261572,#261573,#261574,#261575,#261576,#261577,#261578,#261579,#261580,
#261581,#261582,#261583,#261584,#261585,#261586,#261587,#261588,#261589,
#261590,#261591,#261592,#261593,#261594,#261595,#261596,#261597,#261598,
#261599,#261600,#261601,#261602,#261603,#261604,#261605,#261606,#261607,
#261608,#261609,#261610,#261611,#261612,#261613,#261614,#261615,#261616,
#261617,#261618,#261619,#261620,#261621,#261622,#261623,#261624,#261625,
#261626,#261627,#261628,#261629,#261630,#261631,#261632,#261633,#261634,
#261635,#261636,#261637,#261638,#261639,#261640,#261641,#261642,#261643,
#261644,#261645,#261646,#261647,#261648,#261649,#261650,#261651,#261652,
#261653,#261654,#261655,#261656,#261657,#261658,#261659,#261660,#261661,
#261662,#261663,#261664,#261665,#261666,#261667,#261668,#261669,#261670,
#261671,#261672,#261673,#261674,#261675,#261676,#261677,#261678,#261679,
#261680,#261681,#261682,#261683,#261684,#261685,#261686,#261687,#261688,
#261689,#261690,#261691,#261692,#261693,#261694,#261695,#261696,#261697),
 .UNSPECIFIED.,.F.,.F.,(4,2,2,2,2,2,2,2,2,2,2,2,2,2,2,2,2,2,2,2,2,2,2,2,
2,2,2,2,2,2,2,2,2,2,2,2,2,2,2,2,2,2,2,2,2,2,2,2,2,2,2,2,2,2,2,2,2,2,2,2,
2,2,2,2,2,2,2,2,2,2,2,2,2,2,2,2,2,2,2,2,2,2,2,2,2,2,2,2,2,2,2,2,2,2,2,2,
2,2,2,2,2,2,2,2,2,4),(-1.53345529214133,-1.50623797145372,-1.49666778590912,
-1.49468562835921,-1.49357646710803,-1.49261903591414,-1.4913873033109,
-1.48939310752656,-1.47761518201257,-1.43260330554539,-1.42091188985495,
-1.41778283896294,-1.41588518144206,-1.41417153561813,-1.41197432624087,
-1.40844567634991,-1.38490781828261,-1.35248790390611,-1.34114977072669,
-1.33907451947209,-1.33794525606482,-1.33698998554753,-1.33578586152309,
-1.33334993757023,-1.310344853583,-1.2899061599334,-1.27425450561612,-1.26484871808546,
-1.26194327849021,-1.26009471117923,-1.25836601744075,-1.2561016813172,
-1.2510516762149,-1.20924808508801,-1.18805524002374,-1.18425774448664,
-1.1828177920521,-1.18182724679977,-1.18092974525103,-1.17945981077153,
-1.17575153961848,-1.15139721764207,-1.12753783981288,-1.11032587436593,
-1.10681802966037,-1.10483714246409,-1.10330500467478,-1.10130388675173,
-1.09779983399027,-1.08256045074441,-1.03823381155214,-1.02954926661654,
-1.02762227042416,-1.02652502296403,-1.02556549711038,-1.0243354515801,
-1.0223030501286,-1.00962660013027,-0.981465851632982,-0.955418973806751,
-0.951842505099802,-0.949630618795421,-0.947914730907127,-0.946023910479201,
-0.942927525326686,-0.931611011768376,-0.886308352535297,-0.874340306264157,
-0.872337154902847,-0.871102528501961,-0.870144544065615,-0.869036673994313,
-0.867061502217166,-0.857616191642048,-0.813726209767829,-0.798870236314403,
-0.795392311394328,-0.793396912446735,-0.791710345148474,-0.789659934860234,
-0.785827972708482,-0.759878407236498,-0.73573378499714,-0.718895547609784,
-0.71653190729292,-0.715326293140029,-0.714370589664715,-0.713241663294021,
-0.711169372215316,-0.699906461945282,-0.672596371774356,-0.644013921137628,
-0.640417241078222,-0.638222962205271,-0.636504372237274,-0.634622911961739,
-0.631569693993843,-0.620721821254798,-0.579982296388231,-0.563188511800519,
-0.560825839195544,-0.559620372967933,-0.558664709612266,-0.557535803543035,
-0.555463048841534,-0.552947915177876),.UNSPECIFIED.);
#3738=B_SPLINE_CURVE_WITH_KNOTS('',3,(#261698,#261699,#261700,#261701,#261702,
#261703,#261704,#261705,#261706,#261707,#261708,#261709,#261710,#261711,
#261712,#261713,#261714,#261715,#261716,#261717,#261718,#261719,#261720,
#261721,#261722,#261723,#261724,#261725,#261726,#261727,#261728,#261729,
#261730,#261731,#261732,#261733,#261734,#261735,#261736,#261737,#261738,
#261739,#261740,#261741,#261742,#261743,#261744,#261745,#261746,#261747,
#261748,#261749,#261750,#261751,#261752,#261753,#261754,#261755,#261756,
#261757,#261758,#261759,#261760,#261761,#261762,#261763,#261764,#261765,
#261766,#261767,#261768,#261769,#261770,#261771,#261772,#261773,#261774,
#261775,#261776,#261777,#261778,#261779,#261780,#261781,#261782,#261783,
#261784,#261785,#261786,#261787,#261788,#261789,#261790,#261791,#261792,
#261793,#261794,#261795,#261796,#261797,#261798,#261799,#261800,#261801,
#261802,#261803,#261804,#261805,#261806,#261807,#261808,#261809,#261810,
#261811,#261812,#261813,#261814,#261815,#261816,#261817,#261818,#261819,
#261820,#261821,#261822,#261823,#261824,#261825,#261826,#261827,#261828,
#261829,#261830,#261831,#261832,#261833,#261834,#261835,#261836,#261837,
#261838,#261839,#261840,#261841,#261842,#261843,#261844,#261845,#261846,
#261847,#261848,#261849,#261850,#261851,#261852,#261853,#261854,#261855,
#261856,#261857,#261858,#261859,#261860,#261861,#261862,#261863,#261864,
#261865,#261866,#261867,#261868,#261869,#261870,#261871,#261872,#261873,
#261874,#261875,#261876,#261877,#261878,#261879,#261880,#261881,#261882,
#261883,#261884,#261885,#261886,#261887,#261888,#261889,#261890,#261891,
#261892,#261893,#261894,#261895,#261896,#261897,#261898,#261899,#261900,
#261901,#261902,#261903,#261904,#261905,#261906,#261907,#261908,#261909,
#261910,#261911,#261912,#261913,#261914,#261915),.UNSPECIFIED.,.F.,.F.,
(4,2,2,2,2,2,2,2,2,2,2,2,2,2,2,2,2,2,2,2,2,2,2,2,2,2,2,2,2,2,2,2,2,2,2,
2,2,2,2,2,2,2,2,2,2,2,2,2,2,2,2,2,2,2,2,2,2,2,2,2,2,2,2,2,2,2,2,2,2,2,2,
2,2,2,2,2,2,2,2,2,2,2,2,2,2,2,2,2,2,2,2,2,2,2,2,2,2,2,2,2,2,2,2,2,2,2,2,
2,4),(-1.40933590033974,-1.36873680763542,-1.3585295663257,-1.35649568484385,
-1.35536757973072,-1.35439904341142,-1.35315934536828,-1.35116510804622,
-1.33967674844955,-1.29469961770618,-1.28279432784207,-1.27962074009993,
-1.27769750463332,-1.27596146396164,-1.27373625854639,-1.27016336466128,
-1.23814508520663,-1.21331869966716,-1.20297950979278,-1.20093602729277,
-1.19980462011342,-1.19883556977395,-1.19759752506688,-1.19560874410812,
-1.18423292999466,-1.18143777472054,-1.15591591349934,-1.12859383792929,
-1.12469958595851,-1.12262087979613,-1.12091336561011,-1.1188957129464,
-1.11538472380333,-1.10043203257075,-1.05614521136344,-1.04723743539541,
-1.04527987709019,-1.04416765471278,-1.04319635058693,-1.04195196528199,
-1.03989695713317,-1.027056953605,-0.997880176508862,-0.98116705413691,
-0.979464544434689,-0.978252858937561,-0.970864183644352,-0.968098869278444,
-0.96644850888878,-0.964700600244288,-0.962384545392156,-0.957279726806057,
-0.936270927248185,-0.905454299305012,-0.900909676879024,-0.891865102368475,
-0.889826008433882,-0.888683586653056,-0.887715908698133,-0.886493631815395,
-0.884012394801899,-0.880756124771468,-0.872893772212155,-0.837816007122391,
-0.817338165789125,-0.813869629521449,-0.811676058826272,-0.809943841679992,
-0.808003155477414,-0.804749381881429,-0.791870709350594,-0.742990370048334,
-0.741753466290543,-0.735729813996039,-0.733936205198346,-0.732859931922798,
-0.731879021678569,-0.73054422929792,-0.727462079000046,-0.723160923480397,
-0.711303092606892,-0.669432121913061,-0.667619483096744,-0.667341765710061,
-0.659690660752527,-0.65688615538079,-0.65522793283421,-0.653483037121117,
-0.651190020334603,-0.646212990405797,-0.62621695233956,-0.598047697932467,
-0.581185010605895,-0.578800751394741,-0.57758203601285,-0.57661443217304,
-0.575468823864746,-0.573358192769217,-0.561655372267942,-0.526779453384891,
-0.506098934002557,-0.502612077937401,-0.500412920864941,-0.498680053227548,
-0.496742563048483,-0.493503517609593,-0.480810991169626,-0.434198512552718,
-0.428921571146853),.UNSPECIFIED.);
#3739=B_SPLINE_CURVE_WITH_KNOTS('',3,(#261921,#261922,#261923,#261924,#261925,
#261926,#261927,#261928,#261929,#261930,#261931,#261932,#261933,#261934,
#261935,#261936,#261937,#261938,#261939,#261940,#261941,#261942,#261943,
#261944,#261945,#261946,#261947,#261948,#261949,#261950,#261951,#261952,
#261953,#261954,#261955,#261956,#261957,#261958,#261959,#261960,#261961,
#261962,#261963,#261964,#261965,#261966,#261967,#261968,#261969,#261970,
#261971,#261972,#261973,#261974,#261975,#261976,#261977,#261978,#261979,
#261980,#261981,#261982,#261983,#261984,#261985,#261986,#261987,#261988,
#261989,#261990,#261991,#261992,#261993,#261994,#261995,#261996,#261997,
#261998,#261999,#262000,#262001,#262002,#262003,#262004,#262005,#262006,
#262007,#262008,#262009,#262010,#262011,#262012,#262013,#262014,#262015,
#262016,#262017,#262018,#262019,#262020,#262021,#262022,#262023,#262024,
#262025,#262026,#262027,#262028,#262029,#262030,#262031,#262032,#262033,
#262034,#262035,#262036,#262037,#262038,#262039,#262040,#262041,#262042,
#262043,#262044),.UNSPECIFIED.,.F.,.F.,(4,2,2,2,2,2,2,2,2,2,2,2,2,2,2,2,
2,2,2,2,2,2,2,2,2,2,2,2,2,2,2,2,2,2,2,2,2,2,2,2,2,2,2,2,2,2,2,2,2,2,2,2,
2,2,2,2,2,2,2,2,2,4),(-0.552653709409288,-0.550934822503833,-0.547405028794108,
-0.545207258145108,-0.543493280814131,-0.541595364287432,-0.53846613981931,
-0.5267775329029,-0.481729369420564,-0.46994011210014,-0.467945010901042,
-0.46671287206948,-0.465755219283742,-0.464645900598761,-0.46266371335701,
-0.453097591169776,-0.409269788252985,-0.394488477298573,-0.391016139527422,
-0.389022179702472,-0.387335801025847,-0.385284363563794,-0.381446703137949,
-0.35523561174603,-0.32750681026561,-0.322387971467438,-0.313884898605568,
-0.311901196140213,-0.310779640832601,-0.309919239757913,-0.308752313056401,
-0.30649950447498,-0.290122486717528,-0.249388147950734,-0.238242756816616,
-0.235034173950901,-0.233118764753075,-0.231579335112055,-0.229495875623519,
-0.225504468525894,-0.190546244543438,-0.160699123481394,-0.157097786116065,
-0.155669865901035,-0.15469034019135,-0.153796305928183,-0.152489736773474,
-0.149128735066113,-0.132602820240614,-0.101780357939939,-0.083511942147516,
-0.0801495186860906,-0.0780022809874654,-0.076293676827951,-0.0743659086835844,
-0.0711015120187754,-0.0577423953078272,-0.0321019381278825,-0.00452335382496099,
-0.00166022821521149,-0.000744519849027736,-0.00046009660915402),
 .UNSPECIFIED.);
#3740=B_SPLINE_CURVE_WITH_KNOTS('',3,(#262045,#262046,#262047,#262048,#262049,
#262050,#262051,#262052,#262053,#262054,#262055,#262056,#262057,#262058,
#262059,#262060,#262061,#262062,#262063,#262064,#262065,#262066,#262067,
#262068,#262069,#262070,#262071,#262072,#262073,#262074,#262075,#262076,
#262077,#262078,#262079,#262080,#262081,#262082,#262083,#262084,#262085,
#262086,#262087,#262088,#262089,#262090,#262091,#262092,#262093,#262094,
#262095,#262096,#262097,#262098,#262099,#262100,#262101,#262102,#262103,
#262104,#262105,#262106,#262107,#262108,#262109,#262110,#262111,#262112,
#262113,#262114,#262115,#262116,#262117,#262118,#262119,#262120,#262121,
#262122,#262123,#262124,#262125,#262126,#262127,#262128,#262129,#262130,
#262131,#262132,#262133,#262134,#262135,#262136,#262137,#262138,#262139,
#262140,#262141,#262142,#262143,#262144,#262145,#262146),.UNSPECIFIED.,
 .F.,.F.,(4,2,2,2,2,2,2,2,2,2,2,2,2,2,2,2,2,2,2,2,2,2,2,2,2,2,2,2,2,2,2,
2,2,2,2,2,2,2,2,2,2,2,2,2,2,2,2,2,2,2,4),(-1.96165355527632,-1.96128010600046,
-1.96037377007412,-1.95941733540217,-1.95810332857501,-1.95512425600224,
-1.95207954611179,-1.94444725734518,-1.89921232004835,-1.88786245187576,
-1.88476387934134,-1.88287303892651,-1.88115798633747,-1.87894837628733,
-1.87537802452049,-1.84431116858309,-1.82192140543595,-1.81275543589084,
-1.80737027036756,-1.80614556930356,-1.80501857608304,-1.8040825641375,
-1.80291378371364,-1.80076355688354,-1.78931212618323,-1.74470211981379,
-1.73237102260667,-1.72918815072057,-1.7272788288345,-1.72556793572463,
-1.7233925084727,-1.71993557794375,-1.69897949826961,-1.65657637973759,
-1.65322925066462,-1.65070000241082,-1.64947745120312,-1.64852093440975,
-1.64740564732197,-1.64544856528959,-1.63729569772236,-1.63183731221877,
-1.60409508856384,-1.57789712492263,-1.57406089061736,-1.57201009130559,
-1.57032417114524,-1.5683306767659,-1.56485895134277,-1.55007789823857,
-1.53345529214133),.UNSPECIFIED.);
#3741=B_SPLINE_CURVE_WITH_KNOTS('',3,(#262148,#262149,#262150,#262151,#262152,
#262153,#262154,#262155,#262156,#262157,#262158,#262159,#262160,#262161,
#262162,#262163,#262164,#262165,#262166,#262167,#262168,#262169,#262170,
#262171,#262172,#262173,#262174,#262175,#262176,#262177,#262178,#262179,
#262180,#262181,#262182,#262183,#262184,#262185,#262186,#262187,#262188,
#262189,#262190,#262191,#262192,#262193,#262194,#262195,#262196,#262197,
#262198,#262199,#262200,#262201,#262202,#262203,#262204,#262205,#262206,
#262207,#262208,#262209,#262210,#262211,#262212,#262213,#262214,#262215,
#262216,#262217,#262218,#262219,#262220,#262221,#262222,#262223,#262224,
#262225,#262226,#262227,#262228,#262229,#262230,#262231,#262232,#262233,
#262234,#262235,#262236,#262237,#262238,#262239,#262240,#262241,#262242,
#262243,#262244,#262245,#262246,#262247,#262248,#262249,#262250,#262251,
#262252,#262253),.UNSPECIFIED.,.F.,.F.,(4,2,2,2,2,2,2,2,2,2,2,2,2,2,2,2,
2,2,2,2,2,2,2,2,2,2,2,2,2,2,2,2,2,2,2,2,2,2,2,2,2,2,2,2,2,2,2,2,2,2,2,2,
4),(-0.428921571146853,-0.424968544272072,-0.423096680319819,-0.421893996806391,
-0.420927011708669,-0.419767688591699,-0.417593267307482,-0.404361768701686,
-0.381549437142564,-0.35064637422367,-0.347048400612306,-0.344815597620563,
-0.343078564875199,-0.341159259207509,-0.338003792436699,-0.32630806445896,
-0.281150145284207,-0.269550144429268,-0.267549813665198,-0.266308018734925,
-0.265338489465567,-0.264209536185,-0.262177053892415,-0.25210323750283,
-0.200666519410322,-0.200289359103597,-0.192673510277237,-0.189874020243945,
-0.188216647291982,-0.18647110261026,-0.184220426432803,-0.179424127296979,
-0.173032303496688,-0.15690065245941,-0.133259132557622,-0.114222170209687,
-0.111813215884357,-0.110589165303511,-0.109621141039482,-0.108479501081243,
-0.106387686775185,-0.0952531048343403,-0.0779269994880584,-0.0597811234362074,
-0.0391189537714606,-0.0356304489188435,-0.0334306158212738,-0.0316974428853265,
-0.0300771657471151,-0.0281751615843451,-0.025434668570542,-0.0175897605599473,
-0.000459285835135901),.UNSPECIFIED.);
#3742=B_SPLINE_CURVE_WITH_KNOTS('',3,(#262254,#262255,#262256,#262257,#262258,
#262259,#262260,#262261,#262262,#262263,#262264,#262265,#262266,#262267,
#262268,#262269,#262270,#262271,#262272,#262273,#262274,#262275,#262276,
#262277,#262278,#262279,#262280,#262281,#262282,#262283,#262284,#262285,
#262286,#262287,#262288,#262289,#262290,#262291,#262292,#262293,#262294,
#262295,#262296,#262297,#262298,#262299,#262300,#262301,#262302,#262303,
#262304,#262305,#262306,#262307,#262308,#262309,#262310,#262311,#262312,
#262313,#262314,#262315,#262316,#262317,#262318,#262319,#262320,#262321,
#262322,#262323,#262324,#262325,#262326,#262327,#262328,#262329,#262330,
#262331,#262332,#262333,#262334,#262335,#262336,#262337,#262338,#262339,
#262340,#262341,#262342,#262343,#262344,#262345,#262346,#262347,#262348,
#262349,#262350,#262351,#262352,#262353,#262354,#262355,#262356,#262357,
#262358,#262359,#262360,#262361,#262362,#262363,#262364,#262365,#262366,
#262367,#262368,#262369,#262370,#262371,#262372,#262373),.UNSPECIFIED.,
 .F.,.F.,(4,2,2,2,2,2,2,2,2,2,2,2,2,2,2,2,2,2,2,2,2,2,2,2,2,2,2,2,2,2,2,
2,2,2,2,2,2,2,2,2,2,2,2,2,2,2,2,2,2,2,2,2,2,2,2,2,2,2,2,4),(-1.96149836071343,
-1.92271697299584,-1.91960104043406,-1.91790458130877,-1.91642579372871,
-1.91541861373057,-1.91451326294395,-1.91304322816939,-1.90939552210831,
-1.88016061636188,-1.86415767440557,-1.85094536952365,-1.84260982058666,
-1.83988874093019,-1.8382689185902,-1.83653642994018,-1.83433868182765,
-1.8308558747775,-1.81005008463793,-1.7752563031124,-1.76356935314919,-1.76145590270137,
-1.76030977540865,-1.75934233407634,-1.75812458796808,-1.75574446675404,
-1.73909577528902,-1.69825012629792,-1.69113945576909,-1.68588603616201,
-1.68354306811159,-1.68179083098752,-1.68014800712977,-1.67787238156269,
-1.67196005164735,-1.61792822148563,-1.60773957345381,-1.60570468501316,
-1.60457535979885,-1.60360611873077,-1.60236548545786,-1.60036855329615,
-1.58883024159793,-1.54377745127124,-1.5319719637818,-1.52880727803495,
-1.52688616304685,-1.52514993877195,-1.52292158830651,-1.51933774374819,
-1.48744873071576,-1.46248216436062,-1.45211120408237,-1.45006648609837,
-1.44893507689342,-1.44796615095104,-1.44672863406259,-1.44474190912332,
-1.43341386242247,-1.40942950879856),.UNSPECIFIED.);
#3743=B_SPLINE_CURVE_WITH_KNOTS('',3,(#262378,#262379,#262380,#262381,#262382,
#262383,#262384,#262385,#262386,#262387,#262388,#262389,#262390,#262391,
#262392,#262393,#262394,#262395,#262396,#262397,#262398,#262399,#262400,
#262401,#262402,#262403,#262404,#262405,#262406,#262407,#262408,#262409,
#262410,#262411,#262412,#262413,#262414,#262415,#262416,#262417,#262418,
#262419,#262420,#262421,#262422,#262423,#262424,#262425,#262426,#262427,
#262428,#262429,#262430,#262431,#262432,#262433,#262434,#262435,#262436,
#262437,#262438,#262439,#262440,#262441,#262442,#262443,#262444,#262445,
#262446,#262447,#262448,#262449,#262450,#262451,#262452,#262453,#262454,
#262455,#262456,#262457,#262458,#262459,#262460,#262461,#262462,#262463,
#262464,#262465,#262466,#262467,#262468,#262469,#262470,#262471,#262472,
#262473,#262474,#262475,#262476,#262477,#262478,#262479,#262480,#262481,
#262482,#262483,#262484,#262485,#262486,#262487,#262488,#262489,#262490,
#262491,#262492,#262493,#262494,#262495,#262496,#262497,#262498,#262499,
#262500,#262501,#262502,#262503,#262504,#262505,#262506,#262507,#262508,
#262509,#262510,#262511,#262512,#262513,#262514,#262515,#262516,#262517,
#262518,#262519,#262520,#262521,#262522,#262523,#262524,#262525,#262526,
#262527,#262528,#262529,#262530,#262531,#262532,#262533,#262534,#262535,
#262536,#262537,#262538,#262539,#262540,#262541,#262542,#262543,#262544,
#262545,#262546,#262547,#262548,#262549,#262550,#262551,#262552,#262553,
#262554,#262555,#262556,#262557,#262558,#262559,#262560,#262561,#262562,
#262563,#262564,#262565,#262566,#262567,#262568,#262569,#262570,#262571,
#262572,#262573,#262574,#262575,#262576,#262577,#262578,#262579,#262580,
#262581,#262582,#262583),.UNSPECIFIED.,.F.,.F.,(4,2,2,2,2,2,2,2,2,2,2,2,
2,2,2,2,2,2,2,2,2,2,2,2,2,2,2,2,2,2,2,2,2,2,2,2,2,2,2,2,2,2,2,2,2,2,2,2,
2,2,2,2,2,2,2,2,2,2,2,2,2,2,2,2,2,2,2,2,2,2,2,2,2,2,2,2,2,2,2,2,2,2,2,2,
2,2,2,2,2,2,2,2,2,2,2,2,2,2,2,2,2,2,4),(-1.53294839269393,-1.50715734523062,
-1.48668724489829,-1.4816758773482,-1.47939465594995,-1.47767027686247,
-1.47604022894185,-1.47330474693597,-1.46597263665537,-1.41374072859881,
-1.40364410062386,-1.4016324867234,-1.40051717230878,-1.39956091068862,
-1.39833905531885,-1.39637695301433,-1.38521249522548,-1.38244504690862,
-1.34959390755089,-1.33072532617322,-1.32592095734334,-1.32367773379579,
-1.32195852775607,-1.32031565367334,-1.31751509766915,-1.30974277351457,
-1.30797781676012,-1.25797364547037,-1.24798058889317,-1.24597441216338,
-1.24486013750876,-1.24390353070443,-1.24267963587142,-1.24071119407982,
-1.2294215704208,-1.22668281973664,-1.19962855385,-1.17351002101486,-1.16967568867581,
-1.16762531210876,-1.1659394357966,-1.16394563596818,-1.16047247386088,
-1.14567057439514,-1.10181325983102,-1.09228109449825,-1.09030120905274,
-1.08919255459757,-1.08823507183336,-1.08700263701566,-1.08500606819549,
-1.07325956921364,-1.02828099408303,-1.01653906455637,-1.01340564261391,
-1.0115070372706,-1.00979362891146,-1.00759824343698,-1.00407561873939,
-0.980768739722173,-0.954884476788388,-0.950053569025437,-0.937105811619782,
-0.935063438540616,-0.933830675246918,-0.932871113526241,-0.931776216740182,
-0.92985886788984,-0.921310620840032,-0.876942796516238,-0.861653696028039,
-0.858146845057731,-0.856145448493659,-0.854613791152804,-0.852634339012002,
-0.849131446379631,-0.83199966912809,-0.783915984485502,-0.779978693174232,
-0.778471939679158,-0.777567489192838,-0.776583615037072,-0.775177396041581,
-0.771600516677463,-0.752865078406153,-0.73333833051738,-0.706706901799627,
-0.703126505516105,-0.700913659570756,-0.699197918855124,-0.697308159985908,
-0.694215565435119,-0.682936551839584,-0.642532950543339,-0.625927156810066,
-0.62356833656366,-0.622363885242111,-0.621408456664485,-0.620279119339662,
-0.618204034303994,-0.606873328468868,-0.574502497876915,-0.552653709409288),
 .UNSPECIFIED.);
#3744=B_SPLINE_CURVE_WITH_KNOTS('',3,(#262584,#262585,#262586,#262587,#262588,
#262589,#262590,#262591,#262592,#262593,#262594,#262595,#262596,#262597,
#262598,#262599,#262600,#262601,#262602,#262603,#262604,#262605,#262606,
#262607,#262608,#262609,#262610,#262611,#262612,#262613,#262614,#262615,
#262616,#262617,#262618,#262619,#262620,#262621,#262622,#262623,#262624,
#262625,#262626,#262627,#262628,#262629,#262630,#262631,#262632,#262633,
#262634,#262635,#262636,#262637,#262638,#262639,#262640,#262641,#262642,
#262643,#262644,#262645,#262646,#262647,#262648,#262649,#262650,#262651,
#262652,#262653,#262654,#262655,#262656,#262657,#262658,#262659,#262660,
#262661,#262662,#262663,#262664,#262665,#262666,#262667,#262668,#262669,
#262670,#262671,#262672,#262673,#262674,#262675,#262676,#262677,#262678,
#262679,#262680,#262681,#262682,#262683,#262684,#262685,#262686,#262687,
#262688,#262689,#262690,#262691,#262692,#262693,#262694,#262695,#262696,
#262697,#262698,#262699,#262700,#262701,#262702,#262703,#262704,#262705,
#262706,#262707,#262708,#262709,#262710,#262711,#262712,#262713,#262714,
#262715,#262716,#262717,#262718,#262719,#262720,#262721,#262722,#262723,
#262724,#262725,#262726,#262727,#262728,#262729,#262730,#262731,#262732,
#262733,#262734,#262735,#262736,#262737,#262738,#262739,#262740,#262741,
#262742,#262743,#262744,#262745,#262746,#262747,#262748,#262749,#262750,
#262751,#262752,#262753,#262754,#262755,#262756,#262757,#262758,#262759,
#262760,#262761,#262762,#262763,#262764,#262765,#262766,#262767,#262768,
#262769,#262770,#262771,#262772,#262773,#262774,#262775,#262776,#262777,
#262778,#262779,#262780,#262781,#262782,#262783,#262784,#262785,#262786,
#262787,#262788,#262789,#262790,#262791,#262792,#262793,#262794,#262795,
#262796,#262797,#262798,#262799),.UNSPECIFIED.,.F.,.F.,(4,2,2,2,2,2,2,2,
2,2,2,2,2,2,2,2,2,2,2,2,2,2,2,2,2,2,2,2,2,2,2,2,2,2,2,2,2,2,2,2,2,2,2,2,
2,2,2,2,2,2,2,2,2,2,2,2,2,2,2,2,2,2,2,2,2,2,2,2,2,2,2,2,2,2,2,2,2,2,2,2,
2,2,2,2,2,2,2,2,2,2,2,2,2,2,2,2,2,2,2,2,2,2,2,2,2,2,2,4),(-1.40942950879856,
-1.38861304144377,-1.3805496856759,-1.3747588546159,-1.37232289813186,-1.37055470453129,
-1.36893428696517,-1.36674707004159,-1.36136802938653,-1.32359918641245,
-1.307615493727,-1.29653270004572,-1.29445141793771,-1.29331214353993,-1.29234406177558,
-1.29111731126272,-1.28916612026667,-1.27854639235415,-1.27547356077125,
-1.24707539963117,-1.22428477842012,-1.21896208020509,-1.21660657626528,
-1.21485211020589,-1.21321235319538,-1.21050430842141,-1.20348138814874,
-1.1509089609167,-1.14077693624782,-1.1387449826738,-1.13761620192476,-1.13664674754946,
-1.13540496053058,-1.13340447718157,-1.12179763315987,-1.07665166829597,
-1.06498116947726,-1.06182806854527,-1.05990934406415,-1.05817228176482,
-1.05593866417192,-1.0523377462319,-1.02128847038156,-0.99921439171761,
-0.985397129056081,-0.983201275189535,-0.982037445569841,-0.981070650166951,
-0.979873115810151,-0.977515138225075,-0.956979575243179,-0.938135400528358,
-0.910909014803633,-0.90729617743362,-0.905058954014673,-0.903321407828912,
-0.901404498864463,-0.898259780108079,-0.886684572504042,-0.841450435640829,
-0.829790584165557,-0.827787253034824,-0.826544573236164,-0.825574986912447,
-0.824446694325688,-0.822417213456583,-0.812330511145004,-0.760740033014283,
-0.752959322364347,-0.750135735503812,-0.748473717906294,-0.746730245202018,
-0.744448107644155,-0.739530395502785,-0.719993577785478,-0.700304479201148,
-0.692744829615634,-0.674444666114828,-0.672045364984539,-0.67082338417009,
-0.669855511404987,-0.668712308239237,-0.666613144512317,-0.655160907085027,
-0.622128985326625,-0.599423901356696,-0.595888446229588,-0.593674532367159,
-0.591939897877407,-0.590010619389462,-0.586809317585552,-0.574578533715085,
-0.529755859061051,-0.518434217679464,-0.51644361040841,-0.515204813006902,
-0.514235625642115,-0.51310475904775,-0.511063140776853,-0.500753665586637,
-0.47607771616976,-0.443850004213923,-0.440268275712005,-0.438040324966765,
-0.436303864748369,-0.434381930471452,-0.431214606924753,-0.428814745063029),
 .UNSPECIFIED.);
#3745=B_SPLINE_CURVE_WITH_KNOTS('',3,(#262805,#262806,#262807,#262808,#262809,
#262810,#262811,#262812,#262813,#262814,#262815,#262816,#262817,#262818,
#262819,#262820,#262821,#262822,#262823,#262824,#262825,#262826,#262827,
#262828,#262829,#262830,#262831,#262832,#262833,#262834,#262835,#262836,
#262837,#262838,#262839,#262840,#262841,#262842,#262843,#262844,#262845,
#262846,#262847,#262848,#262849,#262850,#262851,#262852,#262853,#262854,
#262855,#262856,#262857,#262858,#262859,#262860,#262861,#262862,#262863,
#262864,#262865,#262866,#262867,#262868,#262869,#262870,#262871,#262872,
#262873,#262874,#262875,#262876,#262877,#262878,#262879,#262880,#262881,
#262882,#262883,#262884,#262885,#262886,#262887,#262888,#262889,#262890,
#262891,#262892,#262893,#262894,#262895,#262896,#262897,#262898,#262899,
#262900,#262901,#262902,#262903,#262904,#262905,#262906,#262907,#262908,
#262909,#262910,#262911,#262912,#262913,#262914,#262915,#262916,#262917,
#262918,#262919,#262920,#262921,#262922,#262923,#262924,#262925,#262926),
 .UNSPECIFIED.,.F.,.F.,(4,2,2,2,2,2,2,2,2,2,2,2,2,2,2,2,2,2,2,2,2,2,2,2,
2,2,2,2,2,2,2,2,2,2,2,2,2,2,2,2,2,2,2,2,2,2,2,2,2,2,2,2,2,2,2,2,2,2,2,2,
4),(-0.552689914471559,-0.53888975115974,-0.532400108143506,-0.53057076666574,
-0.529495072958845,-0.528530748836056,-0.527241537949452,-0.524360496763293,
-0.500036481612907,-0.46049347862675,-0.455179566002614,-0.453076441484597,
-0.451331350094738,-0.449544166024695,-0.446927402124816,-0.439839691691527,
-0.393568916420078,-0.3875384594585,-0.377187470630721,-0.375265767096169,
-0.374055704787414,-0.373099738071941,-0.371974335989141,-0.369918198958697,
-0.35898666783065,-0.331102666900535,-0.302707803616355,-0.299120914999867,
-0.296929560985358,-0.29521142880357,-0.293328599113484,-0.290268957309992,
-0.279352349096004,-0.238664867078956,-0.22189840475082,-0.219536406979483,
-0.21833108152658,-0.217375353232618,-0.216246123470924,-0.214172428977807,
-0.2028803267417,-0.170783060116345,-0.146910877916098,-0.143364167456997,
-0.141161004349836,-0.139508402273642,-0.137696628212653,-0.134811841798616,
-0.131396197404177,-0.124813631756402,-0.107873719505434,-0.0796227569997071,
-0.0767218008853527,-0.0658347608184948,-0.0638852368526337,-0.0626667194880947,
-0.0617100942006382,-0.0605908994118284,-0.0585636874731907,-0.0481976612391398,
-0.000460427453030607),.UNSPECIFIED.);
#3746=B_SPLINE_CURVE_WITH_KNOTS('',3,(#262927,#262928,#262929,#262930,#262931,
#262932,#262933,#262934,#262935,#262936,#262937,#262938,#262939,#262940,
#262941,#262942,#262943,#262944,#262945,#262946,#262947,#262948,#262949,
#262950,#262951,#262952,#262953,#262954,#262955,#262956,#262957,#262958,
#262959,#262960,#262961,#262962,#262963,#262964,#262965,#262966,#262967,
#262968,#262969,#262970,#262971,#262972,#262973,#262974,#262975,#262976,
#262977,#262978,#262979,#262980,#262981,#262982,#262983,#262984,#262985,
#262986,#262987,#262988,#262989,#262990,#262991,#262992,#262993,#262994,
#262995,#262996,#262997,#262998,#262999,#263000,#263001,#263002,#263003,
#263004,#263005,#263006,#263007,#263008,#263009,#263010,#263011,#263012,
#263013,#263014,#263015,#263016,#263017,#263018,#263019,#263020,#263021,
#263022,#263023,#263024,#263025,#263026,#263027,#263028,#263029,#263030,
#263031,#263032,#263033,#263034,#263035,#263036,#263037,#263038,#263039,
#263040,#263041,#263042,#263043,#263044,#263045,#263046,#263047,#263048,
#263049,#263050,#263051,#263052,#263053,#263054,#263055,#263056,#263057,
#263058,#263059,#263060,#263061,#263062),.UNSPECIFIED.,.F.,.F.,(4,2,2,2,
2,2,2,2,2,2,2,2,2,2,2,2,2,2,2,2,2,2,2,2,2,2,2,2,2,2,2,2,2,2,2,2,2,2,2,2,
2,2,2,2,2,2,2,2,2,2,2,2,2,2,2,2,2,2,2,2,2,2,2,2,2,2,2,4),(-1.96089412384933,
-1.95111155903107,-1.94850265213132,-1.94666474488551,-1.94507028877428,
-1.9433521571946,-1.94114768953157,-1.93641752020172,-1.92503904424038,
-1.88056367329849,-1.87034626162354,-1.86832878004811,-1.86721252977914,
-1.8662569084715,-1.86503773012088,-1.86308347264384,-1.85206509827071,
-1.83770757676361,-1.80870865413596,-1.79963963372712,-1.79535436650305,
-1.79187633694713,-1.78992194540447,-1.78990221780106,-1.78988203700657,
-1.7898677157285,-1.78985186170132,-1.78983431069918,-1.78981488097315,
-1.78979337143355,-1.78976955968104,-1.78974319987673,-1.78971402044014,
-1.78968172115807,-1.78964597111424,-1.78960640794046,-1.78956446585443,
-1.78791900619621,-1.78572815867446,-1.78221788674665,-1.75932877422693,
-1.72636109176316,-1.71494864461973,-1.71287105704267,-1.71174179620534,
-1.71078729155849,-1.70958510123825,-1.7071562035258,-1.68692282854521,
-1.65794663861193,-1.64602253305327,-1.64083169258486,-1.63674192889211,
-1.63463932995941,-1.63293582499214,-1.63098058859212,-1.62767255291511,
-1.61509178296851,-1.56899740250181,-1.55923719541135,-1.55724485420481,
-1.55613389366973,-1.55517737605739,-1.55395002106763,-1.5519691191632,
-1.5404106693462,-1.53736271093113,-1.53294839269393),.UNSPECIFIED.);
#3747=B_SPLINE_CURVE_WITH_KNOTS('',3,(#263064,#263065,#263066,#263067,#263068,
#263069,#263070,#263071,#263072,#263073,#263074,#263075,#263076,#263077,
#263078,#263079,#263080,#263081,#263082,#263083,#263084,#263085,#263086,
#263087,#263088,#263089,#263090,#263091,#263092,#263093,#263094,#263095,
#263096,#263097,#263098,#263099,#263100,#263101,#263102,#263103,#263104,
#263105,#263106,#263107,#263108,#263109,#263110,#263111,#263112,#263113,
#263114,#263115,#263116,#263117,#263118,#263119,#263120,#263121,#263122,
#263123,#263124,#263125,#263126,#263127,#263128,#263129,#263130,#263131,
#263132,#263133,#263134,#263135,#263136,#263137,#263138,#263139,#263140,
#263141,#263142,#263143,#263144,#263145,#263146,#263147,#263148,#263149,
#263150,#263151,#263152,#263153),.UNSPECIFIED.,.F.,.F.,(4,2,2,2,2,2,2,2,
2,2,2,2,2,2,2,2,2,2,2,2,2,2,2,2,2,2,2,2,2,2,2,2,2,2,2,2,2,2,2,2,2,2,2,2,
4),(-0.428814745063029,-0.419384051194465,-0.374312020670882,-0.362775961472799,
-0.36077873576139,-0.359537869855122,-0.358568407715106,-0.35743877054547,
-0.355403202231188,-0.345207637561813,-0.290954712936072,-0.285204544328501,
-0.282954478113407,-0.281317974791492,-0.279561106527703,-0.277192082929494,
-0.271793780344759,-0.264429701809189,-0.223841863174784,-0.207338123235077,
-0.204962172166002,-0.20374509890667,-0.20277741881434,-0.201630092163345,
-0.19951204909479,-0.187724636868222,-0.152155857672964,-0.132184242199741,
-0.128732946806886,-0.126544347386178,-0.124812314167515,-0.123191179605364,
-0.120452161792452,-0.111970009384296,-0.098435349243074,-0.0827281159732794,
-0.0536547568499099,-0.0499956923219941,-0.0485234403619077,-0.0476174481053444,
-0.0466102462583693,-0.0451326359295614,-0.0434381365216323,-0.0403279468249156,
-0.000459537648819321),.UNSPECIFIED.);
#3748=B_SPLINE_CURVE_WITH_KNOTS('',3,(#263154,#263155,#263156,#263157,#263158,
#263159,#263160,#263161,#263162,#263163,#263164,#263165,#263166,#263167,
#263168,#263169,#263170,#263171,#263172,#263173,#263174,#263175,#263176,
#263177,#263178,#263179,#263180,#263181,#263182,#263183,#263184,#263185,
#263186,#263187,#263188,#263189,#263190,#263191,#263192,#263193,#263194,
#263195,#263196,#263197,#263198,#263199,#263200,#263201,#263202,#263203,
#263204,#263205,#263206,#263207,#263208,#263209,#263210,#263211,#263212,
#263213,#263214,#263215,#263216,#263217,#263218,#263219,#263220,#263221,
#263222,#263223,#263224,#263225,#263226,#263227,#263228,#263229,#263230,
#263231,#263232,#263233,#263234,#263235,#263236,#263237,#263238,#263239,
#263240,#263241,#263242,#263243,#263244,#263245,#263246,#263247,#263248,
#263249,#263250,#263251,#263252,#263253,#263254,#263255,#263256,#263257,
#263258,#263259,#263260,#263261,#263262,#263263,#263264,#263265,#263266,
#263267,#263268,#263269,#263270,#263271,#263272,#263273,#263274,#263275,
#263276,#263277,#263278,#263279,#263280,#263281,#263282,#263283,#263284,
#263285,#263286,#263287,#263288,#263289,#263290,#263291,#263292,#263293,
#263294,#263295,#263296,#263297,#263298,#263299,#263300,#263301,#263302,
#263303,#263304,#263305,#263306,#263307,#263308,#263309,#263310,#263311),
 .UNSPECIFIED.,.F.,.F.,(4,2,2,2,2,2,2,2,2,2,2,2,2,2,2,2,2,2,2,2,2,2,2,2,
2,2,2,2,2,2,2,2,2,2,2,2,2,2,2,2,2,2,2,2,2,2,2,2,2,2,2,2,2,2,2,2,2,2,2,2,
2,2,2,2,2,2,2,2,2,2,2,2,2,2,2,2,2,2,4),(-1.96138640067636,-1.93753988811331,
-1.9347858843805,-1.93287862975556,-1.93125818038573,-1.92952663419017,
-1.92733775711206,-1.9238842242701,-1.90383011118708,-1.88467208175021,
-1.86572224418153,-1.85636031406122,-1.85436653906471,-1.85324635290098,
-1.85227621783515,-1.85102302911827,-1.84898360871115,-1.83653863245051,
-1.82420793444266,-1.79657328911591,-1.78645659687477,-1.78181289121297,
-1.77810059683376,-1.77606922209948,-1.77605156459095,-1.77603352605037,
-1.77601509612071,-1.77599626412166,-1.77597701903074,-1.77595734947769,
-1.77593724373396,-1.77591668969965,-1.7759017153278,-1.77588518123298,
-1.77586692113158,-1.77584675032292,-1.77582446354924,-1.77579983260114,
-1.77577260364895,-1.77574249427717,-1.7740117003386,-1.77183040437884,
-1.76840188487783,-1.74903144906365,-1.71113565698982,-1.70087873320262,
-1.69883710164232,-1.69770643395865,-1.6967375404316,-1.69549928731661,
-1.69350989305837,-1.68220373273009,-1.63742324512692,-1.62518482147105,
-1.62198345743502,-1.62005446898891,-1.61832030215597,-1.61610727052186,
-1.61257376540291,-1.58992043060127,-1.55553128405715,-1.54525395501303,
-1.54321451878416,-1.54208435228591,-1.54111544178994,-1.53987659062665,
-1.53788513192151,-1.52645427305035,-1.48153987435252,-1.46952895738865,
-1.46634695382225,-1.46442227887355,-1.46268729179309,-1.46046671294052,
-1.45690796299239,-1.43330769607406,-1.42727426603096,-1.41101453606077,
-1.40924613825003),.UNSPECIFIED.);
#3749=B_SPLINE_CURVE_WITH_KNOTS('',3,(#263316,#263317,#263318,#263319,#263320,
#263321,#263322,#263323,#263324,#263325,#263326,#263327,#263328,#263329,
#263330,#263331,#263332,#263333,#263334,#263335,#263336,#263337,#263338,
#263339,#263340,#263341,#263342,#263343,#263344,#263345,#263346,#263347,
#263348,#263349,#263350,#263351,#263352,#263353,#263354,#263355,#263356,
#263357,#263358,#263359,#263360,#263361,#263362,#263363,#263364,#263365,
#263366,#263367,#263368,#263369,#263370,#263371,#263372,#263373,#263374,
#263375,#263376,#263377,#263378,#263379,#263380,#263381,#263382,#263383,
#263384,#263385,#263386,#263387,#263388,#263389,#263390,#263391,#263392,
#263393,#263394,#263395,#263396,#263397,#263398,#263399,#263400,#263401,
#263402,#263403,#263404,#263405,#263406,#263407,#263408,#263409,#263410,
#263411,#263412,#263413,#263414,#263415,#263416,#263417,#263418,#263419,
#263420,#263421,#263422,#263423,#263424,#263425,#263426,#263427,#263428,
#263429,#263430,#263431,#263432,#263433,#263434,#263435,#263436,#263437,
#263438,#263439,#263440,#263441,#263442,#263443,#263444,#263445,#263446,
#263447,#263448,#263449,#263450,#263451,#263452,#263453,#263454,#263455,
#263456,#263457,#263458,#263459,#263460,#263461,#263462,#263463,#263464,
#263465,#263466,#263467,#263468,#263469,#263470,#263471,#263472,#263473,
#263474,#263475,#263476,#263477,#263478,#263479,#263480,#263481,#263482,
#263483,#263484,#263485,#263486,#263487,#263488,#263489,#263490,#263491,
#263492,#263493,#263494,#263495,#263496,#263497,#263498,#263499,#263500,
#263501,#263502,#263503,#263504,#263505,#263506,#263507,#263508,#263509,
#263510,#263511,#263512,#263513,#263514,#263515,#263516,#263517),
 .UNSPECIFIED.,.F.,.F.,(4,2,2,2,2,2,2,2,2,2,2,2,2,2,2,2,2,2,2,2,2,2,2,2,
2,2,2,2,2,2,2,2,2,2,2,2,2,2,2,2,2,2,2,2,2,2,2,2,2,2,2,2,2,2,2,2,2,2,2,2,
2,2,2,2,2,2,2,2,2,2,2,2,2,2,2,2,2,2,2,2,2,2,2,2,2,2,2,2,2,2,2,2,2,2,2,2,
2,2,2,2,4),(-1.53330080949059,-1.52159254796867,-1.47664759525897,-1.4669630218542,
-1.46497434560148,-1.46386384845335,-1.46290672904625,-1.46167730197349,
-1.4596905378569,-1.44804080654177,-1.44471429391727,-1.41574532421974,
-1.40017750437384,-1.39080676414814,-1.38790533353725,-1.38605774495952,
-1.38432886735644,-1.38206270143341,-1.37700185085542,-1.33528682306582,
-1.31403474741313,-1.31023234032745,-1.30879173320487,-1.30780111966584,
-1.30690386113888,-1.30543488734828,-1.30173165240809,-1.27768428593851,
-1.25371552928813,-1.2363216655335,-1.23280447697778,-1.23082168397464,
-1.22928963914096,-1.22729087249176,-1.22379664311068,-1.20869496133257,
-1.16453689073453,-1.15855892954612,-1.15461100738752,-1.15314889990963,
-1.15215380755164,-1.1512603274393,-1.14981228436362,-1.1462338597832,-1.11577257964686,
-1.08149420049871,-1.07745978983135,-1.0753674568826,-1.07382704747102,
-1.07191754302616,-1.06873575493666,-1.0578531235264,-1.00981463279724,
-0.99992678517416,-0.997925889411925,-0.996812466399093,-0.995855282278934,
-0.994628954763936,-0.992653341323871,-0.981227440979096,-0.946924784723346,
-0.925459695953636,-0.921987297428701,-0.919806601518821,-0.91809435768501,
-0.916186419610415,-0.913012682921902,-0.900806197381744,-0.856070903685685,
-0.844534686097814,-0.842553463558889,-0.841325382231954,-0.840367949075674,
-0.839255514548768,-0.837259541701091,-0.827460382585157,-0.78084310729135,
-0.768701190182902,-0.765396626744238,-0.763459880392136,-0.761923056867151,
-0.759868528409631,-0.756016999864159,-0.729207174076636,-0.700292104491353,
-0.688787835841003,-0.686808335251893,-0.685580834533151,-0.684623536883799,
-0.683510895240562,-0.681513658280727,-0.671689866488207,-0.624673574142428,
-0.612899164290838,-0.60962899683885,-0.607699933617078,-0.606162336667133,
-0.604097941730268,-0.600198706252296,-0.570807023845745,-0.552689914471559),
 .UNSPECIFIED.);
#3750=B_SPLINE_CURVE_WITH_KNOTS('',3,(#263518,#263519,#263520,#263521,#263522,
#263523,#263524,#263525,#263526,#263527,#263528,#263529,#263530,#263531,
#263532,#263533,#263534,#263535,#263536,#263537,#263538,#263539,#263540,
#263541,#263542,#263543,#263544,#263545,#263546,#263547,#263548,#263549,
#263550,#263551,#263552,#263553,#263554,#263555,#263556,#263557,#263558,
#263559,#263560,#263561,#263562,#263563,#263564,#263565,#263566,#263567,
#263568,#263569,#263570,#263571,#263572,#263573,#263574,#263575,#263576,
#263577,#263578,#263579,#263580,#263581,#263582,#263583,#263584,#263585,
#263586,#263587,#263588,#263589,#263590,#263591,#263592,#263593,#263594,
#263595,#263596,#263597,#263598,#263599,#263600,#263601,#263602,#263603,
#263604,#263605,#263606,#263607,#263608,#263609,#263610,#263611,#263612,
#263613,#263614,#263615,#263616,#263617,#263618,#263619,#263620,#263621,
#263622,#263623,#263624,#263625,#263626,#263627,#263628,#263629,#263630,
#263631,#263632,#263633,#263634,#263635,#263636,#263637,#263638,#263639,
#263640,#263641,#263642,#263643,#263644,#263645,#263646,#263647,#263648,
#263649,#263650,#263651,#263652,#263653,#263654,#263655,#263656,#263657,
#263658,#263659,#263660,#263661,#263662,#263663,#263664,#263665,#263666,
#263667,#263668,#263669,#263670,#263671,#263672,#263673,#263674,#263675,
#263676,#263677,#263678,#263679,#263680,#263681,#263682,#263683,#263684,
#263685,#263686,#263687,#263688,#263689,#263690,#263691,#263692,#263693,
#263694,#263695,#263696,#263697,#263698,#263699,#263700,#263701,#263702,
#263703,#263704,#263705,#263706,#263707,#263708,#263709,#263710,#263711,
#263712,#263713,#263714,#263715,#263716,#263717,#263718,#263719,#263720,
#263721,#263722,#263723,#263724,#263725,#263726,#263727,#263728,#263729,
#263730,#263731,#263732,#263733),.UNSPECIFIED.,.F.,.F.,(4,2,2,2,2,2,2,2,
2,2,2,2,2,2,2,2,2,2,2,2,2,2,2,2,2,2,2,2,2,2,2,2,2,2,2,2,2,2,2,2,2,2,2,2,
2,2,2,2,2,2,2,2,2,2,2,2,2,2,2,2,2,2,2,2,2,2,2,2,2,2,2,2,2,2,2,2,2,2,2,2,
2,2,2,2,2,2,2,2,2,2,2,2,2,2,2,2,2,2,2,2,2,2,2,2,2,2,2,4),(-1.40924613825003,
-1.3920519537756,-1.38843713478053,-1.38701450222455,-1.38601851466477,
-1.38510192842546,-1.38357216125138,-1.3795570674253,-1.32716665632577,
-1.31407280283506,-1.31080304653491,-1.30885928918695,-1.307128350303,-1.30494182932298,
-1.30149515233824,-1.28161275254803,-1.24596038299465,-1.23415948757676,
-1.23204493244415,-1.23089873850769,-1.22993155796098,-1.22871454209766,
-1.22625859743881,-1.2051057878793,-1.18747202730614,-1.15966435339812,
-1.15576054441803,-1.15367991458202,-1.1521241311294,-1.15016405427495,
-1.14682046847236,-1.13451740043587,-1.0972976844991,-1.08057210432518,
-1.07717501840345,-1.07578724475558,-1.07479775747969,-1.07387271879958,
-1.07256349998838,-1.06901431789296,-1.03779864425538,-1.00524303283522,
-1.00062654142338,-0.998402163997258,-0.996666889796871,-0.994744635944326,
-0.991573002092818,-0.981007710048585,-0.940162399629186,-0.923516464322548,
-0.92113669995226,-0.919919121268088,-0.918951805775388,-0.917805813678165,
-0.915692585290634,-0.903923752986713,-0.868518484606315,-0.848398529313525,
-0.84494310570162,-0.842753753679539,-0.841022301404241,-0.839079781735084,
-0.835816477618869,-0.822810515648565,-0.772058943781637,-0.766665744623544,
-0.764945847752992,-0.76388611663593,-0.76289884973839,-0.761524780739271,
-0.758212033382876,-0.742310720546279,-0.699906247952902,-0.698203275920053,
-0.690719006976775,-0.687939431922229,-0.686286135536854,-0.684539220746047,
-0.682231421352475,-0.677173187131354,-0.656538054041314,-0.629690228413494,
-0.62621626397745,-0.62340110628864,-0.611950210810646,-0.609957693600707,
-0.608718516635916,-0.607749563257127,-0.606619582794039,-0.604581082044936,
-0.594320577604801,-0.55698117440526,-0.537123528475259,-0.533677204871732,
-0.531490465100231,-0.529759086400023,-0.527814554446985,-0.524542821988681,
-0.511432114884855,-0.458825837099145,-0.454946198874758,-0.453437467580887,
-0.452524675142581,-0.451524617678329,-0.450082421968034,-0.446342958476149,
-0.440801141483845,-0.428888128758527),.UNSPECIFIED.);
#3751=B_SPLINE_CURVE_WITH_KNOTS('',3,(#263739,#263740,#263741,#263742,#263743,
#263744,#263745,#263746,#263747,#263748,#263749,#263750,#263751,#263752,
#263753,#263754,#263755,#263756,#263757,#263758,#263759,#263760,#263761,
#263762,#263763,#263764,#263765,#263766,#263767,#263768,#263769,#263770,
#263771,#263772,#263773,#263774,#263775,#263776,#263777,#263778,#263779,
#263780,#263781,#263782,#263783,#263784,#263785,#263786,#263787,#263788,
#263789,#263790,#263791,#263792,#263793,#263794,#263795,#263796,#263797,
#263798,#263799,#263800,#263801,#263802,#263803,#263804,#263805,#263806,
#263807,#263808,#263809,#263810,#263811,#263812,#263813,#263814,#263815,
#263816,#263817,#263818,#263819,#263820,#263821,#263822,#263823,#263824,
#263825,#263826,#263827,#263828,#263829,#263830,#263831,#263832,#263833,
#263834,#263835,#263836,#263837,#263838,#263839,#263840,#263841,#263842,
#263843,#263844,#263845,#263846,#263847,#263848,#263849,#263850,#263851,
#263852,#263853,#263854,#263855,#263856,#263857,#263858,#263859,#263860,
#263861,#263862,#263863,#263864),.UNSPECIFIED.,.F.,.F.,(4,2,2,2,2,2,2,2,
2,2,2,2,2,2,2,2,2,2,2,2,2,2,2,2,2,2,2,2,2,2,2,2,2,2,2,2,2,2,2,2,2,2,2,2,
2,2,2,2,2,2,2,2,2,2,2,2,2,2,2,2,2,2,4),(-0.552732293014681,-0.544526721663612,
-0.521443127730424,-0.517925922747745,-0.5157319163145,-0.514018367597968,
-0.512118361653583,-0.508979738586424,-0.497183324147925,-0.452203697215895,
-0.440469805914575,-0.43847540222017,-0.437243463969527,-0.436285818214354,
-0.435176337211476,-0.433193446836002,-0.423615724010117,-0.379792803641223,
-0.365017697019254,-0.361545767081861,-0.359551883937695,-0.357865478456037,
-0.355813896294542,-0.351975627845191,-0.325740108391654,-0.30091888290929,
-0.295160809780153,-0.284650279422643,-0.282720365838429,-0.281507920630911,
-0.280551937044157,-0.279428689091944,-0.277382012164753,-0.26663441544752,
-0.23971069293146,-0.233652170519376,-0.21007357601036,-0.206543318400608,
-0.204345337128094,-0.202631243555407,-0.200733247313348,-0.197866419508975,
-0.187762297764411,-0.170302907495981,-0.139921321040147,-0.12903834759887,
-0.127089311294619,-0.125871068529074,-0.12491463882738,-0.124010201867978,
-0.122297285983923,-0.116174002758719,-0.105061876475186,-0.0866783339072084,
-0.0544456451986642,-0.0509002231849731,-0.0486976846775913,-0.0469830271232924,
-0.0450874495901178,-0.043132183430273,-0.0402378723461658,-0.0350321380960057,
-0.000460216426560407),.UNSPECIFIED.);
#3752=B_SPLINE_CURVE_WITH_KNOTS('',3,(#263865,#263866,#263867,#263868,#263869,
#263870,#263871,#263872,#263873,#263874,#263875,#263876,#263877,#263878,
#263879,#263880,#263881,#263882,#263883,#263884,#263885,#263886,#263887,
#263888,#263889,#263890,#263891,#263892,#263893,#263894,#263895,#263896,
#263897,#263898,#263899,#263900,#263901,#263902,#263903,#263904,#263905,
#263906,#263907,#263908,#263909,#263910,#263911,#263912,#263913,#263914,
#263915,#263916,#263917,#263918,#263919,#263920,#263921,#263922,#263923,
#263924,#263925,#263926,#263927,#263928,#263929,#263930,#263931,#263932,
#263933,#263934,#263935,#263936,#263937,#263938,#263939,#263940,#263941,
#263942,#263943,#263944,#263945,#263946,#263947,#263948,#263949,#263950,
#263951,#263952,#263953,#263954,#263955,#263956,#263957,#263958,#263959,
#263960,#263961,#263962,#263963,#263964,#263965,#263966,#263967,#263968,
#263969,#263970),.UNSPECIFIED.,.F.,.F.,(4,2,2,2,2,2,2,2,2,2,2,2,2,2,2,2,
2,2,2,2,2,2,2,2,2,2,2,2,2,2,2,2,2,2,2,2,2,2,2,2,2,2,2,2,2,2,2,2,2,2,2,2,
4),(-1.9612255480559,-1.9405886767412,-1.93449603501467,-1.9328157050967,
-1.93169950834601,-1.93079315603296,-1.9298381208837,-1.9286341750782,-1.92619823164976,
-1.90289450440463,-1.88481491118963,-1.86346440347446,-1.85697678295479,
-1.85502137317573,-1.853125879729,-1.85141214521489,-1.84921197455577,-1.84567274751162,
-1.82169278466138,-1.79359873747615,-1.78347439452138,-1.77772095940746,
-1.77607827153416,-1.77517551457198,-1.77421878708292,-1.77299240711089,
-1.77101548031275,-1.75954648192973,-1.7568303040546,-1.71866896826405,
-1.70838918172379,-1.70152094424652,-1.69889082756806,-1.69710149112821,
-1.69535964781507,-1.69326688571293,-1.68801440987397,-1.64790795331707,
-1.62548139028703,-1.62158071654605,-1.62012579467928,-1.61913242424126,
-1.61823807761331,-1.6167840945605,-1.61316835477589,-1.58349695362429,
-1.54839982601569,-1.54442996702593,-1.54235142620455,-1.5406485568595,
-1.53867290759651,-1.53527858671223,-1.53330080949059),.UNSPECIFIED.);
#3753=B_SPLINE_CURVE_WITH_KNOTS('',3,(#263972,#263973,#263974,#263975,#263976,
#263977,#263978,#263979,#263980,#263981,#263982,#263983,#263984,#263985,
#263986,#263987,#263988,#263989,#263990,#263991,#263992,#263993,#263994,
#263995,#263996,#263997,#263998,#263999,#264000,#264001,#264002,#264003,
#264004,#264005,#264006,#264007,#264008,#264009,#264010,#264011,#264012,
#264013,#264014,#264015,#264016,#264017,#264018,#264019,#264020,#264021,
#264022,#264023,#264024,#264025,#264026,#264027,#264028,#264029,#264030,
#264031,#264032,#264033,#264034,#264035,#264036,#264037,#264038,#264039,
#264040,#264041,#264042,#264043,#264044,#264045,#264046,#264047,#264048,
#264049,#264050,#264051,#264052,#264053,#264054,#264055,#264056,#264057,
#264058,#264059,#264060,#264061),.UNSPECIFIED.,.F.,.F.,(4,2,2,2,2,2,2,2,
2,2,2,2,2,2,2,2,2,2,2,2,2,2,2,2,2,2,2,2,2,2,2,2,2,2,2,2,2,2,2,2,2,2,2,2,
4),(-0.428888128758527,-0.396149256973793,-0.380951640173066,-0.377423098483843,
-0.375401050325071,-0.37369311932673,-0.371617937666183,-0.367742421211991,
-0.341347888932855,-0.312612316858321,-0.300671760432889,-0.298653579684501,
-0.297406587066225,-0.296436814460417,-0.295311952691367,-0.293297545098321,
-0.283470482356494,-0.236637361538213,-0.22480588070762,-0.221505587000739,
-0.219554666063805,-0.217997194006659,-0.215902750986338,-0.211934654893356,
-0.179779493763917,-0.170684231586507,-0.145326264716195,-0.142930477393819,
-0.141709332279537,-0.14079593250481,-0.139696882183857,-0.137819208491731,
-0.135464995242747,-0.13051150020455,-0.115748856860529,-0.109306850298441,
-0.0728741192258072,-0.0714380750948244,-0.0668166219952595,-0.0645909335809879,
-0.0628551140711278,-0.0609327435162668,-0.0577620471575559,-0.0458865390397537,
-0.000459688585513052),.UNSPECIFIED.);
#3754=B_SPLINE_CURVE_WITH_KNOTS('',3,(#264062,#264063,#264064,#264065,#264066,
#264067,#264068,#264069),.UNSPECIFIED.,.F.,.F.,(4,1,1,1,1,4),(53.4070751110266,
53.5034432466949,54.5007770973516,55.4981109480084,56.4954447986652,56.945832495276),
 .UNSPECIFIED.);
#3755=B_SPLINE_CURVE_WITH_KNOTS('',3,(#264074,#264075,#264076,#264077,#264078,
#264079,#264080,#264081,#264082,#264083,#264084,#264085,#264086,#264087,
#264088,#264089,#264090,#264091,#264092,#264093,#264094,#264095,#264096,
#264097,#264098,#264099,#264100,#264101,#264102,#264103,#264104,#264105,
#264106,#264107,#264108,#264109,#264110,#264111,#264112,#264113,#264114,
#264115,#264116,#264117,#264118,#264119,#264120,#264121,#264122,#264123,
#264124,#264125,#264126,#264127,#264128,#264129,#264130,#264131,#264132,
#264133,#264134,#264135,#264136,#264137,#264138,#264139,#264140,#264141,
#264142,#264143,#264144,#264145,#264146,#264147,#264148,#264149,#264150,
#264151,#264152,#264153,#264154,#264155,#264156,#264157,#264158,#264159,
#264160,#264161,#264162,#264163,#264164,#264165,#264166,#264167,#264168,
#264169,#264170,#264171,#264172,#264173,#264174,#264175,#264176,#264177,
#264178,#264179,#264180,#264181,#264182,#264183,#264184,#264185,#264186,
#264187,#264188,#264189,#264190,#264191,#264192,#264193,#264194,#264195,
#264196,#264197,#264198,#264199,#264200,#264201,#264202,#264203,#264204,
#264205,#264206,#264207,#264208,#264209,#264210,#264211,#264212,#264213,
#264214,#264215,#264216,#264217,#264218,#264219,#264220,#264221,#264222,
#264223,#264224,#264225,#264226,#264227,#264228,#264229,#264230,#264231,
#264232,#264233,#264234,#264235,#264236,#264237,#264238,#264239,#264240,
#264241,#264242,#264243,#264244,#264245,#264246,#264247,#264248,#264249,
#264250,#264251,#264252,#264253,#264254,#264255,#264256,#264257,#264258,
#264259,#264260,#264261,#264262,#264263,#264264,#264265,#264266,#264267,
#264268,#264269,#264270,#264271,#264272,#264273,#264274,#264275,#264276,
#264277,#264278,#264279,#264280,#264281,#264282,#264283,#264284,#264285,
#264286,#264287,#264288,#264289,#264290,#264291),.UNSPECIFIED.,.F.,.F.,
(4,2,2,2,2,2,2,2,2,2,2,2,2,2,2,2,2,2,2,2,2,2,2,2,2,2,2,2,2,2,2,2,2,2,2,
2,2,2,2,2,2,2,2,2,2,2,2,2,2,2,2,2,2,2,2,2,2,2,2,2,2,2,2,2,2,2,2,2,2,2,2,
2,2,2,2,2,2,2,2,2,2,2,2,2,2,2,2,2,2,2,2,2,2,2,2,2,2,2,2,2,2,2,2,2,2,2,2,
2,4),(-1.53316853732264,-1.53081551367157,-1.52829084480876,-1.52706928721019,
-1.52611296467185,-1.52499723132008,-1.52303781081447,-1.51485342291321,
-1.50942856401873,-1.48169382206184,-1.45794391741066,-1.45253568003227,
-1.4501832563714,-1.44844698515222,-1.44683569283706,-1.44462990550193,
-1.43904574362156,-1.39817851464175,-1.37701390324708,-1.37321933466248,
-1.37178004054277,-1.37078980634098,-1.36989248801421,-1.36842264584295,
-1.36471364553914,-1.34045277188475,-1.32019267977353,-1.3014102281572,
-1.29661684162022,-1.29437540733383,-1.29265616233146,-1.29101218394169,
-1.28820709096339,-1.28040554207598,-1.27861539451046,-1.22865904745447,
-1.21866694912144,-1.2166605332583,-1.21554606960949,-1.21458926533872,
-1.21336507234076,-1.21139606362848,-1.20010063816694,-1.15985315760856,
-1.149062141103,-1.1418599509632,-1.13922739024492,-1.13743718283085,-1.1356950984785,
-1.13360277770248,-1.12835537222977,-1.08817759759204,-1.0657892218717,
-1.06189109040472,-1.06043627986703,-1.05944272759548,-1.05854802071693,
-1.05709308175168,-1.05347312168424,-1.02392044270956,-0.988691601922453,
-0.984719498058419,-0.982640123242514,-0.98110121389413,-0.979183245198251,
-0.975962675272834,-0.963171081926161,-0.915239598309298,-0.907183750346714,
-0.905233996930918,-0.904120160524173,-0.903163093038548,-0.901937525843802,
-0.899394161783937,-0.896023821664812,-0.887723613756562,-0.846745637911942,
-0.832137863816986,-0.82867739227419,-0.826686111034553,-0.824999584999771,
-0.822945011256146,-0.819092559077852,-0.792221837291364,-0.763433265202599,
-0.751878661977455,-0.749896820952441,-0.748668693002376,-0.747711442688195,
-0.746599472408422,-0.744604948270223,-0.73482556557149,-0.688490548923068,
-0.676113404013373,-0.672820556945495,-0.670867815562935,-0.669162483627626,
-0.667052468962199,-0.662931603590999,-0.630222737197789,-0.598212380874071,
-0.594697593893947,-0.5932601949988,-0.592279972204606,-0.591262586112446,
-0.589696083200367,-0.584970014082902,-0.577337491191725,-0.552732293014681),
 .UNSPECIFIED.);
#3756=B_SPLINE_CURVE_WITH_KNOTS('',3,(#264293,#264294,#264295,#264296,#264297,
#264298,#264299),.UNSPECIFIED.,.F.,.F.,(4,1,1,1,4),(56.945832495276,57.4927786493219,
58.4901124999787,59.4874463506355,59.6902604182062),.UNSPECIFIED.);
#3757=B_SPLINE_CURVE_WITH_KNOTS('',3,(#264300,#264301,#264302,#264303,#264304,
#264305,#264306,#264307,#264308,#264309,#264310,#264311,#264312,#264313,
#264314,#264315,#264316,#264317,#264318,#264319,#264320,#264321,#264322,
#264323,#264324,#264325,#264326,#264327,#264328,#264329,#264330,#264331,
#264332,#264333,#264334,#264335,#264336,#264337,#264338,#264339,#264340,
#264341,#264342,#264343,#264344,#264345,#264346,#264347,#264348,#264349,
#264350,#264351,#264352,#264353,#264354,#264355,#264356,#264357,#264358,
#264359,#264360,#264361,#264362,#264363,#264364,#264365,#264366,#264367,
#264368,#264369,#264370,#264371,#264372,#264373,#264374,#264375,#264376,
#264377,#264378,#264379,#264380,#264381,#264382,#264383,#264384,#264385,
#264386,#264387,#264388,#264389,#264390,#264391,#264392,#264393,#264394,
#264395,#264396,#264397,#264398,#264399,#264400,#264401,#264402,#264403,
#264404,#264405,#264406,#264407,#264408,#264409,#264410,#264411,#264412,
#264413,#264414,#264415,#264416,#264417,#264418,#264419,#264420,#264421),
 .UNSPECIFIED.,.F.,.F.,(4,2,2,2,2,2,2,2,2,2,2,2,2,2,2,2,2,2,2,2,2,2,2,2,
2,2,2,2,2,2,2,2,2,2,2,2,2,2,2,2,2,2,2,2,2,2,2,2,2,2,2,2,2,2,2,2,2,2,2,2,
4),(-1.96243636638787,-1.92873122880033,-1.92345762837139,-1.92052619707091,
-1.91854583558166,-1.9166258280168,-1.91488875034608,-1.91265671532101,
-1.90906163714298,-1.87746944506871,-1.85890238795916,-1.84755329411216,
-1.84132627277157,-1.83959618940266,-1.83867922969657,-1.83771059374843,
-1.83647975383564,-1.83451568587979,-1.82365391048351,-1.79366833211531,
-1.77602800307227,-1.76582801244604,-1.76291983695349,-1.761000548976,-1.75926327589006,
-1.75702980606436,-1.75342998659544,-1.72231437695619,-1.6967274153731,
-1.68622469363991,-1.684172509338,-1.68303928435714,-1.68207024185141,-1.68083442756679,
-1.67885396290855,-1.66766359560826,-1.62300014774661,-1.61476393451037,
-1.60887748613216,-1.60642521992754,-1.60465369139878,-1.60303605252178,
-1.60086137152891,-1.5955571477268,-1.55689061586263,-1.53341901218345,
-1.52941447228155,-1.52793282012685,-1.52692472107987,-1.52601933081797,
-1.52455070023411,-1.52091379352729,-1.4914888424095,-1.45724411427105,
-1.45261175712674,-1.45038355295896,-1.44864697895625,-1.44672500409201,
-1.44355781116524,-1.43304437783208,-1.41001614483363),.UNSPECIFIED.);
#3758=B_SPLINE_CURVE_WITH_KNOTS('',3,(#264427,#264428,#264429,#264430,#264431,
#264432,#264433,#264434),.UNSPECIFIED.,.F.,.F.,(4,1,1,1,1,4),(65.9734457253858,
66.179042922154,67.1767749221439,68.1745069221338,69.1722389221237,69.5126852782938),
 .UNSPECIFIED.);
#3759=B_SPLINE_CURVE_WITH_KNOTS('',3,(#264435,#264436,#264437,#264438,#264439,
#264440,#264441,#264442,#264443,#264444,#264445,#264446,#264447,#264448,
#264449,#264450,#264451,#264452,#264453,#264454,#264455,#264456,#264457,
#264458,#264459,#264460,#264461,#264462,#264463,#264464,#264465,#264466,
#264467,#264468,#264469,#264470,#264471,#264472,#264473,#264474,#264475,
#264476,#264477,#264478,#264479,#264480,#264481,#264482,#264483,#264484,
#264485,#264486,#264487,#264488,#264489,#264490,#264491,#264492,#264493,
#264494,#264495,#264496,#264497,#264498,#264499,#264500,#264501,#264502,
#264503,#264504,#264505,#264506,#264507,#264508,#264509,#264510,#264511,
#264512,#264513,#264514,#264515,#264516,#264517,#264518,#264519,#264520,
#264521,#264522,#264523,#264524,#264525,#264526),.UNSPECIFIED.,.F.,.F.,
(4,2,2,2,2,2,2,2,2,2,2,2,2,2,2,2,2,2,2,2,2,2,2,2,2,2,2,2,2,2,2,2,2,2,2,
2,2,2,2,2,2,2,2,2,2,4),(-1.961444596389,-1.92797148288741,-1.92278945608443,
-1.91990484640394,-1.91795405212732,-1.91606186451412,-1.91434777267141,
-1.91214246088824,-1.90858535102273,-1.8767036812167,-1.85739092388925,
-1.84669630513855,-1.84073661592871,-1.83902964573844,-1.838127458231,-1.83717068021997,
-1.83594181942472,-1.83395621803567,-1.8223179290392,-1.81894017432273,
-1.7832616839657,-1.76686003893351,-1.76305502428428,-1.76097758804903,
-1.75943954900616,-1.75752193746662,-1.75430021824994,-1.74301168724916,
-1.69546421731742,-1.68560972645131,-1.68361155175159,-1.68249911130248,
-1.68154243712619,-1.68031632930557,-1.67834023413792,-1.66688733707865,
-1.62228310176853,-1.60995361789867,-1.60677116269319,-1.60486209074503,
-1.60315142157672,-1.60097627903177,-1.59751980084343,-1.57656646232454,
-1.53415504157875,-1.53316853732264),.UNSPECIFIED.);
#3760=B_SPLINE_CURVE_WITH_KNOTS('',3,(#264527,#264528,#264529,#264530,#264531,
#264532,#264533,#264534,#264535,#264536,#264537,#264538,#264539,#264540,
#264541,#264542,#264543,#264544,#264545,#264546,#264547,#264548,#264549,
#264550,#264551,#264552,#264553,#264554,#264555,#264556,#264557,#264558,
#264559,#264560,#264561,#264562,#264563,#264564,#264565,#264566,#264567,
#264568,#264569,#264570,#264571,#264572,#264573,#264574,#264575,#264576,
#264577,#264578,#264579,#264580,#264581,#264582,#264583,#264584,#264585,
#264586,#264587,#264588,#264589,#264590,#264591,#264592,#264593,#264594,
#264595,#264596,#264597,#264598,#264599,#264600,#264601,#264602,#264603,
#264604,#264605,#264606,#264607,#264608,#264609,#264610,#264611,#264612,
#264613,#264614,#264615,#264616,#264617,#264618,#264619,#264620,#264621,
#264622,#264623,#264624,#264625,#264626,#264627,#264628,#264629,#264630,
#264631,#264632,#264633,#264634,#264635,#264636,#264637,#264638,#264639,
#264640,#264641,#264642,#264643,#264644,#264645,#264646,#264647,#264648,
#264649,#264650,#264651,#264652,#264653,#264654,#264655,#264656,#264657,
#264658,#264659,#264660,#264661,#264662,#264663,#264664,#264665,#264666,
#264667,#264668,#264669,#264670,#264671,#264672,#264673,#264674,#264675,
#264676,#264677,#264678,#264679,#264680,#264681,#264682,#264683,#264684,
#264685,#264686,#264687,#264688,#264689,#264690,#264691,#264692,#264693,
#264694,#264695,#264696,#264697,#264698,#264699,#264700,#264701,#264702,
#264703,#264704,#264705,#264706,#264707,#264708,#264709,#264710,#264711,
#264712,#264713,#264714,#264715,#264716,#264717,#264718,#264719,#264720,
#264721,#264722,#264723,#264724,#264725,#264726,#264727,#264728,#264729,
#264730,#264731,#264732,#264733,#264734,#264735,#264736,#264737,#264738,
#264739,#264740),.UNSPECIFIED.,.F.,.F.,(4,2,2,2,2,2,2,2,2,2,2,2,2,2,2,2,
2,2,2,2,2,2,2,2,2,2,2,2,2,2,2,2,2,2,2,2,2,2,2,2,2,2,2,2,2,2,2,2,2,2,2,2,
2,2,2,2,2,2,2,2,2,2,2,2,2,2,2,2,2,2,2,2,2,2,2,2,2,2,2,2,2,2,2,2,2,2,2,2,
2,2,2,2,2,2,2,2,2,2,2,2,2,2,2,2,2,2,4),(-1.41001614483363,-1.39225513613191,
-1.38065973984924,-1.376421476499,-1.37337426020363,-1.37204543874264,-1.37106530782206,
-1.36998605563137,-1.36817943629454,-1.36203867008771,-1.31665184071068,
-1.30546121509686,-1.29804410829108,-1.29536097604857,-1.29354398226279,
-1.29178143809269,-1.28967105923585,-1.28441160664946,-1.24422366100781,
-1.22191465916282,-1.21800451467768,-1.21653661861258,-1.21553132303034,
-1.21462342845557,-1.21314125408657,-1.2094237054695,-1.18299421871368,
-1.15699808566829,-1.14362689665319,-1.14033431707254,-1.13838466794598,
-1.13665322620501,-1.13447244007195,-1.1310473254096,-1.11180204486799,
-1.0829950071077,-1.06567440482489,-1.06221660516705,-1.0608184682476,-1.05982666920218,
-1.05890354238529,-1.05760267469567,-1.05411253706449,-1.0215481111743,
-0.990108237000798,-0.985560031238105,-0.983348127396927,-0.981613437844249,
-0.979682416626492,-0.976474271423693,-0.964166657090143,-0.919378789263433,
-0.908088046324516,-0.906102513316289,-0.904865121885621,-0.903895881267495,
-0.902763618270317,-0.900716164076702,-0.890303726744272,-0.865149581939166,
-0.833523248932328,-0.82992857594515,-0.827696523580716,-0.825959282040161,
-0.824038940180786,-0.82087991374156,-0.809148784368028,-0.764003561856856,
-0.752415027705897,-0.750414971150481,-0.749173129940184,-0.748203418330058,
-0.74707408132241,-0.745040510205677,-0.734886271452398,-0.681757543573821,
-0.675163483334289,-0.672521483364338,-0.670893665926067,-0.669130160021742,
-0.666723713955244,-0.661110981536136,-0.65336761074115,-0.608218489812041,
-0.596625602948298,-0.594625417977323,-0.593383576453568,-0.592413916530432,
-0.591284699580605,-0.58925149209545,-0.579102229562427,-0.526085175969397,
-0.519410126806953,-0.516754505253086,-0.51512423603572,-0.513362699944944,
-0.510967210879639,-0.505417874058922,-0.497787274338213,-0.452528348348435,
-0.440852928976274,-0.438848619395513,-0.437605575058572,-0.436635862464329,
-0.435507605037135,-0.433478634774835,-0.429017715179976),.UNSPECIFIED.);
#3761=B_SPLINE_CURVE_WITH_KNOTS('',3,(#264746,#264747,#264748,#264749,#264750,
#264751,#264752,#264753,#264754,#264755,#264756,#264757,#264758,#264759,
#264760,#264761,#264762,#264763,#264764,#264765,#264766,#264767,#264768,
#264769,#264770,#264771,#264772,#264773,#264774,#264775,#264776,#264777,
#264778,#264779,#264780,#264781,#264782,#264783,#264784,#264785,#264786,
#264787,#264788,#264789,#264790,#264791,#264792,#264793,#264794,#264795,
#264796,#264797,#264798,#264799,#264800,#264801,#264802,#264803,#264804,
#264805,#264806,#264807,#264808,#264809,#264810,#264811,#264812,#264813,
#264814,#264815,#264816,#264817,#264818,#264819,#264820,#264821,#264822,
#264823,#264824,#264825,#264826,#264827,#264828,#264829,#264830,#264831,
#264832,#264833,#264834,#264835,#264836,#264837,#264838,#264839,#264840,
#264841,#264842,#264843,#264844,#264845,#264846,#264847,#264848,#264849,
#264850,#264851,#264852,#264853,#264854,#264855,#264856,#264857,#264858,
#264859,#264860,#264861,#264862,#264863,#264864,#264865,#264866,#264867,
#264868,#264869,#264870,#264871),.UNSPECIFIED.,.F.,.F.,(4,2,2,2,2,2,2,2,
2,2,2,2,2,2,2,2,2,2,2,2,2,2,2,2,2,2,2,2,2,2,2,2,2,2,2,2,2,2,2,2,2,2,2,2,
2,2,2,2,2,2,2,2,2,2,2,2,2,2,2,2,2,2,4),(-0.552641378009195,-0.540781647137896,
-0.535233133886294,-0.533032912503839,-0.531422649836385,-0.52968460282655,
-0.527324657016637,-0.521876101476598,-0.497779811663714,-0.46874954818786,
-0.457145285080451,-0.455160901218344,-0.453932041216431,-0.452974768855968,
-0.451863402712269,-0.449871499929522,-0.440136434336113,-0.394461432118698,
-0.381469688671962,-0.378130061027684,-0.376166611317052,-0.37446233434963,
-0.372366938580967,-0.36831721201437,-0.363190775635023,-0.351482642274451,
-0.32729370208429,-0.301784826599703,-0.299412922280656,-0.298205739899813,
-0.297250214851437,-0.296123186985811,-0.294058582447317,-0.282944942472228,
-0.266795587014716,-0.229180882302226,-0.226243562427763,-0.222989964282724,
-0.220876195390768,-0.219170702282629,-0.217220919246893,-0.213855274221538,
-0.199045190378691,-0.165314507066046,-0.146155579505983,-0.143765941310845,
-0.14255499193553,-0.141650281186909,-0.14056871296215,-0.138730277521751,
-0.136430803410411,-0.131616844833293,-0.117441525137364,-0.0975863550034039,
-0.071226326335163,-0.0676477925026255,-0.0654354924249702,-0.0637198074745481,
-0.0618297391996461,-0.0587357918562178,-0.0474420888279364,-0.00213289938031032,
-0.000460482320649901),.UNSPECIFIED.);
#3762=B_SPLINE_CURVE_WITH_KNOTS('',3,(#264872,#264873,#264874,#264875,#264876,
#264877,#264878),.UNSPECIFIED.,.F.,.F.,(4,1,1,1,4),(69.5126852782938,70.1699709221136,
71.1677029221035,72.1654349220934,72.2566310325654),.UNSPECIFIED.);
#3763=B_SPLINE_CURVE_WITH_KNOTS('',3,(#264880,#264881,#264882,#264883,#264884,
#264885,#264886,#264887,#264888,#264889,#264890,#264891,#264892,#264893,
#264894,#264895,#264896,#264897,#264898,#264899,#264900,#264901,#264902,
#264903,#264904,#264905,#264906,#264907,#264908,#264909,#264910,#264911,
#264912,#264913,#264914,#264915,#264916,#264917,#264918,#264919,#264920,
#264921,#264922,#264923,#264924,#264925,#264926,#264927,#264928,#264929,
#264930,#264931,#264932,#264933,#264934,#264935,#264936,#264937,#264938,
#264939,#264940,#264941,#264942,#264943,#264944,#264945,#264946,#264947,
#264948,#264949,#264950,#264951,#264952,#264953,#264954,#264955,#264956,
#264957,#264958,#264959,#264960,#264961,#264962,#264963,#264964,#264965,
#264966,#264967,#264968,#264969,#264970,#264971,#264972,#264973,#264974,
#264975),.UNSPECIFIED.,.F.,.F.,(4,2,2,2,2,2,2,2,2,2,2,2,2,2,2,2,2,2,2,2,
2,2,2,2,2,2,2,2,2,2,2,2,2,2,2,2,2,2,2,2,2,2,2,2,2,2,2,4),(-0.429017715179976,
-0.423403954564558,-0.372093636464055,-0.371467916069141,-0.363935600074779,
-0.36114832096306,-0.35949318514206,-0.357746339610022,-0.355442024540115,
-0.350405215805828,-0.329945432012915,-0.299875940613244,-0.296777314673502,
-0.285136710570285,-0.283134449509169,-0.281892124955387,-0.280922614338927,
-0.279794177764365,-0.27776386747213,-0.267660917996547,-0.215698368926963,
-0.208215183171208,-0.205435522846508,-0.203782043248226,-0.2020348374104,
-0.199726488907313,-0.194849116939424,-0.188279414534909,-0.171459642434667,
-0.139926095878457,-0.129347031904572,-0.127397757769541,-0.126171526198963,
-0.12520338666699,-0.124285898634109,-0.122556375741725,-0.116271228017277,
-0.104772083128549,-0.0867835856361286,-0.054851439527974,-0.0512731530003628,
-0.0490463646925665,-0.0473102104214056,-0.0453880027651295,-0.0434042427038484,
-0.0404641866046306,-0.0351677589407834,-0.000459409169756657),
 .UNSPECIFIED.);
#3764=B_SPLINE_CURVE_WITH_KNOTS('',3,(#264976,#264977,#264978,#264979,#264980,
#264981,#264982,#264983,#264984,#264985,#264986,#264987,#264988,#264989,
#264990,#264991,#264992,#264993,#264994,#264995,#264996,#264997,#264998,
#264999,#265000,#265001,#265002,#265003,#265004,#265005,#265006,#265007,
#265008,#265009,#265010,#265011,#265012,#265013,#265014,#265015,#265016,
#265017,#265018,#265019,#265020,#265021,#265022,#265023,#265024,#265025,
#265026,#265027,#265028,#265029,#265030,#265031,#265032,#265033,#265034,
#265035,#265036,#265037,#265038,#265039,#265040,#265041,#265042,#265043,
#265044,#265045,#265046,#265047,#265048,#265049,#265050,#265051,#265052,
#265053,#265054,#265055,#265056,#265057,#265058,#265059,#265060,#265061,
#265062,#265063,#265064,#265065,#265066,#265067,#265068,#265069,#265070,
#265071,#265072,#265073,#265074,#265075,#265076,#265077,#265078,#265079,
#265080,#265081,#265082,#265083,#265084,#265085,#265086,#265087,#265088,
#265089,#265090,#265091,#265092,#265093,#265094,#265095,#265096,#265097,
#265098,#265099,#265100,#265101,#265102,#265103),.UNSPECIFIED.,.F.,.F.,
(4,2,2,2,2,2,2,2,2,2,2,2,2,2,2,2,2,2,2,2,2,2,2,2,2,2,2,2,2,2,2,2,2,2,2,
2,2,2,2,2,2,2,2,2,2,2,2,2,2,2,2,2,2,2,2,2,2,2,2,2,2,2,2,4),(-1.9613855033268,
-1.93508066903094,-1.93337100487253,-1.93223724462457,-1.93131827400647,
-1.93035078653872,-1.92913344926569,-1.92667706329812,-1.90390393165469,
-1.88653238443498,-1.86423273947521,-1.85757798830135,-1.85558998602215,
-1.85366482028954,-1.8519294907388,-1.84970861207128,-1.84614966324438,
-1.82256534237624,-1.79473233025188,-1.78421876084219,-1.77829710629275,
-1.77662505331695,-1.77570968411641,-1.77474065236175,-1.77350165179664,
-1.77150996373025,-1.76007810444082,-1.75727703441271,-1.71286707877054,
-1.70283977167619,-1.69995003840863,-1.69802883628234,-1.69629280596669,
-1.69406508448902,-1.69048302890886,-1.65857609141762,-1.6336258765276,
-1.62325880519486,-1.62121441620711,-1.62008313366752,-1.61911428191488,
-1.61787681546689,-1.61589008651907,-1.60455953972686,-1.55975854910694,
-1.55170004044053,-1.54591199706385,-1.54347662521593,-1.54170864427399,
-1.54008827538572,-1.53790090273535,-1.53252035872154,-1.49477884010259,
-1.4787812579919,-1.46769367164578,-1.46561227852245,-1.46447303630186,
-1.4635050383444,-1.46227846622805,-1.46032769443297,-1.4497138330154,-1.44423865138944,
-1.4283803357202,-1.40944749342716),.UNSPECIFIED.);
#3765=B_SPLINE_CURVE_WITH_KNOTS('',3,(#265108,#265109,#265110,#265111,#265112,
#265113,#265114,#265115,#265116,#265117,#265118,#265119,#265120,#265121,
#265122,#265123,#265124,#265125,#265126,#265127,#265128,#265129,#265130,
#265131,#265132,#265133,#265134,#265135,#265136,#265137,#265138,#265139,
#265140,#265141,#265142,#265143,#265144,#265145,#265146,#265147,#265148,
#265149,#265150,#265151,#265152,#265153,#265154,#265155,#265156,#265157,
#265158,#265159,#265160,#265161,#265162,#265163,#265164,#265165,#265166,
#265167,#265168,#265169,#265170,#265171,#265172,#265173,#265174,#265175,
#265176,#265177,#265178,#265179,#265180,#265181,#265182,#265183,#265184,
#265185,#265186,#265187,#265188,#265189,#265190,#265191,#265192,#265193,
#265194,#265195,#265196,#265197,#265198,#265199,#265200,#265201,#265202,
#265203,#265204,#265205,#265206,#265207,#265208,#265209,#265210,#265211,
#265212,#265213,#265214,#265215,#265216,#265217,#265218,#265219,#265220,
#265221,#265222,#265223,#265224,#265225,#265226,#265227,#265228,#265229,
#265230,#265231,#265232,#265233,#265234,#265235,#265236,#265237,#265238,
#265239,#265240,#265241,#265242,#265243,#265244,#265245,#265246,#265247,
#265248,#265249,#265250,#265251,#265252,#265253,#265254,#265255,#265256,
#265257,#265258,#265259,#265260,#265261,#265262,#265263,#265264,#265265,
#265266,#265267,#265268,#265269,#265270,#265271,#265272,#265273,#265274,
#265275,#265276,#265277,#265278,#265279,#265280,#265281,#265282,#265283,
#265284,#265285,#265286,#265287,#265288,#265289,#265290,#265291,#265292,
#265293,#265294,#265295,#265296,#265297,#265298,#265299,#265300,#265301,
#265302,#265303,#265304,#265305),.UNSPECIFIED.,.F.,.F.,(4,2,2,2,2,2,2,2,
2,2,2,2,2,2,2,2,2,2,2,2,2,2,2,2,2,2,2,2,2,2,2,2,2,2,2,2,2,2,2,2,2,2,2,2,
2,2,2,2,2,2,2,2,2,2,2,2,2,2,2,2,2,2,2,2,2,2,2,2,2,2,2,2,2,2,2,2,2,2,2,2,
2,2,2,2,2,2,2,2,2,2,2,2,2,2,2,2,2,2,4),(-1.53325260190294,-1.52242625781252,
-1.48177886514756,-1.47086017453636,-1.46780092593041,-1.46591851637425,
-1.46420088380173,-1.46201032461387,-1.45842504024837,-1.43095190227417,
-1.41237905773923,-1.39351591331953,-1.38992727548277,-1.3885192097765,
-1.38753497521275,-1.38663092516517,-1.38537376267351,-1.38212302487428,
-1.34719406708861,-1.31674100278451,-1.31282744470658,-1.3107603111279,
-1.30922271351678,-1.30729631638362,-1.30403717291467,-1.29237441448629,
-1.24521662778124,-1.23538294069485,-1.23338530251937,-1.23227267368181,
-1.23131553050119,-1.23008842373757,-1.22810995124981,-1.21662131896378,
-1.17196319845482,-1.16386055173013,-1.15806179030878,-1.15564266123855,
-1.15389423402223,-1.152297255681,-1.15014990003729,-1.14491154101944,-1.10012040650216,
-1.08196253870356,-1.07844036785622,-1.07704260017154,-1.07606021935041,
-1.07515363447275,-1.0738872246539,-1.07057422673835,-1.03620841936487,
-1.00527831725009,-1.00135811733981,-0.999289405848374,-0.997751447789123,
-0.995825657793389,-0.992570120563453,-0.980948402575276,-0.935993394489741,
-0.924277015074869,-0.922284629007087,-0.921053281444805,-0.920095670542737,
-0.918985743835248,-0.917000877428164,-0.907390088228778,-0.863464588742385,
-0.848811456111164,-0.845347801952433,-0.843355779121299,-0.841669260767104,
-0.839615475745699,-0.835766856509783,-0.809074557497812,-0.780038311021655,
-0.768540107948506,-0.766561054460697,-0.765333755002252,-0.764376564786102,
-0.763263991075153,-0.761266736608362,-0.751439973374302,-0.704364513561757,
-0.692649275263066,-0.689384952530542,-0.687457303238192,-0.685919709229434,
-0.68385386778967,-0.679947071754868,-0.650029385346784,-0.616943745121949,
-0.612101152449112,-0.610305936431538,-0.609237880818621,-0.608271458095834,
-0.606967092242401,-0.604001370873981,-0.575274682149757,-0.552641378009195),
 .UNSPECIFIED.);
#3766=B_SPLINE_CURVE_WITH_KNOTS('',3,(#265306,#265307,#265308,#265309,#265310,
#265311,#265312,#265313,#265314,#265315,#265316,#265317,#265318,#265319,
#265320,#265321,#265322,#265323,#265324,#265325,#265326,#265327,#265328,
#265329,#265330,#265331,#265332,#265333,#265334,#265335,#265336,#265337,
#265338,#265339,#265340,#265341,#265342,#265343,#265344,#265345,#265346,
#265347,#265348,#265349,#265350,#265351,#265352,#265353,#265354,#265355,
#265356,#265357,#265358,#265359,#265360,#265361,#265362,#265363,#265364,
#265365,#265366,#265367,#265368,#265369,#265370,#265371,#265372,#265373,
#265374,#265375,#265376,#265377,#265378,#265379,#265380,#265381,#265382,
#265383,#265384,#265385,#265386,#265387,#265388,#265389,#265390,#265391,
#265392,#265393,#265394,#265395,#265396,#265397,#265398,#265399,#265400,
#265401,#265402,#265403,#265404,#265405,#265406,#265407,#265408,#265409,
#265410,#265411,#265412,#265413,#265414,#265415,#265416,#265417,#265418,
#265419,#265420,#265421,#265422,#265423,#265424,#265425,#265426,#265427,
#265428,#265429,#265430,#265431,#265432,#265433,#265434,#265435,#265436,
#265437,#265438,#265439,#265440,#265441,#265442,#265443,#265444,#265445,
#265446,#265447,#265448,#265449,#265450,#265451,#265452,#265453,#265454,
#265455,#265456,#265457,#265458,#265459,#265460,#265461,#265462,#265463,
#265464,#265465,#265466,#265467,#265468,#265469,#265470,#265471,#265472,
#265473,#265474,#265475,#265476,#265477,#265478,#265479,#265480,#265481,
#265482,#265483,#265484,#265485,#265486,#265487,#265488,#265489,#265490,
#265491,#265492,#265493,#265494,#265495,#265496,#265497,#265498,#265499,
#265500,#265501,#265502,#265503,#265504,#265505,#265506,#265507,#265508,
#265509,#265510,#265511,#265512,#265513,#265514,#265515,#265516,#265517,
#265518,#265519,#265520,#265521,#265522,#265523,#265524,#265525,#265526,
#265527,#265528,#265529,#265530,#265531),.UNSPECIFIED.,.F.,.F.,(4,2,2,2,
2,2,2,2,2,2,2,2,2,2,2,2,2,2,2,2,2,2,2,2,2,2,2,2,2,2,2,2,2,2,2,2,2,2,2,2,
2,2,2,2,2,2,2,2,2,2,2,2,2,2,2,2,2,2,2,2,2,2,2,2,2,2,2,2,2,2,2,2,2,2,2,2,
2,2,2,2,2,2,2,2,2,2,2,2,2,2,2,2,2,2,2,2,2,2,2,2,2,2,2,2,2,2,2,2,2,2,2,2,
4),(-1.40944749342716,-1.39341217372204,-1.38939766731936,-1.38729366204968,
-1.38556862571454,-1.38356557824273,-1.38011938465242,-1.36609943832109,
-1.32538159487734,-1.3122440987815,-1.31007350367566,-1.30891513195081,
-1.30794829523266,-1.30674499624919,-1.30487078438903,-1.29559965722073,
-1.29127871094758,-1.26053787408271,-1.23952164303054,-1.23441501349005,
-1.23209829312566,-1.23034993719488,-1.22869918768659,-1.22593331459503,
-1.21854390903335,-1.21704073759394,-1.21538752143635,-1.1693810998379,
-1.15658942778471,-1.15443209770918,-1.15327643803154,-1.15230932218284,
-1.15110248956195,-1.14921704640649,-1.13976994424371,-1.11041363984206,
-1.08199531445636,-1.07807853968733,-1.07599461170209,-1.07443790241986,
-1.07247868709675,-1.06914158920952,-1.05691984351894,-1.05133094855607,
-1.01302705981138,-1.00091160154793,-0.998782282123513,-0.997632546935002,
-0.996665028114012,-0.995450931621492,-0.993541842385773,-0.983699521102618,
-0.98124865528132,-0.941498567575853,-0.925828771845722,-0.922572260369002,
-0.920443216336071,-0.918716304428376,-0.916731810120721,-0.913279383494423,
-0.897556901347341,-0.858707869884544,-0.853930048011537,-0.845115480821931,
-0.843092397721518,-0.841953294967731,-0.840984927385365,-0.839757263246613,
-0.837250028538095,-0.833950546160351,-0.825938029607814,-0.78911792581559,
-0.770464119929121,-0.767061437680973,-0.764887579109853,-0.763156956403062,
-0.761203256613833,-0.757891696030379,-0.744263910891211,-0.717368451479347,
-0.706878905392441,-0.690104605546518,-0.687722266993808,-0.686503839252694,
-0.685536096684031,-0.684389889831171,-0.682277023130487,-0.670530922458198,
-0.635328285677444,-0.631298277055792,-0.616016094628711,-0.611528431110734,
-0.609328508283789,-0.60759529638834,-0.605657690912757,-0.60241909369536,
-0.589736925929533,-0.543252636462868,-0.533888644662619,-0.532008087521358,
-0.530802633179374,-0.529835395091906,-0.528678123796034,-0.526513859732013,
-0.513552848733347,-0.464748666546273,-0.45722288305549,-0.454436655911459,
-0.452781775497855,-0.451034928629009,-0.448730155429978,-0.44369049343699,
-0.428866937278303),.UNSPECIFIED.);
#3767=B_SPLINE_CURVE_WITH_KNOTS('',3,(#265537,#265538,#265539,#265540,#265541,
#265542,#265543,#265544),.UNSPECIFIED.,.F.,.F.,(4,1,1,1,1,4),(84.8230078218033,
85.135950921962,86.1336829219519,87.1314149219419,88.1291469219317,88.3624145086695),
 .UNSPECIFIED.);
#3768=B_SPLINE_CURVE_WITH_KNOTS('',3,(#265545,#265546,#265547,#265548,#265549,
#265550,#265551,#265552,#265553,#265554,#265555,#265556,#265557,#265558,
#265559,#265560,#265561,#265562,#265563,#265564,#265565,#265566,#265567,
#265568,#265569,#265570,#265571,#265572,#265573,#265574,#265575,#265576,
#265577,#265578,#265579,#265580,#265581,#265582,#265583,#265584,#265585,
#265586,#265587,#265588,#265589,#265590,#265591,#265592,#265593,#265594,
#265595,#265596,#265597,#265598,#265599,#265600,#265601,#265602,#265603,
#265604,#265605,#265606,#265607,#265608,#265609,#265610,#265611,#265612,
#265613,#265614,#265615,#265616,#265617,#265618,#265619,#265620,#265621,
#265622,#265623,#265624,#265625,#265626,#265627,#265628,#265629,#265630,
#265631,#265632,#265633,#265634,#265635,#265636,#265637,#265638,#265639,
#265640,#265641,#265642,#265643,#265644,#265645,#265646,#265647,#265648,
#265649,#265650,#265651,#265652,#265653,#265654),.UNSPECIFIED.,.F.,.F.,
(4,2,2,2,2,2,2,2,2,2,2,2,2,2,2,2,2,2,2,2,2,2,2,2,2,2,2,2,2,2,2,2,2,2,2,
2,2,2,2,2,2,2,2,2,2,2,2,2,2,2,2,2,2,2,4),(-1.96159473691807,-1.93952011890684,
-1.93669937117787,-1.93477445021545,-1.93316774712418,-1.93146325880569,
-1.92936606932586,-1.92616665351387,-1.91082409396615,-1.89905984713847,
-1.8674817293113,-1.8580727791185,-1.85609269705463,-1.85498391836113,-1.85402631928996,
-1.85279372303083,-1.85079686979542,-1.8389624032588,-1.82584346183981,
-1.80018120789963,-1.7888770727583,-1.78387374741379,-1.77993815215203,
-1.77787545239181,-1.77617037939151,-1.77421343351222,-1.77090272207376,
-1.75831472800199,-1.75338403115019,-1.72272699557335,-1.70463561341793,
-1.70131815135195,-1.69989926638815,-1.69891283746,-1.69801097724501,-1.6965182063791,
-1.69266984937646,-1.69125473828562,-1.68334346359076,-1.63827022124228,
-1.62666187963963,-1.62353982285794,-1.62164354216759,-1.61992929429808,
-1.61772874126219,-1.61418946509796,-1.5903040320498,-1.55819333146133,
-1.5468999912072,-1.5448266421068,-1.5436976940666,-1.54274225646772,-1.54153737067804,
-1.53917644967491,-1.53325260190294),.UNSPECIFIED.);
#3769=B_SPLINE_CURVE_WITH_KNOTS('',3,(#265656,#265657,#265658,#265659,#265660,
#265661,#265662,#265663,#265664,#265665,#265666,#265667,#265668,#265669,
#265670,#265671,#265672,#265673,#265674,#265675,#265676,#265677,#265678,
#265679,#265680,#265681,#265682,#265683,#265684,#265685,#265686,#265687,
#265688,#265689,#265690,#265691,#265692,#265693,#265694,#265695,#265696,
#265697,#265698,#265699,#265700,#265701,#265702,#265703,#265704,#265705,
#265706,#265707,#265708,#265709,#265710,#265711,#265712,#265713,#265714,
#265715,#265716,#265717,#265718,#265719,#265720,#265721,#265722,#265723,
#265724,#265725,#265726,#265727,#265728,#265729,#265730,#265731,#265732,
#265733,#265734,#265735,#265736,#265737,#265738,#265739,#265740,#265741,
#265742,#265743,#265744,#265745,#265746,#265747,#265748,#265749,#265750,
#265751,#265752,#265753),.UNSPECIFIED.,.F.,.F.,(4,2,2,2,2,2,2,2,2,2,2,2,
2,2,2,2,2,2,2,2,2,2,2,2,2,2,2,2,2,2,2,2,2,2,2,2,2,2,2,2,2,2,2,2,2,2,2,2,
4),(-0.428866937278303,-0.42320732256552,-0.393569772979738,-0.39004470234996,
-0.378428445471691,-0.376427486662957,-0.37518558566945,-0.374216154435437,
-0.373087520844399,-0.371056144111157,-0.360932709214475,-0.308487302947778,
-0.307042580648101,-0.300995483957519,-0.298444783013751,-0.29683383005651,
-0.295056685101948,-0.292572473219648,-0.286488250833324,-0.277887406244554,
-0.226685948116768,-0.222177314863061,-0.220255388560647,-0.219139444607701,
-0.218265494335097,-0.217056418430856,-0.214642103968728,-0.188419145878424,
-0.150319415248422,-0.1449704987427,-0.142788118420279,-0.141168598663867,
-0.139462964355577,-0.137282324520504,-0.134745664090128,-0.130465186969945,
-0.121454504365611,-0.0929685813714968,-0.0802272210570355,-0.0748265394073259,
-0.0666376690446946,-0.0646614887242369,-0.0635331093220079,-0.0625636295368711,
-0.0613213308404195,-0.0587396392407635,-0.0553147526601607,-0.0130298331063881,
-0.000459572696942942),.UNSPECIFIED.);
#3770=B_SPLINE_CURVE_WITH_KNOTS('',3,(#265754,#265755,#265756,#265757,#265758,
#265759,#265760,#265761,#265762,#265763,#265764,#265765,#265766,#265767,
#265768,#265769,#265770,#265771,#265772,#265773,#265774,#265775,#265776,
#265777,#265778,#265779,#265780,#265781,#265782,#265783,#265784,#265785,
#265786,#265787,#265788,#265789,#265790,#265791,#265792,#265793,#265794,
#265795,#265796,#265797,#265798,#265799,#265800,#265801,#265802,#265803,
#265804,#265805,#265806,#265807,#265808,#265809,#265810,#265811,#265812,
#265813,#265814,#265815,#265816,#265817,#265818,#265819,#265820,#265821,
#265822,#265823,#265824,#265825,#265826,#265827,#265828,#265829,#265830,
#265831,#265832,#265833,#265834,#265835,#265836,#265837,#265838,#265839,
#265840,#265841,#265842,#265843,#265844,#265845,#265846,#265847,#265848,
#265849,#265850,#265851,#265852,#265853,#265854,#265855,#265856,#265857,
#265858,#265859,#265860,#265861,#265862,#265863,#265864,#265865,#265866,
#265867,#265868,#265869,#265870,#265871,#265872,#265873),.UNSPECIFIED.,
 .F.,.F.,(4,2,2,2,2,2,2,2,2,2,2,2,2,2,2,2,2,2,2,2,2,2,2,2,2,2,2,2,2,2,2,
2,2,2,2,2,2,2,2,2,2,2,2,2,2,2,2,2,2,2,2,2,2,2,2,2,2,2,2,4),(-1.96219528177021,
-1.95370052296186,-1.95103360796627,-1.94916151951121,-1.94754439225189,
-1.94587978338466,-1.94366525906557,-1.94012731532003,-1.92844967070181,
-1.88451417505534,-1.87289382871881,-1.87078677855098,-1.86964188147441,
-1.86867413363559,-1.86745429605936,-1.8650650684701,-1.84799858690288,
-1.81631719942177,-1.80410433588762,-1.79880954429901,-1.79587002244979,
-1.793299657197,-1.79152463932424,-1.7897579642343,-1.78763081253416,-1.78226529849946,
-1.74309513282626,-1.7200193782832,-1.71604681797504,-1.71456991018287,
-1.71356287136283,-1.71265678169625,-1.71118391709184,-1.70752106346708,
-1.67873805535211,-1.64390249333053,-1.63926596891892,-1.63703712684833,
-1.63530065824877,-1.63337941390567,-1.63021484440797,-1.61972326742647,
-1.57893502942534,-1.56340571911286,-1.56013208784729,-1.55876437831452,
-1.55777804298384,-1.55671550896419,-1.55498369372193,-1.54949434249468,
-1.50338177345386,-1.49215146453805,-1.48471520369557,-1.48202964566041,
-1.48021230505982,-1.47845040914041,-1.47634198436901,-1.47109369720167,
-1.43081744864416,-1.40984887783672),.UNSPECIFIED.);
#3771=B_SPLINE_CURVE_WITH_KNOTS('',3,(#265879,#265880,#265881,#265882,#265883,
#265884,#265885,#265886,#265887,#265888,#265889,#265890,#265891,#265892,
#265893,#265894,#265895,#265896,#265897,#265898,#265899,#265900,#265901,
#265902,#265903,#265904,#265905,#265906,#265907,#265908,#265909,#265910,
#265911,#265912,#265913,#265914,#265915,#265916,#265917,#265918,#265919,
#265920,#265921,#265922,#265923,#265924,#265925,#265926,#265927,#265928,
#265929,#265930,#265931,#265932,#265933,#265934,#265935,#265936,#265937,
#265938,#265939,#265940,#265941,#265942,#265943,#265944,#265945,#265946,
#265947,#265948,#265949,#265950,#265951,#265952,#265953,#265954,#265955,
#265956,#265957,#265958,#265959,#265960,#265961,#265962,#265963,#265964,
#265965,#265966,#265967,#265968,#265969,#265970,#265971,#265972,#265973,
#265974,#265975,#265976,#265977,#265978,#265979,#265980,#265981,#265982,
#265983,#265984,#265985,#265986,#265987,#265988,#265989,#265990,#265991,
#265992,#265993,#265994,#265995,#265996,#265997,#265998,#265999,#266000,
#266001,#266002,#266003,#266004,#266005,#266006,#266007,#266008,#266009,
#266010),.UNSPECIFIED.,.F.,.F.,(4,2,2,2,2,2,2,2,2,2,2,2,2,2,2,2,2,2,2,2,
2,2,2,2,2,2,2,2,2,2,2,2,2,2,2,2,2,2,2,2,2,2,2,2,2,2,2,2,2,2,2,2,2,2,2,2,
2,2,2,2,2,2,2,2,2,4),(-0.552515408999662,-0.550562583847312,-0.5485691073841,
-0.546883270987737,-0.544832656399416,-0.540997026342526,-0.514829200587625,
-0.487392633236008,-0.484148625212631,-0.47368318569461,-0.471756079770518,
-0.470544685020202,-0.469589052214475,-0.468465659835004,-0.466417306951006,
-0.455627025855104,-0.428473796370327,-0.399235265646561,-0.395645839730378,
-0.393454291221716,-0.391736822411601,-0.389855552778546,-0.386800318915267,
-0.375919967445849,-0.335228676595158,-0.318443097765979,-0.316090930433491,
-0.314888045426701,-0.313932893317432,-0.312802747807837,-0.310723237087268,
-0.299291011094534,-0.26620728990669,-0.243436705492283,-0.239928481705376,
-0.237737428683071,-0.236024553178534,-0.234123619485329,-0.230979565084765,
-0.219114615318666,-0.174190110811827,-0.162490105068495,-0.160326700915107,
-0.159154776059503,-0.158218456666738,-0.157094050736013,-0.155872990397383,
-0.153938599055296,-0.150166470411612,-0.140378836319171,-0.11862545123976,
-0.0878648919629591,-0.084302197542259,-0.0820946500710547,-0.0803795818287885,
-0.0784870873031429,-0.0753820560426363,-0.063965122043383,-0.018740854008447,
-0.0103186347474948,-0.00570293104685778,-0.00409665056792943,-0.00317259876107923,
-0.0022540795145313,-0.00121835079695155,-0.000484202096339386),
 .UNSPECIFIED.);
#3772=B_SPLINE_CURVE_WITH_KNOTS('',3,(#266011,#266012,#266013,#266014,#266015,
#266016),.UNSPECIFIED.,.F.,.F.,(4,1,1,4),(88.3624145086695,89.1268789219216,
90.1246109219115,91.1061847853801),.UNSPECIFIED.);
#3773=B_SPLINE_CURVE_WITH_KNOTS('',3,(#266017,#266018,#266019,#266020,#266021,
#266022,#266023,#266024,#266025,#266026,#266027,#266028,#266029,#266030,
#266031,#266032,#266033,#266034,#266035,#266036,#266037,#266038,#266039,
#266040,#266041,#266042,#266043,#266044,#266045,#266046,#266047,#266048,
#266049,#266050,#266051,#266052,#266053,#266054,#266055,#266056,#266057,
#266058,#266059,#266060,#266061,#266062,#266063,#266064,#266065,#266066,
#266067,#266068,#266069,#266070,#266071,#266072,#266073,#266074,#266075,
#266076,#266077,#266078,#266079,#266080,#266081,#266082,#266083,#266084,
#266085,#266086,#266087,#266088,#266089,#266090,#266091,#266092,#266093,
#266094,#266095,#266096,#266097,#266098,#266099,#266100,#266101,#266102,
#266103,#266104,#266105,#266106,#266107,#266108,#266109,#266110,#266111,
#266112,#266113,#266114,#266115,#266116,#266117,#266118,#266119,#266120,
#266121,#266122,#266123,#266124,#266125,#266126,#266127,#266128,#266129,
#266130,#266131,#266132,#266133,#266134,#266135,#266136,#266137,#266138,
#266139,#266140,#266141,#266142,#266143,#266144,#266145,#266146,#266147,
#266148,#266149,#266150,#266151,#266152,#266153,#266154,#266155,#266156,
#266157,#266158,#266159,#266160,#266161,#266162,#266163,#266164,#266165,
#266166,#266167,#266168,#266169,#266170,#266171,#266172,#266173,#266174,
#266175,#266176,#266177,#266178,#266179,#266180,#266181,#266182,#266183,
#266184,#266185,#266186,#266187,#266188,#266189,#266190,#266191,#266192,
#266193,#266194,#266195,#266196,#266197,#266198,#266199,#266200,#266201,
#266202,#266203,#266204,#266205,#266206,#266207,#266208,#266209,#266210,
#266211,#266212,#266213,#266214,#266215,#266216,#266217,#266218,#266219,
#266220,#266221,#266222,#266223,#266224,#266225,#266226,#266227,#266228,
#266229,#266230,#266231,#266232,#266233,#266234,#266235,#266236),
 .UNSPECIFIED.,.F.,.F.,(4,2,2,2,2,2,2,2,2,2,2,2,2,2,2,2,2,2,2,2,2,2,2,2,
2,2,2,2,2,2,2,2,2,2,2,2,2,2,2,2,2,2,2,2,2,2,2,2,2,2,2,2,2,2,2,2,2,2,2,2,
2,2,2,2,2,2,2,2,2,2,2,2,2,2,2,2,2,2,2,2,2,2,2,2,2,2,2,2,2,2,2,2,2,2,2,2,
2,2,2,2,2,2,2,2,2,2,2,2,2,4),(-1.40984887783672,-1.40858109118894,-1.40467723020394,
-1.40321037085499,-1.40220537363299,-1.40129743253415,-1.39981458330455,
-1.39609243885983,-1.37140866560196,-1.35938817646871,-1.33140447122275,
-1.32749555056619,-1.32541320021292,-1.32370482132622,-1.32168864233041,
-1.3181865089127,-1.30337769985326,-1.25918302244788,-1.25308002825821,
-1.24906041727865,-1.24757656543176,-1.24656799307939,-1.24566295435361,
-1.24419634518802,-1.24057167695035,-1.23902061351389,-1.18756430399654,
-1.17895522340259,-1.17286572874282,-1.17038045160242,-1.16860291337359,
-1.16699184729797,-1.16444150190383,-1.15839819515696,-1.10452286728443,
-1.0943374464735,-1.09230226256678,-1.09117265214809,-1.09020309048535,
-1.08896194864078,-1.08696400886707,-1.07541443221742,-1.03033748959946,
-1.0185435398649,-1.01537917837385,-1.01345774225161,-1.01172089414015,
-1.0094912778187,-1.00590444524125,-0.981178689891814,-0.951672077919365,
-0.939050690930436,-0.937003207722224,-0.935747283609764,-0.934776443434211,
-0.933657041478681,-0.931668500146943,-0.922282647414454,-0.900404865010337,
-0.867019850412069,-0.861414850269682,-0.859188866237729,-0.857558310418939,
-0.855796839911998,-0.853402109270118,-0.847857574366884,-0.84023561093515,
-0.794965376147343,-0.783282863548261,-0.781278104852778,-0.780034894991323,
-0.779065126994091,-0.777936889987388,-0.775908164871343,-0.765839114169796,
-0.714657205693773,-0.713806141586569,-0.706340538677844,-0.703563146092031,
-0.701909854653766,-0.700161992931681,-0.697851332971283,-0.692780254111559,
-0.672050503091122,-0.653164454804631,-0.638802024601857,-0.627540546591587,
-0.625556646775046,-0.624319843656763,-0.623350780780778,-0.622218397756811,
-0.620169910903498,-0.609733973074542,-0.584464527244917,-0.552991288534467,
-0.549396262463241,-0.547164277760831,-0.54542726420331,-0.54350735255492,
-0.540349444682187,-0.52862739641612,-0.483484264259973,-0.471893886236024,
-0.469893953694271,-0.468652245850116,-0.467682675238836,-0.466553544927272,
-0.464520450656246,-0.454370836409654,-0.428910700075966),.UNSPECIFIED.);
#3774=B_SPLINE_CURVE_WITH_KNOTS('',3,(#266241,#266242,#266243,#266244,#266245,
#266246,#266247,#266248,#266249,#266250,#266251,#266252,#266253,#266254,
#266255,#266256,#266257,#266258,#266259,#266260,#266261,#266262,#266263,
#266264,#266265,#266266,#266267,#266268,#266269,#266270,#266271,#266272,
#266273,#266274,#266275,#266276,#266277,#266278,#266279,#266280,#266281,
#266282,#266283,#266284,#266285,#266286,#266287,#266288,#266289,#266290,
#266291,#266292,#266293,#266294,#266295,#266296,#266297,#266298,#266299,
#266300,#266301,#266302,#266303,#266304,#266305,#266306,#266307,#266308,
#266309,#266310,#266311,#266312,#266313,#266314,#266315,#266316,#266317,
#266318,#266319,#266320,#266321,#266322,#266323,#266324,#266325,#266326,
#266327,#266328,#266329,#266330,#266331,#266332,#266333,#266334,#266335,
#266336,#266337,#266338,#266339,#266340,#266341,#266342,#266343,#266344,
#266345,#266346,#266347,#266348,#266349,#266350,#266351,#266352,#266353,
#266354,#266355,#266356,#266357,#266358,#266359,#266360,#266361,#266362,
#266363,#266364,#266365,#266366,#266367,#266368,#266369,#266370,#266371,
#266372,#266373,#266374,#266375,#266376,#266377,#266378,#266379,#266380,
#266381,#266382,#266383,#266384,#266385,#266386,#266387,#266388,#266389,
#266390,#266391,#266392,#266393,#266394,#266395,#266396,#266397,#266398,
#266399,#266400,#266401,#266402,#266403,#266404,#266405,#266406,#266407,
#266408,#266409,#266410,#266411,#266412,#266413,#266414,#266415,#266416,
#266417,#266418,#266419,#266420,#266421,#266422,#266423,#266424,#266425,
#266426,#266427,#266428,#266429,#266430,#266431,#266432,#266433,#266434,
#266435,#266436,#266437,#266438,#266439,#266440,#266441,#266442,#266443,
#266444,#266445,#266446),.UNSPECIFIED.,.F.,.F.,(4,2,2,2,2,2,2,2,2,2,2,2,
2,2,2,2,2,2,2,2,2,2,2,2,2,2,2,2,2,2,2,2,2,2,2,2,2,2,2,2,2,2,2,2,2,2,2,2,
2,2,2,2,2,2,2,2,2,2,2,2,2,2,2,2,2,2,2,2,2,2,2,2,2,2,2,2,2,2,2,2,2,2,2,2,
2,2,2,2,2,2,2,2,2,2,2,2,2,2,2,2,2,2,4),(-1.53266505380209,-1.49849600946528,
-1.48710556072061,-1.48400384552523,-1.48211260898317,-1.48039818453306,
-1.47819076986197,-1.47462682072641,-1.44310439031065,-1.41776663031675,
-1.40734159687292,-1.40531233398729,-1.40419321469861,-1.40323739549041,
-1.40202086612147,-1.40007635986551,-1.38926663946939,-1.38631959813282,
-1.35898967925782,-1.33284789840875,-1.32901378318673,-1.3269637447182,
-1.32527825990125,-1.32328505662668,-1.31981327193128,-1.30502274815647,
-1.26118259451269,-1.25163844020031,-1.24965817781261,-1.24854960049733,
-1.24759236799536,-1.2463604944228,-1.24436530067272,-1.23255653475088,
-1.18751008388276,-1.17589193455821,-1.17276982708576,-1.17087400197217,
-1.1691604792869,-1.16696129398885,-1.16342511082118,-1.13956092599805,
-1.10744951032914,-1.09615858182613,-1.09408594157186,-1.09295740992581,
-1.09200234303678,-1.09079794799921,-1.08843805730691,-1.07169894648921,
-1.03107582275221,-1.02015010044846,-1.01709097560005,-1.01520906006167,
-1.01349215354584,-1.01130289670794,-1.00772054554375,-0.980581083968393,
-0.954060344302462,-0.949032867604237,-0.940444816007854,-0.938455393840801,
-0.937332869243849,-0.936377337611118,-0.935165264038896,-0.932688358816214,
-0.929429284737236,-0.921520707418623,-0.885700290016859,-0.865897153891311,
-0.862480793973977,-0.860317759163765,-0.858608361647581,-0.856692083254173,
-0.853477020028921,-0.840744123011053,-0.793470065872141,-0.784804104307314,
-0.782808672427906,-0.781684673243543,-0.780729109699587,-0.779518558209755,
-0.777049896147459,-0.749724337367329,-0.712925618763617,-0.707494981872777,
-0.705315060930709,-0.703710292484619,-0.701969196985548,-0.699588995927991,
-0.694019611656257,-0.686328468736558,-0.641267920883151,-0.6294629149485,
-0.627467387413243,-0.626235322541208,-0.625277945165936,-0.62416919491249,
-0.622188627486733,-0.612642294534342,-0.568820414856862,-0.554034479445235,
-0.552515408999662),.UNSPECIFIED.);
#3775=B_SPLINE_CURVE_WITH_KNOTS('',3,(#266448,#266449,#266450,#266451,#266452,
#266453,#266454,#266455,#266456,#266457,#266458,#266459,#266460,#266461,
#266462,#266463,#266464,#266465,#266466,#266467,#266468,#266469,#266470,
#266471,#266472,#266473,#266474,#266475,#266476,#266477,#266478,#266479,
#266480,#266481,#266482,#266483,#266484,#266485,#266486,#266487,#266488,
#266489,#266490,#266491,#266492,#266493,#266494,#266495,#266496,#266497,
#266498,#266499,#266500,#266501,#266502,#266503,#266504,#266505,#266506,
#266507,#266508,#266509,#266510,#266511,#266512,#266513,#266514,#266515,
#266516,#266517,#266518,#266519,#266520,#266521,#266522,#266523,#266524,
#266525,#266526,#266527,#266528,#266529,#266530,#266531,#266532,#266533,
#266534,#266535,#266536,#266537,#266538,#266539,#266540,#266541,#266542,
#266543,#266544,#266545),.UNSPECIFIED.,.F.,.F.,(4,2,2,2,2,2,2,2,2,2,2,2,
2,2,2,2,2,2,2,2,2,2,2,2,2,2,2,2,2,2,2,2,2,2,2,2,2,2,2,2,2,2,2,2,2,2,2,2,
4),(-0.428910700075966,-0.401327195880147,-0.394676408531252,-0.392024963494874,
-0.390395571031352,-0.388633668509475,-0.386235334247601,-0.380668695047072,
-0.373007130517893,-0.32778432842315,-0.316133126173067,-0.31413021888457,
-0.312887654141444,-0.311918061048298,-0.310789649379656,-0.308759681097413,
-0.298664753279152,-0.246895264192716,-0.239255997029793,-0.236453046160825,
-0.234794999368418,-0.233049746963605,-0.23075535519183,-0.225771710496655,
-0.205726179648854,-0.179684164004229,-0.160806562752999,-0.158408697854989,
-0.157199625455021,-0.156248431113482,-0.155335549346347,-0.153591087697067,
-0.147364149919041,-0.136098558475487,-0.09566174766719,-0.0845010069003123,
-0.0812663184104489,-0.0793296905778867,-0.0777698332817407,-0.0756540875679837,
-0.0715839632477447,-0.0372611061454265,-0.0151554489785241,-0.0104177429443904,
-0.00409972392282309,-0.00231064211441393,-0.00123989900939373,-0.000618795737507542,
-0.000459177337394708),.UNSPECIFIED.);
#3776=B_SPLINE_CURVE_WITH_KNOTS('',3,(#266546,#266547,#266548,#266549,#266550,
#266551,#266552,#266553,#266554,#266555,#266556,#266557,#266558,#266559,
#266560,#266561,#266562,#266563,#266564,#266565,#266566,#266567,#266568,
#266569,#266570,#266571,#266572,#266573,#266574,#266575,#266576,#266577,
#266578,#266579,#266580,#266581,#266582,#266583,#266584,#266585,#266586,
#266587,#266588,#266589,#266590,#266591,#266592,#266593,#266594,#266595,
#266596,#266597,#266598,#266599,#266600,#266601,#266602,#266603,#266604,
#266605,#266606,#266607,#266608,#266609,#266610,#266611,#266612,#266613,
#266614,#266615,#266616,#266617,#266618,#266619,#266620,#266621,#266622,
#266623,#266624,#266625,#266626,#266627,#266628,#266629,#266630,#266631,
#266632,#266633,#266634,#266635,#266636,#266637,#266638,#266639,#266640,
#266641,#266642,#266643,#266644,#266645,#266646,#266647,#266648,#266649,
#266650,#266651,#266652,#266653,#266654,#266655,#266656,#266657,#266658,
#266659,#266660,#266661,#266662,#266663,#266664,#266665,#266666,#266667,
#266668,#266669,#266670,#266671),.UNSPECIFIED.,.F.,.F.,(4,2,2,2,2,2,2,2,
2,2,2,2,2,2,2,2,2,2,2,2,2,2,2,2,2,2,2,2,2,2,2,2,2,2,2,2,2,2,2,2,2,2,2,2,
2,2,2,2,2,2,2,2,2,2,2,2,2,2,2,2,2,2,4),(-1.96154488249404,-1.96129893185349,
-1.96025239001222,-1.9579087962454,-1.94319819707872,-1.91410580065968,
-1.89310558206934,-1.88800192046861,-1.8856862811165,-1.8839386339106,-1.88228847468457,
-1.87952340142396,-1.87213479768615,-1.87094141939202,-1.82795747142864,
-1.81600109233696,-1.80952153450638,-1.80775354808749,-1.80683937008797,
-1.80593025890328,-1.80475301194569,-1.802498762158,-1.78919770031518,-1.76313605075455,
-1.7356378806577,-1.73174007341828,-1.72966065945942,-1.72795317045841,
-1.72593625957732,-1.72242835716419,-1.70751796603955,-1.66322895052082,
-1.65429374669277,-1.65233429275933,-1.65122159332096,-1.65025023090843,
-1.64900623071248,-1.64695283179287,-1.63415931018071,-1.60492299736787,
-1.58224770233286,-1.57693905252869,-1.5745862218616,-1.57283236788994,
-1.57119218814615,-1.56848112614209,-1.5614399657562,-1.50899688680722,
-1.49877950519643,-1.49674303261131,-1.49561336209561,-1.49464415928807,
-1.49340400723117,-1.49140867905184,-1.47990365604023,-1.43489257299263,
-1.42302041755802,-1.41984992196797,-1.4179275235888,-1.41619158153964,
-1.41396560084263,-1.41038966913363,-1.40945693535865),.UNSPECIFIED.);
#3777=B_SPLINE_CURVE_WITH_KNOTS('',3,(#266677,#266678,#266679,#266680,#266681,
#266682,#266683,#266684,#266685,#266686,#266687,#266688,#266689,#266690,
#266691,#266692,#266693,#266694,#266695,#266696,#266697,#266698,#266699,
#266700,#266701,#266702,#266703,#266704,#266705,#266706,#266707,#266708,
#266709,#266710,#266711,#266712,#266713,#266714,#266715,#266716,#266717,
#266718,#266719,#266720,#266721,#266722,#266723,#266724,#266725,#266726,
#266727,#266728,#266729,#266730,#266731,#266732,#266733,#266734,#266735,
#266736,#266737,#266738,#266739,#266740,#266741,#266742,#266743,#266744,
#266745,#266746,#266747,#266748,#266749,#266750,#266751,#266752,#266753,
#266754,#266755,#266756,#266757,#266758,#266759,#266760,#266761,#266762,
#266763,#266764,#266765,#266766,#266767,#266768,#266769,#266770,#266771,
#266772,#266773,#266774,#266775,#266776,#266777,#266778,#266779,#266780,
#266781,#266782,#266783,#266784,#266785,#266786,#266787,#266788,#266789,
#266790,#266791,#266792,#266793,#266794,#266795,#266796,#266797,#266798,
#266799,#266800,#266801,#266802,#266803,#266804,#266805,#266806,#266807,
#266808,#266809,#266810,#266811,#266812,#266813,#266814,#266815,#266816,
#266817,#266818,#266819,#266820,#266821,#266822,#266823,#266824),
 .UNSPECIFIED.,.F.,.F.,(4,2,2,2,2,2,2,2,2,2,2,2,2,2,2,2,2,2,2,2,2,2,2,2,
2,2,2,2,2,2,2,2,2,2,2,2,2,2,2,2,2,2,2,2,2,2,2,2,2,2,2,2,2,2,2,2,2,2,2,2,
2,2,2,2,2,2,2,2,2,2,2,2,2,4),(-0.552785672327454,-0.537478823530765,-0.535041105726873,
-0.533836357281231,-0.532880724479598,-0.53175118269923,-0.529675817416682,
-0.518346069941391,-0.485991210353301,-0.46239336053074,-0.458862174919824,
-0.456663746250476,-0.454949383812827,-0.453051171528342,-0.449921762038409,
-0.438236129923043,-0.393174928575462,-0.381380546581408,-0.37938490740365,
-0.378152473444212,-0.377194615256916,-0.376085086079105,-0.374102589276208,
-0.364536293915182,-0.320698355109572,-0.305912891806877,-0.302439747567133,
-0.300445349993075,-0.298758615846738,-0.296706764005296,-0.292868382674435,
-0.266655622928351,-0.238950353662178,-0.234067936368551,-0.225323902570269,
-0.223321968350755,-0.222196118729412,-0.221240135041514,-0.220030521840422,
-0.217568582065273,-0.19101014965597,-0.153296724498725,-0.15041593525838,
-0.147138819700689,-0.145017460068174,-0.143352928632042,-0.143315551472416,
-0.143286868528517,-0.143264725003336,-0.143226694481738,-0.143190628643951,
-0.143156370934165,-0.143123781088961,-0.143092733072147,-0.143063113317469,
-0.143034819221448,-0.143007757850762,-0.142981844827678,-0.142957003365903,
-0.142933163430683,-0.142910261012062,-0.140840952239203,-0.138600365909729,
-0.135018779518392,-0.127980672657713,-0.087073879279006,-0.0701942544411946,
-0.0678293639304637,-0.0666234069992897,-0.065667621763324,-0.0645388450072447,
-0.0624673244303813,-0.0512217167953855,-0.000460369818743296),
 .UNSPECIFIED.);
#3778=B_SPLINE_CURVE_WITH_KNOTS('',3,(#266825,#266826,#266827,#266828,#266829,
#266830,#266831,#266832,#266833,#266834,#266835,#266836,#266837,#266838,
#266839,#266840,#266841,#266842,#266843,#266844,#266845,#266846,#266847,
#266848,#266849,#266850,#266851,#266852,#266853,#266854,#266855,#266856,
#266857,#266858,#266859,#266860,#266861,#266862,#266863,#266864,#266865,
#266866,#266867,#266868,#266869,#266870,#266871,#266872,#266873,#266874,
#266875,#266876,#266877,#266878,#266879,#266880,#266881,#266882,#266883,
#266884,#266885,#266886,#266887,#266888,#266889,#266890,#266891,#266892,
#266893,#266894,#266895,#266896,#266897,#266898,#266899,#266900,#266901,
#266902,#266903,#266904,#266905,#266906,#266907,#266908,#266909,#266910,
#266911,#266912,#266913,#266914,#266915,#266916,#266917,#266918,#266919,
#266920,#266921,#266922,#266923,#266924,#266925,#266926),.UNSPECIFIED.,
 .F.,.F.,(4,2,2,2,2,2,2,2,2,2,2,2,2,2,2,2,2,2,2,2,2,2,2,2,2,2,2,2,2,2,2,
2,2,2,2,2,2,2,2,2,2,2,2,2,2,2,2,2,2,2,4),(-1.96079981085505,-1.95342043335075,
-1.95131157403659,-1.94965857635379,-1.94799529337163,-1.9460955291017,
-1.94295263153211,-1.93241406535318,-1.88522823021898,-1.87425087267518,
-1.87219395948775,-1.87106908459013,-1.87011413961342,-1.86890610977445,
-1.86652782879441,-1.84815840603686,-1.81254155119779,-1.80345640271211,
-1.79916560383019,-1.79663528584534,-1.79436126316174,-1.79266137729354,
-1.79104947431068,-1.78840903253175,-1.78169311163644,-1.72867487316804,
-1.7185462305063,-1.71653301758151,-1.7154174301808,-1.71446131737511,-1.71324014607761,
-1.71128008636296,-1.70015445102028,-1.69555049687401,-1.6700740172427,
-1.64408383727216,-1.64025351746894,-1.63820437096798,-1.63651903758875,
-1.63452532834209,-1.63105092637364,-1.61622102525889,-1.57234855170949,
-1.56287849928834,-1.56090274729691,-1.55979520366588,-1.55883791170082,
-1.55760472060856,-1.55560497128255,-1.54369028547836,-1.53266505380209),
 .UNSPECIFIED.);
#3779=B_SPLINE_CURVE_WITH_KNOTS('',3,(#266927,#266928,#266929,#266930,#266931,
#266932,#266933,#266934,#266935,#266936,#266937,#266938,#266939,#266940,
#266941,#266942,#266943,#266944,#266945,#266946,#266947,#266948,#266949,
#266950,#266951,#266952,#266953,#266954,#266955,#266956,#266957,#266958,
#266959,#266960,#266961,#266962,#266963,#266964,#266965,#266966,#266967,
#266968,#266969,#266970,#266971,#266972,#266973,#266974,#266975,#266976,
#266977,#266978,#266979,#266980,#266981,#266982,#266983,#266984,#266985,
#266986,#266987,#266988,#266989,#266990,#266991,#266992,#266993,#266994,
#266995,#266996,#266997,#266998,#266999,#267000,#267001,#267002,#267003,
#267004,#267005,#267006,#267007,#267008,#267009,#267010,#267011,#267012,
#267013,#267014,#267015,#267016,#267017,#267018,#267019,#267020,#267021,
#267022,#267023,#267024,#267025,#267026,#267027,#267028,#267029,#267030,
#267031,#267032,#267033,#267034,#267035,#267036,#267037,#267038,#267039,
#267040,#267041,#267042,#267043,#267044,#267045,#267046,#267047,#267048,
#267049,#267050,#267051,#267052,#267053,#267054,#267055,#267056,#267057,
#267058,#267059,#267060,#267061,#267062,#267063,#267064,#267065,#267066,
#267067,#267068,#267069,#267070,#267071,#267072,#267073,#267074,#267075,
#267076,#267077,#267078,#267079,#267080,#267081,#267082,#267083,#267084,
#267085,#267086,#267087,#267088,#267089,#267090,#267091,#267092,#267093,
#267094,#267095,#267096,#267097,#267098,#267099,#267100,#267101,#267102,
#267103,#267104,#267105,#267106,#267107,#267108,#267109,#267110,#267111,
#267112,#267113,#267114,#267115,#267116,#267117,#267118,#267119,#267120,
#267121,#267122,#267123,#267124,#267125,#267126,#267127,#267128),
 .UNSPECIFIED.,.F.,.F.,(4,2,2,2,2,2,2,2,2,2,2,2,2,2,2,2,2,2,2,2,2,2,2,2,
2,2,2,2,2,2,2,2,2,2,2,2,2,2,2,2,2,2,2,2,2,2,2,2,2,2,2,2,2,2,2,2,2,2,2,2,
2,2,2,2,2,2,2,2,2,2,2,2,2,2,2,2,2,2,2,2,2,2,2,2,2,2,2,2,2,2,2,2,2,2,2,2,
2,2,2,2,4),(-1.40945693535865,-1.37838947460745,-1.35350089257598,-1.34314655046212,
-1.34110272464701,-1.33997150714698,-1.33900255738699,-1.33776476753182,
-1.33577714057381,-1.32443042040914,-1.27960865926656,-1.27156830356978,
-1.26579019131671,-1.2633563589074,-1.26158854394664,-1.25996766950727,
-1.25777861763317,-1.25238889280262,-1.21475513144017,-1.1892136361745,
-1.18607180540606,-1.18472672675155,-1.18374430946283,-1.18267285418179,
-1.18090028874194,-1.17506163266528,-1.12484563434287,-1.11187552262099,
-1.1086148391072,-1.10667277217922,-1.10494103203791,-1.10275038125122,
-1.09929102276075,-1.07907376490314,-1.04372319126061,-1.03195855793559,
-1.02984524507958,-1.02869914521696,-1.0277316977101,-1.02651390722933,
-1.02413359502781,-1.0074127280503,-0.981260395843197,-0.957535941138206,
-0.953973782830811,-0.951752033499747,-0.950016734268253,-0.948092329504277,
-0.944912211015954,-0.932926685416591,-0.88796576599348,-0.876512901613823,
-0.874520089272509,-0.873280734560196,-0.872311645999344,-0.87118151228185,
-0.869142745928059,-0.858881141785129,-0.821460108992222,-0.801670676264679,
-0.79822646347277,-0.796040205828108,-0.794308666794342,-0.792363384214712,
-0.789089011803875,-0.775948177113348,-0.729180522752018,-0.720544459338339,
-0.718534711110628,-0.717398679476688,-0.716439316217247,-0.715212574978455,
-0.712709810187156,-0.709417770130657,-0.701431202850471,-0.664923375561086,
-0.645944085854017,-0.642529522144502,-0.640352102250721,-0.638621212366825,
-0.636669936587437,-0.633369138805949,-0.619884768039655,-0.593493089583819,
-0.567564600634969,-0.563843988058514,-0.562361399865462,-0.561453505618237,
-0.560448450082026,-0.558981322531756,-0.555075623720123,-0.532819587383517,
-0.492605477471602,-0.487353244556039,-0.485244175143252,-0.483482094361268,
-0.481664935570213,-0.478980351516481,-0.47155145660358,-0.460334590086816,
-0.428878856138385),.UNSPECIFIED.);
#3780=B_SPLINE_CURVE_WITH_KNOTS('',3,(#267133,#267134,#267135,#267136,#267137,
#267138,#267139,#267140,#267141,#267142,#267143,#267144,#267145,#267146,
#267147,#267148,#267149,#267150,#267151,#267152,#267153,#267154,#267155,
#267156,#267157,#267158,#267159,#267160,#267161,#267162,#267163,#267164,
#267165,#267166,#267167,#267168,#267169,#267170,#267171,#267172,#267173,
#267174,#267175,#267176,#267177,#267178,#267179,#267180,#267181,#267182,
#267183,#267184,#267185,#267186,#267187,#267188,#267189,#267190,#267191,
#267192,#267193,#267194,#267195,#267196,#267197,#267198,#267199,#267200,
#267201,#267202,#267203,#267204,#267205,#267206,#267207,#267208,#267209,
#267210,#267211,#267212,#267213,#267214,#267215,#267216,#267217,#267218,
#267219,#267220,#267221,#267222,#267223,#267224,#267225,#267226,#267227,
#267228,#267229,#267230,#267231,#267232,#267233,#267234,#267235,#267236,
#267237,#267238,#267239,#267240,#267241,#267242,#267243,#267244,#267245,
#267246,#267247,#267248,#267249,#267250,#267251,#267252,#267253,#267254,
#267255,#267256,#267257,#267258,#267259,#267260,#267261,#267262,#267263,
#267264,#267265,#267266,#267267,#267268,#267269,#267270,#267271,#267272,
#267273,#267274,#267275,#267276,#267277,#267278,#267279,#267280,#267281,
#267282,#267283,#267284,#267285,#267286,#267287,#267288,#267289,#267290,
#267291,#267292,#267293,#267294,#267295,#267296,#267297,#267298,#267299,
#267300,#267301,#267302,#267303,#267304,#267305,#267306,#267307,#267308,
#267309,#267310,#267311,#267312,#267313,#267314,#267315,#267316,#267317,
#267318,#267319,#267320,#267321,#267322,#267323,#267324,#267325,#267326,
#267327,#267328,#267329,#267330,#267331,#267332,#267333,#267334,#267335,
#267336,#267337,#267338,#267339,#267340,#267341,#267342,#267343,#267344,
#267345,#267346,#267347,#267348),.UNSPECIFIED.,.F.,.F.,(4,2,2,2,2,2,2,2,
2,2,2,2,2,2,2,2,2,2,2,2,2,2,2,2,2,2,2,2,2,2,2,2,2,2,2,2,2,2,2,2,2,2,2,2,
2,2,2,2,2,2,2,2,2,2,2,2,2,2,2,2,2,2,2,2,2,2,2,2,2,2,2,2,2,2,2,2,2,2,2,2,
2,2,2,2,2,2,2,2,2,2,2,2,2,2,2,2,2,2,2,2,2,2,2,2,2,2,2,4),(-1.53329438485854,
-1.5259062052296,-1.480603133297,-1.47089302354938,-1.46890278666044,-1.46779191186589,
-1.4668347797346,-1.46560574246885,-1.46362039520212,-1.45199453136208,
-1.44888351571002,-1.41965858942628,-1.40409704144739,-1.39472874895801,
-1.39182748500431,-1.38997986613554,-1.38825086476795,-1.38598439861036,
-1.38092228936624,-1.33921241411468,-1.31795382282117,-1.31415074823298,
-1.31270999364298,-1.3117193119623,-1.31082201732667,-1.30935303329966,
-1.30565000066324,-1.28163689618677,-1.2617921957469,-1.24243706497407,
-1.23756759700035,-1.23531164353587,-1.23359005635413,-1.23195044922239,
-1.22916913987559,-1.22153457805077,-1.22056396702445,-1.21883268540074,
-1.17714976079237,-1.16547971816755,-1.1612364069134,-1.15819387794447,
-1.15687594263843,-1.15590746511566,-1.15484567458574,-1.15307864441314,
-1.14717069880328,-1.1141705894017,-1.08519128108787,-1.08129925294514,
-1.07923645695844,-1.07769910610654,-1.07576912342217,-1.07249437895039,
-1.0606701652163,-1.01368349094619,-1.00385963691052,-1.00186237793883,
-1.00074974592119,-0.999792464813292,-0.998565005983239,-0.996585627703639,
-0.985082169055234,-0.981243770102034,-0.94648392980948,-0.940296456308359,
-0.928388678935088,-0.925105771095938,-0.923173795571481,-0.921636409691605,
-0.91957555372042,-0.915693786515719,-0.887357715187065,-0.857848729190882,
-0.848317177892823,-0.846441697426153,-0.845245714726122,-0.844290582937609,
-0.843154004247797,-0.841045701945348,-0.828983198969002,-0.790910921974196,
-0.784352392714729,-0.77265137104738,-0.769387997807632,-0.767460329471485,
-0.765922399620724,-0.763855692893597,-0.759945880358528,-0.729863261114264,
-0.696369525917018,-0.691725220676978,-0.690114729029839,-0.689189743577349,
-0.688219123186576,-0.686888641328333,-0.683774807169631,-0.658243791503835,
-0.62048296779988,-0.617607930943817,-0.61432870249477,-0.61220672882242,
-0.61050012928326,-0.608555078341277,-0.60521272881707,-0.590762969089393,
-0.558786816909496,-0.552785672327454),.UNSPECIFIED.);
#3781=B_SPLINE_CURVE_WITH_KNOTS('',3,(#267350,#267351,#267352,#267353,#267354,
#267355,#267356,#267357,#267358,#267359,#267360,#267361,#267362,#267363,
#267364,#267365,#267366,#267367,#267368,#267369,#267370,#267371,#267372,
#267373,#267374,#267375,#267376,#267377,#267378,#267379,#267380,#267381,
#267382,#267383,#267384,#267385,#267386,#267387,#267388,#267389,#267390,
#267391,#267392,#267393,#267394,#267395,#267396,#267397,#267398,#267399,
#267400,#267401,#267402,#267403,#267404,#267405,#267406,#267407,#267408,
#267409,#267410,#267411,#267412,#267413,#267414,#267415,#267416,#267417,
#267418,#267419,#267420,#267421,#267422,#267423,#267424,#267425,#267426,
#267427,#267428,#267429,#267430,#267431,#267432,#267433,#267434,#267435,
#267436,#267437,#267438,#267439,#267440,#267441,#267442,#267443,#267444,
#267445,#267446,#267447,#267448,#267449,#267450,#267451,#267452,#267453,
#267454,#267455,#267456,#267457),.UNSPECIFIED.,.F.,.F.,(4,2,2,2,2,2,2,2,
2,2,2,2,2,2,2,2,2,2,2,2,2,2,2,2,2,2,2,2,2,2,2,2,2,2,2,2,2,2,2,2,2,2,2,2,
2,2,2,2,2,2,2,2,2,4),(-0.428878856138385,-0.414539067174868,-0.408745235198775,
-0.406977463123421,-0.405906873567645,-0.404923712968806,-0.403575456785685,
-0.400416589639969,-0.385946393982195,-0.347982234667841,-0.334070851631951,
-0.330631589446018,-0.32862967323089,-0.326903876317232,-0.324796765404635,
-0.32076958170194,-0.315694366763854,-0.304206035376409,-0.280181266764184,
-0.274913526395652,-0.254306251572381,-0.251881356743021,-0.250653831437889,
-0.249685462227338,-0.248546220611693,-0.246465956318455,-0.235410961878035,
-0.219504911377629,-0.181627390737452,-0.176260141162723,-0.174074615602289,
-0.172454327115028,-0.170720520256211,-0.168358957171198,-0.16571277973357,
-0.161160663846559,-0.151327650494007,-0.117249102053957,-0.0986305884952339,
-0.0962266732314018,-0.0950036062527597,-0.0940355351680851,-0.0928928735374122,
-0.0907967011352938,-0.0794126896682031,-0.0360801441414657,-0.0244912492889776,
-0.0199920016666521,-0.0177898190531764,-0.0161315529739948,-0.01451368040225,
-0.0126359538946524,-0.00995542805505722,-0.000458834895657056),
 .UNSPECIFIED.);
#3782=B_SPLINE_CURVE_WITH_KNOTS('',3,(#267458,#267459,#267460,#267461,#267462,
#267463,#267464,#267465,#267466,#267467,#267468,#267469,#267470,#267471,
#267472,#267473,#267474,#267475,#267476,#267477,#267478,#267479,#267480,
#267481,#267482,#267483,#267484,#267485,#267486,#267487,#267488,#267489,
#267490,#267491,#267492,#267493,#267494,#267495,#267496,#267497,#267498,
#267499,#267500,#267501,#267502,#267503,#267504,#267505,#267506,#267507,
#267508,#267509,#267510,#267511,#267512,#267513,#267514,#267515,#267516,
#267517,#267518,#267519,#267520,#267521,#267522,#267523,#267524,#267525,
#267526,#267527,#267528,#267529,#267530,#267531,#267532,#267533,#267534,
#267535,#267536,#267537,#267538,#267539,#267540,#267541,#267542,#267543,
#267544,#267545,#267546,#267547,#267548,#267549,#267550,#267551,#267552,
#267553,#267554,#267555,#267556,#267557),.UNSPECIFIED.,.F.,.F.,(4,3,3,3,
3,3,3,3,3,3,3,3,3,3,3,3,3,3,3,3,3,3,3,3,3,3,3,3,3,3,3,3,3,4),(109.955742876003,
110.079083637333,110.202919711225,110.327367828986,110.35147273413,110.463170399599,
110.574669461548,110.686057610363,110.797377778424,110.90867280093,111.020068420613,
111.131510063134,111.243168982288,111.348806584787,111.460504250256,111.572003312205,
111.68339146102,111.794711629081,111.906006651587,112.017402271271,112.128843913791,
112.240502832945,112.346140435444,112.457838100913,112.569337162862,112.680725311677,
112.792045479738,112.903340502244,113.014736121928,113.126177764448,113.237836683603,
113.343474286101,113.45515745485,113.494796146192),.UNSPECIFIED.);
#3783=B_SPLINE_CURVE_WITH_KNOTS('',3,(#267563,#267564,#267565,#267566,#267567,
#267568,#267569,#267570,#267571,#267572,#267573,#267574,#267575,#267576,
#267577,#267578,#267579,#267580,#267581,#267582,#267583,#267584,#267585,
#267586,#267587,#267588,#267589,#267590,#267591,#267592,#267593,#267594,
#267595,#267596,#267597,#267598,#267599,#267600,#267601,#267602,#267603,
#267604,#267605,#267606,#267607,#267608,#267609,#267610,#267611,#267612,
#267613,#267614,#267615,#267616,#267617,#267618,#267619,#267620,#267621,
#267622,#267623,#267624,#267625,#267626,#267627,#267628,#267629,#267630,
#267631,#267632,#267633,#267634,#267635,#267636,#267637,#267638,#267639,
#267640,#267641,#267642,#267643,#267644,#267645,#267646,#267647,#267648,
#267649,#267650,#267651,#267652,#267653,#267654,#267655,#267656,#267657,
#267658,#267659,#267660,#267661,#267662,#267663,#267664,#267665,#267666,
#267667,#267668,#267669,#267670,#267671,#267672,#267673,#267674,#267675,
#267676,#267677,#267678,#267679,#267680,#267681,#267682,#267683,#267684),
 .UNSPECIFIED.,.F.,.F.,(4,2,2,2,2,2,2,2,2,2,2,2,2,2,2,2,2,2,2,2,2,2,2,2,
2,2,2,2,2,2,2,2,2,2,2,2,2,2,2,2,2,2,2,2,2,2,2,2,2,2,2,2,2,2,2,2,2,2,2,2,
4),(-0.552744682324884,-0.539491799904537,-0.524713764816097,-0.52124195532014,
-0.519248262641362,-0.517562088831951,-0.515510874819621,-0.511673554868996,
-0.485460133163769,-0.457693480591708,-0.452233774608359,-0.444074270314207,
-0.442116424640607,-0.441000858687102,-0.440044196854515,-0.438821591884561,
-0.436292667323589,-0.407658195450849,-0.372370765588914,-0.366856423207403,
-0.364662113907197,-0.363053470609611,-0.361314590389507,-0.358948910088451,
-0.353466211478536,-0.345929895836228,-0.300698588616303,-0.288776636779942,
-0.286775816551164,-0.285542020707468,-0.284584289440006,-0.283476262385566,
-0.281499724480592,-0.272026633724511,-0.228158122524084,-0.213327162248706,
-0.209851511001255,-0.207856903484334,-0.206170706652158,-0.204120382005885,
-0.200287483806872,-0.182154629221436,-0.142678681496718,-0.13285990295235,
-0.130967715539691,-0.129766735717618,-0.128811483606482,-0.127904117109684,
-0.126191168710766,-0.119835656448654,-0.108114842245078,-0.0913752337551362,
-0.0611227125542174,-0.0555039882382235,-0.0532918923060263,-0.0516785676441627,
-0.049942542441728,-0.0475947669337017,-0.0450050725458054,-0.0369382998639502,
-0.000460337843206879),.UNSPECIFIED.);
#3784=B_SPLINE_CURVE_WITH_KNOTS('',3,(#267685,#267686,#267687,#267688,#267689,
#267690,#267691,#267692,#267693,#267694,#267695,#267696,#267697,#267698,
#267699,#267700,#267701,#267702,#267703,#267704,#267705,#267706,#267707,
#267708,#267709,#267710,#267711,#267712,#267713,#267714,#267715,#267716,
#267717,#267718,#267719,#267720,#267721,#267722,#267723,#267724,#267725,
#267726,#267727,#267728,#267729,#267730,#267731,#267732,#267733,#267734,
#267735,#267736,#267737,#267738,#267739,#267740,#267741,#267742,#267743,
#267744,#267745,#267746,#267747,#267748,#267749,#267750,#267751,#267752,
#267753,#267754,#267755,#267756,#267757,#267758,#267759,#267760,#267761,
#267762,#267763,#267764,#267765,#267766,#267767,#267768,#267769,#267770,
#267771,#267772,#267773,#267774,#267775,#267776,#267777,#267778,#267779,
#267780,#267781,#267782,#267783,#267784,#267785,#267786,#267787,#267788,
#267789,#267790,#267791,#267792,#267793,#267794,#267795,#267796),
 .UNSPECIFIED.,.F.,.F.,(4,2,2,2,2,2,2,2,2,2,2,2,2,2,2,2,2,2,2,2,2,2,2,2,
2,2,2,2,2,2,2,2,2,2,2,2,2,2,2,2,2,2,2,2,2,2,2,2,2,2,2,2,2,2,2,4),(-1.96112117373986,
-1.93832776576274,-1.93664462059022,-1.9355272830046,-1.93462067799193,
-1.93366577556876,-1.93246347086777,-1.9300355826801,-1.91002528253084,
-1.89268236084572,-1.87306924994882,-1.86192616881238,-1.85883101451738,
-1.85694109581914,-1.8552261222988,-1.85301554977393,-1.8494414463733,-1.82349909405135,
-1.79766957712133,-1.78738618786051,-1.78156964225285,-1.7799209000981,
-1.77901772498458,-1.77806129524977,-1.77683803196797,-1.77487138272681,
-1.76361468733173,-1.7608577783962,-1.73413386995263,-1.71639119420624,
-1.70637685635215,-1.7032699767239,-1.70137743634478,-1.69966302540739,
-1.69745730374043,-1.69389953409202,-1.66153650195464,-1.63686321154794,
-1.62657845779151,-1.62455645673067,-1.62343881571737,-1.62248269292914,
-1.62126376183288,-1.61931158864701,-1.60835262753931,-1.6034358978591,
-1.59290928585705,-1.56894388580332,-1.55745512800824,-1.55239565032577,
-1.54838798531646,-1.54630155539103,-1.54459818355804,-1.54262863849183,
-1.53926122404421,-1.53329438485854),.UNSPECIFIED.);
#3785=B_SPLINE_CURVE_WITH_KNOTS('',3,(#267798,#267799,#267800,#267801,#267802,
#267803,#267804,#267805,#267806,#267807,#267808,#267809,#267810,#267811,
#267812,#267813,#267814,#267815,#267816,#267817,#267818,#267819,#267820,
#267821,#267822,#267823,#267824,#267825,#267826,#267827,#267828,#267829,
#267830,#267831,#267832,#267833,#267834,#267835,#267836,#267837,#267838,
#267839,#267840,#267841,#267842,#267843,#267844,#267845,#267846,#267847,
#267848,#267849,#267850,#267851,#267852,#267853,#267854,#267855,#267856,
#267857,#267858,#267859,#267860,#267861,#267862,#267863,#267864,#267865,
#267866,#267867,#267868,#267869,#267870,#267871,#267872,#267873,#267874,
#267875,#267876),.UNSPECIFIED.,.F.,.F.,(4,3,3,3,3,3,3,3,3,3,3,3,3,3,3,3,
3,3,3,3,3,3,3,3,3,3,4),(113.494796146192,113.606250882577,113.717609971385,
113.828916304694,113.940212695218,114.051620250569,114.163087476167,114.274758952439,
114.340808136758,114.452505802227,114.564004864176,114.675393012991,114.786713181052,
114.898008203558,115.009403823241,115.120845465761,115.232504384916,115.338141987414,
115.450740226908,115.560871664889,115.670896225704,115.780858808389,115.895376082134,
116.005413941336,116.115510914744,116.225774396111,116.238927903367),
 .UNSPECIFIED.);
#3786=B_SPLINE_CURVE_WITH_KNOTS('',3,(#267877,#267878,#267879,#267880,#267881,
#267882,#267883,#267884),.UNSPECIFIED.,.F.,.F.,(4,1,1,1,1,4),(116.238928182822,
116.335475838071,117.332809688728,118.330143539385,119.327477390041,119.777686492919),
 .UNSPECIFIED.);
#3787=B_SPLINE_CURVE_WITH_KNOTS('',3,(#267889,#267890,#267891,#267892,#267893,
#267894,#267895,#267896,#267897,#267898,#267899,#267900,#267901,#267902,
#267903,#267904,#267905,#267906,#267907,#267908,#267909,#267910,#267911,
#267912,#267913,#267914,#267915,#267916,#267917,#267918,#267919,#267920,
#267921,#267922,#267923,#267924,#267925,#267926,#267927,#267928,#267929,
#267930,#267931,#267932,#267933,#267934,#267935,#267936,#267937,#267938,
#267939,#267940,#267941,#267942,#267943,#267944,#267945,#267946,#267947,
#267948,#267949,#267950,#267951,#267952,#267953,#267954,#267955,#267956,
#267957,#267958,#267959,#267960,#267961,#267962,#267963,#267964,#267965,
#267966,#267967,#267968,#267969,#267970,#267971,#267972,#267973,#267974,
#267975,#267976,#267977,#267978,#267979,#267980,#267981,#267982,#267983,
#267984,#267985,#267986,#267987,#267988,#267989,#267990,#267991,#267992,
#267993,#267994,#267995,#267996,#267997,#267998,#267999,#268000,#268001,
#268002,#268003,#268004,#268005,#268006,#268007,#268008,#268009,#268010,
#268011,#268012,#268013,#268014,#268015,#268016,#268017,#268018,#268019,
#268020,#268021,#268022,#268023,#268024,#268025,#268026,#268027,#268028,
#268029,#268030,#268031,#268032,#268033,#268034,#268035,#268036,#268037,
#268038,#268039,#268040,#268041,#268042,#268043,#268044,#268045,#268046,
#268047,#268048,#268049,#268050,#268051,#268052,#268053,#268054,#268055,
#268056,#268057,#268058,#268059,#268060,#268061,#268062,#268063,#268064,
#268065,#268066,#268067,#268068,#268069,#268070,#268071,#268072,#268073,
#268074,#268075,#268076,#268077,#268078,#268079,#268080,#268081,#268082,
#268083,#268084,#268085,#268086,#268087,#268088,#268089,#268090,#268091,
#268092,#268093,#268094,#268095,#268096,#268097,#268098,#268099,#268100,
#268101,#268102,#268103,#268104,#268105,#268106,#268107,#268108,#268109,
#268110,#268111,#268112,#268113,#268114),.UNSPECIFIED.,.F.,.F.,(4,2,2,2,
2,2,2,2,2,2,2,2,2,2,2,2,2,2,2,2,2,2,2,2,2,2,2,2,2,2,2,2,2,2,2,2,2,2,2,2,
2,2,2,2,2,2,2,2,2,2,2,2,2,2,2,2,2,2,2,2,2,2,2,2,2,2,2,2,2,2,2,2,2,2,2,2,
2,2,2,2,2,2,2,2,2,2,2,2,2,2,2,2,2,2,2,2,2,2,2,2,2,2,2,2,2,2,2,2,2,2,2,2,
4),(-1.53304027296573,-1.5316933786242,-1.53059862789435,-1.52963896918988,
-1.52840580818723,-1.52636222400816,-1.51338180602523,-1.47986731226285,
-1.46086274598092,-1.4560396602581,-1.45379252083902,-1.45207234176464,
-1.45043006830222,-1.44763433141302,-1.4398990132202,-1.43929879688,-1.43752180201361,
-1.39577611690525,-1.38402074778217,-1.37975715595556,-1.37670349300103,
-1.37538370234128,-1.37441502483976,-1.37335425565733,-1.37159146258138,
-1.36572016526932,-1.35896876808938,-1.31389858892671,-1.30229649506668,
-1.29917527390024,-1.29727934172938,-1.29556530642887,-1.29336488331976,
-1.28982552372144,-1.26586265434036,-1.23382676724874,-1.22254546405914,
-1.22047289424212,-1.21934420677549,-1.2183888911161,-1.21718403388192,
-1.21482279880908,-1.19804997227739,-1.15736136842732,-1.14650532861651,
-1.14345227090486,-1.14157139083122,-1.13985364898079,-1.13766088945787,
-1.13406760616426,-1.10560515707813,-1.07777913052247,-1.06686010611868,
-1.06480513336529,-1.06368025450795,-1.06272465843784,-1.06151497854141,
-1.05913097837272,-1.04042587742878,-1.01815170145439,-0.994699467949108,
-0.989325134502199,-0.98697833711723,-0.985242748269195,-0.983629619613522,
-0.980986566553452,-0.973708527986447,-0.962762024740855,-0.920722289454511,
-0.911250337706766,-0.909378708109777,-0.908184054914625,-0.907229207742768,
-0.906092047332384,-0.903980229380461,-0.891826343980013,-0.852888345556283,
-0.845385051251205,-0.84373823557601,-0.842233750249596,-0.834638357150912,
-0.831862859584372,-0.830224435130571,-0.828502454189615,-0.826243269710176,
-0.821356080551775,-0.801861767721198,-0.782102464277489,-0.777319312506229,
-0.756202074192142,-0.753765687659272,-0.752561444260335,-0.75160613589723,
-0.750476888193142,-0.748401832073659,-0.737067741766625,-0.704668370777625,
-0.681139457402112,-0.677611017844322,-0.675413792572174,-0.673700057731437,
-0.671802223105242,-0.668672701392535,-0.65697774269502,-0.611940116441193,
-0.600156065133991,-0.598161374450457,-0.596929436096105,-0.595971904814009,
-0.594862687580587,-0.592880586472537,-0.583312991155123,-0.552744682324884),
 .UNSPECIFIED.);
#3788=B_SPLINE_CURVE_WITH_KNOTS('',3,(#268116,#268117,#268118,#268119,#268120,
#268121,#268122),.UNSPECIFIED.,.F.,.F.,(4,1,1,1,4),(119.777686492919,120.324811240698,
121.322145091355,122.319478942012,122.522113490002),.UNSPECIFIED.);
#3789=B_SPLINE_CURVE_WITH_KNOTS('',3,(#268123,#268124,#268125,#268126,#268127,
#268128,#268129,#268130,#268131,#268132,#268133,#268134,#268135,#268136,
#268137,#268138,#268139,#268140,#268141,#268142,#268143,#268144,#268145,
#268146,#268147,#268148,#268149,#268150,#268151,#268152,#268153,#268154,
#268155,#268156,#268157,#268158,#268159,#268160,#268161,#268162,#268163,
#268164,#268165,#268166,#268167,#268168,#268169,#268170,#268171,#268172,
#268173,#268174,#268175,#268176,#268177,#268178,#268179,#268180,#268181,
#268182,#268183,#268184,#268185,#268186,#268187,#268188,#268189,#268190,
#268191,#268192,#268193,#268194,#268195,#268196,#268197,#268198,#268199,
#268200,#268201,#268202,#268203,#268204,#268205,#268206,#268207,#268208,
#268209,#268210,#268211,#268212,#268213,#268214,#268215,#268216,#268217,
#268218,#268219,#268220,#268221,#268222,#268223,#268224,#268225,#268226,
#268227,#268228,#268229,#268230,#268231,#268232,#268233,#268234,#268235,
#268236,#268237,#268238,#268239,#268240,#268241,#268242,#268243,#268244,
#268245,#268246,#268247,#268248),.UNSPECIFIED.,.F.,.F.,(4,2,2,2,2,2,2,2,
2,2,2,2,2,2,2,2,2,2,2,2,2,2,2,2,2,2,2,2,2,2,2,2,2,2,2,2,2,2,2,2,2,2,2,2,
2,2,2,2,2,2,2,2,2,2,2,2,2,2,2,2,2,2,4),(-1.96140461786641,-1.92769353217711,
-1.92242452363725,-1.91949550116251,-1.917516678651,-1.91559812502333,-1.91386225364756,
-1.91163161614589,-1.9080384760744,-1.87663664301394,-1.85851588646038,
-1.84675774764076,-1.84037984140565,-1.83865240462828,-1.83773363402596,
-1.83676658476978,-1.83555063814005,-1.83317786167412,-1.81673692710697,
-1.77627338487616,-1.76884859787116,-1.76347393746544,-1.76107717808805,
-1.75931644559865,-1.75768813906028,-1.75546764655194,-1.74988923849613,
-1.71577810669206,-1.69445703659498,-1.68828776594107,-1.68423648905864,
-1.68274880054525,-1.68173998293721,-1.68083651144448,-1.67937576947549,
-1.67578217545974,-1.64539413071381,-1.61124242736164,-1.6071523018085,
-1.60503317305514,-1.60347369342269,-1.60154119982685,-1.59832209192733,
-1.58730232424351,-1.54262385269019,-1.52993135105201,-1.52777882011535,
-1.52662452863726,-1.52565785508531,-1.52445069291963,-1.52256314522001,
-1.51307058074189,-1.50896831995664,-1.47827904743643,-1.45726463825833,
-1.45215909875675,-1.44984305905339,-1.44809529186693,-1.44644515352447,
-1.44368043706037,-1.43629505540247,-1.4348004361727,-1.40935215081212),
 .UNSPECIFIED.);
#3790=B_SPLINE_CURVE_WITH_KNOTS('',3,(#268254,#268255,#268256,#268257,#268258,
#268259,#268260,#268261,#268262,#268263,#268264,#268265,#268266,#268267,
#268268,#268269,#268270,#268271,#268272,#268273,#268274,#268275,#268276,
#268277,#268278,#268279,#268280,#268281,#268282,#268283,#268284,#268285,
#268286,#268287,#268288,#268289,#268290,#268291,#268292,#268293,#268294,
#268295,#268296,#268297,#268298,#268299,#268300,#268301,#268302,#268303,
#268304,#268305,#268306,#268307,#268308,#268309,#268310,#268311,#268312,
#268313,#268314,#268315,#268316,#268317,#268318,#268319,#268320,#268321,
#268322,#268323,#268324,#268325,#268326,#268327,#268328,#268329,#268330,
#268331,#268332,#268333,#268334,#268335,#268336,#268337,#268338,#268339,
#268340,#268341,#268342,#268343,#268344,#268345,#268346,#268347,#268348,
#268349,#268350,#268351,#268352,#268353,#268354,#268355,#268356,#268357,
#268358,#268359,#268360,#268361,#268362,#268363,#268364,#268365,#268366,
#268367,#268368,#268369,#268370,#268371,#268372,#268373,#268374,#268375,
#268376,#268377),.UNSPECIFIED.,.F.,.F.,(4,2,2,2,2,2,2,2,2,2,2,2,2,2,2,2,
2,2,2,2,2,2,2,2,2,2,2,2,2,2,2,2,2,2,2,2,2,2,2,2,2,2,2,2,2,2,2,2,2,2,2,2,
2,2,2,2,2,2,2,2,2,4),(-0.552568402974919,-0.533818180356304,-0.507622669869086,
-0.505256919662991,-0.504050916278603,-0.503095299981104,-0.501966963901806,
-0.499896873499081,-0.488674999504696,-0.457037227726781,-0.432649183897734,
-0.429099133080411,-0.426895166903973,-0.42518028300109,-0.423285354599918,
-0.420170265507477,-0.408644754825207,-0.363483860427586,-0.351614781241579,
-0.349615994897949,-0.348382683517896,-0.347424831720345,-0.346316097278136,
-0.344336925297352,-0.334824288074235,-0.29096552735152,-0.276152377318475,
-0.272677516954602,-0.270682853061345,-0.268996311892583,-0.266945205998973,
-0.263250925411805,-0.258592090828962,-0.248384144912683,-0.210959912866051,
-0.207521692546721,-0.195863125043467,-0.193875294090291,-0.192645289816032,
-0.191687768998619,-0.190576851902533,-0.188703989824544,-0.180177952027278,
-0.135783508398606,-0.120482117208579,-0.116973378157439,-0.114971053133357,
-0.113438763106351,-0.111458585460992,-0.109382951858319,-0.101398647248031,
-0.0834201594127288,-0.0671972741633204,-0.0424792406047148,-0.0387704868789293,
-0.0373003746695206,-0.0364027637722067,-0.0354120835546178,-0.0344121372081074,
-0.0330206229605259,-0.030668307090341,-0.00046003148883276),
 .UNSPECIFIED.);
#3791=B_SPLINE_CURVE_WITH_KNOTS('',3,(#268378,#268379,#268380,#268381,#268382,
#268383,#268384,#268385,#268386,#268387,#268388,#268389,#268390,#268391,
#268392,#268393,#268394,#268395,#268396,#268397,#268398,#268399,#268400,
#268401,#268402,#268403,#268404,#268405,#268406,#268407,#268408,#268409,
#268410,#268411,#268412,#268413,#268414,#268415,#268416,#268417,#268418,
#268419,#268420,#268421,#268422,#268423,#268424,#268425,#268426,#268427,
#268428,#268429,#268430,#268431,#268432,#268433,#268434,#268435,#268436,
#268437,#268438,#268439,#268440,#268441,#268442,#268443,#268444,#268445,
#268446,#268447,#268448,#268449,#268450,#268451,#268452,#268453,#268454,
#268455,#268456,#268457,#268458,#268459,#268460,#268461,#268462,#268463,
#268464,#268465,#268466,#268467,#268468,#268469,#268470,#268471,#268472,
#268473),.UNSPECIFIED.,.F.,.F.,(4,2,2,2,2,2,2,2,2,2,2,2,2,2,2,2,2,2,2,2,
2,2,2,2,2,2,2,2,2,2,2,2,2,2,2,2,2,2,2,2,2,2,2,2,2,2,2,4),(-1.96142034783854,
-1.92657433847609,-1.9237305089718,-1.92179629247507,-1.91991542049242,
-1.91819781746739,-1.91600541523768,-1.91241310186858,-1.88400082421549,
-1.86688259523144,-1.84849765698183,-1.84425682866014,-1.84308977961811,
-1.84198620836535,-1.84102817572916,-1.83978856185613,-1.83776763320117,
-1.82536289064326,-1.81967137528589,-1.78720718752015,-1.77590103164971,
-1.77089756026477,-1.76698950040469,-1.76529091825504,-1.76356041014398,
-1.76193964650569,-1.75969748433022,-1.75389165525563,-1.71044307049571,
-1.69634448260789,-1.69154745589561,-1.68822697878564,-1.68686525333391,
-1.68588458545841,-1.68497638807889,-1.68344997396578,-1.67938196851299,
-1.63148736639158,-1.61437281373885,-1.61087093117825,-1.60889169858573,
-1.60736004230269,-1.60535841479486,-1.60185054790136,-1.58654807324172,
-1.54214427265775,-1.53360989706048,-1.53304027296573),.UNSPECIFIED.);
#3792=B_SPLINE_CURVE_WITH_KNOTS('',3,(#268474,#268475,#268476,#268477,#268478,
#268479,#268480,#268481,#268482,#268483,#268484,#268485,#268486,#268487,
#268488,#268489,#268490,#268491,#268492,#268493,#268494,#268495,#268496,
#268497,#268498,#268499,#268500,#268501,#268502,#268503,#268504,#268505,
#268506,#268507,#268508,#268509,#268510,#268511,#268512,#268513,#268514,
#268515,#268516,#268517,#268518,#268519,#268520,#268521,#268522,#268523,
#268524,#268525,#268526,#268527,#268528,#268529,#268530,#268531,#268532,
#268533,#268534,#268535,#268536,#268537,#268538,#268539,#268540,#268541,
#268542,#268543,#268544,#268545,#268546,#268547,#268548,#268549,#268550,
#268551,#268552,#268553,#268554,#268555,#268556,#268557,#268558,#268559,
#268560,#268561,#268562,#268563,#268564,#268565,#268566,#268567,#268568,
#268569,#268570,#268571,#268572,#268573,#268574,#268575,#268576,#268577,
#268578,#268579,#268580,#268581,#268582,#268583,#268584,#268585,#268586,
#268587,#268588,#268589,#268590,#268591,#268592,#268593,#268594,#268595,
#268596,#268597,#268598,#268599,#268600,#268601,#268602,#268603,#268604,
#268605,#268606,#268607,#268608,#268609,#268610,#268611,#268612,#268613,
#268614,#268615,#268616,#268617,#268618,#268619,#268620,#268621,#268622,
#268623,#268624,#268625,#268626,#268627,#268628,#268629,#268630,#268631,
#268632,#268633,#268634,#268635,#268636,#268637,#268638,#268639,#268640,
#268641,#268642,#268643,#268644,#268645,#268646,#268647,#268648,#268649,
#268650,#268651,#268652,#268653,#268654,#268655,#268656,#268657,#268658,
#268659,#268660,#268661,#268662,#268663,#268664,#268665,#268666,#268667,
#268668,#268669,#268670,#268671,#268672,#268673,#268674,#268675,#268676,
#268677,#268678,#268679,#268680,#268681,#268682,#268683,#268684,#268685,
#268686,#268687,#268688,#268689,#268690,#268691),.UNSPECIFIED.,.F.,.F.,
(4,2,2,2,2,2,2,2,2,2,2,2,2,2,2,2,2,2,2,2,2,2,2,2,2,2,2,2,2,2,2,2,2,2,2,
2,2,2,2,2,2,2,2,2,2,2,2,2,2,2,2,2,2,2,2,2,2,2,2,2,2,2,2,2,2,2,2,2,2,2,2,
2,2,2,2,2,2,2,2,2,2,2,2,2,2,2,2,2,2,2,2,2,2,2,2,2,2,2,2,2,2,2,2,2,2,2,2,
2,4),(-1.40935215081212,-1.38414989925974,-1.37410809746072,-1.37208173083532,
-1.37095442059732,-1.36998520113837,-1.36874238321402,-1.36673767131879,
-1.35504115585052,-1.30978221365538,-1.30220290135856,-1.29668258589555,
-1.29429284107092,-1.29253297750705,-1.29090244741502,-1.28867423216686,
-1.2830519423058,-1.25055533505058,-1.22799182673477,-1.21845016586842,
-1.21645292499742,-1.21533200443641,-1.21436201195971,-1.21311002446733,
-1.21107455580077,-1.19872273665609,-1.1862735220927,-1.17208011983953,
-1.14416073401425,-1.14025428303527,-1.13817291554743,-1.1364651738715,
-1.13444954872091,-1.13094787793857,-1.11613256457903,-1.07194199297956,
-1.06585673302858,-1.06184620912954,-1.06036399985209,-1.05935602466236,
-1.05845112754953,-1.05698401103913,-1.05335441378921,-1.02373542580131,
-0.989695697719933,-0.985066449059518,-0.982839296809448,-0.981103346970758,
-0.979181863440628,-0.976015018520641,-0.964183039325222,-0.919126716211047,
-0.907596283741008,-0.905599736084144,-0.904359254730039,-0.903390068986468,
-0.902260726139816,-0.900225619746422,-0.890030890920978,-0.83573685320341,
-0.830028623694332,-0.82778586894948,-0.826151543804733,-0.824394053757696,
-0.822018979273781,-0.816583799664372,-0.792825521239947,-0.76475642353124,
-0.752022149523379,-0.749970973510691,-0.748714266748787,-0.747743766598975,
-0.746625831644567,-0.744642456688066,-0.735329257281941,-0.713750728228456,
-0.680001111787145,-0.674410135254135,-0.672187147202926,-0.670557879620062,
-0.668796936710608,-0.666401381299168,-0.6608479123896,-0.653208970243973,
-0.607982229638827,-0.596320609503819,-0.594317654331137,-0.593075303875223,
-0.592106037241798,-0.590978188895139,-0.588949684600726,-0.578871601881753,
-0.527412785990045,-0.527114457262083,-0.519473040575407,-0.516670366071667,
-0.515012767033611,-0.513268192970907,-0.510975039364734,-0.505995471067384,
-0.485975035601746,-0.457584989845919,-0.440982529391697,-0.438604143742915,
-0.437386840864667,-0.436419517083748,-0.435273247420906,-0.433158809815512,
-0.428879403561289),.UNSPECIFIED.);
#3793=B_SPLINE_CURVE_WITH_KNOTS('',3,(#268696,#268697,#268698,#268699,#268700,
#268701,#268702,#268703,#268704,#268705,#268706,#268707,#268708,#268709,
#268710,#268711,#268712,#268713,#268714,#268715,#268716,#268717,#268718,
#268719,#268720,#268721,#268722,#268723,#268724,#268725,#268726,#268727,
#268728,#268729,#268730,#268731,#268732,#268733,#268734,#268735,#268736,
#268737,#268738,#268739,#268740,#268741,#268742,#268743,#268744,#268745,
#268746,#268747,#268748,#268749,#268750,#268751,#268752,#268753,#268754,
#268755,#268756,#268757,#268758,#268759,#268760,#268761,#268762,#268763,
#268764,#268765,#268766,#268767,#268768,#268769,#268770,#268771,#268772,
#268773,#268774,#268775,#268776,#268777,#268778,#268779,#268780,#268781,
#268782,#268783,#268784,#268785,#268786,#268787,#268788,#268789,#268790,
#268791,#268792,#268793,#268794,#268795,#268796,#268797,#268798,#268799,
#268800,#268801,#268802,#268803,#268804,#268805,#268806,#268807,#268808,
#268809,#268810,#268811,#268812,#268813,#268814,#268815,#268816,#268817,
#268818,#268819,#268820,#268821,#268822,#268823,#268824,#268825,#268826,
#268827,#268828,#268829,#268830,#268831,#268832,#268833,#268834,#268835,
#268836,#268837,#268838,#268839,#268840,#268841,#268842,#268843,#268844,
#268845,#268846,#268847,#268848,#268849,#268850,#268851,#268852,#268853,
#268854,#268855,#268856,#268857,#268858,#268859,#268860,#268861,#268862,
#268863,#268864,#268865,#268866,#268867,#268868,#268869,#268870,#268871,
#268872,#268873,#268874,#268875,#268876,#268877,#268878,#268879,#268880,
#268881,#268882,#268883,#268884,#268885,#268886,#268887,#268888,#268889,
#268890,#268891,#268892,#268893,#268894,#268895,#268896,#268897,#268898,
#268899,#268900,#268901,#268902,#268903,#268904,#268905,#268906,#268907,
#268908,#268909,#268910,#268911,#268912,#268913,#268914,#268915,#268916,
#268917,#268918,#268919,#268920,#268921),.UNSPECIFIED.,.F.,.F.,(4,2,2,2,
2,2,2,2,2,2,2,2,2,2,2,2,2,2,2,2,2,2,2,2,2,2,2,2,2,2,2,2,2,2,2,2,2,2,2,2,
2,2,2,2,2,2,2,2,2,2,2,2,2,2,2,2,2,2,2,2,2,2,2,2,2,2,2,2,2,2,2,2,2,2,2,2,
2,2,2,2,2,2,2,2,2,2,2,2,2,2,2,2,2,2,2,2,2,2,2,2,2,2,2,2,2,2,2,2,2,2,2,2,
4),(-1.5331279783234,-1.53271589118596,-1.52111789403578,-1.51799642383371,
-1.51610008588491,-1.5143855196618,-1.51218418609851,-1.50864289377132,
-1.48463609144734,-1.4526241978639,-1.4413445932304,-1.4392716571504,-1.43814269253739,
-1.43718709552344,-1.43598182401986,-1.43361960144915,-1.4168300184983,
-1.37610702308954,-1.3652772091061,-1.3622260505927,-1.36034523842165,-1.35862683020804,
-1.35643222131933,-1.35283377350258,-1.32413965328508,-1.29649732795497,
-1.28561115841552,-1.28355737840486,-1.28243255879028,-1.28147665156574,
-1.28026611635389,-1.27834265326804,-1.26795482906466,-1.26203793115821,
-1.23701082985724,-1.21102973580487,-1.20719744698848,-1.20514704176437,
-1.20346056805247,-1.20146538606876,-1.19798810386291,-1.18314082087345,
-1.13923198649287,-1.12976885972014,-1.12779256423819,-1.1266844423764,
-1.12572647579001,-1.12449218766785,-1.12249021402569,-1.11054768388819,
-1.06529352412716,-1.05393821388452,-1.05083825192968,-1.04894658215367,
-1.04723078932416,-1.04502024245374,-1.04144841172715,-1.01586287342043,
-0.994672189925102,-0.980853099889869,-0.97975604224162,-0.973696314806764,
-0.971912352629215,-0.970846704259775,-0.96987933225583,-0.968569345428101,
-0.965572581068912,-0.961412307370486,-0.950087128778832,-0.908778383745338,
-0.89831637088435,-0.895178792901896,-0.893278881702288,-0.891565072327742,
-0.889370252256426,-0.884823897038116,-0.878892175463459,-0.864405935058884,
-0.837580781683793,-0.819089142892016,-0.816707007870551,-0.815497514928769,
-0.814541671486112,-0.813416033055249,-0.811358490163329,-0.800395497002437,
-0.784650502322319,-0.746375266762727,-0.74105246047064,-0.738890412685334,
-0.737289687068503,-0.735544144605578,-0.733141806451617,-0.72744483594904,
-0.719525662951737,-0.674666678946049,-0.663024487505438,-0.661037680365348,
-0.659807978217846,-0.658850477478963,-0.657739336871963,-0.655749034626371,
-0.64604611982115,-0.600854674791085,-0.587399705166519,-0.584023784346807,
-0.582051782342297,-0.580347805026822,-0.578262552611402,-0.574263167384463,
-0.569216919330978,-0.55777248985308,-0.552568402974919),.UNSPECIFIED.);
#3794=B_SPLINE_CURVE_WITH_KNOTS('',3,(#268923,#268924,#268925,#268926,#268927,
#268928,#268929,#268930,#268931,#268932,#268933,#268934,#268935,#268936,
#268937,#268938,#268939,#268940,#268941,#268942,#268943,#268944,#268945,
#268946,#268947,#268948,#268949,#268950,#268951,#268952,#268953,#268954,
#268955,#268956,#268957,#268958,#268959,#268960,#268961,#268962,#268963,
#268964,#268965,#268966,#268967,#268968,#268969,#268970,#268971,#268972,
#268973,#268974,#268975,#268976,#268977,#268978,#268979,#268980,#268981,
#268982,#268983,#268984,#268985,#268986,#268987,#268988,#268989,#268990,
#268991,#268992,#268993,#268994,#268995,#268996,#268997,#268998,#268999,
#269000,#269001,#269002,#269003,#269004,#269005,#269006,#269007,#269008,
#269009,#269010,#269011,#269012,#269013,#269014),.UNSPECIFIED.,.F.,.F.,
(4,2,2,2,2,2,2,2,2,2,2,2,2,2,2,2,2,2,2,2,2,2,2,2,2,2,2,2,2,2,2,2,2,2,2,
2,2,2,2,2,2,2,2,2,2,4),(-0.428879403561289,-0.421364094033311,-0.385754873086396,
-0.365849832369992,-0.362402067404484,-0.360215007910518,-0.358483751897869,
-0.356539753005891,-0.353269870485476,-0.340180064009024,-0.287963614543592,
-0.283781542226331,-0.282226414648722,-0.281304742182555,-0.280312317570708,
-0.278909715129471,-0.27542277601127,-0.257804230793803,-0.227003868244697,
-0.221662202366041,-0.209333654053757,-0.205986862866056,-0.204025617038048,
-0.202469295745647,-0.200388436593215,-0.196648026409956,-0.17964520351943,
-0.142694772135559,-0.137779546365032,-0.129105222595565,-0.127092701594866,
-0.125956086034931,-0.124987614167213,-0.124046481782052,-0.12213353534955,
-0.112926261379201,-0.0917552362925678,-0.0574438196528032,-0.0518705422515606,
-0.0496501698847528,-0.0480212753648273,-0.0462592613616052,-0.04385961296452,
-0.041205972415941,-0.0325220769531143,-0.000459406881434288),
 .UNSPECIFIED.);
#3795=B_SPLINE_CURVE_WITH_KNOTS('',3,(#269015,#269016,#269017,#269018,#269019,
#269020,#269021,#269022,#269023,#269024,#269025,#269026,#269027,#269028,
#269029,#269030,#269031,#269032,#269033,#269034,#269035,#269036,#269037,
#269038,#269039,#269040,#269041,#269042,#269043,#269044,#269045,#269046,
#269047,#269048,#269049,#269050,#269051,#269052,#269053,#269054,#269055,
#269056,#269057,#269058,#269059,#269060,#269061,#269062,#269063,#269064,
#269065,#269066,#269067,#269068,#269069,#269070,#269071,#269072,#269073,
#269074,#269075,#269076,#269077,#269078,#269079,#269080,#269081,#269082,
#269083,#269084,#269085,#269086,#269087,#269088,#269089,#269090,#269091,
#269092,#269093,#269094,#269095,#269096,#269097,#269098,#269099,#269100,
#269101,#269102,#269103,#269104,#269105,#269106,#269107,#269108,#269109,
#269110,#269111,#269112,#269113,#269114,#269115,#269116,#269117,#269118,
#269119,#269120,#269121,#269122,#269123,#269124,#269125,#269126,#269127,
#269128,#269129,#269130,#269131,#269132,#269133,#269134,#269135,#269136,
#269137,#269138,#269139,#269140,#269141,#269142),.UNSPECIFIED.,.F.,.F.,
(4,2,2,2,2,2,2,2,2,2,2,2,2,2,2,2,2,2,2,2,2,2,2,2,2,2,2,2,2,2,2,2,2,2,2,
2,2,2,2,2,2,2,2,2,2,2,2,2,2,2,2,2,2,2,2,2,2,2,2,2,2,2,2,4),(-1.9614931804776,
-1.93516794709654,-1.9334587770767,-1.93232534427062,-1.93140663883529,
-1.93043943041673,-1.92922244376262,-1.92676676370697,-1.90399138611458,
-1.88670608386381,-1.86428115288063,-1.85767263726173,-1.85568900239295,
-1.85376702989839,-1.8520316262414,-1.84980654990319,-1.8462325078789,-1.82200846571697,
-1.79316961507947,-1.7837971646141,-1.7783323738917,-1.77670826805569,-1.77579658994973,
-1.77482541841812,-1.77358224975683,-1.77153142055365,-1.7587991666777,
-1.72843832271109,-1.71244643307727,-1.7060917776087,-1.7013937542631,-1.69909085977923,
-1.69734491765831,-1.69569050353671,-1.6929041329534,-1.68537242144985,
-1.63346867767306,-1.62336752496367,-1.62133765813044,-1.62020950333927,
-1.61924025141759,-1.61799828986165,-1.61599668986076,-1.60436072238026,
-1.55918294844772,-1.54758193223459,-1.54443553308857,-1.54251859416192,
-1.54078166379389,-1.53854613542431,-1.53493785602654,-1.5084345314858,
-1.50559570587053,-1.47859588600493,-1.46781188556754,-1.46574570280693,
-1.46460974021478,-1.46364143356187,-1.46241050357844,-1.4604453324152,
-1.44955107374389,-1.44669929990243,-1.41634025137202,-1.40961854510899),
 .UNSPECIFIED.);
#3796=B_SPLINE_CURVE_WITH_KNOTS('',3,(#269148,#269149,#269150,#269151,#269152,
#269153,#269154,#269155,#269156,#269157,#269158,#269159,#269160,#269161,
#269162,#269163,#269164,#269165,#269166,#269167,#269168,#269169,#269170,
#269171,#269172,#269173,#269174,#269175,#269176,#269177,#269178,#269179,
#269180,#269181,#269182,#269183,#269184,#269185,#269186,#269187,#269188,
#269189,#269190,#269191,#269192,#269193,#269194,#269195,#269196,#269197,
#269198,#269199,#269200,#269201,#269202,#269203,#269204,#269205,#269206,
#269207,#269208,#269209,#269210,#269211,#269212,#269213,#269214,#269215,
#269216,#269217,#269218,#269219,#269220,#269221,#269222,#269223,#269224,
#269225,#269226,#269227,#269228,#269229,#269230,#269231,#269232,#269233,
#269234,#269235,#269236,#269237,#269238,#269239,#269240,#269241,#269242,
#269243,#269244,#269245,#269246,#269247,#269248,#269249,#269250,#269251,
#269252,#269253,#269254,#269255,#269256,#269257,#269258,#269259,#269260,
#269261,#269262,#269263,#269264,#269265,#269266,#269267,#269268,#269269,
#269270,#269271),.UNSPECIFIED.,.F.,.F.,(4,2,2,2,2,2,2,2,2,2,2,2,2,2,2,2,
2,2,2,2,2,2,2,2,2,2,2,2,2,2,2,2,2,2,2,2,2,2,2,2,2,2,2,2,2,2,2,2,2,2,2,2,
2,2,2,2,2,2,2,2,2,4),(-0.5528747849223,-0.505972514084536,-0.494698071882762,
-0.491476707206178,-0.489558558314461,-0.488019671249651,-0.485940536591137,
-0.481969629183095,-0.476968241094244,-0.465668887209196,-0.417969358499917,
-0.413713084292922,-0.412157879710706,-0.411243867733457,-0.410266881391685,
-0.408898695399195,-0.40556044419842,-0.389258079754503,-0.361022161447314,
-0.340088374844942,-0.336630908837478,-0.334454738744394,-0.332743021372802,
-0.330832530186886,-0.327647121824573,-0.315298960178662,-0.270647749782887,
-0.259186239951686,-0.257208703812095,-0.255981740869574,-0.255024418865194,
-0.253911238535114,-0.251911783486144,-0.242051121162004,-0.194444720042155,
-0.183195873274035,-0.17997659029724,-0.178058631302659,-0.176384903087572,
-0.174282719399547,-0.170146328789071,-0.164829598806549,-0.152489423670334,
-0.120160489571626,-0.103752845699109,-0.10139992704657,-0.100196618860188,
-0.0992411101530231,-0.098110518539815,-0.09603012426652,-0.0845913795460045,
-0.0462731008833756,-0.0351023996990404,-0.0343319119317644,-0.0266469561360505,
-0.0238580113325214,-0.022216730159335,-0.0205673550014028,-0.0188994884150446,
-0.0167475610645804,-0.0109046728631205,-0.000459621179054175),
 .UNSPECIFIED.);
#3797=B_SPLINE_CURVE_WITH_KNOTS('',3,(#269272,#269273,#269274,#269275,#269276,
#269277,#269278,#269279,#269280,#269281,#269282,#269283,#269284,#269285,
#269286,#269287,#269288,#269289,#269290,#269291,#269292,#269293,#269294,
#269295,#269296,#269297,#269298,#269299,#269300,#269301,#269302,#269303,
#269304,#269305,#269306,#269307,#269308,#269309,#269310,#269311,#269312,
#269313,#269314,#269315,#269316,#269317,#269318,#269319,#269320,#269321,
#269322,#269323,#269324,#269325,#269326,#269327,#269328,#269329,#269330,
#269331,#269332,#269333,#269334,#269335,#269336,#269337,#269338,#269339,
#269340,#269341,#269342,#269343,#269344,#269345,#269346,#269347,#269348,
#269349,#269350,#269351,#269352,#269353,#269354,#269355,#269356,#269357,
#269358,#269359,#269360,#269361,#269362,#269363,#269364,#269365,#269366,
#269367,#269368,#269369),.UNSPECIFIED.,.F.,.F.,(4,2,2,2,2,2,2,2,2,2,2,2,
2,2,2,2,2,2,2,2,2,2,2,2,2,2,2,2,2,2,2,2,2,2,2,2,2,2,2,2,2,2,2,2,2,2,2,2,
4),(-1.96147649178031,-1.95505603054594,-1.91261356055287,-1.90927872759127,
-1.90675660111791,-1.9055352170814,-1.90457852385727,-1.90346177263504,
-1.90149921167885,-1.89328266276818,-1.88788401525447,-1.88312367071695,
-1.85178988632294,-1.83967312297814,-1.83442284339744,-1.83033637858477,
-1.82823993528566,-1.82656396391706,-1.82464162969244,-1.82140212171954,
-1.80994719655176,-1.7625454514864,-1.75269521114947,-1.75069632097682,
-1.74958327379444,-1.74862594653794,-1.74739883157897,-1.74484810183656,
-1.74218249656584,-1.69465504147881,-1.67755850821457,-1.67405638270499,
-1.67207652639146,-1.67054416048773,-1.66854128168764,-1.66503038967535,
-1.64970198077823,-1.61293671029031,-1.60234662102942,-1.59836861182143,
-1.59547424316152,-1.5941825577858,-1.59321783559815,-1.59214326763231,
-1.59031923805818,-1.58388204478182,-1.58258691369429,-1.57780407359389,
-1.5331279783234),.UNSPECIFIED.);
#3798=B_SPLINE_CURVE_WITH_KNOTS('',3,(#269370,#269371,#269372,#269373,#269374,
#269375,#269376,#269377,#269378,#269379,#269380,#269381,#269382,#269383,
#269384,#269385,#269386,#269387,#269388,#269389,#269390,#269391,#269392,
#269393,#269394,#269395,#269396,#269397,#269398,#269399,#269400,#269401,
#269402,#269403,#269404,#269405,#269406,#269407,#269408,#269409,#269410,
#269411,#269412,#269413,#269414,#269415,#269416,#269417,#269418,#269419,
#269420,#269421,#269422,#269423,#269424,#269425,#269426,#269427,#269428,
#269429,#269430,#269431,#269432,#269433,#269434,#269435,#269436,#269437,
#269438,#269439,#269440,#269441,#269442,#269443,#269444,#269445,#269446,
#269447,#269448,#269449,#269450,#269451,#269452,#269453,#269454,#269455,
#269456,#269457,#269458,#269459,#269460,#269461,#269462,#269463,#269464,
#269465,#269466,#269467,#269468,#269469,#269470,#269471,#269472,#269473,
#269474,#269475,#269476,#269477,#269478,#269479,#269480,#269481,#269482,
#269483,#269484,#269485,#269486,#269487,#269488,#269489,#269490,#269491,
#269492,#269493,#269494,#269495,#269496,#269497,#269498,#269499,#269500,
#269501,#269502,#269503,#269504,#269505,#269506,#269507,#269508,#269509,
#269510,#269511,#269512,#269513,#269514,#269515,#269516,#269517,#269518,
#269519,#269520,#269521,#269522,#269523,#269524,#269525,#269526,#269527,
#269528,#269529,#269530,#269531,#269532,#269533,#269534,#269535,#269536,
#269537,#269538,#269539,#269540,#269541,#269542,#269543,#269544,#269545,
#269546,#269547,#269548,#269549,#269550,#269551,#269552,#269553,#269554,
#269555,#269556,#269557,#269558,#269559,#269560,#269561,#269562,#269563,
#269564,#269565,#269566,#269567,#269568,#269569,#269570,#269571,#269572,
#269573,#269574,#269575,#269576,#269577,#269578,#269579,#269580,#269581,
#269582,#269583,#269584,#269585,#269586,#269587,#269588,#269589,#269590,
#269591),.UNSPECIFIED.,.F.,.F.,(4,2,2,2,2,2,2,2,2,2,2,2,2,2,2,2,2,2,2,2,
2,2,2,2,2,2,2,2,2,2,2,2,2,2,2,2,2,2,2,2,2,2,2,2,2,2,2,2,2,2,2,2,2,2,2,2,
2,2,2,2,2,2,2,2,2,2,2,2,2,2,2,2,2,2,2,2,2,2,2,2,2,2,2,2,2,2,2,2,2,2,2,2,
2,2,2,2,2,2,2,2,2,2,2,2,2,2,2,2,2,2,4),(-1.40961854510899,-1.39528294752712,
-1.39017139497674,-1.3878538939912,-1.38610553445163,-1.38445521258963,
-1.38169108938066,-1.374313591404,-1.37295651014169,-1.32214863493301,-1.31209716250216,
-1.31006986263412,-1.30894216626392,-1.30797269862926,-1.30672967104351,
-1.30472483042209,-1.29303224721824,-1.26444189492711,-1.24017879626115,
-1.23468458906443,-1.23229883308597,-1.23053914845212,-1.22890682937387,
-1.22667313122772,-1.22102121091431,-1.19040756074199,-1.17640423192621,
-1.15873667530518,-1.155244998724,-1.15384156224724,-1.15284892398987,-1.15192735161789,
-1.15063188715384,-1.14717953470537,-1.11430535747474,-1.08246888652409,
-1.07833775426367,-1.07620946237199,-1.07448271019517,-1.07249790158377,
-1.06913227728624,-1.05616688612967,-1.01054138771595,-1.0007907099465,
-0.998780450192614,-0.997656378600019,-0.996686310446103,-0.995437677224671,
-0.993414402107754,-0.981361496558986,-0.941866242160225,-0.934664375897499,
-0.932978414167962,-0.931644281371084,-0.924265768022248,-0.921501009307394,
-0.919850234863414,-0.918101333597226,-0.915783018571538,-0.910669295189133,
-0.889597698923813,-0.859066066059149,-0.855768714567986,-0.84539736677841,
-0.843458940229042,-0.842235915740885,-0.841267869940053,-0.84012522837066,
-0.838029067607473,-0.826644468316749,-0.79408798834002,-0.770853310184806,
-0.767303165456966,-0.765084692062664,-0.763349350066088,-0.761422228776398,
-0.758231393722498,-0.746127709496577,-0.701223263575436,-0.689826177359938,
-0.687835622731793,-0.686596762660636,-0.68562746357042,-0.684496394167292,
-0.682454230180951,-0.672138050511524,-0.6474338252567,-0.61522673578255,
-0.611648149251927,-0.609420998816315,-0.607684454608237,-0.605761705458147,
-0.602591367110766,-0.590729192897329,-0.545670540509494,-0.534148129184848,
-0.532151385112578,-0.53091058553053,-0.529941022658586,-0.528811092112484,
-0.526774560735353,-0.516564783518236,-0.461941779148298,-0.456441813864775,
-0.454237171363959,-0.452612087598778,-0.450846762892103,-0.448429210024572,
-0.442750413105181,-0.434888605918536,-0.428888253392887),.UNSPECIFIED.);
#3799=B_SPLINE_CURVE_WITH_KNOTS('',3,(#269596,#269597,#269598,#269599,#269600,
#269601,#269602,#269603,#269604,#269605,#269606,#269607,#269608,#269609,
#269610,#269611,#269612,#269613,#269614,#269615,#269616,#269617,#269618,
#269619,#269620,#269621,#269622,#269623,#269624,#269625,#269626,#269627,
#269628,#269629,#269630,#269631,#269632,#269633,#269634,#269635,#269636,
#269637,#269638,#269639,#269640,#269641,#269642,#269643,#269644,#269645,
#269646,#269647,#269648,#269649,#269650,#269651,#269652,#269653,#269654,
#269655,#269656,#269657,#269658,#269659,#269660,#269661,#269662,#269663,
#269664,#269665,#269666,#269667,#269668,#269669,#269670,#269671,#269672,
#269673,#269674,#269675,#269676,#269677,#269678,#269679,#269680,#269681,
#269682,#269683,#269684,#269685,#269686,#269687,#269688,#269689,#269690,
#269691,#269692,#269693,#269694,#269695,#269696,#269697,#269698,#269699,
#269700,#269701,#269702,#269703,#269704,#269705,#269706,#269707,#269708,
#269709,#269710,#269711,#269712,#269713,#269714,#269715,#269716,#269717,
#269718,#269719,#269720,#269721,#269722,#269723,#269724,#269725,#269726,
#269727,#269728,#269729,#269730,#269731,#269732,#269733,#269734,#269735,
#269736,#269737,#269738,#269739,#269740,#269741,#269742,#269743,#269744,
#269745,#269746,#269747,#269748,#269749,#269750,#269751,#269752,#269753,
#269754,#269755,#269756,#269757,#269758,#269759,#269760,#269761,#269762,
#269763,#269764,#269765,#269766,#269767,#269768,#269769,#269770,#269771,
#269772,#269773,#269774,#269775,#269776,#269777,#269778,#269779,#269780,
#269781,#269782,#269783,#269784,#269785,#269786,#269787,#269788,#269789,
#269790,#269791,#269792,#269793,#269794,#269795,#269796,#269797,#269798,
#269799,#269800,#269801,#269802,#269803,#269804,#269805,#269806,#269807,
#269808,#269809,#269810,#269811,#269812,#269813,#269814,#269815,#269816,
#269817),.UNSPECIFIED.,.F.,.F.,(4,2,2,2,2,2,2,2,2,2,2,2,2,2,2,2,2,2,2,2,
2,2,2,2,2,2,2,2,2,2,2,2,2,2,2,2,2,2,2,2,2,2,2,2,2,2,2,2,2,2,2,2,2,2,2,2,
2,2,2,2,2,2,2,2,2,2,2,2,2,2,2,2,2,2,2,2,2,2,2,2,2,2,2,2,2,2,2,2,2,2,2,2,
2,2,2,2,2,2,2,2,2,2,2,2,2,2,2,2,2,2,4),(-1.53326539915105,-1.51441118805452,
-1.50442152866779,-1.50241556872611,-1.50130135391595,-1.50034476052139,
-1.49912083376292,-1.49715224642753,-1.48593582258234,-1.48151042352721,
-1.47103627180541,-1.44697698015568,-1.42943032460901,-1.42590555000756,
-1.42392127980359,-1.42238939199795,-1.42039267377729,-1.41690672944437,
-1.40192052397052,-1.35788981919104,-1.34870013988331,-1.34674101181716,
-1.34563688203472,-1.34467873715503,-1.34343946629258,-1.34142006050601,
-1.3290587111249,-1.32336292323251,-1.30212865474607,-1.27436578335335,
-1.27049585840478,-1.26843779703937,-1.26675136364444,-1.264763649211,-1.26131806003861,
-1.24691984310531,-1.2027061993289,-1.19307288707911,-1.19108680234397,
-1.18997668091952,-1.18901920530666,-1.18778843656621,-1.18579778813956,
-1.17410060856547,-1.12918928949458,-1.11732745774197,-1.11418331156562,
-1.11228213331211,-1.11056891524556,-1.10837725518905,-1.10486768162515,
-1.08207392558648,-1.04896968790573,-1.03753175203287,-1.03545158593828,
-1.03432115612216,-1.03336580283884,-1.03216272045711,-1.02981033159238,
-1.01340945963597,-0.981274539999996,-0.9627547858971,-0.95938354256407,
-0.957233670347246,-0.955524880743624,-0.953598930446261,-0.950342553298724,
-0.937088868806597,-0.911404253094006,-0.884398092641331,-0.880698095120589,
-0.879229561800291,-0.878332290473879,-0.877341393486364,-0.875899919081191,
-0.872092555550014,-0.850788627647346,-0.80917082336085,-0.804099054868068,
-0.801830713192611,-0.800101253661772,-0.798254087388607,-0.795355513878867,
-0.786013685648173,-0.770513916619972,-0.739648525884712,-0.734212395838738,
-0.726028723380377,-0.724068880410922,-0.722952821123224,-0.72199615681779,
-0.720774091379117,-0.718248118217946,-0.714907003993386,-0.672504457360703,
-0.651551069633753,-0.648093923271872,-0.645918101521556,-0.64420675000539,
-0.642296762512592,-0.639112419773774,-0.626771353458799,-0.582127552134743,
-0.570666282615444,-0.568689074562597,-0.567462350944377,-0.566505238999584,
-0.565392329761455,-0.563393427445758,-0.553536859778722,-0.5528747849223),
 .UNSPECIFIED.);
#3800=B_SPLINE_CURVE_WITH_KNOTS('',3,(#269819,#269820,#269821,#269822,#269823,
#269824,#269825,#269826,#269827,#269828,#269829,#269830,#269831,#269832,
#269833,#269834,#269835,#269836,#269837,#269838,#269839,#269840,#269841,
#269842,#269843,#269844,#269845,#269846,#269847,#269848,#269849,#269850,
#269851,#269852,#269853,#269854,#269855,#269856,#269857,#269858,#269859,
#269860,#269861,#269862,#269863,#269864,#269865,#269866,#269867,#269868,
#269869,#269870,#269871,#269872,#269873,#269874,#269875,#269876,#269877,
#269878,#269879,#269880,#269881,#269882,#269883,#269884,#269885,#269886,
#269887,#269888,#269889,#269890,#269891,#269892,#269893,#269894,#269895,
#269896,#269897,#269898,#269899,#269900,#269901,#269902,#269903,#269904,
#269905,#269906,#269907,#269908,#269909,#269910),.UNSPECIFIED.,.F.,.F.,
(4,2,2,2,2,2,2,2,2,2,2,2,2,2,2,2,2,2,2,2,2,2,2,2,2,2,2,2,2,2,2,2,2,2,2,
2,2,2,2,2,2,2,2,2,2,4),(-0.428888253392887,-0.389859328426633,-0.378358579402351,
-0.376362995077369,-0.375122596429184,-0.374153137331245,-0.373023085937846,
-0.37098573958892,-0.360758938600924,-0.312513641509815,-0.302206485955008,
-0.299061935482404,-0.297144969449245,-0.295407266708984,-0.293169695000154,
-0.288488566380338,-0.282351425145204,-0.267177735747699,-0.248292068467238,
-0.233933531333192,-0.222666299052573,-0.220682195170878,-0.219445363767497,
-0.218476343939001,-0.217344086694236,-0.215296015285216,-0.204866403493975,
-0.17962580300663,-0.148114346621445,-0.144522715737607,-0.142291808018878,
-0.140618395217809,-0.138782505179035,-0.13585809218805,-0.132394692094371,
-0.125713363036948,-0.0812843597065226,-0.0784753794816904,-0.0670193387557556,
-0.0650259986512003,-0.0637863187575954,-0.062816977922961,-0.0616865523121097,
-0.0596472650809289,-0.049383163613779,-0.000459594697538254),
 .UNSPECIFIED.);
#3801=B_SPLINE_CURVE_WITH_KNOTS('',3,(#269911,#269912,#269913,#269914,#269915,
#269916,#269917,#269918,#269919,#269920,#269921,#269922,#269923,#269924,
#269925,#269926,#269927,#269928,#269929,#269930,#269931,#269932,#269933,
#269934,#269935,#269936,#269937,#269938,#269939,#269940,#269941,#269942,
#269943,#269944,#269945,#269946,#269947,#269948,#269949,#269950,#269951,
#269952,#269953,#269954,#269955,#269956,#269957,#269958,#269959,#269960,
#269961,#269962,#269963,#269964,#269965,#269966,#269967,#269968,#269969,
#269970,#269971,#269972,#269973,#269974,#269975,#269976,#269977,#269978,
#269979,#269980,#269981,#269982,#269983,#269984,#269985,#269986,#269987,
#269988,#269989,#269990,#269991,#269992,#269993,#269994,#269995,#269996,
#269997,#269998,#269999,#270000,#270001,#270002,#270003,#270004,#270005,
#270006,#270007,#270008,#270009,#270010,#270011,#270012,#270013,#270014,
#270015,#270016,#270017,#270018,#270019,#270020,#270021,#270022,#270023,
#270024,#270025,#270026,#270027,#270028,#270029,#270030,#270031,#270032,
#270033,#270034,#270035,#270036,#270037,#270038,#270039,#270040,#270041,
#270042,#270043,#270044,#270045,#270046,#270047,#270048,#270049,#270050,
#270051,#270052,#270053,#270054),.UNSPECIFIED.,.F.,.F.,(4,2,2,2,2,2,2,2,
2,2,2,2,2,2,2,2,2,2,2,2,2,2,2,2,2,2,2,2,2,2,2,2,2,2,2,2,2,2,2,2,2,2,2,2,
2,2,2,2,2,2,2,2,2,2,2,2,2,2,2,2,2,2,2,2,2,2,2,2,2,2,2,4),(-1.9612040881325,
-1.95267147311146,-1.95000996591669,-1.94814032560028,-1.94652386883341,
-1.94485741353218,-1.94263906333431,-1.93908709900391,-1.92741625365267,
-1.9020119584714,-1.87333145357916,-1.8703437883954,-1.86902607541887,-1.86804813146784,
-1.86696478730102,-1.86513767045306,-1.85879857374555,-1.80916727161314,
-1.8006379616494,-1.79652104137334,-1.79314566437734,-1.79119814565534,
-1.7911768135465,-1.79115325186968,-1.79112722923263,-1.79109849092645,
-1.79106675684813,-1.79103171896284,-1.79099303961576,-1.79096067491587,
-1.79090817464123,-1.78923435367413,-1.78700190512724,-1.78340241064852,
-1.75228854452968,-1.726744721237,-1.71625509555708,-1.71420480047387,-1.71307253508992,
-1.71210426125592,-1.71086936045761,-1.7088902325968,-1.69770376826815,
-1.68335191620711,-1.6645840776608,-1.64375477107296,-1.63867262077675,
-1.63636095688298,-1.63461396905529,-1.63296270493977,-1.63019162778334,
-1.6227600190247,-1.62112671757867,-1.61950104589317,-1.57088919005932,
-1.5606661046734,-1.55862983859817,-1.55750045506403,-1.55653160643218,
-1.55529204705724,-1.5532979401195,-1.54180774819406,-1.49682586185373,
-1.48493644378235,-1.48176520483031,-1.47984307320173,-1.47810783280695,
-1.47588339267295,-1.47231124375276,-1.44013963781075,-1.41540376682114,
-1.40915133348001),.UNSPECIFIED.);
#3802=B_SPLINE_CURVE_WITH_KNOTS('',3,(#270060,#270061,#270062,#270063,#270064,
#270065,#270066,#270067,#270068,#270069,#270070,#270071,#270072,#270073,
#270074,#270075,#270076,#270077,#270078,#270079,#270080,#270081,#270082,
#270083,#270084,#270085,#270086,#270087,#270088,#270089,#270090,#270091,
#270092,#270093,#270094,#270095,#270096,#270097,#270098,#270099,#270100,
#270101,#270102,#270103,#270104,#270105,#270106,#270107,#270108,#270109,
#270110,#270111,#270112,#270113,#270114,#270115,#270116,#270117,#270118,
#270119,#270120,#270121,#270122,#270123,#270124,#270125,#270126,#270127,
#270128,#270129,#270130,#270131,#270132,#270133,#270134,#270135,#270136,
#270137,#270138,#270139,#270140,#270141,#270142,#270143,#270144,#270145,
#270146,#270147,#270148,#270149,#270150,#270151,#270152,#270153,#270154,
#270155,#270156,#270157,#270158,#270159,#270160,#270161,#270162,#270163,
#270164,#270165,#270166,#270167,#270168,#270169,#270170,#270171,#270172,
#270173,#270174,#270175,#270176,#270177,#270178,#270179,#270180,#270181,
#270182,#270183,#270184,#270185),.UNSPECIFIED.,.F.,.F.,(4,2,2,2,2,2,2,2,
2,2,2,2,2,2,2,2,2,2,2,2,2,2,2,2,2,2,2,2,2,2,2,2,2,2,2,2,2,2,2,2,2,2,2,2,
2,2,2,2,2,2,2,2,2,2,2,2,2,2,2,2,2,2,4),(-0.552743087208093,-0.551463645223767,
-0.54956658067619,-0.546441746206178,-0.534805577518398,-0.489718220054633,
-0.477907302734968,-0.475907990292114,-0.474674528531903,-0.473716672362747,
-0.47260806142404,-0.470629420631127,-0.461125444579548,-0.417263029537525,
-0.40244533081584,-0.398970174627786,-0.396975457052239,-0.395288938015448,
-0.393237941555454,-0.389402945754804,-0.36331953863117,-0.336885520914959,
-0.333312049932213,-0.322126859121565,-0.320162836966673,-0.318940032333077,
-0.317983183346863,-0.316867355037947,-0.314855253148225,-0.304764717116578,
-0.252713864175805,-0.245224834697202,-0.242464933780685,-0.240829468877453,
-0.239106039714361,-0.236837322006661,-0.231898959191383,-0.212010395067879,
-0.192531745458719,-0.16674435868709,-0.164379520992794,-0.163173825213962,
-0.162253392146647,-0.161164847488075,-0.159993433562783,-0.158179503489128,
-0.154735457764327,-0.111109549853214,-0.091488356897101,-0.0880776462791279,
-0.0859159384254847,-0.0842061701697754,-0.0822879868149217,-0.0790661507355597,
-0.0662569692942145,-0.0181025773545897,-0.0101837221765631,-0.0082936873134663,
-0.00719361884037062,-0.00625128730748574,-0.00531577404306149,-0.00410080215318163,
-0.000459732030733911),.UNSPECIFIED.);
#3803=B_SPLINE_CURVE_WITH_KNOTS('',3,(#270186,#270187,#270188,#270189,#270190,
#270191,#270192,#270193,#270194,#270195,#270196,#270197,#270198,#270199,
#270200,#270201,#270202,#270203,#270204,#270205,#270206,#270207,#270208,
#270209,#270210,#270211,#270212,#270213,#270214,#270215,#270216,#270217,
#270218,#270219,#270220,#270221,#270222,#270223,#270224,#270225,#270226,
#270227,#270228,#270229,#270230,#270231,#270232,#270233,#270234,#270235,
#270236,#270237,#270238,#270239,#270240,#270241,#270242,#270243,#270244,
#270245,#270246,#270247,#270248,#270249,#270250,#270251,#270252,#270253,
#270254,#270255,#270256,#270257,#270258,#270259,#270260,#270261,#270262,
#270263,#270264,#270265,#270266,#270267,#270268,#270269,#270270,#270271,
#270272,#270273),.UNSPECIFIED.,.F.,.F.,(4,2,2,2,2,2,2,2,2,2,2,2,2,2,2,2,
2,2,2,2,2,2,2,2,2,2,2,2,2,2,2,2,2,2,2,2,2,2,2,2,2,2,2,4),(-1.96139969443972,
-1.92301052490004,-1.89925554019589,-1.89384741182589,-1.89149537379875,
-1.88975951524084,-1.88814869674685,-1.88594369946097,-1.88036227700312,
-1.84695703292058,-1.81904336943247,-1.81612992243739,-1.81451734056035,
-1.81311666723818,-1.81214786267482,-1.811252362167,-1.8097913082852,-1.80616043606158,
-1.77714903053835,-1.74166021980585,-1.73755815576316,-1.73545271362787,
-1.73374860676013,-1.73179455239831,-1.72849300056985,-1.71599753866194,
-1.67282555784453,-1.66027663288336,-1.65814906351459,-1.65700885265265,
-1.65605461456404,-1.65486470156417,-1.65257193362423,-1.63815217947121,
-1.60968290628084,-1.58714493845121,-1.58235366487131,-1.5801129234317,
-1.57839408509754,-1.57675040113243,-1.57394557541505,-1.56614329381475,
-1.56435197886824,-1.53326539915105),.UNSPECIFIED.);
#3804=B_SPLINE_CURVE_WITH_KNOTS('',3,(#270274,#270275,#270276,#270277,#270278,
#270279,#270280,#270281,#270282,#270283,#270284,#270285,#270286,#270287,
#270288,#270289,#270290,#270291,#270292,#270293,#270294,#270295,#270296,
#270297,#270298,#270299,#270300,#270301,#270302,#270303,#270304,#270305,
#270306,#270307,#270308,#270309,#270310,#270311,#270312,#270313,#270314,
#270315,#270316,#270317,#270318,#270319,#270320,#270321,#270322,#270323,
#270324,#270325,#270326,#270327,#270328,#270329,#270330,#270331,#270332,
#270333,#270334,#270335,#270336,#270337,#270338,#270339,#270340,#270341,
#270342,#270343,#270344,#270345,#270346,#270347,#270348,#270349,#270350,
#270351,#270352,#270353,#270354,#270355,#270356,#270357,#270358,#270359,
#270360,#270361,#270362,#270363,#270364,#270365,#270366,#270367,#270368,
#270369,#270370,#270371,#270372,#270373,#270374,#270375,#270376,#270377,
#270378,#270379,#270380,#270381,#270382,#270383,#270384,#270385,#270386,
#270387,#270388,#270389,#270390,#270391,#270392,#270393,#270394,#270395,
#270396,#270397,#270398,#270399,#270400,#270401,#270402,#270403,#270404,
#270405,#270406,#270407,#270408,#270409,#270410,#270411,#270412,#270413,
#270414,#270415,#270416,#270417,#270418,#270419,#270420,#270421,#270422,
#270423,#270424,#270425,#270426,#270427,#270428,#270429,#270430,#270431,
#270432,#270433,#270434,#270435,#270436,#270437,#270438,#270439,#270440,
#270441,#270442,#270443,#270444,#270445,#270446,#270447,#270448,#270449,
#270450,#270451,#270452,#270453,#270454,#270455,#270456,#270457,#270458,
#270459,#270460,#270461,#270462,#270463,#270464,#270465,#270466,#270467,
#270468,#270469,#270470,#270471,#270472,#270473,#270474,#270475,#270476,
#270477,#270478,#270479,#270480,#270481,#270482,#270483,#270484,#270485,
#270486,#270487,#270488,#270489,#270490,#270491),.UNSPECIFIED.,.F.,.F.,
(4,2,2,2,2,2,2,2,2,2,2,2,2,2,2,2,2,2,2,2,2,2,2,2,2,2,2,2,2,2,2,2,2,2,2,
2,2,2,2,2,2,2,2,2,2,2,2,2,2,2,2,2,2,2,2,2,2,2,2,2,2,2,2,2,2,2,2,2,2,2,2,
2,2,2,2,2,2,2,2,2,2,2,2,2,2,2,2,2,2,2,2,2,2,2,2,2,2,2,2,2,2,2,2,2,2,2,2,
2,4),(-1.40915133348001,-1.40508391580612,-1.40304247644158,-1.40191201817527,
-1.40094336836695,-1.39970550964281,-1.39771690763566,-1.38642025125725,
-1.34165807170974,-1.33357200026451,-1.32776908471959,-1.32533162461402,
-1.32356362576985,-1.32194427395641,-1.31975983801312,-1.31439441689396,
-1.2764937377024,-1.26060596855579,-1.24956099127174,-1.24748210837433,
-1.24634359165815,-1.24537581468994,-1.24414901738171,-1.24172549003802,
-1.22107003869045,-1.19877478969409,-1.17714195444833,-1.17195981384783,
-1.16962988190986,-1.16787994837469,-1.16623385157811,-1.16394499399293,
-1.15794324797883,-1.10404343407514,-1.09386118370683,-1.09182691288998,
-1.09069784531232,-1.08972877217392,-1.08848828490619,-1.08649145496779,
-1.07494990806998,-1.02989841241624,-1.0181058444109,-1.01494267235182,
-1.01302211160873,-1.01128615341194,-1.00905781702317,-1.00547332501254,
-0.980787031307708,-0.951134452614773,-0.938642636192832,-0.936601167110025,
-0.935347360372408,-0.93437715148745,-0.933257331183337,-0.931265305263494,
-0.921810652711195,-0.899628081344103,-0.866672630831311,-0.861060233852381,
-0.858833625999757,-0.857203442402559,-0.855443163307646,-0.853051458713777,
-0.847520316822411,-0.839921023637918,-0.794654092326299,-0.782963769433192,
-0.780959255895347,-0.779716439020281,-0.778747134714152,-0.777619618058664,
-0.775592632211924,-0.765541598132576,-0.714659292613148,-0.713417722644121,
-0.706035451980788,-0.703270911545356,-0.701620638403293,-0.699872542827766,
-0.697555762445799,-0.692447350445574,-0.671410162002382,-0.640663568817988,
-0.636288019694443,-0.627069496456753,-0.625018079042758,-0.623872824648781,
-0.622905403773551,-0.62168677583708,-0.619223377029523,-0.591245170842583,
-0.555229149517558,-0.549729320648476,-0.547525296878297,-0.545900859531574,
-0.544136420412792,-0.541720411809742,-0.53604679344736,-0.528193210498726,
-0.483180142221446,-0.471681079668852,-0.469686237288107,-0.468446355058509,
-0.46747733578158,-0.466347838844873,-0.464311595314957,-0.454092568234796,
-0.428759893737338),.UNSPECIFIED.);
#3805=B_SPLINE_CURVE_WITH_KNOTS('',3,(#270496,#270497,#270498,#270499,#270500,
#270501,#270502,#270503,#270504,#270505,#270506,#270507,#270508,#270509,
#270510,#270511,#270512,#270513,#270514,#270515,#270516,#270517,#270518,
#270519,#270520,#270521,#270522,#270523,#270524,#270525,#270526,#270527,
#270528,#270529,#270530,#270531,#270532,#270533,#270534,#270535,#270536,
#270537,#270538,#270539,#270540,#270541,#270542,#270543,#270544,#270545,
#270546,#270547,#270548,#270549,#270550,#270551,#270552,#270553,#270554,
#270555,#270556,#270557,#270558,#270559,#270560,#270561,#270562,#270563,
#270564,#270565,#270566,#270567,#270568,#270569,#270570,#270571,#270572,
#270573,#270574,#270575,#270576,#270577,#270578,#270579,#270580,#270581,
#270582,#270583,#270584,#270585,#270586,#270587,#270588,#270589,#270590,
#270591,#270592,#270593,#270594,#270595,#270596,#270597,#270598,#270599,
#270600,#270601,#270602,#270603,#270604,#270605,#270606,#270607,#270608,
#270609,#270610,#270611,#270612,#270613,#270614,#270615,#270616,#270617,
#270618,#270619,#270620,#270621,#270622,#270623,#270624,#270625,#270626,
#270627,#270628,#270629,#270630,#270631,#270632,#270633,#270634,#270635,
#270636,#270637,#270638,#270639,#270640,#270641,#270642,#270643,#270644,
#270645,#270646,#270647,#270648,#270649,#270650,#270651,#270652,#270653,
#270654,#270655,#270656,#270657,#270658,#270659,#270660,#270661,#270662,
#270663,#270664,#270665,#270666,#270667,#270668,#270669,#270670,#270671,
#270672,#270673,#270674,#270675,#270676,#270677,#270678,#270679,#270680,
#270681,#270682,#270683,#270684,#270685,#270686,#270687,#270688,#270689,
#270690,#270691,#270692,#270693,#270694,#270695,#270696,#270697,#270698,
#270699,#270700,#270701,#270702,#270703,#270704,#270705,#270706,#270707),
 .UNSPECIFIED.,.F.,.F.,(4,2,2,2,2,2,2,2,2,2,2,2,2,2,2,2,2,2,2,2,2,2,2,2,
2,2,2,2,2,2,2,2,2,2,2,2,2,2,2,2,2,2,2,2,2,2,2,2,2,2,2,2,2,2,2,2,2,2,2,2,
2,2,2,2,2,2,2,2,2,2,2,2,2,2,2,2,2,2,2,2,2,2,2,2,2,2,2,2,2,2,2,2,2,2,2,2,
2,2,2,2,2,2,2,2,2,4),(-1.53320397388816,-1.50966452836832,-1.49825110038352,
-1.49321455786972,-1.48922128158519,-1.4871376996192,-1.48543432547076,
-1.48346216608212,-1.48008387280973,-1.46658825100414,-1.42142867176523,
-1.41172794184418,-1.40973810785624,-1.40862725409157,-1.40767001092434,
-1.40644066337572,-1.40445449003373,-1.39281706209862,-1.34798716857844,
-1.34007667138447,-1.33438426795304,-1.33198303019519,-1.33023798413126,
-1.32863749889512,-1.32647545006743,-1.32115101882626,-1.2828863095878,
-1.26712053617903,-1.25615084092342,-1.25409325214859,-1.25296775866684,
-1.25201213719766,-1.25080305859326,-1.2488839537844,-1.23857224866304,
-1.23253287675237,-1.20755141444254,-1.18157807497612,-1.17774666119621,
-1.17569670743855,-1.17401059650931,-1.17201583364374,-1.16853925635632,
-1.15369456906268,-1.10979462708462,-1.10033463391937,-1.0983588289562,
-1.09725095957179,-1.09629319685762,-1.09505915262615,-1.09305753781793,
-1.0811159432783,-1.03586908104928,-1.02451976735837,-1.02142079257929,
-1.01952960018098,-1.01781415911997,-1.01560395131832,-1.01203243310314,
-0.980907882763103,-0.946830801909978,-0.943483755075174,-0.942212709226042,
-0.941304915827275,-0.9403235659916,-0.938931134578296,-0.935442390472182,
-0.91763245860374,-0.900352503326017,-0.896770338363765,-0.870418658840243,
-0.866839776186978,-0.864627232052068,-0.862911340577742,-0.861021027375978,
-0.857926639347896,-0.84663086917273,-0.80131660920427,-0.789341843407383,
-0.787338480226561,-0.786103823990707,-0.785145880622481,-0.784038128866323,
-0.782063337520096,-0.772623089109898,-0.728730834308382,-0.713878799273427,
-0.710401280485735,-0.708406060008061,-0.706719611575979,-0.704669306603929,
-0.700837423278388,-0.674881780103308,-0.650575343825527,-0.63390512614952,
-0.631544054771103,-0.630339055991904,-0.629383509899128,-0.628254405290249,
-0.626180707877962,-0.614882552306129,-0.582736475080812,-0.558914453882635,
-0.555377920765701,-0.553178018698002,-0.552743087208093),.UNSPECIFIED.);
#3806=B_SPLINE_CURVE_WITH_KNOTS('',3,(#270709,#270710,#270711,#270712,#270713,
#270714,#270715,#270716,#270717,#270718,#270719,#270720,#270721,#270722,
#270723,#270724,#270725,#270726,#270727,#270728,#270729,#270730,#270731,
#270732,#270733,#270734,#270735,#270736,#270737,#270738,#270739,#270740,
#270741,#270742,#270743,#270744,#270745,#270746,#270747,#270748,#270749,
#270750,#270751,#270752,#270753,#270754,#270755,#270756,#270757,#270758,
#270759,#270760,#270761,#270762,#270763,#270764,#270765,#270766,#270767,
#270768,#270769,#270770,#270771,#270772,#270773,#270774,#270775,#270776,
#270777,#270778,#270779,#270780,#270781,#270782,#270783,#270784,#270785,
#270786,#270787,#270788,#270789,#270790,#270791,#270792,#270793,#270794,
#270795,#270796,#270797,#270798,#270799,#270800,#270801,#270802,#270803,
#270804,#270805,#270806,#270807,#270808,#270809,#270810,#270811,#270812),
 .UNSPECIFIED.,.F.,.F.,(4,2,2,2,2,2,2,2,2,2,2,2,2,2,2,2,2,2,2,2,2,2,2,2,
2,2,2,2,2,2,2,2,2,2,2,2,2,2,2,2,2,2,2,2,2,2,2,2,2,2,2,4),(-0.428759893737338,
-0.404716844331025,-0.402919395679492,-0.402408249614197,-0.394841801419629,
-0.392050232866161,-0.39039479631456,-0.388649277793538,-0.386349478287384,
-0.381333723302357,-0.36103039735791,-0.331095385157423,-0.325989608056533,
-0.315918560676669,-0.313997320101226,-0.312779797279136,-0.31181247564759,
-0.310666416809,-0.308552910511493,-0.296778285593322,-0.261327808611337,
-0.241255280164544,-0.237801522724213,-0.235612664094383,-0.233881247312594,
-0.231938395040218,-0.228673636288372,-0.215649318905773,-0.164598499888124,
-0.159460609943299,-0.15780545524939,-0.156766136034789,-0.155801514783849,
-0.154826061450868,-0.152413124874335,-0.126344560462695,-0.0880879544475471,
-0.0827520735253491,-0.0805722629789152,-0.0789536535959236,-0.0771838431522886,
-0.0747390824995394,-0.0688956125479379,-0.0607358789217155,-0.0159944835945941,
-0.015518045971129,-0.010656706174842,-0.0041155350938151,-0.0023037002132017,
-0.00122762359849491,-0.00061199511029617,-0.000459178790791266),
 .UNSPECIFIED.);
#3807=B_SPLINE_CURVE_WITH_KNOTS('',3,(#270813,#270814,#270815,#270816,#270817,
#270818,#270819,#270820,#270821,#270822,#270823,#270824,#270825,#270826,
#270827,#270828,#270829,#270830,#270831,#270832,#270833,#270834,#270835,
#270836,#270837,#270838,#270839,#270840,#270841,#270842,#270843,#270844,
#270845,#270846,#270847,#270848,#270849,#270850,#270851,#270852,#270853,
#270854,#270855,#270856,#270857,#270858,#270859,#270860,#270861,#270862,
#270863,#270864,#270865,#270866,#270867,#270868,#270869,#270870,#270871,
#270872,#270873,#270874,#270875,#270876,#270877,#270878,#270879,#270880,
#270881,#270882,#270883,#270884,#270885,#270886,#270887,#270888,#270889,
#270890,#270891,#270892,#270893,#270894,#270895,#270896,#270897,#270898,
#270899,#270900,#270901,#270902,#270903,#270904,#270905,#270906,#270907,
#270908,#270909,#270910,#270911,#270912,#270913,#270914,#270915,#270916,
#270917,#270918,#270919,#270920,#270921,#270922,#270923,#270924,#270925,
#270926,#270927,#270928,#270929,#270930,#270931,#270932,#270933,#270934,
#270935,#270936,#270937,#270938,#270939,#270940),.UNSPECIFIED.,.F.,.F.,
(4,2,2,2,2,2,2,2,2,2,2,2,2,2,2,2,2,2,2,2,2,2,2,2,2,2,2,2,2,2,2,2,2,2,2,
2,2,2,2,2,2,2,2,2,2,2,2,2,2,2,2,2,2,2,2,2,2,2,2,2,2,2,2,4),(-1.96190064593619,
-1.96168461615125,-1.96069057510085,-1.95851065627135,-1.94695118128126,
-1.90185828864699,-1.89011645277352,-1.8869573556812,-1.88503747934445,
-1.88330098565153,-1.8810703508325,-1.87747886034453,-1.84675338089164,
-1.82493177473323,-1.81522115627856,-1.8114579369434,-1.80867935265324,
-1.80766583705941,-1.80676125973021,-1.80579995639157,-1.80439810913233,
-1.80101313141463,-1.76765410610869,-1.73697929888347,-1.73237611593018,
-1.73015392100707,-1.72841847335981,-1.72649410831799,-1.72331453080973,
-1.71947620868156,-1.68241249019077,-1.66598120316435,-1.65473243597924,
-1.65264302178801,-1.65150197386825,-1.65053401105883,-1.64930948394577,
-1.64689793854691,-1.62792858789181,-1.60165984739963,-1.58191077107704,
-1.5769653289044,-1.57467816605182,-1.57293411133833,-1.57127397604316,
-1.56845960225752,-1.56074116168329,-1.5589297775629,-1.50897503072888,
-1.49896526855668,-1.4969401446375,-1.49581284074294,-1.49484319481182,
-1.4935992701191,-1.49159169167385,-1.47985694710387,-1.43657274798547,
-1.42342288937204,-1.42014751417196,-1.41820181962376,-1.41647002649766,
-1.41428360004047,-1.41083938795882,-1.40968633380918),.UNSPECIFIED.);
#3808=B_SPLINE_CURVE_WITH_KNOTS('',3,(#270946,#270947,#270948,#270949,#270950,
#270951,#270952,#270953,#270954,#270955,#270956,#270957,#270958,#270959,
#270960,#270961,#270962,#270963,#270964,#270965,#270966,#270967,#270968,
#270969,#270970,#270971,#270972,#270973,#270974,#270975,#270976,#270977,
#270978,#270979,#270980,#270981,#270982,#270983,#270984,#270985,#270986,
#270987,#270988,#270989,#270990,#270991,#270992,#270993,#270994,#270995,
#270996,#270997,#270998,#270999,#271000,#271001,#271002,#271003,#271004,
#271005,#271006,#271007,#271008,#271009,#271010,#271011,#271012,#271013,
#271014,#271015,#271016,#271017,#271018,#271019,#271020,#271021,#271022,
#271023,#271024,#271025,#271026,#271027,#271028,#271029,#271030,#271031,
#271032,#271033,#271034,#271035,#271036,#271037,#271038,#271039,#271040,
#271041,#271042,#271043,#271044,#271045,#271046,#271047,#271048,#271049,
#271050,#271051,#271052,#271053,#271054,#271055,#271056,#271057,#271058,
#271059,#271060,#271061,#271062,#271063,#271064,#271065,#271066,#271067,
#271068,#271069,#271070,#271071,#271072,#271073),.UNSPECIFIED.,.F.,.F.,
(4,2,2,2,2,2,2,2,2,2,2,2,2,2,2,2,2,2,2,2,2,2,2,2,2,2,2,2,2,2,2,2,2,2,2,
2,2,2,2,2,2,2,2,2,2,2,2,2,2,2,2,2,2,2,2,2,2,2,2,2,2,2,2,4),(-0.552688099404481,
-0.543080226182336,-0.539504565796958,-0.53805672524758,-0.537163091160699,
-0.53616756700887,-0.534704357243157,-0.53075057234971,-0.524762066248855,
-0.480623365040984,-0.465530749174478,-0.46203637809736,-0.460037169602566,
-0.458504601294272,-0.456520903585182,-0.453001459098836,-0.435583191356921,
-0.411571052616499,-0.387531819257294,-0.383826846181367,-0.382357280665463,
-0.381459688388236,-0.380468729446536,-0.379027667458325,-0.375224286509052,
-0.353971633733431,-0.312267525017181,-0.307204858889346,-0.304937865628943,
-0.303208346031917,-0.301360061970108,-0.298457521813873,-0.289083220949639,
-0.273506856760414,-0.244079602444988,-0.241038350357246,-0.229495587397251,
-0.227514205300479,-0.226286152109095,-0.22532882254352,-0.224216601356228,
-0.222221243885509,-0.212429893262151,-0.165921347573548,-0.153686727866053,
-0.150373988210981,-0.148435586993842,-0.146793369908302,-0.146767685125553,
-0.146742833085923,-0.144661257863149,-0.142403430462657,-0.138779885480295,
-0.131624826081075,-0.0908669722810824,-0.0740628942811457,-0.0717002075430645,
-0.0704948320728319,-0.0695392234323915,-0.068410322160803,-0.0663377102429647,
-0.0550639112307698,-0.031404766771521,-0.000460633390386513),
 .UNSPECIFIED.);
#3809=B_SPLINE_CURVE_WITH_KNOTS('',3,(#271074,#271075,#271076,#271077,#271078,
#271079,#271080,#271081,#271082,#271083,#271084,#271085,#271086,#271087,
#271088,#271089,#271090,#271091,#271092,#271093,#271094,#271095,#271096,
#271097,#271098,#271099,#271100,#271101,#271102,#271103,#271104,#271105,
#271106,#271107,#271108,#271109,#271110,#271111,#271112,#271113,#271114,
#271115,#271116,#271117,#271118,#271119,#271120,#271121,#271122,#271123,
#271124,#271125,#271126,#271127,#271128,#271129,#271130,#271131,#271132,
#271133,#271134,#271135,#271136,#271137,#271138,#271139,#271140,#271141,
#271142,#271143,#271144,#271145,#271146,#271147,#271148,#271149,#271150,
#271151,#271152,#271153,#271154,#271155,#271156,#271157,#271158,#271159,
#271160,#271161,#271162,#271163,#271164,#271165,#271166,#271167,#271168,
#271169,#271170,#271171,#271172,#271173,#271174,#271175,#271176,#271177,
#271178,#271179,#271180,#271181),.UNSPECIFIED.,.F.,.F.,(4,2,2,2,2,2,2,2,
2,2,2,2,2,2,2,2,2,2,2,2,2,2,2,2,2,2,2,2,2,2,2,2,2,2,2,2,2,2,2,2,2,2,2,2,
2,2,2,2,2,2,2,2,2,4),(-1.96139844108125,-1.95862844136409,-1.95608434317704,
-1.95439993741817,-1.95276752843083,-1.95092989768122,-1.94807308310635,
-1.93987637397639,-1.89570893868502,-1.884398659602,-1.88024286206601,-1.87724914064632,
-1.87594005117869,-1.87497317614033,-1.87390788235311,-1.87212413415349,
-1.86606151973467,-1.86492223942551,-1.8207625547489,-1.80942705350922,
-1.80441469803589,-1.8015963265701,-1.79967265328359,-1.79783116935074,
-1.79616510496926,-1.79396837401651,-1.79044062736615,-1.76688913963448,
-1.73449036700842,-1.72315654338757,-1.72108177490944,-1.71995273922696,
-1.71899763931417,-1.71779370226622,-1.71535806835029,-1.69422066415637,
-1.67435303256067,-1.65096231054999,-1.64559551229352,-1.64325023494624,
-1.64151509538318,-1.6399019034764,-1.63768891105677,-1.63206220928154,
-1.59124091749299,-1.57008729720638,-1.56629357047034,-1.56485435598024,
-1.56386410079659,-1.5629667052867,-1.56149662505678,-1.55778650913308,
-1.53356319905232,-1.53320397388816),.UNSPECIFIED.);
#3810=B_SPLINE_CURVE_WITH_KNOTS('',3,(#271182,#271183,#271184,#271185,#271186,
#271187,#271188,#271189,#271190,#271191,#271192,#271193,#271194,#271195,
#271196,#271197,#271198,#271199,#271200,#271201,#271202,#271203,#271204,
#271205,#271206,#271207,#271208,#271209,#271210,#271211,#271212,#271213,
#271214,#271215,#271216,#271217,#271218,#271219,#271220,#271221,#271222,
#271223,#271224,#271225,#271226,#271227,#271228,#271229,#271230,#271231,
#271232,#271233,#271234,#271235,#271236,#271237,#271238,#271239,#271240,
#271241,#271242,#271243,#271244,#271245,#271246,#271247,#271248,#271249,
#271250,#271251,#271252,#271253,#271254,#271255,#271256,#271257,#271258,
#271259,#271260,#271261,#271262,#271263,#271264,#271265,#271266,#271267,
#271268,#271269,#271270,#271271,#271272,#271273,#271274,#271275,#271276,
#271277,#271278,#271279,#271280,#271281,#271282,#271283,#271284,#271285,
#271286,#271287,#271288,#271289,#271290,#271291,#271292,#271293,#271294,
#271295,#271296,#271297,#271298,#271299,#271300,#271301,#271302,#271303,
#271304,#271305,#271306,#271307,#271308,#271309,#271310,#271311,#271312,
#271313,#271314,#271315,#271316,#271317,#271318,#271319,#271320,#271321,
#271322,#271323,#271324,#271325,#271326,#271327,#271328,#271329,#271330,
#271331,#271332,#271333,#271334,#271335,#271336,#271337,#271338,#271339,
#271340,#271341,#271342,#271343,#271344,#271345,#271346,#271347,#271348,
#271349,#271350,#271351,#271352,#271353,#271354,#271355,#271356,#271357,
#271358,#271359,#271360,#271361,#271362,#271363,#271364,#271365,#271366,
#271367,#271368,#271369,#271370,#271371,#271372,#271373,#271374,#271375,
#271376,#271377,#271378,#271379,#271380,#271381,#271382,#271383,#271384,
#271385,#271386,#271387,#271388,#271389,#271390,#271391),.UNSPECIFIED.,
 .F.,.F.,(4,2,2,2,2,2,2,2,2,2,2,2,2,2,2,2,2,2,2,2,2,2,2,2,2,2,2,2,2,2,2,
2,2,2,2,2,2,2,2,2,2,2,2,2,2,2,2,2,2,2,2,2,2,2,2,2,2,2,2,2,2,2,2,2,2,2,2,
2,2,2,2,2,2,2,2,2,2,2,2,2,2,2,2,2,2,2,2,2,2,2,2,2,2,2,2,2,2,2,2,2,2,2,2,
2,4),(-1.40968633380918,-1.39106742680057,-1.36246948304688,-1.34546881464893,
-1.342043193426,-1.34065039062903,-1.33965966527309,-1.33873535778086,-1.33742980206677,
-1.33390723691068,-1.3019074788918,-1.2693883787101,-1.26519682504602,-1.26305614603808,
-1.26132845087531,-1.25935254724624,-1.25602586501169,-1.24356350758808,
-1.2384553738643,-1.19998398357561,-1.18785030399311,-1.18572019061832,
-1.18457028338014,-1.18360277167804,-1.18238887581029,-1.18048045237261,
-1.17068118034152,-1.1668665169803,-1.16248498682396,-1.12612554559954,
-1.11225673600861,-1.10892768503792,-1.10697017086597,-1.10524013965216,
-1.10307229749897,-1.09968924715811,-1.08158250230395,-1.0442113848527,
-1.03219990575911,-1.03007503991455,-1.02892622238753,-1.0279585928189,
-1.02674324189647,-1.02437549468282,-1.00813738135619,-0.981492838669131,
-0.957733247361841,-0.954169152711609,-0.951946417928362,-0.950210485774761,
-0.948285519111915,-0.945104797814909,-0.93312103475791,-0.888140708118944,
-0.8766807426488,-0.874687083627747,-0.873447249883194,-0.872477818071752,
-0.871347320386012,-0.869307986752799,-0.859045478216756,-0.820972519713406,
-0.801768519518855,-0.798345051951284,-0.79616469837017,-0.794433221641158,
-0.792483132420461,-0.789188839512947,-0.775797154433583,-0.749729962387388,
-0.723355306327301,-0.719635660403577,-0.718153066161175,-0.717245044169105,
-0.716239726994622,-0.714772013826291,-0.710863562826411,-0.688579344666991,
-0.648389014961514,-0.643132163968524,-0.641022096777244,-0.639259515637705,
-0.637442184553477,-0.634757993576022,-0.627334395658667,-0.616129170063791,
-0.570568931545942,-0.56455542585171,-0.562762609822515,-0.561686316369379,
-0.560704960716779,-0.559369037015774,-0.556282116718981,-0.551972810877206,
-0.540083179658493,-0.497911694747334,-0.496119454022882,-0.488481427233226,
-0.485678182890874,-0.484019762626761,-0.482273971516346,-0.479978627920426,
-0.474991940057305,-0.454928055038549,-0.428975714778273),.UNSPECIFIED.);
#3811=B_SPLINE_CURVE_WITH_KNOTS('',3,(#271396,#271397,#271398,#271399,#271400,
#271401,#271402,#271403,#271404,#271405,#271406,#271407,#271408,#271409,
#271410,#271411,#271412,#271413,#271414,#271415,#271416,#271417,#271418,
#271419,#271420,#271421,#271422,#271423,#271424,#271425,#271426,#271427,
#271428,#271429,#271430,#271431,#271432,#271433,#271434,#271435,#271436,
#271437,#271438,#271439,#271440,#271441,#271442,#271443,#271444,#271445,
#271446,#271447,#271448,#271449,#271450,#271451,#271452,#271453,#271454,
#271455,#271456,#271457,#271458,#271459,#271460,#271461,#271462,#271463,
#271464,#271465,#271466,#271467,#271468,#271469,#271470,#271471,#271472,
#271473,#271474,#271475,#271476,#271477,#271478,#271479,#271480,#271481,
#271482,#271483,#271484,#271485,#271486,#271487,#271488,#271489,#271490,
#271491,#271492,#271493,#271494,#271495,#271496,#271497,#271498,#271499,
#271500,#271501,#271502,#271503,#271504,#271505,#271506,#271507,#271508,
#271509,#271510,#271511,#271512,#271513,#271514,#271515,#271516,#271517,
#271518,#271519,#271520,#271521,#271522,#271523,#271524,#271525,#271526,
#271527,#271528,#271529,#271530,#271531,#271532,#271533,#271534,#271535,
#271536,#271537,#271538,#271539,#271540,#271541,#271542,#271543,#271544,
#271545,#271546,#271547,#271548,#271549,#271550,#271551,#271552,#271553,
#271554,#271555,#271556,#271557,#271558,#271559,#271560,#271561,#271562,
#271563,#271564,#271565,#271566,#271567,#271568,#271569,#271570,#271571,
#271572,#271573,#271574,#271575,#271576,#271577,#271578,#271579,#271580,
#271581,#271582,#271583,#271584,#271585,#271586,#271587,#271588,#271589,
#271590,#271591,#271592,#271593,#271594,#271595,#271596,#271597,#271598,
#271599,#271600,#271601),.UNSPECIFIED.,.F.,.F.,(4,2,2,2,2,2,2,2,2,2,2,2,
2,2,2,2,2,2,2,2,2,2,2,2,2,2,2,2,2,2,2,2,2,2,2,2,2,2,2,2,2,2,2,2,2,2,2,2,
2,2,2,2,2,2,2,2,2,2,2,2,2,2,2,2,2,2,2,2,2,2,2,2,2,2,2,2,2,2,2,2,2,2,2,2,
2,2,2,2,2,2,2,2,2,2,2,2,2,2,2,2,2,2,4),(-1.53336547467346,-1.52837184435063,
-1.48442974513329,-1.47488253058741,-1.47290042235175,-1.47179060832695,
-1.47083248247449,-1.46959945575158,-1.46760190496144,-1.45579765986533,
-1.41069975383796,-1.39909887260053,-1.39597714931827,-1.39408075118677,
-1.39236619062233,-1.3901649484176,-1.38662398159865,-1.36263550520391,
-1.33059653134075,-1.31931253196297,-1.31723954400461,-1.31611064800646,
-1.31515519933782,-1.3139502338751,-1.31158889882908,-1.2948235307505,-1.25416706748176,
-1.2432600914759,-1.24020195105538,-1.23831979853081,-1.23660212294275,
-1.23441113223264,-1.23082434819327,-1.2030964015189,-1.17488958685796,
-1.16361238461625,-1.16153985383053,-1.16041111321517,-1.15945561192927,
-1.15825038498334,-1.15588828341261,-1.13910090731295,-1.09838164875309,
-1.08754909498645,-1.08449765020777,-1.08261675501951,-1.08089833135568,
-1.07870378371674,-1.07510560230137,-1.04642140931866,-1.01877849766069,
-1.00789258149254,-1.00583875196146,-1.00471388690404,-1.00375797635223,
-1.00254745440242,-1.00016033571524,-0.981248841793334,-0.952221101471087,
-0.933198710977822,-0.929809318983887,-0.927653875782813,-0.925944469073865,
-0.924021850089608,-0.920780872771078,-0.907730783989583,-0.856076908028822,
-0.851340763316662,-0.849717652431206,-0.848790116696345,-0.847820675793825,
-0.846497917426387,-0.84342895725636,-0.839138593121752,-0.827274251109634,
-0.785085431849636,-0.783334438478305,-0.775580662580146,-0.772781592659653,
-0.771138236896277,-0.769417546175213,-0.767170775937671,-0.762352554144694,
-0.743389309903729,-0.71011417866222,-0.706029152146253,-0.696466763316421,
-0.694589367860108,-0.693392754735033,-0.692437516822451,-0.691301278696193,
-0.689194880672401,-0.67718006591844,-0.639541317287688,-0.631531720317251,
-0.620640317735664,-0.61745708906259,-0.615546939879591,-0.614006137608468,
-0.611913430961883,-0.607878876761342,-0.57369546293598,-0.552688099404481),
 .UNSPECIFIED.);
#3812=B_SPLINE_CURVE_WITH_KNOTS('',3,(#271603,#271604,#271605,#271606,#271607,
#271608,#271609,#271610,#271611,#271612,#271613,#271614,#271615,#271616,
#271617,#271618,#271619,#271620,#271621,#271622,#271623,#271624,#271625,
#271626,#271627,#271628,#271629,#271630,#271631,#271632,#271633,#271634,
#271635,#271636,#271637,#271638,#271639,#271640,#271641,#271642,#271643,
#271644,#271645,#271646,#271647,#271648,#271649,#271650,#271651,#271652,
#271653,#271654,#271655,#271656,#271657,#271658,#271659,#271660,#271661,
#271662,#271663,#271664,#271665,#271666,#271667,#271668,#271669,#271670,
#271671,#271672,#271673,#271674,#271675,#271676,#271677,#271678,#271679,
#271680,#271681,#271682,#271683,#271684,#271685,#271686,#271687,#271688,
#271689,#271690,#271691,#271692,#271693,#271694,#271695,#271696,#271697,
#271698,#271699,#271700,#271701,#271702,#271703,#271704,#271705,#271706,
#271707,#271708,#271709,#271710),.UNSPECIFIED.,.F.,.F.,(4,2,2,2,2,2,2,2,
2,2,2,2,2,2,2,2,2,2,2,2,2,2,2,2,2,2,2,2,2,2,2,2,2,2,2,2,2,2,2,2,2,2,2,2,
2,2,2,2,2,2,2,2,2,4),(-0.428975714778273,-0.426294289416057,-0.40993005346988,
-0.407558066930467,-0.406341681853969,-0.405373836461037,-0.404225474340388,
-0.402103323387923,-0.390158402561099,-0.353353699220583,-0.334672070253794,
-0.331267833299295,-0.329093278878789,-0.327362292265962,-0.325408383853849,
-0.322096964581708,-0.308477197377358,-0.281614425310441,-0.268637902858494,
-0.265586062554237,-0.253981995449396,-0.251981381344263,-0.250739465741727,
-0.249769868660508,-0.248640859213042,-0.246608378460792,-0.236470268848025,
-0.183707896345193,-0.176840259344229,-0.174155621690342,-0.172520029576801,
-0.170797472072009,-0.168499366602091,-0.165941834277573,-0.161609776557055,
-0.152444782583097,-0.115749441376234,-0.115301071137147,-0.098564513831558,
-0.096183043635308,-0.0949647617296688,-0.0939969867365006,-0.0928505717771237,
-0.0907368404218699,-0.0789728306255426,-0.0360263231000887,-0.0244352099508055,
-0.0199538763255009,-0.0177552350180094,-0.0160988411211704,-0.0144808829084192,
-0.0126017398449633,-0.00991766704936141,-0.000458885783622974),
 .UNSPECIFIED.);
#3813=B_SPLINE_CURVE_WITH_KNOTS('',3,(#271711,#271712,#271713,#271714,#271715,
#271716,#271717,#271718,#271719,#271720,#271721,#271722,#271723,#271724,
#271725,#271726,#271727,#271728,#271729,#271730,#271731,#271732,#271733,
#271734,#271735,#271736,#271737,#271738,#271739,#271740,#271741,#271742,
#271743,#271744,#271745,#271746,#271747,#271748,#271749,#271750,#271751,
#271752,#271753,#271754,#271755,#271756,#271757,#271758,#271759,#271760,
#271761,#271762,#271763,#271764,#271765,#271766,#271767,#271768,#271769,
#271770,#271771,#271772,#271773,#271774,#271775,#271776,#271777,#271778,
#271779,#271780,#271781,#271782,#271783,#271784,#271785,#271786,#271787,
#271788,#271789,#271790,#271791,#271792,#271793,#271794,#271795,#271796,
#271797,#271798,#271799,#271800,#271801,#271802,#271803,#271804,#271805,
#271806,#271807,#271808,#271809,#271810),.UNSPECIFIED.,.F.,.F.,(4,3,3,3,
3,3,3,3,3,3,3,3,3,3,3,3,3,3,3,3,3,3,3,3,3,3,3,3,3,3,3,3,3,4),(172.787595947799,
172.910921322851,173.034741091045,173.159172349731,173.183505325507,173.29520328459,
173.406702633491,173.51809106504,173.629411511197,173.740706806736,173.852102689415,
173.963544589889,174.075203755146,174.180839176163,174.292537996151,174.4040382227,
174.515427541451,174.62674888277,174.738045079852,174.849441866703,174.960884674288,
175.072544739568,175.17817302682,175.289867246144,175.401362865262,175.5127475755,
175.624064314911,175.735355924369,175.846748182612,175.958186486273,176.069842148544,
176.175506877477,176.287193067858,176.326648334931),.UNSPECIFIED.);
#3814=B_SPLINE_CURVE_WITH_KNOTS('',3,(#271816,#271817,#271818,#271819,#271820,
#271821,#271822,#271823,#271824,#271825,#271826,#271827,#271828,#271829,
#271830,#271831,#271832,#271833,#271834,#271835,#271836,#271837,#271838,
#271839,#271840,#271841,#271842,#271843,#271844,#271845,#271846,#271847,
#271848,#271849,#271850,#271851,#271852,#271853,#271854,#271855,#271856,
#271857,#271858,#271859,#271860,#271861,#271862,#271863,#271864,#271865,
#271866,#271867,#271868,#271869,#271870,#271871,#271872,#271873,#271874,
#271875,#271876,#271877,#271878,#271879,#271880,#271881,#271882,#271883,
#271884,#271885,#271886,#271887,#271888,#271889,#271890,#271891,#271892,
#271893,#271894,#271895,#271896,#271897,#271898,#271899,#271900,#271901,
#271902,#271903,#271904,#271905,#271906,#271907,#271908,#271909,#271910,
#271911,#271912,#271913,#271914,#271915),.UNSPECIFIED.,.F.,.F.,(4,3,3,3,
3,3,3,3,3,3,3,3,3,3,3,3,3,3,3,3,3,3,3,3,3,3,3,3,3,3,3,3,3,4),(179.070781255062,
179.180731622204,179.29056170515,179.400316708238,179.51004171136,179.619858971895,
179.729722080855,179.839787565431,179.920490921002,180.032021520138,180.143353165283,
180.254573782191,180.365726576664,180.476854656937,180.588085464791,180.699363098701,
180.810861893943,180.918222920992,181.030131969172,181.141840515982,181.25343684756,
181.364963554317,181.476463128009,181.588058687758,181.69969799648,181.811548524454,
181.915954920982,182.027784331895,182.139452203846,182.256796239415,182.368281431854,
182.479735307744,182.591228863916,182.608828346121),.UNSPECIFIED.);
#3815=B_SPLINE_CURVE_WITH_KNOTS('',3,(#271916,#271917,#271918,#271919,#271920,
#271921,#271922,#271923,#271924,#271925,#271926,#271927,#271928,#271929,
#271930,#271931,#271932,#271933,#271934,#271935,#271936,#271937,#271938,
#271939,#271940,#271941,#271942,#271943,#271944,#271945,#271946,#271947,
#271948,#271949,#271950,#271951,#271952,#271953,#271954,#271955,#271956,
#271957,#271958,#271959,#271960,#271961,#271962,#271963,#271964,#271965,
#271966,#271967,#271968,#271969,#271970,#271971,#271972,#271973,#271974,
#271975,#271976,#271977,#271978,#271979,#271980,#271981,#271982,#271983,
#271984,#271985,#271986,#271987,#271988,#271989,#271990,#271991,#271992,
#271993,#271994,#271995,#271996,#271997,#271998,#271999,#272000,#272001,
#272002,#272003,#272004,#272005,#272006,#272007,#272008,#272009,#272010,
#272011,#272012,#272013,#272014,#272015,#272016,#272017,#272018,#272019,
#272020,#272021,#272022,#272023,#272024,#272025,#272026,#272027,#272028,
#272029,#272030,#272031,#272032,#272033,#272034,#272035,#272036,#272037,
#272038,#272039,#272040,#272041,#272042,#272043,#272044,#272045,#272046,
#272047,#272048,#272049,#272050,#272051,#272052,#272053,#272054,#272055,
#272056,#272057,#272058,#272059,#272060,#272061,#272062,#272063,#272064,
#272065,#272066,#272067,#272068,#272069,#272070,#272071,#272072,#272073,
#272074,#272075,#272076,#272077,#272078,#272079,#272080,#272081,#272082,
#272083,#272084,#272085,#272086,#272087,#272088,#272089,#272090,#272091,
#272092,#272093,#272094,#272095,#272096,#272097,#272098,#272099,#272100,
#272101,#272102,#272103,#272104,#272105),.UNSPECIFIED.,.F.,.F.,(4,2,2,2,
2,2,2,2,2,2,2,2,2,2,2,2,2,2,2,2,2,2,2,2,2,2,2,2,2,2,2,2,2,2,2,2,2,2,2,2,
2,2,2,2,2,2,2,2,2,2,2,2,2,2,2,2,2,2,2,2,2,2,2,2,2,2,2,2,2,2,2,2,2,2,2,2,
2,2,2,2,2,2,2,2,2,2,2,2,2,2,2,2,2,2,4),(-1.9614308235416,-1.94268900312366,
-1.94097478816021,-1.93984265879353,-1.93892930799748,-1.93797196576572,
-1.93677921220793,-1.93491631367841,-1.92560864232203,-1.91834408018366,
-1.90452575359003,-1.89212755721821,-1.86756302972069,-1.8637402797583,
-1.86169175717883,-1.86000517100933,-1.85800789120636,-1.85452196051238,
-1.83955418950439,-1.79576306360682,-1.78942937129978,-1.78663823525168,
-1.78447142584376,-1.78332570005554,-1.78332282173635,-1.78331993323669,
-1.78331703450265,-1.78331412545015,-1.78331120601872,-1.78330827614636,
-1.78330533579758,-1.78330238489228,-1.7832994233645,-1.78329645114521,
-1.78329346816853,-1.78329047438485,-1.78328746972599,-1.78328445411386,
-1.78328142748082,-1.78327838976972,-1.78327534091679,-1.78327228084261,
-1.78326920947643,-1.78326612674772,-1.78326303259987,-1.783259926961,-1.78325680975979,
-1.78325368093163,-1.78325054039445,-1.78324738808096,-1.78324422391465,
-1.78324104783337,-1.78323785974327,-1.78323456594562,-1.78323121572594,
-1.78322780802806,-1.7832243417827,-1.78322081588857,-1.78321722922791,
-1.78321358067877,-1.78320986907769,-1.78320609322951,-1.78320225191204,
-1.78319834390456,-1.78319436794346,-1.78319032273446,-1.78223382367081,
-1.78100584010655,-1.77902206808031,-1.76740288404476,-1.76463201604894,
-1.73216599774,-1.71227154692013,-1.70817406294939,-1.70607025292478,-1.70436713886138,
-1.70241388061299,-1.69911291230588,-1.68661227720452,-1.64035330500017,
-1.63057691350791,-1.62858409354707,-1.62747329241742,-1.62651642311937,
-1.62528847978424,-1.6233074629858,-1.61177054201696,-1.58272870650308,
-1.55611307498688,-1.55226524108138,-1.55021110886266,-1.54852390237823,
-1.54653058526767,-1.54306342431935,-1.53336547467346),.UNSPECIFIED.);
#3816=B_SPLINE_CURVE_WITH_KNOTS('',3,(#272107,#272108,#272109,#272110,#272111,
#272112,#272113,#272114,#272115,#272116,#272117,#272118,#272119,#272120,
#272121,#272122,#272123,#272124,#272125,#272126,#272127,#272128,#272129,
#272130,#272131,#272132,#272133,#272134,#272135,#272136,#272137,#272138,
#272139,#272140,#272141,#272142,#272143,#272144,#272145,#272146,#272147,
#272148,#272149,#272150,#272151,#272152,#272153,#272154,#272155,#272156,
#272157,#272158,#272159,#272160,#272161,#272162,#272163,#272164,#272165,
#272166,#272167,#272168,#272169,#272170,#272171,#272172,#272173,#272174,
#272175,#272176,#272177,#272178,#272179,#272180,#272181,#272182,#272183,
#272184,#272185),.UNSPECIFIED.,.F.,.F.,(4,3,3,3,3,3,3,3,3,3,3,3,3,3,3,3,
3,3,3,3,3,3,3,3,3,3,4),(176.326648334931,176.43810614833,176.549468213479,
176.660777418181,176.772076570763,176.883486761318,176.994956518131,177.106630489581,
177.172840728134,177.284544809411,177.396050364686,177.507445049464,177.618771784714,
177.730073394283,177.841475578811,177.952923784954,178.064589178818,178.170174578791,
178.282750413203,178.392857900582,178.502858512952,178.61279717524,178.727293194952,
178.837307342147,178.947380692747,179.057620733242,179.070781254086),
 .UNSPECIFIED.);
#3817=B_SPLINE_CURVE_WITH_KNOTS('',3,(#272186,#272187,#272188,#272189,#272190,
#272191,#272192,#272193,#272194,#272195,#272196,#272197,#272198,#272199,
#272200,#272201,#272202,#272203,#272204,#272205,#272206,#272207,#272208,
#272209,#272210,#272211,#272212,#272213,#272214,#272215,#272216,#272217,
#272218,#272219,#272220,#272221,#272222,#272223,#272224,#272225,#272226,
#272227,#272228,#272229,#272230,#272231,#272232,#272233,#272234,#272235,
#272236,#272237,#272238,#272239,#272240,#272241,#272242,#272243,#272244,
#272245,#272246,#272247,#272248,#272249,#272250,#272251,#272252,#272253,
#272254,#272255,#272256,#272257,#272258,#272259,#272260,#272261,#272262,
#272263,#272264,#272265,#272266,#272267,#272268,#272269,#272270,#272271,
#272272,#272273,#272274,#272275,#272276,#272277,#272278,#272279,#272280,
#272281,#272282),.UNSPECIFIED.,.F.,.F.,(4,3,3,3,3,3,3,3,3,3,3,3,3,3,3,3,
3,3,3,3,3,3,3,3,3,3,3,3,3,3,3,3,4),(179.070781254618,179.167508429447,179.279232171007,
179.390757034655,179.502170802123,179.613516365171,179.72483651818,179.836256656482,
179.947722524142,180.059404856864,180.164842280104,180.276572613084,180.388104921402,
180.499526644752,180.610880655354,180.722209728673,180.833639447233,180.945115271315,
181.056808057843,181.162176130761,181.273712396525,181.385049880979,181.496276444199,
181.607435281783,181.718569491901,181.829806385347,181.941090169468,182.052594773618,
182.159509981418,182.272001570259,182.383719822213,182.496598079497,182.609476336781),
 .UNSPECIFIED.);
#3818=B_SPLINE_CURVE_WITH_KNOTS('',3,(#272286,#272287,#272288,#272289,#272290,
#272291,#272292,#272293,#272294,#272295,#272296,#272297,#272298,#272299,
#272300,#272301,#272302,#272303,#272304,#272305,#272306,#272307,#272308,
#272309,#272310,#272311,#272312,#272313,#272314,#272315,#272316,#272317,
#272318,#272319,#272320,#272321,#272322,#272323,#272324,#272325,#272326,
#272327,#272328,#272329,#272330,#272331,#272332,#272333,#272334,#272335,
#272336,#272337,#272338,#272339,#272340,#272341,#272342,#272343,#272344,
#272345,#272346),.UNSPECIFIED.,.F.,.F.,(4,3,3,3,3,3,3,3,3,3,3,3,3,3,3,3,
3,3,3,3,4),(-4.09254174883831,-3.98933540262706,-3.88362403077663,-3.77807219570531,
-3.67264620016847,-3.56728749237124,-3.46196026146344,-3.35662874243922,
-3.25118948387453,-3.14568938024508,-3.04001271921558,-2.9920015519703,
-2.88746494371954,-2.78310353644332,-2.6788397915561,-2.57463623079532,
-2.47045545788326,-2.36619046068214,-2.26188581379375,-2.15739845815038,
-2.06549250598675),.UNSPECIFIED.);
#3819=B_SPLINE_CURVE_WITH_KNOTS('',3,(#272350,#272351,#272352,#272353,#272354,
#272355,#272356,#272357,#272358,#272359,#272360,#272361,#272362,#272363,
#272364,#272365,#272366,#272367,#272368,#272369,#272370,#272371,#272372,
#272373,#272374,#272375,#272376,#272377,#272378,#272379,#272380,#272381,
#272382,#272383),.UNSPECIFIED.,.F.,.F.,(4,3,3,3,3,3,3,3,3,3,3,4),(0.,0.107977626581242,
0.219196923257323,0.327096938677548,0.434999393044677,0.542933442426255,
0.650928272809477,0.75909084708409,0.867351523472262,0.975811259859153,
0.997731999989892,1.11419103802964),.UNSPECIFIED.);
#3820=B_SPLINE_CURVE_WITH_KNOTS('',3,(#272385,#272386,#272387,#272388,#272389,
#272390,#272391,#272392,#272393,#272394,#272395,#272396,#272397,#272398,
#272399,#272400,#272401,#272402,#272403,#272404,#272405,#272406,#272407,
#272408,#272409,#272410,#272411,#272412,#272413,#272414,#272415,#272416,
#272417,#272418,#272419,#272420,#272421,#272422,#272423,#272424,#272425,
#272426,#272427,#272428,#272429,#272430,#272431,#272432,#272433,#272434,
#272435,#272436,#272437,#272438,#272439,#272440,#272441,#272442,#272443,
#272444,#272445,#272446,#272447,#272448,#272449,#272450,#272451,#272452,
#272453,#272454,#272455,#272456,#272457,#272458,#272459,#272460,#272461,
#272462,#272463,#272464,#272465,#272466,#272467,#272468,#272469,#272470,
#272471,#272472,#272473,#272474,#272475,#272476,#272477,#272478,#272479,
#272480,#272481,#272482,#272483,#272484,#272485,#272486,#272487,#272488,
#272489,#272490,#272491,#272492,#272493,#272494,#272495,#272496,#272497,
#272498,#272499,#272500,#272501,#272502,#272503,#272504,#272505,#272506,
#272507,#272508,#272509,#272510,#272511,#272512,#272513,#272514,#272515,
#272516,#272517,#272518,#272519,#272520,#272521,#272522,#272523,#272524,
#272525,#272526,#272527,#272528,#272529,#272530,#272531,#272532,#272533,
#272534,#272535,#272536,#272537,#272538,#272539,#272540,#272541,#272542,
#272543,#272544,#272545,#272546,#272547,#272548,#272549,#272550,#272551,
#272552,#272553,#272554,#272555,#272556,#272557,#272558,#272559,#272560,
#272561,#272562,#272563,#272564,#272565,#272566,#272567,#272568,#272569,
#272570,#272571,#272572,#272573,#272574),.UNSPECIFIED.,.F.,.F.,(4,3,3,3,
3,3,3,3,3,3,3,3,3,3,3,3,3,3,3,3,3,3,3,3,3,3,3,3,3,3,3,3,3,3,3,3,3,3,3,3,
3,3,3,3,3,3,3,3,3,3,3,3,3,3,3,3,3,3,3,3,3,3,3,4),(1.11419103844213,1.21719280051008,
1.32003416186357,1.42278762303634,1.52549195609498,1.62818584556488,1.73097732788672,
1.83382151759089,1.93684671784687,1.99546399997979,2.10112854781365,2.20663431253005,
2.31201552937527,2.4173302707785,2.52261439146672,2.62790370121181,2.73330245386298,
2.83876289331518,2.9444018424341,2.99319599996969,3.09888197434551,3.20441296474065,
3.30982494020846,3.41517386477733,3.52049555101897,3.62582577011254,3.73127024136871,
3.83677921532455,3.94247055732954,3.99092799995959,4.09628474419618,4.20148036114117,
4.30654951999312,4.41155120731135,4.51652176472632,4.62149748813044,4.72658479154611,
4.83173454902658,4.93706728469541,4.98865999994949,5.09419322308703,5.19956760510387,
5.30481804223367,5.41000246650403,5.51515694593056,5.62031750420636,5.72558976703579,
5.83092483105164,5.93644146087887,5.98639199993938,6.09191543290443,6.19728038085416,
6.30252196221905,6.40769789584472,6.51284426401526,6.6179971050861,6.72326230422794,
6.8285906675891,6.93410123136067,6.98412399992928,7.10015672991934,7.21584063271221,
7.33095558898145,7.39737594217472),.UNSPECIFIED.);
#3821=B_SPLINE_CURVE_WITH_KNOTS('',3,(#272576,#272577,#272578,#272579,#272580,
#272581,#272582,#272583,#272584,#272585),.UNSPECIFIED.,.F.,.F.,(4,1,1,1,
1,1,1,4),(7.39737634520923,7.98185599991918,8.97958799990908,9.97731999989899,
10.9750519998889,11.9727839998788,12.9705159998687,13.6805616523888),
 .UNSPECIFIED.);
#3822=B_SPLINE_CURVE_WITH_KNOTS('',3,(#272587,#272588,#272589,#272590,#272591,
#272592,#272593,#272594,#272595,#272596,#272597),.UNSPECIFIED.,.F.,.F.,
(4,1,1,1,1,1,1,1,4),(13.6805616523888,13.9682479998586,14.9659799998485,
15.9637119998384,16.9614439998283,17.9591759998182,18.9569079998081,19.954639999798,
19.9637469595684),.UNSPECIFIED.);
#3823=B_SPLINE_CURVE_WITH_KNOTS('',3,(#272599,#272600,#272601,#272602,#272603,
#272604,#272605,#272606,#272607,#272608,#272609,#272610,#272611,#272612,
#272613,#272614,#272615,#272616,#272617,#272618,#272619,#272620,#272621,
#272622,#272623,#272624,#272625,#272626,#272627,#272628,#272629,#272630,
#272631,#272632,#272633,#272634,#272635,#272636,#272637,#272638,#272639,
#272640,#272641,#272642,#272643,#272644,#272645,#272646,#272647,#272648,
#272649,#272650,#272651,#272652,#272653,#272654,#272655,#272656,#272657,
#272658,#272659,#272660,#272661,#272662,#272663,#272664,#272665,#272666,
#272667,#272668,#272669,#272670,#272671,#272672,#272673,#272674,#272675,
#272676,#272677,#272678,#272679,#272680,#272681,#272682,#272683,#272684,
#272685,#272686,#272687,#272688,#272689,#272690,#272691,#272692,#272693,
#272694,#272695,#272696,#272697,#272698,#272699,#272700,#272701,#272702,
#272703,#272704,#272705,#272706,#272707,#272708,#272709,#272710,#272711,
#272712,#272713,#272714,#272715,#272716,#272717,#272718,#272719,#272720,
#272721,#272722,#272723,#272724,#272725,#272726,#272727,#272728,#272729,
#272730,#272731,#272732,#272733,#272734,#272735,#272736,#272737,#272738,
#272739,#272740,#272741,#272742,#272743,#272744,#272745,#272746,#272747,
#272748,#272749,#272750,#272751,#272752,#272753,#272754,#272755,#272756,
#272757,#272758,#272759,#272760,#272761,#272762,#272763,#272764,#272765,
#272766,#272767,#272768,#272769,#272770,#272771,#272772,#272773,#272774,
#272775,#272776,#272777,#272778,#272779,#272780,#272781,#272782,#272783,
#272784,#272785,#272786,#272787,#272788),.UNSPECIFIED.,.F.,.F.,(4,3,3,3,
3,3,3,3,3,3,3,3,3,3,3,3,3,3,3,3,3,3,3,3,3,3,3,3,3,3,3,3,3,3,3,3,3,3,3,3,
3,3,3,3,3,3,3,3,3,3,3,3,3,3,3,3,3,3,3,3,3,3,3,4),(19.9637469595684,20.0690782985152,
20.1794900111743,20.2845353554799,20.3895172806125,20.4944721574661,20.5994363154026,
20.7045140318183,20.8096579909059,20.9149798917531,20.9523719997879,21.0578734648353,
21.1632159338049,21.2684343889456,21.373586807792,21.4787093080487,21.5838379631019,
21.689078658814,21.7943823015801,21.8998680679502,21.9501039997778,22.0556054642515,
22.1609479326213,22.2661663871265,22.3713188053156,22.4764413048939,22.581569959249,
22.6868106542371,22.7921142962635,22.8976000618774,22.9478359997677,23.0533374659502,
23.1586799360592,23.2638983923401,23.3690508123263,23.4741733137208,23.5793019699084,
23.6845426667408,23.7898463106212,23.8953320780843,23.9455679997576,24.0510694651247,
24.1564119344083,24.2616303898528,24.3667828089963,24.4719053095432,24.5770339648792,
24.6822746608604,24.7875783038884,24.8930640705064,24.9432999997475,25.0488014651073,
25.1541439343807,25.2593623898114,25.3645148089389,25.4696373094671,25.5747659647825,
25.6800066607395,25.7853103037412,25.89079607033,25.9410319997374,26.0685438801395,
26.1944144505649,26.2469320748526),.UNSPECIFIED.);
#3824=B_SPLINE_CURVE_WITH_KNOTS('',3,(#272790,#272791,#272792,#272793,#272794,
#272795,#272796,#272797,#272798,#272799),.UNSPECIFIED.,.F.,.F.,(4,1,1,1,
1,1,1,4),(26.246932266748,26.9387639997273,27.9364959997172,28.9342279997071,
29.931959999697,30.9296919996869,31.9274239996768,32.5301175739276),
 .UNSPECIFIED.);
#3825=B_SPLINE_CURVE_WITH_KNOTS('',3,(#272801,#272802,#272803,#272804,#272805,
#272806,#272807,#272808,#272809,#272810),.UNSPECIFIED.,.F.,.F.,(4,1,1,1,
1,1,1,4),(32.5301175739276,32.9251559996667,33.9228879996566,34.9206199996464,
35.9183519996363,36.9160839996262,37.9138159996161,38.813294074911),
 .UNSPECIFIED.);
#3826=B_SPLINE_CURVE_WITH_KNOTS('',3,(#272812,#272813,#272814,#272815,#272816,
#272817,#272818,#272819,#272820,#272821,#272822,#272823,#272824,#272825,
#272826,#272827,#272828,#272829,#272830,#272831,#272832,#272833,#272834,
#272835,#272836,#272837,#272838,#272839,#272840,#272841,#272842,#272843,
#272844,#272845,#272846,#272847,#272848,#272849,#272850,#272851,#272852,
#272853,#272854,#272855,#272856,#272857,#272858,#272859,#272860,#272861,
#272862,#272863,#272864,#272865,#272866,#272867,#272868,#272869,#272870,
#272871,#272872,#272873,#272874,#272875,#272876,#272877,#272878,#272879,
#272880,#272881,#272882,#272883,#272884,#272885,#272886,#272887,#272888,
#272889,#272890,#272891,#272892,#272893,#272894,#272895,#272896,#272897,
#272898,#272899,#272900,#272901,#272902,#272903,#272904,#272905,#272906,
#272907,#272908,#272909,#272910,#272911,#272912,#272913,#272914,#272915,
#272916,#272917,#272918,#272919,#272920,#272921,#272922,#272923,#272924,
#272925,#272926,#272927,#272928,#272929,#272930,#272931,#272932,#272933,
#272934,#272935,#272936,#272937,#272938,#272939,#272940,#272941,#272942,
#272943,#272944,#272945,#272946,#272947,#272948,#272949,#272950,#272951,
#272952,#272953,#272954,#272955,#272956,#272957,#272958,#272959,#272960,
#272961,#272962,#272963,#272964,#272965,#272966,#272967,#272968,#272969,
#272970,#272971,#272972,#272973,#272974,#272975,#272976,#272977,#272978,
#272979,#272980,#272981,#272982,#272983,#272984,#272985,#272986,#272987,
#272988,#272989,#272990,#272991,#272992,#272993,#272994,#272995,#272996,
#272997,#272998,#272999,#273000,#273001),.UNSPECIFIED.,.F.,.F.,(4,3,3,3,
3,3,3,3,3,3,3,3,3,3,3,3,3,3,3,3,3,3,3,3,3,3,3,3,3,3,3,3,3,3,3,3,3,3,3,3,
3,3,3,3,3,3,3,3,3,3,3,3,3,3,3,3,3,3,3,3,3,3,3,4),(38.8133028811072,38.911547999606,
39.0170494650914,39.1223919344932,39.2276103900556,39.3327628093167,39.4378853099806,
39.5430139654329,39.6482546615285,39.7535583046701,39.859044071399,39.9092799995959,
40.0147814650811,40.1201239344827,40.2253423900448,40.3304948093057,40.4356173099693,
40.5407459654213,40.6459866615167,40.751290304658,40.8567760713867,40.9070119995858,
41.0125134650709,41.1178559344726,41.2230743900347,41.3282268092956,41.4333493099592,
41.5384779654113,41.6437186615067,41.749022304648,41.8545080713767,41.9047439995757,
42.0102454650609,42.1155879344627,42.2208063900248,42.3259588092858,42.4310813099494,
42.5362099654016,42.641450661497,42.7467543046384,42.8522400713671,42.9024759995656,
43.0079774650508,43.1133199344525,43.2185383900146,43.3236908092756,43.4288133099392,
43.5339419653913,43.6391826614867,43.7444863046281,43.8499720713568,43.9002079995555,
44.0057094650407,44.1110519344423,44.2162703900044,44.3214228092653,44.4265453099289,
44.5316739653811,44.6369146614765,44.7422183046179,44.8477040713466,44.8979399995454,
45.0494261607052,45.0964881882868),.UNSPECIFIED.);
#3827=B_SPLINE_CURVE_WITH_KNOTS('',3,(#273003,#273004,#273005,#273006,#273007,
#273008,#273009,#273010,#273011,#273012),.UNSPECIFIED.,.F.,.F.,(4,1,1,1,
1,1,1,4),(45.0964914212202,45.8956719995353,46.8934039995252,47.8911359995151,
48.888867999505,49.8865999994949,50.8843319994848,51.3796734954663),
 .UNSPECIFIED.);
#3828=B_SPLINE_CURVE_WITH_KNOTS('',3,(#273014,#273015,#273016,#273017,#273018,
#273019,#273020,#273021,#273022,#273023),.UNSPECIFIED.,.F.,.F.,(4,1,1,1,
1,1,1,4),(51.3796734954663,51.8820639994747,52.8797959994646,53.8775279994545,
54.8752599994444,55.8729919994343,56.8707239994242,57.6628562328904),
 .UNSPECIFIED.);
#3829=B_SPLINE_CURVE_WITH_KNOTS('',3,(#273025,#273026,#273027,#273028,#273029,
#273030,#273031,#273032,#273033,#273034,#273035,#273036,#273037,#273038,
#273039,#273040,#273041,#273042,#273043,#273044,#273045,#273046,#273047,
#273048,#273049,#273050,#273051,#273052,#273053,#273054,#273055,#273056,
#273057,#273058,#273059,#273060,#273061,#273062,#273063,#273064,#273065,
#273066,#273067,#273068,#273069,#273070,#273071,#273072,#273073,#273074,
#273075,#273076,#273077,#273078,#273079,#273080,#273081,#273082,#273083,
#273084,#273085,#273086,#273087,#273088,#273089,#273090,#273091,#273092,
#273093,#273094,#273095,#273096,#273097,#273098,#273099,#273100,#273101,
#273102,#273103,#273104,#273105,#273106,#273107,#273108,#273109,#273110,
#273111,#273112,#273113,#273114,#273115,#273116,#273117,#273118,#273119,
#273120,#273121,#273122,#273123,#273124,#273125,#273126,#273127,#273128,
#273129,#273130,#273131,#273132,#273133,#273134,#273135,#273136,#273137,
#273138,#273139,#273140,#273141,#273142,#273143,#273144,#273145,#273146,
#273147,#273148,#273149,#273150,#273151,#273152,#273153,#273154,#273155,
#273156,#273157,#273158,#273159,#273160,#273161,#273162,#273163,#273164,
#273165,#273166,#273167,#273168,#273169,#273170,#273171,#273172,#273173,
#273174,#273175,#273176,#273177,#273178,#273179,#273180,#273181,#273182,
#273183,#273184,#273185,#273186,#273187,#273188,#273189,#273190,#273191,
#273192,#273193,#273194,#273195,#273196,#273197,#273198,#273199,#273200,
#273201,#273202,#273203,#273204,#273205,#273206,#273207,#273208,#273209,
#273210,#273211,#273212,#273213,#273214),.UNSPECIFIED.,.F.,.F.,(4,3,3,3,
3,3,3,3,3,3,3,3,3,3,3,3,3,3,3,3,3,3,3,3,3,3,3,3,3,3,3,3,3,3,3,3,3,3,3,3,
3,3,3,3,3,3,3,3,3,3,3,3,3,3,3,3,3,3,3,3,3,3,3,4),(57.6628588026459,57.8117407599622,
57.8684559994141,57.9739574648993,58.079299934301,58.1845183898631,58.289670809124,
58.3947933097876,58.4999219652397,58.6051626613351,58.7104663044764,58.8159520712051,
58.866187999404,58.9716894648892,59.0770319342909,59.1822503898531,59.287402809114,
59.3925253097776,59.4976539652298,59.6028946613253,59.7081983044666,59.8136840711954,
59.8639199993939,59.9694214648791,60.0747639342808,60.179982389843,60.2851348091039,
60.3902573097675,60.4953859652196,60.600626661315,60.7059303044564,60.8114160711851,
60.8616519993838,60.967153464869,61.0724959342707,61.1777143898329,61.2828668090938,
61.3879893097574,61.4931179652095,61.5983586613049,61.7036623044463,61.809148071175,
61.8593839993737,61.9648854648589,62.0702279342605,62.1754463898227,62.2805988090836,
62.3857213097472,62.4908499651993,62.5960906612947,62.7013943044361,62.8068800711648,
62.8571159993636,62.9626174648488,63.0679599342505,63.1731783898126,63.2783308090735,
63.3834533097371,63.4885819651894,63.5938226612848,63.6991263044261,63.8046120711549,
63.8548479993535,63.9460441098255),.UNSPECIFIED.);
#3830=B_SPLINE_CURVE_WITH_KNOTS('',3,(#273216,#273217,#273218,#273219,#273220,
#273221,#273222,#273223,#273224,#273225),.UNSPECIFIED.,.F.,.F.,(4,1,1,1,
1,1,1,4),(63.9460528086984,64.8525799993434,65.8503119993333,66.8480439993232,
67.8457759993131,68.843507999303,69.8412399992929,70.2292294170051),
 .UNSPECIFIED.);
#3831=B_SPLINE_CURVE_WITH_KNOTS('',3,(#273227,#273228,#273229,#273230,#273231,
#273232,#273233,#273234,#273235,#273236),.UNSPECIFIED.,.F.,.F.,(4,1,1,1,
1,1,1,4),(70.2292294170051,70.8389719992828,71.8367039992727,72.8344359992626,
73.8321679992525,74.8298999992424,75.8276319992323,76.5124147241847),
 .UNSPECIFIED.);
#3832=B_SPLINE_CURVE_WITH_KNOTS('',3,(#273238,#273239,#273240,#273241,#273242,
#273243,#273244,#273245,#273246,#273247,#273248,#273249,#273250,#273251,
#273252,#273253,#273254,#273255,#273256,#273257,#273258,#273259,#273260,
#273261,#273262,#273263,#273264,#273265,#273266,#273267,#273268,#273269,
#273270,#273271,#273272,#273273,#273274,#273275,#273276,#273277,#273278,
#273279,#273280,#273281,#273282,#273283,#273284,#273285,#273286,#273287,
#273288,#273289,#273290,#273291,#273292,#273293,#273294,#273295,#273296,
#273297,#273298,#273299,#273300,#273301,#273302,#273303,#273304,#273305,
#273306,#273307,#273308,#273309,#273310,#273311,#273312,#273313,#273314,
#273315,#273316,#273317,#273318,#273319,#273320,#273321,#273322,#273323,
#273324,#273325,#273326,#273327,#273328,#273329,#273330,#273331,#273332,
#273333,#273334,#273335,#273336,#273337,#273338,#273339,#273340,#273341,
#273342,#273343,#273344,#273345,#273346,#273347,#273348,#273349,#273350,
#273351,#273352,#273353,#273354,#273355,#273356,#273357,#273358,#273359,
#273360,#273361,#273362,#273363,#273364,#273365,#273366,#273367,#273368,
#273369,#273370,#273371,#273372,#273373,#273374,#273375,#273376,#273377,
#273378,#273379,#273380,#273381,#273382,#273383,#273384,#273385,#273386,
#273387,#273388,#273389,#273390,#273391,#273392,#273393,#273394,#273395,
#273396,#273397,#273398,#273399,#273400,#273401,#273402,#273403,#273404,
#273405,#273406,#273407,#273408,#273409,#273410,#273411,#273412,#273413,
#273414,#273415,#273416,#273417,#273418,#273419,#273420,#273421,#273422,
#273423,#273424,#273425,#273426,#273427),.UNSPECIFIED.,.F.,.F.,(4,3,3,3,
3,3,3,3,3,3,3,3,3,3,3,3,3,3,3,3,3,3,3,3,3,3,3,3,3,3,3,3,3,3,3,3,3,3,3,3,
3,3,3,3,3,3,3,3,3,3,3,3,3,3,3,3,3,3,3,3,3,3,3,4),(76.5124149285909,76.637196824743,
76.7635407964299,76.8253639992222,76.9308654647074,77.0362079341089,77.1414263896711,
77.2465788089319,77.3517013095955,77.4568299650476,77.562070661143,77.6673743042843,
77.772860071013,77.8230959992121,77.9285974646973,78.0339399340991,78.1391583896612,
78.2443108089222,78.3494333095858,78.454561965038,78.5598026611334,78.6651063042747,
78.7705920710035,78.820827999202,78.9263294646872,79.0316719340889,79.1368903896511,
79.242042808912,79.3471653095756,79.4522939650277,79.5575346611232,79.6628383042645,
79.7683240709932,79.8185599991919,79.9240614646771,80.0294039340788,80.134622389641,
80.2397748089019,80.3448973095655,80.4500259650177,80.5552666611131,80.6605703042544,
80.7660560709831,80.8162919991818,80.921793464667,81.0271359340687,81.1323543896309,
81.2375068088918,81.3426293095554,81.4477579650076,81.552998661103,81.6583023042443,
81.763788070973,81.8140239991717,81.9192319607283,82.0287779695578,82.1337006658273,
82.2385600199007,82.3433925828576,82.4482348643447,82.5531902794066,82.6582126869609,
82.7634106837078,82.7956000313643),.UNSPECIFIED.);
#3833=B_SPLINE_CURVE_WITH_KNOTS('',3,(#273429,#273430,#273431,#273432,#273433,
#273434,#273435,#273436,#273437,#273438,#273439,#273440),.UNSPECIFIED.,
 .F.,.F.,(4,2,1,1,1,1,1,1,4),(82.7956000313643,82.8117559991616,83.8094879991515,
84.8072199991414,85.8049519991313,86.8026839991212,87.8004159991111,88.798147999101,
89.0787811501394),.UNSPECIFIED.);
#3834=B_SPLINE_CURVE_WITH_KNOTS('',3,(#273442,#273443,#273444,#273445,#273446,
#273447,#273448,#273449,#273450,#273451,#273452,#273453,#273454,#273455,
#273456,#273457,#273458,#273459,#273460,#273461,#273462,#273463,#273464,
#273465,#273466,#273467,#273468,#273469,#273470,#273471,#273472,#273473,
#273474,#273475,#273476,#273477,#273478,#273479,#273480,#273481,#273482,
#273483,#273484,#273485,#273486,#273487,#273488,#273489,#273490,#273491,
#273492,#273493,#273494,#273495,#273496,#273497,#273498,#273499,#273500,
#273501,#273502,#273503,#273504,#273505,#273506,#273507,#273508,#273509,
#273510,#273511,#273512,#273513,#273514,#273515,#273516,#273517,#273518,
#273519,#273520,#273521,#273522,#273523,#273524,#273525,#273526,#273527,
#273528,#273529,#273530,#273531,#273532,#273533,#273534,#273535,#273536,
#273537,#273538,#273539,#273540,#273541,#273542,#273543,#273544,#273545,
#273546,#273547,#273548,#273549,#273550,#273551,#273552,#273553,#273554,
#273555,#273556,#273557,#273558,#273559,#273560,#273561,#273562,#273563,
#273564,#273565,#273566,#273567,#273568,#273569,#273570,#273571,#273572,
#273573,#273574,#273575,#273576,#273577,#273578,#273579,#273580,#273581,
#273582,#273583,#273584,#273585,#273586,#273587,#273588,#273589,#273590,
#273591,#273592,#273593,#273594,#273595,#273596,#273597,#273598,#273599,
#273600,#273601,#273602,#273603,#273604,#273605,#273606,#273607,#273608,
#273609,#273610,#273611,#273612,#273613,#273614,#273615,#273616,#273617,
#273618,#273619,#273620,#273621,#273622,#273623,#273624,#273625,#273626,
#273627,#273628,#273629,#273630,#273631),.UNSPECIFIED.,.F.,.F.,(4,3,3,3,
3,3,3,3,3,3,3,3,3,3,3,3,3,3,3,3,3,3,3,3,3,3,3,3,3,3,3,3,3,3,3,3,3,3,3,3,
3,3,3,3,3,3,3,3,3,3,3,3,3,3,3,3,3,3,3,3,3,3,3,4),(89.0787853385439,89.1830981544274,
89.2873607770994,89.3916104742801,89.4959590610254,89.6003555960421,89.7049471415805,
89.7958799990909,89.901381464576,90.0067239339778,90.1119423895399,90.2170948088009,
90.3222173094644,90.4273459649163,90.5325866610117,90.6378903041529,90.7433760708817,
90.7936119990808,90.899113464566,91.0044559339678,91.10967438953,91.214826808791,
91.3199493094545,91.4250779649066,91.530318661002,91.6356223041434,91.7411080708722,
91.7913439990707,91.8968454645558,92.0021879339574,92.1074063895196,92.2125588087803,
92.3176813094439,92.4228099648959,92.5280506609912,92.6333543041327,92.7388400708613,
92.7890759990606,92.8945774645458,92.9999199339476,93.1051383895098,93.2102908087707,
93.3154133094343,93.4205419648867,93.5257826609821,93.6310863041234,93.7365720708521,
93.7868079990505,93.8923094645358,93.9976519339373,94.1028703894995,94.2080228087603,
94.313145309424,94.4182739648759,94.5235146609713,94.6288183041127,94.7343040708413,
94.7845399990404,94.8922505472161,94.9997777540247,95.1071208600479,95.2143559113678,
95.3215053251644,95.3619706457235),.UNSPECIFIED.);
#3835=B_SPLINE_CURVE_WITH_KNOTS('',3,(#273633,#273634,#273635,#273636,#273637,
#273638,#273639,#273640,#273641,#273642,#273643,#273644,#273645,#273646,
#273647,#273648,#273649,#273650,#273651,#273652,#273653,#273654,#273655,
#273656,#273657,#273658,#273659,#273660,#273661,#273662,#273663,#273664,
#273665,#273666,#273667,#273668,#273669,#273670,#273671,#273672,#273673,
#273674,#273675,#273676,#273677,#273678,#273679,#273680,#273681,#273682,
#273683,#273684,#273685,#273686,#273687,#273688,#273689,#273690,#273691,
#273692,#273693,#273694,#273695,#273696,#273697,#273698,#273699,#273700,
#273701,#273702,#273703,#273704,#273705,#273706,#273707,#273708,#273709,
#273710,#273711,#273712,#273713,#273714,#273715,#273716,#273717,#273718,
#273719,#273720,#273721,#273722,#273723,#273724,#273725,#273726,#273727,
#273728,#273729,#273730,#273731,#273732,#273733,#273734,#273735,#273736,
#273737,#273738,#273739,#273740,#273741,#273742,#273743,#273744,#273745,
#273746,#273747,#273748,#273749,#273750,#273751,#273752,#273753,#273754,
#273755,#273756,#273757,#273758,#273759,#273760,#273761,#273762,#273763,
#273764,#273765,#273766,#273767,#273768,#273769,#273770,#273771,#273772,
#273773,#273774,#273775,#273776,#273777,#273778,#273779,#273780,#273781,
#273782,#273783,#273784,#273785,#273786,#273787,#273788,#273789,#273790,
#273791,#273792,#273793,#273794,#273795,#273796,#273797,#273798,#273799,
#273800,#273801,#273802,#273803,#273804,#273805,#273806,#273807,#273808,
#273809,#273810,#273811,#273812,#273813,#273814,#273815,#273816,#273817,
#273818,#273819,#273820,#273821,#273822),.UNSPECIFIED.,.F.,.F.,(4,3,3,3,
3,3,3,3,3,3,3,3,3,3,3,3,3,3,3,3,3,3,3,3,3,3,3,3,3,3,3,3,3,3,3,3,3,3,3,3,
3,3,3,3,3,3,3,3,3,3,3,3,3,3,3,3,3,3,3,3,3,3,3,4),(95.3619706460871,95.4766888558802,
95.591751289489,95.7073231093368,95.7822719990302,95.8877734645154,95.9931159339172,
96.0983343894794,96.2034868087403,96.308609309404,96.4137379648561,96.5189786609516,
96.624282304093,96.7297680708218,96.7800039990202,96.8855054645054,96.990847933907,
97.0960663894692,97.2012188087301,97.3063413093937,97.4114699648458,97.5167106609412,
97.6220143040825,97.7275000708112,97.7777359990101,97.8832374644953,97.988579933897,
98.0937983894591,98.19895080872,98.3040733093836,98.4092019648357,98.5144426609311,
98.6197463040725,98.7252320708012,98.775467999,98.8809694644852,98.9863119338869,
99.091530389449,99.1966828087099,99.3018053093735,99.4069339648256,99.512174660921,
99.6174783040623,99.722964070791,99.7731999989899,99.8787014644752,99.984043933877,
100.089262389439,100.1944148087,100.299537309364,100.404665964816,100.509906660912,
100.615210304053,100.720696070782,100.77093199898,100.88020999322,100.984063595876,
101.087819532397,101.191515830589,101.295190429698,101.398937371334,101.502726497014,
101.606663108459,101.645155952903),.UNSPECIFIED.);
#3836=B_SPLINE_CURVE_WITH_KNOTS('',3,(#273824,#273825,#273826,#273827,#273828,
#273829,#273830,#273831,#273832,#273833,#273834),.UNSPECIFIED.,.F.,.F.,
(4,1,1,1,1,1,1,1,4),(101.645155952903,101.76866399897,102.76639599896,103.764127998949,
104.761859998939,105.759591998929,106.757323998919,107.755055998909,107.928341260083),
 .UNSPECIFIED.);
#3837=B_SPLINE_CURVE_WITH_KNOTS('',3,(#273836,#273837,#273838,#273839,#273840,
#273841,#273842,#273843,#273844,#273845,#273846,#273847,#273848,#273849,
#273850,#273851,#273852,#273853,#273854,#273855,#273856,#273857,#273858,
#273859,#273860,#273861,#273862,#273863,#273864,#273865,#273866,#273867,
#273868,#273869,#273870,#273871,#273872,#273873,#273874,#273875,#273876,
#273877,#273878,#273879,#273880,#273881,#273882,#273883,#273884,#273885,
#273886,#273887,#273888,#273889,#273890,#273891,#273892,#273893,#273894,
#273895,#273896,#273897,#273898,#273899,#273900,#273901,#273902,#273903,
#273904,#273905,#273906,#273907,#273908,#273909,#273910,#273911,#273912,
#273913,#273914,#273915,#273916,#273917,#273918,#273919,#273920,#273921,
#273922,#273923,#273924,#273925,#273926,#273927,#273928,#273929,#273930,
#273931,#273932,#273933,#273934,#273935,#273936,#273937,#273938,#273939,
#273940,#273941,#273942,#273943,#273944,#273945,#273946,#273947,#273948,
#273949,#273950,#273951,#273952,#273953,#273954,#273955,#273956,#273957,
#273958,#273959,#273960,#273961,#273962,#273963,#273964,#273965,#273966,
#273967,#273968,#273969,#273970,#273971,#273972,#273973,#273974,#273975,
#273976,#273977,#273978,#273979,#273980,#273981,#273982,#273983,#273984,
#273985,#273986,#273987,#273988,#273989,#273990,#273991,#273992,#273993,
#273994,#273995,#273996,#273997,#273998,#273999,#274000,#274001,#274002,
#274003,#274004,#274005,#274006,#274007,#274008,#274009,#274010,#274011,
#274012,#274013,#274014,#274015,#274016,#274017,#274018,#274019,#274020,
#274021,#274022,#274023,#274024,#274025),.UNSPECIFIED.,.F.,.F.,(4,3,3,3,
3,3,3,3,3,3,3,3,3,3,3,3,3,3,3,3,3,3,3,3,3,3,3,3,3,3,3,3,3,3,3,3,3,3,3,3,
3,3,3,3,3,3,3,3,3,3,3,3,3,3,3,3,3,3,3,3,3,3,3,4),(107.928341260083,108.032099150482,
108.135757208958,108.239353576204,108.342926301162,108.446586291681,108.550286108514,
108.654177288281,108.752787998899,108.858289464384,108.963631933786,109.068850389348,
109.174002808609,109.279125309273,109.384253964725,109.48949466082,109.594798303962,
109.700284070691,109.750519998889,109.856021464374,109.961363933776,110.066582389338,
110.171734808599,110.276857309263,110.381985964715,110.48722666081,110.592530303952,
110.69801607068,110.748251998879,110.853753464364,110.959095933766,111.064314389328,
111.169466808589,111.274589309252,111.379717964704,111.4849586608,111.590262303941,
111.69574807067,111.745983998869,111.851485464354,111.956827933756,112.062046389318,
112.167198808579,112.272321309243,112.377449964695,112.482690660791,112.587994303932,
112.693480070661,112.743715998859,112.849217464344,112.954559933746,113.059778389308,
113.164930808568,113.270053309232,113.375181964683,113.480422660778,113.585726303919,
113.691212070648,113.741447998848,113.858967602029,113.971035808353,114.082867908485,
114.194397089511,114.211526411573),.UNSPECIFIED.);
#3838=B_SPLINE_CURVE_WITH_KNOTS('',3,(#274027,#274028,#274029,#274030,#274031,
#274032,#274033,#274034,#274035,#274036),.UNSPECIFIED.,.F.,.F.,(4,1,1,1,
1,1,1,4),(114.211526567262,114.739179998838,115.736911998828,116.734643998818,
117.732375998808,118.730107998798,119.727839998788,120.494711874442),
 .UNSPECIFIED.);
#3839=B_SPLINE_CURVE_WITH_KNOTS('',3,(#274038,#274039,#274040,#274041,#274042,
#274043,#274044,#274045,#274046,#274047,#274048),.UNSPECIFIED.,.F.,.F.,
(4,1,1,1,1,1,1,1,4),(120.494711874442,120.725571998778,121.723303998768,
122.721035998758,123.718767998747,124.716499998737,125.714231998727,126.711963998717,
126.777897181621),.UNSPECIFIED.);
#3840=B_SPLINE_CURVE_WITH_KNOTS('',3,(#274050,#274051,#274052,#274053,#274054,
#274055,#274056,#274057,#274058,#274059,#274060,#274061,#274062,#274063,
#274064,#274065,#274066,#274067,#274068,#274069,#274070,#274071,#274072,
#274073,#274074,#274075,#274076,#274077,#274078,#274079,#274080,#274081,
#274082,#274083,#274084,#274085,#274086,#274087,#274088,#274089,#274090,
#274091,#274092,#274093,#274094,#274095,#274096,#274097,#274098,#274099,
#274100,#274101,#274102,#274103,#274104,#274105,#274106,#274107,#274108,
#274109,#274110,#274111,#274112,#274113,#274114,#274115,#274116,#274117,
#274118,#274119,#274120,#274121,#274122,#274123,#274124,#274125,#274126,
#274127,#274128,#274129,#274130,#274131,#274132,#274133,#274134,#274135,
#274136,#274137,#274138,#274139,#274140,#274141,#274142,#274143,#274144,
#274145,#274146,#274147,#274148,#274149,#274150,#274151,#274152,#274153,
#274154,#274155,#274156,#274157,#274158,#274159,#274160,#274161,#274162,
#274163,#274164,#274165,#274166,#274167,#274168,#274169,#274170,#274171,
#274172,#274173,#274174,#274175,#274176,#274177,#274178,#274179,#274180,
#274181,#274182,#274183,#274184,#274185,#274186,#274187,#274188,#274189,
#274190,#274191,#274192,#274193,#274194,#274195,#274196,#274197,#274198,
#274199,#274200,#274201,#274202,#274203,#274204,#274205,#274206,#274207,
#274208,#274209,#274210,#274211,#274212,#274213,#274214,#274215,#274216,
#274217,#274218,#274219,#274220,#274221,#274222,#274223,#274224,#274225,
#274226,#274227,#274228,#274229,#274230,#274231,#274232,#274233,#274234,
#274235,#274236),.UNSPECIFIED.,.F.,.F.,(4,3,3,3,3,3,3,3,3,3,3,3,3,3,3,3,
3,3,3,3,3,3,3,3,3,3,3,3,3,3,3,3,3,3,3,3,3,3,3,3,3,3,3,3,3,3,3,3,3,3,3,3,
3,3,3,3,3,3,3,3,3,3,4),(126.777897181621,126.882369364822,126.986673464764,
127.090884174499,127.195039013725,127.299175425165,127.403404764753,127.507677502594,
127.612144068716,127.709695998707,127.815197464192,127.920539933594,128.025758389156,
128.130910808417,128.236033309081,128.341161964533,128.446402660628,128.55170630377,
128.657192070498,128.707427998697,128.812929464182,128.918271933584,129.023490389146,
129.128642808407,129.23376530907,129.338893964523,129.444134660618,129.549438303759,
129.654924070488,129.705159998687,129.810661464172,129.916003933574,130.021222389136,
130.126374808397,130.231497309061,130.336625964513,130.441866660608,130.54717030375,
130.652656070478,130.702891998677,130.808393464162,130.913735933564,131.018954389126,
131.124106808387,131.22922930905,131.334357964503,131.439598660598,131.54490230374,
131.650388070468,131.700623998667,131.806125464152,131.911467933554,132.016686389117,
132.121838808378,132.226961309041,132.332089964493,132.437330660589,132.54263430373,
132.648120070459,132.698355998657,132.818881802562,132.939982145448,133.061082488334),
 .UNSPECIFIED.);
#3841=B_SPLINE_CURVE_WITH_KNOTS('',3,(#274238,#274239,#274240,#274241,#274242,
#274243,#274244,#274245,#274246,#274247,#274248,#274249,#274250,#274251,
#274252,#274253,#274254,#274255,#274256,#274257,#274258,#274259,#274260,
#274261,#274262,#274263,#274264,#274265,#274266,#274267,#274268,#274269,
#274270,#274271,#274272,#274273,#274274,#274275,#274276,#274277,#274278,
#274279,#274280,#274281,#274282,#274283,#274284,#274285,#274286,#274287,
#274288,#274289,#274290,#274291,#274292,#274293,#274294,#274295,#274296,
#274297,#274298,#274299,#274300,#274301,#274302,#274303,#274304,#274305,
#274306,#274307,#274308,#274309,#274310,#274311,#274312,#274313,#274314,
#274315,#274316,#274317,#274318,#274319,#274320,#274321,#274322,#274323,
#274324,#274325,#274326,#274327,#274328,#274329,#274330,#274331,#274332,
#274333,#274334,#274335,#274336,#274337,#274338,#274339,#274340,#274341,
#274342,#274343,#274344,#274345,#274346,#274347,#274348,#274349,#274350,
#274351,#274352,#274353,#274354,#274355,#274356,#274357,#274358,#274359,
#274360,#274361,#274362,#274363,#274364,#274365,#274366,#274367,#274368,
#274369,#274370,#274371,#274372,#274373,#274374,#274375,#274376,#274377,
#274378,#274379,#274380,#274381,#274382,#274383,#274384,#274385,#274386,
#274387,#274388,#274389,#274390,#274391,#274392,#274393,#274394,#274395,
#274396,#274397,#274398,#274399,#274400,#274401,#274402,#274403,#274404,
#274405,#274406,#274407,#274408,#274409,#274410,#274411,#274412,#274413,
#274414,#274415,#274416,#274417,#274418,#274419,#274420,#274421,#274422,
#274423,#274424,#274425,#274426,#274427),.UNSPECIFIED.,.F.,.F.,(4,3,3,3,
3,3,3,3,3,3,3,3,3,3,3,3,3,3,3,3,3,3,3,3,3,3,3,3,3,3,3,3,3,3,3,3,3,3,3,3,
3,3,3,3,3,3,3,3,3,3,3,3,3,3,3,3,3,3,3,3,3,3,3,4),(133.061082488801,133.166734977793,
133.27239290649,133.378316679529,133.484159022686,133.590220236502,133.696087998646,
133.801589464131,133.906931933533,134.012150389095,134.117302808356,134.22242530902,
134.327553964472,134.432794660568,134.538098303709,134.643584070438,134.693819998636,
134.799321464121,134.904663933523,135.009882389085,135.115034808346,135.22015730901,
135.325285964462,135.430526660558,135.535830303699,135.641316070428,135.691551998626,
135.797053464111,135.902395933513,136.007614389075,136.112766808336,136.217889308999,
136.323017964452,136.428258660547,136.533562303688,136.639048070417,136.689283998616,
136.794785464101,136.900127933503,137.005346389065,137.110498808326,137.215621308989,
137.320749964441,137.425990660537,137.531294303678,137.636780070407,137.687015998606,
137.792517464091,137.897859933493,138.003078389055,138.108230808316,138.213353308979,
138.318481964432,138.423722660527,138.529026303669,138.634512070397,138.684747998596,
138.790292825569,138.895681075761,139.000948945222,139.106136392543,139.211278460255,
139.316431600199,139.344267795981),.UNSPECIFIED.);
#3842=B_SPLINE_CURVE_WITH_KNOTS('',3,(#274429,#274430,#274431,#274432,#274433,
#274434,#274435,#274436,#274437,#274438),.UNSPECIFIED.,.F.,.F.,(4,1,1,1,
1,1,1,4),(139.344275098717,139.682479998586,140.680211998576,141.677943998566,
142.675675998556,143.673407998545,144.671139998535,145.627447736301),
 .UNSPECIFIED.);
#3843=B_SPLINE_CURVE_WITH_KNOTS('',3,(#274440,#274441,#274442,#274443,#274444,
#274445,#274446,#274447,#274448,#274449,#274450,#274451,#274452,#274453,
#274454,#274455,#274456,#274457,#274458,#274459,#274460,#274461,#274462,
#274463,#274464,#274465,#274466,#274467,#274468,#274469,#274470,#274471,
#274472,#274473,#274474,#274475,#274476,#274477,#274478,#274479,#274480,
#274481,#274482,#274483,#274484,#274485,#274486,#274487,#274488,#274489,
#274490,#274491,#274492,#274493,#274494,#274495,#274496,#274497,#274498,
#274499,#274500,#274501,#274502,#274503,#274504,#274505,#274506,#274507,
#274508,#274509,#274510,#274511,#274512,#274513,#274514,#274515,#274516,
#274517,#274518,#274519,#274520,#274521,#274522,#274523,#274524,#274525,
#274526,#274527,#274528,#274529,#274530,#274531,#274532,#274533,#274534,
#274535,#274536,#274537,#274538,#274539,#274540,#274541,#274542,#274543,
#274544,#274545,#274546,#274547,#274548,#274549,#274550,#274551,#274552,
#274553,#274554,#274555,#274556,#274557,#274558,#274559,#274560,#274561,
#274562,#274563,#274564,#274565,#274566,#274567,#274568,#274569,#274570,
#274571,#274572,#274573,#274574,#274575,#274576,#274577,#274578,#274579,
#274580,#274581,#274582,#274583,#274584,#274585,#274586,#274587,#274588,
#274589,#274590,#274591,#274592,#274593,#274594,#274595,#274596,#274597,
#274598,#274599,#274600,#274601,#274602,#274603,#274604,#274605,#274606,
#274607,#274608,#274609,#274610,#274611,#274612,#274613,#274614,#274615,
#274616,#274617,#274618,#274619,#274620,#274621,#274622,#274623,#274624,
#274625,#274626,#274627,#274628,#274629),.UNSPECIFIED.,.F.,.F.,(4,3,3,3,
3,3,3,3,3,3,3,3,3,3,3,3,3,3,3,3,3,3,3,3,3,3,3,3,3,3,3,3,3,3,3,3,3,3,3,3,
3,3,3,3,3,3,3,3,3,3,3,3,3,3,3,3,3,3,3,3,3,3,3,4),(145.62745310316,145.668871998525,
145.774373464006,145.879715933403,145.98493438896,146.090086808217,146.195209308876,
146.300337964323,146.405578660414,146.51088230355,146.616368070275,146.666603998515,
146.772105464016,146.877447933434,146.982666389013,147.08781880829,147.192941308969,
147.298069964437,147.403310660548,147.508614303705,147.614100070449,147.664335998505,
147.769837463974,147.875179933359,147.980398388905,148.085550808149,148.190673308797,
148.295801964233,148.401042660313,148.506346303439,148.611832070153,148.662067998495,
148.767569463956,148.872911933333,148.978130388871,149.083282808107,149.188405308746,
149.293533964173,149.398774660243,149.504078303359,149.609564070063,149.659799998485,
149.76530146408,149.870643933592,149.975862389264,150.081014808635,150.186137309408,
150.291265964969,150.396506661172,150.50181030442,150.607296071254,150.657531998475,
150.763033463821,150.868375933084,150.973594388508,151.078746807633,151.183869308161,
151.288997963479,151.394238659443,151.499542302455,151.605028069057,151.655263998465,
151.790594856147,151.910638270564),.UNSPECIFIED.);
#3844=B_SPLINE_CURVE_WITH_KNOTS('',3,(#274631,#274632,#274633,#274634,#274635,
#274636,#274637,#274638,#274639,#274640),.UNSPECIFIED.,.F.,.F.,(4,1,1,1,
1,1,1,4),(151.91063841034,152.652995998454,153.650727998444,154.648459998434,
155.646191998424,156.643923998414,157.641655998404,158.193823717519),
 .UNSPECIFIED.);
#3845=B_SPLINE_CURVE_WITH_KNOTS('',3,(#274642,#274643,#274644,#274645,#274646,
#274647,#274648,#274649,#274650,#274651),.UNSPECIFIED.,.F.,.F.,(4,1,1,1,
1,1,1,4),(158.193823717519,158.639387998394,159.637119998384,160.634851998374,
161.632583998364,162.630315998353,163.628047998343,164.477009024699),
 .UNSPECIFIED.);
#3846=B_SPLINE_CURVE_WITH_KNOTS('',3,(#274653,#274654,#274655,#274656,#274657,
#274658,#274659,#274660,#274661,#274662,#274663),.UNSPECIFIED.,.F.,.F.,
(4,1,1,1,1,1,1,1,4),(164.477009024699,164.625779998333,165.623511998323,
166.621243998313,167.618975998303,168.616707998293,169.614439998283,170.612171998273,
170.760194331878),.UNSPECIFIED.);
#3847=B_SPLINE_CURVE_WITH_KNOTS('',3,(#274668,#274669,#274670,#274671,#274672,
#274673,#274674,#274675,#274676,#274677,#274678,#274679,#274680,#274681,
#274682,#274683,#274684,#274685,#274686,#274687,#274688,#274689,#274690,
#274691,#274692,#274693,#274694,#274695,#274696,#274697,#274698,#274699,
#274700,#274701,#274702,#274703,#274704,#274705,#274706,#274707,#274708,
#274709,#274710,#274711,#274712,#274713,#274714,#274715,#274716,#274717,
#274718,#274719,#274720,#274721,#274722,#274723,#274724,#274725,#274726,
#274727,#274728,#274729,#274730,#274731,#274732,#274733,#274734,#274735,
#274736,#274737,#274738,#274739,#274740,#274741,#274742,#274743,#274744,
#274745,#274746,#274747,#274748,#274749,#274750,#274751,#274752,#274753,
#274754,#274755,#274756,#274757,#274758,#274759,#274760,#274761,#274762,
#274763,#274764,#274765,#274766,#274767,#274768,#274769,#274770,#274771,
#274772,#274773,#274774,#274775,#274776,#274777,#274778,#274779,#274780,
#274781,#274782,#274783,#274784,#274785,#274786,#274787,#274788,#274789,
#274790,#274791,#274792,#274793,#274794,#274795,#274796,#274797,#274798,
#274799,#274800,#274801,#274802,#274803,#274804,#274805,#274806,#274807,
#274808,#274809,#274810,#274811,#274812,#274813,#274814,#274815,#274816,
#274817,#274818,#274819,#274820,#274821,#274822,#274823,#274824,#274825,
#274826,#274827,#274828,#274829,#274830,#274831,#274832,#274833,#274834,
#274835,#274836),.UNSPECIFIED.,.F.,.F.,(4,3,3,3,3,3,3,3,3,3,3,3,3,3,3,3,
3,3,3,3,3,3,3,3,3,3,3,3,3,3,3,3,3,3,3,3,3,3,3,3,3,3,3,3,3,3,3,3,3,3,3,3,
3,3,3,3,4),(-173.021636066298,-172.91157443677,-172.801170755521,-172.690579717821,
-172.579669097854,-172.53875616362,-172.433085791181,-172.327574069382,
-172.222186749637,-172.116865811022,-172.011575408995,-171.906279743881,
-171.800874686078,-171.695407888946,-171.589762867262,-171.541422312964,
-171.435731408906,-171.330195372576,-171.224778225876,-171.119424047321,
-171.014097033089,-170.908761420676,-170.803311614756,-170.697797258801,
-170.592100821095,-170.544088462307,-170.43872635681,-170.333525260378,
-170.228450493165,-170.123443112452,-170.018466785104,-169.913485223641,
-169.808392138527,-169.703236548867,-169.59789827101,-169.54675461165,-169.441215904193,
-169.335835914169,-169.230579733942,-169.125389478107,-169.020229087856,
-168.915062548622,-168.809784359216,-168.704443317738,-168.598920998279,
-168.549420760993,-168.443892091303,-168.33852178728,-168.233274719997,
-168.128093214986,-168.022941198748,-167.917782641628,-167.81251178253,
-167.707177709489,-167.601661723545,-167.552086910337,-167.455359735508),
 .UNSPECIFIED.);
#3848=B_SPLINE_CURVE_WITH_KNOTS('',3,(#274838,#274839,#274840,#274841,#274842,
#274843,#274844,#274845,#274846,#274847),.UNSPECIFIED.,.F.,.F.,(4,1,1,1,
1,1,1,4),(-167.455350961157,-166.55475305968,-165.557419209023,-164.560085358366,
-163.562751507709,-162.565417657053,-161.568083806396,-161.172174428328),
 .UNSPECIFIED.);
#3849=B_SPLINE_CURVE_WITH_KNOTS('',3,(#274849,#274850,#274851,#274852,#274853,
#274854,#274855,#274856,#274857,#274858),.UNSPECIFIED.,.F.,.F.,(4,1,1,1,
1,1,1,4),(-161.172174428328,-160.570749955739,-159.573416105082,-158.576082254426,
-157.578748403769,-156.581414553112,-155.584080702455,-154.888989121148),
 .UNSPECIFIED.);
#3850=B_SPLINE_CURVE_WITH_KNOTS('',3,(#274860,#274861,#274862,#274863,#274864,
#274865,#274866,#274867,#274868,#274869,#274870,#274871,#274872,#274873,
#274874,#274875,#274876,#274877,#274878,#274879,#274880,#274881,#274882,
#274883,#274884,#274885,#274886,#274887,#274888,#274889,#274890,#274891,
#274892,#274893,#274894,#274895,#274896,#274897,#274898,#274899,#274900,
#274901,#274902,#274903,#274904,#274905,#274906,#274907,#274908,#274909,
#274910,#274911,#274912,#274913,#274914,#274915,#274916,#274917,#274918,
#274919,#274920,#274921,#274922,#274923,#274924,#274925,#274926,#274927,
#274928,#274929,#274930,#274931,#274932,#274933,#274934,#274935,#274936,
#274937,#274938,#274939,#274940,#274941,#274942,#274943,#274944,#274945,
#274946,#274947,#274948,#274949,#274950,#274951,#274952,#274953,#274954,
#274955,#274956,#274957,#274958,#274959,#274960,#274961,#274962,#274963,
#274964,#274965,#274966,#274967,#274968,#274969,#274970,#274971,#274972,
#274973,#274974,#274975,#274976,#274977,#274978,#274979,#274980,#274981,
#274982,#274983,#274984,#274985,#274986,#274987,#274988,#274989,#274990,
#274991,#274992,#274993,#274994,#274995,#274996,#274997,#274998,#274999,
#275000,#275001,#275002,#275003,#275004,#275005,#275006,#275007,#275008,
#275009,#275010,#275011,#275012,#275013,#275014,#275015,#275016,#275017,
#275018,#275019,#275020,#275021,#275022,#275023,#275024,#275025,#275026,
#275027,#275028,#275029,#275030,#275031,#275032,#275033,#275034,#275035,
#275036,#275037,#275038,#275039,#275040,#275041,#275042,#275043,#275044,
#275045,#275046,#275047,#275048,#275049),.UNSPECIFIED.,.F.,.F.,(4,3,3,3,
3,3,3,3,3,3,3,3,3,3,3,3,3,3,3,3,3,3,3,3,3,3,3,3,3,3,3,3,3,3,3,3,3,3,3,3,
3,3,3,3,3,3,3,3,3,3,3,3,3,3,3,3,3,3,3,3,3,3,3,4),(-154.888988936303,-154.762828432452,
-154.634933804719,-154.586746851799,-154.481240045005,-154.375892113708,
-154.270668064878,-154.165509965993,-154.060381708233,-153.955247227016,
-153.850000760823,-153.744691297408,-153.63919999852,-153.589413001142,
-153.48390619939,-153.378558273193,-153.273334229522,-153.168176135829,
-153.063047883287,-152.957913407306,-152.85266694634,-152.747357488154,
-152.641866194445,-152.592079150485,-152.486572349276,-152.381224423647,
-152.276000380581,-152.170842287513,-152.065714035617,-151.960579560302,
-151.855333100027,-151.750023642549,-151.644532349564,-151.594745299828,
-151.489238496917,-151.383890569556,-151.27866652472,-151.173508429862,
-151.068380176156,-150.963245699015,-150.857999236903,-150.752689777577,
-150.647198482749,-150.597411449172,-150.491904647082,-150.386556720551,
-150.281332676557,-150.176174582548,-150.071046329696,-149.965911853412,
-149.860665392157,-149.755355933689,-149.649864639712,-149.600077598515,
-149.494628879985,-149.389338992167,-149.284172777986,-149.179072286532,
-149.074001319397,-148.968923722142,-148.863734045917,-148.758480836203,
-148.653046701498,-148.605803814421),.UNSPECIFIED.);
#3851=B_SPLINE_CURVE_WITH_KNOTS('',3,(#275051,#275052,#275053,#275054,#275055,
#275056,#275057,#275058,#275059,#275060,#275061,#275062,#275063,#275064,
#275065,#275066,#275067,#275068,#275069,#275070,#275071,#275072,#275073,
#275074,#275075,#275076,#275077,#275078,#275079,#275080,#275081,#275082,
#275083,#275084,#275085,#275086,#275087,#275088,#275089,#275090,#275091,
#275092,#275093,#275094,#275095,#275096,#275097,#275098,#275099,#275100,
#275101,#275102,#275103,#275104,#275105,#275106,#275107,#275108,#275109,
#275110,#275111,#275112,#275113,#275114,#275115,#275116,#275117,#275118,
#275119,#275120,#275121,#275122,#275123,#275124,#275125,#275126,#275127,
#275128,#275129,#275130,#275131,#275132,#275133,#275134,#275135,#275136,
#275137,#275138,#275139,#275140,#275141,#275142,#275143,#275144,#275145,
#275146,#275147,#275148,#275149,#275150,#275151,#275152,#275153,#275154,
#275155,#275156,#275157,#275158,#275159,#275160,#275161,#275162,#275163,
#275164,#275165,#275166,#275167,#275168,#275169,#275170,#275171,#275172,
#275173,#275174,#275175,#275176,#275177,#275178,#275179,#275180,#275181,
#275182,#275183,#275184,#275185,#275186,#275187,#275188,#275189,#275190,
#275191,#275192,#275193,#275194,#275195,#275196,#275197,#275198,#275199,
#275200,#275201,#275202,#275203,#275204,#275205,#275206,#275207,#275208,
#275209,#275210,#275211,#275212,#275213,#275214,#275215,#275216,#275217,
#275218,#275219,#275220,#275221,#275222,#275223,#275224,#275225,#275226,
#275227,#275228,#275229,#275230,#275231,#275232,#275233,#275234,#275235,
#275236,#275237,#275238,#275239,#275240,#275241,#275242,#275243),
 .UNSPECIFIED.,.F.,.F.,(4,3,3,3,3,3,3,3,3,3,3,3,3,3,3,3,3,3,3,3,3,3,3,3,
3,3,3,3,3,3,3,3,3,3,3,3,3,3,3,3,3,3,3,3,3,3,3,3,3,3,3,3,3,3,3,3,3,3,3,3,
3,3,3,3,4),(-148.605803813969,-148.602743747858,-148.497236945542,-148.391889018784,
-148.286664974561,-148.181506880321,-148.076378627239,-147.971244150725,
-147.865997689241,-147.760688230545,-147.655196936343,-147.605409897201,
-147.499903095014,-147.394555168387,-147.289331124297,-147.184173030192,
-147.079044777245,-146.973910300866,-146.868663839518,-146.763354380959,
-146.657863086891,-146.608076046544,-146.502569244347,-146.397221317709,
-146.29199727361,-146.186839179494,-146.081710926538,-145.97657645015,-145.871329988793,
-145.766020530225,-145.66052923615,-145.610742195888,-145.505235393661,
-145.399887466993,-145.294663422862,-145.189505328716,-145.084377075727,
-144.979242599307,-144.873996137918,-144.768686679317,-144.663195385209,
-144.613408345231,-144.507901543024,-144.402553616376,-144.297329572265,
-144.192171478139,-144.087043225171,-143.981908748772,-143.876662287403,
-143.771352828823,-143.665861534735,-143.616074494574,-143.510567692364,
-143.405219765713,-143.299995721599,-143.19483762747,-143.089709374499,
-142.984574898097,-142.879328436725,-142.774018978142,-142.668527684052,
-142.618740643917,-142.489762712696,-142.362605638187,-142.322618679647),
 .UNSPECIFIED.);
#3852=B_SPLINE_CURVE_WITH_KNOTS('',3,(#275245,#275246,#275247,#275248,#275249,
#275250,#275251,#275252,#275253,#275254),.UNSPECIFIED.,.F.,.F.,(4,1,1,1,
1,1,1,4),(-142.322618506789,-141.621406793261,-140.624072942604,-139.626739091947,
-138.62940524129,-137.632071390634,-136.634737539977,-136.03943319961),
 .UNSPECIFIED.);
#3853=B_SPLINE_CURVE_WITH_KNOTS('',3,(#275256,#275257,#275258,#275259,#275260,
#275261,#275262,#275263,#275264,#275265,#275266,#275267,#275268,#275269,
#275270,#275271,#275272,#275273,#275274,#275275,#275276,#275277,#275278,
#275279,#275280,#275281,#275282,#275283,#275284,#275285,#275286,#275287,
#275288,#275289,#275290,#275291,#275292,#275293,#275294,#275295,#275296,
#275297,#275298,#275299,#275300,#275301,#275302,#275303,#275304,#275305,
#275306,#275307,#275308,#275309,#275310,#275311,#275312,#275313,#275314,
#275315,#275316,#275317,#275318,#275319,#275320,#275321,#275322,#275323,
#275324,#275325,#275326,#275327,#275328,#275329,#275330,#275331,#275332,
#275333,#275334,#275335,#275336,#275337,#275338,#275339,#275340,#275341,
#275342,#275343,#275344,#275345,#275346,#275347,#275348,#275349,#275350,
#275351,#275352,#275353,#275354,#275355,#275356,#275357,#275358,#275359,
#275360,#275361,#275362,#275363,#275364,#275365,#275366,#275367,#275368,
#275369,#275370,#275371,#275372,#275373,#275374,#275375,#275376,#275377,
#275378,#275379,#275380,#275381,#275382,#275383,#275384,#275385,#275386,
#275387,#275388,#275389,#275390,#275391,#275392,#275393,#275394,#275395,
#275396,#275397,#275398,#275399,#275400,#275401,#275402,#275403,#275404,
#275405,#275406,#275407,#275408,#275409,#275410,#275411,#275412,#275413,
#275414,#275415,#275416,#275417,#275418,#275419,#275420,#275421,#275422,
#275423,#275424,#275425,#275426,#275427,#275428,#275429,#275430,#275431,
#275432,#275433,#275434,#275435,#275436,#275437,#275438,#275439,#275440,
#275441,#275442,#275443,#275444,#275445),.UNSPECIFIED.,.F.,.F.,(4,3,3,3,
3,3,3,3,3,3,3,3,3,3,3,3,3,3,3,3,3,3,3,3,3,3,3,3,3,3,3,3,3,3,3,3,3,3,3,3,
3,3,3,3,3,3,3,3,3,3,3,3,3,3,3,3,3,3,3,3,3,3,3,4),(-136.039432767475,-135.923411947058,
-135.806976229731,-135.689983518335,-135.63740368932,-135.531896887108,
-135.426548960456,-135.321324916341,-135.21616682221,-135.111038569238,
-135.005904092834,-134.900657631461,-134.795348172876,-134.689856878784,
-134.640069838663,-134.534563036451,-134.429215109799,-134.323991065684,
-134.218832971554,-134.113704718582,-134.008570242178,-133.903323780805,
-133.798014322221,-133.692523028129,-133.642735988007,-133.537229185795,
-133.431881259143,-133.326657215027,-133.221499120897,-133.116370867924,
-133.01123639152,-132.905989930147,-132.800680471562,-132.69518917747,-132.64540213735,
-132.539895335138,-132.434547408486,-132.32932336437,-132.224165270239,
-132.119037017267,-132.013902540862,-131.908656079489,-131.803346620904,
-131.697855326812,-131.648068286693,-131.542561484481,-131.437213557829,
-131.331989513713,-131.226831419583,-131.12170316661,-131.016568690206,
-130.911322228833,-130.806012770248,-130.700521476156,-130.650734436036,
-130.546565876061,-130.44257619085,-130.338685988997,-130.234857369735,
-130.131052521105,-130.027172036681,-129.923251693136,-129.819169881673,
-129.756247892881),.UNSPECIFIED.);
#3854=B_SPLINE_CURVE_WITH_KNOTS('',3,(#275447,#275448,#275449,#275450,#275451,
#275452,#275453,#275454,#275455,#275456,#275457,#275458,#275459,#275460,
#275461,#275462,#275463,#275464,#275465,#275466,#275467,#275468,#275469,
#275470,#275471,#275472,#275473,#275474,#275475,#275476,#275477,#275478,
#275479,#275480,#275481,#275482,#275483,#275484,#275485,#275486,#275487,
#275488,#275489,#275490,#275491,#275492,#275493,#275494,#275495,#275496,
#275497,#275498,#275499,#275500,#275501,#275502,#275503,#275504,#275505,
#275506,#275507,#275508,#275509,#275510,#275511,#275512,#275513,#275514,
#275515,#275516,#275517,#275518,#275519,#275520,#275521,#275522,#275523,
#275524,#275525,#275526,#275527,#275528,#275529,#275530,#275531,#275532,
#275533,#275534,#275535,#275536,#275537,#275538,#275539,#275540,#275541,
#275542,#275543,#275544,#275545,#275546,#275547,#275548,#275549,#275550,
#275551,#275552,#275553,#275554,#275555,#275556,#275557,#275558,#275559,
#275560,#275561,#275562,#275563,#275564,#275565,#275566,#275567,#275568,
#275569,#275570,#275571,#275572,#275573,#275574,#275575,#275576,#275577,
#275578,#275579,#275580,#275581,#275582,#275583,#275584,#275585,#275586,
#275587,#275588,#275589,#275590,#275591,#275592,#275593,#275594,#275595,
#275596,#275597,#275598,#275599,#275600,#275601,#275602,#275603,#275604,
#275605,#275606,#275607,#275608,#275609,#275610,#275611,#275612,#275613,
#275614,#275615,#275616,#275617,#275618,#275619,#275620,#275621,#275622,
#275623,#275624,#275625,#275626,#275627,#275628,#275629,#275630,#275631,
#275632,#275633,#275634,#275635,#275636),.UNSPECIFIED.,.F.,.F.,(4,3,3,3,
3,3,3,3,3,3,3,3,3,3,3,3,3,3,3,3,3,3,3,3,3,3,3,3,3,3,3,3,3,3,3,3,3,3,3,3,
3,3,3,3,3,3,3,3,3,3,3,3,3,3,3,3,3,3,3,3,3,3,3,4),(-129.75624789243,-129.65340058538,
-129.547893783166,-129.442545856511,-129.337321812392,-129.232163718259,
-129.127035465284,-129.021900988877,-128.9166545275,-128.811345068913,-128.705853774818,
-128.656066734723,-128.550559932512,-128.44521200586,-128.339987961745,
-128.234829867614,-128.129701614642,-128.024567138239,-127.919320676866,
-127.814011218282,-127.70851992419,-127.658732884066,-127.553226081855,
-127.447878155202,-127.342654111087,-127.237496016957,-127.132367763985,
-127.027233287581,-126.921986826208,-126.816677367624,-126.711186073532,
-126.661399033409,-126.555892231197,-126.450544304544,-126.345320260428,
-126.240162166297,-126.135033913324,-126.02989943692,-125.924652975546,
-125.819343516961,-125.713852222868,-125.664065182752,-125.558558380541,
-125.453210453889,-125.347986409774,-125.242828315643,-125.137700062671,
-125.032565586267,-124.927319124894,-124.82200966631,-124.716518372218,
-124.666731332096,-124.561224529884,-124.455876603232,-124.350652559116,
-124.245494464986,-124.140366212013,-124.035231735609,-123.929985274236,
-123.824675815651,-123.719184521559,-123.669397481439,-123.517141233146,
-123.473062585251),.UNSPECIFIED.);
#3855=B_SPLINE_CURVE_WITH_KNOTS('',3,(#275638,#275639,#275640,#275641,#275642,
#275643,#275644,#275645,#275646,#275647),.UNSPECIFIED.,.F.,.F.,(4,1,1,1,
1,1,1,4),(-123.473059165501,-122.672063630782,-121.674729780125,-120.677395929469,
-119.680062078812,-118.682728228155,-117.685394377498,-117.189877278071),
 .UNSPECIFIED.);
#3856=B_SPLINE_CURVE_WITH_KNOTS('',3,(#275649,#275650,#275651,#275652,#275653,
#275654,#275655,#275656,#275657,#275658),.UNSPECIFIED.,.F.,.F.,(4,1,1,1,
1,1,1,4),(-117.189877278071,-116.688060526842,-115.690726676185,-114.693392825528,
-113.696058974871,-112.698725124214,-111.701391273558,-110.906694804064),
 .UNSPECIFIED.);
#3857=B_SPLINE_CURVE_WITH_KNOTS('',3,(#275660,#275661,#275662,#275663,#275664,
#275665,#275666,#275667,#275668,#275669,#275670,#275671,#275672,#275673,
#275674,#275675,#275676,#275677,#275678,#275679,#275680,#275681,#275682,
#275683,#275684,#275685,#275686,#275687,#275688,#275689,#275690,#275691,
#275692,#275693,#275694,#275695,#275696,#275697,#275698,#275699,#275700,
#275701,#275702,#275703,#275704,#275705,#275706,#275707,#275708,#275709,
#275710,#275711,#275712,#275713,#275714,#275715,#275716,#275717,#275718,
#275719,#275720,#275721,#275722,#275723,#275724,#275725,#275726,#275727,
#275728,#275729,#275730,#275731,#275732,#275733,#275734,#275735,#275736,
#275737,#275738,#275739,#275740,#275741,#275742,#275743,#275744,#275745,
#275746,#275747,#275748,#275749,#275750,#275751,#275752,#275753,#275754,
#275755,#275756,#275757,#275758,#275759,#275760,#275761,#275762,#275763,
#275764,#275765,#275766,#275767,#275768,#275769,#275770,#275771,#275772,
#275773,#275774,#275775,#275776,#275777,#275778,#275779,#275780,#275781,
#275782,#275783,#275784,#275785,#275786,#275787,#275788,#275789,#275790,
#275791,#275792,#275793,#275794,#275795,#275796,#275797,#275798,#275799,
#275800,#275801,#275802,#275803,#275804,#275805,#275806,#275807,#275808,
#275809,#275810,#275811,#275812,#275813,#275814,#275815,#275816,#275817,
#275818,#275819,#275820,#275821,#275822,#275823,#275824,#275825,#275826,
#275827,#275828,#275829,#275830,#275831,#275832,#275833,#275834,#275835,
#275836,#275837,#275838,#275839,#275840,#275841,#275842,#275843,#275844,
#275845,#275846,#275847,#275848,#275849),.UNSPECIFIED.,.F.,.F.,(4,3,3,3,
3,3,3,3,3,3,3,3,3,3,3,3,3,3,3,3,3,3,3,3,3,3,3,3,3,3,3,3,3,3,3,3,3,3,3,3,
3,3,3,3,3,3,3,3,3,3,3,3,3,3,3,3,3,3,3,3,3,3,3,4),(-110.906691970891,-110.756832769008,
-110.704057422901,-110.598550620688,-110.493202694035,-110.387978649919,
-110.282820555787,-110.177692302814,-110.072557826409,-109.967311365035,
-109.86200190645,-109.756510612357,-109.706723572244,-109.601216770032,
-109.49586884338,-109.390644799264,-109.285486705133,-109.180358452161,
-109.075223975757,-108.969977514384,-108.864668055799,-108.759176761707,
-108.709389721587,-108.603882919376,-108.498534992724,-108.393310948609,
-108.288152854478,-108.183024601506,-108.077890125102,-107.972643663729,
-107.867334205145,-107.761842911054,-107.712055870931,-107.606549068719,
-107.501201142067,-107.395977097951,-107.29081900382,-107.185690750848,
-107.080556274444,-106.97530981307,-106.870000354486,-106.764509060394,
-106.714722020274,-106.609215218062,-106.503867291409,-106.398643247294,
-106.293485153163,-106.18835690019,-106.083222423786,-105.977975962413,
-105.872666503828,-105.767175209736,-105.717388169617,-105.611881367405,
-105.506533440753,-105.401309396637,-105.296151302506,-105.191023049534,
-105.08588857313,-104.980642111756,-104.875332653172,-104.76984135908,-104.72005431896,
-104.623506663712),.UNSPECIFIED.);
#3858=B_SPLINE_CURVE_WITH_KNOTS('',3,(#275851,#275852,#275853,#275854,#275855,
#275856,#275857,#275858,#275859,#275860),.UNSPECIFIED.,.F.,.F.,(4,1,1,1,
1,1,1,4),(-104.623497903185,-103.722720468304,-102.725386617647,-101.72805276699,
-100.730718916333,-99.7333850656765,-98.7360512150198,-98.3403213565322),
 .UNSPECIFIED.);
#3859=B_SPLINE_CURVE_WITH_KNOTS('',3,(#275862,#275863,#275864,#275865,#275866,
#275867,#275868,#275869,#275870,#275871),.UNSPECIFIED.,.F.,.F.,(4,1,1,1,
1,1,1,4),(-98.3403213565322,-97.738717364363,-96.7413835137062,-95.7440496630495,
-94.7467158123927,-93.7493819617359,-92.7520481110792,-92.0571360493526),
 .UNSPECIFIED.);
#3860=B_SPLINE_CURVE_WITH_KNOTS('',3,(#275873,#275874,#275875,#275876,#275877,
#275878,#275879,#275880,#275881,#275882,#275883,#275884,#275885,#275886,
#275887,#275888,#275889,#275890,#275891,#275892,#275893,#275894,#275895,
#275896,#275897,#275898,#275899,#275900,#275901,#275902,#275903,#275904,
#275905,#275906,#275907,#275908,#275909,#275910,#275911,#275912,#275913,
#275914,#275915,#275916,#275917,#275918,#275919,#275920,#275921,#275922,
#275923,#275924,#275925,#275926,#275927,#275928,#275929,#275930,#275931,
#275932,#275933,#275934,#275935,#275936,#275937,#275938,#275939,#275940,
#275941,#275942,#275943,#275944,#275945,#275946,#275947,#275948,#275949,
#275950,#275951,#275952,#275953,#275954,#275955,#275956,#275957,#275958,
#275959,#275960,#275961,#275962,#275963,#275964,#275965,#275966,#275967,
#275968,#275969,#275970,#275971,#275972,#275973,#275974,#275975,#275976,
#275977,#275978,#275979,#275980,#275981,#275982,#275983,#275984,#275985,
#275986,#275987,#275988,#275989,#275990,#275991,#275992,#275993,#275994,
#275995,#275996,#275997,#275998,#275999,#276000,#276001,#276002,#276003,
#276004,#276005,#276006,#276007,#276008,#276009,#276010,#276011,#276012,
#276013,#276014,#276015,#276016,#276017,#276018,#276019,#276020,#276021,
#276022,#276023,#276024,#276025,#276026,#276027,#276028,#276029,#276030,
#276031,#276032,#276033,#276034,#276035,#276036,#276037,#276038,#276039,
#276040,#276041,#276042,#276043,#276044,#276045,#276046,#276047,#276048,
#276049,#276050,#276051,#276052,#276053,#276054,#276055,#276056,#276057,
#276058,#276059,#276060,#276061,#276062),.UNSPECIFIED.,.F.,.F.,(4,3,3,3,
3,3,3,3,3,3,3,3,3,3,3,3,3,3,3,3,3,3,3,3,3,3,3,3,3,3,3,3,3,3,3,3,3,3,3,3,
3,3,3,3,3,3,3,3,3,3,3,3,3,3,3,3,3,3,3,3,3,3,3,4),(-92.0571358641713,-91.930999755056,
-91.8031327507075,-91.7547142604224,-91.6492074582106,-91.5438595315583,
-91.4386354874429,-91.333477393312,-91.2283491403396,-91.1232146639356,
-91.0179682025622,-90.9126587439777,-90.8071674498857,-90.7573804097656,
-90.6518736075538,-90.5465256809014,-90.4413016367861,-90.3361435426553,
-90.231015289683,-90.1258808132789,-90.0206343519056,-89.9153248933212,
-89.8098335992292,-89.7600465591089,-89.6545397568971,-89.5491918302447,
-89.4439677861294,-89.3388096919985,-89.2336814390262,-89.1285469626221,
-89.0233005012487,-88.9179910426643,-88.8124997485723,-88.7627127084521,
-88.6572059062403,-88.5518579795879,-88.4466339354725,-88.3414758413416,
-88.2363475883693,-88.1312131119652,-88.0259666505918,-87.9206571920073,
-87.8151658979152,-87.7653788577953,-87.6598720555835,-87.5545241289311,
-87.4493000848158,-87.344141990685,-87.2390137377127,-87.1338792613086,
-87.0286327999352,-86.9233233413509,-86.8178320472589,-86.7680450071386,
-86.6625996592658,-86.5573131394121,-86.4521502811752,-86.3470531325385,
-86.2419854899419,-86.136911193783,-86.0317248142074,-85.9264748702226,
-85.8210440559206,-85.7739507426472),.UNSPECIFIED.);
#3861=B_SPLINE_CURVE_WITH_KNOTS('',3,(#276064,#276065,#276066,#276067,#276068,
#276069,#276070,#276071,#276072,#276073,#276074,#276075,#276076,#276077,
#276078,#276079,#276080,#276081,#276082,#276083,#276084,#276085,#276086,
#276087,#276088,#276089,#276090,#276091,#276092,#276093,#276094,#276095,
#276096,#276097,#276098,#276099,#276100,#276101,#276102,#276103,#276104,
#276105,#276106,#276107,#276108,#276109,#276110,#276111,#276112,#276113,
#276114,#276115,#276116,#276117,#276118,#276119,#276120,#276121,#276122,
#276123,#276124,#276125,#276126,#276127,#276128,#276129,#276130,#276131,
#276132,#276133,#276134,#276135,#276136,#276137,#276138,#276139,#276140,
#276141,#276142,#276143,#276144,#276145,#276146,#276147,#276148,#276149,
#276150,#276151,#276152,#276153,#276154,#276155,#276156,#276157,#276158,
#276159,#276160,#276161,#276162,#276163,#276164,#276165,#276166,#276167,
#276168,#276169,#276170,#276171,#276172,#276173,#276174,#276175,#276176,
#276177,#276178,#276179,#276180,#276181,#276182,#276183,#276184,#276185,
#276186,#276187,#276188,#276189,#276190,#276191,#276192,#276193,#276194,
#276195,#276196,#276197,#276198,#276199,#276200,#276201,#276202,#276203,
#276204,#276205,#276206,#276207,#276208,#276209,#276210,#276211,#276212,
#276213,#276214,#276215,#276216,#276217,#276218,#276219,#276220,#276221,
#276222,#276223,#276224,#276225,#276226,#276227,#276228,#276229,#276230,
#276231,#276232,#276233,#276234,#276235,#276236,#276237,#276238,#276239,
#276240,#276241,#276242,#276243,#276244,#276245,#276246,#276247,#276248,
#276249,#276250,#276251,#276252,#276253,#276254,#276255,#276256),
 .UNSPECIFIED.,.F.,.F.,(4,3,3,3,3,3,3,3,3,3,3,3,3,3,3,3,3,3,3,3,3,3,3,3,
3,3,3,3,3,3,3,3,3,3,3,3,3,3,3,3,3,3,3,3,3,3,3,3,3,3,3,3,3,3,3,3,3,3,3,3,
3,3,3,3,4),(-85.773950742173,-85.7707111564818,-85.6652043542701,-85.5598564276176,
-85.4546323835023,-85.3494742893715,-85.2443460363991,-85.139211559995,
-85.0339650986217,-84.9286556400373,-84.8231643459452,-84.7733773058251,
-84.6678705036133,-84.5625225769609,-84.4572985328455,-84.3521404387147,
-84.2470121857423,-84.1418777093383,-84.0366312479649,-83.9313217893805,
-83.8258304952885,-83.7760434551683,-83.6705366529565,-83.5651887263041,
-83.4599646821888,-83.3548065880579,-83.2496783350855,-83.1445438586814,
-83.039297397308,-82.9339879387236,-82.8284966446315,-82.7787096045115,
-82.6732028022997,-82.5678548756473,-82.462630831532,-82.3574727374011,
-82.2523444844288,-82.1472100080247,-82.0419635466513,-81.9366540880669,
-81.8311627939748,-81.7813757538547,-81.6758689516429,-81.5705210249905,
-81.4652969808752,-81.3601388867444,-81.2550106337721,-81.149876157368,
-81.0446296959946,-80.9393202374102,-80.8338289433182,-80.784041903198,
-80.6785351009862,-80.5731871743338,-80.4679631302184,-80.3628050360876,
-80.2576767831152,-80.1525423067111,-80.0472958453377,-79.9419863867533,
-79.8364950926612,-79.7867080525412,-79.657701481349,-79.5305194816838,
-79.4907656074844),.UNSPECIFIED.);
#3862=B_SPLINE_CURVE_WITH_KNOTS('',3,(#276258,#276259,#276260,#276261,#276262,
#276263,#276264,#276265,#276266,#276267),.UNSPECIFIED.,.F.,.F.,(4,1,1,1,
1,1,1,4),(-79.4907654349934,-78.7893742018845,-77.7920403512277,-76.7947065005709,
-75.7973726499142,-74.8000387992574,-73.8027049486006,-73.2075801278138),
 .UNSPECIFIED.);
#3863=B_SPLINE_CURVE_WITH_KNOTS('',3,(#276269,#276270,#276271,#276272,#276273,
#276274,#276275,#276276,#276277,#276278,#276279,#276280,#276281,#276282,
#276283,#276284,#276285,#276286,#276287,#276288,#276289,#276290,#276291,
#276292,#276293,#276294,#276295,#276296,#276297,#276298,#276299,#276300,
#276301,#276302,#276303,#276304,#276305,#276306,#276307,#276308,#276309,
#276310,#276311,#276312,#276313,#276314,#276315,#276316,#276317,#276318,
#276319,#276320,#276321,#276322,#276323,#276324,#276325,#276326,#276327,
#276328,#276329,#276330,#276331,#276332,#276333,#276334,#276335,#276336,
#276337,#276338,#276339,#276340,#276341,#276342,#276343,#276344,#276345,
#276346,#276347,#276348,#276349,#276350,#276351,#276352,#276353,#276354,
#276355,#276356,#276357,#276358,#276359,#276360,#276361,#276362,#276363,
#276364,#276365,#276366,#276367,#276368,#276369,#276370,#276371,#276372,
#276373,#276374,#276375,#276376,#276377,#276378,#276379,#276380,#276381,
#276382,#276383,#276384,#276385,#276386,#276387,#276388,#276389,#276390,
#276391,#276392,#276393,#276394,#276395,#276396,#276397,#276398,#276399,
#276400,#276401,#276402,#276403,#276404,#276405,#276406,#276407,#276408,
#276409,#276410,#276411,#276412,#276413,#276414,#276415,#276416,#276417,
#276418,#276419,#276420,#276421,#276422,#276423,#276424,#276425,#276426,
#276427,#276428,#276429,#276430,#276431,#276432,#276433,#276434,#276435,
#276436,#276437,#276438,#276439,#276440,#276441,#276442,#276443,#276444,
#276445,#276446,#276447,#276448,#276449,#276450,#276451,#276452,#276453,
#276454,#276455,#276456,#276457,#276458),.UNSPECIFIED.,.F.,.F.,(4,3,3,3,
3,3,3,3,3,3,3,3,3,3,3,3,3,3,3,3,3,3,3,3,3,3,3,3,3,3,3,3,3,3,3,3,3,3,3,3,
3,3,3,3,3,3,3,3,3,3,3,3,3,3,3,3,3,3,3,3,3,3,3,4),(-73.2075796961327,-73.0915724254084,
-72.975151035254,-72.8581731739681,-72.8053710979439,-72.6998642957321,
-72.5945163690796,-72.4892923249642,-72.3841342308334,-72.279005977861,
-72.1738715014568,-72.0686250400834,-71.9633155814988,-71.8578242874068,
-71.8080372472871,-71.7025304450754,-71.5971825184229,-71.4919584743076,
-71.3868003801767,-71.2816721272044,-71.1765376508003,-71.0712911894269,
-70.9659817308425,-70.8604904367505,-70.8107033966303,-70.7051965944186,
-70.5998486677662,-70.4946246236509,-70.3894665295201,-70.2843382765477,
-70.1792038001437,-70.0739573387704,-69.968647880186,-69.863156586094,-69.8133695459736,
-69.7078627437618,-69.6025148171094,-69.4972907729941,-69.3921326788632,
-69.2870044258909,-69.1818699494868,-69.0766234881134,-68.971314029529,
-68.8658227354369,-68.8160356953168,-68.710528893105,-68.6051809664526,
-68.4999569223372,-68.3947988282064,-68.289670575234,-68.1845360988299,
-68.0792896374565,-67.973980178872,-67.8684888847799,-67.81870184466,-67.7145345612462,
-67.6105461545448,-67.5066572304383,-67.4028298868347,-67.2990263104663,
-67.195147136985,-67.091228097057,-66.9871477021693,-66.9243948210848),
 .UNSPECIFIED.);
#3864=B_SPLINE_CURVE_WITH_KNOTS('',3,(#276460,#276461,#276462,#276463,#276464,
#276465,#276466,#276467,#276468,#276469,#276470,#276471,#276472,#276473,
#276474,#276475,#276476,#276477,#276478,#276479,#276480,#276481,#276482,
#276483,#276484,#276485,#276486,#276487,#276488,#276489,#276490,#276491,
#276492,#276493,#276494,#276495,#276496,#276497,#276498,#276499,#276500,
#276501,#276502,#276503,#276504,#276505,#276506,#276507,#276508,#276509,
#276510,#276511,#276512,#276513,#276514,#276515,#276516,#276517,#276518,
#276519,#276520,#276521,#276522,#276523,#276524,#276525,#276526,#276527,
#276528,#276529,#276530,#276531,#276532,#276533,#276534,#276535,#276536,
#276537,#276538,#276539,#276540,#276541,#276542,#276543,#276544,#276545,
#276546,#276547,#276548,#276549,#276550,#276551,#276552,#276553,#276554,
#276555,#276556,#276557,#276558,#276559,#276560,#276561,#276562,#276563,
#276564,#276565,#276566,#276567,#276568,#276569,#276570,#276571,#276572,
#276573,#276574,#276575,#276576,#276577,#276578,#276579,#276580,#276581,
#276582,#276583,#276584,#276585,#276586,#276587,#276588,#276589,#276590,
#276591,#276592,#276593,#276594,#276595,#276596,#276597,#276598,#276599,
#276600,#276601,#276602,#276603,#276604,#276605,#276606,#276607,#276608,
#276609,#276610,#276611,#276612,#276613,#276614,#276615,#276616,#276617,
#276618,#276619,#276620,#276621,#276622,#276623,#276624,#276625,#276626,
#276627,#276628,#276629,#276630,#276631,#276632,#276633,#276634,#276635,
#276636,#276637,#276638,#276639,#276640,#276641,#276642,#276643,#276644,
#276645,#276646,#276647,#276648,#276649),.UNSPECIFIED.,.F.,.F.,(4,3,3,3,
3,3,3,3,3,3,3,3,3,3,3,3,3,3,3,3,3,3,3,3,3,3,3,3,3,3,3,3,3,3,3,3,3,3,3,3,
3,3,3,3,3,3,3,3,3,3,3,3,3,3,3,3,3,3,3,3,3,3,3,4),(-66.9243948206342,-66.8213679940033,
-66.7158611917913,-66.6105132651389,-66.5052892210233,-66.4001311268923,
-66.2950028739198,-66.1898683975154,-66.0846219361418,-65.9793124775572,
-65.873821183465,-65.8240341433465,-65.7185273411348,-65.6131794144823,
-65.507955370367,-65.4027972762362,-65.2976690232639,-65.1925345468598,
-65.0872880854865,-64.9819786269021,-64.8764873328101,-64.8267002926897,
-64.721193490478,-64.6158455638255,-64.5106215197102,-64.4054634255794,
-64.3003351726071,-64.1952006962031,-64.0899542348298,-63.9846447762454,
-63.8791534821534,-63.829366442033,-63.7238596398212,-63.6185117131688,
-63.5132876690534,-63.4081295749225,-63.3030013219502,-63.1978668455461,
-63.0926203841727,-62.9873109255882,-62.8818196314961,-62.8320325913762,
-62.7265257891644,-62.6211778625121,-62.5159538183968,-62.410795724266,
-62.3056674712936,-62.2005329948896,-62.0952865335163,-61.9899770749318,
-61.8844857808398,-61.8346987407195,-61.7291919385078,-61.6238440118554,
-61.5186199677401,-61.4134618736093,-61.308333620637,-61.203199144233,-61.0979526828596,
-60.9926432242751,-60.8871519301831,-60.8373648900627,-60.6850374634616,
-60.6412095134546),.UNSPECIFIED.);
#3865=B_SPLINE_CURVE_WITH_KNOTS('',3,(#276651,#276652,#276653,#276654,#276655,
#276656,#276657,#276658,#276659,#276660),.UNSPECIFIED.,.F.,.F.,(4,1,1,1,
1,1,1,4),(-60.6412060771752,-59.8400310394059,-58.8426971887492,-57.8453633380924,
-56.8480294874356,-55.8506956367789,-54.8533617861221,-54.358024206275),
 .UNSPECIFIED.);
#3866=B_SPLINE_CURVE_WITH_KNOTS('',3,(#276662,#276663,#276664,#276665,#276666,
#276667,#276668,#276669,#276670,#276671),.UNSPECIFIED.,.F.,.F.,(4,1,1,1,
1,1,1,4),(-54.358024206275,-53.8560279354653,-52.8586940848086,-51.8613602341518,
-50.864026383495,-49.8666925328383,-48.8693586821815,-48.0748417153853),
 .UNSPECIFIED.);
#3867=B_SPLINE_CURVE_WITH_KNOTS('',3,(#276673,#276674,#276675,#276676,#276677,
#276678,#276679,#276680,#276681,#276682,#276683,#276684,#276685,#276686,
#276687,#276688,#276689,#276690,#276691,#276692,#276693,#276694,#276695,
#276696,#276697,#276698,#276699,#276700,#276701,#276702,#276703,#276704,
#276705,#276706,#276707,#276708,#276709,#276710,#276711,#276712,#276713,
#276714,#276715,#276716,#276717,#276718,#276719,#276720,#276721,#276722,
#276723,#276724,#276725,#276726,#276727,#276728,#276729,#276730,#276731,
#276732,#276733,#276734,#276735,#276736,#276737,#276738,#276739,#276740,
#276741,#276742,#276743,#276744,#276745,#276746,#276747,#276748,#276749,
#276750,#276751,#276752,#276753,#276754,#276755,#276756,#276757,#276758,
#276759,#276760,#276761,#276762,#276763,#276764,#276765,#276766,#276767,
#276768,#276769,#276770,#276771,#276772,#276773,#276774,#276775,#276776,
#276777,#276778,#276779,#276780,#276781,#276782,#276783,#276784,#276785,
#276786,#276787,#276788,#276789,#276790,#276791,#276792,#276793,#276794,
#276795,#276796,#276797,#276798,#276799,#276800,#276801,#276802,#276803,
#276804,#276805,#276806,#276807,#276808,#276809,#276810,#276811,#276812,
#276813,#276814,#276815,#276816,#276817,#276818,#276819,#276820,#276821,
#276822,#276823,#276824,#276825,#276826,#276827,#276828,#276829,#276830,
#276831,#276832,#276833,#276834,#276835,#276836,#276837,#276838,#276839,
#276840,#276841,#276842,#276843,#276844,#276845,#276846,#276847,#276848,
#276849,#276850,#276851,#276852,#276853,#276854,#276855,#276856,#276857,
#276858,#276859,#276860,#276861,#276862),.UNSPECIFIED.,.F.,.F.,(4,3,3,3,
3,3,3,3,3,3,3,3,3,3,3,3,3,3,3,3,3,3,3,3,3,3,3,3,3,3,3,3,3,3,3,3,3,3,3,3,
3,3,3,3,3,3,3,3,3,3,3,3,3,3,3,3,3,3,3,3,3,3,3,4),(-48.0748388990954,-47.9250452568101,
-47.8720248315247,-47.766518029313,-47.6611701026606,-47.5559460585454,
-47.4507879644146,-47.3456597114423,-47.2405252350384,-47.1352787736651,
-47.0299693150807,-46.9244780209887,-46.874690980868,-46.7691841786562,
-46.6638362520038,-46.5586122078884,-46.4534541137576,-46.3483258607852,
-46.2431913843811,-46.1379449230077,-46.0326354644232,-45.9271441703312,
-45.8773571302112,-45.7718503279994,-45.6665024013469,-45.5612783572316,
-45.4561202631007,-45.3509920101283,-45.2458575337242,-45.1406110723508,
-45.0353016137664,-44.9298103196743,-44.8800232795544,-44.7745164773427,
-44.6691685506903,-44.563944506575,-44.4587864124442,-44.3536581594719,
-44.2485236830678,-44.1432772216945,-44.0379677631101,-43.9324764690181,
-43.8826894288977,-43.777182626686,-43.6718347000335,-43.5666106559182,
-43.4614525617874,-43.356324308815,-43.251189832411,-43.1459433710376,-43.0406339124532,
-42.9351426183611,-42.8853555782409,-42.7798487760291,-42.6745008493767,
-42.5692768052613,-42.4641187111305,-42.3589904581581,-42.2538559817541,
-42.1486095203807,-42.0433000617962,-41.9378087677041,-41.8880217275841,
-41.7916535919158),.UNSPECIFIED.);
#3868=B_SPLINE_CURVE_WITH_KNOTS('',3,(#276864,#276865,#276866,#276867,#276868,
#276869,#276870,#276871,#276872,#276873),.UNSPECIFIED.,.F.,.F.,(4,1,1,1,
1,1,1,4),(-41.7916448335886,-40.8906878769274,-39.8933540262706,-38.8960201756138,
-37.8986863249571,-36.9013524743003,-35.9040186236436,-35.5084682847362),
 .UNSPECIFIED.);
#3869=B_SPLINE_CURVE_WITH_KNOTS('',3,(#276875,#276876,#276877,#276878,#276879,
#276880,#276881,#276882,#276883,#276884),.UNSPECIFIED.,.F.,.F.,(4,1,1,1,
1,1,1,4),(-35.5084682847362,-34.9066847729868,-33.90935092233,-32.9120170716733,
-31.9146832210165,-30.9173493703597,-29.920015519703,-29.2252829775566),
 .UNSPECIFIED.);
#3870=B_SPLINE_CURVE_WITH_KNOTS('',3,(#276886,#276887,#276888,#276889,#276890,
#276891,#276892,#276893,#276894,#276895,#276896,#276897,#276898,#276899,
#276900,#276901,#276902,#276903,#276904,#276905,#276906,#276907,#276908,
#276909,#276910,#276911,#276912,#276913,#276914,#276915,#276916,#276917,
#276918,#276919,#276920,#276921,#276922,#276923,#276924,#276925,#276926,
#276927,#276928,#276929,#276930,#276931,#276932,#276933,#276934,#276935,
#276936,#276937,#276938,#276939,#276940,#276941,#276942,#276943,#276944,
#276945,#276946,#276947,#276948,#276949,#276950,#276951,#276952,#276953,
#276954,#276955,#276956,#276957,#276958,#276959,#276960,#276961,#276962,
#276963,#276964,#276965,#276966,#276967,#276968,#276969,#276970,#276971,
#276972,#276973,#276974,#276975,#276976,#276977,#276978,#276979,#276980,
#276981,#276982,#276983,#276984,#276985,#276986,#276987,#276988,#276989,
#276990,#276991,#276992,#276993,#276994,#276995,#276996,#276997,#276998,
#276999,#277000,#277001,#277002,#277003,#277004,#277005,#277006,#277007,
#277008,#277009,#277010,#277011,#277012,#277013,#277014,#277015,#277016,
#277017,#277018,#277019,#277020,#277021,#277022,#277023,#277024,#277025,
#277026,#277027,#277028,#277029,#277030,#277031,#277032,#277033,#277034,
#277035,#277036,#277037,#277038,#277039,#277040,#277041,#277042,#277043,
#277044,#277045,#277046,#277047,#277048,#277049,#277050,#277051,#277052,
#277053,#277054,#277055,#277056,#277057,#277058,#277059,#277060,#277061,
#277062,#277063,#277064,#277065,#277066,#277067,#277068,#277069,#277070,
#277071,#277072,#277073,#277074,#277075),.UNSPECIFIED.,.F.,.F.,(4,3,3,3,
3,3,3,3,3,3,3,3,3,3,3,3,3,3,3,3,3,3,3,3,3,3,3,3,3,3,3,3,3,3,3,3,3,3,3,3,
3,3,3,3,3,3,3,3,3,3,3,3,3,3,3,3,3,3,3,3,3,3,3,4),(-29.2252827920403,-29.0991710721254,
-28.9713316793409,-28.9226816690462,-28.8171748668507,-28.7118269402145,
-28.606602896115,-28.501444802,-28.3963165490433,-28.2911820726547,-28.1859356112964,
-28.0806261527268,-27.9751348586492,-27.9253478183894,-27.8198410162024,
-27.7144930895749,-27.6092690454849,-27.5041109513795,-27.3989826984327,
-27.2938482220543,-27.1886017607065,-27.0832923021477,-26.977801008081,
-26.9280139677327,-26.8225071654109,-26.7171592386482,-26.6119351944228,
-26.506777100182,-26.4016488471,-26.2965143705868,-26.1912679091058,-26.0859584504144,
-25.9804671562175,-25.9306801170759,-25.8251733150019,-25.7198253884868,
-25.6146013445074,-25.5094432505115,-25.404314997673,-25.2991805214014,
-25.1939340601577,-25.0886246017014,-24.983133307734,-24.9333462664191,
-24.8278394643211,-24.7224915377845,-24.6172674937872,-24.5121093997757,
-24.4069811469239,-24.3018466706412,-24.1966002093899,-24.0912907509281,
-23.9857994569581,-23.9360124157624,-23.8305704338793,-23.7252872773173,
-23.620127770382,-23.5150339599447,-23.4099696373072,-23.3048986377144,
-23.1997155503862,-23.094468867793,-22.9890413697073,-22.9420976708737),
 .UNSPECIFIED.);
#3871=B_SPLINE_CURVE_WITH_KNOTS('',3,(#277077,#277078,#277079,#277080,#277081,
#277082,#277083,#277084,#277085,#277086,#277087,#277088,#277089,#277090,
#277091,#277092,#277093,#277094,#277095,#277096,#277097,#277098,#277099,
#277100,#277101,#277102,#277103,#277104,#277105,#277106,#277107,#277108,
#277109,#277110,#277111,#277112,#277113,#277114,#277115,#277116,#277117,
#277118,#277119,#277120,#277121,#277122,#277123,#277124,#277125,#277126,
#277127,#277128,#277129,#277130,#277131,#277132,#277133,#277134,#277135,
#277136,#277137,#277138,#277139,#277140,#277141,#277142,#277143,#277144,
#277145,#277146,#277147,#277148,#277149,#277150,#277151,#277152,#277153,
#277154,#277155,#277156,#277157,#277158,#277159,#277160,#277161,#277162,
#277163,#277164,#277165,#277166,#277167,#277168,#277169,#277170,#277171,
#277172,#277173,#277174,#277175,#277176,#277177,#277178,#277179,#277180,
#277181,#277182,#277183,#277184,#277185,#277186,#277187,#277188,#277189,
#277190,#277191,#277192,#277193,#277194,#277195,#277196,#277197,#277198,
#277199,#277200,#277201,#277202,#277203,#277204,#277205,#277206,#277207,
#277208,#277209,#277210,#277211,#277212,#277213,#277214,#277215,#277216,
#277217,#277218,#277219,#277220,#277221,#277222,#277223,#277224,#277225,
#277226,#277227,#277228,#277229,#277230,#277231,#277232,#277233,#277234,
#277235,#277236,#277237,#277238,#277239,#277240,#277241,#277242,#277243,
#277244,#277245,#277246,#277247,#277248,#277249,#277250,#277251,#277252,
#277253,#277254,#277255,#277256,#277257,#277258,#277259,#277260,#277261,
#277262,#277263,#277264,#277265,#277266,#277267,#277268,#277269),
 .UNSPECIFIED.,.F.,.F.,(4,3,3,3,3,3,3,3,3,3,3,3,3,3,3,3,3,3,3,3,3,3,3,3,
3,3,3,3,3,3,3,3,3,3,3,3,3,3,3,3,3,3,3,3,3,3,3,3,3,3,3,3,3,3,3,3,3,3,3,3,
3,3,3,3,4),(-22.9420976703771,-22.9386785651056,-22.833171763997,-22.7278238384453,
-22.6225997954218,-22.5174417023766,-22.4123134504822,-22.3071789751466,
-22.2019325148207,-22.0966230572732,-21.9911317641911,-21.9413447144488,
-21.8358379126161,-21.7304899863559,-21.62526594265,-21.520107848939,-21.4149795963963,
-21.3098451204308,-21.2045986595064,-21.0992892013775,-20.9937979077462,
-20.9440108637921,-20.8385040568042,-20.7331561253577,-20.6279320764448,
-20.5227739775171,-20.4176457197557,-20.3125112385776,-20.2072647724855,
-20.1019553092069,-19.9964640105077,-19.9466770131353,-19.8411702194118,
-19.7358223012373,-19.6305982655446,-19.5254401797971,-19.4203119351568,
-19.3151774670212,-19.2099310137648,-19.1046215632227,-18.9991302769745,
-18.9493431624785,-18.8438363600323,-18.7384884332319,-18.6332643890952,
-18.5281062950215,-18.4229780421838,-18.3178435659912,-18.2125971049424,
-18.1072876467475,-18.0017963531398,-17.9520093118218,-17.8465024793659,
-17.7411545223281,-17.6359304477663,-17.530772323169,-17.425644039756,-17.3205095329828,
-17.2152630415555,-17.1099535530528,-17.0044622295655,-16.954675461165,
-16.8256403797072,-16.6984335818362,-16.6589125353209),.UNSPECIFIED.);
#3872=B_SPLINE_CURVE_WITH_KNOTS('',3,(#277271,#277272,#277273,#277274,#277275,
#277276,#277277,#277278,#277279,#277280),.UNSPECIFIED.,.F.,.F.,(4,1,1,1,
1,1,1,4),(-16.6589123631975,-15.9573416105082,-14.9600077598515,-13.9626739091947,
-12.9653400585379,-11.9680062078812,-10.9706723572244,-10.3757270560179),
 .UNSPECIFIED.);
#3873=B_SPLINE_CURVE_WITH_KNOTS('',3,(#277281,#277282,#277283,#277284,#277285,
#277286,#277287,#277288,#277289,#277290),.UNSPECIFIED.,.F.,.F.,(4,1,1,1,
1,1,1,4),(-10.3757270560179,-9.97333850656766,-8.97600465591089,-7.97867080525412,
-6.98133695459736,-5.98400310394059,-4.98666925328383,-4.09255055993695),
 .UNSPECIFIED.);
#3874=B_SPLINE_CURVE_WITH_KNOTS('',3,(#277293,#277294,#277295,#277296,#277297,
#277298,#277299,#277300,#277301,#277302,#277303,#277304,#277305,#277306,
#277307,#277308,#277309,#277310,#277311,#277312,#277313,#277314,#277315,
#277316,#277317,#277318,#277319,#277320,#277321,#277322,#277323,#277324,
#277325,#277326,#277327,#277328,#277329,#277330,#277331,#277332,#277333,
#277334,#277335,#277336,#277337,#277338,#277339,#277340,#277341,#277342,
#277343,#277344,#277345,#277346,#277347,#277348,#277349,#277350,#277351,
#277352,#277353,#277354,#277355,#277356,#277357,#277358,#277359,#277360,
#277361,#277362,#277363,#277364,#277365,#277366,#277367,#277368),
 .UNSPECIFIED.,.F.,.F.,(4,3,3,3,3,3,3,3,3,3,3,3,3,3,3,3,3,3,3,3,3,3,3,3,
3,4),(182.609476336781,182.720981410639,182.832583305898,182.944230107119,
183.056086738955,183.156843832074,183.268703246413,183.380368125164,183.491924434765,
183.603414787061,183.714881699591,183.826450437116,183.93806614918,184.049898405165,
184.154177682731,184.264652382406,184.375509776279,184.485678175887,184.595782248961,
184.705866563965,184.81727780632,184.927534423388,185.039522978388,185.151511533388,
185.3342658208,185.353966561798),.UNSPECIFIED.);
#3875=B_SPLINE_CURVE_WITH_KNOTS('',3,(#277369,#277370,#277371,#277372,#277373,
#277374,#277375,#277376,#277377,#277378,#277379,#277380,#277381,#277382,
#277383,#277384,#277385,#277386,#277387,#277388,#277389,#277390),
 .UNSPECIFIED.,.F.,.F.,(4,3,3,3,3,3,3,4),(185.353966562125,185.466365028953,
185.578618560049,185.690768460106,185.805287691091,185.917389176518,186.033117280281,
186.148845384045),.UNSPECIFIED.);
#3876=B_SPLINE_CURVE_WITH_KNOTS('',3,(#277391,#277392,#277393,#277394,#277395,
#277396,#277397,#277398,#277399,#277400,#277401,#277402,#277403,#277404,
#277405,#277406,#277407,#277408,#277409,#277410,#277411,#277412,#277413,
#277414,#277415,#277416,#277417,#277418,#277419,#277420,#277421,#277422,
#277423,#277424,#277425,#277426,#277427,#277428,#277429,#277430,#277431,
#277432,#277433,#277434,#277435,#277436,#277437,#277438,#277439,#277440,
#277441,#277442,#277443,#277444,#277445,#277446,#277447,#277448,#277449,
#277450,#277451,#277452,#277453,#277454),.UNSPECIFIED.,.F.,.F.,(4,3,3,3,
3,3,3,3,3,3,3,3,3,3,3,3,3,3,3,3,3,4),(182.608828346121,182.720452013284,
182.832284778709,182.913686920972,183.024155546641,183.135063468431,183.245225477106,
183.355323083989,183.465400865193,183.576905379135,183.687155538369,183.799287229665,
183.911418920962,184.02624684209,184.140827409106,184.255261915833,184.369585299384,
184.48383233761,184.598072078494,184.712299653782,184.826611607649,184.909150920952),
 .UNSPECIFIED.);
#3877=B_SPLINE_CURVE_WITH_KNOTS('',3,(#277456,#277457,#277458,#277459,#277460,
#277461,#277462,#277463,#277464,#277465,#277466,#277467,#277468,#277469,
#277470,#277471,#277472,#277473,#277474,#277475,#277476,#277477,#277478,
#277479,#277480,#277481,#277482,#277483),.UNSPECIFIED.,.F.,.F.,(4,3,3,3,
3,3,3,3,3,4),(-0.271362855059747,-0.249815162449229,-0.228817987081128,
-0.214757039459256,-0.202712716314943,-0.199280160428694,-0.179100594986104,
-0.172574196593642,-0.151847730093891,-0.1354956858039),.UNSPECIFIED.);
#3878=B_SPLINE_CURVE_WITH_KNOTS('',3,(#278196,#278197,#278198,#278199,#278200,
#278201,#278202,#278203,#278204,#278205,#278206,#278207,#278208,#278209,
#278210,#278211,#278212,#278213,#278214,#278215,#278216,#278217,#278218,
#278219,#278220,#278221,#278222,#278223,#278224,#278225,#278226,#278227,
#278228,#278229,#278230,#278231,#278232,#278233,#278234,#278235,#278236,
#278237,#278238,#278239,#278240,#278241,#278242,#278243,#278244,#278245,
#278246,#278247,#278248,#278249,#278250,#278251,#278252,#278253,#278254,
#278255,#278256,#278257,#278258,#278259,#278260,#278261,#278262,#278263,
#278264,#278265,#278266,#278267,#278268,#278269,#278270,#278271,#278272,
#278273,#278274,#278275,#278276,#278277,#278278,#278279,#278280),
 .UNSPECIFIED.,.F.,.F.,(4,3,3,3,3,3,3,3,3,3,3,3,3,3,3,3,3,3,3,3,3,3,3,3,
3,3,3,3,4),(-0.364629307890672,-0.35088498418457,-0.32922248441233,-0.318977271176652,
-0.31373572999827,-0.309363560225569,-0.288064487980142,-0.26690192544149,
-0.264003434189125,-0.260297566857666,-0.239602118261299,-0.219188400900535,
-0.199416811699232,-0.194875855288817,-0.191398750352895,-0.171813098007178,
-0.16617324728061,-0.146077800662944,-0.126706278567434,-0.123378888671009,
-0.103932070266397,-0.0846696063770791,-0.0655665987659766,-0.0621850320486812,
-0.058954655734169,-0.0403439049005739,-0.0223158895279108,-0.00443448004250249,
-3.33131800984143E-15),.UNSPECIFIED.);
#3879=B_SPLINE_CURVE_WITH_KNOTS('',3,(#279001,#279002,#279003,#279004,#279005,
#279006,#279007,#279008,#279009,#279010,#279011,#279012,#279013,#279014,
#279015,#279016,#279017,#279018,#279019,#279020,#279021,#279022,#279023,
#279024,#279025,#279026,#279027,#279028,#279029,#279030,#279031,#279032,
#279033,#279034,#279035,#279036,#279037,#279038,#279039,#279040,#279041,
#279042,#279043,#279044,#279045,#279046,#279047,#279048,#279049,#279050,
#279051,#279052,#279053,#279054,#279055,#279056,#279057,#279058,#279059,
#279060,#279061,#279062,#279063,#279064,#279065,#279066,#279067,#279068,
#279069,#279070,#279071,#279072,#279073,#279074,#279075,#279076,#279077,
#279078,#279079,#279080,#279081,#279082),.UNSPECIFIED.,.F.,.F.,(4,3,3,3,
3,3,3,3,3,3,3,3,3,3,3,3,3,3,3,3,3,3,3,3,3,3,3,4),(-0.366397579005839,-0.355373790886745,
-0.337291596355845,-0.327068869252799,-0.321659955027813,-0.303056283858023,
-0.2839439572191,-0.281261647266766,-0.277594690433741,-0.258106988423997,
-0.238287343590241,-0.225542977825418,-0.218358221560673,-0.214836850115746,
-0.194406992337549,-0.187160363760496,-0.167265720489167,-0.149318298208285,
-0.146103234631719,-0.125762615585401,-0.104752145197835,-0.0837416748102686,
-0.0753034310399412,-0.0721935754585015,-0.0505500221103818,-0.028856412602834,
-0.00762632909558976,0.),.UNSPECIFIED.);
#3880=B_SPLINE_CURVE_WITH_KNOTS('',3,(#279133,#279134,#279135,#279136,#279137,
#279138,#279139,#279140,#279141,#279142,#279143,#279144,#279145,#279146,
#279147,#279148,#279149,#279150,#279151,#279152,#279153,#279154,#279155,
#279156,#279157,#279158,#279159,#279160,#279161,#279162,#279163,#279164,
#279165,#279166,#279167,#279168,#279169,#279170,#279171,#279172,#279173,
#279174,#279175,#279176,#279177,#279178,#279179,#279180,#279181,#279182,
#279183,#279184,#279185,#279186,#279187,#279188,#279189,#279190,#279191,
#279192,#279193),.UNSPECIFIED.,.F.,.F.,(4,3,3,3,3,3,3,3,3,3,3,3,3,3,3,3,
3,3,3,3,4),(-4.09254174883833,-3.98934337020898,-3.88363221779152,-3.77808060077488,
-3.67265482016529,-3.56729632526176,-3.46196930491298,-3.35663799380962,
-3.25119893725734,-3.14569903290218,-3.04002256345967,-2.99200752765673,
-2.88747169635222,-2.78311107345422,-2.6788481173541,-2.57464534892016,
-2.470465371017,-2.3662011665343,-2.26189731347916,-2.15741074042207,-2.06549299936852),
 .UNSPECIFIED.);
#3881=B_SPLINE_CURVE_WITH_KNOTS('',3,(#279197,#279198,#279199,#279200,#279201,
#279202,#279203,#279204,#279205,#279206,#279207,#279208,#279209,#279210,
#279211,#279212,#279213,#279214,#279215,#279216,#279217,#279218,#279219,
#279220,#279221,#279222,#279223,#279224,#279225,#279226,#279227,#279228,
#279229,#279230),.UNSPECIFIED.,.F.,.F.,(4,3,3,3,3,3,3,3,3,3,3,4),(0.,0.107973995962156,
0.219228117795647,0.327124364615333,0.435023022759881,0.542953260606805,
0.650944276415295,0.759103142526299,0.867360126689599,0.97581640543646,
0.998006970630082,1.11419103802948),.UNSPECIFIED.);
#3882=B_SPLINE_CURVE_WITH_KNOTS('',3,(#279232,#279233,#279234,#279235,#279236,
#279237,#279238,#279239,#279240,#279241,#279242,#279243,#279244,#279245,
#279246,#279247,#279248,#279249,#279250,#279251,#279252,#279253,#279254,
#279255,#279256,#279257,#279258,#279259,#279260,#279261,#279262,#279263,
#279264,#279265,#279266,#279267,#279268,#279269,#279270,#279271,#279272,
#279273,#279274,#279275,#279276,#279277,#279278,#279279,#279280,#279281,
#279282,#279283,#279284,#279285,#279286,#279287,#279288,#279289,#279290,
#279291,#279292,#279293,#279294,#279295,#279296,#279297,#279298,#279299,
#279300,#279301,#279302,#279303,#279304,#279305,#279306,#279307,#279308,
#279309,#279310,#279311,#279312,#279313,#279314,#279315,#279316,#279317,
#279318,#279319,#279320,#279321,#279322,#279323,#279324,#279325,#279326,
#279327,#279328,#279329,#279330,#279331,#279332,#279333,#279334,#279335,
#279336,#279337,#279338,#279339,#279340,#279341,#279342,#279343,#279344,
#279345,#279346,#279347,#279348,#279349,#279350,#279351,#279352,#279353,
#279354,#279355,#279356,#279357,#279358,#279359,#279360,#279361,#279362,
#279363,#279364,#279365,#279366,#279367,#279368,#279369,#279370,#279371,
#279372,#279373,#279374,#279375,#279376,#279377,#279378,#279379,#279380,
#279381,#279382,#279383,#279384,#279385,#279386,#279387,#279388,#279389,
#279390,#279391,#279392,#279393,#279394,#279395,#279396,#279397,#279398,
#279399,#279400,#279401,#279402,#279403,#279404,#279405,#279406,#279407,
#279408,#279409,#279410,#279411,#279412,#279413,#279414,#279415,#279416,
#279417,#279418,#279419,#279420,#279421),.UNSPECIFIED.,.F.,.F.,(4,3,3,3,
3,3,3,3,3,3,3,3,3,3,3,3,3,3,3,3,3,3,3,3,3,3,3,3,3,3,3,3,3,3,3,3,3,3,3,3,
3,3,3,3,3,3,3,3,3,3,3,3,3,3,3,3,3,3,3,3,3,3,3,4),(1.11419103844308,1.21719187770655,
1.32003209885005,1.42278427700502,1.52548718566634,1.6281795105233,1.73096939481268,
1.83381185890053,1.93683560088162,1.99601394126018,2.10167359162095,2.20717435751719,
2.31255046470255,2.41786002560773,2.5231389034132,2.62842291627881,2.73381640871969,
2.83927155151866,2.94490541042443,2.99402091189026,3.09970332166566,3.20523066244488,
3.31063889552096,3.41598401676772,3.52130184505124,3.62662815778746,3.73206875948818,
3.83757382877443,3.94326146232322,3.99202788252035,4.09738133007778,4.20257357461044,
4.30763927886319,4.41263745687271,4.51760445552907,4.62257657593037,4.72766031671474,
4.83280647814355,4.93813581606208,4.99003485315045,5.0955641079553,5.20093443441008,
5.30618072088195,5.41136093238526,5.51651114356894,5.62166738469945,5.72693536855835,
5.83226611849798,5.93777863534395,5.98804182378054,6.0935615968424,6.19892280124285,
6.30416054776096,6.40933258652753,6.51447500595197,6.61962385045829,6.72488509082588,
6.83020946041486,6.93571622877576,6.98604879441062,7.10224037718433,7.21807745680911,
7.33333553933627,7.39737593502646),.UNSPECIFIED.);
#3883=B_SPLINE_CURVE_WITH_KNOTS('',3,(#279423,#279424,#279425,#279426,#279427,
#279428,#279429,#279430,#279431,#279432),.UNSPECIFIED.,.F.,.F.,(4,1,1,1,
1,1,1,4),(7.39737634520907,7.98405576504071,8.9820627356708,9.98006970630089,
10.978076676931,11.9760836475611,12.9740906181912,13.6805616523887),
 .UNSPECIFIED.);
#3884=B_SPLINE_CURVE_WITH_KNOTS('',3,(#279434,#279435,#279436,#279437,#279438,
#279439,#279440,#279441,#279442,#279443,#279444,#279445,#279446,#279447,
#279448,#279449,#279450,#279451,#279452,#279453,#279454,#279455,#279456,
#279457,#279458,#279459,#279460,#279461,#279462,#279463,#279464,#279465,
#279466,#279467,#279468,#279469,#279470,#279471,#279472,#279473,#279474,
#279475,#279476,#279477,#279478,#279479,#279480,#279481,#279482,#279483,
#279484,#279485,#279486,#279487,#279488,#279489,#279490,#279491,#279492,
#279493,#279494,#279495,#279496,#279497,#279498,#279499,#279500,#279501,
#279502,#279503,#279504,#279505,#279506,#279507,#279508,#279509,#279510,
#279511,#279512,#279513,#279514,#279515,#279516,#279517,#279518,#279519,
#279520,#279521,#279522,#279523,#279524,#279525,#279526,#279527,#279528,
#279529,#279530,#279531,#279532,#279533,#279534,#279535,#279536,#279537,
#279538,#279539,#279540,#279541,#279542,#279543,#279544,#279545,#279546,
#279547,#279548,#279549,#279550,#279551,#279552,#279553,#279554,#279555,
#279556,#279557,#279558,#279559,#279560,#279561,#279562,#279563,#279564,
#279565,#279566,#279567,#279568,#279569,#279570,#279571,#279572,#279573,
#279574,#279575,#279576,#279577,#279578,#279579,#279580,#279581,#279582,
#279583,#279584,#279585,#279586,#279587,#279588,#279589,#279590,#279591,
#279592,#279593,#279594,#279595,#279596,#279597,#279598,#279599,#279600,
#279601,#279602,#279603,#279604,#279605,#279606,#279607,#279608,#279609,
#279610,#279611,#279612,#279613,#279614,#279615,#279616,#279617,#279618,
#279619,#279620,#279621,#279622,#279623,#279624,#279625,#279626),
 .UNSPECIFIED.,.F.,.F.,(4,3,3,3,3,3,3,3,3,3,3,3,3,3,3,3,3,3,3,3,3,3,3,3,
3,3,3,3,3,3,3,3,3,3,3,3,3,3,3,3,3,3,3,3,3,3,3,3,3,3,3,3,3,3,3,3,3,3,3,3,
3,3,3,3,4),(13.6805618160026,13.8082883325048,13.9379733142516,13.9720975888212,
14.077595545405,14.1829344247124,14.2881492016154,14.3932978838084,14.4984165948394,
14.6035414138825,14.7087783117543,14.8140781221029,14.919560253473,14.9701045594513,
15.0756023545526,15.1809410711868,15.2861556844645,15.391304202538,15.4964227492074,
15.6015474038986,15.7067841385673,15.8120837861284,15.9175657570756,15.9681115300814,
16.0736092504098,16.1789478903724,16.2841624245375,16.3893108620278,16.4944293267638,
16.5995538982904,16.7047905484922,16.8100901107186,16.9155719958822,16.9661185007115,
17.0716163081709,17.1769550366742,17.2821696610324,17.3873181896896,17.4924367464281,
17.5975614106554,17.7027981539825,17.8080978097136,17.9135797879851,17.9641254713416,
18.0696232498215,18.1749619490664,18.280176543899,18.3853250428819,18.4904435698429,
18.5955682042347,18.7008049178441,18.8061045438807,18.9115864928076,18.9621324419717,
19.0676302129107,19.1729689043845,19.2781834911422,19.3833319818661,19.4884505003964,
19.593575126198,19.6988118310328,19.8041114481769,19.9095933881216,19.9601394126018,
19.9637469595682),.UNSPECIFIED.);
#3885=B_SPLINE_CURVE_WITH_KNOTS('',3,(#279628,#279629,#279630,#279631,#279632,
#279633,#279634,#279635,#279636,#279637,#279638,#279639,#279640,#279641,
#279642,#279643,#279644,#279645,#279646,#279647,#279648,#279649,#279650,
#279651,#279652,#279653,#279654,#279655,#279656,#279657,#279658,#279659,
#279660,#279661,#279662,#279663,#279664,#279665,#279666,#279667,#279668,
#279669,#279670,#279671,#279672,#279673,#279674,#279675,#279676,#279677,
#279678,#279679,#279680,#279681,#279682,#279683,#279684,#279685,#279686,
#279687,#279688,#279689,#279690,#279691,#279692,#279693,#279694,#279695,
#279696,#279697,#279698,#279699,#279700,#279701,#279702,#279703,#279704,
#279705,#279706,#279707,#279708,#279709,#279710,#279711,#279712,#279713,
#279714,#279715,#279716,#279717,#279718,#279719,#279720,#279721,#279722,
#279723,#279724,#279725,#279726,#279727,#279728,#279729,#279730,#279731,
#279732,#279733,#279734,#279735,#279736,#279737,#279738,#279739,#279740,
#279741,#279742,#279743,#279744,#279745,#279746,#279747,#279748,#279749,
#279750,#279751,#279752,#279753,#279754,#279755,#279756,#279757,#279758,
#279759,#279760,#279761,#279762,#279763,#279764,#279765,#279766,#279767,
#279768,#279769,#279770,#279771,#279772,#279773,#279774,#279775,#279776,
#279777,#279778,#279779,#279780,#279781,#279782,#279783,#279784,#279785,
#279786,#279787,#279788,#279789,#279790,#279791,#279792,#279793,#279794,
#279795,#279796,#279797,#279798,#279799,#279800,#279801,#279802,#279803,
#279804,#279805,#279806,#279807,#279808,#279809,#279810,#279811,#279812,
#279813,#279814,#279815,#279816,#279817),.UNSPECIFIED.,.F.,.F.,(4,3,3,3,
3,3,3,3,3,3,3,3,3,3,3,3,3,3,3,3,3,3,3,3,3,3,3,3,3,3,3,3,3,3,3,3,3,3,3,3,
3,3,3,3,3,3,3,3,3,3,3,3,3,3,3,3,3,3,3,3,3,3,3,4),(19.9637469599589,20.0691762496,
20.1744465389314,20.2795930074112,20.3846736705057,20.4897247569757,20.5947824515381,
20.6999523658092,20.8051858417855,20.9106005879211,20.9581463832319,21.0636441615438,
21.1689828605436,21.2741974550174,21.3793459535709,21.4844644800325,21.5895891138554,
21.6948258267937,21.8001254520998,21.9056074002119,21.956153353862,22.0616511315823,
22.1669898299647,22.2722044237851,22.3773529216633,22.4824714474289,22.5875960805357,
22.6928327927324,22.7981324172816,22.9036143646201,22.954160324492,23.0596581039059,
23.1649968040116,23.2702113995914,23.3753598992505,23.4804784268152,23.5856030617377,
23.6908397757618,23.7961394021476,23.9016213513182,23.9521672951221,24.057665073735,
24.1630037730298,24.2682183677881,24.3733668666195,24.4784853933521,24.5836100274381,
24.6888467406263,24.7941463661753,24.8996283145162,24.9501742657522,25.0556720443539,
25.1610107436346,25.2662253383753,25.3713738371867,25.4764923638964,25.5816169979577,
25.6868537111176,25.7921533366363,25.8976352849442,25.9481812363823,26.0768101553301,
26.2036580691034,26.2469320881093),.UNSPECIFIED.);
#3886=B_SPLINE_CURVE_WITH_KNOTS('',3,(#279819,#279820,#279821,#279822,#279823,
#279824,#279825,#279826,#279827,#279828),.UNSPECIFIED.,.F.,.F.,(4,1,1,1,
1,1,1,4),(26.2469322667478,26.9461882070124,27.9441951776425,28.9422021482726,
29.9402091189027,30.9382160895327,31.9362230601628,32.5301175739274),
 .UNSPECIFIED.);
#3887=B_SPLINE_CURVE_WITH_KNOTS('',3,(#279830,#279831,#279832,#279833,#279834,
#279835,#279836,#279837,#279838,#279839,#279840,#279841,#279842,#279843,
#279844,#279845,#279846,#279847,#279848,#279849,#279850,#279851,#279852,
#279853,#279854,#279855,#279856,#279857,#279858,#279859,#279860,#279861,
#279862,#279863,#279864,#279865,#279866,#279867,#279868,#279869,#279870,
#279871,#279872,#279873,#279874,#279875,#279876,#279877,#279878,#279879,
#279880,#279881,#279882,#279883,#279884,#279885,#279886,#279887,#279888,
#279889,#279890,#279891,#279892,#279893,#279894,#279895,#279896,#279897,
#279898,#279899,#279900,#279901,#279902,#279903,#279904,#279905,#279906,
#279907,#279908,#279909,#279910,#279911,#279912,#279913,#279914,#279915,
#279916,#279917,#279918,#279919,#279920,#279921,#279922,#279923,#279924,
#279925,#279926,#279927,#279928,#279929,#279930,#279931,#279932,#279933,
#279934,#279935,#279936,#279937,#279938,#279939,#279940,#279941,#279942,
#279943,#279944,#279945,#279946,#279947,#279948,#279949,#279950,#279951,
#279952,#279953,#279954,#279955,#279956,#279957,#279958,#279959,#279960,
#279961,#279962,#279963,#279964,#279965,#279966,#279967,#279968,#279969,
#279970,#279971,#279972,#279973,#279974,#279975,#279976,#279977,#279978,
#279979,#279980,#279981,#279982,#279983,#279984,#279985,#279986,#279987,
#279988,#279989,#279990,#279991,#279992,#279993,#279994,#279995,#279996,
#279997,#279998,#279999,#280000,#280001,#280002,#280003,#280004,#280005,
#280006,#280007,#280008,#280009,#280010,#280011,#280012,#280013,#280014,
#280015,#280016,#280017,#280018,#280019),.UNSPECIFIED.,.F.,.F.,(4,3,3,3,
3,3,3,3,3,3,3,3,3,3,3,3,3,3,3,3,3,3,3,3,3,3,3,3,3,3,3,3,3,3,3,3,3,3,3,3,
3,3,3,3,3,3,3,3,3,3,3,3,3,3,3,3,3,3,3,3,3,3,3,4),(32.530118003655,32.64600712011,
32.762304561712,32.879155677441,32.9342300307929,33.0397278095187,33.1450665089264,
33.2502811037972,33.3554296027407,33.4605481295847,33.5656727637819,33.670909477079,
33.7762091027359,33.8816910511823,33.932237001423,34.0377347801494,34.1430734795579,
34.2482880744293,34.3534365733734,34.458555100218,34.5636797344156,34.6689164477134,
34.7742160733709,34.8796980218179,34.9302439720531,35.03574175078,35.1410804501888,
35.2462950450607,35.3514435440053,35.4565620708504,35.5616867050485,35.6669234183467,
35.7722230440048,35.8777049924522,35.9282509426832,36.0337487214096,36.1390874208181,
36.2443020156895,36.3494505146337,36.4545690414783,36.5596936756759,36.6649303889737,
36.7702300146313,36.8757119630783,36.9262579133133,37.0317556920399,37.1370943914484,
37.2423089863199,37.3474574852643,37.452576012109,37.5577006463068,37.6629373596046,
37.7682369852624,37.8737189337095,37.9242648839434,38.0283818027737,38.1323195313251,
38.2361576431265,38.3399340926199,38.4436867444814,38.5475137381468,38.6513807199573,
38.7554057475333,38.813302881107),.UNSPECIFIED.);
#3888=B_SPLINE_CURVE_WITH_KNOTS('',3,(#280021,#280022,#280023,#280024,#280025,
#280026,#280027,#280028,#280029,#280030,#280031),.UNSPECIFIED.,.F.,.F.,
(4,1,1,1,1,1,1,1,4),(38.813302881107,38.9222718545735,39.9202788252036,
40.9182857958337,41.9162927664637,42.9142997370938,43.9123067077239,44.910313678354,
45.0964881882866),.UNSPECIFIED.);
#3889=B_SPLINE_CURVE_WITH_KNOTS('',3,(#280033,#280034,#280035,#280036,#280037,
#280038,#280039,#280040,#280041,#280042),.UNSPECIFIED.,.F.,.F.,(4,1,1,1,
1,1,1,4),(45.0964881882866,45.9083206489841,46.9063276196142,47.9043345902443,
48.9023415608744,49.9003485315045,50.8983555021345,51.3796721305015),
 .UNSPECIFIED.);
#3890=B_SPLINE_CURVE_WITH_KNOTS('',3,(#280044,#280045,#280046,#280047,#280048,
#280049,#280050,#280051,#280052,#280053,#280054,#280055,#280056,#280057,
#280058,#280059,#280060,#280061,#280062,#280063,#280064,#280065,#280066,
#280067,#280068,#280069,#280070,#280071,#280072,#280073,#280074,#280075,
#280076,#280077,#280078,#280079,#280080,#280081,#280082,#280083,#280084,
#280085,#280086,#280087,#280088,#280089,#280090,#280091,#280092,#280093,
#280094,#280095,#280096,#280097,#280098,#280099,#280100,#280101,#280102,
#280103,#280104,#280105,#280106,#280107,#280108,#280109,#280110,#280111,
#280112,#280113,#280114,#280115,#280116,#280117,#280118,#280119,#280120,
#280121,#280122,#280123,#280124,#280125,#280126,#280127,#280128,#280129,
#280130,#280131,#280132,#280133,#280134,#280135,#280136,#280137,#280138,
#280139,#280140,#280141,#280142,#280143,#280144,#280145,#280146,#280147,
#280148,#280149,#280150,#280151,#280152,#280153,#280154,#280155,#280156,
#280157,#280158,#280159,#280160,#280161,#280162,#280163,#280164,#280165,
#280166,#280167,#280168,#280169,#280170,#280171,#280172,#280173,#280174,
#280175,#280176,#280177,#280178,#280179,#280180,#280181,#280182,#280183,
#280184,#280185,#280186,#280187,#280188,#280189,#280190,#280191,#280192,
#280193,#280194,#280195,#280196,#280197,#280198,#280199,#280200,#280201,
#280202,#280203,#280204,#280205,#280206,#280207,#280208,#280209,#280210,
#280211,#280212,#280213,#280214,#280215,#280216,#280217,#280218,#280219,
#280220,#280221,#280222,#280223,#280224,#280225,#280226,#280227,#280228,
#280229,#280230,#280231,#280232,#280233),.UNSPECIFIED.,.F.,.F.,(4,3,3,3,
3,3,3,3,3,3,3,3,3,3,3,3,3,3,3,3,3,3,3,3,3,3,3,3,3,3,3,3,3,3,3,3,3,3,3,3,
3,3,3,3,3,3,3,3,3,3,3,3,3,3,3,3,3,3,3,3,3,3,3,4),(51.3796734954662,51.4890034742577,
51.5986022051298,51.70834049393,51.8183684296074,51.8963624727646,52.0018602514911,
52.1071989508998,52.2124135457714,52.3175620447157,52.4226805715604,52.5278052057581,
52.6330419190561,52.7383415447139,52.843823493161,52.8943694433947,52.9998672221213,
53.1052059215298,53.2104205164014,53.3155690153457,53.4206875421904,53.5258121763882,
53.6310488896862,53.7363485153438,53.8418304637909,53.8923764140248,53.9978741927513,
54.1032128921599,54.2084274870315,54.3135759859757,54.4186945128204,54.5238191470182,
54.6290558603161,54.734355485974,54.839837434421,54.8903833846549,54.9958811633815,
55.10121986279,55.2064344576615,55.3115829566059,55.4167014834508,55.5218261176487,
55.6270628309466,55.7323624566042,55.8378444050512,55.888390355285,55.9938881340116,
56.0992268334203,56.2044414282919,56.3095899272362,56.414708454081,56.5198330882791,
56.625069801577,56.7303694272347,56.835851375682,56.8863973259151,56.9904386065909,
57.0943385322742,57.1981352595082,57.3018667940288,57.405608533537,57.5093549662644,
57.6132006623058,57.6628588026458),.UNSPECIFIED.);
#3891=B_SPLINE_CURVE_WITH_KNOTS('',3,(#280235,#280236,#280237,#280238,#280239,
#280240,#280241,#280242,#280243,#280244,#280245),.UNSPECIFIED.,.F.,.F.,
(4,1,1,1,1,1,1,1,4),(57.6628588026458,57.8844042965452,58.8824112671752,
59.8804182378054,60.8784252084354,61.8764321790655,62.8744391496956,63.8724461203257,
63.9460441098254),.UNSPECIFIED.);
#3892=B_SPLINE_CURVE_WITH_KNOTS('',3,(#280247,#280248,#280249,#280250,#280251,
#280252,#280253,#280254,#280255,#280256),.UNSPECIFIED.,.F.,.F.,(4,1,1,1,
1,1,1,4),(63.9460441098254,64.8704530909558,65.8684600615859,66.866467032216,
67.8644740028461,68.8624809734761,69.8604879441062,70.2292218444269),
 .UNSPECIFIED.);
#3893=B_SPLINE_CURVE_WITH_KNOTS('',3,(#280258,#280259,#280260,#280261,#280262,
#280263,#280264,#280265,#280266,#280267,#280268,#280269,#280270,#280271,
#280272,#280273,#280274,#280275,#280276,#280277,#280278,#280279,#280280,
#280281,#280282,#280283,#280284,#280285,#280286,#280287,#280288,#280289,
#280290,#280291,#280292,#280293,#280294,#280295,#280296,#280297,#280298,
#280299,#280300,#280301,#280302,#280303,#280304,#280305,#280306,#280307,
#280308,#280309,#280310,#280311,#280312,#280313,#280314,#280315,#280316,
#280317,#280318,#280319,#280320,#280321,#280322,#280323,#280324,#280325,
#280326,#280327,#280328,#280329,#280330,#280331,#280332,#280333,#280334,
#280335,#280336,#280337,#280338,#280339,#280340,#280341,#280342,#280343,
#280344,#280345,#280346,#280347,#280348,#280349,#280350,#280351,#280352,
#280353,#280354,#280355,#280356,#280357,#280358,#280359,#280360,#280361,
#280362,#280363,#280364,#280365,#280366,#280367,#280368,#280369,#280370,
#280371,#280372,#280373,#280374,#280375,#280376,#280377,#280378,#280379,
#280380,#280381,#280382,#280383,#280384,#280385,#280386,#280387,#280388,
#280389,#280390,#280391,#280392,#280393,#280394,#280395,#280396,#280397,
#280398,#280399,#280400,#280401,#280402,#280403,#280404,#280405,#280406,
#280407,#280408,#280409,#280410,#280411,#280412,#280413,#280414,#280415,
#280416,#280417,#280418,#280419,#280420,#280421,#280422,#280423,#280424,
#280425,#280426,#280427,#280428,#280429,#280430,#280431,#280432,#280433,
#280434,#280435,#280436,#280437,#280438,#280439,#280440,#280441,#280442,
#280443,#280444,#280445,#280446,#280447),.UNSPECIFIED.,.F.,.F.,(4,3,3,3,
3,3,3,3,3,3,3,3,3,3,3,3,3,3,3,3,3,3,3,3,3,3,3,3,3,3,3,3,3,3,3,3,3,3,3,3,
3,3,3,3,3,3,3,3,3,3,3,3,3,3,3,3,3,3,3,3,3,3,3,4),(70.229229417005,70.335009033057,
70.4407990188872,70.5467185962429,70.6527015297735,70.7589032664553,70.8584949147363,
70.9639926934621,71.0693313928698,71.1745459877406,71.2796944866842,71.3848130135281,
71.4899376477252,71.5951743610223,71.7004739866793,71.8059559351256,71.8565018853664,
71.9619996640953,72.0673383635062,72.17255295838,72.2777014573267,72.3828199841735,
72.4879446183735,72.5931813316736,72.6984809573335,72.8039629057828,72.8545088559965,
72.9600066347213,73.065345334128,73.1705599289978,73.2757084279404,73.3808269547834,
73.4859515889798,73.5911883022759,73.696487927932,73.8019698763775,73.8525158266266,
73.9580136053487,74.0633523047526,74.1685668996196,74.2737153985593,74.3788339253994,
74.4839585595926,74.589195272886,74.6944948985394,74.799976846982,74.8505227972567,
74.9560205759993,75.0613592754235,75.1665738703108,75.271722369271,75.3768408961317,
75.4819655303449,75.5872022436584,75.6925018693315,75.7979838177936,75.8485297678868,
75.9539872943584,76.0592890581743,76.1644713975019,76.2695756454254,76.3746355093251,
76.4797099416953,76.5124147241846),.UNSPECIFIED.);
#3894=B_SPLINE_CURVE_WITH_KNOTS('',3,(#280449,#280450,#280451,#280452,#280453,
#280454,#280455,#280456,#280457,#280458),.UNSPECIFIED.,.F.,.F.,(4,1,1,1,
1,1,1,4),(76.5124219319248,76.8465367385169,77.8445437091469,78.842550679777,
79.8405576504071,80.8385646210372,81.8365715916673,82.7955949071842),
 .UNSPECIFIED.);
#3895=B_SPLINE_CURVE_WITH_KNOTS('',3,(#280460,#280461,#280462,#280463,#280464,
#280465,#280466,#280467,#280468,#280469,#280470,#280471,#280472,#280473,
#280474,#280475,#280476,#280477,#280478,#280479,#280480,#280481,#280482,
#280483,#280484,#280485,#280486,#280487,#280488,#280489,#280490,#280491,
#280492,#280493,#280494,#280495,#280496,#280497,#280498,#280499,#280500,
#280501,#280502,#280503,#280504,#280505,#280506,#280507,#280508,#280509,
#280510,#280511,#280512,#280513,#280514,#280515,#280516,#280517,#280518,
#280519,#280520,#280521,#280522,#280523,#280524,#280525,#280526,#280527,
#280528,#280529,#280530,#280531,#280532,#280533,#280534,#280535,#280536,
#280537,#280538,#280539,#280540,#280541,#280542,#280543,#280544,#280545,
#280546,#280547,#280548,#280549,#280550,#280551,#280552,#280553,#280554,
#280555,#280556,#280557,#280558,#280559,#280560,#280561,#280562,#280563,
#280564,#280565,#280566,#280567,#280568,#280569,#280570,#280571,#280572,
#280573,#280574,#280575,#280576,#280577,#280578,#280579,#280580,#280581,
#280582,#280583,#280584,#280585,#280586,#280587,#280588,#280589,#280590,
#280591,#280592,#280593,#280594,#280595,#280596,#280597,#280598,#280599,
#280600,#280601,#280602,#280603,#280604,#280605,#280606,#280607,#280608,
#280609,#280610,#280611,#280612,#280613,#280614,#280615,#280616,#280617,
#280618,#280619,#280620,#280621,#280622,#280623,#280624,#280625,#280626,
#280627,#280628,#280629,#280630,#280631,#280632,#280633,#280634,#280635,
#280636,#280637,#280638,#280639,#280640,#280641,#280642,#280643,#280644,
#280645,#280646,#280647,#280648,#280649),.UNSPECIFIED.,.F.,.F.,(4,3,3,3,
3,3,3,3,3,3,3,3,3,3,3,3,3,3,3,3,3,3,3,3,3,3,3,3,3,3,3,3,3,3,3,3,3,3,3,3,
3,3,3,3,3,3,3,3,3,3,3,3,3,3,3,3,3,3,3,3,3,3,3,4),(82.7956000313642,82.8345785622974,
82.9400763406927,83.0454150397571,83.1506296342673,83.2557781328398,83.360896659303,
83.4660212931101,83.5712580060064,83.6765576312558,83.7820395792885,83.8325855329275,
83.9380833163443,84.0434220204612,84.1486366200449,84.253785123701,84.3589036552502,
84.4640282941382,84.5692650120724,84.6745646423428,84.7800465953174,84.8305925035576,
84.9360902738077,85.0414289647494,85.1466435512085,85.2517920417788,85.3569105603002,
85.4620351862373,85.567271891425,85.6725715090463,85.7780534496546,85.8285994741877,
85.9340972534072,86.0394359532236,86.1446505483768,86.2497990475246,86.354917574495,
86.4600422087412,86.5652789219716,86.6705785474958,86.7760604957101,86.8266064448178,
86.9321042532473,87.0374429824998,87.1426576072785,87.2478061361519,87.3529246929027,
87.4580493569388,87.5632860997688,87.6685857548277,87.7740677321644,87.8246134154479,
87.9301111310943,88.0354497674402,88.140664299576,88.2458127360226,88.3509312006986,
88.4560557731484,88.5612924257495,88.6665919912204,88.772073880896,88.822620386078,
88.9578209224006,89.0787851943848),.UNSPECIFIED.);
#3896=B_SPLINE_CURVE_WITH_KNOTS('',3,(#280651,#280652,#280653,#280654,#280655,
#280656,#280657,#280658,#280659,#280660),.UNSPECIFIED.,.F.,.F.,(4,1,1,1,
1,1,1,4),(89.0787853385438,89.820627356708,90.8186343273381,91.8166412979682,
92.8146482685983,93.8126552392284,94.8106622098585,95.3619706457233),
 .UNSPECIFIED.);
#3897=B_SPLINE_CURVE_WITH_KNOTS('',3,(#280662,#280663,#280664,#280665,#280666,
#280667,#280668,#280669),.UNSPECIFIED.,.F.,.F.,(4,1,1,1,1,4),(95.3619706457233,
95.8086691804886,96.8066761511186,97.8046831217487,98.8026900923788,99.1486641472938),
 .UNSPECIFIED.);
#3898=B_SPLINE_CURVE_WITH_KNOTS('',3,(#280673,#280674,#280675,#280676,#280677,
#280678,#280679,#280680,#280681,#280682,#280683,#280684,#280685,#280686,
#280687,#280688,#280689,#280690,#280691,#280692,#280693,#280694,#280695,
#280696,#280697,#280698,#280699,#280700,#280701,#280702,#280703,#280704,
#280705,#280706,#280707,#280708,#280709,#280710,#280711,#280712,#280713,
#280714,#280715,#280716,#280717,#280718,#280719,#280720,#280721,#280722,
#280723,#280724,#280725,#280726,#280727,#280728,#280729,#280730,#280731,
#280732,#280733,#280734,#280735,#280736,#280737,#280738,#280739,#280740,
#280741,#280742,#280743,#280744,#280745,#280746,#280747,#280748,#280749,
#280750,#280751,#280752,#280753,#280754,#280755,#280756,#280757,#280758,
#280759,#280760),.UNSPECIFIED.,.F.,.F.,(4,3,3,3,3,3,3,3,3,3,3,3,3,3,3,3,
3,3,3,3,3,3,3,3,3,3,3,3,3,4),(-101.213781757955,-101.103717934714,-100.993312031664,
-100.882718756788,-100.77180592249,-100.730920097777,-100.625250669449,
-100.519739902776,-100.414353549507,-100.309033583812,-100.203744159594,
-100.098449475631,-99.9930453966476,-99.8875795787119,-99.7819355250837,
-99.7335842552244,-99.6278935405064,-99.522357699021,-99.4169407542712,
-99.3115867820018,-99.2062599780791,-99.1009245796907,-98.9954749913784,
-98.8899608557558,-98.7842646387928,-98.7362484126722,-98.6191022761829,
-98.5023548078507,-98.3862549016326,-98.3403218112339),.UNSPECIFIED.);
#3899=B_SPLINE_CURVE_WITH_KNOTS('',3,(#280762,#280763,#280764,#280765,#280766,
#280767,#280768,#280769,#280770,#280771),.UNSPECIFIED.,.F.,.F.,(4,1,1,1,
1,1,1,4),(-98.3403213565322,-97.7389125701199,-96.7415767275677,-95.7442408850154,
-94.7469050424632,-93.7495691999109,-92.7522333573587,-92.0571360493526),
 .UNSPECIFIED.);
#3900=B_SPLINE_CURVE_WITH_KNOTS('',3,(#280773,#280774,#280775,#280776,#280777,
#280778,#280779,#280780,#280781,#280782,#280783,#280784,#280785,#280786,
#280787,#280788,#280789,#280790,#280791,#280792,#280793,#280794,#280795,
#280796,#280797,#280798,#280799,#280800,#280801,#280802,#280803,#280804,
#280805,#280806,#280807,#280808,#280809,#280810,#280811,#280812,#280813,
#280814,#280815,#280816,#280817,#280818,#280819,#280820,#280821,#280822,
#280823,#280824,#280825,#280826,#280827,#280828,#280829,#280830,#280831,
#280832,#280833,#280834,#280835,#280836,#280837,#280838,#280839,#280840,
#280841,#280842,#280843,#280844,#280845,#280846,#280847,#280848,#280849,
#280850,#280851,#280852,#280853,#280854,#280855,#280856,#280857,#280858,
#280859,#280860,#280861,#280862,#280863,#280864,#280865,#280866,#280867,
#280868,#280869,#280870,#280871,#280872,#280873,#280874,#280875,#280876,
#280877,#280878,#280879,#280880,#280881,#280882,#280883,#280884,#280885,
#280886,#280887,#280888,#280889,#280890,#280891,#280892,#280893,#280894,
#280895,#280896,#280897,#280898,#280899,#280900,#280901,#280902,#280903,
#280904,#280905,#280906,#280907,#280908,#280909,#280910,#280911,#280912,
#280913,#280914,#280915,#280916,#280917,#280918,#280919,#280920,#280921,
#280922,#280923,#280924,#280925,#280926,#280927,#280928,#280929,#280930,
#280931,#280932,#280933,#280934,#280935,#280936,#280937,#280938,#280939,
#280940,#280941,#280942,#280943,#280944,#280945,#280946,#280947,#280948,
#280949,#280950,#280951,#280952,#280953,#280954,#280955,#280956,#280957,
#280958,#280959,#280960,#280961,#280962),.UNSPECIFIED.,.F.,.F.,(4,3,3,3,
3,3,3,3,3,3,3,3,3,3,3,3,3,3,3,3,3,3,3,3,3,3,3,3,3,3,3,3,3,3,3,3,3,3,3,3,
3,3,3,3,3,3,3,3,3,3,3,3,3,3,3,3,3,3,3,3,3,3,3,4),(-92.0571358644987,-91.9309798648606,
-91.8030898888977,-91.7548975148065,-91.6493896706802,-91.5440406918723,
-91.4388155855705,-91.333656423695,-91.2285270990573,-91.1233915487001,
-91.0181440166959,-90.9128334881802,-90.8073411349775,-90.7575616722542,
-90.6520546685707,-90.546706533492,-90.4414822715455,-90.3363239539049,
-90.2311954720731,-90.126060761783,-90.0208140598827,-89.9155043569929,
-89.8100128137758,-89.760225829702,-89.6547194791003,-89.54937201196,-89.444148436697,
-89.3389908169854,-89.2338630432782,-89.1287290502691,-89.0234830746453,
-88.9181741042341,-88.8126832954185,-88.7628899871497,-88.6573830323899,
-88.552034951717,-88.4468107520647,-88.3416525015875,-88.2365240916977,
-88.1313894580427,-88.0261428393948,-87.9208332236598,-87.8153417727399,
-87.7655541445975,-87.6600473539947,-87.5546994387229,-87.4494754054875,
-87.3443173219588,-87.2391890792919,-87.1340546128773,-87.0288081603432,
-86.9234987103214,-86.818007422749,-86.7682183020452,-86.6627698224436,
-86.5574801750676,-86.4523142026813,-86.3472139535958,-86.242143229031,
-86.13706587418,-86.0318764403095,-85.9266234721262,-85.8211895798944,-85.7739507426258),
 .UNSPECIFIED.);
#3901=B_SPLINE_CURVE_WITH_KNOTS('',3,(#280964,#280965,#280966,#280967,#280968,
#280969,#280970,#280971,#280972,#280973,#280974,#280975,#280976,#280977,
#280978,#280979,#280980,#280981,#280982,#280983,#280984,#280985,#280986,
#280987,#280988,#280989,#280990,#280991,#280992,#280993,#280994,#280995,
#280996,#280997,#280998,#280999,#281000,#281001,#281002,#281003,#281004,
#281005,#281006,#281007,#281008,#281009,#281010,#281011,#281012,#281013,
#281014,#281015,#281016,#281017,#281018,#281019,#281020,#281021,#281022,
#281023,#281024,#281025,#281026,#281027,#281028,#281029,#281030,#281031,
#281032,#281033,#281034,#281035,#281036,#281037,#281038,#281039,#281040,
#281041,#281042,#281043,#281044,#281045,#281046,#281047,#281048,#281049,
#281050,#281051,#281052,#281053,#281054,#281055,#281056,#281057,#281058,
#281059,#281060,#281061,#281062,#281063,#281064,#281065,#281066,#281067,
#281068,#281069,#281070,#281071,#281072,#281073,#281074,#281075,#281076,
#281077,#281078,#281079,#281080,#281081,#281082,#281083,#281084,#281085,
#281086,#281087,#281088,#281089,#281090,#281091,#281092,#281093,#281094,
#281095,#281096,#281097,#281098,#281099,#281100,#281101,#281102,#281103,
#281104,#281105,#281106,#281107,#281108,#281109,#281110,#281111,#281112,
#281113,#281114,#281115,#281116,#281117,#281118,#281119,#281120,#281121,
#281122,#281123,#281124,#281125,#281126,#281127,#281128,#281129,#281130,
#281131,#281132,#281133,#281134,#281135,#281136,#281137,#281138,#281139,
#281140,#281141,#281142,#281143,#281144,#281145,#281146,#281147,#281148,
#281149,#281150,#281151,#281152,#281153,#281154,#281155,#281156),
 .UNSPECIFIED.,.F.,.F.,(4,3,3,3,3,3,3,3,3,3,3,3,3,3,3,3,3,3,3,3,3,3,3,3,
3,3,3,3,3,3,3,3,3,3,3,3,3,3,3,3,3,3,3,3,3,3,3,3,3,3,3,3,3,3,3,3,3,3,3,3,
3,3,3,3,4),(-85.773950742173,-85.770882459493,-85.6653756550451,-85.5600277263926,
-85.4548036805353,-85.3496455848643,-85.2445173305549,-85.1393828530184,
-85.0341363902315,-84.9288269304384,-84.8233356339455,-84.7735466169407,
-84.6680398418928,-84.5626919429278,-84.4574679270362,-84.3523098614858,
-84.2471816374057,-84.142047190161,-84.0368007575523,-83.9314913279168,
-83.8260000612317,-83.7762107743885,-83.6707040065865,-83.5653561150936,
-83.4601321069731,-83.3549740493751,-83.2498458334168,-83.1447113944518,
-83.0394649703059,-82.9341555492503,-82.8286642912366,-82.7788749318363,
-82.6733681517915,-82.5680202478474,-82.4627962270287,-82.3576381565863,
-82.2525099276572,-82.147375475614,-82.042129038317,-81.9368196040492,-81.8313283328676,
-81.781539089284,-81.6760323142181,-81.5706844153093,-81.4654603995842,
-81.3603023342687,-81.2551741104917,-81.1500396636184,-81.0447932314822,
-80.9394838023778,-80.8339925363091,-80.7842032467318,-80.6786964722063,
-80.5733485738632,-80.4681245587387,-80.3629664940452,-80.2578382709107,
-80.1527038246994,-80.0474573932505,-79.9421479648487,-79.8366566994992,
-79.7868674041795,-79.6578860557949,-79.5307260217994,-79.4907656077684),
 .UNSPECIFIED.);
#3902=B_SPLINE_CURVE_WITH_KNOTS('',3,(#281158,#281159,#281160,#281161,#281162,
#281163,#281164,#281165,#281166,#281167),.UNSPECIFIED.,.F.,.F.,(4,1,1,1,
1,1,1,4),(-79.4907654349934,-78.7895315616273,-77.792195719075,-76.7948598765228,
-75.7975240339705,-74.8001881914183,-73.802852348866,-73.2075801278138),
 .UNSPECIFIED.);
#3903=B_SPLINE_CURVE_WITH_KNOTS('',3,(#281169,#281170,#281171,#281172,#281173,
#281174,#281175,#281176,#281177,#281178,#281179,#281180,#281181,#281182,
#281183,#281184,#281185,#281186,#281187,#281188,#281189,#281190,#281191,
#281192,#281193,#281194,#281195,#281196,#281197,#281198,#281199,#281200,
#281201,#281202,#281203,#281204,#281205,#281206,#281207,#281208,#281209,
#281210,#281211,#281212,#281213,#281214,#281215,#281216,#281217,#281218,
#281219,#281220,#281221,#281222,#281223,#281224,#281225,#281226,#281227,
#281228,#281229,#281230,#281231,#281232,#281233,#281234,#281235,#281236,
#281237,#281238,#281239,#281240,#281241,#281242,#281243,#281244,#281245,
#281246,#281247,#281248,#281249,#281250,#281251,#281252,#281253,#281254,
#281255,#281256,#281257,#281258,#281259,#281260,#281261,#281262,#281263,
#281264,#281265,#281266,#281267,#281268,#281269,#281270,#281271,#281272,
#281273,#281274,#281275,#281276,#281277,#281278,#281279,#281280,#281281,
#281282,#281283,#281284,#281285,#281286,#281287,#281288,#281289,#281290,
#281291,#281292,#281293,#281294,#281295,#281296,#281297,#281298,#281299,
#281300,#281301,#281302,#281303,#281304,#281305,#281306,#281307,#281308,
#281309,#281310,#281311,#281312,#281313,#281314,#281315,#281316,#281317,
#281318,#281319,#281320,#281321,#281322,#281323,#281324,#281325,#281326,
#281327,#281328,#281329,#281330,#281331,#281332,#281333,#281334,#281335,
#281336,#281337,#281338,#281339,#281340,#281341,#281342,#281343,#281344,
#281345,#281346,#281347,#281348,#281349,#281350,#281351,#281352,#281353,
#281354,#281355,#281356,#281357,#281358),.UNSPECIFIED.,.F.,.F.,(4,3,3,3,
3,3,3,3,3,3,3,3,3,3,3,3,3,3,3,3,3,3,3,3,3,3,3,3,3,3,3,3,3,3,3,3,3,3,3,3,
3,3,3,3,3,3,3,3,3,3,3,3,3,3,3,3,3,3,3,3,3,3,3,4),(-73.2075796958044,-73.0915613768673,
-72.9751283017546,-72.8581383239148,-72.8055165063138,-72.700009730801,
-72.5946618314507,-72.4894378152941,-72.3842797495539,-72.2791515253595,
-72.1740170780766,-72.068770645546,-71.9634612160551,-71.8579699496164,
-71.8081806637616,-71.7026738882456,-71.5973259888921,-71.4921019727325,
-71.3869439069892,-71.2818156827917,-71.1766812355058,-71.0714348029722,
-70.9661253734783,-70.8606341070367,-70.8108448212093,-70.7053380456898,
-70.5999901463325,-70.4947661301691,-70.389608064422,-70.2844798402206,
-70.1793453929309,-70.0740989603933,-69.9687895308954,-69.8632982644497,
-69.8135089786571,-69.7080022031405,-69.6026543037862,-69.4974302876257,
-69.3922722218816,-69.2871439976833,-69.1820095503966,-69.0767631178621,
-68.9714536883672,-68.8659624219246,-68.8161731361048,-68.7106663605875,
-68.6053184612326,-68.5000944450716,-68.3949363793268,-68.2898081551279,
-68.1846737078405,-68.0794272753054,-67.9741178458099,-67.8686265793667,
-67.8188372935526,-67.7146690912171,-67.610679764849,-67.5067899220888,
-67.4029616617978,-67.2991571716489,-67.1952770554739,-67.0913570786103,
-66.9872756614915,-66.9243948210848),.UNSPECIFIED.);
#3904=B_SPLINE_CURVE_WITH_KNOTS('',3,(#281360,#281361,#281362,#281363,#281364,
#281365,#281366,#281367,#281368,#281369,#281370,#281371,#281372,#281373,
#281374,#281375,#281376,#281377,#281378,#281379,#281380,#281381,#281382,
#281383,#281384,#281385,#281386,#281387,#281388,#281389,#281390,#281391,
#281392,#281393,#281394,#281395,#281396,#281397,#281398,#281399,#281400,
#281401,#281402,#281403,#281404,#281405,#281406,#281407,#281408,#281409,
#281410,#281411,#281412,#281413,#281414,#281415,#281416,#281417,#281418,
#281419,#281420,#281421,#281422,#281423,#281424,#281425,#281426,#281427,
#281428,#281429,#281430,#281431,#281432,#281433,#281434,#281435,#281436,
#281437,#281438,#281439,#281440,#281441,#281442,#281443,#281444,#281445,
#281446,#281447,#281448,#281449,#281450,#281451,#281452,#281453,#281454,
#281455,#281456,#281457,#281458,#281459,#281460,#281461,#281462,#281463,
#281464,#281465,#281466,#281467,#281468,#281469,#281470,#281471,#281472,
#281473,#281474,#281475,#281476,#281477,#281478,#281479,#281480,#281481,
#281482,#281483,#281484,#281485,#281486,#281487,#281488,#281489,#281490,
#281491,#281492,#281493,#281494,#281495,#281496,#281497,#281498,#281499,
#281500,#281501,#281502,#281503,#281504,#281505,#281506,#281507,#281508,
#281509,#281510,#281511,#281512,#281513,#281514,#281515,#281516,#281517,
#281518,#281519,#281520,#281521,#281522,#281523,#281524,#281525,#281526,
#281527,#281528,#281529,#281530,#281531,#281532,#281533,#281534,#281535,
#281536,#281537,#281538,#281539,#281540,#281541,#281542,#281543,#281544,
#281545,#281546,#281547,#281548,#281549),.UNSPECIFIED.,.F.,.F.,(4,3,3,3,
3,3,3,3,3,3,3,3,3,3,3,3,3,3,3,3,3,3,3,3,3,3,3,3,3,3,3,3,3,3,3,3,3,3,3,3,
3,3,3,3,3,3,3,3,3,3,3,3,3,3,3,3,3,3,3,3,3,3,3,4),(-66.9243948206342,-66.8215014510004,
-66.7159946754828,-66.6106467761274,-66.5054227599659,-66.4002646942207,
-66.2951364700213,-66.1900020227335,-66.0847555901979,-65.979446160702,
-65.8739548942583,-65.8241656084481,-65.7186588329308,-65.6133109335758,
-65.5080869174147,-65.4029288516699,-65.2978006274709,-65.1926661801835,
-65.0874197476483,-64.9821103181527,-64.8766190517094,-64.8268297658959,
-64.7213229903785,-64.6159750910234,-64.5107510748621,-64.4055930091172,
-64.3004647849181,-64.1953303376305,-64.0900839050952,-63.9847744755996,
-63.8792832091562,-63.8294939233436,-63.7239871478262,-63.6186392484711,
-63.5134152323099,-63.4082571665649,-63.3031289423658,-63.1979944950782,
-63.0927480625429,-62.9874386330473,-62.8819473666039,-62.8321580807914,
-62.726651305274,-62.6213034059189,-62.5160793897577,-62.4109213240128,
-62.3057930998137,-62.2006586525262,-62.0954122199908,-61.9901027904952,
-61.8846115240518,-61.8348222382391,-61.7293154627217,-61.6239675633666,
-61.5187435472054,-61.4135854814605,-61.3084572572614,-61.203322809974,
-61.0980763774386,-60.992766947943,-60.8872756814996,-60.8374863956869,
-60.6852066800683,-60.6412095134546),.UNSPECIFIED.);
#3905=B_SPLINE_CURVE_WITH_KNOTS('',3,(#281551,#281552,#281553,#281554,#281555,
#281556,#281557,#281558,#281559,#281560),.UNSPECIFIED.,.F.,.F.,(4,1,1,1,
1,1,1,4),(-60.6412060868095,-59.8401505531347,-58.8428147105824,-57.8454788680302,
-56.8481430254779,-55.8508071829257,-54.8534713403734,-54.3580242062751),
 .UNSPECIFIED.);
#3906=B_SPLINE_CURVE_WITH_KNOTS('',3,(#281562,#281563,#281564,#281565,#281566,
#281567,#281568,#281569,#281570,#281571),.UNSPECIFIED.,.F.,.F.,(4,1,1,1,
1,1,1,4),(-54.3580242062751,-53.8561354978212,-52.8587996552689,-51.8614638127167,
-50.8641279701645,-49.8667921276122,-48.86945628506,-48.0748417259287),
 .UNSPECIFIED.);
#3907=B_SPLINE_CURVE_WITH_KNOTS('',3,(#281573,#281574,#281575,#281576,#281577,
#281578,#281579,#281580,#281581,#281582,#281583,#281584,#281585,#281586,
#281587,#281588,#281589,#281590,#281591,#281592,#281593,#281594,#281595,
#281596,#281597,#281598,#281599,#281600,#281601,#281602,#281603,#281604,
#281605,#281606,#281607,#281608,#281609,#281610,#281611,#281612,#281613,
#281614,#281615,#281616,#281617,#281618,#281619,#281620,#281621,#281622,
#281623,#281624,#281625,#281626,#281627,#281628,#281629,#281630,#281631,
#281632,#281633,#281634,#281635,#281636,#281637,#281638,#281639,#281640,
#281641,#281642,#281643,#281644,#281645,#281646,#281647,#281648,#281649,
#281650,#281651,#281652,#281653,#281654,#281655,#281656,#281657,#281658,
#281659,#281660,#281661,#281662,#281663,#281664,#281665,#281666,#281667,
#281668,#281669,#281670,#281671,#281672,#281673,#281674,#281675,#281676,
#281677,#281678,#281679,#281680,#281681,#281682,#281683,#281684,#281685,
#281686,#281687,#281688,#281689,#281690,#281691,#281692,#281693,#281694,
#281695,#281696,#281697,#281698,#281699,#281700,#281701,#281702,#281703,
#281704,#281705,#281706,#281707,#281708,#281709,#281710,#281711,#281712,
#281713,#281714,#281715,#281716,#281717,#281718,#281719,#281720,#281721,
#281722,#281723,#281724,#281725,#281726,#281727,#281728,#281729,#281730,
#281731,#281732,#281733,#281734,#281735,#281736,#281737,#281738,#281739,
#281740,#281741,#281742,#281743,#281744,#281745,#281746,#281747,#281748,
#281749,#281750,#281751,#281752,#281753,#281754,#281755,#281756,#281757,
#281758,#281759,#281760,#281761,#281762),.UNSPECIFIED.,.F.,.F.,(4,3,3,3,
3,3,3,3,3,3,3,3,3,3,3,3,3,3,3,3,3,3,3,3,3,3,3,3,3,3,3,3,3,3,3,3,3,3,3,3,
3,3,3,3,3,3,3,3,3,3,3,3,3,3,3,3,3,3,3,3,3,3,3,4),(-48.0748388990955,-47.9250099117185,
-47.8721204425077,-47.7666136669904,-47.6612657676354,-47.5560417514743,
-47.4508836857296,-47.3457554615306,-47.2406210142432,-47.135374581708,
-47.0300651522125,-46.9245738857692,-46.8747845999555,-46.769277824438,
-46.6639299250828,-46.5587059089216,-46.4535478431766,-46.3484196189775,
-46.2432851716899,-46.1380387391545,-46.0327293096589,-45.9272380432155,
-45.8774487574032,-45.7719419818858,-45.6665940825307,-45.5613700663695,
-45.4562120006246,-45.3510837764254,-45.2459493291379,-45.1407028966025,
-45.0353934671069,-44.9299022006635,-44.880112914851,-44.7746061393336,
-44.6692582399785,-44.5640342238173,-44.4588761580724,-44.3537479338733,
-44.2486134865857,-44.1433670540504,-44.0380576245548,-43.9325663581114,
-43.8827770722987,-43.7772702967813,-43.6719223974262,-43.566698381265,
-43.46154031552,-43.3564120913209,-43.2512776440333,-43.146031211498,-43.0407217820023,
-42.9352305155589,-42.8854412297465,-42.779934454229,-42.674586554874,-42.5693625387129,
-42.4642044729679,-42.3590762487688,-42.2539418014812,-42.1486953689459,
-42.0433859394503,-41.9378946730069,-41.8881053871943,-41.7916535919159),
 .UNSPECIFIED.);
#3908=B_SPLINE_CURVE_WITH_KNOTS('',3,(#281764,#281765,#281766,#281767,#281768,
#281769,#281770,#281771,#281772,#281773),.UNSPECIFIED.,.F.,.F.,(4,1,1,1,
1,1,1,4),(-41.7916448313401,-40.890769544642,-39.8934337020898,-38.8960978595375,
-37.8987620169853,-36.901426174433,-35.9040903318808,-35.5084682847363),
 .UNSPECIFIED.);
#3909=B_SPLINE_CURVE_WITH_KNOTS('',3,(#281775,#281776,#281777,#281778,#281779,
#281780,#281781,#281782,#281783,#281784),.UNSPECIFIED.,.F.,.F.,(4,1,1,1,
1,1,1,4),(-35.5084682847363,-34.9067544893285,-33.9094186467763,-32.9120828042241,
-31.9147469616718,-30.9174111191196,-29.9200752765673,-29.2252829775567),
 .UNSPECIFIED.);
#3910=B_SPLINE_CURVE_WITH_KNOTS('',3,(#281786,#281787,#281788,#281789,#281790,
#281791,#281792,#281793,#281794,#281795,#281796,#281797,#281798,#281799,
#281800,#281801,#281802,#281803,#281804,#281805,#281806,#281807,#281808,
#281809,#281810,#281811,#281812,#281813,#281814,#281815,#281816,#281817,
#281818,#281819,#281820,#281821,#281822,#281823,#281824,#281825,#281826,
#281827,#281828,#281829,#281830,#281831,#281832,#281833,#281834,#281835,
#281836,#281837,#281838,#281839,#281840,#281841,#281842,#281843,#281844,
#281845,#281846,#281847,#281848,#281849,#281850,#281851,#281852,#281853,
#281854,#281855,#281856,#281857,#281858,#281859,#281860,#281861,#281862,
#281863,#281864,#281865,#281866,#281867,#281868,#281869,#281870,#281871,
#281872,#281873,#281874,#281875,#281876,#281877,#281878,#281879,#281880,
#281881,#281882,#281883,#281884,#281885,#281886,#281887,#281888,#281889,
#281890,#281891,#281892,#281893,#281894,#281895,#281896,#281897,#281898,
#281899,#281900,#281901,#281902,#281903,#281904,#281905,#281906,#281907,
#281908,#281909,#281910,#281911,#281912,#281913,#281914,#281915,#281916,
#281917,#281918,#281919,#281920,#281921,#281922,#281923,#281924,#281925,
#281926,#281927,#281928,#281929,#281930,#281931,#281932,#281933,#281934,
#281935,#281936,#281937,#281938,#281939,#281940,#281941,#281942,#281943,
#281944,#281945,#281946,#281947,#281948,#281949,#281950,#281951,#281952,
#281953,#281954,#281955,#281956,#281957,#281958,#281959,#281960,#281961,
#281962,#281963,#281964,#281965,#281966,#281967,#281968,#281969,#281970,
#281971,#281972,#281973,#281974,#281975),.UNSPECIFIED.,.F.,.F.,(4,3,3,3,
3,3,3,3,3,3,3,3,3,3,3,3,3,3,3,3,3,3,3,3,3,3,3,3,3,3,3,3,3,3,3,3,3,3,3,3,
3,3,3,3,3,3,3,3,3,3,3,3,3,3,3,3,3,3,3,3,3,3,3,4),(-29.2252827921887,-29.0991630781067,
-28.9713146182254,-28.9227394340151,-28.8172326585138,-28.7118847591747,
-28.6066607430293,-28.5015026773,-28.3963744531164,-28.291240005844,-28.1859935733236,
-28.0806841438427,-27.9751928774136,-27.9254035914628,-27.8198968159696,
-27.7145489166391,-27.6093249005027,-27.5041668347828,-27.3990386106088,
-27.2939041633464,-27.1886577308362,-27.0833483013658,-26.9778570349473,
-26.9280677489106,-26.8225609732847,-26.717213073821,-26.6119890575513,
-26.506830991698,-26.4017027673908,-26.2965683199958,-26.1913218873543,
-26.0860124577533,-25.9805211912066,-25.9307319063583,-25.825225130977,
-25.7198772317575,-25.6146532157305,-25.5094951501189,-25.404366926052,
-25.2992324788953,-25.193986046488,-25.088676617119,-24.9831853507987,-24.9333960638061,
-24.8278892884005,-24.7225413891591,-24.6173173731139,-24.5121593074863,
-24.4070310834057,-24.3018966362376,-24.1966502038223,-24.0913407744472,
-23.9858495081238,-23.9360602212539,-23.8306174073625,-23.7253334200811,
-23.6201730861378,-23.5150784524654,-23.4100133116324,-23.3049415001546,
-23.1997576017589,-23.0945101162213,-22.9890817997621,-22.942097670868),
 .UNSPECIFIED.);
#3911=B_SPLINE_CURVE_WITH_KNOTS('',3,(#281977,#281978,#281979,#281980,#281981,
#281982,#281983,#281984,#281985,#281986,#281987,#281988,#281989,#281990,
#281991,#281992,#281993,#281994,#281995,#281996,#281997,#281998,#281999,
#282000,#282001,#282002,#282003,#282004,#282005,#282006,#282007,#282008,
#282009,#282010,#282011,#282012,#282013,#282014,#282015,#282016,#282017,
#282018,#282019,#282020,#282021,#282022,#282023,#282024,#282025,#282026,
#282027,#282028,#282029,#282030,#282031,#282032,#282033,#282034,#282035,
#282036,#282037,#282038,#282039,#282040,#282041,#282042,#282043,#282044,
#282045,#282046,#282047,#282048,#282049,#282050,#282051,#282052,#282053,
#282054,#282055,#282056,#282057,#282058,#282059,#282060,#282061,#282062,
#282063,#282064,#282065,#282066,#282067,#282068,#282069,#282070,#282071,
#282072,#282073,#282074,#282075,#282076,#282077,#282078,#282079,#282080,
#282081,#282082,#282083,#282084,#282085,#282086,#282087,#282088,#282089,
#282090,#282091,#282092,#282093,#282094,#282095,#282096,#282097,#282098,
#282099,#282100,#282101,#282102,#282103,#282104,#282105,#282106,#282107,
#282108,#282109,#282110,#282111,#282112,#282113,#282114,#282115,#282116,
#282117,#282118,#282119,#282120,#282121,#282122,#282123,#282124,#282125,
#282126,#282127,#282128,#282129,#282130,#282131,#282132,#282133,#282134,
#282135,#282136,#282137,#282138,#282139,#282140,#282141,#282142,#282143,
#282144,#282145,#282146,#282147,#282148,#282149,#282150,#282151,#282152,
#282153,#282154,#282155,#282156,#282157,#282158,#282159,#282160,#282161,
#282162,#282163,#282164,#282165,#282166,#282167,#282168,#282169),
 .UNSPECIFIED.,.F.,.F.,(4,3,3,3,3,3,3,3,3,3,3,3,3,3,3,3,3,3,3,3,3,3,3,3,
3,3,3,3,3,3,3,3,3,3,3,3,3,3,3,3,3,3,3,3,3,3,3,3,3,3,3,3,3,3,3,3,3,3,3,3,
3,3,3,3,4),(-22.9420976703771,-22.9387243787016,-22.8332176042749,-22.7278697060081,
-22.6226456909265,-22.517487626255,-22.4123594031217,-22.3072249568909,
-22.2019785253912,-22.0966690969209,-21.9911778314761,-21.9413885361494,
-21.8358817610032,-21.7305338620323,-21.6253098462723,-21.5201517809389,
-21.4150235571609,-21.3098891103034,-21.2046426782084,-21.0993332491597,
-20.9938419831684,-20.9440526935971,-20.8385459133601,-20.7331980092675,
-20.6279739883655,-20.5228159178805,-20.417687688949,-20.3125532369439,
-20.2073067997456,-20.1019973656113,-19.9965060946152,-19.9467168510449,
-19.8412100839312,-19.7358621929697,-19.6306381851473,-19.5254801277023,
-19.4203519117524,-19.3152174726511,-19.2099710481519,-19.1046616266188,
-18.9991703679413,-18.9493810084926,-18.8438742327198,-18.7385263331949,
-18.6333023169894,-18.5281442512778,-18.4230160271889,-18.3178815800877,
-18.212635147851,-18.1073257187186,-18.0018344527325,-17.9520451659404,
-17.8465383604957,-17.741190431073,-17.635966384784,-17.5308082888913,-17.4256800345698,
-17.3205455572306,-17.2152990949553,-17.1099896358541,-17.0044983403225,
-16.9547093233881,-16.8256794531442,-16.6984772039481,-16.6589125353486),
 .UNSPECIFIED.);
#3912=B_SPLINE_CURVE_WITH_KNOTS('',3,(#282171,#282172,#282173,#282174,#282175,
#282176,#282177,#282178,#282179,#282180),.UNSPECIFIED.,.F.,.F.,(4,1,1,1,
1,1,1,4),(-16.6589123631975,-15.9573734808359,-14.9600376382837,-13.9627017957314,
-12.9653659531792,-11.9680301106269,-10.9706942680747,-10.3757270560179),
 .UNSPECIFIED.);
#3913=B_SPLINE_CURVE_WITH_KNOTS('',3,(#282181,#282182,#282183,#282184,#282185,
#282186,#282187,#282188,#282189,#282190),.UNSPECIFIED.,.F.,.F.,(4,1,1,1,
1,1,1,4),(-10.3757270560179,-9.97335842552244,-8.9760225829702,-7.97868674041795,
-6.9813508978657,-5.98401505531347,-4.98667921276122,-4.09255056054366),
 .UNSPECIFIED.);
#3914=B_SPLINE_CURVE_WITH_KNOTS('',3,(#282194,#282195,#282196,#282197,#282198,
#282199,#282200,#282201,#282202,#282203,#282204,#282205,#282206,#282207,
#282208,#282209,#282210,#282211,#282212,#282213,#282214,#282215,#282216,
#282217,#282218,#282219,#282220,#282221,#282222,#282223,#282224,#282225,
#282226,#282227,#282228,#282229,#282230,#282231,#282232,#282233,#282234,
#282235,#282236,#282237,#282238,#282239,#282240,#282241,#282242,#282243,
#282244,#282245,#282246,#282247,#282248,#282249,#282250,#282251,#282252,
#282253,#282254,#282255,#282256,#282257,#282258,#282259,#282260,#282261,
#282262,#282263,#282264,#282265,#282266,#282267,#282268,#282269,#282270,
#282271,#282272,#282273,#282274,#282275,#282276,#282277,#282278,#282279,
#282280,#282281,#282282,#282283,#282284,#282285,#282286,#282287,#282288,
#282289,#282290,#282291,#282292,#282293,#282294,#282295,#282296,#282297,
#282298,#282299,#282300,#282301,#282302,#282303,#282304,#282305,#282306,
#282307,#282308,#282309,#282310,#282311,#282312,#282313,#282314),
 .UNSPECIFIED.,.F.,.F.,(4,3,3,3,3,3,3,3,3,3,3,3,3,3,3,3,3,3,3,3,3,3,3,3,
3,3,3,3,3,3,3,3,3,3,3,3,3,3,3,3,4),(109.955742876009,110.078760970684,110.202268469162,
110.326390822107,110.351669931783,110.463583938193,110.575297619248,110.686899193039,
110.798431239825,110.909936241335,111.021537194555,111.133181961873,111.245037630442,
111.349005774335,111.460864169076,111.572528019857,111.68408329714,111.795572614607,
111.907038491634,112.018606201699,112.130220888686,112.242052138939,112.346341616887,
112.456818232952,112.567675636263,112.677845964136,112.787951966345,112.898038209298,
113.009448021833,113.119706546789,113.231692003114,113.343677459439,113.458507052372,
113.573089536432,113.687526101063,113.801851673508,113.916101021905,114.030343155428,
114.144573216633,114.258887551681,114.341013301992),.UNSPECIFIED.);
#3915=B_SPLINE_CURVE_WITH_KNOTS('',3,(#282318,#282319,#282320,#282321,#282322,
#282323,#282324,#282325,#282326,#282327,#282328,#282329,#282330,#282331,
#282332,#282333,#282334,#282335,#282336,#282337,#282338,#282339,#282340,
#282341,#282342,#282343,#282344,#282345,#282346,#282347,#282348,#282349,
#282350,#282351,#282352,#282353,#282354,#282355,#282356,#282357,#282358,
#282359,#282360,#282361,#282362,#282363,#282364,#282365,#282366,#282367,
#282368,#282369,#282370,#282371,#282372,#282373,#282374,#282375,#282376,
#282377,#282378,#282379,#282380,#282381,#282382,#282383,#282384,#282385,
#282386,#282387,#282388,#282389,#282390,#282391,#282392,#282393,#282394,
#282395,#282396,#282397,#282398,#282399,#282400,#282401,#282402),
 .UNSPECIFIED.,.F.,.F.,(4,3,3,3,3,3,3,3,3,3,3,3,3,3,3,3,3,3,3,3,3,3,3,3,
3,3,3,3,4),(109.955742875643,110.107297927009,110.219145865768,110.330798976391,
110.442343339323,110.553821588649,110.665276263946,110.776832873734,110.888436368332,
111.000257029606,111.105304897639,111.215771188973,111.326713773885,111.436873242123,
111.546968257781,111.657043400247,111.768610517253,111.878858070651,111.99108496946,
112.103311868269,112.218136295745,112.332713184882,112.447143914003,112.561463435156,
112.675706541026,112.789942338138,112.904165931924,113.018474048525,113.101318838899),
 .UNSPECIFIED.);
#3916=B_SPLINE_CURVE_WITH_KNOTS('',3,(#282404,#282405,#282406,#282407,#282408,
#282409,#282410,#282411,#282412,#282413,#282414,#282415,#282416,#282417,
#282418,#282419,#282420,#282421,#282422,#282423,#282424,#282425,#282426,
#282427,#282428,#282429,#282430,#282431,#282432,#282433,#282434,#282435,
#282436,#282437,#282438,#282439,#282440,#282441,#282442,#282443,#282444,
#282445,#282446,#282447,#282448,#282449,#282450,#282451,#282452,#282453,
#282454,#282455,#282456,#282457,#282458,#282459,#282460,#282461,#282462,
#282463,#282464,#282465,#282466,#282467,#282468,#282469,#282470,#282471,
#282472,#282473,#282474,#282475,#282476,#282477,#282478,#282479,#282480,
#282481,#282482,#282483,#282484,#282485,#282486,#282487,#282488,#282489,
#282490,#282491,#282492,#282493,#282494,#282495,#282496,#282497,#282498,
#282499,#282500,#282501,#282502,#282503,#282504,#282505,#282506,#282507,
#282508,#282509,#282510,#282511,#282512,#282513,#282514,#282515,#282516,
#282517,#282518,#282519,#282520,#282521,#282522,#282523,#282524,#282525,
#282526,#282527,#282528,#282529,#282530,#282531,#282532,#282533,#282534,
#282535,#282536,#282537,#282538,#282539,#282540,#282541,#282542,#282543,
#282544,#282545,#282546,#282547,#282548,#282549,#282550,#282551,#282552,
#282553,#282554,#282555,#282556,#282557,#282558,#282559,#282560,#282561,
#282562,#282563,#282564,#282565,#282566,#282567,#282568,#282569,#282570,
#282571,#282572,#282573,#282574,#282575,#282576,#282577,#282578,#282579,
#282580,#282581,#282582,#282583,#282584,#282585,#282586,#282587,#282588,
#282589,#282590,#282591,#282592,#282593,#282594,#282595,#282596,#282597,
#282598,#282599,#282600,#282601,#282602,#282603,#282604,#282605,#282606,
#282607,#282608,#282609,#282610,#282611,#282612,#282613,#282614,#282615,
#282616,#282617,#282618,#282619,#282620,#282621,#282622,#282623,#282624,
#282625,#282626,#282627,#282628,#282629,#282630,#282631,#282632,#282633,
#282634,#282635,#282636,#282637,#282638,#282639,#282640,#282641,#282642,
#282643,#282644,#282645,#282646,#282647,#282648,#282649,#282650,#282651,
#282652,#282653,#282654,#282655,#282656,#282657,#282658,#282659,#282660,
#282661,#282662,#282663,#282664,#282665,#282666,#282667,#282668,#282669,
#282670,#282671,#282672,#282673,#282674,#282675,#282676,#282677,#282678,
#282679,#282680,#282681,#282682,#282683,#282684,#282685,#282686,#282687,
#282688,#282689,#282690,#282691,#282692,#282693,#282694,#282695,#282696,
#282697,#282698,#282699,#282700,#282701,#282702,#282703,#282704,#282705,
#282706,#282707,#282708,#282709,#282710,#282711,#282712,#282713,#282714,
#282715,#282716,#282717,#282718,#282719,#282720,#282721,#282722,#282723,
#282724,#282725,#282726,#282727,#282728,#282729,#282730,#282731,#282732,
#282733,#282734,#282735,#282736,#282737,#282738,#282739,#282740,#282741,
#282742,#282743,#282744,#282745,#282746,#282747,#282748,#282749,#282750,
#282751,#282752,#282753,#282754,#282755,#282756,#282757,#282758,#282759,
#282760,#282761,#282762,#282763,#282764,#282765,#282766,#282767,#282768,
#282769,#282770,#282771,#282772,#282773,#282774,#282775,#282776,#282777,
#282778,#282779,#282780,#282781,#282782,#282783,#282784,#282785,#282786,
#282787,#282788,#282789,#282790,#282791,#282792,#282793,#282794,#282795,
#282796,#282797,#282798,#282799,#282800,#282801,#282802,#282803,#282804,
#282805,#282806,#282807,#282808,#282809,#282810,#282811,#282812,#282813,
#282814,#282815,#282816,#282817,#282818,#282819,#282820,#282821,#282822,
#282823,#282824,#282825,#282826,#282827,#282828,#282829,#282830,#282831,
#282832,#282833,#282834,#282835,#282836,#282837,#282838,#282839,#282840,
#282841,#282842,#282843,#282844,#282845,#282846,#282847,#282848,#282849,
#282850,#282851,#282852,#282853,#282854,#282855,#282856,#282857,#282858,
#282859),.UNSPECIFIED.,.F.,.F.,(4,2,2,2,2,2,2,2,2,2,2,2,2,2,2,2,2,2,2,2,
2,2,2,2,2,2,2,2,2,2,2,2,2,2,2,2,2,2,2,2,2,2,2,2,2,2,2,2,2,2,2,2,2,2,2,2,
2,2,2,2,2,2,2,2,2,2,2,2,2,2,2,2,2,2,2,2,2,2,2,2,2,2,2,2,2,2,2,2,2,2,2,2,
2,2,2,2,2,2,2,2,2,2,2,2,2,2,2,2,2,2,2,2,2,2,2,2,2,2,2,2,2,2,2,2,2,2,2,2,
2,2,2,2,2,2,2,2,2,2,2,2,2,2,2,2,2,2,2,2,2,2,2,2,2,2,2,2,2,2,2,2,2,2,2,2,
2,2,2,2,2,2,2,2,2,2,2,2,2,2,2,2,2,2,2,2,2,2,2,2,2,2,2,2,2,2,2,2,2,2,2,2,
2,2,2,2,2,2,2,2,2,2,2,2,2,2,2,2,2,2,2,2,2,2,2,2,2,2,2,4),(-1.96134596005299,
-1.92320411814298,-1.91683960670163,-1.91154752211252,-1.90834736782571,
-1.90543887769198,-1.9017168444316,-1.8955077480057,-1.86854562523828,-1.84488691487139,
-1.83762076146846,-1.83266440438021,-1.8305683353551,-1.83054834816283,
-1.8305282948152,-1.83050816978186,-1.83048796743229,-1.83047723424409,
-1.83046617358847,-1.83045476969429,-1.83044300574037,-1.83043086377228,
-1.83041832460025,-1.83040536769386,-1.8303919710629,-1.83037811111419,
-1.8303637625119,-1.83034889800978,-1.83033348826399,-1.83031750162281,
-1.83030090390035,-1.83028365811244,-1.83026572417907,-1.83024705859217,
-1.83022761404223,-1.83020733898793,-1.83018617716757,-1.8301640670428,
-1.83014094116354,-1.83011672543508,-1.8300913382757,-1.83006468964201,
-1.8284526754288,-1.8264457735443,-1.82235816897249,-1.79077011051556,-1.76553775262294,
-1.7573219564942,-1.7535727113588,-1.75069959681956,-1.7475469720678,-1.74235672037468,
-1.72233557364014,-1.69064080275324,-1.68234815384251,-1.67680439251776,
-1.67454359080352,-1.672913372592,-1.67108432296876,-1.66789420722315,-1.65411530591151,
-1.62545396231887,-1.60438173959295,-1.59923069395448,-1.59606587313137,
-1.59315723073407,-1.58938973360294,-1.58096195077707,-1.54495366279498,
-1.52530106324672,-1.52081365134075,-1.51871775183872,-1.51724866878963,
-1.51536381669079,-1.51201245900382,-1.49263831275019,-1.48758275217834,
-1.46794352165621,-1.45518117515106,-1.44622697242567,-1.4423342171477,
-1.43942190336144,-1.43629335230179,-1.43129169887772,-1.41443617471032,
-1.38513100777365,-1.37323544586131,-1.3683748068879,-1.36465257411225,
-1.3627117363032,-1.36109385065202,-1.35900075764574,-1.35465118897059,
-1.32723765149952,-1.30478008218077,-1.29178536072229,-1.28733172389266,
-1.28432061417718,-1.28138232148989,-1.27714935568482,-1.26672976101249,
-1.23273668958479,-1.2137184958182,-1.2093041504301,-1.20722865585897,-1.20576671583297,
-1.20387967849958,-1.20051222910936,-1.17868971868284,-1.17659051577337,
-1.14186610322758,-1.13409856059281,-1.13041214099272,-1.12752713146479,
-1.12429928864984,-1.11883185221412,-1.09220395502573,-1.06667295278604,
-1.05914007867478,-1.05396336572059,-1.05175042698459,-1.05011892086801,
-1.04825318713209,-1.04498085825219,-1.02898871799472,-0.996616895159001,
-0.980943092646712,-0.976205412111835,-0.973133641184649,-0.970197213592707,
-0.966149980218765,-0.956214815899105,-0.941425004060726,-0.923686718167545,
-0.900710994671843,-0.897327138519964,-0.895436764250386,-0.893974657300571,
-0.891902557989352,-0.887512298108303,-0.868735901791538,-0.835412908052433,
-0.824331509882609,-0.820005022489831,-0.8173158869,-0.814366000101075,
-0.8102403063064,-0.799773677160084,-0.783812236608273,-0.772087606614392,
-0.74671145522867,-0.742226637015615,-0.7401369405901,-0.738518476175967,
-0.736573031478298,-0.732829523300687,-0.727933229471062,-0.715900061524462,
-0.67691320999565,-0.667876299797195,-0.664259528026053,-0.661573746803908,
-0.658619895335551,-0.654474104214096,-0.643870446319955,-0.627598025377892,
-0.593054935535115,-0.587229332565578,-0.584849714896073,-0.583209210877953,
-0.581426327958067,-0.57844639534849,-0.566334662512619,-0.543561334604584,
-0.515213800786896,-0.509759190580938,-0.506535156382603,-0.503651296299562,
-0.499963285314192,-0.492180791509951,-0.463448410858983,-0.435129406120473,
-0.431168188777623,-0.429155087072102,-0.427512559855908,-0.425734241837209,
-0.422775021685134,-0.410950629736337,-0.387947923476124,-0.359499752004406,
-0.35404536501043,-0.350821380343177,-0.347937515683542,-0.344249432177406,
-0.336466524525731,-0.307509024143815,-0.279457032055029,-0.275095941456518,
-0.273021642336195,-0.271401699031108,-0.269470904834471,-0.26579869581264,
-0.241155611606478,-0.205636410784264,-0.199760925546063,-0.196104923614451,
-0.193224380626739,-0.18998134330574,-0.184437572184014,-0.17767642811731,
-0.162955529927346,-0.136600262176787,-0.121814639214398,-0.118576745758897,
-0.11673775303086,-0.115100380215487,-0.112839316114304,-0.107683100981236,
-0.0953527260318766,-0.065440740316503,-0.0473873156799378,-0.0422936227695306,
-0.0391465356797224,-0.0362428866832389,-0.0334015628955676,-0.029664141270674,
-0.0204810725935979,-0.000463005431037473),.UNSPECIFIED.);
#3917=B_SPLINE_CURVE_WITH_KNOTS('',3,(#282861,#282862,#282863,#282864,#282865,
#282866,#282867,#282868,#282869,#282870,#282871,#282872,#282873,#282874,
#282875,#282876,#282877,#282878,#282879,#282880,#282881,#282882,#282883,
#282884,#282885,#282886,#282887,#282888,#282889,#282890,#282891,#282892,
#282893,#282894,#282895,#282896,#282897,#282898,#282899,#282900,#282901,
#282902,#282903,#282904,#282905,#282906,#282907,#282908,#282909,#282910,
#282911,#282912,#282913,#282914,#282915,#282916,#282917,#282918,#282919,
#282920,#282921,#282922,#282923,#282924,#282925,#282926,#282927,#282928,
#282929,#282930,#282931,#282932,#282933,#282934,#282935,#282936,#282937,
#282938,#282939,#282940,#282941,#282942,#282943,#282944,#282945,#282946,
#282947,#282948,#282949,#282950,#282951,#282952,#282953,#282954,#282955,
#282956,#282957,#282958,#282959,#282960,#282961,#282962,#282963,#282964,
#282965,#282966,#282967,#282968,#282969,#282970,#282971,#282972,#282973,
#282974,#282975,#282976,#282977,#282978,#282979,#282980,#282981,#282982,
#282983,#282984,#282985,#282986,#282987,#282988,#282989,#282990,#282991,
#282992,#282993,#282994,#282995,#282996,#282997,#282998,#282999,#283000,
#283001,#283002,#283003,#283004,#283005,#283006,#283007,#283008,#283009,
#283010,#283011,#283012,#283013,#283014,#283015,#283016,#283017,#283018,
#283019,#283020,#283021,#283022,#283023,#283024,#283025,#283026,#283027,
#283028,#283029,#283030,#283031,#283032,#283033,#283034,#283035,#283036,
#283037,#283038,#283039,#283040,#283041,#283042,#283043,#283044,#283045,
#283046,#283047,#283048,#283049,#283050,#283051,#283052,#283053,#283054,
#283055,#283056,#283057,#283058,#283059,#283060,#283061,#283062,#283063,
#283064,#283065,#283066,#283067,#283068,#283069,#283070,#283071,#283072,
#283073,#283074,#283075,#283076,#283077,#283078,#283079,#283080,#283081,
#283082,#283083,#283084,#283085,#283086,#283087,#283088,#283089,#283090,
#283091,#283092,#283093,#283094,#283095,#283096,#283097,#283098,#283099,
#283100,#283101,#283102,#283103,#283104,#283105,#283106,#283107,#283108,
#283109,#283110,#283111,#283112,#283113,#283114,#283115,#283116,#283117,
#283118,#283119,#283120,#283121,#283122,#283123,#283124,#283125,#283126,
#283127,#283128,#283129,#283130,#283131,#283132,#283133,#283134,#283135,
#283136,#283137,#283138,#283139,#283140,#283141,#283142,#283143,#283144,
#283145,#283146,#283147,#283148,#283149,#283150,#283151,#283152,#283153,
#283154,#283155,#283156,#283157,#283158,#283159,#283160,#283161,#283162,
#283163,#283164,#283165,#283166,#283167,#283168,#283169,#283170,#283171,
#283172,#283173,#283174,#283175,#283176,#283177,#283178,#283179,#283180,
#283181,#283182,#283183,#283184,#283185,#283186,#283187,#283188,#283189,
#283190,#283191,#283192,#283193,#283194,#283195,#283196,#283197,#283198,
#283199,#283200,#283201,#283202,#283203,#283204,#283205,#283206,#283207,
#283208,#283209,#283210,#283211,#283212,#283213,#283214,#283215,#283216,
#283217,#283218,#283219,#283220,#283221,#283222,#283223,#283224,#283225,
#283226,#283227,#283228,#283229,#283230,#283231,#283232,#283233,#283234,
#283235,#283236,#283237,#283238,#283239,#283240,#283241,#283242,#283243,
#283244,#283245,#283246,#283247,#283248,#283249,#283250,#283251,#283252,
#283253,#283254,#283255,#283256,#283257,#283258,#283259,#283260,#283261,
#283262,#283263,#283264,#283265,#283266,#283267,#283268,#283269,#283270),
 .UNSPECIFIED.,.F.,.F.,(4,2,2,2,2,2,2,2,2,2,2,2,2,2,2,2,2,2,2,2,2,2,2,2,
2,2,2,2,2,2,2,2,2,2,2,2,2,2,2,2,2,2,2,2,2,2,2,2,2,2,2,2,2,2,2,2,2,2,2,2,
2,2,2,2,2,2,2,2,2,2,2,2,2,2,2,2,2,2,2,2,2,2,2,2,2,2,2,2,2,2,2,2,2,2,2,2,
2,2,2,2,2,2,2,2,2,2,2,2,2,2,2,2,2,2,2,2,2,2,2,2,2,2,2,2,2,2,2,2,2,2,2,2,
2,2,2,2,2,2,2,2,2,2,2,2,2,2,2,2,2,2,2,2,2,2,2,2,2,2,2,2,2,2,2,2,2,2,2,2,
2,2,2,2,2,2,2,2,2,2,2,2,2,2,2,2,2,2,2,2,2,2,2,2,2,2,2,2,2,2,2,2,2,2,2,2,
4),(-1.96120734884475,-1.9329238431295,-1.92667649358171,-1.92437579718932,
-1.92229554106251,-1.9208322559288,-1.91894674504486,-1.91558579958792,
-1.89528526779122,-1.87075070958967,-1.858404189914,-1.84972955769284,-1.84639177994775,
-1.84626159504513,-1.84330472034741,-1.84062121064667,-1.83633017915434,
-1.82548973911512,-1.79188859446564,-1.77303102016817,-1.76863157585871,
-1.76655737062743,-1.76509469171669,-1.76320480983605,-1.75982450482497,
-1.73702634591811,-1.7206009200413,-1.70491571735483,-1.69457053622545,
-1.69046174975455,-1.68751414035074,-1.6848204109009,-1.68117215023371,
-1.67194460135601,-1.6367915999586,-1.61738290890347,-1.61292578684856,
-1.61084073384937,-1.60937677950044,-1.60749420773741,-1.60414694482114,
-1.58488300835589,-1.57970580741659,-1.56010318720656,-1.5472847507949,
-1.53830134796716,-1.53440425422268,-1.53149184037439,-1.52836618116202,
-1.52337576495278,-1.50662913013879,-1.47727856090541,-1.46536708414599,
-1.46050209442759,-1.45677709057786,-1.45483513064317,-1.45321573506028,
-1.45111997344099,-1.44676426747682,-1.41940490170312,-1.38976620635212,
-1.38198121136441,-1.37829205976953,-1.37540729993235,-1.37218224883767,
-1.36672592128419,-1.34027543909824,-1.31453990499003,-1.30697708430465,
-1.30178545639366,-1.29957059756044,-1.29793924070412,-1.29607523132558,
-1.29281081948795,-1.27696416726496,-1.24444733640245,-1.23396687477194,
-1.22621395142566,-1.22253070620007,-1.21964663969088,-1.21641829728009,
-1.21094630695213,-1.18311210488112,-1.16224886602917,-1.15260080918932,
-1.14641719771057,-1.14404695780121,-1.14239155104824,-1.14059925148802,
-1.13757750717473,-1.12633829925246,-1.10054391131459,-1.07425651506294,
-1.06887963822924,-1.06567162317512,-1.06278356410061,-1.05906428590169,
-1.05297115287619,-1.02111195357638,-1.0013550692677,-0.994760077100172,
-0.99006839098625,-0.987940449308012,-0.98631864991227,-0.98440053068455,
-0.980893014534244,-0.97632415142728,-0.96551627018509,-0.945661041918234,
-0.918736154539604,-0.913242132500549,-0.910009144249384,-0.907125986544771,
-0.903450860705764,-0.895742150169642,-0.871074096063297,-0.841490466330516,
-0.83514536694182,-0.832681400236937,-0.831025145846189,-0.829270101650238,
-0.826418642658594,-0.815961227994418,-0.793624806352471,-0.765301062795747,
-0.759142627897215,-0.75544464476572,-0.752551466028968,-0.749364887114753,
-0.74408873931067,-0.720431312819312,-0.704612959536957,-0.683027746355497,
-0.678507793107124,-0.676433296073625,-0.67481299648718,-0.672881537754907,
-0.669207363183667,-0.644521082435461,-0.60904438395258,-0.603161725466596,
-0.599503219248634,-0.596621883103081,-0.593379192026751,-0.587839148554125,
-0.581084255662564,-0.566386363253881,-0.548560040894815,-0.525525655533315,
-0.522139797522101,-0.520248673530019,-0.51878614718332,-0.516713646364208,
-0.512323367469958,-0.493553197717968,-0.46025074687675,-0.449140509524315,
-0.444808905899923,-0.442118252962409,-0.439168014203132,-0.435044290600442,
-0.424596762445513,-0.408680132398467,-0.395862891421224,-0.371586283713681,
-0.367044232170259,-0.364965811513034,-0.363345303031543,-0.361417090005063,
-0.357758227958913,-0.333559770008304,-0.297465914562447,-0.291641819487452,
-0.28800049790867,-0.285121041270967,-0.281868162201887,-0.276279389102895,
-0.269448017855639,-0.254489214986801,-0.243075181732033,-0.21564181305878,
-0.211289441117452,-0.209194544093134,-0.207575456175351,-0.205633407976656,
-0.201907048880401,-0.197040053874561,-0.185119963380706,-0.147163725848762,
-0.137243040984035,-0.13309388499212,-0.130168654657908,-0.127300833839552,
-0.123054100396915,-0.118101053692855,-0.108902262384983,-0.0841889471967438,
-0.0600742653719997,-0.0555597355545908,-0.053464273600083,-0.0518452179885775,
-0.0499037740630693,-0.0461800909815272,-0.0413175708434384,-0.000460996019999361),
 .UNSPECIFIED.);
#3918=B_SPLINE_CURVE_WITH_KNOTS('',3,(#283272,#283273,#283274,#283275,#283276,
#283277,#283278,#283279,#283280,#283281),.UNSPECIFIED.,.F.,.F.,(4,1,1,1,
1,1,1,4),(78.5398163397448,79.169081837476,80.1670888081061,81.1650957787362,
82.1631027493663,83.1611097199964,84.1591166906264,84.8230016469244),
 .UNSPECIFIED.);
#3919=B_SPLINE_CURVE_WITH_KNOTS('',3,(#283283,#283284,#283285,#283286,#283287,
#283288,#283289,#283290,#283291,#283292,#283293,#283294,#283295,#283296,
#283297,#283298,#283299,#283300,#283301,#283302,#283303,#283304,#283305,
#283306,#283307,#283308,#283309,#283310,#283311,#283312,#283313,#283314,
#283315,#283316,#283317,#283318,#283319,#283320,#283321,#283322,#283323,
#283324,#283325,#283326,#283327,#283328,#283329,#283330,#283331,#283332,
#283333,#283334,#283335,#283336,#283337,#283338,#283339,#283340,#283341,
#283342,#283343,#283344,#283345,#283346,#283347,#283348,#283349,#283350,
#283351,#283352,#283353,#283354,#283355,#283356,#283357,#283358,#283359,
#283360,#283361,#283362,#283363,#283364,#283365,#283366,#283367,#283368,
#283369,#283370,#283371,#283372,#283373,#283374,#283375,#283376,#283377,
#283378,#283379,#283380,#283381,#283382,#283383,#283384,#283385,#283386,
#283387,#283388,#283389,#283390,#283391,#283392,#283393,#283394,#283395,
#283396,#283397,#283398,#283399,#283400,#283401,#283402,#283403,#283404,
#283405,#283406,#283407,#283408,#283409,#283410,#283411,#283412,#283413,
#283414,#283415,#283416,#283417,#283418,#283419,#283420,#283421,#283422,
#283423,#283424,#283425,#283426,#283427,#283428,#283429,#283430,#283431,
#283432,#283433,#283434,#283435,#283436,#283437,#283438,#283439,#283440,
#283441,#283442,#283443,#283444,#283445,#283446,#283447,#283448,#283449,
#283450,#283451,#283452,#283453,#283454,#283455,#283456,#283457,#283458,
#283459,#283460,#283461,#283462,#283463,#283464,#283465,#283466,#283467,
#283468,#283469,#283470,#283471,#283472,#283473,#283474,#283475,#283476,
#283477,#283478,#283479,#283480,#283481,#283482,#283483,#283484,#283485,
#283486,#283487,#283488,#283489,#283490,#283491,#283492,#283493,#283494,
#283495,#283496,#283497,#283498,#283499,#283500,#283501,#283502,#283503,
#283504,#283505,#283506,#283507,#283508,#283509,#283510,#283511,#283512,
#283513,#283514,#283515,#283516,#283517,#283518,#283519,#283520,#283521,
#283522,#283523,#283524,#283525,#283526,#283527,#283528,#283529,#283530,
#283531,#283532,#283533,#283534,#283535,#283536,#283537,#283538,#283539,
#283540,#283541,#283542,#283543,#283544,#283545,#283546,#283547,#283548,
#283549,#283550,#283551,#283552,#283553,#283554,#283555,#283556,#283557,
#283558,#283559,#283560,#283561,#283562,#283563,#283564,#283565,#283566,
#283567,#283568,#283569,#283570,#283571,#283572,#283573,#283574,#283575,
#283576,#283577,#283578,#283579,#283580,#283581,#283582,#283583,#283584,
#283585,#283586,#283587,#283588,#283589,#283590,#283591,#283592,#283593,
#283594,#283595,#283596,#283597,#283598,#283599,#283600,#283601,#283602,
#283603,#283604,#283605,#283606,#283607,#283608,#283609,#283610,#283611,
#283612,#283613,#283614,#283615,#283616,#283617,#283618,#283619,#283620,
#283621,#283622,#283623,#283624,#283625,#283626,#283627,#283628,#283629,
#283630,#283631,#283632,#283633,#283634,#283635,#283636,#283637,#283638,
#283639,#283640,#283641,#283642,#283643,#283644,#283645,#283646,#283647,
#283648,#283649,#283650,#283651,#283652,#283653,#283654,#283655,#283656,
#283657,#283658,#283659,#283660,#283661,#283662,#283663,#283664,#283665,
#283666,#283667,#283668,#283669,#283670,#283671,#283672,#283673,#283674,
#283675,#283676,#283677,#283678,#283679,#283680),.UNSPECIFIED.,.F.,.F.,
(4,2,2,2,2,2,2,2,2,2,2,2,2,2,2,2,2,2,2,2,2,2,2,2,2,2,2,2,2,2,2,2,2,2,2,
2,2,2,2,2,2,2,2,2,2,2,2,2,2,2,2,2,2,2,2,2,2,2,2,2,2,2,2,2,2,2,2,2,2,2,2,
2,2,2,2,2,2,2,2,2,2,2,2,2,2,2,2,2,2,2,2,2,2,2,2,2,2,2,2,2,2,2,2,2,2,2,2,
2,2,2,2,2,2,2,2,2,2,2,2,2,2,2,2,2,2,2,2,2,2,2,2,2,2,2,2,2,2,2,2,2,2,2,2,
2,2,2,2,2,2,2,2,2,2,2,2,2,2,2,2,2,2,2,2,2,2,2,2,2,2,2,2,2,2,2,2,2,2,2,2,
2,2,2,2,2,2,2,2,2,2,2,2,2,2,2,2,2,2,2,4),(-1.96053344110796,-1.92968691991721,
-1.91055048298032,-1.9061233569176,-1.90404479251844,-1.90258244773755,
-1.90069779644516,-1.8973375922818,-1.87680523446693,-1.87327167107956,
-1.85418214867251,-1.8408864322038,-1.8345579053475,-1.82939170057257,-1.82629969095901,
-1.82342075636068,-1.81977005791869,-1.81390988454385,-1.77835081058486,
-1.75371236266834,-1.75004111098677,-1.74811099150082,-1.74649168130467,
-1.7444183129971,-1.74005959929675,-1.71204237086999,-1.68310623896729,
-1.67532824260053,-1.67164188121702,-1.66875908154425,-1.66553599262994,
-1.66008241713623,-1.63162998100072,-1.60878814014973,-1.59681474923814,
-1.59384532603972,-1.59206517123355,-1.59042440456851,-1.58841699201733,
-1.58447736675957,-1.55601993420657,-1.52378918607622,-1.51822077307732,
-1.51497326955132,-1.512094696404,-1.50844925016096,-1.50260754357464,-1.46671018031895,
-1.44235617054664,-1.43869350815066,-1.43676508763112,-1.43514548593234,
-1.43306960517091,-1.42853813690989,-1.40440840912775,-1.39146520843914,
-1.3755724574329,-1.36513622663663,-1.36101542405418,-1.35806675013848,
-1.35537715315105,-1.35104647533156,-1.33993434429303,-1.30662967220022,
-1.28785849459179,-1.28346924633632,-1.28139750231834,-1.27993563376905,
-1.27804549422379,-1.27466177658614,-1.25166553042387,-1.23388155478177,
-1.21917685810568,-1.21242086750445,-1.20688018125452,-1.20363825483928,
-1.20075827178417,-1.19710240314383,-1.19122585714207,-1.15568935744395,
-1.13104368380562,-1.12737159440556,-1.12544105418401,-1.12382140297389,
-1.12174761293088,-1.11722867233391,-1.09558589047466,-1.07889449441558,
-1.05615242282734,-1.05092141569482,-1.04774530483463,-1.04485088081463,
-1.04113644247854,-1.03491660320841,-0.992881609056747,-0.980516681571756,
-0.973322320459725,-0.97073603936278,-0.969207064900069,-0.967521704837486,
-0.964993002647571,-0.957635423444112,-0.945193217524613,-0.902400787269249,
-0.896676202592614,-0.893064449631609,-0.890188322231025,-0.886917760668263,
-0.881243057487627,-0.849897868629513,-0.820575568563779,-0.816285649517556,
-0.814232451991065,-0.812615816908899,-0.810640167180081,-0.806746982981803,
-0.801593809440625,-0.788549094180412,-0.769688744013373,-0.745032078909484,
-0.739621408125712,-0.736406787311403,-0.73352115535427,-0.729816700180218,
-0.72194340273459,-0.692826781674622,-0.665061920254774,-0.660709072641957,
-0.658614266361268,-0.656995406923766,-0.655053823780055,-0.651328869454544,
-0.646464040368877,-0.634551228080059,-0.605242686934453,-0.588513660487068,
-0.583526109240286,-0.580401688567089,-0.57749004337316,-0.57359339637715,
-0.564608479708384,-0.551783716664436,-0.532176321192252,-0.527005388685896,
-0.50772942322851,-0.504382406394867,-0.502500226444007,-0.501036709486796,
-0.498952495664981,-0.494497897133751,-0.47510710521946,-0.439988492359812,
-0.430762670675787,-0.427115327223792,-0.424422323470096,-0.421475552260034,
-0.41736805191031,-0.407027134631118,-0.391347383462544,-0.374784108578653,
-0.352087157175161,-0.348709627024167,-0.346820662192318,-0.345358274082086,
-0.343283979781338,-0.338882359007789,-0.319998818633091,-0.286364937514228,
-0.275616144597339,-0.271337275188286,-0.268656345957405,-0.265698234391899,
-0.261528094469031,-0.250751902030441,-0.23408236340897,-0.197916109022278,
-0.193971042477316,-0.191961934443897,-0.190320371532765,-0.188540085133019,
-0.185571875607219,-0.173623607312659,-0.150780945848837,-0.122315025128356,
-0.116860965390557,-0.113637054324961,-0.11075318059271,-0.107064979995398,
-0.0994980728488588,-0.0794121500077125,-0.0578724433652814,-0.0405361975418842,
-0.0372412699647678,-0.035370758717511,-0.0337414912643039,-0.0321250789126551,
-0.0299549206399665,-0.0263828312756159,-0.000460541927694245),
 .UNSPECIFIED.);
#3920=B_SPLINE_CURVE_WITH_KNOTS('',3,(#283682,#283683,#283684,#283685,#283686,
#283687,#283688,#283689,#283690,#283691),.UNSPECIFIED.,.F.,.F.,(4,1,1,1,
1,1,1,4),(59.690260418206,60.2069493955043,61.2049563661344,62.2029633367645,
63.2009703073946,64.1989772780247,65.1969842486548,65.9734446845719),
 .UNSPECIFIED.);
#3921=B_SPLINE_CURVE_WITH_KNOTS('',3,(#283693,#283694,#283695,#283696,#283697,
#283698,#283699,#283700,#283701,#283702,#283703,#283704,#283705,#283706,
#283707,#283708,#283709,#283710,#283711,#283712,#283713,#283714,#283715,
#283716,#283717,#283718,#283719,#283720,#283721,#283722,#283723,#283724,
#283725,#283726,#283727,#283728,#283729,#283730,#283731,#283732,#283733,
#283734,#283735,#283736,#283737,#283738,#283739,#283740,#283741,#283742,
#283743,#283744,#283745,#283746,#283747,#283748,#283749,#283750,#283751,
#283752,#283753,#283754,#283755,#283756,#283757,#283758,#283759,#283760,
#283761,#283762,#283763,#283764,#283765,#283766,#283767,#283768,#283769,
#283770,#283771,#283772,#283773,#283774,#283775,#283776,#283777,#283778,
#283779,#283780,#283781,#283782,#283783,#283784,#283785,#283786,#283787,
#283788,#283789,#283790,#283791,#283792,#283793,#283794,#283795,#283796,
#283797,#283798,#283799,#283800,#283801,#283802,#283803,#283804,#283805,
#283806,#283807,#283808,#283809,#283810,#283811,#283812,#283813,#283814,
#283815,#283816,#283817,#283818,#283819,#283820,#283821,#283822,#283823,
#283824,#283825,#283826,#283827,#283828,#283829,#283830,#283831,#283832,
#283833,#283834,#283835,#283836,#283837,#283838,#283839,#283840,#283841,
#283842,#283843,#283844,#283845,#283846,#283847,#283848,#283849,#283850,
#283851,#283852,#283853,#283854,#283855,#283856,#283857,#283858,#283859,
#283860,#283861,#283862,#283863,#283864,#283865,#283866,#283867,#283868,
#283869,#283870,#283871,#283872,#283873,#283874,#283875,#283876,#283877,
#283878,#283879,#283880,#283881,#283882,#283883,#283884,#283885,#283886,
#283887,#283888,#283889,#283890,#283891,#283892,#283893,#283894,#283895,
#283896,#283897,#283898,#283899,#283900,#283901,#283902,#283903,#283904,
#283905,#283906,#283907,#283908,#283909,#283910,#283911,#283912,#283913,
#283914,#283915,#283916,#283917,#283918,#283919,#283920,#283921,#283922,
#283923,#283924,#283925,#283926,#283927,#283928,#283929,#283930,#283931,
#283932,#283933,#283934,#283935,#283936,#283937,#283938,#283939,#283940,
#283941,#283942,#283943,#283944,#283945,#283946,#283947,#283948,#283949,
#283950,#283951,#283952,#283953,#283954,#283955,#283956,#283957,#283958,
#283959,#283960,#283961,#283962,#283963,#283964,#283965,#283966,#283967,
#283968,#283969,#283970,#283971,#283972,#283973,#283974,#283975,#283976,
#283977,#283978,#283979,#283980,#283981,#283982,#283983,#283984,#283985,
#283986,#283987,#283988,#283989,#283990,#283991,#283992,#283993,#283994,
#283995,#283996,#283997,#283998,#283999,#284000,#284001,#284002,#284003,
#284004,#284005,#284006,#284007,#284008,#284009,#284010,#284011,#284012,
#284013,#284014,#284015,#284016,#284017,#284018,#284019,#284020,#284021,
#284022,#284023,#284024,#284025,#284026,#284027,#284028,#284029,#284030,
#284031,#284032,#284033,#284034,#284035,#284036,#284037,#284038,#284039,
#284040,#284041,#284042,#284043,#284044,#284045,#284046,#284047,#284048,
#284049,#284050,#284051,#284052,#284053,#284054,#284055,#284056,#284057,
#284058,#284059,#284060,#284061,#284062,#284063,#284064,#284065,#284066,
#284067,#284068,#284069,#284070,#284071,#284072,#284073,#284074,#284075,
#284076,#284077,#284078,#284079,#284080,#284081,#284082,#284083,#284084,
#284085,#284086,#284087,#284088,#284089,#284090,#284091,#284092,#284093,
#284094,#284095,#284096,#284097,#284098,#284099,#284100,#284101,#284102,
#284103,#284104),.UNSPECIFIED.,.F.,.F.,(4,2,2,2,2,2,2,2,2,2,2,2,2,2,2,2,
2,2,2,2,2,2,2,2,2,2,2,2,2,2,2,2,2,2,2,2,2,2,2,2,2,2,2,2,2,2,2,2,2,2,2,2,
2,2,2,2,2,2,2,2,2,2,2,2,2,2,2,2,2,2,2,2,2,2,2,2,2,2,2,2,2,2,2,2,2,2,2,2,
2,2,2,2,2,2,2,2,2,2,2,2,2,2,2,2,2,2,2,2,2,2,2,2,2,2,2,2,2,2,2,2,2,2,2,2,
2,2,2,2,2,2,2,2,2,2,2,2,2,2,2,2,2,2,2,2,2,2,2,2,2,2,2,2,2,2,2,2,2,2,2,2,
2,2,2,2,2,2,2,2,2,2,2,2,2,2,2,2,2,2,2,2,2,2,2,2,2,2,2,2,2,2,2,2,2,2,2,2,
2,2,2,2,2,2,2,2,2,4),(-1.96074350940351,-1.95917447291995,-1.95671350899246,
-1.94917971597731,-1.9123925266757,-1.89311953730399,-1.88867772530256,
-1.88659617447291,-1.88513325318232,-1.88325000330616,-1.87989707818968,
-1.86021508902107,-1.85565788050471,-1.83417429114077,-1.81640260314938,
-1.81148585030099,-1.80858850085177,-1.80580320003331,-1.80218623979858,
-1.79619319774473,-1.7546613312234,-1.74169159403833,-1.73655724866933,
-1.73267538131483,-1.73070211953118,-1.72908554107684,-1.72703002277448,
-1.72272726540563,-1.68625913422958,-1.6697436318915,-1.65903354735689,
-1.65487311476724,-1.65191702120589,-1.64923465828054,-1.6449464184678,
-1.63411842085676,-1.60053701930469,-1.58166875780566,-1.57726901045711,
-1.57519517584489,-1.57373296221407,-1.57184397045185,-1.56846590006631,
-1.54572604942813,-1.52924529754197,-1.51357087721261,-1.50323167493191,
-1.49912466078596,-1.49617813313554,-1.49348526375511,-1.48983797129163,
-1.48061177479173,-1.44547268545429,-1.42607126636259,-1.42161574201211,
-1.41953142090873,-1.41806797352049,-1.41618604331374,-1.41283990395091,
-1.39358117315324,-1.38840933545866,-1.36882032484893,-1.35600105900136,
-1.34701811294616,-1.34312192484604,-1.34021044547451,-1.33708603224572,
-1.33209813922853,-1.31536587757116,-1.28602072579389,-1.27410972418891,
-1.26924546000267,-1.26552117884254,-1.26357977143758,-1.26196094169405,
-1.25986604720019,-1.25551257973577,-1.22777146655256,-1.19866775938329,
-1.19079681751974,-1.18709282121814,-1.18420725129045,-1.18099239425393,
-1.17558060751334,-1.15091073900901,-1.1320361621118,-1.11898345585879,
-1.1138282941744,-1.10993429807784,-1.1079584888374,-1.10634185863982,-1.10428885071513,
-1.09999991071284,-1.07069075437743,-1.03955247366408,-1.03377503037985,
-1.03048274832177,-1.02760910375651,-1.02402883787984,-1.01841144528615,
-0.980410374922927,-0.957312790550657,-0.95392592017682,-0.952034821866809,
-0.950572677672377,-0.948501188441025,-0.944114828961308,-0.925376622040968,
-0.892161204092339,-0.880969872546063,-0.876626824199373,-0.873934579839489,
-0.870986969423271,-0.866875158207545,-0.856505359834304,-0.840761372636222,
-0.824980595245874,-0.803373863511543,-0.798854607160077,-0.796758439663589,
-0.79513953068634,-0.793199096555113,-0.789479583626837,-0.784623950701396,
-0.772746093684703,-0.743482809889265,-0.72667254251809,-0.72167751879759,
-0.718551566518469,-0.715640624324773,-0.711748156980437,-0.702788166667672,
-0.690012843158084,-0.670343170482305,-0.665134576215712,-0.64587485113954,
-0.642528239631406,-0.640646182212771,-0.639182694857536,-0.637098437638912,
-0.63264341572802,-0.613247852626881,-0.57811438205515,-0.568904083926527,
-0.565259279867758,-0.562566942292256,-0.559619729492917,-0.555509412826898,
-0.545148782655604,-0.529424840992287,-0.513393198679142,-0.490255315052111,
-0.486867578267891,-0.484976369989036,-0.483514369737414,-0.48144338148785,
-0.477059204685858,-0.458339913499957,-0.425177129599025,-0.413933848114941,
-0.409583321247437,-0.406889895550808,-0.403943722547694,-0.399839046094038,
-0.389516617206656,-0.373877735092742,-0.356901291671155,-0.334545045826474,
-0.331173114948465,-0.329285447512543,-0.327822933834425,-0.325746992975945,
-0.321336291244035,-0.302365482093407,-0.268478462984107,-0.258005506977063,
-0.253761583633471,-0.250819395282126,-0.247807269615527,-0.243357640616498,
-0.230416660739951,-0.208119895793539,-0.180453673722901,-0.176105372189886,
-0.174011572819604,-0.172392906147713,-0.170450847870261,-0.166723085733385,
-0.161853363487741,-0.149921257428941,-0.120589127597403,-0.103909377824713,
-0.0989267546882721,-0.0958035579980236,-0.0928917903425926,-0.0889930553048363,
-0.0799942084884878,-0.0416492524753233,-0.0266198591389201,-0.0210409164424102,
-0.0189262818004382,-0.0174077763562326,-0.0158946722602569,-0.0142038132499826,
-0.0118325809587982,-0.000460124348572881),.UNSPECIFIED.);
#3922=B_SPLINE_CURVE_WITH_KNOTS('',3,(#284106,#284107,#284108,#284109,#284110,
#284111,#284112,#284113,#284114,#284115),.UNSPECIFIED.,.F.,.F.,(4,1,1,1,
1,1,1,4),(40.840710987977,41.2448169535326,42.2428239241627,43.2408308947928,
44.2388378654229,45.236844836053,46.2348518066831,47.123880997786),
 .UNSPECIFIED.);
#3923=B_SPLINE_CURVE_WITH_KNOTS('',3,(#284117,#284118,#284119,#284120,#284121,
#284122,#284123,#284124,#284125,#284126,#284127,#284128,#284129,#284130,
#284131,#284132,#284133,#284134,#284135,#284136,#284137,#284138,#284139,
#284140,#284141,#284142,#284143,#284144,#284145,#284146,#284147,#284148,
#284149,#284150,#284151,#284152,#284153,#284154,#284155,#284156,#284157,
#284158,#284159,#284160,#284161,#284162,#284163,#284164,#284165,#284166,
#284167,#284168,#284169,#284170,#284171,#284172,#284173,#284174,#284175,
#284176,#284177,#284178,#284179,#284180,#284181,#284182,#284183,#284184,
#284185,#284186,#284187,#284188,#284189,#284190,#284191,#284192,#284193,
#284194,#284195,#284196,#284197,#284198,#284199,#284200,#284201,#284202,
#284203,#284204,#284205,#284206,#284207,#284208,#284209,#284210,#284211,
#284212,#284213,#284214,#284215,#284216,#284217,#284218,#284219,#284220,
#284221,#284222,#284223,#284224,#284225,#284226,#284227,#284228,#284229,
#284230,#284231,#284232,#284233,#284234,#284235,#284236,#284237,#284238,
#284239,#284240,#284241,#284242,#284243,#284244,#284245,#284246,#284247,
#284248,#284249,#284250,#284251,#284252,#284253,#284254,#284255,#284256,
#284257,#284258,#284259,#284260,#284261,#284262,#284263,#284264,#284265,
#284266,#284267,#284268,#284269,#284270,#284271,#284272,#284273,#284274,
#284275,#284276,#284277,#284278,#284279,#284280,#284281,#284282,#284283,
#284284,#284285,#284286,#284287,#284288,#284289,#284290,#284291,#284292,
#284293,#284294,#284295,#284296,#284297,#284298,#284299,#284300,#284301,
#284302,#284303,#284304,#284305,#284306,#284307,#284308,#284309,#284310,
#284311,#284312,#284313,#284314,#284315,#284316,#284317,#284318,#284319,
#284320,#284321,#284322,#284323,#284324,#284325,#284326,#284327,#284328,
#284329,#284330,#284331,#284332,#284333,#284334,#284335,#284336,#284337,
#284338,#284339,#284340,#284341,#284342,#284343,#284344,#284345,#284346,
#284347,#284348,#284349,#284350,#284351,#284352,#284353,#284354,#284355,
#284356,#284357,#284358,#284359,#284360,#284361,#284362,#284363,#284364,
#284365,#284366,#284367,#284368,#284369,#284370,#284371,#284372,#284373,
#284374,#284375,#284376,#284377,#284378,#284379,#284380,#284381,#284382,
#284383,#284384,#284385,#284386,#284387,#284388,#284389,#284390,#284391,
#284392,#284393,#284394,#284395,#284396,#284397,#284398,#284399,#284400,
#284401,#284402,#284403,#284404,#284405,#284406,#284407,#284408,#284409,
#284410,#284411,#284412,#284413,#284414,#284415,#284416,#284417,#284418,
#284419,#284420,#284421,#284422,#284423,#284424,#284425,#284426,#284427,
#284428,#284429,#284430,#284431,#284432,#284433,#284434,#284435,#284436,
#284437,#284438,#284439,#284440,#284441,#284442,#284443,#284444,#284445,
#284446,#284447,#284448,#284449,#284450,#284451,#284452,#284453,#284454,
#284455,#284456,#284457,#284458,#284459,#284460,#284461,#284462,#284463,
#284464,#284465,#284466,#284467,#284468,#284469,#284470,#284471,#284472,
#284473,#284474,#284475,#284476,#284477,#284478,#284479,#284480,#284481,
#284482,#284483,#284484,#284485,#284486,#284487,#284488,#284489,#284490,
#284491,#284492,#284493,#284494,#284495,#284496,#284497,#284498,#284499,
#284500,#284501,#284502,#284503,#284504,#284505,#284506,#284507,#284508,
#284509,#284510,#284511,#284512,#284513,#284514,#284515,#284516),
 .UNSPECIFIED.,.F.,.F.,(4,2,2,2,2,2,2,2,2,2,2,2,2,2,2,2,2,2,2,2,2,2,2,2,
2,2,2,2,2,2,2,2,2,2,2,2,2,2,2,2,2,2,2,2,2,2,2,2,2,2,2,2,2,2,2,2,2,2,2,2,
2,2,2,2,2,2,2,2,2,2,2,2,2,2,2,2,2,2,2,2,2,2,2,2,2,2,2,2,2,2,2,2,2,2,2,2,
2,2,2,2,2,2,2,2,2,2,2,2,2,2,2,2,2,2,2,2,2,2,2,2,2,2,2,2,2,2,2,2,2,2,2,2,
2,2,2,2,2,2,2,2,2,2,2,2,2,2,2,2,2,2,2,2,2,2,2,2,2,2,2,2,2,2,2,2,2,2,2,2,
2,2,2,2,2,2,2,2,2,2,2,2,2,2,2,2,2,2,2,2,2,2,2,2,2,2,2,2,2,2,2,4),(-1.96114492875287,
-1.95576637931755,-1.951446667606,-1.94859517363792,-1.94585143044094,-1.94276410837109,
-1.9379495198647,-1.92281222802353,-1.88465513711007,-1.87331458819503,
-1.87039192502045,-1.86862177611939,-1.86697537751122,-1.86494592768585,
-1.85993562537325,-1.82447838504788,-1.80810053210915,-1.80086596391414,
-1.79502215970159,-1.791716072214,-1.78884401621589,-1.78528343446254,-1.77840693998898,
-1.73645498864894,-1.72409870341728,-1.71911919823099,-1.71532731999055,
-1.71337213245214,-1.71175438919187,-1.70967696337979,-1.70525855594959,
-1.67731788893727,-1.6482944280941,-1.64051386731501,-1.6368263425757,-1.63394265505342,
-1.6307185961465,-1.62526343551025,-1.59679206125115,-1.57377161344205,
-1.56195398927882,-1.55899521813389,-1.55721704813573,-1.55557453285952,
-1.55356135137965,-1.54959968013638,-1.5213215942493,-1.48888205576646,
-1.48333688606303,-1.48009368368249,-1.47721337573702,-1.47355819496577,
-1.46768506809618,-1.43209496645531,-1.40748343083231,-1.40381192755028,
-1.40188132415746,-1.40026139409704,-1.39818696584068,-1.39382513231902,
-1.36582171508401,-1.33685320431929,-1.32907229375153,-1.32538456546125,
-1.32250070285318,-1.31927643174753,-1.31382087133583,-1.28547685527371,
-1.26358336900253,-1.25487522569929,-1.2491257421775,-1.24682130216123,
-1.24517732415398,-1.24335868660361,-1.2402146781448,-1.22726782871177,
-1.19877173364137,-1.18415455952539,-1.1774239576004,-1.17189926825107,
-1.16866032612286,-1.16577915526009,-1.1621165413588,-1.15447243614956,
-1.11344222345047,-1.10118064399329,-1.0938944888935,-1.09137459204419,
-1.08969092287681,-1.08794796168932,-1.08515058871851,-1.07619994376864,
-1.04874212885248,-1.02583026248366,-1.01778211819715,-1.01404603414751,
-1.01115643917933,-1.0079583798575,-1.00262633575032,-0.98059470178565,
-0.962883134199216,-0.939927174853375,-0.93654369270583,-0.934653275069281,
-0.933190914222677,-0.931118153664723,-0.926725454114284,-0.907928894359782,
-0.874547548067435,-0.863526966763021,-0.859209166816556,-0.856521238649713,
-0.853569323279406,-0.84943442056772,-0.838906930815121,-0.822808525685492,
-0.815371028106317,-0.785592192781932,-0.781322318143366,-0.779272790867857,
-0.77765609569484,-0.775676750952046,-0.77176584949165,-0.748215461411428,
-0.711841966187339,-0.706046985070254,-0.702414392950313,-0.699536070341747,
-0.696278350409146,-0.690665552776482,-0.683796221854088,-0.668706226018213,
-0.652879142178664,-0.64772108714329,-0.628438091395846,-0.625090850788478,
-0.623208588213808,-0.621745033890179,-0.619660801883373,-0.615206299946208,
-0.595817127539822,-0.560703990336907,-0.551471645088069,-0.547823203248531,
-0.545129881120517,-0.542183238132664,-0.538076811672501,-0.527743720521503,
-0.51208162060548,-0.495324141169928,-0.472786241970681,-0.469411448480073,
-0.467523061485594,-0.466060534274226,-0.463985280773575,-0.459578728328218,
-0.440649022367267,-0.406882453994987,-0.396280551626905,-0.39201759083044,
-0.389339354643281,-0.386378316820212,-0.38219268427536,-0.37130690677469,
-0.354382117308863,-0.338437650744959,-0.317077049919405,-0.313712093493294,
-0.311825926109864,-0.31036308928403,-0.308284758038825,-0.303861600876152,
-0.284773076728942,-0.250544894129886,-0.240403038206404,-0.236219404864892,
-0.233288255850289,-0.230261606925782,-0.225740734411683,-0.212180161046693,
-0.187987983707784,-0.163159749288675,-0.158749051252414,-0.156657932775563,
-0.155083789341134,-0.153558565098084,-0.150580277503387,-0.138489547329619,
-0.115708015956755,-0.0873474679874398,-0.0818930642097595,-0.0786691829708695,
-0.0757854784153475,-0.0720976912152042,-0.0643157561470027,-0.0355731630768982,
-0.00695792209858334,-0.00294883740074442,-0.0013212046580614,-0.000460615870580507),
 .UNSPECIFIED.);
#3924=B_SPLINE_CURVE_WITH_KNOTS('',3,(#284518,#284519,#284520,#284521,#284522,
#284523,#284524,#284525,#284526,#284527,#284528,#284529,#284530,#284531,
#284532,#284533,#284534,#284535,#284536,#284537,#284538,#284539,#284540,
#284541,#284542,#284543,#284544,#284545,#284546,#284547,#284548,#284549,
#284550,#284551,#284552,#284553,#284554,#284555,#284556,#284557,#284558,
#284559,#284560,#284561,#284562,#284563,#284564,#284565,#284566,#284567,
#284568,#284569,#284570,#284571,#284572,#284573,#284574,#284575,#284576,
#284577,#284578,#284579,#284580,#284581,#284582,#284583,#284584,#284585,
#284586,#284587,#284588,#284589,#284590,#284591,#284592,#284593,#284594,
#284595,#284596,#284597,#284598,#284599,#284600,#284601,#284602,#284603,
#284604,#284605,#284606,#284607,#284608,#284609,#284610,#284611,#284612,
#284613,#284614,#284615,#284616,#284617,#284618,#284619,#284620,#284621,
#284622,#284623,#284624,#284625,#284626,#284627,#284628,#284629,#284630,
#284631,#284632,#284633,#284634,#284635,#284636,#284637,#284638,#284639,
#284640,#284641,#284642,#284643,#284644,#284645,#284646,#284647,#284648,
#284649,#284650,#284651,#284652,#284653,#284654,#284655,#284656,#284657,
#284658,#284659,#284660,#284661,#284662,#284663,#284664,#284665,#284666,
#284667,#284668,#284669,#284670,#284671,#284672,#284673,#284674,#284675,
#284676,#284677,#284678,#284679,#284680,#284681,#284682,#284683,#284684,
#284685,#284686,#284687,#284688,#284689,#284690,#284691,#284692,#284693,
#284694,#284695,#284696,#284697,#284698,#284699,#284700,#284701,#284702,
#284703,#284704,#284705,#284706,#284707,#284708,#284709,#284710,#284711,
#284712,#284713,#284714,#284715,#284716,#284717,#284718,#284719,#284720,
#284721,#284722,#284723,#284724,#284725,#284726,#284727,#284728,#284729,
#284730,#284731,#284732,#284733,#284734,#284735,#284736,#284737,#284738,
#284739,#284740,#284741,#284742,#284743,#284744,#284745,#284746,#284747,
#284748,#284749,#284750,#284751,#284752,#284753,#284754,#284755,#284756,
#284757,#284758,#284759,#284760,#284761,#284762,#284763,#284764,#284765,
#284766,#284767,#284768,#284769,#284770,#284771,#284772,#284773,#284774,
#284775,#284776,#284777,#284778,#284779,#284780,#284781,#284782,#284783,
#284784,#284785,#284786,#284787,#284788,#284789,#284790,#284791,#284792,
#284793,#284794,#284795,#284796,#284797,#284798,#284799,#284800,#284801,
#284802,#284803,#284804,#284805,#284806,#284807,#284808,#284809,#284810,
#284811,#284812,#284813,#284814,#284815,#284816,#284817,#284818,#284819,
#284820,#284821,#284822,#284823,#284824,#284825,#284826,#284827,#284828,
#284829,#284830,#284831,#284832,#284833,#284834,#284835,#284836,#284837,
#284838,#284839,#284840,#284841,#284842,#284843,#284844,#284845,#284846,
#284847,#284848,#284849,#284850,#284851,#284852,#284853,#284854,#284855,
#284856,#284857,#284858,#284859,#284860,#284861,#284862,#284863,#284864,
#284865,#284866,#284867,#284868,#284869,#284870,#284871,#284872,#284873,
#284874,#284875,#284876,#284877,#284878,#284879,#284880,#284881,#284882,
#284883,#284884,#284885,#284886,#284887,#284888,#284889,#284890,#284891,
#284892,#284893,#284894,#284895,#284896,#284897,#284898,#284899,#284900,
#284901,#284902,#284903,#284904,#284905,#284906,#284907,#284908,#284909,
#284910,#284911,#284912,#284913,#284914,#284915,#284916,#284917,#284918,
#284919,#284920,#284921),.UNSPECIFIED.,.F.,.F.,(4,2,2,2,2,2,2,2,2,2,2,2,
2,2,2,2,2,2,2,2,2,2,2,2,2,2,2,2,2,2,2,2,2,2,2,2,2,2,2,2,2,2,2,2,2,2,2,2,
2,2,2,2,2,2,2,2,2,2,2,2,2,2,2,2,2,2,2,2,2,2,2,2,2,2,2,2,2,2,2,2,2,2,2,2,
2,2,2,2,2,2,2,2,2,2,2,2,2,2,2,2,2,2,2,2,2,2,2,2,2,2,2,2,2,2,2,2,2,2,2,2,
2,2,2,2,2,2,2,2,2,2,2,2,2,2,2,2,2,2,2,2,2,2,2,2,2,2,2,2,2,2,2,2,2,2,2,2,
2,2,2,2,2,2,2,2,2,2,2,2,2,2,2,2,2,2,2,2,2,2,2,2,2,2,2,2,2,2,2,2,2,2,2,2,
2,2,2,2,2,2,2,2,2,4),(-1.96091714897476,-1.96012176149206,-1.95853632991965,
-1.95589451949815,-1.94783216974802,-1.91599294862312,-1.89990466072315,
-1.889382634788,-1.88525002517998,-1.88229974712249,-1.87925530128157,-1.87464317266051,
-1.86144809406078,-1.83007205183936,-1.81665269911615,-1.81140810041174,
-1.80746293509928,-1.80584886682636,-1.80424933478267,-1.80243842795593,
-1.79930307591602,-1.78530696648465,-1.75728332091529,-1.74309652020047,
-1.73344602498232,-1.72944403832998,-1.72651658680164,-1.72343270313497,
-1.7186317963624,-1.70366916045486,-1.65916461975297,-1.65284700413774,
-1.65045825566845,-1.64880030465387,-1.64701656914454,-1.64403080122351,
-1.63311742963153,-1.6071034191073,-1.58069257613081,-1.57531452639657,
-1.5721075323954,-1.56922146069732,-1.56550623998223,-1.55942301733818,
-1.52739066094712,-1.49992001098603,-1.49607476229571,-1.49410907304509,
-1.49249241497452,-1.49042880364124,-1.48608219537813,-1.45747245891014,
-1.42531570969157,-1.41977354037265,-1.41653156477214,-1.41365202960026,
-1.40999739874575,-1.40412425055969,-1.36856280642021,-1.34394349558166,
-1.34027258699271,-1.33834244194475,-1.33672298659296,-1.33464927925256,
-1.33012989701472,-1.30641106214823,-1.29300260817071,-1.27713152139155,
-1.26670484578545,-1.26258537776457,-1.25963689736741,-1.25694696281351,
-1.25331085272942,-1.24415211231845,-1.20530222643581,-1.19328098941709,
-1.1883882012856,-1.18464725250626,-1.18270258520751,-1.18108424782528,
-1.1789941143488,-1.17450669996355,-1.14919099192974,-1.12535429698282,
-1.11190645969541,-1.10739861832612,-1.1043748023704,-1.10144198627579,
-1.09724825939276,-1.08705011963588,-1.05285953462524,-1.03378071468631,
-1.02935879814419,-1.02728078838383,-1.02581810497575,-1.02393200334928,
-1.02056688454017,-0.99897141682679,-0.981022705305819,-0.957963970394677,
-0.952592240250594,-0.949386103802839,-0.946498996581501,-0.942779907884808,
-0.934824403505638,-0.889199588072917,-0.875961978038965,-0.872806647417739,
-0.87098552021877,-0.869342338301719,-0.867043291751737,-0.861328698054324,
-0.852695494375835,-0.830726800221035,-0.802367518306779,-0.796912384311203,
-0.793688093273761,-0.790804036773963,-0.787115820424476,-0.779333061128802,
-0.750618457623808,-0.72227669246232,-0.718317574034866,-0.71630487548091,
-0.714662292538344,-0.712883288773786,-0.709921948799899,-0.698073593073806,
-0.675077084283756,-0.646652065543619,-0.641196958451298,-0.637972491717449,
-0.635088151163068,-0.63139938707036,-0.623614709106851,-0.594286155940436,
-0.56657749700128,-0.562231776161498,-0.560138207955578,-0.558519333960722,
-0.556576637631852,-0.552846101138243,-0.547971801951243,-0.536022951709776,
-0.506667681393957,-0.490014266208289,-0.485033834752996,-0.481910980576953,
-0.478998844899453,-0.47509858552568,-0.466091454910691,-0.453222589429769,
-0.433669463304257,-0.428526104767491,-0.409235119807618,-0.405887751585524,
-0.404005523095146,-0.402542026521058,-0.400457984958688,-0.396004507592167,
-0.37662678566424,-0.341553828636569,-0.332270038940211,-0.328613303778719,
-0.325917761991184,-0.322972460004503,-0.318874966112368,-0.308604459956545,
-0.293081550063853,-0.275258394187928,-0.253549671587606,-0.250182485170955,
-0.248295490452269,-0.246831733204854,-0.244751850883159,-0.240325664785076,
-0.2212196154148,-0.186927436357936,-0.176869659195013,-0.172699251924792,
-0.169769296366712,-0.166736997289291,-0.162194189588239,-0.156952378014564,
-0.146945432940435,-0.121122024362682,-0.0996479943551831,-0.095131156120863,
-0.0930351662220358,-0.0914167907493631,-0.0894780981363024,-0.0857612175790483,
-0.08090898033239,-0.0690404703623535,-0.0368923994444007,-0.0224030075793857,
-0.0176574110021688,-0.0145861917680512,-0.0118506224603147,-0.00899193696603837,
-0.00510495444921737,-0.000462804239319024),.UNSPECIFIED.);
#3925=B_SPLINE_CURVE_WITH_KNOTS('',3,(#284923,#284924,#284925,#284926,#284927,
#284928,#284929,#284930,#284931,#284932,#284933,#284934,#284935,#284936,
#284937,#284938,#284939,#284940,#284941,#284942,#284943,#284944,#284945,
#284946,#284947,#284948,#284949,#284950,#284951,#284952,#284953,#284954,
#284955,#284956,#284957,#284958,#284959,#284960,#284961,#284962,#284963,
#284964,#284965,#284966,#284967,#284968,#284969,#284970,#284971,#284972,
#284973,#284974,#284975,#284976,#284977,#284978,#284979,#284980,#284981,
#284982,#284983,#284984,#284985,#284986,#284987,#284988,#284989,#284990,
#284991,#284992,#284993,#284994,#284995,#284996,#284997,#284998,#284999,
#285000,#285001,#285002,#285003,#285004,#285005,#285006,#285007,#285008,
#285009,#285010,#285011,#285012,#285013,#285014,#285015,#285016,#285017,
#285018,#285019,#285020,#285021,#285022,#285023,#285024,#285025,#285026,
#285027,#285028,#285029,#285030,#285031,#285032,#285033,#285034,#285035,
#285036,#285037,#285038,#285039,#285040,#285041,#285042,#285043,#285044,
#285045,#285046,#285047,#285048,#285049,#285050,#285051,#285052,#285053,
#285054,#285055,#285056,#285057,#285058,#285059,#285060,#285061,#285062,
#285063,#285064,#285065,#285066,#285067,#285068,#285069,#285070),
 .UNSPECIFIED.,.F.,.F.,(4,3,3,3,3,3,3,3,3,3,3,3,3,3,3,3,3,3,3,3,3,3,3,3,
3,3,3,3,3,3,3,3,3,3,3,3,3,3,3,3,3,3,3,3,3,3,3,3,3,4),(10.376098452114,10.4921621249285,
10.6026274765781,10.7129932812893,10.8233039758027,10.9336039089491,11.0440096347695,
11.154477276847,11.2651345766751,11.30460783463,11.4164914118551,11.5281823562147,
11.6397658689834,11.7512845347586,11.8627808451948,11.9743807417522,12.0860284953431,
12.1978945566487,12.30261480526,12.4141501176243,12.5254833531454,12.6367036629042,
12.7478542641654,12.8589782743019,12.9702021872946,13.0814713211549,13.1929592520497,
13.3006217758901,13.4123432114113,13.5238659124788,13.6352775951744,13.7466211513991,
13.8579393757764,13.9693579342981,14.0808222795534,14.1925038146001,14.2986287465202,
14.4103401439347,14.5218534506597,14.6332561369876,14.7445911107436,14.8559011829471,
14.9673123393611,15.0787696795503,15.1904449850493,15.2966357171503,15.4196451177831,
15.5422562405462,15.6642417287656,15.7079632676177),.UNSPECIFIED.);
#3926=B_SPLINE_CURVE_WITH_KNOTS('',3,(#285074,#285075,#285076,#285077,#285078,
#285079,#285080,#285081,#285082,#285083,#285084,#285085,#285086,#285087,
#285088,#285089,#285090,#285091,#285092,#285093,#285094,#285095,#285096,
#285097,#285098,#285099,#285100,#285101,#285102,#285103,#285104,#285105,
#285106,#285107,#285108,#285109,#285110,#285111,#285112,#285113,#285114,
#285115,#285116,#285117,#285118,#285119,#285120,#285121,#285122,#285123,
#285124,#285125,#285126,#285127,#285128,#285129,#285130,#285131,#285132,
#285133,#285134,#285135,#285136,#285137,#285138,#285139,#285140,#285141,
#285142,#285143,#285144,#285145,#285146,#285147,#285148,#285149,#285150,
#285151,#285152,#285153,#285154,#285155,#285156,#285157,#285158,#285159,
#285160,#285161,#285162,#285163,#285164,#285165,#285166,#285167,#285168,
#285169,#285170,#285171,#285172,#285173,#285174,#285175,#285176,#285177,
#285178,#285179,#285180,#285181,#285182,#285183,#285184,#285185),
 .UNSPECIFIED.,.F.,.F.,(4,3,3,3,3,3,3,3,3,3,3,3,3,3,3,3,3,3,3,3,3,3,3,3,
3,3,3,3,3,3,3,3,3,3,3,3,3,4),(11.6154215191105,11.7297374029347,11.8439982074357,
11.9582309631743,12.0724702603026,12.1867506876971,12.3012039081309,12.4157458296163,
12.5305312494344,12.6127573616628,12.7233077204432,12.8341559059147,12.9443566479614,
13.0544767872351,13.1645609189115,13.2759439902374,13.3861606467071,13.4981269254611,
13.610093204215,13.7219630382752,13.8336341156697,13.945194057846,14.0566854855328,
14.1681509220921,14.2797142005244,14.3913222669152,14.50314328189,14.6074290467673,
14.7193214162471,14.8310214301151,14.9426141838145,15.0541422442932,15.1656480857482,
15.2772574285571,15.3889147272786,15.5007897623193,15.6047648893195,15.7079632679489),
 .UNSPECIFIED.);
#3927=B_SPLINE_CURVE_WITH_KNOTS('',3,(#285187,#285188,#285189,#285190,#285191,
#285192,#285193,#285194,#285195,#285196,#285197,#285198,#285199,#285200,
#285201,#285202,#285203,#285204,#285205,#285206,#285207,#285208,#285209,
#285210,#285211,#285212,#285213,#285214,#285215,#285216,#285217,#285218,
#285219,#285220,#285221,#285222,#285223,#285224,#285225,#285226,#285227,
#285228,#285229,#285230,#285231,#285232,#285233,#285234,#285235,#285236,
#285237,#285238,#285239,#285240,#285241,#285242,#285243,#285244,#285245,
#285246,#285247,#285248,#285249,#285250,#285251,#285252,#285253,#285254,
#285255,#285256,#285257,#285258,#285259,#285260,#285261,#285262,#285263,
#285264,#285265,#285266,#285267,#285268,#285269,#285270,#285271,#285272,
#285273,#285274,#285275,#285276,#285277,#285278,#285279,#285280,#285281,
#285282,#285283,#285284,#285285,#285286,#285287,#285288,#285289,#285290,
#285291,#285292,#285293,#285294,#285295,#285296,#285297,#285298,#285299,
#285300,#285301,#285302,#285303,#285304,#285305,#285306,#285307,#285308,
#285309,#285310,#285311,#285312,#285313,#285314,#285315,#285316,#285317,
#285318,#285319,#285320,#285321,#285322,#285323,#285324,#285325,#285326,
#285327,#285328,#285329,#285330,#285331,#285332,#285333,#285334,#285335,
#285336,#285337,#285338,#285339,#285340,#285341,#285342,#285343,#285344,
#285345,#285346,#285347,#285348,#285349,#285350,#285351,#285352,#285353,
#285354,#285355,#285356,#285357,#285358,#285359,#285360,#285361,#285362,
#285363,#285364,#285365,#285366,#285367,#285368,#285369,#285370,#285371,
#285372,#285373,#285374,#285375,#285376,#285377,#285378,#285379,#285380,
#285381,#285382,#285383,#285384,#285385,#285386,#285387,#285388,#285389,
#285390,#285391,#285392,#285393,#285394,#285395,#285396,#285397,#285398,
#285399,#285400,#285401,#285402,#285403,#285404,#285405,#285406,#285407,
#285408,#285409,#285410,#285411,#285412,#285413,#285414,#285415,#285416,
#285417,#285418,#285419,#285420,#285421,#285422,#285423,#285424,#285425,
#285426,#285427,#285428,#285429,#285430,#285431,#285432,#285433,#285434,
#285435,#285436,#285437,#285438,#285439,#285440,#285441,#285442,#285443,
#285444,#285445,#285446,#285447,#285448,#285449,#285450,#285451,#285452,
#285453,#285454,#285455,#285456,#285457,#285458,#285459,#285460,#285461,
#285462,#285463,#285464,#285465,#285466,#285467,#285468,#285469,#285470,
#285471,#285472,#285473,#285474,#285475,#285476,#285477,#285478,#285479,
#285480,#285481,#285482,#285483,#285484,#285485,#285486,#285487,#285488,
#285489,#285490,#285491,#285492,#285493,#285494,#285495,#285496,#285497,
#285498,#285499,#285500,#285501,#285502,#285503,#285504,#285505,#285506,
#285507,#285508,#285509,#285510,#285511,#285512,#285513,#285514,#285515,
#285516,#285517,#285518,#285519,#285520,#285521,#285522,#285523,#285524,
#285525,#285526,#285527,#285528,#285529,#285530,#285531,#285532,#285533,
#285534,#285535,#285536,#285537,#285538,#285539,#285540,#285541,#285542,
#285543,#285544,#285545,#285546,#285547,#285548,#285549,#285550,#285551,
#285552,#285553,#285554,#285555,#285556,#285557,#285558,#285559,#285560,
#285561,#285562,#285563,#285564,#285565,#285566,#285567,#285568,#285569,
#285570,#285571,#285572,#285573,#285574,#285575,#285576),.UNSPECIFIED.,
 .F.,.F.,(4,2,2,2,2,2,2,2,2,2,2,2,2,2,2,2,2,2,2,2,2,2,2,2,2,2,2,2,2,2,2,
2,2,2,2,2,2,2,2,2,2,2,2,2,2,2,2,2,2,2,2,2,2,2,2,2,2,2,2,2,2,2,2,2,2,2,2,
2,2,2,2,2,2,2,2,2,2,2,2,2,2,2,2,2,2,2,2,2,2,2,2,2,2,2,2,2,2,2,2,2,2,2,2,
2,2,2,2,2,2,2,2,2,2,2,2,2,2,2,2,2,2,2,2,2,2,2,2,2,2,2,2,2,2,2,2,2,2,2,2,
2,2,2,2,2,2,2,2,2,2,2,2,2,2,2,2,2,2,2,2,2,2,2,2,2,2,2,2,2,2,2,2,2,2,2,2,
2,2,2,2,2,2,2,2,2,2,2,2,2,2,2,2,2,2,2,4),(-1.96144530502008,-1.93247498786435,
-1.91353558129345,-1.90557328408703,-1.90182194876998,-1.89889613009993,
-1.89563200041529,-1.89012366035219,-1.86261338290726,-1.84264468269137,
-1.83216927446595,-1.82767811113443,-1.82430001539754,-1.82237289087038,
-1.82082090019645,-1.81872457774149,-1.81434669450849,-1.78595816191742,
-1.7537602948305,-1.74811046476254,-1.74479536679182,-1.74184270487633,
-1.73808167351323,-1.73200108902136,-1.69917281564604,-1.67313250773391,
-1.6690879797367,-1.66705142660046,-1.66539435404016,-1.66329526210157,
-1.65890993199517,-1.63043197928439,-1.59852931736083,-1.59284828791651,
-1.58953124807139,-1.58658687059593,-1.58285039631289,-1.57684079942884,
-1.53528197559511,-1.51783681667502,-1.51355509819816,-1.51147782211423,
-1.50982714553679,-1.50778674946864,-1.50368981762125,-1.47177856473146,
-1.44250534297963,-1.43698592484077,-1.43370620427395,-1.43076015798068,
-1.42697344117612,-1.4207795001759,-1.38286523394912,-1.36262264413497,
-1.35804564303371,-1.35591372739082,-1.35441879885597,-1.35249424633418,
-1.34906601330943,-1.32612150426807,-1.3082800418873,-1.29369488981543,
-1.28381811580387,-1.27972772286298,-1.2767341744703,-1.27395606328977,
-1.26937051250131,-1.25687158620433,-1.22496623208017,-1.21144558112075,
-1.20614906989429,-1.20215779290578,-1.20013631520272,-1.19848311131509,
-1.19637945333172,-1.19196253696438,-1.16372710123389,-1.13144587809553,
-1.12583799623071,-1.12253713375895,-1.11959112085485,-1.11583064342519,
-1.10973564157068,-1.07682633189008,-1.05796765044349,-1.05151358654305,
-1.04687936656118,-1.0447355883856,-1.04323863195804,-1.04132084366624,
-1.03792162817364,-1.01809572876024,-1.01346319719988,-0.99359381973634,
-0.981074719714654,-0.972210814068069,-0.968327584034351,-0.965357311172369,
-0.962151405066845,-0.956988488027418,-0.936667115455978,-0.909213691381452,
-0.893795707589246,-0.890510301564211,-0.888618055148226,-0.886947644724336,
-0.884655408636248,-0.879164407762766,-0.871040434269514,-0.848283721645345,
-0.820067810080994,-0.814545586142895,-0.811262674084308,-0.808312716223862,
-0.804519381157505,-0.796418838484311,-0.773829466566902,-0.746794905214226,
-0.737367105864967,-0.734483056363565,-0.73269683439966,-0.730978172698518,
-0.728410409780187,-0.721002315962728,-0.708504887994237,-0.666064793484975,
-0.660258479143926,-0.656581926771106,-0.653643863351469,-0.6502900313723,
-0.644431501800792,-0.63720951206192,-0.621003572707466,-0.590348181346645,
-0.581577449643865,-0.578765184137104,-0.576994817128898,-0.575264558817581,
-0.572639435079613,-0.564762791862318,-0.551034646653108,-0.518394711258836,
-0.506682389390157,-0.50220819684779,-0.499450981840181,-0.496443732344158,
-0.492267801069473,-0.48181766182671,-0.465976954076878,-0.435842357682096,
-0.426161628119392,-0.423251765222197,-0.421460063523569,-0.41974541873305,
-0.417197526769793,-0.409944655860342,-0.397839016948237,-0.358079290939424,
-0.349557291243556,-0.345731404748461,-0.342769270729409,-0.339536504849065,
-0.334248766111482,-0.311751482994435,-0.296929463123666,-0.273333274367298,
-0.268767070924094,-0.266635697594257,-0.264981867431886,-0.262985515668597,
-0.259114724534632,-0.254026115725754,-0.2413399079417,-0.199374122236426,
-0.193469181037138,-0.189763965424481,-0.18682365970767,-0.183489384362261,
-0.177722790788746,-0.146100973740853,-0.117370340801937,-0.113009879655894,
-0.110917218883706,-0.109265167824724,-0.107236116696215,-0.103202388991913,
-0.0773980882934182,-0.0523623833717121,-0.0400086742239438,-0.0354440959479153,
-0.0326707257230633,-0.0296762235914756,-0.0267196348771048,-0.0227468179464109,
-0.000459287936663319),.UNSPECIFIED.);
#3928=B_SPLINE_CURVE_WITH_KNOTS('',3,(#285578,#285579,#285580,#285581,#285582,
#285583,#285584,#285585,#285586,#285587,#285588,#285589,#285590,#285591,
#285592,#285593,#285594,#285595,#285596,#285597,#285598,#285599,#285600,
#285601,#285602,#285603,#285604,#285605,#285606,#285607,#285608,#285609,
#285610,#285611,#285612,#285613,#285614,#285615,#285616,#285617,#285618,
#285619,#285620,#285621,#285622,#285623,#285624,#285625,#285626,#285627,
#285628,#285629,#285630,#285631,#285632,#285633,#285634,#285635,#285636,
#285637,#285638,#285639,#285640,#285641,#285642,#285643,#285644,#285645,
#285646,#285647,#285648,#285649,#285650,#285651,#285652,#285653,#285654,
#285655,#285656,#285657,#285658,#285659,#285660,#285661,#285662,#285663,
#285664,#285665,#285666,#285667,#285668,#285669,#285670,#285671,#285672,
#285673,#285674,#285675,#285676,#285677,#285678,#285679,#285680,#285681,
#285682,#285683,#285684,#285685,#285686,#285687,#285688,#285689,#285690,
#285691,#285692,#285693,#285694,#285695,#285696,#285697,#285698,#285699,
#285700,#285701,#285702,#285703,#285704,#285705,#285706,#285707,#285708,
#285709,#285710,#285711,#285712,#285713,#285714,#285715,#285716,#285717,
#285718,#285719,#285720,#285721,#285722,#285723,#285724,#285725,#285726,
#285727,#285728,#285729,#285730,#285731,#285732,#285733,#285734,#285735,
#285736,#285737,#285738,#285739,#285740,#285741,#285742,#285743,#285744,
#285745,#285746,#285747,#285748,#285749,#285750,#285751,#285752,#285753,
#285754,#285755,#285756,#285757,#285758,#285759,#285760,#285761,#285762,
#285763,#285764,#285765,#285766,#285767,#285768,#285769,#285770,#285771,
#285772,#285773,#285774,#285775,#285776,#285777,#285778,#285779,#285780,
#285781,#285782,#285783,#285784,#285785,#285786,#285787,#285788,#285789,
#285790,#285791,#285792,#285793,#285794,#285795,#285796,#285797,#285798,
#285799,#285800,#285801,#285802,#285803,#285804,#285805,#285806,#285807,
#285808,#285809,#285810,#285811,#285812,#285813,#285814,#285815,#285816,
#285817,#285818,#285819,#285820,#285821,#285822,#285823,#285824,#285825,
#285826,#285827,#285828,#285829,#285830,#285831,#285832,#285833,#285834,
#285835,#285836,#285837,#285838,#285839,#285840,#285841,#285842,#285843,
#285844,#285845,#285846,#285847,#285848,#285849,#285850,#285851,#285852,
#285853,#285854,#285855,#285856,#285857,#285858,#285859,#285860,#285861,
#285862,#285863,#285864,#285865,#285866,#285867,#285868,#285869,#285870,
#285871,#285872,#285873,#285874,#285875,#285876,#285877,#285878,#285879,
#285880,#285881,#285882,#285883,#285884,#285885,#285886,#285887,#285888,
#285889,#285890,#285891,#285892,#285893,#285894,#285895,#285896,#285897,
#285898,#285899,#285900,#285901,#285902,#285903,#285904,#285905,#285906,
#285907,#285908,#285909,#285910,#285911,#285912,#285913,#285914,#285915,
#285916,#285917,#285918,#285919,#285920,#285921,#285922,#285923,#285924,
#285925,#285926,#285927,#285928,#285929,#285930,#285931,#285932,#285933,
#285934,#285935,#285936,#285937,#285938,#285939,#285940,#285941,#285942,
#285943,#285944,#285945,#285946,#285947,#285948,#285949,#285950,#285951,
#285952,#285953,#285954,#285955,#285956,#285957,#285958,#285959,#285960,
#285961,#285962,#285963,#285964,#285965,#285966,#285967,#285968,#285969,
#285970,#285971,#285972,#285973,#285974,#285975,#285976,#285977,#285978,
#285979,#285980,#285981,#285982,#285983,#285984,#285985,#285986,#285987,
#285988,#285989,#285990,#285991,#285992,#285993,#285994,#285995,#285996,
#285997,#285998,#285999),.UNSPECIFIED.,.F.,.F.,(4,2,2,2,2,2,2,2,2,2,2,2,
2,2,2,2,2,2,2,2,2,2,2,2,2,2,2,2,2,2,2,2,2,2,2,2,2,2,2,2,2,2,2,2,2,2,2,2,
2,2,2,2,2,2,2,2,2,2,2,2,2,2,2,2,2,2,2,2,2,2,2,2,2,2,2,2,2,2,2,2,2,2,2,2,
2,2,2,2,2,2,2,2,2,2,2,2,2,2,2,2,2,2,2,2,2,2,2,2,2,2,2,2,2,2,2,2,2,2,2,2,
2,2,2,2,2,2,2,2,2,2,2,2,2,2,2,2,2,2,2,2,2,2,2,2,2,2,2,2,2,2,2,2,2,2,2,2,
2,2,2,2,2,2,2,2,2,2,2,2,2,2,2,2,2,2,2,2,2,2,2,2,2,2,2,2,2,2,2,2,2,2,2,2,
2,2,2,2,2,2,2,2,2,2,2,2,2,2,2,2,2,2,4),(-1.96097617311119,-1.92648172026095,
-1.92144978303859,-1.91761256870394,-1.91562326363793,-1.91396921007816,
-1.91182977798171,-1.90738110749659,-1.88132017505689,-1.85816072997489,
-1.8449191029552,-1.84047048366102,-1.84033328447453,-1.84019566491065,
-1.84005707251167,-1.83991692533481,-1.8398751872902,-1.83982787418988,
-1.83977393865892,-1.83971205264128,-1.8396405041543,-1.83955704383589,
-1.83945864973141,-1.83934115347022,-1.83919861986885,-1.83902226156514,
-1.83812360742327,-1.83517857845841,-1.83142341418022,-1.82534566221748,
-1.79223855705023,-1.77352058243651,-1.76709413917351,-1.76247490024346,
-1.76033393844578,-1.75883734267968,-1.75691769147421,-1.75351015155785,
-1.7322010626931,-1.704303008726,-1.68963748892342,-1.68493937869517,-1.6818311871399,
-1.67884667853989,-1.6746284068573,-1.66460738859007,-1.62687776212102,
-1.61027952339574,-1.60643484654714,-1.60444390589062,-1.60278981460966,
-1.60065203101947,-1.59621227249215,-1.56989777605179,-1.54690343073262,
-1.53368668259779,-1.52914758706272,-1.52607151897191,-1.52306273569114,
-1.51871262471361,-1.50787595945546,-1.47109781867542,-1.4593345327151,
-1.45222042839303,-1.44969068610485,-1.44797971553756,-1.44618269262047,
-1.44324822989912,-1.43331912105908,-1.40667528154168,-1.38432102468044,
-1.3762312235098,-1.37244018340436,-1.3694908682763,-1.366207507867,-1.36068172848989,
-1.33343635568799,-1.31380030815897,-1.30314189678026,-1.2964895370781,
-1.29402229594152,-1.29232323886345,-1.29073223529663,-1.28793965234552,
-1.279339360943,-1.24862276845309,-1.23235306109823,-1.22511340472582,-1.21924332795144,
-1.21588718909187,-1.21294957191915,-1.20927683185984,-1.20348310431166,
-1.16676901274106,-1.14373330606955,-1.13972454604812,-1.13770041437847,
-1.13604810619861,-1.13394973188053,-1.12955951658998,-1.10111235522408,
-1.06897947212993,-1.06337971530366,-1.0600806289454,-1.05713437856048,
-1.05337108304634,-1.04726608968305,-1.01461889654089,-0.995589815322286,
-0.989103223382697,-0.984451522179699,-0.982304428340557,-0.980806932201921,
-0.978890870593016,-0.975406611278072,-0.948812683939885,-0.915322179147616,
-0.909259861495045,-0.905508906334006,-0.902564030144349,-0.899257850257001,
-0.893624431492202,-0.861829152006804,-0.833011838486564,-0.828659845685071,
-0.826568741387078,-0.824916662407224,-0.822886027352813,-0.818844606294295,
-0.792590734494492,-0.759747147692339,-0.753652532292492,-0.749892217609193,
-0.746946299185632,-0.743645504480912,-0.738037684882965,-0.705979328666654,
-0.67741971312468,-0.673039359346898,-0.670942830667103,-0.669290556234762,
-0.66726470896295,-0.663247474292977,-0.639326381450649,-0.603758430761133,
-0.597852264313704,-0.594146546988543,-0.591206005968892,-0.587871637222211,
-0.582105331041332,-0.550695345166428,-0.521712415915215,-0.517374470296042,
-0.515286008528386,-0.513633950570073,-0.511600792039232,-0.507546851776991,
-0.480096020660247,-0.448552928829871,-0.442411834691272,-0.438638075974812,
-0.435690610408103,-0.432397368939924,-0.426825469486252,-0.420054771595755,
-0.405416393889887,-0.387607902436536,-0.364682375318631,-0.361254646608957,
-0.359330312303794,-0.357834222486458,-0.355699449321314,-0.351114857249901,
-0.330815179228958,-0.292672923416853,-0.286675509216833,-0.282943304059214,
-0.2800002969124,-0.276682721816685,-0.270995662275378,-0.240195513443058,
-0.210394011935839,-0.206098172323915,-0.204017797183644,-0.202365941259967,
-0.200325364531526,-0.196233846329197,-0.190762107869839,-0.176508524886542,
-0.141976324150346,-0.13223993879323,-0.128473031436335,-0.125711656222681,
-0.122707884716176,-0.122661249473911,-0.122620081809211,-0.122480029330314,
-0.122341511730251,-0.122203946501924,-0.12206678052895,-0.117617805043081,
-0.104382708559042,-0.08124223812719,-0.0551039462552787,-0.0506554313418783,
-0.0485158069987081,-0.0468614766232517,-0.044871660251827,-0.0410330249596302,
-0.0359994959093764,-0.000459535627139337),.UNSPECIFIED.);
#3929=B_SPLINE_CURVE_WITH_KNOTS('',3,(#286001,#286002,#286003,#286004,#286005,
#286006,#286007,#286008,#286009,#286010,#286011,#286012,#286013,#286014,
#286015,#286016,#286017,#286018,#286019,#286020,#286021,#286022,#286023,
#286024,#286025,#286026,#286027,#286028,#286029,#286030,#286031,#286032,
#286033,#286034,#286035,#286036,#286037,#286038,#286039,#286040,#286041,
#286042,#286043,#286044,#286045,#286046,#286047,#286048,#286049,#286050,
#286051,#286052,#286053,#286054,#286055,#286056,#286057,#286058,#286059,
#286060,#286061,#286062,#286063,#286064,#286065,#286066,#286067,#286068,
#286069,#286070,#286071,#286072,#286073,#286074,#286075,#286076,#286077,
#286078,#286079,#286080,#286081,#286082,#286083,#286084,#286085,#286086,
#286087,#286088,#286089,#286090,#286091,#286092,#286093,#286094,#286095,
#286096,#286097,#286098,#286099,#286100,#286101,#286102,#286103,#286104,
#286105,#286106,#286107,#286108,#286109,#286110,#286111,#286112,#286113,
#286114,#286115,#286116,#286117,#286118,#286119,#286120,#286121,#286122,
#286123,#286124,#286125,#286126,#286127,#286128,#286129,#286130,#286131,
#286132,#286133,#286134,#286135,#286136,#286137,#286138,#286139,#286140,
#286141,#286142,#286143,#286144,#286145,#286146,#286147,#286148,#286149,
#286150,#286151,#286152,#286153,#286154,#286155,#286156,#286157,#286158,
#286159,#286160,#286161,#286162,#286163,#286164,#286165,#286166,#286167,
#286168,#286169,#286170,#286171,#286172,#286173,#286174,#286175,#286176,
#286177,#286178,#286179,#286180,#286181,#286182,#286183,#286184,#286185,
#286186,#286187,#286188,#286189,#286190,#286191,#286192,#286193,#286194,
#286195,#286196,#286197,#286198,#286199,#286200,#286201,#286202,#286203,
#286204,#286205,#286206,#286207,#286208,#286209,#286210,#286211,#286212,
#286213,#286214,#286215,#286216,#286217,#286218,#286219,#286220,#286221,
#286222,#286223,#286224,#286225,#286226,#286227,#286228,#286229,#286230,
#286231,#286232,#286233,#286234,#286235,#286236,#286237,#286238,#286239,
#286240,#286241,#286242,#286243,#286244,#286245,#286246,#286247,#286248,
#286249,#286250,#286251,#286252,#286253,#286254,#286255,#286256,#286257,
#286258,#286259,#286260,#286261,#286262,#286263,#286264,#286265,#286266,
#286267,#286268,#286269,#286270,#286271,#286272,#286273,#286274,#286275,
#286276,#286277,#286278,#286279,#286280,#286281,#286282,#286283,#286284,
#286285,#286286,#286287,#286288,#286289,#286290,#286291,#286292,#286293,
#286294,#286295,#286296,#286297,#286298,#286299,#286300,#286301,#286302,
#286303,#286304,#286305,#286306,#286307,#286308,#286309,#286310,#286311,
#286312,#286313,#286314,#286315,#286316,#286317,#286318,#286319,#286320,
#286321,#286322,#286323,#286324,#286325,#286326,#286327,#286328,#286329,
#286330,#286331,#286332,#286333,#286334,#286335,#286336,#286337,#286338,
#286339,#286340,#286341,#286342,#286343,#286344,#286345,#286346,#286347,
#286348,#286349,#286350,#286351,#286352,#286353,#286354,#286355,#286356,
#286357,#286358,#286359,#286360,#286361,#286362,#286363,#286364,#286365,
#286366,#286367,#286368,#286369,#286370,#286371,#286372,#286373,#286374,
#286375,#286376,#286377,#286378,#286379,#286380,#286381,#286382,#286383,
#286384,#286385,#286386,#286387,#286388,#286389,#286390,#286391,#286392,
#286393,#286394,#286395,#286396,#286397,#286398),.UNSPECIFIED.,.F.,.F.,
(4,2,2,2,2,2,2,2,2,2,2,2,2,2,2,2,2,2,2,2,2,2,2,2,2,2,2,2,2,2,2,2,2,2,2,
2,2,2,2,2,2,2,2,2,2,2,2,2,2,2,2,2,2,2,2,2,2,2,2,2,2,2,2,2,2,2,2,2,2,2,2,
2,2,2,2,2,2,2,2,2,2,2,2,2,2,2,2,2,2,2,2,2,2,2,2,2,2,2,2,2,2,2,2,2,2,2,2,
2,2,2,2,2,2,2,2,2,2,2,2,2,2,2,2,2,2,2,2,2,2,2,2,2,2,2,2,2,2,2,2,2,2,2,2,
2,2,2,2,2,2,2,2,2,2,2,2,2,2,2,2,2,2,2,2,2,2,2,2,2,2,2,2,2,2,2,2,2,2,2,2,
2,2,2,2,2,2,2,2,2,2,2,2,2,2,2,2,2,2,2,4),(-1.96116707136439,-1.94032938098075,
-1.93623603192376,-1.93323577925446,-1.93021664785143,-1.92747356243321,
-1.92307788032648,-1.91189426027027,-1.88795224819068,-1.86303303323596,
-1.85660660487735,-1.85412674889354,-1.85242549393443,-1.85083796869957,
-1.848062502269,-1.83960717823325,-1.80880726769486,-1.79248211697445,-1.78181740607288,
-1.77761070027276,-1.77459838702911,-1.77148041381797,-1.76673468902211,
-1.75284501180551,-1.71935975976403,-1.70802308246174,-1.70108455036899,
-1.69857832238842,-1.69687205873429,-1.69506796865554,-1.69210051955368,
-1.68182447539323,-1.65543615720249,-1.63323809174561,-1.62515476202088,
-1.62136518778792,-1.61841636630745,-1.61513289322957,-1.60960529993182,
-1.58311545464052,-1.56318472128824,-1.55223989871783,-1.54546569561789,
-1.54298180659112,-1.54127980998297,-1.539468411491,-1.53646743554575,-1.52581334495316,
-1.4962433237916,-1.48080103679117,-1.47379592459779,-1.4680742377852,-1.46474966063157,
-1.46180826605517,-1.45808869022918,-1.45213369790441,-1.41709670023302,
-1.3925201108095,-1.38862092302812,-1.38661896701896,-1.38496574920625,
-1.38284189925286,-1.37831525546671,-1.35336239090258,-1.32943655282561,
-1.31591870308003,-1.31134503070556,-1.30826210747142,-1.30525915133156,
-1.30093979646001,-1.29031364703222,-1.2532989429309,-1.24150734479943,
-1.23438183421352,-1.23185066196743,-1.23013946252314,-1.228342985901,-1.22541079976777,
-1.21550397169141,-1.18884530996934,-1.16648233078714,-1.15839252245577,
-1.15460157894644,-1.15165238023701,-1.14836919169945,-1.14284380528737,
-1.11557787562328,-1.09588150205664,-1.08527614035128,-1.08074062089714,
-1.07719824908455,-1.07526997308623,-1.07360776081509,-1.07141784600631,
-1.06639349297778,-1.03092004800497,-1.01455874279342,-1.00387784357576,
-0.999668525453434,-0.996655512267341,-0.993905367259333,-0.990184084665382,
-0.980774994246127,-0.966725522207575,-0.938861716387815,-0.924632520309472,
-0.92137879237249,-0.919512205278452,-0.917834135400416,-0.91548945237802,
-0.909668292717997,-0.900857179781513,-0.86390255649341,-0.849579730544484,
-0.844788208871641,-0.84166052731335,-0.83865373726345,-0.834479348532444,
-0.824038175838477,-0.808216833837496,-0.778109559374263,-0.768385999912533,
-0.765471972148649,-0.763679456975874,-0.761965631559021,-0.759421248052782,
-0.752194213394201,-0.74015246395096,-0.700955636462519,-0.692163065700046,
-0.688552455451004,-0.685556028806131,-0.682464485091984,-0.67784841739255,
-0.663953752639336,-0.638805750528158,-0.615573972090987,-0.611445832651618,
-0.609370179295457,-0.607687605243971,-0.605876304169358,-0.602876202218796,
-0.591034294566917,-0.562371522182849,-0.53964305779209,-0.534216374437366,
-0.530954279039788,-0.528000487123094,-0.524170293074934,-0.515859712085657,
-0.491277662271067,-0.460011135743046,-0.455415528562843,-0.45327882465695,
-0.451624789776603,-0.449632951343047,-0.445783953655136,-0.42269392421623,
-0.385763771615181,-0.379997799234613,-0.376333314440817,-0.373396512145373,
-0.370035009648928,-0.364138814150675,-0.356856637842032,-0.34043305319035,
-0.30393668717358,-0.299633358729507,-0.297551630209894,-0.295899857267152,
-0.293860814323333,-0.289776640144051,-0.284317680599918,-0.270117608809778,
-0.235767565068731,-0.225834395206718,-0.221626776433031,-0.21864397605268,
-0.215532529348914,-0.21081946700866,-0.196012422557768,-0.170819006834098,
-0.148749894710541,-0.144623829172003,-0.142548662776975,-0.140866188121952,
-0.139095923550034,-0.136412379258326,-0.133031834155479,-0.126201784087867,
-0.105290659463639,-0.0753270472301669,-0.0691473323490282,-0.0653626963230127,
-0.0624142743786168,-0.0591277139279507,-0.0535862383955478,-0.0232906407447269,
-0.000459678636155689),.UNSPECIFIED.);
#3930=B_SPLINE_CURVE_WITH_KNOTS('',3,(#286400,#286401,#286402,#286403,#286404,
#286405,#286406,#286407,#286408,#286409,#286410),.UNSPECIFIED.,.F.,.F.,
(4,1,1,1,1,1,1,1,4),(53.4070751110265,53.5035269063048,54.500862748857,
55.4981985914093,56.4955344339615,57.4928702765138,58.490206119066,59.4875419616182,
59.690260418206),.UNSPECIFIED.);
#3931=B_SPLINE_CURVE_WITH_KNOTS('',3,(#286412,#286413,#286414,#286415,#286416,
#286417,#286418,#286419,#286420,#286421,#286422,#286423,#286424,#286425,
#286426,#286427,#286428,#286429,#286430,#286431,#286432,#286433,#286434,
#286435,#286436,#286437,#286438,#286439,#286440,#286441,#286442,#286443,
#286444,#286445,#286446,#286447,#286448,#286449,#286450,#286451,#286452,
#286453,#286454,#286455,#286456,#286457,#286458,#286459,#286460,#286461,
#286462,#286463,#286464,#286465,#286466,#286467,#286468,#286469,#286470,
#286471,#286472,#286473,#286474,#286475,#286476,#286477,#286478,#286479,
#286480,#286481,#286482,#286483,#286484,#286485,#286486,#286487,#286488,
#286489,#286490,#286491,#286492,#286493,#286494,#286495,#286496,#286497,
#286498,#286499,#286500,#286501,#286502,#286503,#286504,#286505,#286506,
#286507,#286508,#286509,#286510,#286511,#286512,#286513,#286514,#286515,
#286516,#286517,#286518,#286519,#286520,#286521,#286522,#286523,#286524,
#286525,#286526,#286527,#286528,#286529,#286530,#286531,#286532,#286533,
#286534,#286535,#286536,#286537,#286538,#286539,#286540,#286541,#286542,
#286543,#286544,#286545,#286546,#286547,#286548,#286549,#286550,#286551,
#286552,#286553,#286554,#286555,#286556,#286557,#286558,#286559,#286560,
#286561,#286562,#286563,#286564,#286565,#286566,#286567,#286568,#286569,
#286570,#286571,#286572,#286573,#286574,#286575,#286576,#286577,#286578,
#286579,#286580,#286581,#286582,#286583,#286584,#286585,#286586,#286587,
#286588,#286589,#286590,#286591,#286592,#286593,#286594,#286595,#286596,
#286597,#286598,#286599,#286600,#286601,#286602,#286603,#286604,#286605,
#286606,#286607,#286608,#286609,#286610,#286611,#286612,#286613,#286614,
#286615,#286616,#286617,#286618,#286619,#286620,#286621,#286622,#286623,
#286624,#286625,#286626,#286627,#286628,#286629,#286630,#286631,#286632,
#286633,#286634,#286635,#286636,#286637,#286638,#286639,#286640,#286641,
#286642,#286643,#286644,#286645,#286646,#286647,#286648,#286649,#286650,
#286651,#286652,#286653,#286654,#286655,#286656,#286657,#286658,#286659,
#286660,#286661,#286662,#286663,#286664,#286665,#286666,#286667,#286668,
#286669,#286670,#286671,#286672,#286673,#286674,#286675,#286676,#286677,
#286678,#286679,#286680,#286681,#286682,#286683,#286684,#286685,#286686,
#286687,#286688,#286689,#286690,#286691,#286692,#286693,#286694,#286695,
#286696,#286697,#286698,#286699,#286700,#286701,#286702,#286703,#286704,
#286705,#286706,#286707,#286708,#286709,#286710,#286711,#286712,#286713,
#286714,#286715,#286716,#286717,#286718,#286719,#286720,#286721,#286722,
#286723,#286724,#286725,#286726,#286727,#286728,#286729,#286730,#286731,
#286732,#286733,#286734,#286735,#286736,#286737,#286738,#286739,#286740,
#286741,#286742,#286743,#286744,#286745,#286746,#286747,#286748,#286749,
#286750,#286751,#286752,#286753,#286754,#286755,#286756,#286757,#286758,
#286759,#286760,#286761,#286762,#286763,#286764,#286765,#286766,#286767,
#286768,#286769,#286770,#286771,#286772,#286773,#286774,#286775,#286776,
#286777,#286778,#286779,#286780,#286781,#286782,#286783,#286784,#286785,
#286786,#286787,#286788,#286789,#286790,#286791,#286792,#286793,#286794,
#286795,#286796,#286797,#286798,#286799,#286800,#286801,#286802,#286803,
#286804,#286805,#286806,#286807,#286808,#286809,#286810,#286811,#286812,
#286813,#286814,#286815,#286816,#286817,#286818,#286819,#286820,#286821,
#286822,#286823,#286824,#286825,#286826,#286827,#286828,#286829,#286830,
#286831,#286832,#286833,#286834,#286835,#286836,#286837,#286838,#286839,
#286840,#286841,#286842,#286843,#286844,#286845,#286846,#286847,#286848,
#286849,#286850,#286851,#286852,#286853,#286854,#286855,#286856,#286857,
#286858,#286859,#286860,#286861,#286862,#286863,#286864,#286865,#286866,
#286867,#286868,#286869),.UNSPECIFIED.,.F.,.F.,(4,2,2,2,2,2,2,2,2,2,2,2,
2,2,2,2,2,2,2,2,2,2,2,2,2,2,2,2,2,2,2,2,2,2,2,2,2,2,2,2,2,2,2,2,2,2,2,2,
2,2,2,2,2,2,2,2,2,2,2,2,2,2,2,2,2,2,2,2,2,2,2,2,2,2,2,2,2,2,2,2,2,2,2,2,
2,2,2,2,2,2,2,2,2,2,2,2,2,2,2,2,2,2,2,2,2,2,2,2,2,2,2,2,2,2,2,2,2,2,2,2,
2,2,2,2,2,2,2,2,2,2,2,2,2,2,2,2,2,2,2,2,2,2,2,2,2,2,2,2,2,2,2,2,2,2,2,2,
2,2,2,2,2,2,2,2,2,2,2,2,2,2,2,2,2,2,2,2,2,2,2,2,2,2,2,2,2,2,2,2,2,2,2,2,
2,2,2,2,2,2,2,2,2,2,2,2,2,2,2,2,2,2,2,2,2,2,2,2,2,2,2,2,2,2,2,2,2,2,2,2,
4),(-1.96125649093128,-1.93249964309487,-1.92527261925194,-1.9210310812038,
-1.9171621004257,-1.91420354232668,-1.91096114332999,-1.90562610438211,
-1.88472509267201,-1.8549121737987,-1.84243462342552,-1.839438444461,-1.837859686341,
-1.8362065093369,-1.83408216688999,-1.82955257743335,-1.80453203680034,
-1.78065987849674,-1.76715930968027,-1.76258773773602,-1.7595053320455,
-1.75650220216325,-1.75218139301695,-1.74154622625011,-1.70454442026726,
-1.69275469692247,-1.68563004953296,-1.68309906010746,-1.68138794946653,
-1.67959152902365,-1.67665936935549,-1.66675194487389,-1.64009519586762,
-1.61773364628296,-1.60964420709852,-1.60585343188556,-1.60290436216941,
-1.59962131525331,-1.59409616232599,-1.56683241856893,-1.54713963172143,
-1.53653236917927,-1.52990217928761,-1.52743816467588,-1.52573980893973,
-1.52392143847442,-1.52088882245048,-1.50987497741403,-1.48401341373018,
-1.46213438853691,-1.45406188916704,-1.45027420966382,-1.44732554704481,
-1.4440409027673,-1.43850802766859,-1.41194588076752,-1.39206979940513,
-1.3811415411255,-1.37651678627932,-1.3729207616357,-1.37098128361803,-1.36932115062559,
-1.36714882092381,-1.36222572958359,-1.32663074493653,-1.31025559665232,
-1.30298685510167,-1.29709860608208,-1.29373882674215,-1.29080190363784,
-1.28713513397081,-1.2813611814991,-1.2387500674556,-1.22630749131946,-1.21892181240517,
-1.21635708933794,-1.21463923891366,-1.21285268375927,-1.20996592290161,
-1.20050744894822,-1.17351847000204,-1.1509577008131,-1.142860667075,-1.13906840340673,
-1.13611902931045,-1.13283651687061,-1.127314403531,-1.09900825252285,-1.07732473567713,
-1.06859432629704,-1.06281189828915,-1.06047327355603,-1.05879618526777,
-1.05692684169353,-1.05366030888086,-1.03915274614539,-1.01124829593109,
-0.997427783183198,-0.987917091988905,-0.98388541486729,-0.980902644567638,
-0.977727971556189,-0.972712771385518,-0.954507472564632,-0.933976505964483,
-0.929353721577123,-0.909450560832053,-0.906049806438441,-0.904131598624798,
-0.902634601153879,-0.900491115575262,-0.895858600708775,-0.889408400241348,
-0.87056594422121,-0.837688115475842,-0.831595462859419,-0.82783583266088,
-0.824890138183091,-0.821589270069411,-0.815980514672311,-0.78369195274406,
-0.755424519020071,-0.751007968445111,-0.74890465680967,-0.747252241003928,
-0.745232601058283,-0.741246077878919,-0.735957638570671,-0.722467436509166,
-0.690672821384971,-0.678053870729042,-0.673453339480083,-0.670673448671575,
-0.667683515499592,-0.663608134238003,-0.653820837719149,-0.639420830021098,
-0.611046811063528,-0.597815549616595,-0.594613237786827,-0.592757761864305,
-0.591075655338963,-0.58870587344619,-0.582722093492122,-0.573563446114192,
-0.531681730296335,-0.521578376069416,-0.517349229493336,-0.514362646424345,
-0.511257104647362,-0.50657256770214,-0.492040807694588,-0.464651319189557,
-0.442634910922687,-0.439222407693773,-0.437301560184945,-0.435805009572928,
-0.433665436260411,-0.429054287771109,-0.422643833374612,-0.404007344541578,
-0.370823964571023,-0.364745656962799,-0.360990143698776,-0.358044861629998,
-0.354741529567779,-0.34912125617906,-0.342274806647899,-0.327379048541418,
-0.314658667233377,-0.288761494777877,-0.28424939209484,-0.282128192909907,
-0.280475051826967,-0.278470750167468,-0.274560236886838,-0.2509669969311,
-0.214793595741306,-0.208947437178412,-0.205259457968505,-0.202320764745333,
-0.198975370645524,-0.193155689374181,-0.162757416005791,-0.132753852753097,
-0.128489483515492,-0.126415283668854,-0.12476367526785,-0.124732297688759,
-0.124702296542198,-0.12467357295759,-0.1246460373232,-0.124619608225699,
-0.124594211530914,-0.124569779583865,-0.12454625051809,-0.124523567643961,
-0.12450167891428,-0.12448053645648,-0.124460096158748,-0.124440317305584,
-0.124421162255323,-0.124402596149197,-0.124384586658954,-0.124367103756732,
-0.124350119516051,-0.124333607925302,-0.124317544724245,-0.124301907254373,
-0.124286674331743,-0.124271826124383,-0.124257344045043,-0.124243210650526,
-0.124229409558503,-0.124215925361643,-0.124202743557482,-0.124189850476127,
-0.12202245600517,-0.11678894468266,-0.108990823794884,-0.0817257648201424,
-0.057378486359362,-0.0519080092400297,-0.0486365198836584,-0.0456848002917184,
-0.041872269708007,-0.0377109310250489,-0.0306901428147373,-0.0004594071072521),
 .UNSPECIFIED.);
#3932=B_SPLINE_CURVE_WITH_KNOTS('',3,(#286871,#286872,#286873,#286874,#286875,
#286876,#286877,#286878,#286879,#286880,#286881,#286882,#286883,#286884,
#286885,#286886,#286887,#286888,#286889,#286890,#286891,#286892,#286893,
#286894,#286895,#286896,#286897,#286898,#286899,#286900,#286901,#286902,
#286903,#286904,#286905,#286906,#286907,#286908,#286909,#286910,#286911,
#286912,#286913,#286914,#286915,#286916,#286917,#286918,#286919,#286920,
#286921,#286922,#286923,#286924,#286925,#286926,#286927,#286928,#286929,
#286930,#286931,#286932,#286933,#286934,#286935,#286936,#286937,#286938,
#286939,#286940,#286941,#286942,#286943,#286944,#286945,#286946,#286947,
#286948,#286949,#286950,#286951,#286952,#286953,#286954,#286955,#286956,
#286957,#286958,#286959,#286960,#286961,#286962,#286963,#286964,#286965,
#286966,#286967,#286968,#286969,#286970,#286971,#286972,#286973,#286974,
#286975,#286976,#286977,#286978,#286979,#286980,#286981,#286982,#286983,
#286984,#286985,#286986,#286987,#286988,#286989,#286990,#286991,#286992,
#286993,#286994,#286995,#286996,#286997,#286998,#286999,#287000,#287001,
#287002,#287003,#287004,#287005,#287006,#287007,#287008,#287009,#287010,
#287011,#287012,#287013,#287014,#287015,#287016,#287017,#287018,#287019,
#287020,#287021,#287022,#287023,#287024,#287025,#287026,#287027,#287028,
#287029,#287030,#287031,#287032,#287033,#287034,#287035,#287036,#287037,
#287038,#287039,#287040,#287041,#287042,#287043,#287044,#287045,#287046,
#287047,#287048,#287049,#287050,#287051,#287052,#287053,#287054,#287055,
#287056,#287057,#287058,#287059,#287060,#287061,#287062,#287063,#287064,
#287065,#287066,#287067,#287068,#287069,#287070,#287071,#287072,#287073,
#287074,#287075,#287076,#287077,#287078,#287079,#287080,#287081,#287082,
#287083,#287084,#287085,#287086,#287087,#287088,#287089,#287090,#287091,
#287092,#287093,#287094,#287095,#287096,#287097,#287098,#287099,#287100,
#287101,#287102,#287103,#287104,#287105,#287106,#287107,#287108,#287109,
#287110,#287111,#287112,#287113,#287114,#287115,#287116,#287117,#287118,
#287119,#287120,#287121,#287122,#287123,#287124,#287125,#287126,#287127,
#287128,#287129,#287130,#287131,#287132,#287133,#287134,#287135,#287136,
#287137,#287138,#287139,#287140,#287141,#287142,#287143,#287144,#287145,
#287146,#287147,#287148,#287149,#287150,#287151,#287152,#287153,#287154,
#287155,#287156,#287157,#287158,#287159,#287160,#287161,#287162,#287163,
#287164,#287165,#287166,#287167,#287168,#287169,#287170,#287171,#287172,
#287173,#287174,#287175,#287176,#287177,#287178,#287179,#287180,#287181,
#287182,#287183,#287184,#287185,#287186,#287187,#287188,#287189,#287190,
#287191,#287192,#287193,#287194,#287195,#287196,#287197,#287198,#287199,
#287200,#287201,#287202,#287203,#287204,#287205,#287206,#287207,#287208,
#287209,#287210,#287211,#287212,#287213,#287214,#287215,#287216,#287217,
#287218,#287219,#287220,#287221,#287222,#287223,#287224,#287225,#287226,
#287227,#287228,#287229,#287230,#287231,#287232,#287233,#287234,#287235,
#287236,#287237,#287238,#287239,#287240,#287241,#287242,#287243,#287244,
#287245,#287246,#287247,#287248,#287249,#287250,#287251,#287252,#287253,
#287254,#287255,#287256,#287257,#287258,#287259,#287260,#287261,#287262,
#287263,#287264,#287265,#287266,#287267,#287268,#287269,#287270,#287271,
#287272,#287273,#287274),.UNSPECIFIED.,.F.,.F.,(4,2,2,2,2,2,2,2,2,2,2,2,
2,2,2,2,2,2,2,2,2,2,2,2,2,2,2,2,2,2,2,2,2,2,2,2,2,2,2,2,2,2,2,2,2,2,2,2,
2,2,2,2,2,2,2,2,2,2,2,2,2,2,2,2,2,2,2,2,2,2,2,2,2,2,2,2,2,2,2,2,2,2,2,2,
2,2,2,2,2,2,2,2,2,2,2,2,2,2,2,2,2,2,2,2,2,2,2,2,2,2,2,2,2,2,2,2,2,2,2,2,
2,2,2,2,2,2,2,2,2,2,2,2,2,2,2,2,2,2,2,2,2,2,2,2,2,2,2,2,2,2,2,2,2,2,2,2,
2,2,2,2,2,2,2,2,2,2,2,2,2,2,2,2,2,2,2,2,2,2,2,2,2,2,2,2,2,2,2,2,2,2,2,2,
2,2,2,2,2,2,2,2,2,4),(-1.96117523376116,-1.9425871113232,-1.93582413289111,
-1.93356944763943,-1.9319048855407,-1.93023509530763,-1.92834224070789,
-1.92505361015502,-1.90952745767491,-1.88709371903652,-1.86295356598266,
-1.85735185262359,-1.85400524143428,-1.85106700210845,-1.8473816160519,
-1.84154365867909,-1.79907408936262,-1.78220084698977,-1.77798460336861,
-1.77591977381511,-1.77426832093338,-1.77221337093403,-1.76804783281997,
-1.7369360840567,-1.70806847270669,-1.70194596819273,-1.6985372411934,-1.69560460641459,
-1.692003467634,-1.68645167259274,-1.64768908377773,-1.62717173439072,-1.62256575632003,
-1.62042715145894,-1.61893074983333,-1.61700930405983,-1.61359407819643,
-1.59129697258016,-1.57384502960741,-1.55862153955374,-1.54844995952658,
-1.54431576349085,-1.54131593331185,-1.5385498964627,-1.53402574858458,
-1.5219627818578,-1.48963032564364,-1.47598560201299,-1.47065952452288,
-1.46665170565154,-1.46462781104101,-1.46297556343292,-1.46087709770335,
-1.45648613167355,-1.42804753523019,-1.39597946780613,-1.39034242557826,
-1.38703551358725,-1.38409081370666,-1.3803412211144,-1.37428346399596,
-1.32746837487048,-1.31804693994638,-1.31194252648618,-1.30955433813698,
-1.30786908115524,-1.3060211185988,-1.30285396005132,-1.29009812957261,
-1.26546705863994,-1.2484343821876,-1.23746315500973,-1.23321200009674,
-1.23019105196488,-1.22744838911326,-1.22305793816902,-1.21191343296223,
-1.17546609068989,-1.16374208899384,-1.1566436289,-1.15411570637544,-1.15240491070424,
-1.15060694637229,-1.14766895970902,-1.13770690909045,-1.11108203482744,
-1.0887383720867,-1.08064787184621,-1.07685636120765,-1.07390662107459,
-1.07062272720899,-1.06509590223077,-1.03787815120095,-1.01833260223083,
-1.00759302434389,-1.00090556981874,-0.998433219918652,-0.996733033796596,
-0.994916950281445,-0.991896022495409,-0.981018549502324,-0.956356948880598,
-0.928868120827255,-0.923345124084904,-0.920062118321725,-0.917112308735936,
-0.913319499134517,-0.905221499880774,-0.882711551884798,-0.855813147171446,
-0.846196196829128,-0.84329268917213,-0.841502292164372,-0.839786591086042,
-0.837233698164022,-0.829942586931405,-0.817741404974387,-0.777114842096857,
-0.769262526201464,-0.765514403805289,-0.762569569954733,-0.759261159669255,
-0.753618202526029,-0.746736476030524,-0.731721400596798,-0.7160024082303,
-0.711378480646719,-0.69155917495168,-0.688159106745386,-0.686240919769652,
-0.68474370743409,-0.68259961203249,-0.677964581606929,-0.671509947677267,
-0.652646107575983,-0.619792756218384,-0.613698152466842,-0.609937730003768,
-0.606991658963416,-0.603690622457731,-0.598082215027035,-0.566053751553693,
-0.537454379288816,-0.533078339530897,-0.530982560359543,-0.52933022158672,
-0.527303489724267,-0.523282157771495,-0.498987088380991,-0.463872587888669,
-0.45792526499283,-0.454207452086069,-0.45126564116114,-0.447938673114906,
-0.442207971923826,-0.410519851609205,-0.38178042053347,-0.377419948769166,
-0.375327117350919,-0.373674849154067,-0.3716454286692,-0.367610661170329,
-0.342028770352246,-0.30842566119763,-0.302368883386296,-0.298619314141658,
-0.295674308750209,-0.292366713449642,-0.286727684966135,-0.25462722712635,
-0.226184127271019,-0.221788662205397,-0.219689158400265,-0.218036650861948,
-0.216013111108445,-0.212007964384416,-0.206687384714323,-0.193066335281392,
-0.16081157631273,-0.148685318741221,-0.144151907571838,-0.14138391389431,
-0.138541736294864,-0.138443487584753,-0.138354902608545,-0.138274130023016,
-0.138199748716675,-0.138130644953762,-0.138065929582462,-0.138004880677656,
-0.134409769665758,-0.12988548965373,-0.121921998401925,-0.102914998011306,
-0.0732463525957487,-0.0670866595308566,-0.0646235313852827,-0.0629418291035602,
-0.061127853858408,-0.0581165951381371,-0.0461290615911358,-0.000459593433154411),
 .UNSPECIFIED.);
#3933=B_SPLINE_CURVE_WITH_KNOTS('',3,(#287276,#287277,#287278,#287279,#287280,
#287281,#287282,#287283,#287284,#287285,#287286,#287287,#287288,#287289,
#287290,#287291,#287292,#287293,#287294,#287295,#287296,#287297,#287298,
#287299,#287300,#287301,#287302,#287303,#287304,#287305,#287306,#287307,
#287308,#287309,#287310,#287311,#287312,#287313,#287314,#287315,#287316,
#287317,#287318,#287319,#287320,#287321,#287322,#287323,#287324,#287325,
#287326,#287327,#287328,#287329,#287330,#287331,#287332,#287333,#287334,
#287335,#287336,#287337,#287338,#287339,#287340,#287341,#287342,#287343,
#287344,#287345,#287346,#287347,#287348,#287349,#287350,#287351,#287352,
#287353,#287354,#287355,#287356,#287357,#287358,#287359,#287360,#287361,
#287362,#287363,#287364,#287365,#287366,#287367,#287368,#287369,#287370,
#287371,#287372,#287373,#287374,#287375,#287376,#287377,#287378,#287379,
#287380,#287381,#287382,#287383,#287384,#287385,#287386,#287387,#287388,
#287389,#287390,#287391,#287392,#287393,#287394,#287395,#287396,#287397,
#287398,#287399,#287400,#287401,#287402,#287403,#287404,#287405,#287406,
#287407,#287408,#287409,#287410,#287411,#287412,#287413,#287414,#287415,
#287416,#287417,#287418,#287419,#287420,#287421,#287422,#287423,#287424,
#287425,#287426,#287427,#287428,#287429,#287430,#287431,#287432,#287433,
#287434,#287435,#287436,#287437,#287438,#287439,#287440,#287441,#287442,
#287443,#287444,#287445,#287446,#287447,#287448,#287449,#287450,#287451,
#287452,#287453,#287454,#287455,#287456,#287457,#287458,#287459,#287460,
#287461,#287462,#287463,#287464,#287465,#287466,#287467,#287468,#287469,
#287470,#287471,#287472,#287473,#287474,#287475,#287476,#287477,#287478,
#287479,#287480,#287481,#287482,#287483,#287484,#287485,#287486,#287487,
#287488,#287489,#287490,#287491,#287492,#287493,#287494,#287495,#287496,
#287497,#287498,#287499,#287500,#287501,#287502,#287503,#287504,#287505,
#287506,#287507,#287508,#287509,#287510,#287511,#287512,#287513,#287514,
#287515,#287516,#287517,#287518,#287519,#287520,#287521,#287522,#287523,
#287524,#287525,#287526,#287527,#287528,#287529,#287530,#287531,#287532,
#287533,#287534,#287535,#287536,#287537,#287538,#287539,#287540,#287541,
#287542,#287543,#287544,#287545,#287546,#287547,#287548,#287549,#287550,
#287551,#287552,#287553,#287554,#287555,#287556,#287557,#287558,#287559,
#287560,#287561,#287562,#287563,#287564,#287565,#287566,#287567,#287568,
#287569,#287570,#287571,#287572,#287573,#287574,#287575,#287576,#287577,
#287578,#287579,#287580,#287581,#287582,#287583,#287584,#287585,#287586,
#287587,#287588,#287589,#287590,#287591,#287592,#287593,#287594,#287595,
#287596,#287597,#287598,#287599,#287600,#287601,#287602,#287603,#287604,
#287605,#287606,#287607,#287608,#287609,#287610,#287611,#287612,#287613,
#287614,#287615,#287616,#287617,#287618,#287619,#287620,#287621,#287622,
#287623,#287624,#287625,#287626,#287627,#287628,#287629,#287630,#287631,
#287632,#287633,#287634,#287635,#287636,#287637,#287638,#287639,#287640,
#287641,#287642,#287643,#287644,#287645,#287646,#287647,#287648,#287649,
#287650,#287651,#287652,#287653,#287654,#287655,#287656,#287657,#287658,
#287659,#287660,#287661,#287662,#287663,#287664,#287665),.UNSPECIFIED.,
 .F.,.F.,(4,2,2,2,2,2,2,2,2,2,2,2,2,2,2,2,2,2,2,2,2,2,2,2,2,2,2,2,2,2,2,
2,2,2,2,2,2,2,2,2,2,2,2,2,2,2,2,2,2,2,2,2,2,2,2,2,2,2,2,2,2,2,2,2,2,2,2,
2,2,2,2,2,2,2,2,2,2,2,2,2,2,2,2,2,2,2,2,2,2,2,2,2,2,2,2,2,2,2,2,2,2,2,2,
2,2,2,2,2,2,2,2,2,2,2,2,2,2,2,2,2,2,2,2,2,2,2,2,2,2,2,2,2,2,2,2,2,2,2,2,
2,2,2,2,2,2,2,2,2,2,2,2,2,2,2,2,2,2,2,2,2,2,2,2,2,2,2,2,2,2,2,2,2,2,2,2,
2,2,2,2,2,2,2,2,2,2,2,2,2,2,2,2,2,2,2,4),(-1.96104829234917,-1.95562578488271,
-1.95119962367166,-1.9482848213421,-1.94548168844373,-1.94232769765138,
-1.93740838667848,-1.92181122818972,-1.90144905710625,-1.87470367379065,
-1.87082277072753,-1.86882469190365,-1.86717146903657,-1.86504350710011,
-1.86049375427697,-1.83597398092297,-1.81176924572673,-1.79816448213047,
-1.79358138831612,-1.79049687231796,-1.78749594583543,-1.7838660451886,
-1.77501435278891,-1.73955410055214,-1.72505214493821,-1.71952255372207,
-1.71539875062142,-1.71335210337081,-1.71170073920461,-1.70962776509182,
-1.70536882564841,-1.67505875230187,-1.64498138287798,-1.63917503515137,
-1.63583269846025,-1.63289399116935,-1.62920240449327,-1.62334308302571,
-1.58114095177767,-1.56853818734285,-1.5610900005564,-1.55851754952362,
-1.55679826843684,-1.55501416342521,-1.5521380859804,-1.54277978083191,
-1.51571963128851,-1.49311746956612,-1.48501964397204,-1.4812274725302,
-1.47827836101775,-1.47499633604394,-1.46947552096949,-1.44309356049383,
-1.42310619217173,-1.41212046890976,-1.40532897658317,-1.40284272377062,
-1.40114028689987,-1.39932969338928,-1.39633237923103,-1.38572010344219,
-1.35612862553347,-1.34066956369736,-1.33365963792748,-1.32793489930486,
-1.32460968403595,-1.32166839762211,-1.31794986653969,-1.31199844562999,
-1.27023601667175,-1.25294264095831,-1.24867825362724,-1.24660407847479,
-1.24495250699374,-1.24290652808938,-1.23878687479586,-1.20706798089512,
-1.18209912131909,-1.17388276224925,-1.17006928578109,-1.16711753594338,
-1.16384672175825,-1.15837911859481,-1.13421216648516,-1.10676584821308,
-1.09515115893936,-1.09216800077745,-1.09036039983754,-1.08867578843895,
-1.08659208894007,-1.08140904374581,-1.05087864040884,-1.02670620654232,
-1.01835283322309,-1.01451505509316,-1.0115602372279,-1.00830184345696,
-1.00289288695995,-0.980626562145746,-0.965752131220844,-0.942226858389223,
-0.937709364879942,-0.935579053573708,-0.933922917316097,-0.931953590827468,
-0.928214337457664,-0.90287736406926,-0.868457023292409,-0.862455637045603,
-0.858722469045465,-0.855779609727459,-0.852463155423185,-0.846780446009887,
-0.81504180239075,-0.786271239235246,-0.78191521871105,-0.779823449258368,
-0.778171481381033,-0.776141767022511,-0.772104475446446,-0.746218497458143,
-0.712969865568958,-0.706895109473288,-0.703140686792894,-0.700195603748465,
-0.696891811739635,-0.691269041872597,-0.684418620676052,-0.669509057031735,
-0.656290903173045,-0.63092658892971,-0.626408254314294,-0.624285937770609,
-0.622632792960377,-0.620629542395053,-0.616724021250156,-0.594030907040117,
-0.556716632612083,-0.550994253014773,-0.547342682583301,-0.544406968692705,
-0.541036582341685,-0.535097577840513,-0.504358525383716,-0.474992338569497,
-0.470677188626253,-0.468593279390831,-0.466941572087641,-0.464904828710772,
-0.460831852670636,-0.455392417899417,-0.441274166276935,-0.407222546131526,
-0.396979000491341,-0.39272938866145,-0.389739251203292,-0.386639300102201,
-0.381981504688189,-0.3677011655834,-0.341224022370567,-0.319769261644209,
-0.315217033054216,-0.313088438463031,-0.311434984240698,-0.30943692280356,
-0.305556906668377,-0.279306805244778,-0.246182646921141,-0.240102127294107,
-0.236346162762977,-0.233401070820366,-0.230098518024297,-0.224480989536222,
-0.192473473150695,-0.16388621508564,-0.159509715836151,-0.157455203662948,
-0.155830625770511,-0.154253975644828,-0.150980029631323,-0.134319316703853,
-0.101223408466219,-0.0869708181774452,-0.082187148631304,-0.079061232020367,
-0.0760536828529272,-0.0718741958664859,-0.0613972647754574,-0.0454953477256854,
-0.0117766791592439,-0.00503669273596484,-0.00253609892261398,-0.00120573359873185,
-0.000459188421704137),.UNSPECIFIED.);
#3934=B_SPLINE_CURVE_WITH_KNOTS('',3,(#287666,#287667,#287668,#287669,#287670,
#287671,#287672,#287673,#287674,#287675,#287676,#287677,#287678,#287679,
#287680,#287681,#287682,#287683,#287684,#287685,#287686,#287687,#287688,
#287689,#287690,#287691,#287692,#287693,#287694,#287695,#287696,#287697,
#287698,#287699,#287700,#287701,#287702,#287703,#287704,#287705,#287706,
#287707,#287708,#287709,#287710,#287711,#287712,#287713,#287714,#287715,
#287716,#287717,#287718,#287719,#287720,#287721,#287722,#287723,#287724,
#287725,#287726,#287727,#287728,#287729,#287730,#287731,#287732,#287733,
#287734,#287735,#287736,#287737,#287738,#287739,#287740,#287741,#287742,
#287743,#287744,#287745,#287746,#287747,#287748,#287749,#287750,#287751,
#287752,#287753,#287754,#287755,#287756,#287757,#287758,#287759,#287760,
#287761,#287762,#287763,#287764,#287765,#287766,#287767,#287768,#287769,
#287770,#287771,#287772,#287773,#287774,#287775,#287776,#287777,#287778,
#287779,#287780,#287781,#287782,#287783,#287784,#287785,#287786,#287787,
#287788,#287789,#287790,#287791,#287792,#287793,#287794,#287795,#287796,
#287797,#287798,#287799,#287800,#287801,#287802,#287803,#287804,#287805,
#287806,#287807,#287808,#287809,#287810,#287811,#287812,#287813,#287814,
#287815,#287816,#287817,#287818,#287819,#287820,#287821,#287822,#287823,
#287824,#287825,#287826,#287827,#287828,#287829,#287830,#287831,#287832,
#287833,#287834,#287835,#287836,#287837,#287838,#287839,#287840,#287841,
#287842,#287843,#287844,#287845,#287846,#287847,#287848,#287849,#287850,
#287851,#287852,#287853,#287854,#287855,#287856,#287857,#287858,#287859,
#287860,#287861,#287862,#287863,#287864,#287865,#287866,#287867,#287868,
#287869,#287870,#287871,#287872,#287873,#287874,#287875,#287876,#287877,
#287878,#287879,#287880,#287881,#287882,#287883,#287884,#287885,#287886,
#287887,#287888,#287889,#287890,#287891,#287892,#287893,#287894,#287895,
#287896,#287897,#287898,#287899,#287900,#287901,#287902,#287903,#287904,
#287905,#287906,#287907,#287908,#287909,#287910,#287911,#287912,#287913,
#287914,#287915,#287916,#287917,#287918,#287919,#287920,#287921,#287922,
#287923,#287924,#287925,#287926,#287927,#287928,#287929,#287930,#287931,
#287932,#287933,#287934,#287935,#287936,#287937,#287938,#287939,#287940,
#287941,#287942,#287943,#287944,#287945,#287946,#287947,#287948,#287949,
#287950,#287951,#287952,#287953,#287954,#287955,#287956,#287957,#287958,
#287959,#287960,#287961,#287962,#287963,#287964,#287965,#287966,#287967,
#287968,#287969,#287970,#287971,#287972,#287973,#287974,#287975,#287976,
#287977,#287978,#287979,#287980,#287981,#287982,#287983,#287984,#287985,
#287986,#287987,#287988,#287989,#287990,#287991,#287992,#287993,#287994,
#287995,#287996,#287997,#287998,#287999,#288000,#288001,#288002,#288003,
#288004,#288005,#288006,#288007,#288008,#288009,#288010,#288011,#288012,
#288013,#288014,#288015,#288016,#288017,#288018,#288019,#288020,#288021,
#288022,#288023,#288024,#288025,#288026,#288027,#288028,#288029,#288030,
#288031,#288032,#288033,#288034,#288035,#288036,#288037,#288038,#288039,
#288040,#288041,#288042,#288043,#288044,#288045,#288046,#288047,#288048,
#288049,#288050,#288051,#288052,#288053,#288054,#288055,#288056,#288057,
#288058,#288059),.UNSPECIFIED.,.F.,.F.,(4,2,2,2,2,2,2,2,2,2,2,2,2,2,2,2,
2,2,2,2,2,2,2,2,2,2,2,2,2,2,2,2,2,2,2,2,2,2,2,2,2,2,2,2,2,2,2,2,2,2,2,2,
2,2,2,2,2,2,2,2,2,2,2,2,2,2,2,2,2,2,2,2,2,2,2,2,2,2,2,2,2,2,2,2,2,2,2,2,
2,2,2,2,2,2,2,2,2,2,2,2,2,2,2,2,2,2,2,2,2,2,2,2,2,2,2,2,2,2,2,2,2,2,2,2,
2,2,2,2,2,2,2,2,2,2,2,2,2,2,2,2,2,2,2,2,2,2,2,2,2,2,2,2,2,2,2,2,2,2,2,2,
2,2,2,2,2,2,2,2,2,2,2,2,2,2,2,2,2,2,2,2,2,2,2,2,2,2,2,2,2,2,2,2,2,2,2,2,
4),(-1.9611673957392,-1.96016519546567,-1.95806538538097,-1.95278185055767,
-1.92364544687139,-1.89436234085666,-1.88839906744968,-1.88502417177433,
-1.88208976907284,-1.87844663995391,-1.87138498223882,-1.82523864669928,
-1.81131457205485,-1.80817724511147,-1.80661198665112,-1.80503286300625,
-1.80294845355175,-1.79840870030172,-1.77335105337488,-1.74952112883501,
-1.73603458245084,-1.73146493035852,-1.72838314132594,-1.72538010075568,
-1.72174178211632,-1.71274134917748,-1.67740646933661,-1.66293791591079,
-1.65741613364037,-1.65329676537599,-1.65125099478705,-1.64959961310219,
-1.64752570551909,-1.64326198815116,-1.61301500819911,-1.58346032774662,
-1.57732951285517,-1.5739192553444,-1.57098700560496,-1.56738849405611,
-1.56184493976454,-1.52302542333784,-1.5025499704124,-1.49794839041937,
-1.49581071980139,-1.49431455817983,-1.49239285293329,-1.48897585029047,
-1.46653589014626,-1.44033503255081,-1.42522077937578,-1.4204772665667,
-1.41735980959863,-1.41438140923533,-1.41019723486105,-1.40045601130615,
-1.3659081961078,-1.35165105251854,-1.34617877205721,-1.34208748441745,
-1.34004718626234,-1.3383956443995,-1.33631579057709,-1.33202142795984,
-1.30224086670305,-1.27160103189081,-1.2658391302085,-1.26250603709949,
-1.25956586151176,-1.25585958926541,-1.2499503675809,-1.21439732416657,
-1.19017252824694,-1.18632138550885,-1.18432913671439,-1.18267507371549,
-1.1805387636451,-1.1759456998215,-1.15260536820296,-1.12759142186693,-1.11373749971027,
-1.10912588280886,-1.10603509595507,-1.10303772639204,-1.09874973639694,
-1.08829507911383,-1.04683355271912,-1.03769688604123,-1.03172377170882,
-1.02935553230645,-1.02767370017678,-1.0258177510275,-1.02261263008967,
-1.00932326852602,-0.981008977022601,-0.959635617359899,-0.954272034446866,
-0.951023485142151,-0.948066467553294,-0.944209850276027,-0.935747962742308,
-0.924003554405793,-0.903016213465774,-0.899570304842173,-0.878288119037644,
-0.874879972801479,-0.87296021427923,-0.87146362229038,-0.869322898507965,
-0.864705172039215,-0.858282536669326,-0.839584271391387,-0.806477244695053,
-0.80039366696955,-0.79663648932047,-0.793690859339245,-0.790388134409911,
-0.784771385638642,-0.777930488199467,-0.763053741948654,-0.751011459186111,
-0.724361076229272,-0.720316173979186,-0.718260704439915,-0.716582639652633,
-0.714759860196404,-0.711711225023784,-0.699209560324061,-0.666555405839308,
-0.648129225779971,-0.642946402973789,-0.639735216273813,-0.636764676574435,
-0.632819935596121,-0.623848778231175,-0.611118747481093,-0.591458523056005,
-0.587032305596243,-0.567115638374932,-0.56371437882382,-0.561795908648431,
-0.560300002934469,-0.558159234916667,-0.553533867101322,-0.547095395556165,
-0.528308420461051,-0.495312692365467,-0.489225328597204,-0.485469200234375,
-0.482526532002409,-0.479229443962417,-0.473628359517275,-0.441294490502044,
-0.413061951103913,-0.408642309859204,-0.406539593377406,-0.404888207682348,
-0.402870625101657,-0.398892978374733,-0.373718499471914,-0.339483567433424,
-0.333460015780257,-0.329719324433717,-0.326774321659905,-0.323459406606933,
-0.317789233447674,-0.285697930154697,-0.257383744529701,-0.252972870071412,
-0.250868802025502,-0.249211428455891,-0.247178898514742,-0.24315520439613,
-0.219066434949421,-0.183997054195899,-0.178069014690526,-0.174351947776504,
-0.171403285390817,-0.168060339157487,-0.162280065897901,-0.130174799117912,
-0.101962090833413,-0.0975347085064821,-0.0954288346192596,-0.0937818577306343,
-0.091782605764983,-0.0878475325360492,-0.0826388017654838,-0.0694404849422195,
-0.041018148063621,-0.0250328156673991,-0.020094173685207,-0.0169509929212847,
-0.0141621129991528,-0.0112755590203426,-0.00655231744414157,-0.000479338372087868),
 .UNSPECIFIED.);
#3935=B_SPLINE_CURVE_WITH_KNOTS('',3,(#288062,#288063,#288064,#288065,#288066,
#288067,#288068,#288069,#288070,#288071,#288072,#288073,#288074,#288075,
#288076,#288077,#288078,#288079,#288080,#288081,#288082,#288083),
 .UNSPECIFIED.,.F.,.F.,(4,2,2,2,2,2,2,2,2,2,4),(-0.474818783494366,-0.449281592936105,
-0.422497485793653,-0.381203422480266,-0.329907980372939,-0.265893426931644,
-0.195666061625486,-0.136911508948015,-0.0686118601292609,-0.0311014517309063,
-2.45319125318871E-5),.UNSPECIFIED.);
#3936=B_SPLINE_CURVE_WITH_KNOTS('',3,(#288084,#288085,#288086,#288087,#288088,
#288089,#288090,#288091,#288092,#288093,#288094,#288095,#288096,#288097,
#288098,#288099,#288100,#288101,#288102,#288103,#288104,#288105,#288106,
#288107,#288108,#288109,#288110,#288111,#288112,#288113,#288114,#288115,
#288116,#288117,#288118,#288119,#288120,#288121,#288122,#288123,#288124,
#288125,#288126,#288127,#288128,#288129,#288130,#288131,#288132,#288133,
#288134,#288135,#288136,#288137,#288138,#288139,#288140,#288141,#288142,
#288143,#288144),.UNSPECIFIED.,.F.,.F.,(4,3,3,3,3,3,3,3,3,3,3,3,3,3,3,3,
3,3,3,3,4),(-0.271362855059921,-0.249815156703991,-0.228817954605844,-0.214757059032555,
-0.202695986178297,-0.199258382274391,-0.179079040584676,-0.172574372312687,
-0.151002575773601,-0.132127253801901,-0.128545223737615,-0.108660382312346,
-0.0889046320299183,-0.0695673553379917,-0.0643976613730527,-0.0611873083345303,
-0.0424332578302701,-0.0240014673407122,-0.00742675770561789,-0.00610701619818059,
-1.67978587627156E-14),.UNSPECIFIED.);
#3937=B_SPLINE_CURVE_WITH_KNOTS('',3,(#288146,#288147,#288148,#288149,#288150,
#288151,#288152,#288153,#288154,#288155,#288156,#288157,#288158,#288159,
#288160,#288161,#288162,#288163,#288164,#288165,#288166,#288167,#288168,
#288169,#288170,#288171,#288172,#288173,#288174,#288175,#288176,#288177,
#288178,#288179,#288180,#288181,#288182,#288183,#288184,#288185,#288186,
#288187,#288188,#288189,#288190,#288191,#288192,#288193,#288194,#288195,
#288196,#288197,#288198,#288199,#288200,#288201,#288202,#288203,#288204,
#288205,#288206,#288207,#288208,#288209,#288210,#288211,#288212,#288213,
#288214,#288215,#288216,#288217,#288218,#288219,#288220,#288221,#288222,
#288223,#288224,#288225,#288226,#288227,#288228,#288229,#288230,#288231,
#288232,#288233,#288234,#288235,#288236,#288237,#288238,#288239,#288240,
#288241,#288242,#288243,#288244,#288245,#288246,#288247,#288248,#288249,
#288250,#288251),.UNSPECIFIED.,.F.,.F.,(4,3,3,3,3,3,3,3,3,3,3,3,3,3,3,3,
3,3,3,3,3,3,3,3,3,3,3,3,3,3,3,3,3,3,3,4),(-0.468287143792459,-0.449159592277506,
-0.442679572366002,-0.439139523917826,-0.418501747794262,-0.397540534942074,
-0.376759689901926,-0.369408338867191,-0.366188435771172,-0.344993296658329,
-0.324164935680159,-0.314417154781481,-0.302674036643168,-0.298303152413865,
-0.294792657786698,-0.273759483634418,-0.252453791079512,-0.23671297526563,
-0.228622459040654,-0.22484613779528,-0.221071692886511,-0.199520974492535,
-0.177947952659577,-0.156760757052952,-0.151824997028116,-0.148277425274246,
-0.12652726456846,-0.106361541521481,-0.105236270462937,-0.0835127492652271,
-0.0784406535722348,-0.0733870619889256,-0.0516031153801045,-0.029512914496819,
-0.0074997402847098,-5.64290021016797E-6),.UNSPECIFIED.);
#3938=B_SPLINE_CURVE_WITH_KNOTS('',3,(#288255,#288256,#288257,#288258),
 .UNSPECIFIED.,.F.,.F.,(4,4),(-0.468408500436428,-0.468287143792459),
 .UNSPECIFIED.);
#3939=B_SPLINE_CURVE_WITH_KNOTS('',3,(#288683,#288684,#288685,#288686,#288687,
#288688,#288689,#288690,#288691,#288692,#288693,#288694,#288695,#288696,
#288697,#288698,#288699,#288700,#288701,#288702,#288703,#288704,#288705,
#288706,#288707,#288708,#288709,#288710,#288711,#288712,#288713,#288714,
#288715,#288716,#288717,#288718,#288719,#288720,#288721,#288722,#288723,
#288724,#288725,#288726,#288727,#288728,#288729,#288730,#288731,#288732,
#288733,#288734,#288735,#288736,#288737,#288738,#288739,#288740,#288741,
#288742,#288743,#288744,#288745,#288746,#288747,#288748,#288749,#288750,
#288751,#288752,#288753,#288754,#288755,#288756,#288757,#288758,#288759,
#288760,#288761,#288762,#288763,#288764),.UNSPECIFIED.,.F.,.F.,(4,3,3,3,
3,3,3,3,3,3,3,3,3,3,3,3,3,3,3,3,3,3,3,3,3,3,3,4),(-0.364629307890661,-0.350885759085945,
-0.329296488089375,-0.313741431878983,-0.309365163672801,-0.288066104157163,
-0.266903491756204,-0.264006177467146,-0.26029818106468,-0.239602719874145,
-0.219188969841738,-0.199417322698614,-0.194876880502573,-0.191399047668888,
-0.171813366976952,-0.166173598315468,-0.146078147584166,-0.126706873608775,
-0.123379860192083,-0.103933041502093,-0.0846705822529982,-0.065567586070534,
-0.0621782887363481,-0.05894467115978,-0.0403543924363754,-0.0220984153978988,
-0.00442511139655304,0.),.UNSPECIFIED.);
#3940=B_SPLINE_CURVE_WITH_KNOTS('',3,(#289197,#289198,#289199,#289200,#289201,
#289202,#289203,#289204,#289205,#289206,#289207,#289208,#289209,#289210,
#289211,#289212,#289213,#289214,#289215,#289216,#289217,#289218,#289219,
#289220,#289221,#289222,#289223,#289224,#289225,#289226,#289227,#289228,
#289229,#289230,#289231,#289232,#289233,#289234,#289235,#289236,#289237,
#289238,#289239,#289240,#289241,#289242,#289243,#289244,#289245,#289246,
#289247,#289248,#289249,#289250,#289251,#289252,#289253,#289254,#289255,
#289256,#289257,#289258,#289259,#289260,#289261,#289262,#289263,#289264,
#289265,#289266,#289267,#289268,#289269,#289270,#289271,#289272,#289273,
#289274,#289275,#289276,#289277,#289278),.UNSPECIFIED.,.F.,.F.,(4,3,3,3,
3,3,3,3,3,3,3,3,3,3,3,3,3,3,3,3,3,3,3,3,3,3,3,4),(-0.366397579005845,-0.355461226466819,
-0.337381714695455,-0.327214164040339,-0.321649482146298,-0.302845846606557,
-0.288386907394637,-0.281257238921911,-0.277593927902022,-0.258058508053395,
-0.238234782514783,-0.218411056976172,-0.214856426708649,-0.194426531580489,
-0.187209422476688,-0.167411754208573,-0.156894426252658,-0.149523127563347,
-0.145921626399787,-0.125575048930976,-0.104563171293481,-0.0835512936559854,
-0.0752831225832569,-0.0721648689176682,-0.0505208253806571,-0.028827309114918,
-0.00759789022673524,-5.75490197052316E-15),.UNSPECIFIED.);
#3941=LINE('',#20217,#4578);
#3942=LINE('',#20566,#4579);
#3943=LINE('',#21035,#4580);
#3944=LINE('',#21501,#4581);
#3945=LINE('',#21964,#4582);
#3946=LINE('',#22427,#4583);
#3947=LINE('',#22893,#4584);
#3948=LINE('',#23356,#4585);
#3949=LINE('',#23822,#4586);
#3950=LINE('',#24291,#4587);
#3951=LINE('',#24533,#4588);
#3952=LINE('',#24635,#4589);
#3953=LINE('',#24776,#4590);
#3954=LINE('',#25167,#4591);
#3955=LINE('',#25554,#4592);
#3956=LINE('',#25939,#4593);
#3957=LINE('',#26330,#4594);
#3958=LINE('',#26717,#4595);
#3959=LINE('',#27098,#4596);
#3960=LINE('',#27491,#4597);
#3961=LINE('',#27897,#4598);
#3962=LINE('',#28208,#4599);
#3963=LINE('',#28557,#4600);
#3964=LINE('',#29026,#4601);
#3965=LINE('',#29492,#4602);
#3966=LINE('',#29955,#4603);
#3967=LINE('',#30418,#4604);
#3968=LINE('',#30884,#4605);
#3969=LINE('',#31347,#4606);
#3970=LINE('',#31813,#4607);
#3971=LINE('',#32282,#4608);
#3972=LINE('',#32524,#4609);
#3973=LINE('',#32626,#4610);
#3974=LINE('',#32771,#4611);
#3975=LINE('',#33164,#4612);
#3976=LINE('',#33543,#4613);
#3977=LINE('',#33926,#4614);
#3978=LINE('',#34313,#4615);
#3979=LINE('',#34708,#4616);
#3980=LINE('',#35089,#4617);
#3981=LINE('',#35484,#4618);
#3982=LINE('',#35890,#4619);
#3983=LINE('',#36203,#4620);
#3984=LINE('',#36552,#4621);
#3985=LINE('',#37021,#4622);
#3986=LINE('',#37487,#4623);
#3987=LINE('',#37950,#4624);
#3988=LINE('',#38413,#4625);
#3989=LINE('',#38879,#4626);
#3990=LINE('',#39342,#4627);
#3991=LINE('',#39808,#4628);
#3992=LINE('',#40277,#4629);
#3993=LINE('',#40519,#4630);
#3994=LINE('',#40621,#4631);
#3995=LINE('',#40766,#4632);
#3996=LINE('',#41159,#4633);
#3997=LINE('',#41550,#4634);
#3998=LINE('',#41935,#4635);
#3999=LINE('',#42328,#4636);
#4000=LINE('',#42719,#4637);
#4001=LINE('',#43104,#4638);
#4002=LINE('',#43499,#4639);
#4003=LINE('',#43903,#4640);
#4004=LINE('',#44214,#4641);
#4005=LINE('',#44563,#4642);
#4006=LINE('',#45032,#4643);
#4007=LINE('',#45498,#4644);
#4008=LINE('',#45961,#4645);
#4009=LINE('',#46424,#4646);
#4010=LINE('',#46890,#4647);
#4011=LINE('',#47353,#4648);
#4012=LINE('',#47819,#4649);
#4013=LINE('',#48288,#4650);
#4014=LINE('',#48530,#4651);
#4015=LINE('',#48632,#4652);
#4016=LINE('',#48777,#4653);
#4017=LINE('',#49166,#4654);
#4018=LINE('',#49553,#4655);
#4019=LINE('',#49934,#4656);
#4020=LINE('',#50327,#4657);
#4021=LINE('',#50722,#4658);
#4022=LINE('',#51105,#4659);
#4023=LINE('',#51502,#4660);
#4024=LINE('',#51908,#4661);
#4025=LINE('',#59449,#4662);
#4026=LINE('',#59455,#4663);
#4027=LINE('',#59461,#4664);
#4028=LINE('',#59467,#4665);
#4029=LINE('',#59472,#4666);
#4030=LINE('',#59474,#4667);
#4031=LINE('',#59476,#4668);
#4032=LINE('',#59477,#4669);
#4033=LINE('',#59480,#4670);
#4034=LINE('',#59482,#4671);
#4035=LINE('',#59483,#4672);
#4036=LINE('',#59486,#4673);
#4037=LINE('',#59488,#4674);
#4038=LINE('',#59489,#4675);
#4039=LINE('',#59491,#4676);
#4040=LINE('',#59492,#4677);
#4041=LINE('',#59499,#4678);
#4042=LINE('',#59541,#4679);
#4043=LINE('',#59868,#4680);
#4044=LINE('',#60262,#4681);
#4045=LINE('',#60653,#4682);
#4046=LINE('',#61044,#4683);
#4047=LINE('',#61432,#4684);
#4048=LINE('',#61823,#4685);
#4049=LINE('',#62214,#4686);
#4050=LINE('',#62602,#4687);
#4051=LINE('',#62996,#4688);
#4052=LINE('',#63387,#4689);
#4053=LINE('',#63778,#4690);
#4054=LINE('',#64172,#4691);
#4055=LINE('',#64563,#4692);
#4056=LINE('',#64951,#4693);
#4057=LINE('',#65160,#4694);
#4058=LINE('',#65336,#4695);
#4059=LINE('',#65587,#4696);
#4060=LINE('',#65817,#4697);
#4061=LINE('',#66230,#4698);
#4062=LINE('',#66676,#4699);
#4063=LINE('',#67132,#4700);
#4064=LINE('',#67564,#4701);
#4065=LINE('',#67996,#4702);
#4066=LINE('',#68396,#4703);
#4067=LINE('',#68850,#4704);
#4068=LINE('',#69286,#4705);
#4069=LINE('',#69714,#4706);
#4070=LINE('',#70126,#4707);
#4071=LINE('',#70554,#4708);
#4072=LINE('',#70970,#4709);
#4073=LINE('',#71313,#4710);
#4074=LINE('',#71355,#4711);
#4075=LINE('',#71682,#4712);
#4076=LINE('',#72076,#4713);
#4077=LINE('',#72467,#4714);
#4078=LINE('',#72858,#4715);
#4079=LINE('',#73246,#4716);
#4080=LINE('',#73637,#4717);
#4081=LINE('',#74028,#4718);
#4082=LINE('',#74416,#4719);
#4083=LINE('',#74810,#4720);
#4084=LINE('',#75201,#4721);
#4085=LINE('',#75592,#4722);
#4086=LINE('',#75986,#4723);
#4087=LINE('',#76377,#4724);
#4088=LINE('',#76765,#4725);
#4089=LINE('',#76974,#4726);
#4090=LINE('',#77152,#4727);
#4091=LINE('',#77449,#4728);
#4092=LINE('',#77683,#4729);
#4093=LINE('',#78094,#4730);
#4094=LINE('',#78510,#4731);
#4095=LINE('',#78968,#4732);
#4096=LINE('',#79396,#4733);
#4097=LINE('',#79806,#4734);
#4098=LINE('',#80234,#4735);
#4099=LINE('',#80686,#4736);
#4100=LINE('',#81130,#4737);
#4101=LINE('',#81558,#4738);
#4102=LINE('',#81970,#4739);
#4103=LINE('',#82394,#4740);
#4104=LINE('',#82820,#4741);
#4105=LINE('',#83177,#4742);
#4106=LINE('',#83333,#4743);
#4107=LINE('',#83663,#4744);
#4108=LINE('',#84054,#4745);
#4109=LINE('',#84442,#4746);
#4110=LINE('',#84833,#4747);
#4111=LINE('',#85224,#4748);
#4112=LINE('',#85612,#4749);
#4113=LINE('',#86003,#4750);
#4114=LINE('',#86394,#4751);
#4115=LINE('',#86785,#4752);
#4116=LINE('',#87179,#4753);
#4117=LINE('',#87454,#4754);
#4118=LINE('',#87781,#4755);
#4119=LINE('',#87990,#4756);
#4120=LINE('',#88146,#4757);
#4121=LINE('',#88476,#4758);
#4122=LINE('',#88867,#4759);
#4123=LINE('',#89255,#4760);
#4124=LINE('',#89646,#4761);
#4125=LINE('',#90037,#4762);
#4126=LINE('',#90425,#4763);
#4127=LINE('',#90816,#4764);
#4128=LINE('',#91207,#4765);
#4129=LINE('',#91598,#4766);
#4130=LINE('',#91992,#4767);
#4131=LINE('',#92267,#4768);
#4132=LINE('',#92594,#4769);
#4133=LINE('',#92803,#4770);
#4134=LINE('',#92959,#4771);
#4135=LINE('',#93289,#4772);
#4136=LINE('',#93680,#4773);
#4137=LINE('',#94068,#4774);
#4138=LINE('',#94459,#4775);
#4139=LINE('',#94850,#4776);
#4140=LINE('',#95238,#4777);
#4141=LINE('',#95629,#4778);
#4142=LINE('',#96020,#4779);
#4143=LINE('',#96411,#4780);
#4144=LINE('',#96805,#4781);
#4145=LINE('',#97196,#4782);
#4146=LINE('',#97584,#4783);
#4147=LINE('',#97793,#4784);
#4148=LINE('',#97949,#4785);
#4149=LINE('',#98279,#4786);
#4150=LINE('',#98670,#4787);
#4151=LINE('',#99058,#4788);
#4152=LINE('',#99449,#4789);
#4153=LINE('',#99840,#4790);
#4154=LINE('',#100228,#4791);
#4155=LINE('',#100619,#4792);
#4156=LINE('',#101010,#4793);
#4157=LINE('',#101401,#4794);
#4158=LINE('',#101795,#4795);
#4159=LINE('',#102186,#4796);
#4160=LINE('',#102574,#4797);
#4161=LINE('',#102783,#4798);
#4162=LINE('',#102974,#4799);
#4163=LINE('',#103403,#4800);
#4164=LINE('',#103836,#4801);
#4165=LINE('',#104273,#4802);
#4166=LINE('',#104758,#4803);
#4167=LINE('',#105201,#4804);
#4168=LINE('',#105621,#4805);
#4169=LINE('',#105871,#4806);
#4170=LINE('',#106275,#4807);
#4171=LINE('',#106710,#4808);
#4172=LINE('',#107119,#4809);
#4173=LINE('',#107520,#4810);
#4174=LINE('',#107937,#4811);
#4175=LINE('',#108254,#4812);
#4176=LINE('',#108443,#4813);
#4177=LINE('',#108860,#4814);
#4178=LINE('',#109293,#4815);
#4179=LINE('',#109730,#4816);
#4180=LINE('',#110223,#4817);
#4181=LINE('',#110666,#4818);
#4182=LINE('',#111088,#4819);
#4183=LINE('',#111338,#4820);
#4184=LINE('',#111736,#4821);
#4185=LINE('',#112169,#4822);
#4186=LINE('',#112582,#4823);
#4187=LINE('',#112999,#4824);
#4188=LINE('',#113420,#4825);
#4189=LINE('',#113731,#4826);
#4190=LINE('',#113930,#4827);
#4191=LINE('',#114356,#4828);
#4192=LINE('',#114781,#4829);
#4193=LINE('',#115193,#4830);
#4194=LINE('',#115682,#4831);
#4195=LINE('',#116111,#4832);
#4196=LINE('',#116525,#4833);
#4197=LINE('',#116775,#4834);
#4198=LINE('',#117189,#4835);
#4199=LINE('',#117622,#4836);
#4200=LINE('',#118021,#4837);
#4201=LINE('',#118414,#4838);
#4202=LINE('',#118834,#4839);
#4203=LINE('',#119159,#4840);
#4204=LINE('',#119362,#4841);
#4205=LINE('',#119788,#4842);
#4206=LINE('',#120211,#4843);
#4207=LINE('',#120627,#4844);
#4208=LINE('',#121124,#4845);
#4209=LINE('',#121573,#4846);
#4210=LINE('',#121979,#4847);
#4211=LINE('',#122231,#4848);
#4212=LINE('',#122647,#4849);
#4213=LINE('',#123080,#4850);
#4214=LINE('',#123499,#4851);
#4215=LINE('',#123906,#4852);
#4216=LINE('',#124326,#4853);
#4217=LINE('',#131966,#4854);
#4218=LINE('',#131968,#4855);
#4219=LINE('',#131970,#4856);
#4220=LINE('',#131971,#4857);
#4221=LINE('',#131976,#4858);
#4222=LINE('',#131977,#4859);
#4223=LINE('',#131980,#4860);
#4224=LINE('',#131982,#4861);
#4225=LINE('',#131983,#4862);
#4226=LINE('',#131986,#4863);
#4227=LINE('',#131991,#4864);
#4228=LINE('',#131997,#4865);
#4229=LINE('',#132003,#4866);
#4230=LINE('',#132009,#4867);
#4231=LINE('',#136459,#4868);
#4232=LINE('',#136464,#4869);
#4233=LINE('',#136466,#4870);
#4234=LINE('',#136468,#4871);
#4235=LINE('',#136469,#4872);
#4236=LINE('',#136472,#4873);
#4237=LINE('',#136474,#4874);
#4238=LINE('',#136476,#4875);
#4239=LINE('',#136477,#4876);
#4240=LINE('',#136481,#4877);
#4241=LINE('',#136482,#4878);
#4242=LINE('',#136483,#4879);
#4243=LINE('',#136486,#4880);
#4244=LINE('',#136487,#4881);
#4245=LINE('',#136490,#4882);
#4246=LINE('',#136491,#4883);
#4247=LINE('',#136493,#4884);
#4248=LINE('',#136497,#4885);
#4249=LINE('',#136499,#4886);
#4250=LINE('',#136500,#4887);
#4251=LINE('',#136503,#4888);
#4252=LINE('',#136504,#4889);
#4253=LINE('',#136507,#4890);
#4254=LINE('',#136508,#4891);
#4255=LINE('',#136510,#4892);
#4256=LINE('',#136516,#4893);
#4257=LINE('',#136518,#4894);
#4258=LINE('',#136520,#4895);
#4259=LINE('',#136521,#4896);
#4260=LINE('',#136525,#4897);
#4261=LINE('',#136527,#4898);
#4262=LINE('',#136529,#4899);
#4263=LINE('',#136530,#4900);
#4264=LINE('',#136543,#4901);
#4265=LINE('',#136687,#4902);
#4266=LINE('',#136902,#4903);
#4267=LINE('',#137410,#4904);
#4268=LINE('',#137921,#4905);
#4269=LINE('',#138414,#4906);
#4270=LINE('',#138922,#4907);
#4271=LINE('',#139433,#4908);
#4272=LINE('',#139941,#4909);
#4273=LINE('',#140452,#4910);
#4274=LINE('',#140960,#4911);
#4275=LINE('',#141474,#4912);
#4276=LINE('',#141967,#4913);
#4277=LINE('',#142475,#4914);
#4278=LINE('',#142983,#4915);
#4279=LINE('',#143479,#4916);
#4280=LINE('',#143993,#4917);
#4281=LINE('',#144501,#4918);
#4282=LINE('',#145015,#4919);
#4283=LINE('',#145526,#4920);
#4284=LINE('',#146034,#4921);
#4285=LINE('',#146548,#4922);
#4286=LINE('',#147038,#4923);
#4287=LINE('',#147549,#4924);
#4288=LINE('',#148060,#4925);
#4289=LINE('',#148550,#4926);
#4290=LINE('',#149049,#4927);
#4291=LINE('',#149566,#4928);
#4292=LINE('',#150059,#4929);
#4293=LINE('',#150573,#4930);
#4294=LINE('',#151084,#4931);
#4295=LINE('',#151583,#4932);
#4296=LINE('',#152088,#4933);
#4297=LINE('',#152596,#4934);
#4298=LINE('',#153110,#4935);
#4299=LINE('',#153624,#4936);
#4300=LINE('',#154138,#4937);
#4301=LINE('',#154640,#4938);
#4302=LINE('',#155133,#4939);
#4303=LINE('',#155644,#4940);
#4304=LINE('',#156155,#4941);
#4305=LINE('',#156648,#4942);
#4306=LINE('',#157153,#4943);
#4307=LINE('',#157667,#4944);
#4308=LINE('',#158181,#4945);
#4309=LINE('',#158692,#4946);
#4310=LINE('',#159203,#4947);
#4311=LINE('',#159711,#4948);
#4312=LINE('',#160204,#4949);
#4313=LINE('',#160712,#4950);
#4314=LINE('',#180360,#4951);
#4315=LINE('',#180365,#4952);
#4316=LINE('',#180367,#4953);
#4317=LINE('',#180369,#4954);
#4318=LINE('',#180370,#4955);
#4319=LINE('',#180374,#4956);
#4320=LINE('',#180375,#4957);
#4321=LINE('',#180376,#4958);
#4322=LINE('',#180380,#4959);
#4323=LINE('',#180381,#4960);
#4324=LINE('',#180382,#4961);
#4325=LINE('',#185142,#4962);
#4326=LINE('',#185153,#4963);
#4327=LINE('',#185160,#4964);
#4328=LINE('',#185163,#4965);
#4329=LINE('',#185169,#4966);
#4330=LINE('',#185175,#4967);
#4331=LINE('',#185180,#4968);
#4332=LINE('',#185182,#4969);
#4333=LINE('',#185184,#4970);
#4334=LINE('',#185185,#4971);
#4335=LINE('',#185188,#4972);
#4336=LINE('',#185190,#4973);
#4337=LINE('',#185192,#4974);
#4338=LINE('',#185193,#4975);
#4339=LINE('',#185196,#4976);
#4340=LINE('',#185198,#4977);
#4341=LINE('',#185199,#4978);
#4342=LINE('',#185202,#4979);
#4343=LINE('',#185203,#4980);
#4344=LINE('',#185206,#4981);
#4345=LINE('',#185207,#4982);
#4346=LINE('',#185209,#4983);
#4347=LINE('',#185214,#4984);
#4348=LINE('',#185215,#4985);
#4349=LINE('',#185216,#4986);
#4350=LINE('',#185219,#4987);
#4351=LINE('',#185220,#4988);
#4352=LINE('',#185223,#4989);
#4353=LINE('',#185224,#4990);
#4354=LINE('',#185226,#4991);
#4355=LINE('',#185232,#4992);
#4356=LINE('',#185234,#4993);
#4357=LINE('',#185236,#4994);
#4358=LINE('',#185237,#4995);
#4359=LINE('',#185240,#4996);
#4360=LINE('',#185242,#4997);
#4361=LINE('',#185243,#4998);
#4362=LINE('',#185246,#4999);
#4363=LINE('',#185247,#5000);
#4364=LINE('',#185261,#5001);
#4365=LINE('',#185265,#5002);
#4366=LINE('',#185269,#5003);
#4367=LINE('',#185273,#5004);
#4368=LINE('',#185277,#5005);
#4369=LINE('',#185280,#5006);
#4370=LINE('',#185281,#5007);
#4371=LINE('',#185283,#5008);
#4372=LINE('',#185290,#5009);
#4373=LINE('',#185296,#5010);
#4374=LINE('',#185304,#5011);
#4375=LINE('',#185526,#5012);
#4376=LINE('',#186025,#5013);
#4377=LINE('',#186521,#5014);
#4378=LINE('',#187032,#5015);
#4379=LINE('',#187540,#5016);
#4380=LINE('',#188033,#5017);
#4381=LINE('',#188535,#5018);
#4382=LINE('',#189028,#5019);
#4383=LINE('',#189530,#5020);
#4384=LINE('',#190041,#5021);
#4385=LINE('',#190552,#5022);
#4386=LINE('',#191051,#5023);
#4387=LINE('',#191553,#5024);
#4388=LINE('',#192058,#5025);
#4389=LINE('',#192566,#5026);
#4390=LINE('',#193068,#5027);
#4391=LINE('',#193558,#5028);
#4392=LINE('',#194045,#5029);
#4393=LINE('',#194547,#5030);
#4394=LINE('',#195055,#5031);
#4395=LINE('',#195569,#5032);
#4396=LINE('',#196062,#5033);
#4397=LINE('',#196558,#5034);
#4398=LINE('',#197063,#5035);
#4399=LINE('',#197574,#5036);
#4400=LINE('',#198073,#5037);
#4401=LINE('',#198560,#5038);
#4402=LINE('',#199065,#5039);
#4403=LINE('',#199576,#5040);
#4404=LINE('',#200087,#5041);
#4405=LINE('',#200586,#5042);
#4406=LINE('',#201085,#5043);
#4407=LINE('',#201578,#5044);
#4408=LINE('',#202053,#5045);
#4409=LINE('',#202537,#5046);
#4410=LINE('',#203033,#5047);
#4411=LINE('',#203532,#5048);
#4412=LINE('',#204037,#5049);
#4413=LINE('',#204536,#5050);
#4414=LINE('',#205029,#5051);
#4415=LINE('',#205519,#5052);
#4416=LINE('',#206018,#5053);
#4417=LINE('',#206520,#5054);
#4418=LINE('',#207022,#5055);
#4419=LINE('',#207518,#5056);
#4420=LINE('',#208008,#5057);
#4421=LINE('',#208510,#5058);
#4422=LINE('',#209003,#5059);
#4423=LINE('',#209493,#5060);
#4424=LINE('',#209983,#5061);
#4425=LINE('',#210470,#5062);
#4426=LINE('',#210813,#5063);
#4427=LINE('',#211230,#5064);
#4428=LINE('',#211735,#5065);
#4429=LINE('',#212234,#5066);
#4430=LINE('',#212733,#5067);
#4431=LINE('',#213241,#5068);
#4432=LINE('',#213737,#5069);
#4433=LINE('',#214230,#5070);
#4434=LINE('',#214708,#5071);
#4435=LINE('',#215192,#5072);
#4436=LINE('',#215694,#5073);
#4437=LINE('',#216202,#5074);
#4438=LINE('',#216698,#5075);
#4439=LINE('',#241824,#5076);
#4440=LINE('',#247031,#5077);
#4441=LINE('',#247033,#5078);
#4442=LINE('',#247035,#5079);
#4443=LINE('',#247083,#5080);
#4444=LINE('',#247161,#5081);
#4445=LINE('',#247206,#5082);
#4446=LINE('',#247212,#5083);
#4447=LINE('',#247218,#5084);
#4448=LINE('',#247224,#5085);
#4449=LINE('',#247230,#5086);
#4450=LINE('',#247236,#5087);
#4451=LINE('',#247241,#5088);
#4452=LINE('',#247243,#5089);
#4453=LINE('',#247251,#5090);
#4454=LINE('',#247252,#5091);
#4455=LINE('',#247257,#5092);
#4456=LINE('',#247266,#5093);
#4457=LINE('',#247277,#5094);
#4458=LINE('',#247285,#5095);
#4459=LINE('',#247289,#5096);
#4460=LINE('',#247296,#5097);
#4461=LINE('',#247302,#5098);
#4462=LINE('',#247310,#5099);
#4463=LINE('',#247312,#5100);
#4464=LINE('',#247314,#5101);
#4465=LINE('',#247315,#5102);
#4466=LINE('',#247319,#5103);
#4467=LINE('',#247321,#5104);
#4468=LINE('',#247323,#5105);
#4469=LINE('',#247324,#5106);
#4470=LINE('',#247338,#5107);
#4471=LINE('',#247344,#5108);
#4472=LINE('',#247352,#5109);
#4473=LINE('',#247633,#5110);
#4474=LINE('',#247689,#5111);
#4475=LINE('',#248010,#5112);
#4476=LINE('',#248430,#5113);
#4477=LINE('',#248863,#5114);
#4478=LINE('',#249360,#5115);
#4479=LINE('',#249795,#5116);
#4480=LINE('',#250224,#5117);
#4481=LINE('',#250654,#5118);
#4482=LINE('',#251094,#5119);
#4483=LINE('',#251558,#5120);
#4484=LINE('',#251998,#5121);
#4485=LINE('',#252425,#5122);
#4486=LINE('',#252858,#5123);
#4487=LINE('',#253365,#5124);
#4488=LINE('',#253788,#5125);
#4489=LINE('',#254217,#5126);
#4490=LINE('',#260630,#5127);
#4491=LINE('',#260632,#5128);
#4492=LINE('',#260634,#5129);
#4493=LINE('',#260635,#5130);
#4494=LINE('',#260638,#5131);
#4495=LINE('',#260640,#5132);
#4496=LINE('',#260641,#5133);
#4497=LINE('',#260644,#5134);
#4498=LINE('',#260646,#5135);
#4499=LINE('',#260647,#5136);
#4500=LINE('',#260650,#5137);
#4501=LINE('',#260652,#5138);
#4502=LINE('',#260653,#5139);
#4503=LINE('',#260656,#5140);
#4504=LINE('',#260658,#5141);
#4505=LINE('',#260659,#5142);
#4506=LINE('',#260661,#5143);
#4507=LINE('',#260662,#5144);
#4508=LINE('',#260669,#5145);
#4509=LINE('',#260677,#5146);
#4510=LINE('',#260922,#5147);
#4511=LINE('',#260963,#5148);
#4512=LINE('',#261083,#5149);
#4513=LINE('',#261485,#5150);
#4514=LINE('',#261919,#5151);
#4515=LINE('',#262377,#5152);
#4516=LINE('',#262803,#5153);
#4517=LINE('',#263315,#5154);
#4518=LINE('',#263737,#5155);
#4519=LINE('',#264073,#5156);
#4520=LINE('',#264425,#5157);
#4521=LINE('',#264744,#5158);
#4522=LINE('',#265107,#5159);
#4523=LINE('',#265535,#5160);
#4524=LINE('',#265877,#5161);
#4525=LINE('',#266240,#5162);
#4526=LINE('',#266675,#5163);
#4527=LINE('',#267132,#5164);
#4528=LINE('',#267561,#5165);
#4529=LINE('',#267888,#5166);
#4530=LINE('',#268252,#5167);
#4531=LINE('',#268695,#5168);
#4532=LINE('',#269146,#5169);
#4533=LINE('',#269595,#5170);
#4534=LINE('',#270058,#5171);
#4535=LINE('',#270495,#5172);
#4536=LINE('',#270944,#5173);
#4537=LINE('',#271395,#5174);
#4538=LINE('',#271814,#5175);
#4539=LINE('',#279086,#5176);
#4540=LINE('',#279088,#5177);
#4541=LINE('',#279090,#5178);
#4542=LINE('',#279091,#5179);
#4543=LINE('',#279094,#5180);
#4544=LINE('',#279096,#5181);
#4545=LINE('',#279097,#5182);
#4546=LINE('',#279100,#5183);
#4547=LINE('',#279102,#5184);
#4548=LINE('',#279103,#5185);
#4549=LINE('',#279106,#5186);
#4550=LINE('',#279108,#5187);
#4551=LINE('',#279109,#5188);
#4552=LINE('',#279112,#5189);
#4553=LINE('',#279114,#5190);
#4554=LINE('',#279115,#5191);
#4555=LINE('',#279117,#5192);
#4556=LINE('',#279118,#5193);
#4557=LINE('',#279125,#5194);
#4558=LINE('',#288253,#5195);
#4559=LINE('',#289282,#5196);
#4560=LINE('',#289284,#5197);
#4561=LINE('',#289286,#5198);
#4562=LINE('',#289287,#5199);
#4563=LINE('',#289290,#5200);
#4564=LINE('',#289292,#5201);
#4565=LINE('',#289293,#5202);
#4566=LINE('',#289296,#5203);
#4567=LINE('',#289298,#5204);
#4568=LINE('',#289299,#5205);
#4569=LINE('',#289302,#5206);
#4570=LINE('',#289304,#5207);
#4571=LINE('',#289305,#5208);
#4572=LINE('',#289308,#5209);
#4573=LINE('',#289310,#5210);
#4574=LINE('',#289311,#5211);
#4575=LINE('',#289313,#5212);
#4576=LINE('',#289314,#5213);
#4577=LINE('',#289321,#5214);
#4578=VECTOR('',#17895,4.085);
#4579=VECTOR('',#17900,4.085);
#4580=VECTOR('',#17903,4.085);
#4581=VECTOR('',#17906,4.085);
#4582=VECTOR('',#17909,4.085);
#4583=VECTOR('',#17912,4.085);
#4584=VECTOR('',#17915,4.085);
#4585=VECTOR('',#17918,4.085);
#4586=VECTOR('',#17921,4.085);
#4587=VECTOR('',#17924,4.085);
#4588=VECTOR('',#17929,3.38975);
#4589=VECTOR('',#17932,3.38975);
#4590=VECTOR('',#17939,3.38975);
#4591=VECTOR('',#17942,3.38975);
#4592=VECTOR('',#17945,3.38975);
#4593=VECTOR('',#17948,3.38975);
#4594=VECTOR('',#17951,3.38975);
#4595=VECTOR('',#17954,3.38975);
#4596=VECTOR('',#17957,3.38975);
#4597=VECTOR('',#17960,3.38975);
#4598=VECTOR('',#17963,3.38975);
#4599=VECTOR('',#17968,4.085);
#4600=VECTOR('',#17973,4.085);
#4601=VECTOR('',#17976,4.085);
#4602=VECTOR('',#17979,4.085);
#4603=VECTOR('',#17982,4.085);
#4604=VECTOR('',#17985,4.085);
#4605=VECTOR('',#17988,4.085);
#4606=VECTOR('',#17991,4.085);
#4607=VECTOR('',#17994,4.085);
#4608=VECTOR('',#17997,4.085);
#4609=VECTOR('',#18002,3.38975);
#4610=VECTOR('',#18005,3.38975);
#4611=VECTOR('',#18012,3.38975);
#4612=VECTOR('',#18015,3.38975);
#4613=VECTOR('',#18018,3.38975);
#4614=VECTOR('',#18021,3.38975);
#4615=VECTOR('',#18024,3.38975);
#4616=VECTOR('',#18027,3.38975);
#4617=VECTOR('',#18030,3.38975);
#4618=VECTOR('',#18033,3.38975);
#4619=VECTOR('',#18036,3.38975);
#4620=VECTOR('',#18041,4.085);
#4621=VECTOR('',#18046,4.085);
#4622=VECTOR('',#18049,4.085);
#4623=VECTOR('',#18052,4.085);
#4624=VECTOR('',#18055,4.085);
#4625=VECTOR('',#18058,4.085);
#4626=VECTOR('',#18061,4.085);
#4627=VECTOR('',#18064,4.085);
#4628=VECTOR('',#18067,4.085);
#4629=VECTOR('',#18070,4.085);
#4630=VECTOR('',#18075,3.38975);
#4631=VECTOR('',#18078,3.38975);
#4632=VECTOR('',#18085,3.38975);
#4633=VECTOR('',#18088,3.38975);
#4634=VECTOR('',#18091,3.38975);
#4635=VECTOR('',#18094,3.38975);
#4636=VECTOR('',#18097,3.38975);
#4637=VECTOR('',#18100,3.38975);
#4638=VECTOR('',#18103,3.38975);
#4639=VECTOR('',#18106,3.38975);
#4640=VECTOR('',#18109,3.38975);
#4641=VECTOR('',#18114,4.085);
#4642=VECTOR('',#18119,4.085);
#4643=VECTOR('',#18122,4.085);
#4644=VECTOR('',#18125,4.085);
#4645=VECTOR('',#18128,4.085);
#4646=VECTOR('',#18131,4.085);
#4647=VECTOR('',#18134,4.085);
#4648=VECTOR('',#18137,4.085);
#4649=VECTOR('',#18140,4.085);
#4650=VECTOR('',#18143,4.085);
#4651=VECTOR('',#18148,3.38975);
#4652=VECTOR('',#18151,3.38975);
#4653=VECTOR('',#18158,3.38975);
#4654=VECTOR('',#18161,3.38975);
#4655=VECTOR('',#18164,3.38975);
#4656=VECTOR('',#18167,3.38975);
#4657=VECTOR('',#18170,3.38975);
#4658=VECTOR('',#18173,3.38975);
#4659=VECTOR('',#18176,3.38975);
#4660=VECTOR('',#18179,3.38975);
#4661=VECTOR('',#18182,3.38975);
#4662=VECTOR('',#18221,4.5);
#4663=VECTOR('',#18228,4.5);
#4664=VECTOR('',#18235,4.5);
#4665=VECTOR('',#18242,4.5);
#4666=VECTOR('',#18247,10.);
#4667=VECTOR('',#18248,10.);
#4668=VECTOR('',#18249,10.);
#4669=VECTOR('',#18250,10.);
#4670=VECTOR('',#18253,10.);
#4671=VECTOR('',#18254,10.);
#4672=VECTOR('',#18255,10.);
#4673=VECTOR('',#18258,10.);
#4674=VECTOR('',#18259,10.);
#4675=VECTOR('',#18260,10.);
#4676=VECTOR('',#18263,10.);
#4677=VECTOR('',#18264,10.);
#4678=VECTOR('',#18273,2.05475);
#4679=VECTOR('',#18278,2.05475);
#4680=VECTOR('',#18281,2.05475);
#4681=VECTOR('',#18284,2.05475);
#4682=VECTOR('',#18287,2.05475);
#4683=VECTOR('',#18290,2.05475);
#4684=VECTOR('',#18293,2.05475);
#4685=VECTOR('',#18296,2.05475);
#4686=VECTOR('',#18299,2.05475);
#4687=VECTOR('',#18302,2.05475);
#4688=VECTOR('',#18305,2.05475);
#4689=VECTOR('',#18308,2.05475);
#4690=VECTOR('',#18311,2.05475);
#4691=VECTOR('',#18314,2.05475);
#4692=VECTOR('',#18317,2.05475);
#4693=VECTOR('',#18320,2.05475);
#4694=VECTOR('',#18325,1.666);
#4695=VECTOR('',#18328,1.666);
#4696=VECTOR('',#18333,1.666);
#4697=VECTOR('',#18336,1.666);
#4698=VECTOR('',#18339,1.666);
#4699=VECTOR('',#18342,1.666);
#4700=VECTOR('',#18345,1.666);
#4701=VECTOR('',#18348,1.666);
#4702=VECTOR('',#18351,1.666);
#4703=VECTOR('',#18354,1.666);
#4704=VECTOR('',#18357,1.666);
#4705=VECTOR('',#18360,1.666);
#4706=VECTOR('',#18363,1.666);
#4707=VECTOR('',#18366,1.666);
#4708=VECTOR('',#18369,1.666);
#4709=VECTOR('',#18372,1.666);
#4710=VECTOR('',#18377,2.05475);
#4711=VECTOR('',#18382,2.05475);
#4712=VECTOR('',#18385,2.05475);
#4713=VECTOR('',#18388,2.05475);
#4714=VECTOR('',#18391,2.05475);
#4715=VECTOR('',#18394,2.05475);
#4716=VECTOR('',#18397,2.05475);
#4717=VECTOR('',#18400,2.05475);
#4718=VECTOR('',#18403,2.05475);
#4719=VECTOR('',#18406,2.05475);
#4720=VECTOR('',#18409,2.05475);
#4721=VECTOR('',#18412,2.05475);
#4722=VECTOR('',#18415,2.05475);
#4723=VECTOR('',#18418,2.05475);
#4724=VECTOR('',#18421,2.05475);
#4725=VECTOR('',#18424,2.05475);
#4726=VECTOR('',#18429,1.666);
#4727=VECTOR('',#18432,1.666);
#4728=VECTOR('',#18437,1.666);
#4729=VECTOR('',#18440,1.666);
#4730=VECTOR('',#18443,1.666);
#4731=VECTOR('',#18446,1.666);
#4732=VECTOR('',#18449,1.666);
#4733=VECTOR('',#18452,1.666);
#4734=VECTOR('',#18455,1.666);
#4735=VECTOR('',#18458,1.666);
#4736=VECTOR('',#18461,1.666);
#4737=VECTOR('',#18464,1.666);
#4738=VECTOR('',#18467,1.666);
#4739=VECTOR('',#18470,1.666);
#4740=VECTOR('',#18473,1.666);
#4741=VECTOR('',#18476,1.666);
#4742=VECTOR('',#18481,2.05475);
#4743=VECTOR('',#18486,2.05475);
#4744=VECTOR('',#18489,2.05475);
#4745=VECTOR('',#18492,2.05475);
#4746=VECTOR('',#18495,2.05475);
#4747=VECTOR('',#18498,2.05475);
#4748=VECTOR('',#18501,2.05475);
#4749=VECTOR('',#18504,2.05475);
#4750=VECTOR('',#18507,2.05475);
#4751=VECTOR('',#18510,2.05475);
#4752=VECTOR('',#18513,2.05475);
#4753=VECTOR('',#18516,2.05475);
#4754=VECTOR('',#18519,2.05475);
#4755=VECTOR('',#18522,2.05475);
#4756=VECTOR('',#18527,2.05475);
#4757=VECTOR('',#18532,2.05475);
#4758=VECTOR('',#18535,2.05475);
#4759=VECTOR('',#18538,2.05475);
#4760=VECTOR('',#18541,2.05475);
#4761=VECTOR('',#18544,2.05475);
#4762=VECTOR('',#18547,2.05475);
#4763=VECTOR('',#18550,2.05475);
#4764=VECTOR('',#18553,2.05475);
#4765=VECTOR('',#18556,2.05475);
#4766=VECTOR('',#18559,2.05475);
#4767=VECTOR('',#18562,2.05475);
#4768=VECTOR('',#18565,2.05475);
#4769=VECTOR('',#18568,2.05475);
#4770=VECTOR('',#18573,2.05475);
#4771=VECTOR('',#18578,2.05475);
#4772=VECTOR('',#18581,2.05475);
#4773=VECTOR('',#18584,2.05475);
#4774=VECTOR('',#18587,2.05475);
#4775=VECTOR('',#18590,2.05475);
#4776=VECTOR('',#18593,2.05475);
#4777=VECTOR('',#18596,2.05475);
#4778=VECTOR('',#18599,2.05475);
#4779=VECTOR('',#18602,2.05475);
#4780=VECTOR('',#18605,2.05475);
#4781=VECTOR('',#18608,2.05475);
#4782=VECTOR('',#18611,2.05475);
#4783=VECTOR('',#18614,2.05475);
#4784=VECTOR('',#18619,2.05475);
#4785=VECTOR('',#18624,2.05475);
#4786=VECTOR('',#18627,2.05475);
#4787=VECTOR('',#18630,2.05475);
#4788=VECTOR('',#18633,2.05475);
#4789=VECTOR('',#18636,2.05475);
#4790=VECTOR('',#18639,2.05475);
#4791=VECTOR('',#18642,2.05475);
#4792=VECTOR('',#18645,2.05475);
#4793=VECTOR('',#18648,2.05475);
#4794=VECTOR('',#18651,2.05475);
#4795=VECTOR('',#18654,2.05475);
#4796=VECTOR('',#18657,2.05475);
#4797=VECTOR('',#18660,2.05475);
#4798=VECTOR('',#18665,1.666);
#4799=VECTOR('',#18670,1.666);
#4800=VECTOR('',#18673,1.666);
#4801=VECTOR('',#18676,1.666);
#4802=VECTOR('',#18679,1.666);
#4803=VECTOR('',#18682,1.666);
#4804=VECTOR('',#18685,1.666);
#4805=VECTOR('',#18688,1.666);
#4806=VECTOR('',#18691,1.666);
#4807=VECTOR('',#18694,1.666);
#4808=VECTOR('',#18697,1.666);
#4809=VECTOR('',#18700,1.666);
#4810=VECTOR('',#18703,1.666);
#4811=VECTOR('',#18706,1.666);
#4812=VECTOR('',#18711,1.666);
#4813=VECTOR('',#18716,1.666);
#4814=VECTOR('',#18719,1.666);
#4815=VECTOR('',#18722,1.666);
#4816=VECTOR('',#18725,1.666);
#4817=VECTOR('',#18728,1.666);
#4818=VECTOR('',#18731,1.666);
#4819=VECTOR('',#18734,1.666);
#4820=VECTOR('',#18737,1.666);
#4821=VECTOR('',#18740,1.666);
#4822=VECTOR('',#18743,1.666);
#4823=VECTOR('',#18746,1.666);
#4824=VECTOR('',#18749,1.666);
#4825=VECTOR('',#18752,1.666);
#4826=VECTOR('',#18757,1.666);
#4827=VECTOR('',#18762,1.666);
#4828=VECTOR('',#18765,1.666);
#4829=VECTOR('',#18768,1.666);
#4830=VECTOR('',#18771,1.666);
#4831=VECTOR('',#18774,1.666);
#4832=VECTOR('',#18777,1.666);
#4833=VECTOR('',#18780,1.666);
#4834=VECTOR('',#18783,1.666);
#4835=VECTOR('',#18786,1.666);
#4836=VECTOR('',#18789,1.666);
#4837=VECTOR('',#18792,1.666);
#4838=VECTOR('',#18795,1.666);
#4839=VECTOR('',#18798,1.666);
#4840=VECTOR('',#18803,1.666);
#4841=VECTOR('',#18808,1.666);
#4842=VECTOR('',#18811,1.666);
#4843=VECTOR('',#18814,1.666);
#4844=VECTOR('',#18817,1.666);
#4845=VECTOR('',#18820,1.666);
#4846=VECTOR('',#18823,1.666);
#4847=VECTOR('',#18826,1.666);
#4848=VECTOR('',#18829,1.666);
#4849=VECTOR('',#18832,1.666);
#4850=VECTOR('',#18835,1.666);
#4851=VECTOR('',#18838,1.666);
#4852=VECTOR('',#18841,1.666);
#4853=VECTOR('',#18844,1.666);
#4854=VECTOR('',#18881,10.);
#4855=VECTOR('',#18882,10.);
#4856=VECTOR('',#18883,10.);
#4857=VECTOR('',#18884,10.);
#4858=VECTOR('',#18889,10.);
#4859=VECTOR('',#18890,10.);
#4860=VECTOR('',#18893,10.);
#4861=VECTOR('',#18894,10.);
#4862=VECTOR('',#18895,10.);
#4863=VECTOR('',#18900,10.);
#4864=VECTOR('',#18905,4.5);
#4865=VECTOR('',#18912,4.5);
#4866=VECTOR('',#18919,4.5);
#4867=VECTOR('',#18926,4.5);
#4868=VECTOR('',#18941,22.);
#4869=VECTOR('',#18946,10.);
#4870=VECTOR('',#18947,10.);
#4871=VECTOR('',#18948,10.);
#4872=VECTOR('',#18949,10.);
#4873=VECTOR('',#18950,10.);
#4874=VECTOR('',#18951,10.);
#4875=VECTOR('',#18952,10.);
#4876=VECTOR('',#18953,10.);
#4877=VECTOR('',#18956,10.);
#4878=VECTOR('',#18957,10.);
#4879=VECTOR('',#18958,10.);
#4880=VECTOR('',#18961,10.);
#4881=VECTOR('',#18962,10.);
#4882=VECTOR('',#18965,10.);
#4883=VECTOR('',#18966,10.);
#4884=VECTOR('',#18969,10.);
#4885=VECTOR('',#18974,10.);
#4886=VECTOR('',#18975,10.);
#4887=VECTOR('',#18976,10.);
#4888=VECTOR('',#18979,10.);
#4889=VECTOR('',#18980,10.);
#4890=VECTOR('',#18983,10.);
#4891=VECTOR('',#18984,10.);
#4892=VECTOR('',#18987,10.);
#4893=VECTOR('',#18994,10.);
#4894=VECTOR('',#18995,10.);
#4895=VECTOR('',#18996,10.);
#4896=VECTOR('',#18997,10.);
#4897=VECTOR('',#19000,10.);
#4898=VECTOR('',#19001,10.);
#4899=VECTOR('',#19002,10.);
#4900=VECTOR('',#19003,10.);
#4901=VECTOR('',#19024,7.01125);
#4902=VECTOR('',#19027,7.01125);
#4903=VECTOR('',#19034,7.01125);
#4904=VECTOR('',#19037,7.01125);
#4905=VECTOR('',#19040,7.01125);
#4906=VECTOR('',#19043,7.01125);
#4907=VECTOR('',#19046,7.01125);
#4908=VECTOR('',#19049,7.01125);
#4909=VECTOR('',#19052,7.01125);
#4910=VECTOR('',#19055,7.01125);
#4911=VECTOR('',#19058,7.01125);
#4912=VECTOR('',#19061,7.01125);
#4913=VECTOR('',#19064,7.01125);
#4914=VECTOR('',#19067,7.01125);
#4915=VECTOR('',#19070,7.01125);
#4916=VECTOR('',#19073,7.01125);
#4917=VECTOR('',#19076,7.01125);
#4918=VECTOR('',#19079,7.01125);
#4919=VECTOR('',#19082,7.01125);
#4920=VECTOR('',#19085,7.01125);
#4921=VECTOR('',#19088,7.01125);
#4922=VECTOR('',#19091,7.01125);
#4923=VECTOR('',#19094,7.01125);
#4924=VECTOR('',#19097,7.01125);
#4925=VECTOR('',#19100,7.01125);
#4926=VECTOR('',#19103,7.01125);
#4927=VECTOR('',#19106,7.01125);
#4928=VECTOR('',#19109,7.01125);
#4929=VECTOR('',#19112,7.01125);
#4930=VECTOR('',#19115,7.01125);
#4931=VECTOR('',#19118,7.01125);
#4932=VECTOR('',#19121,7.01125);
#4933=VECTOR('',#19124,7.01125);
#4934=VECTOR('',#19127,7.01125);
#4935=VECTOR('',#19130,7.01125);
#4936=VECTOR('',#19133,7.01125);
#4937=VECTOR('',#19136,7.01125);
#4938=VECTOR('',#19139,7.01125);
#4939=VECTOR('',#19142,7.01125);
#4940=VECTOR('',#19145,7.01125);
#4941=VECTOR('',#19148,7.01125);
#4942=VECTOR('',#19151,7.01125);
#4943=VECTOR('',#19154,7.01125);
#4944=VECTOR('',#19157,7.01125);
#4945=VECTOR('',#19160,7.01125);
#4946=VECTOR('',#19163,7.01125);
#4947=VECTOR('',#19166,7.01125);
#4948=VECTOR('',#19169,7.01125);
#4949=VECTOR('',#19172,7.01125);
#4950=VECTOR('',#19175,7.01125);
#4951=VECTOR('',#19194,8.5);
#4952=VECTOR('',#19199,10.);
#4953=VECTOR('',#19200,10.);
#4954=VECTOR('',#19201,10.);
#4955=VECTOR('',#19202,10.);
#4956=VECTOR('',#19205,10.);
#4957=VECTOR('',#19206,10.);
#4958=VECTOR('',#19207,10.);
#4959=VECTOR('',#19210,10.);
#4960=VECTOR('',#19211,10.);
#4961=VECTOR('',#19212,10.);
#4962=VECTOR('',#19225,4.);
#4963=VECTOR('',#19242,8.5);
#4964=VECTOR('',#19251,13.);
#4965=VECTOR('',#19254,13.);
#4966=VECTOR('',#19261,2.5);
#4967=VECTOR('',#19268,2.5);
#4968=VECTOR('',#19273,10.);
#4969=VECTOR('',#19274,10.);
#4970=VECTOR('',#19275,10.);
#4971=VECTOR('',#19276,10.);
#4972=VECTOR('',#19277,10.);
#4973=VECTOR('',#19278,10.);
#4974=VECTOR('',#19279,10.);
#4975=VECTOR('',#19280,10.);
#4976=VECTOR('',#19283,10.);
#4977=VECTOR('',#19284,10.);
#4978=VECTOR('',#19285,10.);
#4979=VECTOR('',#19288,10.);
#4980=VECTOR('',#19289,10.);
#4981=VECTOR('',#19292,10.);
#4982=VECTOR('',#19293,10.);
#4983=VECTOR('',#19296,10.);
#4984=VECTOR('',#19301,10.);
#4985=VECTOR('',#19302,10.);
#4986=VECTOR('',#19303,10.);
#4987=VECTOR('',#19306,10.);
#4988=VECTOR('',#19307,10.);
#4989=VECTOR('',#19310,10.);
#4990=VECTOR('',#19311,10.);
#4991=VECTOR('',#19314,10.);
#4992=VECTOR('',#19321,10.);
#4993=VECTOR('',#19322,10.);
#4994=VECTOR('',#19323,10.);
#4995=VECTOR('',#19324,10.);
#4996=VECTOR('',#19327,10.);
#4997=VECTOR('',#19328,10.);
#4998=VECTOR('',#19329,10.);
#4999=VECTOR('',#19332,10.);
#5000=VECTOR('',#19333,10.);
#5001=VECTOR('',#19348,2.5);
#5002=VECTOR('',#19353,2.5);
#5003=VECTOR('',#19358,2.5);
#5004=VECTOR('',#19363,2.5);
#5005=VECTOR('',#19368,7.);
#5006=VECTOR('',#19371,10.);
#5007=VECTOR('',#19372,10.);
#5008=VECTOR('',#19375,10.);
#5009=VECTOR('',#19384,6.);
#5010=VECTOR('',#19391,7.);
#5011=VECTOR('',#19402,6.767);
#5012=VECTOR('',#19407,6.767);
#5013=VECTOR('',#19410,6.767);
#5014=VECTOR('',#19413,6.767);
#5015=VECTOR('',#19416,6.767);
#5016=VECTOR('',#19419,6.767);
#5017=VECTOR('',#19422,6.767);
#5018=VECTOR('',#19425,6.767);
#5019=VECTOR('',#19428,6.767);
#5020=VECTOR('',#19431,6.767);
#5021=VECTOR('',#19434,6.767);
#5022=VECTOR('',#19437,6.767);
#5023=VECTOR('',#19440,6.767);
#5024=VECTOR('',#19443,6.767);
#5025=VECTOR('',#19446,6.767);
#5026=VECTOR('',#19449,6.767);
#5027=VECTOR('',#19452,6.767);
#5028=VECTOR('',#19455,6.767);
#5029=VECTOR('',#19458,6.767);
#5030=VECTOR('',#19461,6.767);
#5031=VECTOR('',#19464,6.767);
#5032=VECTOR('',#19467,6.767);
#5033=VECTOR('',#19470,6.767);
#5034=VECTOR('',#19473,6.767);
#5035=VECTOR('',#19476,6.767);
#5036=VECTOR('',#19479,6.767);
#5037=VECTOR('',#19482,6.767);
#5038=VECTOR('',#19485,6.767);
#5039=VECTOR('',#19488,6.767);
#5040=VECTOR('',#19491,6.767);
#5041=VECTOR('',#19494,6.767);
#5042=VECTOR('',#19497,6.767);
#5043=VECTOR('',#19500,6.767);
#5044=VECTOR('',#19503,6.767);
#5045=VECTOR('',#19506,6.767);
#5046=VECTOR('',#19509,6.767);
#5047=VECTOR('',#19512,6.767);
#5048=VECTOR('',#19515,6.767);
#5049=VECTOR('',#19518,6.767);
#5050=VECTOR('',#19521,6.767);
#5051=VECTOR('',#19524,6.767);
#5052=VECTOR('',#19527,6.767);
#5053=VECTOR('',#19530,6.767);
#5054=VECTOR('',#19533,6.767);
#5055=VECTOR('',#19536,6.767);
#5056=VECTOR('',#19539,6.767);
#5057=VECTOR('',#19542,6.767);
#5058=VECTOR('',#19545,6.767);
#5059=VECTOR('',#19548,6.767);
#5060=VECTOR('',#19551,6.767);
#5061=VECTOR('',#19554,6.767);
#5062=VECTOR('',#19557,6.767);
#5063=VECTOR('',#19560,6.767);
#5064=VECTOR('',#19563,6.767);
#5065=VECTOR('',#19566,6.767);
#5066=VECTOR('',#19569,6.767);
#5067=VECTOR('',#19572,6.767);
#5068=VECTOR('',#19575,6.767);
#5069=VECTOR('',#19578,6.767);
#5070=VECTOR('',#19581,6.767);
#5071=VECTOR('',#19584,6.767);
#5072=VECTOR('',#19587,6.767);
#5073=VECTOR('',#19590,6.767);
#5074=VECTOR('',#19593,6.767);
#5075=VECTOR('',#19596,6.767);
#5076=VECTOR('',#19609,2.);
#5077=VECTOR('',#19622,10.);
#5078=VECTOR('',#19625,6.);
#5079=VECTOR('',#19626,6.);
#5080=VECTOR('',#19637,2.);
#5081=VECTOR('',#19640,2.);
#5082=VECTOR('',#19645,8.);
#5083=VECTOR('',#19652,8.);
#5084=VECTOR('',#19659,8.);
#5085=VECTOR('',#19666,8.);
#5086=VECTOR('',#19673,8.);
#5087=VECTOR('',#19680,8.);
#5088=VECTOR('',#19687,14.);
#5089=VECTOR('',#19688,14.);
#5090=VECTOR('',#19699,6.);
#5091=VECTOR('',#19700,6.);
#5092=VECTOR('',#19705,45.);
#5093=VECTOR('',#19718,1.5);
#5094=VECTOR('',#19733,2.);
#5095=VECTOR('',#19742,3.5);
#5096=VECTOR('',#19749,2.);
#5097=VECTOR('',#19758,2.);
#5098=VECTOR('',#19765,3.5);
#5099=VECTOR('',#19776,10.);
#5100=VECTOR('',#19777,10.);
#5101=VECTOR('',#19778,10.);
#5102=VECTOR('',#19779,10.);
#5103=VECTOR('',#19782,10.);
#5104=VECTOR('',#19783,10.);
#5105=VECTOR('',#19784,10.);
#5106=VECTOR('',#19785,10.);
#5107=VECTOR('',#19808,6.);
#5108=VECTOR('',#19815,12.);
#5109=VECTOR('',#19826,3.5);
#5110=VECTOR('',#19831,3.5);
#5111=VECTOR('',#19838,3.22275);
#5112=VECTOR('',#19843,3.22275);
#5113=VECTOR('',#19846,3.22275);
#5114=VECTOR('',#19849,3.22275);
#5115=VECTOR('',#19852,3.22275);
#5116=VECTOR('',#19855,3.22275);
#5117=VECTOR('',#19858,3.22275);
#5118=VECTOR('',#19861,3.22275);
#5119=VECTOR('',#19864,3.22275);
#5120=VECTOR('',#19867,3.22275);
#5121=VECTOR('',#19870,3.22275);
#5122=VECTOR('',#19873,3.22275);
#5123=VECTOR('',#19876,3.22275);
#5124=VECTOR('',#19879,3.22275);
#5125=VECTOR('',#19882,3.22275);
#5126=VECTOR('',#19885,3.22275);
#5127=VECTOR('',#19898,10.);
#5128=VECTOR('',#19899,10.);
#5129=VECTOR('',#19900,10.);
#5130=VECTOR('',#19901,10.);
#5131=VECTOR('',#19904,10.);
#5132=VECTOR('',#19905,10.);
#5133=VECTOR('',#19906,10.);
#5134=VECTOR('',#19909,10.);
#5135=VECTOR('',#19910,10.);
#5136=VECTOR('',#19911,10.);
#5137=VECTOR('',#19914,10.);
#5138=VECTOR('',#19915,10.);
#5139=VECTOR('',#19916,10.);
#5140=VECTOR('',#19919,10.);
#5141=VECTOR('',#19920,10.);
#5142=VECTOR('',#19921,10.);
#5143=VECTOR('',#19924,10.);
#5144=VECTOR('',#19925,10.);
#5145=VECTOR('',#19934,6.5);
#5146=VECTOR('',#19945,1.5);
#5147=VECTOR('',#19950,1.5);
#5148=VECTOR('',#19957,1.5555);
#5149=VECTOR('',#19962,1.5555);
#5150=VECTOR('',#19965,1.5555);
#5151=VECTOR('',#19968,1.5555);
#5152=VECTOR('',#19971,1.5555);
#5153=VECTOR('',#19974,1.5555);
#5154=VECTOR('',#19977,1.5555);
#5155=VECTOR('',#19980,1.5555);
#5156=VECTOR('',#19983,1.5555);
#5157=VECTOR('',#19986,1.5555);
#5158=VECTOR('',#19989,1.5555);
#5159=VECTOR('',#19992,1.5555);
#5160=VECTOR('',#19995,1.5555);
#5161=VECTOR('',#19998,1.5555);
#5162=VECTOR('',#20001,1.5555);
#5163=VECTOR('',#20004,1.5555);
#5164=VECTOR('',#20007,1.5555);
#5165=VECTOR('',#20010,1.5555);
#5166=VECTOR('',#20013,1.5555);
#5167=VECTOR('',#20016,1.5555);
#5168=VECTOR('',#20019,1.5555);
#5169=VECTOR('',#20022,1.5555);
#5170=VECTOR('',#20025,1.5555);
#5171=VECTOR('',#20028,1.5555);
#5172=VECTOR('',#20031,1.5555);
#5173=VECTOR('',#20034,1.5555);
#5174=VECTOR('',#20037,1.5555);
#5175=VECTOR('',#20040,1.5555);
#5176=VECTOR('',#20055,10.);
#5177=VECTOR('',#20056,10.);
#5178=VECTOR('',#20057,10.);
#5179=VECTOR('',#20058,10.);
#5180=VECTOR('',#20061,10.);
#5181=VECTOR('',#20062,10.);
#5182=VECTOR('',#20063,10.);
#5183=VECTOR('',#20066,10.);
#5184=VECTOR('',#20067,10.);
#5185=VECTOR('',#20068,10.);
#5186=VECTOR('',#20071,10.);
#5187=VECTOR('',#20072,10.);
#5188=VECTOR('',#20073,10.);
#5189=VECTOR('',#20076,10.);
#5190=VECTOR('',#20077,10.);
#5191=VECTOR('',#20078,10.);
#5192=VECTOR('',#20081,10.);
#5193=VECTOR('',#20082,10.);
#5194=VECTOR('',#20091,3.5);
#5195=VECTOR('',#20114,1.5);
#5196=VECTOR('',#20119,10.);
#5197=VECTOR('',#20120,10.);
#5198=VECTOR('',#20121,10.);
#5199=VECTOR('',#20122,10.);
#5200=VECTOR('',#20125,10.);
#5201=VECTOR('',#20126,10.);
#5202=VECTOR('',#20127,10.);
#5203=VECTOR('',#20130,10.);
#5204=VECTOR('',#20131,10.);
#5205=VECTOR('',#20132,10.);
#5206=VECTOR('',#20135,10.);
#5207=VECTOR('',#20136,10.);
#5208=VECTOR('',#20137,10.);
#5209=VECTOR('',#20140,10.);
#5210=VECTOR('',#20141,10.);
#5211=VECTOR('',#20142,10.);
#5212=VECTOR('',#20145,10.);
#5213=VECTOR('',#20146,10.);
#5214=VECTOR('',#20155,3.5);
#5215=VERTEX_POINT('',#20215);
#5216=VERTEX_POINT('',#20216);
#5217=VERTEX_POINT('',#20218);
#5218=VERTEX_POINT('',#20364);
#5219=VERTEX_POINT('',#20369);
#5220=VERTEX_POINT('',#20371);
#5221=VERTEX_POINT('',#20564);
#5222=VERTEX_POINT('',#20565);
#5223=VERTEX_POINT('',#20567);
#5224=VERTEX_POINT('',#20801);
#5225=VERTEX_POINT('',#21033);
#5226=VERTEX_POINT('',#21034);
#5227=VERTEX_POINT('',#21036);
#5228=VERTEX_POINT('',#21264);
#5229=VERTEX_POINT('',#21499);
#5230=VERTEX_POINT('',#21500);
#5231=VERTEX_POINT('',#21502);
#5232=VERTEX_POINT('',#21730);
#5233=VERTEX_POINT('',#21962);
#5234=VERTEX_POINT('',#21963);
#5235=VERTEX_POINT('',#21965);
#5236=VERTEX_POINT('',#22199);
#5237=VERTEX_POINT('',#22425);
#5238=VERTEX_POINT('',#22426);
#5239=VERTEX_POINT('',#22428);
#5240=VERTEX_POINT('',#22656);
#5241=VERTEX_POINT('',#22891);
#5242=VERTEX_POINT('',#22892);
#5243=VERTEX_POINT('',#22894);
#5244=VERTEX_POINT('',#23125);
#5245=VERTEX_POINT('',#23354);
#5246=VERTEX_POINT('',#23355);
#5247=VERTEX_POINT('',#23357);
#5248=VERTEX_POINT('',#23588);
#5249=VERTEX_POINT('',#23820);
#5250=VERTEX_POINT('',#23821);
#5251=VERTEX_POINT('',#23823);
#5252=VERTEX_POINT('',#24054);
#5253=VERTEX_POINT('',#24289);
#5254=VERTEX_POINT('',#24290);
#5255=VERTEX_POINT('',#24292);
#5256=VERTEX_POINT('',#24375);
#5257=VERTEX_POINT('',#24381);
#5258=VERTEX_POINT('',#24383);
#5259=VERTEX_POINT('',#24531);
#5260=VERTEX_POINT('',#24532);
#5261=VERTEX_POINT('',#24534);
#5262=VERTEX_POINT('',#24632);
#5263=VERTEX_POINT('',#24634);
#5264=VERTEX_POINT('',#24637);
#5265=VERTEX_POINT('',#24774);
#5266=VERTEX_POINT('',#24775);
#5267=VERTEX_POINT('',#24777);
#5268=VERTEX_POINT('',#25165);
#5269=VERTEX_POINT('',#25166);
#5270=VERTEX_POINT('',#25360);
#5271=VERTEX_POINT('',#25552);
#5272=VERTEX_POINT('',#25553);
#5273=VERTEX_POINT('',#25555);
#5274=VERTEX_POINT('',#25937);
#5275=VERTEX_POINT('',#25938);
#5276=VERTEX_POINT('',#26134);
#5277=VERTEX_POINT('',#26328);
#5278=VERTEX_POINT('',#26329);
#5279=VERTEX_POINT('',#26331);
#5280=VERTEX_POINT('',#26715);
#5281=VERTEX_POINT('',#26716);
#5282=VERTEX_POINT('',#26900);
#5283=VERTEX_POINT('',#27096);
#5284=VERTEX_POINT('',#27097);
#5285=VERTEX_POINT('',#27099);
#5286=VERTEX_POINT('',#27489);
#5287=VERTEX_POINT('',#27490);
#5288=VERTEX_POINT('',#27686);
#5289=VERTEX_POINT('',#27895);
#5290=VERTEX_POINT('',#27896);
#5291=VERTEX_POINT('',#27898);
#5292=VERTEX_POINT('',#28025);
#5293=VERTEX_POINT('',#28206);
#5294=VERTEX_POINT('',#28207);
#5295=VERTEX_POINT('',#28209);
#5296=VERTEX_POINT('',#28355);
#5297=VERTEX_POINT('',#28360);
#5298=VERTEX_POINT('',#28362);
#5299=VERTEX_POINT('',#28555);
#5300=VERTEX_POINT('',#28556);
#5301=VERTEX_POINT('',#28558);
#5302=VERTEX_POINT('',#28792);
#5303=VERTEX_POINT('',#29024);
#5304=VERTEX_POINT('',#29025);
#5305=VERTEX_POINT('',#29027);
#5306=VERTEX_POINT('',#29255);
#5307=VERTEX_POINT('',#29490);
#5308=VERTEX_POINT('',#29491);
#5309=VERTEX_POINT('',#29493);
#5310=VERTEX_POINT('',#29721);
#5311=VERTEX_POINT('',#29953);
#5312=VERTEX_POINT('',#29954);
#5313=VERTEX_POINT('',#29956);
#5314=VERTEX_POINT('',#30190);
#5315=VERTEX_POINT('',#30416);
#5316=VERTEX_POINT('',#30417);
#5317=VERTEX_POINT('',#30419);
#5318=VERTEX_POINT('',#30647);
#5319=VERTEX_POINT('',#30882);
#5320=VERTEX_POINT('',#30883);
#5321=VERTEX_POINT('',#30885);
#5322=VERTEX_POINT('',#31116);
#5323=VERTEX_POINT('',#31345);
#5324=VERTEX_POINT('',#31346);
#5325=VERTEX_POINT('',#31348);
#5326=VERTEX_POINT('',#31579);
#5327=VERTEX_POINT('',#31811);
#5328=VERTEX_POINT('',#31812);
#5329=VERTEX_POINT('',#31814);
#5330=VERTEX_POINT('',#32045);
#5331=VERTEX_POINT('',#32280);
#5332=VERTEX_POINT('',#32281);
#5333=VERTEX_POINT('',#32283);
#5334=VERTEX_POINT('',#32366);
#5335=VERTEX_POINT('',#32372);
#5336=VERTEX_POINT('',#32374);
#5337=VERTEX_POINT('',#32522);
#5338=VERTEX_POINT('',#32523);
#5339=VERTEX_POINT('',#32525);
#5340=VERTEX_POINT('',#32623);
#5341=VERTEX_POINT('',#32625);
#5342=VERTEX_POINT('',#32628);
#5343=VERTEX_POINT('',#32769);
#5344=VERTEX_POINT('',#32770);
#5345=VERTEX_POINT('',#32772);
#5346=VERTEX_POINT('',#33162);
#5347=VERTEX_POINT('',#33163);
#5348=VERTEX_POINT('',#33353);
#5349=VERTEX_POINT('',#33541);
#5350=VERTEX_POINT('',#33542);
#5351=VERTEX_POINT('',#33544);
#5352=VERTEX_POINT('',#33924);
#5353=VERTEX_POINT('',#33925);
#5354=VERTEX_POINT('',#34117);
#5355=VERTEX_POINT('',#34311);
#5356=VERTEX_POINT('',#34312);
#5357=VERTEX_POINT('',#34314);
#5358=VERTEX_POINT('',#34706);
#5359=VERTEX_POINT('',#34707);
#5360=VERTEX_POINT('',#34893);
#5361=VERTEX_POINT('',#35087);
#5362=VERTEX_POINT('',#35088);
#5363=VERTEX_POINT('',#35090);
#5364=VERTEX_POINT('',#35482);
#5365=VERTEX_POINT('',#35483);
#5366=VERTEX_POINT('',#35679);
#5367=VERTEX_POINT('',#35888);
#5368=VERTEX_POINT('',#35889);
#5369=VERTEX_POINT('',#35891);
#5370=VERTEX_POINT('',#36020);
#5371=VERTEX_POINT('',#36201);
#5372=VERTEX_POINT('',#36202);
#5373=VERTEX_POINT('',#36204);
#5374=VERTEX_POINT('',#36350);
#5375=VERTEX_POINT('',#36355);
#5376=VERTEX_POINT('',#36357);
#5377=VERTEX_POINT('',#36550);
#5378=VERTEX_POINT('',#36551);
#5379=VERTEX_POINT('',#36553);
#5380=VERTEX_POINT('',#36787);
#5381=VERTEX_POINT('',#37019);
#5382=VERTEX_POINT('',#37020);
#5383=VERTEX_POINT('',#37022);
#5384=VERTEX_POINT('',#37250);
#5385=VERTEX_POINT('',#37485);
#5386=VERTEX_POINT('',#37486);
#5387=VERTEX_POINT('',#37488);
#5388=VERTEX_POINT('',#37716);
#5389=VERTEX_POINT('',#37948);
#5390=VERTEX_POINT('',#37949);
#5391=VERTEX_POINT('',#37951);
#5392=VERTEX_POINT('',#38185);
#5393=VERTEX_POINT('',#38411);
#5394=VERTEX_POINT('',#38412);
#5395=VERTEX_POINT('',#38414);
#5396=VERTEX_POINT('',#38642);
#5397=VERTEX_POINT('',#38877);
#5398=VERTEX_POINT('',#38878);
#5399=VERTEX_POINT('',#38880);
#5400=VERTEX_POINT('',#39111);
#5401=VERTEX_POINT('',#39340);
#5402=VERTEX_POINT('',#39341);
#5403=VERTEX_POINT('',#39343);
#5404=VERTEX_POINT('',#39574);
#5405=VERTEX_POINT('',#39806);
#5406=VERTEX_POINT('',#39807);
#5407=VERTEX_POINT('',#39809);
#5408=VERTEX_POINT('',#40040);
#5409=VERTEX_POINT('',#40275);
#5410=VERTEX_POINT('',#40276);
#5411=VERTEX_POINT('',#40278);
#5412=VERTEX_POINT('',#40361);
#5413=VERTEX_POINT('',#40367);
#5414=VERTEX_POINT('',#40369);
#5415=VERTEX_POINT('',#40517);
#5416=VERTEX_POINT('',#40518);
#5417=VERTEX_POINT('',#40520);
#5418=VERTEX_POINT('',#40618);
#5419=VERTEX_POINT('',#40620);
#5420=VERTEX_POINT('',#40623);
#5421=VERTEX_POINT('',#40764);
#5422=VERTEX_POINT('',#40765);
#5423=VERTEX_POINT('',#40767);
#5424=VERTEX_POINT('',#41157);
#5425=VERTEX_POINT('',#41158);
#5426=VERTEX_POINT('',#41350);
#5427=VERTEX_POINT('',#41548);
#5428=VERTEX_POINT('',#41549);
#5429=VERTEX_POINT('',#41551);
#5430=VERTEX_POINT('',#41933);
#5431=VERTEX_POINT('',#41934);
#5432=VERTEX_POINT('',#42130);
#5433=VERTEX_POINT('',#42326);
#5434=VERTEX_POINT('',#42327);
#5435=VERTEX_POINT('',#42329);
#5436=VERTEX_POINT('',#42717);
#5437=VERTEX_POINT('',#42718);
#5438=VERTEX_POINT('',#42904);
#5439=VERTEX_POINT('',#43102);
#5440=VERTEX_POINT('',#43103);
#5441=VERTEX_POINT('',#43105);
#5442=VERTEX_POINT('',#43497);
#5443=VERTEX_POINT('',#43498);
#5444=VERTEX_POINT('',#43692);
#5445=VERTEX_POINT('',#43901);
#5446=VERTEX_POINT('',#43902);
#5447=VERTEX_POINT('',#43904);
#5448=VERTEX_POINT('',#44033);
#5449=VERTEX_POINT('',#44212);
#5450=VERTEX_POINT('',#44213);
#5451=VERTEX_POINT('',#44215);
#5452=VERTEX_POINT('',#44361);
#5453=VERTEX_POINT('',#44366);
#5454=VERTEX_POINT('',#44368);
#5455=VERTEX_POINT('',#44561);
#5456=VERTEX_POINT('',#44562);
#5457=VERTEX_POINT('',#44564);
#5458=VERTEX_POINT('',#44798);
#5459=VERTEX_POINT('',#45030);
#5460=VERTEX_POINT('',#45031);
#5461=VERTEX_POINT('',#45033);
#5462=VERTEX_POINT('',#45261);
#5463=VERTEX_POINT('',#45496);
#5464=VERTEX_POINT('',#45497);
#5465=VERTEX_POINT('',#45499);
#5466=VERTEX_POINT('',#45727);
#5467=VERTEX_POINT('',#45959);
#5468=VERTEX_POINT('',#45960);
#5469=VERTEX_POINT('',#45962);
#5470=VERTEX_POINT('',#46196);
#5471=VERTEX_POINT('',#46422);
#5472=VERTEX_POINT('',#46423);
#5473=VERTEX_POINT('',#46425);
#5474=VERTEX_POINT('',#46653);
#5475=VERTEX_POINT('',#46888);
#5476=VERTEX_POINT('',#46889);
#5477=VERTEX_POINT('',#46891);
#5478=VERTEX_POINT('',#47122);
#5479=VERTEX_POINT('',#47351);
#5480=VERTEX_POINT('',#47352);
#5481=VERTEX_POINT('',#47354);
#5482=VERTEX_POINT('',#47585);
#5483=VERTEX_POINT('',#47817);
#5484=VERTEX_POINT('',#47818);
#5485=VERTEX_POINT('',#47820);
#5486=VERTEX_POINT('',#48051);
#5487=VERTEX_POINT('',#48286);
#5488=VERTEX_POINT('',#48287);
#5489=VERTEX_POINT('',#48289);
#5490=VERTEX_POINT('',#48372);
#5491=VERTEX_POINT('',#48378);
#5492=VERTEX_POINT('',#48380);
#5493=VERTEX_POINT('',#48528);
#5494=VERTEX_POINT('',#48529);
#5495=VERTEX_POINT('',#48531);
#5496=VERTEX_POINT('',#48629);
#5497=VERTEX_POINT('',#48631);
#5498=VERTEX_POINT('',#48634);
#5499=VERTEX_POINT('',#48775);
#5500=VERTEX_POINT('',#48776);
#5501=VERTEX_POINT('',#48778);
#5502=VERTEX_POINT('',#49164);
#5503=VERTEX_POINT('',#49165);
#5504=VERTEX_POINT('',#49361);
#5505=VERTEX_POINT('',#49551);
#5506=VERTEX_POINT('',#49552);
#5507=VERTEX_POINT('',#49554);
#5508=VERTEX_POINT('',#49932);
#5509=VERTEX_POINT('',#49933);
#5510=VERTEX_POINT('',#50131);
#5511=VERTEX_POINT('',#50325);
#5512=VERTEX_POINT('',#50326);
#5513=VERTEX_POINT('',#50328);
#5514=VERTEX_POINT('',#50720);
#5515=VERTEX_POINT('',#50721);
#5516=VERTEX_POINT('',#50905);
#5517=VERTEX_POINT('',#51103);
#5518=VERTEX_POINT('',#51104);
#5519=VERTEX_POINT('',#51106);
#5520=VERTEX_POINT('',#51500);
#5521=VERTEX_POINT('',#51501);
#5522=VERTEX_POINT('',#51697);
#5523=VERTEX_POINT('',#51906);
#5524=VERTEX_POINT('',#51907);
#5525=VERTEX_POINT('',#51909);
#5526=VERTEX_POINT('',#52038);
#5527=VERTEX_POINT('',#52221);
#5528=VERTEX_POINT('',#52410);
#5529=VERTEX_POINT('',#52603);
#5530=VERTEX_POINT('',#52831);
#5531=VERTEX_POINT('',#53063);
#5532=VERTEX_POINT('',#53254);
#5533=VERTEX_POINT('',#53445);
#5534=VERTEX_POINT('',#53673);
#5535=VERTEX_POINT('',#53905);
#5536=VERTEX_POINT('',#54090);
#5537=VERTEX_POINT('',#54283);
#5538=VERTEX_POINT('',#54511);
#5539=VERTEX_POINT('',#54743);
#5540=VERTEX_POINT('',#54934);
#5541=VERTEX_POINT('',#55125);
#5542=VERTEX_POINT('',#55353);
#5543=VERTEX_POINT('',#56447);
#5544=VERTEX_POINT('',#57409);
#5545=VERTEX_POINT('',#58377);
#5546=VERTEX_POINT('',#59339);
#5547=VERTEX_POINT('',#59446);
#5548=VERTEX_POINT('',#59448);
#5549=VERTEX_POINT('',#59452);
#5550=VERTEX_POINT('',#59454);
#5551=VERTEX_POINT('',#59458);
#5552=VERTEX_POINT('',#59460);
#5553=VERTEX_POINT('',#59464);
#5554=VERTEX_POINT('',#59466);
#5555=VERTEX_POINT('',#59470);
#5556=VERTEX_POINT('',#59471);
#5557=VERTEX_POINT('',#59473);
#5558=VERTEX_POINT('',#59475);
#5559=VERTEX_POINT('',#59479);
#5560=VERTEX_POINT('',#59481);
#5561=VERTEX_POINT('',#59485);
#5562=VERTEX_POINT('',#59487);
#5563=VERTEX_POINT('',#59497);
#5564=VERTEX_POINT('',#59498);
#5565=VERTEX_POINT('',#59500);
#5566=VERTEX_POINT('',#59505);
#5567=VERTEX_POINT('',#59539);
#5568=VERTEX_POINT('',#59540);
#5569=VERTEX_POINT('',#59542);
#5570=VERTEX_POINT('',#59670);
#5571=VERTEX_POINT('',#59866);
#5572=VERTEX_POINT('',#59867);
#5573=VERTEX_POINT('',#59869);
#5574=VERTEX_POINT('',#60067);
#5575=VERTEX_POINT('',#60260);
#5576=VERTEX_POINT('',#60261);
#5577=VERTEX_POINT('',#60263);
#5578=VERTEX_POINT('',#60458);
#5579=VERTEX_POINT('',#60651);
#5580=VERTEX_POINT('',#60652);
#5581=VERTEX_POINT('',#60654);
#5582=VERTEX_POINT('',#60846);
#5583=VERTEX_POINT('',#61042);
#5584=VERTEX_POINT('',#61043);
#5585=VERTEX_POINT('',#61045);
#5586=VERTEX_POINT('',#61237);
#5587=VERTEX_POINT('',#61430);
#5588=VERTEX_POINT('',#61431);
#5589=VERTEX_POINT('',#61433);
#5590=VERTEX_POINT('',#61628);
#5591=VERTEX_POINT('',#61821);
#5592=VERTEX_POINT('',#61822);
#5593=VERTEX_POINT('',#61824);
#5594=VERTEX_POINT('',#62013);
#5595=VERTEX_POINT('',#62212);
#5596=VERTEX_POINT('',#62213);
#5597=VERTEX_POINT('',#62215);
#5598=VERTEX_POINT('',#62407);
#5599=VERTEX_POINT('',#62600);
#5600=VERTEX_POINT('',#62601);
#5601=VERTEX_POINT('',#62603);
#5602=VERTEX_POINT('',#62801);
#5603=VERTEX_POINT('',#62994);
#5604=VERTEX_POINT('',#62995);
#5605=VERTEX_POINT('',#62997);
#5606=VERTEX_POINT('',#63189);
#5607=VERTEX_POINT('',#63385);
#5608=VERTEX_POINT('',#63386);
#5609=VERTEX_POINT('',#63388);
#5610=VERTEX_POINT('',#63580);
#5611=VERTEX_POINT('',#63776);
#5612=VERTEX_POINT('',#63777);
#5613=VERTEX_POINT('',#63779);
#5614=VERTEX_POINT('',#63977);
#5615=VERTEX_POINT('',#64170);
#5616=VERTEX_POINT('',#64171);
#5617=VERTEX_POINT('',#64173);
#5618=VERTEX_POINT('',#64365);
#5619=VERTEX_POINT('',#64561);
#5620=VERTEX_POINT('',#64562);
#5621=VERTEX_POINT('',#64564);
#5622=VERTEX_POINT('',#64753);
#5623=VERTEX_POINT('',#64949);
#5624=VERTEX_POINT('',#64950);
#5625=VERTEX_POINT('',#64952);
#5626=VERTEX_POINT('',#65023);
#5627=VERTEX_POINT('',#65029);
#5628=VERTEX_POINT('',#65031);
#5629=VERTEX_POINT('',#65158);
#5630=VERTEX_POINT('',#65159);
#5631=VERTEX_POINT('',#65161);
#5632=VERTEX_POINT('',#65322);
#5633=VERTEX_POINT('',#65324);
#5634=VERTEX_POINT('',#65335);
#5635=VERTEX_POINT('',#65585);
#5636=VERTEX_POINT('',#65586);
#5637=VERTEX_POINT('',#65794);
#5638=VERTEX_POINT('',#65815);
#5639=VERTEX_POINT('',#65816);
#5640=VERTEX_POINT('',#65818);
#5641=VERTEX_POINT('',#66025);
#5642=VERTEX_POINT('',#66228);
#5643=VERTEX_POINT('',#66229);
#5644=VERTEX_POINT('',#66674);
#5645=VERTEX_POINT('',#66675);
#5646=VERTEX_POINT('',#66677);
#5647=VERTEX_POINT('',#66924);
#5648=VERTEX_POINT('',#67130);
#5649=VERTEX_POINT('',#67131);
#5650=VERTEX_POINT('',#67562);
#5651=VERTEX_POINT('',#67563);
#5652=VERTEX_POINT('',#67565);
#5653=VERTEX_POINT('',#67792);
#5654=VERTEX_POINT('',#67994);
#5655=VERTEX_POINT('',#67995);
#5656=VERTEX_POINT('',#68394);
#5657=VERTEX_POINT('',#68395);
#5658=VERTEX_POINT('',#68397);
#5659=VERTEX_POINT('',#68614);
#5660=VERTEX_POINT('',#68848);
#5661=VERTEX_POINT('',#68849);
#5662=VERTEX_POINT('',#69284);
#5663=VERTEX_POINT('',#69285);
#5664=VERTEX_POINT('',#69287);
#5665=VERTEX_POINT('',#69488);
#5666=VERTEX_POINT('',#69712);
#5667=VERTEX_POINT('',#69713);
#5668=VERTEX_POINT('',#70124);
#5669=VERTEX_POINT('',#70125);
#5670=VERTEX_POINT('',#70127);
#5671=VERTEX_POINT('',#70340);
#5672=VERTEX_POINT('',#70552);
#5673=VERTEX_POINT('',#70553);
#5674=VERTEX_POINT('',#70968);
#5675=VERTEX_POINT('',#70969);
#5676=VERTEX_POINT('',#70971);
#5677=VERTEX_POINT('',#71106);
#5678=VERTEX_POINT('',#71311);
#5679=VERTEX_POINT('',#71312);
#5680=VERTEX_POINT('',#71314);
#5681=VERTEX_POINT('',#71319);
#5682=VERTEX_POINT('',#71353);
#5683=VERTEX_POINT('',#71354);
#5684=VERTEX_POINT('',#71356);
#5685=VERTEX_POINT('',#71484);
#5686=VERTEX_POINT('',#71680);
#5687=VERTEX_POINT('',#71681);
#5688=VERTEX_POINT('',#71683);
#5689=VERTEX_POINT('',#71881);
#5690=VERTEX_POINT('',#72074);
#5691=VERTEX_POINT('',#72075);
#5692=VERTEX_POINT('',#72077);
#5693=VERTEX_POINT('',#72272);
#5694=VERTEX_POINT('',#72465);
#5695=VERTEX_POINT('',#72466);
#5696=VERTEX_POINT('',#72468);
#5697=VERTEX_POINT('',#72660);
#5698=VERTEX_POINT('',#72856);
#5699=VERTEX_POINT('',#72857);
#5700=VERTEX_POINT('',#72859);
#5701=VERTEX_POINT('',#73051);
#5702=VERTEX_POINT('',#73244);
#5703=VERTEX_POINT('',#73245);
#5704=VERTEX_POINT('',#73247);
#5705=VERTEX_POINT('',#73442);
#5706=VERTEX_POINT('',#73635);
#5707=VERTEX_POINT('',#73636);
#5708=VERTEX_POINT('',#73638);
#5709=VERTEX_POINT('',#73827);
#5710=VERTEX_POINT('',#74026);
#5711=VERTEX_POINT('',#74027);
#5712=VERTEX_POINT('',#74029);
#5713=VERTEX_POINT('',#74221);
#5714=VERTEX_POINT('',#74414);
#5715=VERTEX_POINT('',#74415);
#5716=VERTEX_POINT('',#74417);
#5717=VERTEX_POINT('',#74615);
#5718=VERTEX_POINT('',#74808);
#5719=VERTEX_POINT('',#74809);
#5720=VERTEX_POINT('',#74811);
#5721=VERTEX_POINT('',#75003);
#5722=VERTEX_POINT('',#75199);
#5723=VERTEX_POINT('',#75200);
#5724=VERTEX_POINT('',#75202);
#5725=VERTEX_POINT('',#75394);
#5726=VERTEX_POINT('',#75590);
#5727=VERTEX_POINT('',#75591);
#5728=VERTEX_POINT('',#75593);
#5729=VERTEX_POINT('',#75791);
#5730=VERTEX_POINT('',#75984);
#5731=VERTEX_POINT('',#75985);
#5732=VERTEX_POINT('',#75987);
#5733=VERTEX_POINT('',#76179);
#5734=VERTEX_POINT('',#76375);
#5735=VERTEX_POINT('',#76376);
#5736=VERTEX_POINT('',#76378);
#5737=VERTEX_POINT('',#76567);
#5738=VERTEX_POINT('',#76763);
#5739=VERTEX_POINT('',#76764);
#5740=VERTEX_POINT('',#76766);
#5741=VERTEX_POINT('',#76837);
#5742=VERTEX_POINT('',#76843);
#5743=VERTEX_POINT('',#76845);
#5744=VERTEX_POINT('',#76972);
#5745=VERTEX_POINT('',#76973);
#5746=VERTEX_POINT('',#76975);
#5747=VERTEX_POINT('',#77136);
#5748=VERTEX_POINT('',#77138);
#5749=VERTEX_POINT('',#77151);
#5750=VERTEX_POINT('',#77447);
#5751=VERTEX_POINT('',#77448);
#5752=VERTEX_POINT('',#77658);
#5753=VERTEX_POINT('',#77681);
#5754=VERTEX_POINT('',#77682);
#5755=VERTEX_POINT('',#77684);
#5756=VERTEX_POINT('',#77887);
#5757=VERTEX_POINT('',#78092);
#5758=VERTEX_POINT('',#78093);
#5759=VERTEX_POINT('',#78508);
#5760=VERTEX_POINT('',#78509);
#5761=VERTEX_POINT('',#78511);
#5762=VERTEX_POINT('',#78758);
#5763=VERTEX_POINT('',#78966);
#5764=VERTEX_POINT('',#78967);
#5765=VERTEX_POINT('',#79394);
#5766=VERTEX_POINT('',#79395);
#5767=VERTEX_POINT('',#79397);
#5768=VERTEX_POINT('',#79604);
#5769=VERTEX_POINT('',#79804);
#5770=VERTEX_POINT('',#79805);
#5771=VERTEX_POINT('',#80232);
#5772=VERTEX_POINT('',#80233);
#5773=VERTEX_POINT('',#80235);
#5774=VERTEX_POINT('',#80448);
#5775=VERTEX_POINT('',#80684);
#5776=VERTEX_POINT('',#80685);
#5777=VERTEX_POINT('',#81128);
#5778=VERTEX_POINT('',#81129);
#5779=VERTEX_POINT('',#81131);
#5780=VERTEX_POINT('',#81332);
#5781=VERTEX_POINT('',#81556);
#5782=VERTEX_POINT('',#81557);
#5783=VERTEX_POINT('',#81968);
#5784=VERTEX_POINT('',#81969);
#5785=VERTEX_POINT('',#81971);
#5786=VERTEX_POINT('',#82182);
#5787=VERTEX_POINT('',#82392);
#5788=VERTEX_POINT('',#82393);
#5789=VERTEX_POINT('',#82818);
#5790=VERTEX_POINT('',#82819);
#5791=VERTEX_POINT('',#82821);
#5792=VERTEX_POINT('',#82966);
#5793=VERTEX_POINT('',#83175);
#5794=VERTEX_POINT('',#83176);
#5795=VERTEX_POINT('',#83178);
#5796=VERTEX_POINT('',#83187);
#5797=VERTEX_POINT('',#83189);
#5798=VERTEX_POINT('',#83331);
#5799=VERTEX_POINT('',#83332);
#5800=VERTEX_POINT('',#83334);
#5801=VERTEX_POINT('',#83468);
#5802=VERTEX_POINT('',#83661);
#5803=VERTEX_POINT('',#83662);
#5804=VERTEX_POINT('',#83664);
#5805=VERTEX_POINT('',#83856);
#5806=VERTEX_POINT('',#84052);
#5807=VERTEX_POINT('',#84053);
#5808=VERTEX_POINT('',#84055);
#5809=VERTEX_POINT('',#84247);
#5810=VERTEX_POINT('',#84440);
#5811=VERTEX_POINT('',#84441);
#5812=VERTEX_POINT('',#84443);
#5813=VERTEX_POINT('',#84638);
#5814=VERTEX_POINT('',#84831);
#5815=VERTEX_POINT('',#84832);
#5816=VERTEX_POINT('',#84834);
#5817=VERTEX_POINT('',#85023);
#5818=VERTEX_POINT('',#85222);
#5819=VERTEX_POINT('',#85223);
#5820=VERTEX_POINT('',#85225);
#5821=VERTEX_POINT('',#85417);
#5822=VERTEX_POINT('',#85610);
#5823=VERTEX_POINT('',#85611);
#5824=VERTEX_POINT('',#85613);
#5825=VERTEX_POINT('',#85808);
#5826=VERTEX_POINT('',#86001);
#5827=VERTEX_POINT('',#86002);
#5828=VERTEX_POINT('',#86004);
#5829=VERTEX_POINT('',#86196);
#5830=VERTEX_POINT('',#86392);
#5831=VERTEX_POINT('',#86393);
#5832=VERTEX_POINT('',#86395);
#5833=VERTEX_POINT('',#86587);
#5834=VERTEX_POINT('',#86783);
#5835=VERTEX_POINT('',#86784);
#5836=VERTEX_POINT('',#86786);
#5837=VERTEX_POINT('',#86984);
#5838=VERTEX_POINT('',#87177);
#5839=VERTEX_POINT('',#87178);
#5840=VERTEX_POINT('',#87180);
#5841=VERTEX_POINT('',#87256);
#5842=VERTEX_POINT('',#87452);
#5843=VERTEX_POINT('',#87453);
#5844=VERTEX_POINT('',#87455);
#5845=VERTEX_POINT('',#87583);
#5846=VERTEX_POINT('',#87779);
#5847=VERTEX_POINT('',#87780);
#5848=VERTEX_POINT('',#87782);
#5849=VERTEX_POINT('',#87853);
#5850=VERTEX_POINT('',#87859);
#5851=VERTEX_POINT('',#87861);
#5852=VERTEX_POINT('',#87988);
#5853=VERTEX_POINT('',#87989);
#5854=VERTEX_POINT('',#87991);
#5855=VERTEX_POINT('',#88000);
#5856=VERTEX_POINT('',#88002);
#5857=VERTEX_POINT('',#88144);
#5858=VERTEX_POINT('',#88145);
#5859=VERTEX_POINT('',#88147);
#5860=VERTEX_POINT('',#88281);
#5861=VERTEX_POINT('',#88474);
#5862=VERTEX_POINT('',#88475);
#5863=VERTEX_POINT('',#88477);
#5864=VERTEX_POINT('',#88669);
#5865=VERTEX_POINT('',#88865);
#5866=VERTEX_POINT('',#88866);
#5867=VERTEX_POINT('',#88868);
#5868=VERTEX_POINT('',#89060);
#5869=VERTEX_POINT('',#89253);
#5870=VERTEX_POINT('',#89254);
#5871=VERTEX_POINT('',#89256);
#5872=VERTEX_POINT('',#89451);
#5873=VERTEX_POINT('',#89644);
#5874=VERTEX_POINT('',#89645);
#5875=VERTEX_POINT('',#89647);
#5876=VERTEX_POINT('',#89836);
#5877=VERTEX_POINT('',#90035);
#5878=VERTEX_POINT('',#90036);
#5879=VERTEX_POINT('',#90038);
#5880=VERTEX_POINT('',#90230);
#5881=VERTEX_POINT('',#90423);
#5882=VERTEX_POINT('',#90424);
#5883=VERTEX_POINT('',#90426);
#5884=VERTEX_POINT('',#90621);
#5885=VERTEX_POINT('',#90814);
#5886=VERTEX_POINT('',#90815);
#5887=VERTEX_POINT('',#90817);
#5888=VERTEX_POINT('',#91009);
#5889=VERTEX_POINT('',#91205);
#5890=VERTEX_POINT('',#91206);
#5891=VERTEX_POINT('',#91208);
#5892=VERTEX_POINT('',#91400);
#5893=VERTEX_POINT('',#91596);
#5894=VERTEX_POINT('',#91597);
#5895=VERTEX_POINT('',#91599);
#5896=VERTEX_POINT('',#91797);
#5897=VERTEX_POINT('',#91990);
#5898=VERTEX_POINT('',#91991);
#5899=VERTEX_POINT('',#91993);
#5900=VERTEX_POINT('',#92069);
#5901=VERTEX_POINT('',#92265);
#5902=VERTEX_POINT('',#92266);
#5903=VERTEX_POINT('',#92268);
#5904=VERTEX_POINT('',#92396);
#5905=VERTEX_POINT('',#92592);
#5906=VERTEX_POINT('',#92593);
#5907=VERTEX_POINT('',#92595);
#5908=VERTEX_POINT('',#92666);
#5909=VERTEX_POINT('',#92672);
#5910=VERTEX_POINT('',#92674);
#5911=VERTEX_POINT('',#92801);
#5912=VERTEX_POINT('',#92802);
#5913=VERTEX_POINT('',#92804);
#5914=VERTEX_POINT('',#92813);
#5915=VERTEX_POINT('',#92815);
#5916=VERTEX_POINT('',#92957);
#5917=VERTEX_POINT('',#92958);
#5918=VERTEX_POINT('',#92960);
#5919=VERTEX_POINT('',#93094);
#5920=VERTEX_POINT('',#93287);
#5921=VERTEX_POINT('',#93288);
#5922=VERTEX_POINT('',#93290);
#5923=VERTEX_POINT('',#93482);
#5924=VERTEX_POINT('',#93678);
#5925=VERTEX_POINT('',#93679);
#5926=VERTEX_POINT('',#93681);
#5927=VERTEX_POINT('',#93873);
#5928=VERTEX_POINT('',#94066);
#5929=VERTEX_POINT('',#94067);
#5930=VERTEX_POINT('',#94069);
#5931=VERTEX_POINT('',#94264);
#5932=VERTEX_POINT('',#94457);
#5933=VERTEX_POINT('',#94458);
#5934=VERTEX_POINT('',#94460);
#5935=VERTEX_POINT('',#94649);
#5936=VERTEX_POINT('',#94848);
#5937=VERTEX_POINT('',#94849);
#5938=VERTEX_POINT('',#94851);
#5939=VERTEX_POINT('',#95043);
#5940=VERTEX_POINT('',#95236);
#5941=VERTEX_POINT('',#95237);
#5942=VERTEX_POINT('',#95239);
#5943=VERTEX_POINT('',#95434);
#5944=VERTEX_POINT('',#95627);
#5945=VERTEX_POINT('',#95628);
#5946=VERTEX_POINT('',#95630);
#5947=VERTEX_POINT('',#95822);
#5948=VERTEX_POINT('',#96018);
#5949=VERTEX_POINT('',#96019);
#5950=VERTEX_POINT('',#96021);
#5951=VERTEX_POINT('',#96213);
#5952=VERTEX_POINT('',#96409);
#5953=VERTEX_POINT('',#96410);
#5954=VERTEX_POINT('',#96412);
#5955=VERTEX_POINT('',#96610);
#5956=VERTEX_POINT('',#96803);
#5957=VERTEX_POINT('',#96804);
#5958=VERTEX_POINT('',#96806);
#5959=VERTEX_POINT('',#96998);
#5960=VERTEX_POINT('',#97194);
#5961=VERTEX_POINT('',#97195);
#5962=VERTEX_POINT('',#97197);
#5963=VERTEX_POINT('',#97386);
#5964=VERTEX_POINT('',#97582);
#5965=VERTEX_POINT('',#97583);
#5966=VERTEX_POINT('',#97585);
#5967=VERTEX_POINT('',#97656);
#5968=VERTEX_POINT('',#97662);
#5969=VERTEX_POINT('',#97664);
#5970=VERTEX_POINT('',#97791);
#5971=VERTEX_POINT('',#97792);
#5972=VERTEX_POINT('',#97794);
#5973=VERTEX_POINT('',#97803);
#5974=VERTEX_POINT('',#97805);
#5975=VERTEX_POINT('',#97947);
#5976=VERTEX_POINT('',#97948);
#5977=VERTEX_POINT('',#97950);
#5978=VERTEX_POINT('',#98084);
#5979=VERTEX_POINT('',#98277);
#5980=VERTEX_POINT('',#98278);
#5981=VERTEX_POINT('',#98280);
#5982=VERTEX_POINT('',#98472);
#5983=VERTEX_POINT('',#98668);
#5984=VERTEX_POINT('',#98669);
#5985=VERTEX_POINT('',#98671);
#5986=VERTEX_POINT('',#98863);
#5987=VERTEX_POINT('',#99056);
#5988=VERTEX_POINT('',#99057);
#5989=VERTEX_POINT('',#99059);
#5990=VERTEX_POINT('',#99254);
#5991=VERTEX_POINT('',#99447);
#5992=VERTEX_POINT('',#99448);
#5993=VERTEX_POINT('',#99450);
#5994=VERTEX_POINT('',#99639);
#5995=VERTEX_POINT('',#99838);
#5996=VERTEX_POINT('',#99839);
#5997=VERTEX_POINT('',#99841);
#5998=VERTEX_POINT('',#100033);
#5999=VERTEX_POINT('',#100226);
#6000=VERTEX_POINT('',#100227);
#6001=VERTEX_POINT('',#100229);
#6002=VERTEX_POINT('',#100424);
#6003=VERTEX_POINT('',#100617);
#6004=VERTEX_POINT('',#100618);
#6005=VERTEX_POINT('',#100620);
#6006=VERTEX_POINT('',#100812);
#6007=VERTEX_POINT('',#101008);
#6008=VERTEX_POINT('',#101009);
#6009=VERTEX_POINT('',#101011);
#6010=VERTEX_POINT('',#101203);
#6011=VERTEX_POINT('',#101399);
#6012=VERTEX_POINT('',#101400);
#6013=VERTEX_POINT('',#101402);
#6014=VERTEX_POINT('',#101600);
#6015=VERTEX_POINT('',#101793);
#6016=VERTEX_POINT('',#101794);
#6017=VERTEX_POINT('',#101796);
#6018=VERTEX_POINT('',#101988);
#6019=VERTEX_POINT('',#102184);
#6020=VERTEX_POINT('',#102185);
#6021=VERTEX_POINT('',#102187);
#6022=VERTEX_POINT('',#102376);
#6023=VERTEX_POINT('',#102572);
#6024=VERTEX_POINT('',#102573);
#6025=VERTEX_POINT('',#102575);
#6026=VERTEX_POINT('',#102646);
#6027=VERTEX_POINT('',#102652);
#6028=VERTEX_POINT('',#102654);
#6029=VERTEX_POINT('',#102781);
#6030=VERTEX_POINT('',#102782);
#6031=VERTEX_POINT('',#102784);
#6032=VERTEX_POINT('',#102849);
#6033=VERTEX_POINT('',#102972);
#6034=VERTEX_POINT('',#102973);
#6035=VERTEX_POINT('',#102975);
#6036=VERTEX_POINT('',#103401);
#6037=VERTEX_POINT('',#103402);
#6038=VERTEX_POINT('',#103620);
#6039=VERTEX_POINT('',#103834);
#6040=VERTEX_POINT('',#103835);
#6041=VERTEX_POINT('',#103837);
#6042=VERTEX_POINT('',#104271);
#6043=VERTEX_POINT('',#104272);
#6044=VERTEX_POINT('',#104474);
#6045=VERTEX_POINT('',#104756);
#6046=VERTEX_POINT('',#104757);
#6047=VERTEX_POINT('',#104759);
#6048=VERTEX_POINT('',#105199);
#6049=VERTEX_POINT('',#105200);
#6050=VERTEX_POINT('',#105438);
#6051=VERTEX_POINT('',#105619);
#6052=VERTEX_POINT('',#105620);
#6053=VERTEX_POINT('',#105622);
#6054=VERTEX_POINT('',#105845);
#6055=VERTEX_POINT('',#105869);
#6056=VERTEX_POINT('',#105870);
#6057=VERTEX_POINT('',#106078);
#6058=VERTEX_POINT('',#106273);
#6059=VERTEX_POINT('',#106274);
#6060=VERTEX_POINT('',#106276);
#6061=VERTEX_POINT('',#106708);
#6062=VERTEX_POINT('',#106709);
#6063=VERTEX_POINT('',#106909);
#6064=VERTEX_POINT('',#107117);
#6065=VERTEX_POINT('',#107118);
#6066=VERTEX_POINT('',#107120);
#6067=VERTEX_POINT('',#107518);
#6068=VERTEX_POINT('',#107519);
#6069=VERTEX_POINT('',#107719);
#6070=VERTEX_POINT('',#107935);
#6071=VERTEX_POINT('',#107936);
#6072=VERTEX_POINT('',#107938);
#6073=VERTEX_POINT('',#107959);
#6074=VERTEX_POINT('',#108069);
#6075=VERTEX_POINT('',#108252);
#6076=VERTEX_POINT('',#108253);
#6077=VERTEX_POINT('',#108255);
#6078=VERTEX_POINT('',#108320);
#6079=VERTEX_POINT('',#108441);
#6080=VERTEX_POINT('',#108442);
#6081=VERTEX_POINT('',#108444);
#6082=VERTEX_POINT('',#108858);
#6083=VERTEX_POINT('',#108859);
#6084=VERTEX_POINT('',#109077);
#6085=VERTEX_POINT('',#109291);
#6086=VERTEX_POINT('',#109292);
#6087=VERTEX_POINT('',#109294);
#6088=VERTEX_POINT('',#109728);
#6089=VERTEX_POINT('',#109729);
#6090=VERTEX_POINT('',#109939);
#6091=VERTEX_POINT('',#110221);
#6092=VERTEX_POINT('',#110222);
#6093=VERTEX_POINT('',#110224);
#6094=VERTEX_POINT('',#110664);
#6095=VERTEX_POINT('',#110665);
#6096=VERTEX_POINT('',#110903);
#6097=VERTEX_POINT('',#111086);
#6098=VERTEX_POINT('',#111087);
#6099=VERTEX_POINT('',#111089);
#6100=VERTEX_POINT('',#111312);
#6101=VERTEX_POINT('',#111336);
#6102=VERTEX_POINT('',#111337);
#6103=VERTEX_POINT('',#111545);
#6104=VERTEX_POINT('',#111734);
#6105=VERTEX_POINT('',#111735);
#6106=VERTEX_POINT('',#111737);
#6107=VERTEX_POINT('',#112167);
#6108=VERTEX_POINT('',#112168);
#6109=VERTEX_POINT('',#112388);
#6110=VERTEX_POINT('',#112580);
#6111=VERTEX_POINT('',#112581);
#6112=VERTEX_POINT('',#112583);
#6113=VERTEX_POINT('',#112997);
#6114=VERTEX_POINT('',#112998);
#6115=VERTEX_POINT('',#113202);
#6116=VERTEX_POINT('',#113418);
#6117=VERTEX_POINT('',#113419);
#6118=VERTEX_POINT('',#113421);
#6119=VERTEX_POINT('',#113442);
#6120=VERTEX_POINT('',#113552);
#6121=VERTEX_POINT('',#113729);
#6122=VERTEX_POINT('',#113730);
#6123=VERTEX_POINT('',#113732);
#6124=VERTEX_POINT('',#113805);
#6125=VERTEX_POINT('',#113928);
#6126=VERTEX_POINT('',#113929);
#6127=VERTEX_POINT('',#114354);
#6128=VERTEX_POINT('',#114355);
#6129=VERTEX_POINT('',#114571);
#6130=VERTEX_POINT('',#114779);
#6131=VERTEX_POINT('',#114780);
#6132=VERTEX_POINT('',#115191);
#6133=VERTEX_POINT('',#115192);
#6134=VERTEX_POINT('',#115398);
#6135=VERTEX_POINT('',#115680);
#6136=VERTEX_POINT('',#115681);
#6137=VERTEX_POINT('',#115683);
#6138=VERTEX_POINT('',#116109);
#6139=VERTEX_POINT('',#116110);
#6140=VERTEX_POINT('',#116342);
#6141=VERTEX_POINT('',#116523);
#6142=VERTEX_POINT('',#116524);
#6143=VERTEX_POINT('',#116526);
#6144=VERTEX_POINT('',#116749);
#6145=VERTEX_POINT('',#116773);
#6146=VERTEX_POINT('',#116774);
#6147=VERTEX_POINT('',#116988);
#6148=VERTEX_POINT('',#117187);
#6149=VERTEX_POINT('',#117188);
#6150=VERTEX_POINT('',#117190);
#6151=VERTEX_POINT('',#117620);
#6152=VERTEX_POINT('',#117621);
#6153=VERTEX_POINT('',#117815);
#6154=VERTEX_POINT('',#118019);
#6155=VERTEX_POINT('',#118020);
#6156=VERTEX_POINT('',#118022);
#6157=VERTEX_POINT('',#118412);
#6158=VERTEX_POINT('',#118413);
#6159=VERTEX_POINT('',#118832);
#6160=VERTEX_POINT('',#118833);
#6161=VERTEX_POINT('',#118835);
#6162=VERTEX_POINT('',#118966);
#6163=VERTEX_POINT('',#119157);
#6164=VERTEX_POINT('',#119158);
#6165=VERTEX_POINT('',#119160);
#6166=VERTEX_POINT('',#119235);
#6167=VERTEX_POINT('',#119360);
#6168=VERTEX_POINT('',#119361);
#6169=VERTEX_POINT('',#119786);
#6170=VERTEX_POINT('',#119787);
#6171=VERTEX_POINT('',#120003);
#6172=VERTEX_POINT('',#120209);
#6173=VERTEX_POINT('',#120210);
#6174=VERTEX_POINT('',#120625);
#6175=VERTEX_POINT('',#120626);
#6176=VERTEX_POINT('',#120840);
#6177=VERTEX_POINT('',#121122);
#6178=VERTEX_POINT('',#121123);
#6179=VERTEX_POINT('',#121125);
#6180=VERTEX_POINT('',#121571);
#6181=VERTEX_POINT('',#121572);
#6182=VERTEX_POINT('',#121794);
#6183=VERTEX_POINT('',#121977);
#6184=VERTEX_POINT('',#121978);
#6185=VERTEX_POINT('',#121980);
#6186=VERTEX_POINT('',#122205);
#6187=VERTEX_POINT('',#122229);
#6188=VERTEX_POINT('',#122230);
#6189=VERTEX_POINT('',#122438);
#6190=VERTEX_POINT('',#122645);
#6191=VERTEX_POINT('',#122646);
#6192=VERTEX_POINT('',#122648);
#6193=VERTEX_POINT('',#123078);
#6194=VERTEX_POINT('',#123079);
#6195=VERTEX_POINT('',#123287);
#6196=VERTEX_POINT('',#123497);
#6197=VERTEX_POINT('',#123498);
#6198=VERTEX_POINT('',#123500);
#6199=VERTEX_POINT('',#123904);
#6200=VERTEX_POINT('',#123905);
#6201=VERTEX_POINT('',#124324);
#6202=VERTEX_POINT('',#124325);
#6203=VERTEX_POINT('',#124327);
#6204=VERTEX_POINT('',#124460);
#6205=VERTEX_POINT('',#124651);
#6206=VERTEX_POINT('',#125149);
#6207=VERTEX_POINT('',#125647);
#6208=VERTEX_POINT('',#126059);
#6209=VERTEX_POINT('',#126461);
#6210=VERTEX_POINT('',#126653);
#6211=VERTEX_POINT('',#126846);
#6212=VERTEX_POINT('',#127038);
#6213=VERTEX_POINT('',#127231);
#6214=VERTEX_POINT('',#127423);
#6215=VERTEX_POINT('',#127616);
#6216=VERTEX_POINT('',#127808);
#6217=VERTEX_POINT('',#128001);
#6218=VERTEX_POINT('',#128415);
#6219=VERTEX_POINT('',#128607);
#6220=VERTEX_POINT('',#128800);
#6221=VERTEX_POINT('',#129218);
#6222=VERTEX_POINT('',#129410);
#6223=VERTEX_POINT('',#130690);
#6224=VERTEX_POINT('',#131871);
#6225=VERTEX_POINT('',#131964);
#6226=VERTEX_POINT('',#131965);
#6227=VERTEX_POINT('',#131967);
#6228=VERTEX_POINT('',#131969);
#6229=VERTEX_POINT('',#131973);
#6230=VERTEX_POINT('',#131975);
#6231=VERTEX_POINT('',#131979);
#6232=VERTEX_POINT('',#131981);
#6233=VERTEX_POINT('',#131988);
#6234=VERTEX_POINT('',#131990);
#6235=VERTEX_POINT('',#131994);
#6236=VERTEX_POINT('',#131996);
#6237=VERTEX_POINT('',#132000);
#6238=VERTEX_POINT('',#132002);
#6239=VERTEX_POINT('',#132006);
#6240=VERTEX_POINT('',#132008);
#6241=VERTEX_POINT('',#132391);
#6242=VERTEX_POINT('',#133031);
#6243=VERTEX_POINT('',#133501);
#6244=VERTEX_POINT('',#134141);
#6245=VERTEX_POINT('',#134611);
#6246=VERTEX_POINT('',#135251);
#6247=VERTEX_POINT('',#135721);
#6248=VERTEX_POINT('',#136361);
#6249=VERTEX_POINT('',#136456);
#6250=VERTEX_POINT('',#136458);
#6251=VERTEX_POINT('',#136462);
#6252=VERTEX_POINT('',#136463);
#6253=VERTEX_POINT('',#136465);
#6254=VERTEX_POINT('',#136467);
#6255=VERTEX_POINT('',#136470);
#6256=VERTEX_POINT('',#136471);
#6257=VERTEX_POINT('',#136473);
#6258=VERTEX_POINT('',#136475);
#6259=VERTEX_POINT('',#136479);
#6260=VERTEX_POINT('',#136480);
#6261=VERTEX_POINT('',#136485);
#6262=VERTEX_POINT('',#136489);
#6263=VERTEX_POINT('',#136496);
#6264=VERTEX_POINT('',#136498);
#6265=VERTEX_POINT('',#136502);
#6266=VERTEX_POINT('',#136506);
#6267=VERTEX_POINT('',#136514);
#6268=VERTEX_POINT('',#136515);
#6269=VERTEX_POINT('',#136517);
#6270=VERTEX_POINT('',#136519);
#6271=VERTEX_POINT('',#136523);
#6272=VERTEX_POINT('',#136524);
#6273=VERTEX_POINT('',#136526);
#6274=VERTEX_POINT('',#136528);
#6275=VERTEX_POINT('',#136541);
#6276=VERTEX_POINT('',#136542);
#6277=VERTEX_POINT('',#136544);
#6278=VERTEX_POINT('',#136684);
#6279=VERTEX_POINT('',#136686);
#6280=VERTEX_POINT('',#136689);
#6281=VERTEX_POINT('',#136900);
#6282=VERTEX_POINT('',#136901);
#6283=VERTEX_POINT('',#136903);
#6284=VERTEX_POINT('',#137152);
#6285=VERTEX_POINT('',#137408);
#6286=VERTEX_POINT('',#137409);
#6287=VERTEX_POINT('',#137411);
#6288=VERTEX_POINT('',#137666);
#6289=VERTEX_POINT('',#137919);
#6290=VERTEX_POINT('',#137920);
#6291=VERTEX_POINT('',#137922);
#6292=VERTEX_POINT('',#138174);
#6293=VERTEX_POINT('',#138412);
#6294=VERTEX_POINT('',#138413);
#6295=VERTEX_POINT('',#138415);
#6296=VERTEX_POINT('',#138667);
#6297=VERTEX_POINT('',#138920);
#6298=VERTEX_POINT('',#138921);
#6299=VERTEX_POINT('',#138923);
#6300=VERTEX_POINT('',#139178);
#6301=VERTEX_POINT('',#139431);
#6302=VERTEX_POINT('',#139432);
#6303=VERTEX_POINT('',#139434);
#6304=VERTEX_POINT('',#139692);
#6305=VERTEX_POINT('',#139939);
#6306=VERTEX_POINT('',#139940);
#6307=VERTEX_POINT('',#139942);
#6308=VERTEX_POINT('',#140197);
#6309=VERTEX_POINT('',#140450);
#6310=VERTEX_POINT('',#140451);
#6311=VERTEX_POINT('',#140453);
#6312=VERTEX_POINT('',#140705);
#6313=VERTEX_POINT('',#140958);
#6314=VERTEX_POINT('',#140959);
#6315=VERTEX_POINT('',#140961);
#6316=VERTEX_POINT('',#141213);
#6317=VERTEX_POINT('',#141472);
#6318=VERTEX_POINT('',#141473);
#6319=VERTEX_POINT('',#141475);
#6320=VERTEX_POINT('',#141727);
#6321=VERTEX_POINT('',#141965);
#6322=VERTEX_POINT('',#141966);
#6323=VERTEX_POINT('',#141968);
#6324=VERTEX_POINT('',#142217);
#6325=VERTEX_POINT('',#142473);
#6326=VERTEX_POINT('',#142474);
#6327=VERTEX_POINT('',#142476);
#6328=VERTEX_POINT('',#142725);
#6329=VERTEX_POINT('',#142981);
#6330=VERTEX_POINT('',#142982);
#6331=VERTEX_POINT('',#142984);
#6332=VERTEX_POINT('',#143236);
#6333=VERTEX_POINT('',#143477);
#6334=VERTEX_POINT('',#143478);
#6335=VERTEX_POINT('',#143480);
#6336=VERTEX_POINT('',#143738);
#6337=VERTEX_POINT('',#143991);
#6338=VERTEX_POINT('',#143992);
#6339=VERTEX_POINT('',#143994);
#6340=VERTEX_POINT('',#144249);
#6341=VERTEX_POINT('',#144499);
#6342=VERTEX_POINT('',#144500);
#6343=VERTEX_POINT('',#144502);
#6344=VERTEX_POINT('',#144760);
#6345=VERTEX_POINT('',#145013);
#6346=VERTEX_POINT('',#145014);
#6347=VERTEX_POINT('',#145016);
#6348=VERTEX_POINT('',#145271);
#6349=VERTEX_POINT('',#145524);
#6350=VERTEX_POINT('',#145525);
#6351=VERTEX_POINT('',#145527);
#6352=VERTEX_POINT('',#145779);
#6353=VERTEX_POINT('',#146032);
#6354=VERTEX_POINT('',#146033);
#6355=VERTEX_POINT('',#146035);
#6356=VERTEX_POINT('',#146290);
#6357=VERTEX_POINT('',#146546);
#6358=VERTEX_POINT('',#146547);
#6359=VERTEX_POINT('',#146549);
#6360=VERTEX_POINT('',#146801);
#6361=VERTEX_POINT('',#147036);
#6362=VERTEX_POINT('',#147037);
#6363=VERTEX_POINT('',#147039);
#6364=VERTEX_POINT('',#147288);
#6365=VERTEX_POINT('',#147547);
#6366=VERTEX_POINT('',#147548);
#6367=VERTEX_POINT('',#147550);
#6368=VERTEX_POINT('',#147802);
#6369=VERTEX_POINT('',#148058);
#6370=VERTEX_POINT('',#148059);
#6371=VERTEX_POINT('',#148061);
#6372=VERTEX_POINT('',#148310);
#6373=VERTEX_POINT('',#148548);
#6374=VERTEX_POINT('',#148549);
#6375=VERTEX_POINT('',#148551);
#6376=VERTEX_POINT('',#148791);
#6377=VERTEX_POINT('',#149047);
#6378=VERTEX_POINT('',#149048);
#6379=VERTEX_POINT('',#149050);
#6380=VERTEX_POINT('',#149308);
#6381=VERTEX_POINT('',#149564);
#6382=VERTEX_POINT('',#149565);
#6383=VERTEX_POINT('',#149567);
#6384=VERTEX_POINT('',#149801);
#6385=VERTEX_POINT('',#150057);
#6386=VERTEX_POINT('',#150058);
#6387=VERTEX_POINT('',#150060);
#6388=VERTEX_POINT('',#150318);
#6389=VERTEX_POINT('',#150571);
#6390=VERTEX_POINT('',#150572);
#6391=VERTEX_POINT('',#150574);
#6392=VERTEX_POINT('',#150829);
#6393=VERTEX_POINT('',#151082);
#6394=VERTEX_POINT('',#151083);
#6395=VERTEX_POINT('',#151085);
#6396=VERTEX_POINT('',#151325);
#6397=VERTEX_POINT('',#151581);
#6398=VERTEX_POINT('',#151582);
#6399=VERTEX_POINT('',#151584);
#6400=VERTEX_POINT('',#151836);
#6401=VERTEX_POINT('',#152086);
#6402=VERTEX_POINT('',#152087);
#6403=VERTEX_POINT('',#152089);
#6404=VERTEX_POINT('',#152341);
#6405=VERTEX_POINT('',#152594);
#6406=VERTEX_POINT('',#152595);
#6407=VERTEX_POINT('',#152597);
#6408=VERTEX_POINT('',#152849);
#6409=VERTEX_POINT('',#153108);
#6410=VERTEX_POINT('',#153109);
#6411=VERTEX_POINT('',#153111);
#6412=VERTEX_POINT('',#153363);
#6413=VERTEX_POINT('',#153622);
#6414=VERTEX_POINT('',#153623);
#6415=VERTEX_POINT('',#153625);
#6416=VERTEX_POINT('',#153877);
#6417=VERTEX_POINT('',#154136);
#6418=VERTEX_POINT('',#154137);
#6419=VERTEX_POINT('',#154139);
#6420=VERTEX_POINT('',#154388);
#6421=VERTEX_POINT('',#154638);
#6422=VERTEX_POINT('',#154639);
#6423=VERTEX_POINT('',#154641);
#6424=VERTEX_POINT('',#154875);
#6425=VERTEX_POINT('',#155131);
#6426=VERTEX_POINT('',#155132);
#6427=VERTEX_POINT('',#155134);
#6428=VERTEX_POINT('',#155392);
#6429=VERTEX_POINT('',#155642);
#6430=VERTEX_POINT('',#155643);
#6431=VERTEX_POINT('',#155645);
#6432=VERTEX_POINT('',#155903);
#6433=VERTEX_POINT('',#156153);
#6434=VERTEX_POINT('',#156154);
#6435=VERTEX_POINT('',#156156);
#6436=VERTEX_POINT('',#156393);
#6437=VERTEX_POINT('',#156646);
#6438=VERTEX_POINT('',#156647);
#6439=VERTEX_POINT('',#156649);
#6440=VERTEX_POINT('',#156901);
#6441=VERTEX_POINT('',#157151);
#6442=VERTEX_POINT('',#157152);
#6443=VERTEX_POINT('',#157154);
#6444=VERTEX_POINT('',#157409);
#6445=VERTEX_POINT('',#157665);
#6446=VERTEX_POINT('',#157666);
#6447=VERTEX_POINT('',#157668);
#6448=VERTEX_POINT('',#157920);
#6449=VERTEX_POINT('',#158179);
#6450=VERTEX_POINT('',#158180);
#6451=VERTEX_POINT('',#158182);
#6452=VERTEX_POINT('',#158434);
#6453=VERTEX_POINT('',#158690);
#6454=VERTEX_POINT('',#158691);
#6455=VERTEX_POINT('',#158693);
#6456=VERTEX_POINT('',#158945);
#6457=VERTEX_POINT('',#159201);
#6458=VERTEX_POINT('',#159202);
#6459=VERTEX_POINT('',#159204);
#6460=VERTEX_POINT('',#159459);
#6461=VERTEX_POINT('',#159709);
#6462=VERTEX_POINT('',#159710);
#6463=VERTEX_POINT('',#159712);
#6464=VERTEX_POINT('',#159946);
#6465=VERTEX_POINT('',#160202);
#6466=VERTEX_POINT('',#160203);
#6467=VERTEX_POINT('',#160205);
#6468=VERTEX_POINT('',#160460);
#6469=VERTEX_POINT('',#160710);
#6470=VERTEX_POINT('',#160711);
#6471=VERTEX_POINT('',#160713);
#6472=VERTEX_POINT('',#160727);
#6473=VERTEX_POINT('',#160882);
#6474=VERTEX_POINT('',#160884);
#6475=VERTEX_POINT('',#161122);
#6476=VERTEX_POINT('',#161377);
#6477=VERTEX_POINT('',#161630);
#6478=VERTEX_POINT('',#161631);
#6479=VERTEX_POINT('',#161687);
#6480=VERTEX_POINT('',#161689);
#6481=VERTEX_POINT('',#161698);
#6482=VERTEX_POINT('',#161714);
#6483=VERTEX_POINT('',#161971);
#6484=VERTEX_POINT('',#162228);
#6485=VERTEX_POINT('',#162935);
#6486=VERTEX_POINT('',#163468);
#6487=VERTEX_POINT('',#163484);
#6488=VERTEX_POINT('',#163744);
#6489=VERTEX_POINT('',#164001);
#6490=VERTEX_POINT('',#164017);
#6491=VERTEX_POINT('',#164274);
#6492=VERTEX_POINT('',#164534);
#6493=VERTEX_POINT('',#165259);
#6494=VERTEX_POINT('',#165802);
#6495=VERTEX_POINT('',#166395);
#6496=VERTEX_POINT('',#166652);
#6497=VERTEX_POINT('',#166668);
#6498=VERTEX_POINT('',#166925);
#6499=VERTEX_POINT('',#167182);
#6500=VERTEX_POINT('',#167201);
#6501=VERTEX_POINT('',#167214);
#6502=VERTEX_POINT('',#167233);
#6503=VERTEX_POINT('',#167814);
#6504=VERTEX_POINT('',#167833);
#6505=VERTEX_POINT('',#168436);
#6506=VERTEX_POINT('',#168452);
#6507=VERTEX_POINT('',#168709);
#6508=VERTEX_POINT('',#168726);
#6509=VERTEX_POINT('',#168983);
#6510=VERTEX_POINT('',#169002);
#6511=VERTEX_POINT('',#169018);
#6512=VERTEX_POINT('',#169272);
#6513=VERTEX_POINT('',#169291);
#6514=VERTEX_POINT('',#170058);
#6515=VERTEX_POINT('',#170074);
#6516=VERTEX_POINT('',#170089);
#6517=VERTEX_POINT('',#170106);
#6518=VERTEX_POINT('',#170363);
#6519=VERTEX_POINT('',#170898);
#6520=VERTEX_POINT('',#170913);
#6521=VERTEX_POINT('',#170932);
#6522=VERTEX_POINT('',#170988);
#6523=VERTEX_POINT('',#170990);
#6524=VERTEX_POINT('',#170999);
#6525=VERTEX_POINT('',#171015);
#6526=VERTEX_POINT('',#171802);
#6527=VERTEX_POINT('',#172507);
#6528=VERTEX_POINT('',#173050);
#6529=VERTEX_POINT('',#173066);
#6530=VERTEX_POINT('',#173326);
#6531=VERTEX_POINT('',#173583);
#6532=VERTEX_POINT('',#173599);
#6533=VERTEX_POINT('',#173856);
#6534=VERTEX_POINT('',#174116);
#6535=VERTEX_POINT('',#174841);
#6536=VERTEX_POINT('',#175378);
#6537=VERTEX_POINT('',#175947);
#6538=VERTEX_POINT('',#176204);
#6539=VERTEX_POINT('',#176220);
#6540=VERTEX_POINT('',#176477);
#6541=VERTEX_POINT('',#176734);
#6542=VERTEX_POINT('',#176753);
#6543=VERTEX_POINT('',#177013);
#6544=VERTEX_POINT('',#177032);
#6545=VERTEX_POINT('',#177739);
#6546=VERTEX_POINT('',#177758);
#6547=VERTEX_POINT('',#178589);
#6548=VERTEX_POINT('',#178605);
#6549=VERTEX_POINT('',#178862);
#6550=VERTEX_POINT('',#178879);
#6551=VERTEX_POINT('',#179136);
#6552=VERTEX_POINT('',#179155);
#6553=VERTEX_POINT('',#179171);
#6554=VERTEX_POINT('',#179425);
#6555=VERTEX_POINT('',#179444);
#6556=VERTEX_POINT('',#179459);
#6557=VERTEX_POINT('',#179476);
#6558=VERTEX_POINT('',#179492);
#6559=VERTEX_POINT('',#179507);
#6560=VERTEX_POINT('',#179524);
#6561=VERTEX_POINT('',#179781);
#6562=VERTEX_POINT('',#180320);
#6563=VERTEX_POINT('',#180354);
#6564=VERTEX_POINT('',#180356);
#6565=VERTEX_POINT('',#180359);
#6566=VERTEX_POINT('',#180363);
#6567=VERTEX_POINT('',#180364);
#6568=VERTEX_POINT('',#180366);
#6569=VERTEX_POINT('',#180368);
#6570=VERTEX_POINT('',#180372);
#6571=VERTEX_POINT('',#180373);
#6572=VERTEX_POINT('',#180378);
#6573=VERTEX_POINT('',#180379);
#6574=VERTEX_POINT('',#185139);
#6575=VERTEX_POINT('',#185148);
#6576=VERTEX_POINT('',#185151);
#6577=VERTEX_POINT('',#185155);
#6578=VERTEX_POINT('',#185158);
#6579=VERTEX_POINT('',#185162);
#6580=VERTEX_POINT('',#185166);
#6581=VERTEX_POINT('',#185168);
#6582=VERTEX_POINT('',#185172);
#6583=VERTEX_POINT('',#185174);
#6584=VERTEX_POINT('',#185178);
#6585=VERTEX_POINT('',#185179);
#6586=VERTEX_POINT('',#185181);
#6587=VERTEX_POINT('',#185183);
#6588=VERTEX_POINT('',#185186);
#6589=VERTEX_POINT('',#185187);
#6590=VERTEX_POINT('',#185189);
#6591=VERTEX_POINT('',#185191);
#6592=VERTEX_POINT('',#185195);
#6593=VERTEX_POINT('',#185197);
#6594=VERTEX_POINT('',#185201);
#6595=VERTEX_POINT('',#185205);
#6596=VERTEX_POINT('',#185212);
#6597=VERTEX_POINT('',#185213);
#6598=VERTEX_POINT('',#185218);
#6599=VERTEX_POINT('',#185222);
#6600=VERTEX_POINT('',#185230);
#6601=VERTEX_POINT('',#185231);
#6602=VERTEX_POINT('',#185233);
#6603=VERTEX_POINT('',#185235);
#6604=VERTEX_POINT('',#185239);
#6605=VERTEX_POINT('',#185241);
#6606=VERTEX_POINT('',#185245);
#6607=VERTEX_POINT('',#185248);
#6608=VERTEX_POINT('',#185250);
#6609=VERTEX_POINT('',#185252);
#6610=VERTEX_POINT('',#185254);
#6611=VERTEX_POINT('',#185256);
#6612=VERTEX_POINT('',#185259);
#6613=VERTEX_POINT('',#185263);
#6614=VERTEX_POINT('',#185267);
#6615=VERTEX_POINT('',#185271);
#6616=VERTEX_POINT('',#185275);
#6617=VERTEX_POINT('',#185279);
#6618=VERTEX_POINT('',#185287);
#6619=VERTEX_POINT('',#185289);
#6620=VERTEX_POINT('',#185293);
#6621=VERTEX_POINT('',#185295);
#6622=VERTEX_POINT('',#185302);
#6623=VERTEX_POINT('',#185303);
#6624=VERTEX_POINT('',#185305);
#6625=VERTEX_POINT('',#185439);
#6626=VERTEX_POINT('',#185524);
#6627=VERTEX_POINT('',#185525);
#6628=VERTEX_POINT('',#185527);
#6629=VERTEX_POINT('',#185767);
#6630=VERTEX_POINT('',#186023);
#6631=VERTEX_POINT('',#186024);
#6632=VERTEX_POINT('',#186026);
#6633=VERTEX_POINT('',#186272);
#6634=VERTEX_POINT('',#186519);
#6635=VERTEX_POINT('',#186520);
#6636=VERTEX_POINT('',#186522);
#6637=VERTEX_POINT('',#186777);
#6638=VERTEX_POINT('',#187030);
#6639=VERTEX_POINT('',#187031);
#6640=VERTEX_POINT('',#187033);
#6641=VERTEX_POINT('',#187282);
#6642=VERTEX_POINT('',#187538);
#6643=VERTEX_POINT('',#187539);
#6644=VERTEX_POINT('',#187541);
#6645=VERTEX_POINT('',#187790);
#6646=VERTEX_POINT('',#188031);
#6647=VERTEX_POINT('',#188032);
#6648=VERTEX_POINT('',#188034);
#6649=VERTEX_POINT('',#188286);
#6650=VERTEX_POINT('',#188533);
#6651=VERTEX_POINT('',#188534);
#6652=VERTEX_POINT('',#188536);
#6653=VERTEX_POINT('',#188785);
#6654=VERTEX_POINT('',#189026);
#6655=VERTEX_POINT('',#189027);
#6656=VERTEX_POINT('',#189029);
#6657=VERTEX_POINT('',#189281);
#6658=VERTEX_POINT('',#189528);
#6659=VERTEX_POINT('',#189529);
#6660=VERTEX_POINT('',#189531);
#6661=VERTEX_POINT('',#189786);
#6662=VERTEX_POINT('',#190039);
#6663=VERTEX_POINT('',#190040);
#6664=VERTEX_POINT('',#190042);
#6665=VERTEX_POINT('',#190297);
#6666=VERTEX_POINT('',#190550);
#6667=VERTEX_POINT('',#190551);
#6668=VERTEX_POINT('',#190553);
#6669=VERTEX_POINT('',#190790);
#6670=VERTEX_POINT('',#191049);
#6671=VERTEX_POINT('',#191050);
#6672=VERTEX_POINT('',#191052);
#6673=VERTEX_POINT('',#191298);
#6674=VERTEX_POINT('',#191551);
#6675=VERTEX_POINT('',#191552);
#6676=VERTEX_POINT('',#191554);
#6677=VERTEX_POINT('',#191803);
#6678=VERTEX_POINT('',#192056);
#6679=VERTEX_POINT('',#192057);
#6680=VERTEX_POINT('',#192059);
#6681=VERTEX_POINT('',#192308);
#6682=VERTEX_POINT('',#192564);
#6683=VERTEX_POINT('',#192565);
#6684=VERTEX_POINT('',#192567);
#6685=VERTEX_POINT('',#192810);
#6686=VERTEX_POINT('',#193066);
#6687=VERTEX_POINT('',#193067);
#6688=VERTEX_POINT('',#193069);
#6689=VERTEX_POINT('',#193315);
#6690=VERTEX_POINT('',#193556);
#6691=VERTEX_POINT('',#193557);
#6692=VERTEX_POINT('',#193559);
#6693=VERTEX_POINT('',#193808);
#6694=VERTEX_POINT('',#194043);
#6695=VERTEX_POINT('',#194044);
#6696=VERTEX_POINT('',#194046);
#6697=VERTEX_POINT('',#194298);
#6698=VERTEX_POINT('',#194545);
#6699=VERTEX_POINT('',#194546);
#6700=VERTEX_POINT('',#194548);
#6701=VERTEX_POINT('',#194800);
#6702=VERTEX_POINT('',#195053);
#6703=VERTEX_POINT('',#195054);
#6704=VERTEX_POINT('',#195056);
#6705=VERTEX_POINT('',#195311);
#6706=VERTEX_POINT('',#195567);
#6707=VERTEX_POINT('',#195568);
#6708=VERTEX_POINT('',#195570);
#6709=VERTEX_POINT('',#195807);
#6710=VERTEX_POINT('',#196060);
#6711=VERTEX_POINT('',#196061);
#6712=VERTEX_POINT('',#196063);
#6713=VERTEX_POINT('',#196306);
#6714=VERTEX_POINT('',#196556);
#6715=VERTEX_POINT('',#196557);
#6716=VERTEX_POINT('',#196559);
#6717=VERTEX_POINT('',#196808);
#6718=VERTEX_POINT('',#197061);
#6719=VERTEX_POINT('',#197062);
#6720=VERTEX_POINT('',#197064);
#6721=VERTEX_POINT('',#197316);
#6722=VERTEX_POINT('',#197572);
#6723=VERTEX_POINT('',#197573);
#6724=VERTEX_POINT('',#197575);
#6725=VERTEX_POINT('',#197818);
#6726=VERTEX_POINT('',#198071);
#6727=VERTEX_POINT('',#198072);
#6728=VERTEX_POINT('',#198074);
#6729=VERTEX_POINT('',#198317);
#6730=VERTEX_POINT('',#198558);
#6731=VERTEX_POINT('',#198559);
#6732=VERTEX_POINT('',#198561);
#6733=VERTEX_POINT('',#198816);
#6734=VERTEX_POINT('',#199063);
#6735=VERTEX_POINT('',#199064);
#6736=VERTEX_POINT('',#199066);
#6737=VERTEX_POINT('',#199318);
#6738=VERTEX_POINT('',#199574);
#6739=VERTEX_POINT('',#199575);
#6740=VERTEX_POINT('',#199577);
#6741=VERTEX_POINT('',#199832);
#6742=VERTEX_POINT('',#200085);
#6743=VERTEX_POINT('',#200086);
#6744=VERTEX_POINT('',#200088);
#6745=VERTEX_POINT('',#200328);
#6746=VERTEX_POINT('',#200584);
#6747=VERTEX_POINT('',#200585);
#6748=VERTEX_POINT('',#200587);
#6749=VERTEX_POINT('',#200833);
#6750=VERTEX_POINT('',#201083);
#6751=VERTEX_POINT('',#201084);
#6752=VERTEX_POINT('',#201086);
#6753=VERTEX_POINT('',#201326);
#6754=VERTEX_POINT('',#201576);
#6755=VERTEX_POINT('',#201577);
#6756=VERTEX_POINT('',#201579);
#6757=VERTEX_POINT('',#201813);
#6758=VERTEX_POINT('',#202051);
#6759=VERTEX_POINT('',#202052);
#6760=VERTEX_POINT('',#202054);
#6761=VERTEX_POINT('',#202288);
#6762=VERTEX_POINT('',#202535);
#6763=VERTEX_POINT('',#202536);
#6764=VERTEX_POINT('',#202538);
#6765=VERTEX_POINT('',#202772);
#6766=VERTEX_POINT('',#203031);
#6767=VERTEX_POINT('',#203032);
#6768=VERTEX_POINT('',#203034);
#6769=VERTEX_POINT('',#203277);
#6770=VERTEX_POINT('',#203530);
#6771=VERTEX_POINT('',#203531);
#6772=VERTEX_POINT('',#203533);
#6773=VERTEX_POINT('',#203785);
#6774=VERTEX_POINT('',#204035);
#6775=VERTEX_POINT('',#204036);
#6776=VERTEX_POINT('',#204038);
#6777=VERTEX_POINT('',#204290);
#6778=VERTEX_POINT('',#204534);
#6779=VERTEX_POINT('',#204535);
#6780=VERTEX_POINT('',#204537);
#6781=VERTEX_POINT('',#204777);
#6782=VERTEX_POINT('',#205027);
#6783=VERTEX_POINT('',#205028);
#6784=VERTEX_POINT('',#205030);
#6785=VERTEX_POINT('',#205276);
#6786=VERTEX_POINT('',#205517);
#6787=VERTEX_POINT('',#205518);
#6788=VERTEX_POINT('',#205520);
#6789=VERTEX_POINT('',#205772);
#6790=VERTEX_POINT('',#206016);
#6791=VERTEX_POINT('',#206017);
#6792=VERTEX_POINT('',#206019);
#6793=VERTEX_POINT('',#206259);
#6794=VERTEX_POINT('',#206518);
#6795=VERTEX_POINT('',#206519);
#6796=VERTEX_POINT('',#206521);
#6797=VERTEX_POINT('',#206767);
#6798=VERTEX_POINT('',#207020);
#6799=VERTEX_POINT('',#207021);
#6800=VERTEX_POINT('',#207023);
#6801=VERTEX_POINT('',#207263);
#6802=VERTEX_POINT('',#207516);
#6803=VERTEX_POINT('',#207517);
#6804=VERTEX_POINT('',#207519);
#6805=VERTEX_POINT('',#207753);
#6806=VERTEX_POINT('',#208006);
#6807=VERTEX_POINT('',#208007);
#6808=VERTEX_POINT('',#208009);
#6809=VERTEX_POINT('',#208255);
#6810=VERTEX_POINT('',#208508);
#6811=VERTEX_POINT('',#208509);
#6812=VERTEX_POINT('',#208511);
#6813=VERTEX_POINT('',#208763);
#6814=VERTEX_POINT('',#209001);
#6815=VERTEX_POINT('',#209002);
#6816=VERTEX_POINT('',#209004);
#6817=VERTEX_POINT('',#209256);
#6818=VERTEX_POINT('',#209491);
#6819=VERTEX_POINT('',#209492);
#6820=VERTEX_POINT('',#209494);
#6821=VERTEX_POINT('',#209734);
#6822=VERTEX_POINT('',#209981);
#6823=VERTEX_POINT('',#209982);
#6824=VERTEX_POINT('',#209984);
#6825=VERTEX_POINT('',#210230);
#6826=VERTEX_POINT('',#210468);
#6827=VERTEX_POINT('',#210469);
#6828=VERTEX_POINT('',#210471);
#6829=VERTEX_POINT('',#210723);
#6830=VERTEX_POINT('',#210811);
#6831=VERTEX_POINT('',#210812);
#6832=VERTEX_POINT('',#210814);
#6833=VERTEX_POINT('',#211051);
#6834=VERTEX_POINT('',#211228);
#6835=VERTEX_POINT('',#211229);
#6836=VERTEX_POINT('',#211231);
#6837=VERTEX_POINT('',#211480);
#6838=VERTEX_POINT('',#211733);
#6839=VERTEX_POINT('',#211734);
#6840=VERTEX_POINT('',#211736);
#6841=VERTEX_POINT('',#211976);
#6842=VERTEX_POINT('',#212232);
#6843=VERTEX_POINT('',#212233);
#6844=VERTEX_POINT('',#212235);
#6845=VERTEX_POINT('',#212478);
#6846=VERTEX_POINT('',#212731);
#6847=VERTEX_POINT('',#212732);
#6848=VERTEX_POINT('',#212734);
#6849=VERTEX_POINT('',#212986);
#6850=VERTEX_POINT('',#213239);
#6851=VERTEX_POINT('',#213240);
#6852=VERTEX_POINT('',#213242);
#6853=VERTEX_POINT('',#213497);
#6854=VERTEX_POINT('',#213735);
#6855=VERTEX_POINT('',#213736);
#6856=VERTEX_POINT('',#213738);
#6857=VERTEX_POINT('',#213993);
#6858=VERTEX_POINT('',#214228);
#6859=VERTEX_POINT('',#214229);
#6860=VERTEX_POINT('',#214231);
#6861=VERTEX_POINT('',#214471);
#6862=VERTEX_POINT('',#214706);
#6863=VERTEX_POINT('',#214707);
#6864=VERTEX_POINT('',#214709);
#6865=VERTEX_POINT('',#214955);
#6866=VERTEX_POINT('',#215190);
#6867=VERTEX_POINT('',#215191);
#6868=VERTEX_POINT('',#215193);
#6869=VERTEX_POINT('',#215445);
#6870=VERTEX_POINT('',#215692);
#6871=VERTEX_POINT('',#215693);
#6872=VERTEX_POINT('',#215695);
#6873=VERTEX_POINT('',#215944);
#6874=VERTEX_POINT('',#216200);
#6875=VERTEX_POINT('',#216201);
#6876=VERTEX_POINT('',#216203);
#6877=VERTEX_POINT('',#216443);
#6878=VERTEX_POINT('',#216696);
#6879=VERTEX_POINT('',#216697);
#6880=VERTEX_POINT('',#216699);
#6881=VERTEX_POINT('',#216933);
#6882=VERTEX_POINT('',#217177);
#6883=VERTEX_POINT('',#217178);
#6884=VERTEX_POINT('',#217187);
#6885=VERTEX_POINT('',#217189);
#6886=VERTEX_POINT('',#217530);
#6887=VERTEX_POINT('',#217549);
#6888=VERTEX_POINT('',#217562);
#6889=VERTEX_POINT('',#218121);
#6890=VERTEX_POINT('',#218662);
#6891=VERTEX_POINT('',#219193);
#6892=VERTEX_POINT('',#219453);
#6893=VERTEX_POINT('',#219467);
#6894=VERTEX_POINT('',#219486);
#6895=VERTEX_POINT('',#219749);
#6896=VERTEX_POINT('',#219763);
#6897=VERTEX_POINT('',#220020);
#6898=VERTEX_POINT('',#220559);
#6899=VERTEX_POINT('',#220573);
#6900=VERTEX_POINT('',#220836);
#6901=VERTEX_POINT('',#220849);
#6902=VERTEX_POINT('',#221390);
#6903=VERTEX_POINT('',#222005);
#6904=VERTEX_POINT('',#222019);
#6905=VERTEX_POINT('',#222038);
#6906=VERTEX_POINT('',#222052);
#6907=VERTEX_POINT('',#222315);
#6908=VERTEX_POINT('',#222329);
#6909=VERTEX_POINT('',#222592);
#6910=VERTEX_POINT('',#223135);
#6911=VERTEX_POINT('',#223154);
#6912=VERTEX_POINT('',#223665);
#6913=VERTEX_POINT('',#223684);
#6914=VERTEX_POINT('',#224223);
#6915=VERTEX_POINT('',#224483);
#6916=VERTEX_POINT('',#225018);
#6917=VERTEX_POINT('',#225031);
#6918=VERTEX_POINT('',#225560);
#6919=VERTEX_POINT('',#226085);
#6920=VERTEX_POINT('',#226620);
#6921=VERTEX_POINT('',#226880);
#6922=VERTEX_POINT('',#226899);
#6923=VERTEX_POINT('',#226913);
#6924=VERTEX_POINT('',#226928);
#6925=VERTEX_POINT('',#227453);
#6926=VERTEX_POINT('',#227472);
#6927=VERTEX_POINT('',#227735);
#6928=VERTEX_POINT('',#227749);
#6929=VERTEX_POINT('',#228012);
#6930=VERTEX_POINT('',#228026);
#6931=VERTEX_POINT('',#228045);
#6932=VERTEX_POINT('',#228578);
#6933=VERTEX_POINT('',#228591);
#6934=VERTEX_POINT('',#229072);
#6935=VERTEX_POINT('',#229074);
#6936=VERTEX_POINT('',#229247);
#6937=VERTEX_POINT('',#229266);
#6938=VERTEX_POINT('',#229791);
#6939=VERTEX_POINT('',#230051);
#6940=VERTEX_POINT('',#230588);
#6941=VERTEX_POINT('',#231103);
#6942=VERTEX_POINT('',#231360);
#6943=VERTEX_POINT('',#231871);
#6944=VERTEX_POINT('',#232436);
#6945=VERTEX_POINT('',#232696);
#6946=VERTEX_POINT('',#233199);
#6947=VERTEX_POINT('',#233730);
#6948=VERTEX_POINT('',#234271);
#6949=VERTEX_POINT('',#234878);
#6950=VERTEX_POINT('',#235135);
#6951=VERTEX_POINT('',#235150);
#6952=VERTEX_POINT('',#235169);
#6953=VERTEX_POINT('',#235188);
#6954=VERTEX_POINT('',#235207);
#6955=VERTEX_POINT('',#235226);
#6956=VERTEX_POINT('',#235755);
#6957=VERTEX_POINT('',#235769);
#6958=VERTEX_POINT('',#235788);
#6959=VERTEX_POINT('',#235802);
#6960=VERTEX_POINT('',#236315);
#6961=VERTEX_POINT('',#236852);
#6962=VERTEX_POINT('',#236865);
#6963=VERTEX_POINT('',#236884);
#6964=VERTEX_POINT('',#237147);
#6965=VERTEX_POINT('',#237162);
#6966=VERTEX_POINT('',#237176);
#6967=VERTEX_POINT('',#237705);
#6968=VERTEX_POINT('',#238228);
#6969=VERTEX_POINT('',#238241);
#6970=VERTEX_POINT('',#238774);
#6971=VERTEX_POINT('',#239037);
#6972=VERTEX_POINT('',#239570);
#6973=VERTEX_POINT('',#239830);
#6974=VERTEX_POINT('',#239844);
#6975=VERTEX_POINT('',#240381);
#6976=VERTEX_POINT('',#240400);
#6977=VERTEX_POINT('',#240935);
#6978=VERTEX_POINT('',#240954);
#6979=VERTEX_POINT('',#240968);
#6980=VERTEX_POINT('',#241225);
#6981=VERTEX_POINT('',#241499);
#6982=VERTEX_POINT('',#241576);
#6983=VERTEX_POINT('',#241665);
#6984=VERTEX_POINT('',#241667);
#6985=VERTEX_POINT('',#241782);
#6986=VERTEX_POINT('',#241783);
#6987=VERTEX_POINT('',#241794);
#6988=VERTEX_POINT('',#241823);
#6989=VERTEX_POINT('',#241825);
#6990=VERTEX_POINT('',#241836);
#6991=VERTEX_POINT('',#247024);
#6992=VERTEX_POINT('',#247026);
#6993=VERTEX_POINT('',#247029);
#6994=VERTEX_POINT('',#247034);
#6995=VERTEX_POINT('',#247041);
#6996=VERTEX_POINT('',#247042);
#6997=VERTEX_POINT('',#247053);
#6998=VERTEX_POINT('',#247082);
#6999=VERTEX_POINT('',#247119);
#7000=VERTEX_POINT('',#247120);
#7001=VERTEX_POINT('',#247131);
#7002=VERTEX_POINT('',#247160);
#7003=VERTEX_POINT('',#247162);
#7004=VERTEX_POINT('',#247173);
#7005=VERTEX_POINT('',#247203);
#7006=VERTEX_POINT('',#247205);
#7007=VERTEX_POINT('',#247209);
#7008=VERTEX_POINT('',#247211);
#7009=VERTEX_POINT('',#247215);
#7010=VERTEX_POINT('',#247217);
#7011=VERTEX_POINT('',#247221);
#7012=VERTEX_POINT('',#247223);
#7013=VERTEX_POINT('',#247227);
#7014=VERTEX_POINT('',#247229);
#7015=VERTEX_POINT('',#247233);
#7016=VERTEX_POINT('',#247235);
#7017=VERTEX_POINT('',#247239);
#7018=VERTEX_POINT('',#247242);
#7019=VERTEX_POINT('',#247246);
#7020=VERTEX_POINT('',#247249);
#7021=VERTEX_POINT('',#247254);
#7022=VERTEX_POINT('',#247256);
#7023=VERTEX_POINT('',#247263);
#7024=VERTEX_POINT('',#247265);
#7025=VERTEX_POINT('',#247269);
#7026=VERTEX_POINT('',#247272);
#7027=VERTEX_POINT('',#247275);
#7028=VERTEX_POINT('',#247279);
#7029=VERTEX_POINT('',#247281);
#7030=VERTEX_POINT('',#247284);
#7031=VERTEX_POINT('',#247293);
#7032=VERTEX_POINT('',#247295);
#7033=VERTEX_POINT('',#247299);
#7034=VERTEX_POINT('',#247301);
#7035=VERTEX_POINT('',#247308);
#7036=VERTEX_POINT('',#247309);
#7037=VERTEX_POINT('',#247311);
#7038=VERTEX_POINT('',#247313);
#7039=VERTEX_POINT('',#247317);
#7040=VERTEX_POINT('',#247318);
#7041=VERTEX_POINT('',#247320);
#7042=VERTEX_POINT('',#247322);
#7043=VERTEX_POINT('',#247335);
#7044=VERTEX_POINT('',#247337);
#7045=VERTEX_POINT('',#247341);
#7046=VERTEX_POINT('',#247343);
#7047=VERTEX_POINT('',#247350);
#7048=VERTEX_POINT('',#247351);
#7049=VERTEX_POINT('',#247353);
#7050=VERTEX_POINT('',#247355);
#7051=VERTEX_POINT('',#247630);
#7052=VERTEX_POINT('',#247632);
#7053=VERTEX_POINT('',#247635);
#7054=VERTEX_POINT('',#247687);
#7055=VERTEX_POINT('',#247688);
#7056=VERTEX_POINT('',#247690);
#7057=VERTEX_POINT('',#247869);
#7058=VERTEX_POINT('',#248008);
#7059=VERTEX_POINT('',#248009);
#7060=VERTEX_POINT('',#248428);
#7061=VERTEX_POINT('',#248429);
#7062=VERTEX_POINT('',#248431);
#7063=VERTEX_POINT('',#248861);
#7064=VERTEX_POINT('',#248862);
#7065=VERTEX_POINT('',#249134);
#7066=VERTEX_POINT('',#249358);
#7067=VERTEX_POINT('',#249359);
#7068=VERTEX_POINT('',#249577);
#7069=VERTEX_POINT('',#249793);
#7070=VERTEX_POINT('',#249794);
#7071=VERTEX_POINT('',#249796);
#7072=VERTEX_POINT('',#250222);
#7073=VERTEX_POINT('',#250223);
#7074=VERTEX_POINT('',#250225);
#7075=VERTEX_POINT('',#250438);
#7076=VERTEX_POINT('',#250652);
#7077=VERTEX_POINT('',#250653);
#7078=VERTEX_POINT('',#251092);
#7079=VERTEX_POINT('',#251093);
#7080=VERTEX_POINT('',#251556);
#7081=VERTEX_POINT('',#251557);
#7082=VERTEX_POINT('',#251559);
#7083=VERTEX_POINT('',#251776);
#7084=VERTEX_POINT('',#251996);
#7085=VERTEX_POINT('',#251997);
#7086=VERTEX_POINT('',#252209);
#7087=VERTEX_POINT('',#252423);
#7088=VERTEX_POINT('',#252424);
#7089=VERTEX_POINT('',#252426);
#7090=VERTEX_POINT('',#252856);
#7091=VERTEX_POINT('',#252857);
#7092=VERTEX_POINT('',#252859);
#7093=VERTEX_POINT('',#253363);
#7094=VERTEX_POINT('',#253364);
#7095=VERTEX_POINT('',#253572);
#7096=VERTEX_POINT('',#253786);
#7097=VERTEX_POINT('',#253787);
#7098=VERTEX_POINT('',#254216);
#7099=VERTEX_POINT('',#254629);
#7100=VERTEX_POINT('',#254630);
#7101=VERTEX_POINT('',#254637);
#7102=VERTEX_POINT('',#254639);
#7103=VERTEX_POINT('',#254645);
#7104=VERTEX_POINT('',#254875);
#7105=VERTEX_POINT('',#255105);
#7106=VERTEX_POINT('',#255335);
#7107=VERTEX_POINT('',#255562);
#7108=VERTEX_POINT('',#255789);
#7109=VERTEX_POINT('',#256019);
#7110=VERTEX_POINT('',#256246);
#7111=VERTEX_POINT('',#256476);
#7112=VERTEX_POINT('',#256703);
#7113=VERTEX_POINT('',#256933);
#7114=VERTEX_POINT('',#257163);
#7115=VERTEX_POINT('',#257393);
#7116=VERTEX_POINT('',#257620);
#7117=VERTEX_POINT('',#257847);
#7118=VERTEX_POINT('',#258090);
#7119=VERTEX_POINT('',#258092);
#7120=VERTEX_POINT('',#258304);
#7121=VERTEX_POINT('',#258315);
#7122=VERTEX_POINT('',#258327);
#7123=VERTEX_POINT('',#258338);
#7124=VERTEX_POINT('',#258568);
#7125=VERTEX_POINT('',#258795);
#7126=VERTEX_POINT('',#259022);
#7127=VERTEX_POINT('',#259252);
#7128=VERTEX_POINT('',#259479);
#7129=VERTEX_POINT('',#259491);
#7130=VERTEX_POINT('',#259502);
#7131=VERTEX_POINT('',#259513);
#7132=VERTEX_POINT('',#259525);
#7133=VERTEX_POINT('',#260628);
#7134=VERTEX_POINT('',#260629);
#7135=VERTEX_POINT('',#260631);
#7136=VERTEX_POINT('',#260633);
#7137=VERTEX_POINT('',#260637);
#7138=VERTEX_POINT('',#260639);
#7139=VERTEX_POINT('',#260643);
#7140=VERTEX_POINT('',#260645);
#7141=VERTEX_POINT('',#260649);
#7142=VERTEX_POINT('',#260651);
#7143=VERTEX_POINT('',#260655);
#7144=VERTEX_POINT('',#260657);
#7145=VERTEX_POINT('',#260665);
#7146=VERTEX_POINT('',#260668);
#7147=VERTEX_POINT('',#260675);
#7148=VERTEX_POINT('',#260676);
#7149=VERTEX_POINT('',#260678);
#7150=VERTEX_POINT('',#260680);
#7151=VERTEX_POINT('',#260919);
#7152=VERTEX_POINT('',#260921);
#7153=VERTEX_POINT('',#260924);
#7154=VERTEX_POINT('',#260961);
#7155=VERTEX_POINT('',#260962);
#7156=VERTEX_POINT('',#260964);
#7157=VERTEX_POINT('',#261038);
#7158=VERTEX_POINT('',#261081);
#7159=VERTEX_POINT('',#261082);
#7160=VERTEX_POINT('',#261084);
#7161=VERTEX_POINT('',#261285);
#7162=VERTEX_POINT('',#261483);
#7163=VERTEX_POINT('',#261484);
#7164=VERTEX_POINT('',#261917);
#7165=VERTEX_POINT('',#261918);
#7166=VERTEX_POINT('',#261920);
#7167=VERTEX_POINT('',#262147);
#7168=VERTEX_POINT('',#262375);
#7169=VERTEX_POINT('',#262376);
#7170=VERTEX_POINT('',#262801);
#7171=VERTEX_POINT('',#262802);
#7172=VERTEX_POINT('',#262804);
#7173=VERTEX_POINT('',#263063);
#7174=VERTEX_POINT('',#263313);
#7175=VERTEX_POINT('',#263314);
#7176=VERTEX_POINT('',#263735);
#7177=VERTEX_POINT('',#263736);
#7178=VERTEX_POINT('',#263738);
#7179=VERTEX_POINT('',#263971);
#7180=VERTEX_POINT('',#264071);
#7181=VERTEX_POINT('',#264072);
#7182=VERTEX_POINT('',#264292);
#7183=VERTEX_POINT('',#264423);
#7184=VERTEX_POINT('',#264424);
#7185=VERTEX_POINT('',#264426);
#7186=VERTEX_POINT('',#264742);
#7187=VERTEX_POINT('',#264743);
#7188=VERTEX_POINT('',#264745);
#7189=VERTEX_POINT('',#264879);
#7190=VERTEX_POINT('',#265105);
#7191=VERTEX_POINT('',#265106);
#7192=VERTEX_POINT('',#265533);
#7193=VERTEX_POINT('',#265534);
#7194=VERTEX_POINT('',#265536);
#7195=VERTEX_POINT('',#265655);
#7196=VERTEX_POINT('',#265875);
#7197=VERTEX_POINT('',#265876);
#7198=VERTEX_POINT('',#265878);
#7199=VERTEX_POINT('',#266238);
#7200=VERTEX_POINT('',#266239);
#7201=VERTEX_POINT('',#266447);
#7202=VERTEX_POINT('',#266673);
#7203=VERTEX_POINT('',#266674);
#7204=VERTEX_POINT('',#266676);
#7205=VERTEX_POINT('',#267130);
#7206=VERTEX_POINT('',#267131);
#7207=VERTEX_POINT('',#267349);
#7208=VERTEX_POINT('',#267559);
#7209=VERTEX_POINT('',#267560);
#7210=VERTEX_POINT('',#267562);
#7211=VERTEX_POINT('',#267797);
#7212=VERTEX_POINT('',#267886);
#7213=VERTEX_POINT('',#267887);
#7214=VERTEX_POINT('',#268115);
#7215=VERTEX_POINT('',#268250);
#7216=VERTEX_POINT('',#268251);
#7217=VERTEX_POINT('',#268253);
#7218=VERTEX_POINT('',#268693);
#7219=VERTEX_POINT('',#268694);
#7220=VERTEX_POINT('',#268922);
#7221=VERTEX_POINT('',#269144);
#7222=VERTEX_POINT('',#269145);
#7223=VERTEX_POINT('',#269147);
#7224=VERTEX_POINT('',#269593);
#7225=VERTEX_POINT('',#269594);
#7226=VERTEX_POINT('',#269818);
#7227=VERTEX_POINT('',#270056);
#7228=VERTEX_POINT('',#270057);
#7229=VERTEX_POINT('',#270059);
#7230=VERTEX_POINT('',#270493);
#7231=VERTEX_POINT('',#270494);
#7232=VERTEX_POINT('',#270708);
#7233=VERTEX_POINT('',#270942);
#7234=VERTEX_POINT('',#270943);
#7235=VERTEX_POINT('',#270945);
#7236=VERTEX_POINT('',#271393);
#7237=VERTEX_POINT('',#271394);
#7238=VERTEX_POINT('',#271602);
#7239=VERTEX_POINT('',#271812);
#7240=VERTEX_POINT('',#271813);
#7241=VERTEX_POINT('',#271815);
#7242=VERTEX_POINT('',#272106);
#7243=VERTEX_POINT('',#272284);
#7244=VERTEX_POINT('',#272285);
#7245=VERTEX_POINT('',#272347);
#7246=VERTEX_POINT('',#272349);
#7247=VERTEX_POINT('',#272384);
#7248=VERTEX_POINT('',#272575);
#7249=VERTEX_POINT('',#272586);
#7250=VERTEX_POINT('',#272598);
#7251=VERTEX_POINT('',#272789);
#7252=VERTEX_POINT('',#272800);
#7253=VERTEX_POINT('',#272811);
#7254=VERTEX_POINT('',#273002);
#7255=VERTEX_POINT('',#273013);
#7256=VERTEX_POINT('',#273024);
#7257=VERTEX_POINT('',#273215);
#7258=VERTEX_POINT('',#273226);
#7259=VERTEX_POINT('',#273237);
#7260=VERTEX_POINT('',#273428);
#7261=VERTEX_POINT('',#273441);
#7262=VERTEX_POINT('',#273632);
#7263=VERTEX_POINT('',#273823);
#7264=VERTEX_POINT('',#273835);
#7265=VERTEX_POINT('',#274026);
#7266=VERTEX_POINT('',#274037);
#7267=VERTEX_POINT('',#274049);
#7268=VERTEX_POINT('',#274237);
#7269=VERTEX_POINT('',#274428);
#7270=VERTEX_POINT('',#274439);
#7271=VERTEX_POINT('',#274630);
#7272=VERTEX_POINT('',#274641);
#7273=VERTEX_POINT('',#274652);
#7274=VERTEX_POINT('',#274665);
#7275=VERTEX_POINT('',#274667);
#7276=VERTEX_POINT('',#274837);
#7277=VERTEX_POINT('',#274848);
#7278=VERTEX_POINT('',#274859);
#7279=VERTEX_POINT('',#275050);
#7280=VERTEX_POINT('',#275244);
#7281=VERTEX_POINT('',#275255);
#7282=VERTEX_POINT('',#275446);
#7283=VERTEX_POINT('',#275637);
#7284=VERTEX_POINT('',#275648);
#7285=VERTEX_POINT('',#275659);
#7286=VERTEX_POINT('',#275850);
#7287=VERTEX_POINT('',#275861);
#7288=VERTEX_POINT('',#275872);
#7289=VERTEX_POINT('',#276063);
#7290=VERTEX_POINT('',#276257);
#7291=VERTEX_POINT('',#276268);
#7292=VERTEX_POINT('',#276459);
#7293=VERTEX_POINT('',#276650);
#7294=VERTEX_POINT('',#276661);
#7295=VERTEX_POINT('',#276672);
#7296=VERTEX_POINT('',#276863);
#7297=VERTEX_POINT('',#276874);
#7298=VERTEX_POINT('',#276885);
#7299=VERTEX_POINT('',#277076);
#7300=VERTEX_POINT('',#277270);
#7301=VERTEX_POINT('',#277292);
#7302=VERTEX_POINT('',#279084);
#7303=VERTEX_POINT('',#279085);
#7304=VERTEX_POINT('',#279087);
#7305=VERTEX_POINT('',#279089);
#7306=VERTEX_POINT('',#279093);
#7307=VERTEX_POINT('',#279095);
#7308=VERTEX_POINT('',#279099);
#7309=VERTEX_POINT('',#279101);
#7310=VERTEX_POINT('',#279105);
#7311=VERTEX_POINT('',#279107);
#7312=VERTEX_POINT('',#279111);
#7313=VERTEX_POINT('',#279113);
#7314=VERTEX_POINT('',#279121);
#7315=VERTEX_POINT('',#279124);
#7316=VERTEX_POINT('',#279131);
#7317=VERTEX_POINT('',#279132);
#7318=VERTEX_POINT('',#279194);
#7319=VERTEX_POINT('',#279196);
#7320=VERTEX_POINT('',#279231);
#7321=VERTEX_POINT('',#279422);
#7322=VERTEX_POINT('',#279433);
#7323=VERTEX_POINT('',#279627);
#7324=VERTEX_POINT('',#279818);
#7325=VERTEX_POINT('',#279829);
#7326=VERTEX_POINT('',#280020);
#7327=VERTEX_POINT('',#280032);
#7328=VERTEX_POINT('',#280043);
#7329=VERTEX_POINT('',#280234);
#7330=VERTEX_POINT('',#280246);
#7331=VERTEX_POINT('',#280257);
#7332=VERTEX_POINT('',#280448);
#7333=VERTEX_POINT('',#280459);
#7334=VERTEX_POINT('',#280650);
#7335=VERTEX_POINT('',#280661);
#7336=VERTEX_POINT('',#280670);
#7337=VERTEX_POINT('',#280672);
#7338=VERTEX_POINT('',#280761);
#7339=VERTEX_POINT('',#280772);
#7340=VERTEX_POINT('',#280963);
#7341=VERTEX_POINT('',#281157);
#7342=VERTEX_POINT('',#281168);
#7343=VERTEX_POINT('',#281359);
#7344=VERTEX_POINT('',#281550);
#7345=VERTEX_POINT('',#281561);
#7346=VERTEX_POINT('',#281572);
#7347=VERTEX_POINT('',#281763);
#7348=VERTEX_POINT('',#281774);
#7349=VERTEX_POINT('',#281785);
#7350=VERTEX_POINT('',#281976);
#7351=VERTEX_POINT('',#282170);
#7352=VERTEX_POINT('',#282192);
#7353=VERTEX_POINT('',#282193);
#7354=VERTEX_POINT('',#282315);
#7355=VERTEX_POINT('',#282317);
#7356=VERTEX_POINT('',#282403);
#7357=VERTEX_POINT('',#282860);
#7358=VERTEX_POINT('',#283271);
#7359=VERTEX_POINT('',#283282);
#7360=VERTEX_POINT('',#283681);
#7361=VERTEX_POINT('',#283692);
#7362=VERTEX_POINT('',#284105);
#7363=VERTEX_POINT('',#284116);
#7364=VERTEX_POINT('',#284517);
#7365=VERTEX_POINT('',#284922);
#7366=VERTEX_POINT('',#285071);
#7367=VERTEX_POINT('',#285073);
#7368=VERTEX_POINT('',#285186);
#7369=VERTEX_POINT('',#285577);
#7370=VERTEX_POINT('',#286000);
#7371=VERTEX_POINT('',#286399);
#7372=VERTEX_POINT('',#286411);
#7373=VERTEX_POINT('',#286870);
#7374=VERTEX_POINT('',#287275);
#7375=VERTEX_POINT('',#288061);
#7376=VERTEX_POINT('',#288145);
#7377=VERTEX_POINT('',#288252);
#7378=VERTEX_POINT('',#289280);
#7379=VERTEX_POINT('',#289281);
#7380=VERTEX_POINT('',#289283);
#7381=VERTEX_POINT('',#289285);
#7382=VERTEX_POINT('',#289289);
#7383=VERTEX_POINT('',#289291);
#7384=VERTEX_POINT('',#289295);
#7385=VERTEX_POINT('',#289297);
#7386=VERTEX_POINT('',#289301);
#7387=VERTEX_POINT('',#289303);
#7388=VERTEX_POINT('',#289307);
#7389=VERTEX_POINT('',#289309);
#7390=VERTEX_POINT('',#289317);
#7391=VERTEX_POINT('',#289320);
#7392=EDGE_CURVE('',#5215,#5216,#3941,.T.);
#7393=EDGE_CURVE('',#5216,#5217,#1989,.T.);
#7394=EDGE_CURVE('',#5217,#5218,#1990,.T.);
#7395=EDGE_CURVE('',#5219,#5218,#1809,.T.);
#7396=EDGE_CURVE('',#5220,#5219,#1991,.T.);
#7397=EDGE_CURVE('',#5215,#5220,#1992,.T.);
#7398=EDGE_CURVE('',#5221,#5222,#3942,.T.);
#7399=EDGE_CURVE('',#5222,#5223,#1993,.T.);
#7400=EDGE_CURVE('',#5223,#5216,#1994,.T.);
#7401=EDGE_CURVE('',#5224,#5215,#1995,.T.);
#7402=EDGE_CURVE('',#5221,#5224,#1996,.T.);
#7403=EDGE_CURVE('',#5225,#5226,#3943,.T.);
#7404=EDGE_CURVE('',#5226,#5227,#1997,.T.);
#7405=EDGE_CURVE('',#5227,#5222,#1998,.T.);
#7406=EDGE_CURVE('',#5228,#5221,#1999,.T.);
#7407=EDGE_CURVE('',#5225,#5228,#2000,.T.);
#7408=EDGE_CURVE('',#5229,#5230,#3944,.T.);
#7409=EDGE_CURVE('',#5230,#5231,#2001,.T.);
#7410=EDGE_CURVE('',#5231,#5226,#2002,.T.);
#7411=EDGE_CURVE('',#5232,#5225,#2003,.T.);
#7412=EDGE_CURVE('',#5229,#5232,#2004,.T.);
#7413=EDGE_CURVE('',#5233,#5234,#3945,.T.);
#7414=EDGE_CURVE('',#5234,#5235,#2005,.T.);
#7415=EDGE_CURVE('',#5235,#5230,#2006,.T.);
#7416=EDGE_CURVE('',#5236,#5229,#2007,.T.);
#7417=EDGE_CURVE('',#5233,#5236,#2008,.T.);
#7418=EDGE_CURVE('',#5237,#5238,#3946,.T.);
#7419=EDGE_CURVE('',#5238,#5239,#2009,.T.);
#7420=EDGE_CURVE('',#5239,#5234,#2010,.T.);
#7421=EDGE_CURVE('',#5240,#5233,#2011,.T.);
#7422=EDGE_CURVE('',#5237,#5240,#2012,.T.);
#7423=EDGE_CURVE('',#5241,#5242,#3947,.T.);
#7424=EDGE_CURVE('',#5242,#5243,#2013,.T.);
#7425=EDGE_CURVE('',#5243,#5238,#2014,.T.);
#7426=EDGE_CURVE('',#5244,#5237,#2015,.T.);
#7427=EDGE_CURVE('',#5241,#5244,#2016,.T.);
#7428=EDGE_CURVE('',#5245,#5246,#3948,.T.);
#7429=EDGE_CURVE('',#5246,#5247,#2017,.T.);
#7430=EDGE_CURVE('',#5247,#5242,#2018,.T.);
#7431=EDGE_CURVE('',#5248,#5241,#2019,.T.);
#7432=EDGE_CURVE('',#5245,#5248,#2020,.T.);
#7433=EDGE_CURVE('',#5249,#5250,#3949,.T.);
#7434=EDGE_CURVE('',#5250,#5251,#2021,.T.);
#7435=EDGE_CURVE('',#5251,#5246,#2022,.T.);
#7436=EDGE_CURVE('',#5252,#5245,#2023,.T.);
#7437=EDGE_CURVE('',#5249,#5252,#2024,.T.);
#7438=EDGE_CURVE('',#5253,#5254,#3950,.T.);
#7439=EDGE_CURVE('',#5255,#5253,#2025,.T.);
#7440=EDGE_CURVE('',#5256,#5255,#2026,.T.);
#7441=EDGE_CURVE('',#5257,#5256,#1810,.T.);
#7442=EDGE_CURVE('',#5257,#5258,#2027,.T.);
#7443=EDGE_CURVE('',#5258,#5254,#2028,.T.);
#7444=EDGE_CURVE('',#5259,#5260,#3951,.T.);
#7445=EDGE_CURVE('',#5260,#5261,#2029,.T.);
#7446=EDGE_CURVE('',#5261,#5262,#1811,.T.);
#7447=EDGE_CURVE('',#5262,#5263,#3952,.T.);
#7448=EDGE_CURVE('',#5263,#5263,#1812,.F.);
#7449=EDGE_CURVE('',#5262,#5264,#1813,.T.);
#7450=EDGE_CURVE('',#5264,#5259,#2030,.T.);
#7451=EDGE_CURVE('',#5265,#5266,#3953,.T.);
#7452=EDGE_CURVE('',#5266,#5267,#2031,.T.);
#7453=EDGE_CURVE('',#5267,#5260,#2032,.T.);
#7454=EDGE_CURVE('',#5259,#5265,#2033,.T.);
#7455=EDGE_CURVE('',#5268,#5269,#3954,.T.);
#7456=EDGE_CURVE('',#5269,#5266,#2034,.T.);
#7457=EDGE_CURVE('',#5265,#5270,#2035,.T.);
#7458=EDGE_CURVE('',#5270,#5268,#2036,.T.);
#7459=EDGE_CURVE('',#5271,#5272,#3955,.T.);
#7460=EDGE_CURVE('',#5272,#5273,#2037,.T.);
#7461=EDGE_CURVE('',#5273,#5269,#2038,.T.);
#7462=EDGE_CURVE('',#5268,#5271,#2039,.T.);
#7463=EDGE_CURVE('',#5274,#5275,#3956,.T.);
#7464=EDGE_CURVE('',#5275,#5272,#2040,.T.);
#7465=EDGE_CURVE('',#5271,#5276,#2041,.T.);
#7466=EDGE_CURVE('',#5276,#5274,#2042,.T.);
#7467=EDGE_CURVE('',#5277,#5278,#3957,.T.);
#7468=EDGE_CURVE('',#5278,#5279,#2043,.T.);
#7469=EDGE_CURVE('',#5279,#5275,#2044,.T.);
#7470=EDGE_CURVE('',#5274,#5277,#2045,.T.);
#7471=EDGE_CURVE('',#5280,#5281,#3958,.T.);
#7472=EDGE_CURVE('',#5281,#5278,#2046,.T.);
#7473=EDGE_CURVE('',#5277,#5282,#2047,.T.);
#7474=EDGE_CURVE('',#5282,#5280,#2048,.T.);
#7475=EDGE_CURVE('',#5283,#5284,#3959,.T.);
#7476=EDGE_CURVE('',#5284,#5285,#2049,.T.);
#7477=EDGE_CURVE('',#5285,#5281,#2050,.T.);
#7478=EDGE_CURVE('',#5280,#5283,#2051,.T.);
#7479=EDGE_CURVE('',#5286,#5287,#3960,.T.);
#7480=EDGE_CURVE('',#5287,#5284,#2052,.T.);
#7481=EDGE_CURVE('',#5283,#5288,#2053,.T.);
#7482=EDGE_CURVE('',#5288,#5286,#2054,.T.);
#7483=EDGE_CURVE('',#5289,#5290,#3961,.T.);
#7484=EDGE_CURVE('',#5289,#5291,#2055,.F.);
#7485=EDGE_CURVE('',#5292,#5291,#1814,.T.);
#7486=EDGE_CURVE('',#5292,#5290,#2056,.T.);
#7487=EDGE_CURVE('',#5293,#5294,#3962,.T.);
#7488=EDGE_CURVE('',#5294,#5295,#2057,.T.);
#7489=EDGE_CURVE('',#5295,#5296,#2058,.T.);
#7490=EDGE_CURVE('',#5297,#5296,#1815,.T.);
#7491=EDGE_CURVE('',#5298,#5297,#2059,.T.);
#7492=EDGE_CURVE('',#5293,#5298,#2060,.T.);
#7493=EDGE_CURVE('',#5299,#5300,#3963,.T.);
#7494=EDGE_CURVE('',#5300,#5301,#2061,.T.);
#7495=EDGE_CURVE('',#5301,#5294,#2062,.T.);
#7496=EDGE_CURVE('',#5302,#5293,#2063,.T.);
#7497=EDGE_CURVE('',#5299,#5302,#2064,.T.);
#7498=EDGE_CURVE('',#5303,#5304,#3964,.T.);
#7499=EDGE_CURVE('',#5304,#5305,#2065,.T.);
#7500=EDGE_CURVE('',#5305,#5300,#2066,.T.);
#7501=EDGE_CURVE('',#5306,#5299,#2067,.T.);
#7502=EDGE_CURVE('',#5303,#5306,#2068,.T.);
#7503=EDGE_CURVE('',#5307,#5308,#3965,.T.);
#7504=EDGE_CURVE('',#5308,#5309,#2069,.T.);
#7505=EDGE_CURVE('',#5309,#5304,#2070,.T.);
#7506=EDGE_CURVE('',#5310,#5303,#2071,.T.);
#7507=EDGE_CURVE('',#5307,#5310,#2072,.T.);
#7508=EDGE_CURVE('',#5311,#5312,#3966,.T.);
#7509=EDGE_CURVE('',#5312,#5313,#2073,.T.);
#7510=EDGE_CURVE('',#5313,#5308,#2074,.T.);
#7511=EDGE_CURVE('',#5314,#5307,#2075,.T.);
#7512=EDGE_CURVE('',#5311,#5314,#2076,.T.);
#7513=EDGE_CURVE('',#5315,#5316,#3967,.T.);
#7514=EDGE_CURVE('',#5316,#5317,#2077,.T.);
#7515=EDGE_CURVE('',#5317,#5312,#2078,.T.);
#7516=EDGE_CURVE('',#5318,#5311,#2079,.T.);
#7517=EDGE_CURVE('',#5315,#5318,#2080,.T.);
#7518=EDGE_CURVE('',#5319,#5320,#3968,.T.);
#7519=EDGE_CURVE('',#5320,#5321,#2081,.T.);
#7520=EDGE_CURVE('',#5321,#5316,#2082,.T.);
#7521=EDGE_CURVE('',#5322,#5315,#2083,.T.);
#7522=EDGE_CURVE('',#5319,#5322,#2084,.T.);
#7523=EDGE_CURVE('',#5323,#5324,#3969,.T.);
#7524=EDGE_CURVE('',#5324,#5325,#2085,.T.);
#7525=EDGE_CURVE('',#5325,#5320,#2086,.T.);
#7526=EDGE_CURVE('',#5326,#5319,#2087,.T.);
#7527=EDGE_CURVE('',#5323,#5326,#2088,.T.);
#7528=EDGE_CURVE('',#5327,#5328,#3970,.T.);
#7529=EDGE_CURVE('',#5328,#5329,#2089,.T.);
#7530=EDGE_CURVE('',#5329,#5324,#2090,.T.);
#7531=EDGE_CURVE('',#5330,#5323,#2091,.T.);
#7532=EDGE_CURVE('',#5327,#5330,#2092,.T.);
#7533=EDGE_CURVE('',#5331,#5332,#3971,.T.);
#7534=EDGE_CURVE('',#5333,#5331,#2093,.T.);
#7535=EDGE_CURVE('',#5334,#5333,#2094,.T.);
#7536=EDGE_CURVE('',#5335,#5334,#1816,.T.);
#7537=EDGE_CURVE('',#5335,#5336,#2095,.T.);
#7538=EDGE_CURVE('',#5336,#5332,#2096,.T.);
#7539=EDGE_CURVE('',#5337,#5338,#3972,.T.);
#7540=EDGE_CURVE('',#5338,#5339,#2097,.T.);
#7541=EDGE_CURVE('',#5339,#5340,#1817,.T.);
#7542=EDGE_CURVE('',#5340,#5341,#3973,.T.);
#7543=EDGE_CURVE('',#5341,#5341,#1818,.F.);
#7544=EDGE_CURVE('',#5340,#5342,#1819,.T.);
#7545=EDGE_CURVE('',#5342,#5337,#2098,.T.);
#7546=EDGE_CURVE('',#5343,#5344,#3974,.T.);
#7547=EDGE_CURVE('',#5344,#5345,#2099,.T.);
#7548=EDGE_CURVE('',#5345,#5338,#2100,.T.);
#7549=EDGE_CURVE('',#5337,#5343,#2101,.T.);
#7550=EDGE_CURVE('',#5346,#5347,#3975,.T.);
#7551=EDGE_CURVE('',#5347,#5344,#2102,.T.);
#7552=EDGE_CURVE('',#5343,#5348,#2103,.T.);
#7553=EDGE_CURVE('',#5348,#5346,#2104,.T.);
#7554=EDGE_CURVE('',#5349,#5350,#3976,.T.);
#7555=EDGE_CURVE('',#5350,#5351,#2105,.T.);
#7556=EDGE_CURVE('',#5351,#5347,#2106,.T.);
#7557=EDGE_CURVE('',#5346,#5349,#2107,.T.);
#7558=EDGE_CURVE('',#5352,#5353,#3977,.T.);
#7559=EDGE_CURVE('',#5353,#5350,#2108,.T.);
#7560=EDGE_CURVE('',#5349,#5354,#2109,.T.);
#7561=EDGE_CURVE('',#5354,#5352,#2110,.T.);
#7562=EDGE_CURVE('',#5355,#5356,#3978,.T.);
#7563=EDGE_CURVE('',#5356,#5357,#2111,.T.);
#7564=EDGE_CURVE('',#5357,#5353,#2112,.T.);
#7565=EDGE_CURVE('',#5352,#5355,#2113,.T.);
#7566=EDGE_CURVE('',#5358,#5359,#3979,.T.);
#7567=EDGE_CURVE('',#5359,#5356,#2114,.T.);
#7568=EDGE_CURVE('',#5355,#5360,#2115,.T.);
#7569=EDGE_CURVE('',#5360,#5358,#2116,.T.);
#7570=EDGE_CURVE('',#5361,#5362,#3980,.T.);
#7571=EDGE_CURVE('',#5362,#5363,#2117,.T.);
#7572=EDGE_CURVE('',#5363,#5359,#2118,.T.);
#7573=EDGE_CURVE('',#5358,#5361,#2119,.T.);
#7574=EDGE_CURVE('',#5364,#5365,#3981,.T.);
#7575=EDGE_CURVE('',#5365,#5362,#2120,.T.);
#7576=EDGE_CURVE('',#5361,#5366,#2121,.T.);
#7577=EDGE_CURVE('',#5366,#5364,#2122,.T.);
#7578=EDGE_CURVE('',#5367,#5368,#3982,.T.);
#7579=EDGE_CURVE('',#5367,#5369,#2123,.F.);
#7580=EDGE_CURVE('',#5370,#5369,#1820,.T.);
#7581=EDGE_CURVE('',#5370,#5368,#2124,.T.);
#7582=EDGE_CURVE('',#5371,#5372,#3983,.T.);
#7583=EDGE_CURVE('',#5372,#5373,#2125,.T.);
#7584=EDGE_CURVE('',#5373,#5374,#2126,.T.);
#7585=EDGE_CURVE('',#5375,#5374,#1821,.T.);
#7586=EDGE_CURVE('',#5376,#5375,#2127,.T.);
#7587=EDGE_CURVE('',#5371,#5376,#2128,.T.);
#7588=EDGE_CURVE('',#5377,#5378,#3984,.T.);
#7589=EDGE_CURVE('',#5378,#5379,#2129,.T.);
#7590=EDGE_CURVE('',#5379,#5372,#2130,.T.);
#7591=EDGE_CURVE('',#5380,#5371,#2131,.T.);
#7592=EDGE_CURVE('',#5377,#5380,#2132,.T.);
#7593=EDGE_CURVE('',#5381,#5382,#3985,.T.);
#7594=EDGE_CURVE('',#5382,#5383,#2133,.T.);
#7595=EDGE_CURVE('',#5383,#5378,#2134,.T.);
#7596=EDGE_CURVE('',#5384,#5377,#2135,.T.);
#7597=EDGE_CURVE('',#5381,#5384,#2136,.T.);
#7598=EDGE_CURVE('',#5385,#5386,#3986,.T.);
#7599=EDGE_CURVE('',#5386,#5387,#2137,.T.);
#7600=EDGE_CURVE('',#5387,#5382,#2138,.T.);
#7601=EDGE_CURVE('',#5388,#5381,#2139,.T.);
#7602=EDGE_CURVE('',#5385,#5388,#2140,.T.);
#7603=EDGE_CURVE('',#5389,#5390,#3987,.T.);
#7604=EDGE_CURVE('',#5390,#5391,#2141,.T.);
#7605=EDGE_CURVE('',#5391,#5386,#2142,.T.);
#7606=EDGE_CURVE('',#5392,#5385,#2143,.T.);
#7607=EDGE_CURVE('',#5389,#5392,#2144,.T.);
#7608=EDGE_CURVE('',#5393,#5394,#3988,.T.);
#7609=EDGE_CURVE('',#5394,#5395,#2145,.T.);
#7610=EDGE_CURVE('',#5395,#5390,#2146,.T.);
#7611=EDGE_CURVE('',#5396,#5389,#2147,.T.);
#7612=EDGE_CURVE('',#5393,#5396,#2148,.T.);
#7613=EDGE_CURVE('',#5397,#5398,#3989,.T.);
#7614=EDGE_CURVE('',#5398,#5399,#2149,.T.);
#7615=EDGE_CURVE('',#5399,#5394,#2150,.T.);
#7616=EDGE_CURVE('',#5400,#5393,#2151,.T.);
#7617=EDGE_CURVE('',#5397,#5400,#2152,.T.);
#7618=EDGE_CURVE('',#5401,#5402,#3990,.T.);
#7619=EDGE_CURVE('',#5402,#5403,#2153,.T.);
#7620=EDGE_CURVE('',#5403,#5398,#2154,.T.);
#7621=EDGE_CURVE('',#5404,#5397,#2155,.T.);
#7622=EDGE_CURVE('',#5401,#5404,#2156,.T.);
#7623=EDGE_CURVE('',#5405,#5406,#3991,.T.);
#7624=EDGE_CURVE('',#5406,#5407,#2157,.T.);
#7625=EDGE_CURVE('',#5407,#5402,#2158,.T.);
#7626=EDGE_CURVE('',#5408,#5401,#2159,.T.);
#7627=EDGE_CURVE('',#5405,#5408,#2160,.T.);
#7628=EDGE_CURVE('',#5409,#5410,#3992,.T.);
#7629=EDGE_CURVE('',#5411,#5409,#2161,.T.);
#7630=EDGE_CURVE('',#5412,#5411,#2162,.T.);
#7631=EDGE_CURVE('',#5413,#5412,#1822,.T.);
#7632=EDGE_CURVE('',#5413,#5414,#2163,.T.);
#7633=EDGE_CURVE('',#5414,#5410,#2164,.T.);
#7634=EDGE_CURVE('',#5415,#5416,#3993,.T.);
#7635=EDGE_CURVE('',#5416,#5417,#2165,.T.);
#7636=EDGE_CURVE('',#5417,#5418,#1823,.T.);
#7637=EDGE_CURVE('',#5418,#5419,#3994,.T.);
#7638=EDGE_CURVE('',#5419,#5419,#1824,.F.);
#7639=EDGE_CURVE('',#5418,#5420,#1825,.T.);
#7640=EDGE_CURVE('',#5420,#5415,#2166,.T.);
#7641=EDGE_CURVE('',#5421,#5422,#3995,.T.);
#7642=EDGE_CURVE('',#5422,#5423,#2167,.T.);
#7643=EDGE_CURVE('',#5423,#5416,#2168,.T.);
#7644=EDGE_CURVE('',#5415,#5421,#2169,.T.);
#7645=EDGE_CURVE('',#5424,#5425,#3996,.T.);
#7646=EDGE_CURVE('',#5425,#5422,#2170,.T.);
#7647=EDGE_CURVE('',#5421,#5426,#2171,.T.);
#7648=EDGE_CURVE('',#5426,#5424,#2172,.T.);
#7649=EDGE_CURVE('',#5427,#5428,#3997,.T.);
#7650=EDGE_CURVE('',#5428,#5429,#2173,.T.);
#7651=EDGE_CURVE('',#5429,#5425,#2174,.T.);
#7652=EDGE_CURVE('',#5424,#5427,#2175,.T.);
#7653=EDGE_CURVE('',#5430,#5431,#3998,.T.);
#7654=EDGE_CURVE('',#5431,#5428,#2176,.T.);
#7655=EDGE_CURVE('',#5427,#5432,#2177,.T.);
#7656=EDGE_CURVE('',#5432,#5430,#2178,.T.);
#7657=EDGE_CURVE('',#5433,#5434,#3999,.T.);
#7658=EDGE_CURVE('',#5434,#5435,#2179,.T.);
#7659=EDGE_CURVE('',#5435,#5431,#2180,.T.);
#7660=EDGE_CURVE('',#5430,#5433,#2181,.T.);
#7661=EDGE_CURVE('',#5436,#5437,#4000,.T.);
#7662=EDGE_CURVE('',#5437,#5434,#2182,.T.);
#7663=EDGE_CURVE('',#5433,#5438,#2183,.T.);
#7664=EDGE_CURVE('',#5438,#5436,#2184,.T.);
#7665=EDGE_CURVE('',#5439,#5440,#4001,.T.);
#7666=EDGE_CURVE('',#5440,#5441,#2185,.T.);
#7667=EDGE_CURVE('',#5441,#5437,#2186,.T.);
#7668=EDGE_CURVE('',#5436,#5439,#2187,.T.);
#7669=EDGE_CURVE('',#5442,#5443,#4002,.T.);
#7670=EDGE_CURVE('',#5443,#5440,#2188,.T.);
#7671=EDGE_CURVE('',#5439,#5444,#2189,.T.);
#7672=EDGE_CURVE('',#5444,#5442,#2190,.T.);
#7673=EDGE_CURVE('',#5445,#5446,#4003,.T.);
#7674=EDGE_CURVE('',#5445,#5447,#2191,.F.);
#7675=EDGE_CURVE('',#5448,#5447,#1826,.T.);
#7676=EDGE_CURVE('',#5448,#5446,#2192,.T.);
#7677=EDGE_CURVE('',#5449,#5450,#4004,.T.);
#7678=EDGE_CURVE('',#5450,#5451,#2193,.T.);
#7679=EDGE_CURVE('',#5451,#5452,#2194,.T.);
#7680=EDGE_CURVE('',#5453,#5452,#1827,.T.);
#7681=EDGE_CURVE('',#5454,#5453,#2195,.T.);
#7682=EDGE_CURVE('',#5449,#5454,#2196,.T.);
#7683=EDGE_CURVE('',#5455,#5456,#4005,.T.);
#7684=EDGE_CURVE('',#5456,#5457,#2197,.T.);
#7685=EDGE_CURVE('',#5457,#5450,#2198,.T.);
#7686=EDGE_CURVE('',#5458,#5449,#2199,.T.);
#7687=EDGE_CURVE('',#5455,#5458,#2200,.T.);
#7688=EDGE_CURVE('',#5459,#5460,#4006,.T.);
#7689=EDGE_CURVE('',#5460,#5461,#2201,.T.);
#7690=EDGE_CURVE('',#5461,#5456,#2202,.T.);
#7691=EDGE_CURVE('',#5462,#5455,#2203,.T.);
#7692=EDGE_CURVE('',#5459,#5462,#2204,.T.);
#7693=EDGE_CURVE('',#5463,#5464,#4007,.T.);
#7694=EDGE_CURVE('',#5464,#5465,#2205,.T.);
#7695=EDGE_CURVE('',#5465,#5460,#2206,.T.);
#7696=EDGE_CURVE('',#5466,#5459,#2207,.T.);
#7697=EDGE_CURVE('',#5463,#5466,#2208,.T.);
#7698=EDGE_CURVE('',#5467,#5468,#4008,.T.);
#7699=EDGE_CURVE('',#5468,#5469,#2209,.T.);
#7700=EDGE_CURVE('',#5469,#5464,#2210,.T.);
#7701=EDGE_CURVE('',#5470,#5463,#2211,.T.);
#7702=EDGE_CURVE('',#5467,#5470,#2212,.T.);
#7703=EDGE_CURVE('',#5471,#5472,#4009,.T.);
#7704=EDGE_CURVE('',#5472,#5473,#2213,.T.);
#7705=EDGE_CURVE('',#5473,#5468,#2214,.T.);
#7706=EDGE_CURVE('',#5474,#5467,#2215,.T.);
#7707=EDGE_CURVE('',#5471,#5474,#2216,.T.);
#7708=EDGE_CURVE('',#5475,#5476,#4010,.T.);
#7709=EDGE_CURVE('',#5476,#5477,#2217,.T.);
#7710=EDGE_CURVE('',#5477,#5472,#2218,.T.);
#7711=EDGE_CURVE('',#5478,#5471,#2219,.T.);
#7712=EDGE_CURVE('',#5475,#5478,#2220,.T.);
#7713=EDGE_CURVE('',#5479,#5480,#4011,.T.);
#7714=EDGE_CURVE('',#5480,#5481,#2221,.T.);
#7715=EDGE_CURVE('',#5481,#5476,#2222,.T.);
#7716=EDGE_CURVE('',#5482,#5475,#2223,.T.);
#7717=EDGE_CURVE('',#5479,#5482,#2224,.T.);
#7718=EDGE_CURVE('',#5483,#5484,#4012,.T.);
#7719=EDGE_CURVE('',#5484,#5485,#2225,.T.);
#7720=EDGE_CURVE('',#5485,#5480,#2226,.T.);
#7721=EDGE_CURVE('',#5486,#5479,#2227,.T.);
#7722=EDGE_CURVE('',#5483,#5486,#2228,.T.);
#7723=EDGE_CURVE('',#5487,#5488,#4013,.T.);
#7724=EDGE_CURVE('',#5489,#5487,#2229,.T.);
#7725=EDGE_CURVE('',#5490,#5489,#2230,.T.);
#7726=EDGE_CURVE('',#5491,#5490,#1828,.T.);
#7727=EDGE_CURVE('',#5491,#5492,#2231,.T.);
#7728=EDGE_CURVE('',#5492,#5488,#2232,.T.);
#7729=EDGE_CURVE('',#5493,#5494,#4014,.T.);
#7730=EDGE_CURVE('',#5494,#5495,#2233,.T.);
#7731=EDGE_CURVE('',#5495,#5496,#1829,.T.);
#7732=EDGE_CURVE('',#5496,#5497,#4015,.T.);
#7733=EDGE_CURVE('',#5497,#5497,#1830,.F.);
#7734=EDGE_CURVE('',#5496,#5498,#1831,.T.);
#7735=EDGE_CURVE('',#5498,#5493,#2234,.T.);
#7736=EDGE_CURVE('',#5499,#5500,#4016,.T.);
#7737=EDGE_CURVE('',#5500,#5501,#2235,.T.);
#7738=EDGE_CURVE('',#5501,#5494,#2236,.T.);
#7739=EDGE_CURVE('',#5493,#5499,#2237,.T.);
#7740=EDGE_CURVE('',#5502,#5503,#4017,.T.);
#7741=EDGE_CURVE('',#5503,#5500,#2238,.T.);
#7742=EDGE_CURVE('',#5499,#5504,#2239,.T.);
#7743=EDGE_CURVE('',#5504,#5502,#2240,.T.);
#7744=EDGE_CURVE('',#5505,#5506,#4018,.T.);
#7745=EDGE_CURVE('',#5506,#5507,#2241,.T.);
#7746=EDGE_CURVE('',#5507,#5503,#2242,.T.);
#7747=EDGE_CURVE('',#5502,#5505,#2243,.T.);
#7748=EDGE_CURVE('',#5508,#5509,#4019,.T.);
#7749=EDGE_CURVE('',#5509,#5506,#2244,.T.);
#7750=EDGE_CURVE('',#5505,#5510,#2245,.T.);
#7751=EDGE_CURVE('',#5510,#5508,#2246,.T.);
#7752=EDGE_CURVE('',#5511,#5512,#4020,.T.);
#7753=EDGE_CURVE('',#5512,#5513,#2247,.T.);
#7754=EDGE_CURVE('',#5513,#5509,#2248,.T.);
#7755=EDGE_CURVE('',#5508,#5511,#2249,.T.);
#7756=EDGE_CURVE('',#5514,#5515,#4021,.T.);
#7757=EDGE_CURVE('',#5515,#5512,#2250,.T.);
#7758=EDGE_CURVE('',#5511,#5516,#2251,.T.);
#7759=EDGE_CURVE('',#5516,#5514,#2252,.T.);
#7760=EDGE_CURVE('',#5517,#5518,#4022,.T.);
#7761=EDGE_CURVE('',#5518,#5519,#2253,.T.);
#7762=EDGE_CURVE('',#5519,#5515,#2254,.T.);
#7763=EDGE_CURVE('',#5514,#5517,#2255,.T.);
#7764=EDGE_CURVE('',#5520,#5521,#4023,.T.);
#7765=EDGE_CURVE('',#5521,#5518,#2256,.T.);
#7766=EDGE_CURVE('',#5517,#5522,#2257,.T.);
#7767=EDGE_CURVE('',#5522,#5520,#2258,.T.);
#7768=EDGE_CURVE('',#5523,#5524,#4024,.T.);
#7769=EDGE_CURVE('',#5523,#5525,#2259,.F.);
#7770=EDGE_CURVE('',#5526,#5525,#1832,.T.);
#7771=EDGE_CURVE('',#5526,#5524,#2260,.T.);
#7772=EDGE_CURVE('',#5524,#5527,#2261,.T.);
#7773=EDGE_CURVE('',#5527,#5521,#2262,.T.);
#7774=EDGE_CURVE('',#5520,#5528,#2263,.T.);
#7775=EDGE_CURVE('',#5528,#5523,#2264,.F.);
#7776=EDGE_CURVE('',#5488,#5529,#2265,.T.);
#7777=EDGE_CURVE('',#5529,#5484,#2266,.T.);
#7778=EDGE_CURVE('',#5530,#5483,#2267,.T.);
#7779=EDGE_CURVE('',#5487,#5530,#2268,.T.);
#7780=EDGE_CURVE('',#5446,#5531,#2269,.T.);
#7781=EDGE_CURVE('',#5531,#5443,#2270,.T.);
#7782=EDGE_CURVE('',#5442,#5532,#2271,.T.);
#7783=EDGE_CURVE('',#5532,#5445,#2272,.F.);
#7784=EDGE_CURVE('',#5410,#5533,#2273,.T.);
#7785=EDGE_CURVE('',#5533,#5406,#2274,.T.);
#7786=EDGE_CURVE('',#5534,#5405,#2275,.T.);
#7787=EDGE_CURVE('',#5409,#5534,#2276,.T.);
#7788=EDGE_CURVE('',#5368,#5535,#2277,.T.);
#7789=EDGE_CURVE('',#5535,#5365,#2278,.T.);
#7790=EDGE_CURVE('',#5364,#5536,#2279,.T.);
#7791=EDGE_CURVE('',#5536,#5367,#2280,.F.);
#7792=EDGE_CURVE('',#5332,#5537,#2281,.T.);
#7793=EDGE_CURVE('',#5537,#5328,#2282,.T.);
#7794=EDGE_CURVE('',#5538,#5327,#2283,.T.);
#7795=EDGE_CURVE('',#5331,#5538,#2284,.T.);
#7796=EDGE_CURVE('',#5290,#5539,#2285,.T.);
#7797=EDGE_CURVE('',#5539,#5287,#2286,.T.);
#7798=EDGE_CURVE('',#5286,#5540,#2287,.T.);
#7799=EDGE_CURVE('',#5540,#5289,#2288,.F.);
#7800=EDGE_CURVE('',#5254,#5541,#2289,.T.);
#7801=EDGE_CURVE('',#5541,#5250,#2290,.T.);
#7802=EDGE_CURVE('',#5542,#5249,#2291,.T.);
#7803=EDGE_CURVE('',#5253,#5542,#2292,.T.);
#7804=EDGE_CURVE('',#5261,#5219,#2293,.T.);
#7805=EDGE_CURVE('',#5218,#5264,#2294,.T.);
#7806=EDGE_CURVE('',#5291,#5257,#2295,.T.);
#7807=EDGE_CURVE('',#5543,#5292,#2296,.T.);
#7808=EDGE_CURVE('',#5256,#5543,#2297,.T.);
#7809=EDGE_CURVE('',#5339,#5297,#2298,.T.);
#7810=EDGE_CURVE('',#5296,#5342,#2299,.T.);
#7811=EDGE_CURVE('',#5369,#5335,#2300,.T.);
#7812=EDGE_CURVE('',#5544,#5370,#2301,.T.);
#7813=EDGE_CURVE('',#5334,#5544,#2302,.T.);
#7814=EDGE_CURVE('',#5417,#5375,#2303,.T.);
#7815=EDGE_CURVE('',#5374,#5420,#2304,.T.);
#7816=EDGE_CURVE('',#5447,#5413,#2305,.T.);
#7817=EDGE_CURVE('',#5545,#5448,#2306,.T.);
#7818=EDGE_CURVE('',#5412,#5545,#2307,.T.);
#7819=EDGE_CURVE('',#5495,#5453,#2308,.T.);
#7820=EDGE_CURVE('',#5452,#5498,#2309,.T.);
#7821=EDGE_CURVE('',#5525,#5491,#2310,.T.);
#7822=EDGE_CURVE('',#5546,#5526,#2311,.T.);
#7823=EDGE_CURVE('',#5490,#5546,#2312,.T.);
#7824=EDGE_CURVE('',#5547,#5547,#1833,.T.);
#7825=EDGE_CURVE('',#5547,#5548,#4025,.T.);
#7826=EDGE_CURVE('',#5548,#5548,#1834,.T.);
#7827=EDGE_CURVE('',#5549,#5549,#1835,.T.);
#7828=EDGE_CURVE('',#5549,#5550,#4026,.T.);
#7829=EDGE_CURVE('',#5550,#5550,#1836,.T.);
#7830=EDGE_CURVE('',#5551,#5551,#1837,.T.);
#7831=EDGE_CURVE('',#5551,#5552,#4027,.T.);
#7832=EDGE_CURVE('',#5552,#5552,#1838,.T.);
#7833=EDGE_CURVE('',#5553,#5553,#1839,.T.);
#7834=EDGE_CURVE('',#5553,#5554,#4028,.T.);
#7835=EDGE_CURVE('',#5554,#5554,#1840,.T.);
#7836=EDGE_CURVE('',#5555,#5556,#4029,.F.);
#7837=EDGE_CURVE('',#5556,#5557,#4030,.T.);
#7838=EDGE_CURVE('',#5558,#5557,#4031,.F.);
#7839=EDGE_CURVE('',#5555,#5558,#4032,.T.);
#7840=EDGE_CURVE('',#5559,#5555,#4033,.F.);
#7841=EDGE_CURVE('',#5560,#5558,#4034,.F.);
#7842=EDGE_CURVE('',#5559,#5560,#4035,.F.);
#7843=EDGE_CURVE('',#5561,#5559,#4036,.F.);
#7844=EDGE_CURVE('',#5562,#5560,#4037,.F.);
#7845=EDGE_CURVE('',#5561,#5562,#4038,.F.);
#7846=EDGE_CURVE('',#5556,#5561,#4039,.F.);
#7847=EDGE_CURVE('',#5557,#5562,#4040,.F.);
#7848=EDGE_CURVE('',#5563,#5564,#4041,.T.);
#7849=EDGE_CURVE('',#5564,#5565,#2313,.T.);
#7850=EDGE_CURVE('',#5566,#5565,#1841,.T.);
#7851=EDGE_CURVE('',#5563,#5566,#2314,.T.);
#7852=EDGE_CURVE('',#5567,#5568,#4042,.T.);
#7853=EDGE_CURVE('',#5568,#5569,#2315,.T.);
#7854=EDGE_CURVE('',#5569,#5564,#2316,.T.);
#7855=EDGE_CURVE('',#5570,#5563,#2317,.T.);
#7856=EDGE_CURVE('',#5567,#5570,#2318,.T.);
#7857=EDGE_CURVE('',#5571,#5572,#4043,.T.);
#7858=EDGE_CURVE('',#5572,#5573,#2319,.T.);
#7859=EDGE_CURVE('',#5573,#5568,#2320,.T.);
#7860=EDGE_CURVE('',#5574,#5567,#2321,.T.);
#7861=EDGE_CURVE('',#5571,#5574,#2322,.T.);
#7862=EDGE_CURVE('',#5575,#5576,#4044,.T.);
#7863=EDGE_CURVE('',#5576,#5577,#2323,.T.);
#7864=EDGE_CURVE('',#5577,#5572,#2324,.T.);
#7865=EDGE_CURVE('',#5578,#5571,#2325,.T.);
#7866=EDGE_CURVE('',#5575,#5578,#2326,.T.);
#7867=EDGE_CURVE('',#5579,#5580,#4045,.T.);
#7868=EDGE_CURVE('',#5580,#5581,#2327,.T.);
#7869=EDGE_CURVE('',#5581,#5576,#2328,.T.);
#7870=EDGE_CURVE('',#5582,#5575,#2329,.T.);
#7871=EDGE_CURVE('',#5579,#5582,#2330,.T.);
#7872=EDGE_CURVE('',#5583,#5584,#4046,.T.);
#7873=EDGE_CURVE('',#5584,#5585,#2331,.T.);
#7874=EDGE_CURVE('',#5585,#5580,#2332,.T.);
#7875=EDGE_CURVE('',#5586,#5579,#2333,.T.);
#7876=EDGE_CURVE('',#5583,#5586,#2334,.T.);
#7877=EDGE_CURVE('',#5587,#5588,#4047,.T.);
#7878=EDGE_CURVE('',#5588,#5589,#2335,.T.);
#7879=EDGE_CURVE('',#5589,#5584,#2336,.T.);
#7880=EDGE_CURVE('',#5590,#5583,#2337,.T.);
#7881=EDGE_CURVE('',#5587,#5590,#2338,.T.);
#7882=EDGE_CURVE('',#5591,#5592,#4048,.T.);
#7883=EDGE_CURVE('',#5592,#5593,#2339,.T.);
#7884=EDGE_CURVE('',#5593,#5588,#2340,.T.);
#7885=EDGE_CURVE('',#5594,#5587,#2341,.T.);
#7886=EDGE_CURVE('',#5591,#5594,#2342,.T.);
#7887=EDGE_CURVE('',#5595,#5596,#4049,.T.);
#7888=EDGE_CURVE('',#5596,#5597,#2343,.T.);
#7889=EDGE_CURVE('',#5597,#5592,#2344,.T.);
#7890=EDGE_CURVE('',#5598,#5591,#2345,.T.);
#7891=EDGE_CURVE('',#5595,#5598,#2346,.T.);
#7892=EDGE_CURVE('',#5599,#5600,#4050,.T.);
#7893=EDGE_CURVE('',#5600,#5601,#2347,.T.);
#7894=EDGE_CURVE('',#5601,#5596,#2348,.T.);
#7895=EDGE_CURVE('',#5602,#5595,#2349,.T.);
#7896=EDGE_CURVE('',#5599,#5602,#2350,.T.);
#7897=EDGE_CURVE('',#5603,#5604,#4051,.T.);
#7898=EDGE_CURVE('',#5604,#5605,#2351,.T.);
#7899=EDGE_CURVE('',#5605,#5600,#2352,.T.);
#7900=EDGE_CURVE('',#5606,#5599,#2353,.T.);
#7901=EDGE_CURVE('',#5603,#5606,#2354,.T.);
#7902=EDGE_CURVE('',#5607,#5608,#4052,.T.);
#7903=EDGE_CURVE('',#5608,#5609,#2355,.T.);
#7904=EDGE_CURVE('',#5609,#5604,#2356,.T.);
#7905=EDGE_CURVE('',#5610,#5603,#2357,.T.);
#7906=EDGE_CURVE('',#5607,#5610,#2358,.T.);
#7907=EDGE_CURVE('',#5611,#5612,#4053,.T.);
#7908=EDGE_CURVE('',#5612,#5613,#2359,.T.);
#7909=EDGE_CURVE('',#5613,#5608,#2360,.T.);
#7910=EDGE_CURVE('',#5614,#5607,#2361,.T.);
#7911=EDGE_CURVE('',#5611,#5614,#2362,.T.);
#7912=EDGE_CURVE('',#5615,#5616,#4054,.T.);
#7913=EDGE_CURVE('',#5616,#5617,#2363,.T.);
#7914=EDGE_CURVE('',#5617,#5612,#2364,.T.);
#7915=EDGE_CURVE('',#5618,#5611,#2365,.T.);
#7916=EDGE_CURVE('',#5615,#5618,#2366,.T.);
#7917=EDGE_CURVE('',#5619,#5620,#4055,.T.);
#7918=EDGE_CURVE('',#5620,#5621,#2367,.T.);
#7919=EDGE_CURVE('',#5621,#5616,#2368,.T.);
#7920=EDGE_CURVE('',#5622,#5615,#2369,.T.);
#7921=EDGE_CURVE('',#5619,#5622,#2370,.T.);
#7922=EDGE_CURVE('',#5623,#5624,#4056,.T.);
#7923=EDGE_CURVE('',#5625,#5623,#2371,.T.);
#7924=EDGE_CURVE('',#5626,#5625,#2372,.T.);
#7925=EDGE_CURVE('',#5627,#5626,#1842,.T.);
#7926=EDGE_CURVE('',#5627,#5628,#2373,.T.);
#7927=EDGE_CURVE('',#5628,#5624,#2374,.T.);
#7928=EDGE_CURVE('',#5629,#5630,#4057,.T.);
#7929=EDGE_CURVE('',#5630,#5631,#2375,.T.);
#7930=EDGE_CURVE('',#5631,#5632,#1843,.T.);
#7931=EDGE_CURVE('',#5632,#5633,#2376,.T.);
#7932=EDGE_CURVE('',#5633,#5634,#4058,.T.);
#7933=EDGE_CURVE('',#5634,#5634,#1844,.F.);
#7934=EDGE_CURVE('',#5633,#5629,#2377,.T.);
#7935=EDGE_CURVE('',#5635,#5636,#4059,.T.);
#7936=EDGE_CURVE('',#5636,#5630,#2378,.T.);
#7937=EDGE_CURVE('',#5629,#5637,#2379,.T.);
#7938=EDGE_CURVE('',#5637,#5635,#2380,.T.);
#7939=EDGE_CURVE('',#5638,#5639,#4060,.T.);
#7940=EDGE_CURVE('',#5639,#5640,#2381,.T.);
#7941=EDGE_CURVE('',#5640,#5636,#2382,.T.);
#7942=EDGE_CURVE('',#5635,#5641,#2383,.T.);
#7943=EDGE_CURVE('',#5641,#5638,#2384,.T.);
#7944=EDGE_CURVE('',#5642,#5643,#4061,.T.);
#7945=EDGE_CURVE('',#5643,#5639,#2385,.T.);
#7946=EDGE_CURVE('',#5638,#5642,#2386,.T.);
#7947=EDGE_CURVE('',#5644,#5645,#4062,.T.);
#7948=EDGE_CURVE('',#5645,#5646,#2387,.T.);
#7949=EDGE_CURVE('',#5646,#5643,#2388,.T.);
#7950=EDGE_CURVE('',#5642,#5647,#2389,.T.);
#7951=EDGE_CURVE('',#5647,#5644,#2390,.T.);
#7952=EDGE_CURVE('',#5648,#5649,#4063,.T.);
#7953=EDGE_CURVE('',#5649,#5645,#2391,.T.);
#7954=EDGE_CURVE('',#5644,#5648,#2392,.T.);
#7955=EDGE_CURVE('',#5650,#5651,#4064,.T.);
#7956=EDGE_CURVE('',#5651,#5652,#2393,.T.);
#7957=EDGE_CURVE('',#5652,#5649,#2394,.T.);
#7958=EDGE_CURVE('',#5648,#5653,#2395,.T.);
#7959=EDGE_CURVE('',#5653,#5650,#2396,.T.);
#7960=EDGE_CURVE('',#5654,#5655,#4065,.T.);
#7961=EDGE_CURVE('',#5655,#5651,#2397,.T.);
#7962=EDGE_CURVE('',#5650,#5654,#2398,.T.);
#7963=EDGE_CURVE('',#5656,#5657,#4066,.T.);
#7964=EDGE_CURVE('',#5657,#5658,#2399,.T.);
#7965=EDGE_CURVE('',#5658,#5655,#2400,.T.);
#7966=EDGE_CURVE('',#5654,#5659,#2401,.T.);
#7967=EDGE_CURVE('',#5659,#5656,#2402,.T.);
#7968=EDGE_CURVE('',#5660,#5661,#4067,.T.);
#7969=EDGE_CURVE('',#5661,#5657,#2403,.T.);
#7970=EDGE_CURVE('',#5656,#5660,#2404,.T.);
#7971=EDGE_CURVE('',#5662,#5663,#4068,.T.);
#7972=EDGE_CURVE('',#5663,#5664,#2405,.T.);
#7973=EDGE_CURVE('',#5664,#5661,#2406,.T.);
#7974=EDGE_CURVE('',#5660,#5665,#2407,.T.);
#7975=EDGE_CURVE('',#5665,#5662,#2408,.T.);
#7976=EDGE_CURVE('',#5666,#5667,#4069,.T.);
#7977=EDGE_CURVE('',#5667,#5663,#2409,.T.);
#7978=EDGE_CURVE('',#5662,#5666,#2410,.T.);
#7979=EDGE_CURVE('',#5668,#5669,#4070,.T.);
#7980=EDGE_CURVE('',#5669,#5670,#2411,.T.);
#7981=EDGE_CURVE('',#5670,#5667,#2412,.T.);
#7982=EDGE_CURVE('',#5666,#5671,#2413,.T.);
#7983=EDGE_CURVE('',#5671,#5668,#2414,.T.);
#7984=EDGE_CURVE('',#5672,#5673,#4071,.T.);
#7985=EDGE_CURVE('',#5673,#5669,#2415,.T.);
#7986=EDGE_CURVE('',#5668,#5672,#2416,.T.);
#7987=EDGE_CURVE('',#5674,#5675,#4072,.T.);
#7988=EDGE_CURVE('',#5674,#5676,#2417,.T.);
#7989=EDGE_CURVE('',#5677,#5676,#1845,.T.);
#7990=EDGE_CURVE('',#5677,#5675,#2418,.T.);
#7991=EDGE_CURVE('',#5678,#5679,#4073,.T.);
#7992=EDGE_CURVE('',#5679,#5680,#2419,.T.);
#7993=EDGE_CURVE('',#5681,#5680,#1846,.T.);
#7994=EDGE_CURVE('',#5678,#5681,#2420,.T.);
#7995=EDGE_CURVE('',#5682,#5683,#4074,.T.);
#7996=EDGE_CURVE('',#5683,#5684,#2421,.T.);
#7997=EDGE_CURVE('',#5684,#5679,#2422,.T.);
#7998=EDGE_CURVE('',#5685,#5678,#2423,.T.);
#7999=EDGE_CURVE('',#5682,#5685,#2424,.T.);
#8000=EDGE_CURVE('',#5686,#5687,#4075,.T.);
#8001=EDGE_CURVE('',#5687,#5688,#2425,.T.);
#8002=EDGE_CURVE('',#5688,#5683,#2426,.T.);
#8003=EDGE_CURVE('',#5689,#5682,#2427,.T.);
#8004=EDGE_CURVE('',#5686,#5689,#2428,.T.);
#8005=EDGE_CURVE('',#5690,#5691,#4076,.T.);
#8006=EDGE_CURVE('',#5691,#5692,#2429,.T.);
#8007=EDGE_CURVE('',#5692,#5687,#2430,.T.);
#8008=EDGE_CURVE('',#5693,#5686,#2431,.T.);
#8009=EDGE_CURVE('',#5690,#5693,#2432,.T.);
#8010=EDGE_CURVE('',#5694,#5695,#4077,.T.);
#8011=EDGE_CURVE('',#5695,#5696,#2433,.T.);
#8012=EDGE_CURVE('',#5696,#5691,#2434,.T.);
#8013=EDGE_CURVE('',#5697,#5690,#2435,.T.);
#8014=EDGE_CURVE('',#5694,#5697,#2436,.T.);
#8015=EDGE_CURVE('',#5698,#5699,#4078,.T.);
#8016=EDGE_CURVE('',#5699,#5700,#2437,.T.);
#8017=EDGE_CURVE('',#5700,#5695,#2438,.T.);
#8018=EDGE_CURVE('',#5701,#5694,#2439,.T.);
#8019=EDGE_CURVE('',#5698,#5701,#2440,.T.);
#8020=EDGE_CURVE('',#5702,#5703,#4079,.T.);
#8021=EDGE_CURVE('',#5703,#5704,#2441,.T.);
#8022=EDGE_CURVE('',#5704,#5699,#2442,.T.);
#8023=EDGE_CURVE('',#5705,#5698,#2443,.T.);
#8024=EDGE_CURVE('',#5702,#5705,#2444,.T.);
#8025=EDGE_CURVE('',#5706,#5707,#4080,.T.);
#8026=EDGE_CURVE('',#5707,#5708,#2445,.T.);
#8027=EDGE_CURVE('',#5708,#5703,#2446,.T.);
#8028=EDGE_CURVE('',#5709,#5702,#2447,.T.);
#8029=EDGE_CURVE('',#5706,#5709,#2448,.T.);
#8030=EDGE_CURVE('',#5710,#5711,#4081,.T.);
#8031=EDGE_CURVE('',#5711,#5712,#2449,.T.);
#8032=EDGE_CURVE('',#5712,#5707,#2450,.T.);
#8033=EDGE_CURVE('',#5713,#5706,#2451,.T.);
#8034=EDGE_CURVE('',#5710,#5713,#2452,.T.);
#8035=EDGE_CURVE('',#5714,#5715,#4082,.T.);
#8036=EDGE_CURVE('',#5715,#5716,#2453,.T.);
#8037=EDGE_CURVE('',#5716,#5711,#2454,.T.);
#8038=EDGE_CURVE('',#5717,#5710,#2455,.T.);
#8039=EDGE_CURVE('',#5714,#5717,#2456,.T.);
#8040=EDGE_CURVE('',#5718,#5719,#4083,.T.);
#8041=EDGE_CURVE('',#5719,#5720,#2457,.T.);
#8042=EDGE_CURVE('',#5720,#5715,#2458,.T.);
#8043=EDGE_CURVE('',#5721,#5714,#2459,.T.);
#8044=EDGE_CURVE('',#5718,#5721,#2460,.T.);
#8045=EDGE_CURVE('',#5722,#5723,#4084,.T.);
#8046=EDGE_CURVE('',#5723,#5724,#2461,.T.);
#8047=EDGE_CURVE('',#5724,#5719,#2462,.T.);
#8048=EDGE_CURVE('',#5725,#5718,#2463,.T.);
#8049=EDGE_CURVE('',#5722,#5725,#2464,.T.);
#8050=EDGE_CURVE('',#5726,#5727,#4085,.T.);
#8051=EDGE_CURVE('',#5727,#5728,#2465,.T.);
#8052=EDGE_CURVE('',#5728,#5723,#2466,.T.);
#8053=EDGE_CURVE('',#5729,#5722,#2467,.T.);
#8054=EDGE_CURVE('',#5726,#5729,#2468,.T.);
#8055=EDGE_CURVE('',#5730,#5731,#4086,.T.);
#8056=EDGE_CURVE('',#5731,#5732,#2469,.T.);
#8057=EDGE_CURVE('',#5732,#5727,#2470,.T.);
#8058=EDGE_CURVE('',#5733,#5726,#2471,.T.);
#8059=EDGE_CURVE('',#5730,#5733,#2472,.T.);
#8060=EDGE_CURVE('',#5734,#5735,#4087,.T.);
#8061=EDGE_CURVE('',#5735,#5736,#2473,.T.);
#8062=EDGE_CURVE('',#5736,#5731,#2474,.T.);
#8063=EDGE_CURVE('',#5737,#5730,#2475,.T.);
#8064=EDGE_CURVE('',#5734,#5737,#2476,.T.);
#8065=EDGE_CURVE('',#5738,#5739,#4088,.T.);
#8066=EDGE_CURVE('',#5740,#5738,#2477,.T.);
#8067=EDGE_CURVE('',#5741,#5740,#2478,.T.);
#8068=EDGE_CURVE('',#5742,#5741,#1847,.T.);
#8069=EDGE_CURVE('',#5742,#5743,#2479,.T.);
#8070=EDGE_CURVE('',#5743,#5739,#2480,.T.);
#8071=EDGE_CURVE('',#5744,#5745,#4089,.T.);
#8072=EDGE_CURVE('',#5745,#5746,#2481,.T.);
#8073=EDGE_CURVE('',#5746,#5747,#1848,.T.);
#8074=EDGE_CURVE('',#5747,#5748,#2482,.T.);
#8075=EDGE_CURVE('',#5748,#5749,#4090,.T.);
#8076=EDGE_CURVE('',#5749,#5749,#1849,.F.);
#8077=EDGE_CURVE('',#5748,#5744,#2483,.T.);
#8078=EDGE_CURVE('',#5750,#5751,#4091,.T.);
#8079=EDGE_CURVE('',#5751,#5745,#2484,.T.);
#8080=EDGE_CURVE('',#5744,#5752,#2485,.T.);
#8081=EDGE_CURVE('',#5752,#5750,#2486,.T.);
#8082=EDGE_CURVE('',#5753,#5754,#4092,.T.);
#8083=EDGE_CURVE('',#5754,#5755,#2487,.T.);
#8084=EDGE_CURVE('',#5755,#5751,#2488,.T.);
#8085=EDGE_CURVE('',#5750,#5756,#2489,.T.);
#8086=EDGE_CURVE('',#5756,#5753,#2490,.T.);
#8087=EDGE_CURVE('',#5757,#5758,#4093,.T.);
#8088=EDGE_CURVE('',#5758,#5754,#2491,.T.);
#8089=EDGE_CURVE('',#5753,#5757,#2492,.T.);
#8090=EDGE_CURVE('',#5759,#5760,#4094,.T.);
#8091=EDGE_CURVE('',#5760,#5761,#2493,.T.);
#8092=EDGE_CURVE('',#5761,#5758,#2494,.T.);
#8093=EDGE_CURVE('',#5757,#5762,#2495,.T.);
#8094=EDGE_CURVE('',#5762,#5759,#2496,.T.);
#8095=EDGE_CURVE('',#5763,#5764,#4095,.T.);
#8096=EDGE_CURVE('',#5764,#5760,#2497,.T.);
#8097=EDGE_CURVE('',#5759,#5763,#2498,.T.);
#8098=EDGE_CURVE('',#5765,#5766,#4096,.T.);
#8099=EDGE_CURVE('',#5766,#5767,#2499,.T.);
#8100=EDGE_CURVE('',#5767,#5764,#2500,.T.);
#8101=EDGE_CURVE('',#5763,#5768,#2501,.T.);
#8102=EDGE_CURVE('',#5768,#5765,#2502,.T.);
#8103=EDGE_CURVE('',#5769,#5770,#4097,.T.);
#8104=EDGE_CURVE('',#5770,#5766,#2503,.T.);
#8105=EDGE_CURVE('',#5765,#5769,#2504,.T.);
#8106=EDGE_CURVE('',#5771,#5772,#4098,.T.);
#8107=EDGE_CURVE('',#5772,#5773,#2505,.T.);
#8108=EDGE_CURVE('',#5773,#5770,#2506,.T.);
#8109=EDGE_CURVE('',#5769,#5774,#2507,.T.);
#8110=EDGE_CURVE('',#5774,#5771,#2508,.T.);
#8111=EDGE_CURVE('',#5775,#5776,#4099,.T.);
#8112=EDGE_CURVE('',#5776,#5772,#2509,.T.);
#8113=EDGE_CURVE('',#5771,#5775,#2510,.T.);
#8114=EDGE_CURVE('',#5777,#5778,#4100,.T.);
#8115=EDGE_CURVE('',#5778,#5779,#2511,.T.);
#8116=EDGE_CURVE('',#5779,#5776,#2512,.T.);
#8117=EDGE_CURVE('',#5775,#5780,#2513,.T.);
#8118=EDGE_CURVE('',#5780,#5777,#2514,.T.);
#8119=EDGE_CURVE('',#5781,#5782,#4101,.T.);
#8120=EDGE_CURVE('',#5782,#5778,#2515,.T.);
#8121=EDGE_CURVE('',#5777,#5781,#2516,.T.);
#8122=EDGE_CURVE('',#5783,#5784,#4102,.T.);
#8123=EDGE_CURVE('',#5784,#5785,#2517,.T.);
#8124=EDGE_CURVE('',#5785,#5782,#2518,.T.);
#8125=EDGE_CURVE('',#5781,#5786,#2519,.T.);
#8126=EDGE_CURVE('',#5786,#5783,#2520,.T.);
#8127=EDGE_CURVE('',#5787,#5788,#4103,.T.);
#8128=EDGE_CURVE('',#5788,#5784,#2521,.T.);
#8129=EDGE_CURVE('',#5783,#5787,#2522,.T.);
#8130=EDGE_CURVE('',#5789,#5790,#4104,.T.);
#8131=EDGE_CURVE('',#5789,#5791,#2523,.T.);
#8132=EDGE_CURVE('',#5792,#5791,#1850,.T.);
#8133=EDGE_CURVE('',#5792,#5790,#2524,.T.);
#8134=EDGE_CURVE('',#5793,#5794,#4105,.T.);
#8135=EDGE_CURVE('',#5794,#5795,#2525,.T.);
#8136=EDGE_CURVE('',#5796,#5795,#1851,.T.);
#8137=EDGE_CURVE('',#5797,#5796,#2526,.T.);
#8138=EDGE_CURVE('',#5793,#5797,#2527,.T.);
#8139=EDGE_CURVE('',#5798,#5799,#4106,.T.);
#8140=EDGE_CURVE('',#5799,#5800,#2528,.T.);
#8141=EDGE_CURVE('',#5800,#5794,#2529,.T.);
#8142=EDGE_CURVE('',#5801,#5793,#2530,.T.);
#8143=EDGE_CURVE('',#5798,#5801,#2531,.T.);
#8144=EDGE_CURVE('',#5802,#5803,#4107,.T.);
#8145=EDGE_CURVE('',#5803,#5804,#2532,.T.);
#8146=EDGE_CURVE('',#5804,#5799,#2533,.T.);
#8147=EDGE_CURVE('',#5805,#5798,#2534,.T.);
#8148=EDGE_CURVE('',#5802,#5805,#2535,.T.);
#8149=EDGE_CURVE('',#5806,#5807,#4108,.T.);
#8150=EDGE_CURVE('',#5807,#5808,#2536,.T.);
#8151=EDGE_CURVE('',#5808,#5803,#2537,.T.);
#8152=EDGE_CURVE('',#5809,#5802,#2538,.T.);
#8153=EDGE_CURVE('',#5806,#5809,#2539,.T.);
#8154=EDGE_CURVE('',#5810,#5811,#4109,.T.);
#8155=EDGE_CURVE('',#5811,#5812,#2540,.T.);
#8156=EDGE_CURVE('',#5812,#5807,#2541,.T.);
#8157=EDGE_CURVE('',#5813,#5806,#2542,.T.);
#8158=EDGE_CURVE('',#5810,#5813,#2543,.T.);
#8159=EDGE_CURVE('',#5814,#5815,#4110,.T.);
#8160=EDGE_CURVE('',#5815,#5816,#2544,.T.);
#8161=EDGE_CURVE('',#5816,#5811,#2545,.T.);
#8162=EDGE_CURVE('',#5817,#5810,#2546,.T.);
#8163=EDGE_CURVE('',#5814,#5817,#2547,.T.);
#8164=EDGE_CURVE('',#5818,#5819,#4111,.T.);
#8165=EDGE_CURVE('',#5819,#5820,#2548,.T.);
#8166=EDGE_CURVE('',#5820,#5815,#2549,.T.);
#8167=EDGE_CURVE('',#5821,#5814,#2550,.T.);
#8168=EDGE_CURVE('',#5818,#5821,#2551,.T.);
#8169=EDGE_CURVE('',#5822,#5823,#4112,.T.);
#8170=EDGE_CURVE('',#5823,#5824,#2552,.T.);
#8171=EDGE_CURVE('',#5824,#5819,#2553,.T.);
#8172=EDGE_CURVE('',#5825,#5818,#2554,.T.);
#8173=EDGE_CURVE('',#5822,#5825,#2555,.T.);
#8174=EDGE_CURVE('',#5826,#5827,#4113,.T.);
#8175=EDGE_CURVE('',#5827,#5828,#2556,.T.);
#8176=EDGE_CURVE('',#5828,#5823,#2557,.T.);
#8177=EDGE_CURVE('',#5829,#5822,#2558,.T.);
#8178=EDGE_CURVE('',#5826,#5829,#2559,.T.);
#8179=EDGE_CURVE('',#5830,#5831,#4114,.T.);
#8180=EDGE_CURVE('',#5831,#5832,#2560,.T.);
#8181=EDGE_CURVE('',#5832,#5827,#2561,.T.);
#8182=EDGE_CURVE('',#5833,#5826,#2562,.T.);
#8183=EDGE_CURVE('',#5830,#5833,#2563,.T.);
#8184=EDGE_CURVE('',#5834,#5835,#4115,.T.);
#8185=EDGE_CURVE('',#5835,#5836,#2564,.T.);
#8186=EDGE_CURVE('',#5836,#5831,#2565,.T.);
#8187=EDGE_CURVE('',#5837,#5830,#2566,.T.);
#8188=EDGE_CURVE('',#5834,#5837,#2567,.T.);
#8189=EDGE_CURVE('',#5838,#5839,#4116,.T.);
#8190=EDGE_CURVE('',#5839,#5840,#2568,.T.);
#8191=EDGE_CURVE('',#5840,#5835,#2569,.T.);
#8192=EDGE_CURVE('',#5841,#5834,#2570,.T.);
#8193=EDGE_CURVE('',#5838,#5841,#2571,.T.);
#8194=EDGE_CURVE('',#5842,#5843,#4117,.T.);
#8195=EDGE_CURVE('',#5843,#5844,#2572,.T.);
#8196=EDGE_CURVE('',#5844,#5839,#2573,.T.);
#8197=EDGE_CURVE('',#5845,#5838,#2574,.T.);
#8198=EDGE_CURVE('',#5842,#5845,#2575,.T.);
#8199=EDGE_CURVE('',#5846,#5847,#4118,.T.);
#8200=EDGE_CURVE('',#5848,#5846,#2576,.T.);
#8201=EDGE_CURVE('',#5849,#5848,#2577,.T.);
#8202=EDGE_CURVE('',#5850,#5849,#1852,.T.);
#8203=EDGE_CURVE('',#5850,#5851,#2578,.T.);
#8204=EDGE_CURVE('',#5851,#5847,#2579,.T.);
#8205=EDGE_CURVE('',#5852,#5853,#4119,.T.);
#8206=EDGE_CURVE('',#5853,#5854,#2580,.T.);
#8207=EDGE_CURVE('',#5855,#5854,#1853,.T.);
#8208=EDGE_CURVE('',#5856,#5855,#2581,.T.);
#8209=EDGE_CURVE('',#5852,#5856,#2582,.T.);
#8210=EDGE_CURVE('',#5857,#5858,#4120,.T.);
#8211=EDGE_CURVE('',#5858,#5859,#2583,.T.);
#8212=EDGE_CURVE('',#5859,#5853,#2584,.T.);
#8213=EDGE_CURVE('',#5860,#5852,#2585,.T.);
#8214=EDGE_CURVE('',#5857,#5860,#2586,.T.);
#8215=EDGE_CURVE('',#5861,#5862,#4121,.T.);
#8216=EDGE_CURVE('',#5862,#5863,#2587,.T.);
#8217=EDGE_CURVE('',#5863,#5858,#2588,.T.);
#8218=EDGE_CURVE('',#5864,#5857,#2589,.T.);
#8219=EDGE_CURVE('',#5861,#5864,#2590,.T.);
#8220=EDGE_CURVE('',#5865,#5866,#4122,.T.);
#8221=EDGE_CURVE('',#5866,#5867,#2591,.T.);
#8222=EDGE_CURVE('',#5867,#5862,#2592,.T.);
#8223=EDGE_CURVE('',#5868,#5861,#2593,.T.);
#8224=EDGE_CURVE('',#5865,#5868,#2594,.T.);
#8225=EDGE_CURVE('',#5869,#5870,#4123,.T.);
#8226=EDGE_CURVE('',#5870,#5871,#2595,.T.);
#8227=EDGE_CURVE('',#5871,#5866,#2596,.T.);
#8228=EDGE_CURVE('',#5872,#5865,#2597,.T.);
#8229=EDGE_CURVE('',#5869,#5872,#2598,.T.);
#8230=EDGE_CURVE('',#5873,#5874,#4124,.T.);
#8231=EDGE_CURVE('',#5874,#5875,#2599,.T.);
#8232=EDGE_CURVE('',#5875,#5870,#2600,.T.);
#8233=EDGE_CURVE('',#5876,#5869,#2601,.T.);
#8234=EDGE_CURVE('',#5873,#5876,#2602,.T.);
#8235=EDGE_CURVE('',#5877,#5878,#4125,.T.);
#8236=EDGE_CURVE('',#5878,#5879,#2603,.T.);
#8237=EDGE_CURVE('',#5879,#5874,#2604,.T.);
#8238=EDGE_CURVE('',#5880,#5873,#2605,.T.);
#8239=EDGE_CURVE('',#5877,#5880,#2606,.T.);
#8240=EDGE_CURVE('',#5881,#5882,#4126,.T.);
#8241=EDGE_CURVE('',#5882,#5883,#2607,.T.);
#8242=EDGE_CURVE('',#5883,#5878,#2608,.T.);
#8243=EDGE_CURVE('',#5884,#5877,#2609,.T.);
#8244=EDGE_CURVE('',#5881,#5884,#2610,.T.);
#8245=EDGE_CURVE('',#5885,#5886,#4127,.T.);
#8246=EDGE_CURVE('',#5886,#5887,#2611,.T.);
#8247=EDGE_CURVE('',#5887,#5882,#2612,.T.);
#8248=EDGE_CURVE('',#5888,#5881,#2613,.T.);
#8249=EDGE_CURVE('',#5885,#5888,#2614,.T.);
#8250=EDGE_CURVE('',#5889,#5890,#4128,.T.);
#8251=EDGE_CURVE('',#5890,#5891,#2615,.T.);
#8252=EDGE_CURVE('',#5891,#5886,#2616,.T.);
#8253=EDGE_CURVE('',#5892,#5885,#2617,.T.);
#8254=EDGE_CURVE('',#5889,#5892,#2618,.T.);
#8255=EDGE_CURVE('',#5893,#5894,#4129,.T.);
#8256=EDGE_CURVE('',#5894,#5895,#2619,.T.);
#8257=EDGE_CURVE('',#5895,#5890,#2620,.T.);
#8258=EDGE_CURVE('',#5896,#5889,#2621,.T.);
#8259=EDGE_CURVE('',#5893,#5896,#2622,.T.);
#8260=EDGE_CURVE('',#5897,#5898,#4130,.T.);
#8261=EDGE_CURVE('',#5898,#5899,#2623,.T.);
#8262=EDGE_CURVE('',#5899,#5894,#2624,.T.);
#8263=EDGE_CURVE('',#5900,#5893,#2625,.T.);
#8264=EDGE_CURVE('',#5897,#5900,#2626,.T.);
#8265=EDGE_CURVE('',#5901,#5902,#4131,.T.);
#8266=EDGE_CURVE('',#5902,#5903,#2627,.T.);
#8267=EDGE_CURVE('',#5903,#5898,#2628,.T.);
#8268=EDGE_CURVE('',#5904,#5897,#2629,.T.);
#8269=EDGE_CURVE('',#5901,#5904,#2630,.T.);
#8270=EDGE_CURVE('',#5905,#5906,#4132,.T.);
#8271=EDGE_CURVE('',#5907,#5905,#2631,.T.);
#8272=EDGE_CURVE('',#5908,#5907,#2632,.T.);
#8273=EDGE_CURVE('',#5909,#5908,#1854,.T.);
#8274=EDGE_CURVE('',#5909,#5910,#2633,.T.);
#8275=EDGE_CURVE('',#5910,#5906,#2634,.T.);
#8276=EDGE_CURVE('',#5911,#5912,#4133,.T.);
#8277=EDGE_CURVE('',#5912,#5913,#2635,.T.);
#8278=EDGE_CURVE('',#5914,#5913,#1855,.T.);
#8279=EDGE_CURVE('',#5915,#5914,#2636,.T.);
#8280=EDGE_CURVE('',#5911,#5915,#2637,.T.);
#8281=EDGE_CURVE('',#5916,#5917,#4134,.T.);
#8282=EDGE_CURVE('',#5917,#5918,#2638,.T.);
#8283=EDGE_CURVE('',#5918,#5912,#2639,.T.);
#8284=EDGE_CURVE('',#5919,#5911,#2640,.T.);
#8285=EDGE_CURVE('',#5916,#5919,#2641,.T.);
#8286=EDGE_CURVE('',#5920,#5921,#4135,.T.);
#8287=EDGE_CURVE('',#5921,#5922,#2642,.T.);
#8288=EDGE_CURVE('',#5922,#5917,#2643,.T.);
#8289=EDGE_CURVE('',#5923,#5916,#2644,.T.);
#8290=EDGE_CURVE('',#5920,#5923,#2645,.T.);
#8291=EDGE_CURVE('',#5924,#5925,#4136,.T.);
#8292=EDGE_CURVE('',#5925,#5926,#2646,.T.);
#8293=EDGE_CURVE('',#5926,#5921,#2647,.T.);
#8294=EDGE_CURVE('',#5927,#5920,#2648,.T.);
#8295=EDGE_CURVE('',#5924,#5927,#2649,.T.);
#8296=EDGE_CURVE('',#5928,#5929,#4137,.T.);
#8297=EDGE_CURVE('',#5929,#5930,#2650,.T.);
#8298=EDGE_CURVE('',#5930,#5925,#2651,.T.);
#8299=EDGE_CURVE('',#5931,#5924,#2652,.T.);
#8300=EDGE_CURVE('',#5928,#5931,#2653,.T.);
#8301=EDGE_CURVE('',#5932,#5933,#4138,.T.);
#8302=EDGE_CURVE('',#5933,#5934,#2654,.T.);
#8303=EDGE_CURVE('',#5934,#5929,#2655,.T.);
#8304=EDGE_CURVE('',#5935,#5928,#2656,.T.);
#8305=EDGE_CURVE('',#5932,#5935,#2657,.T.);
#8306=EDGE_CURVE('',#5936,#5937,#4139,.T.);
#8307=EDGE_CURVE('',#5937,#5938,#2658,.T.);
#8308=EDGE_CURVE('',#5938,#5933,#2659,.T.);
#8309=EDGE_CURVE('',#5939,#5932,#2660,.T.);
#8310=EDGE_CURVE('',#5936,#5939,#2661,.T.);
#8311=EDGE_CURVE('',#5940,#5941,#4140,.T.);
#8312=EDGE_CURVE('',#5941,#5942,#2662,.T.);
#8313=EDGE_CURVE('',#5942,#5937,#2663,.T.);
#8314=EDGE_CURVE('',#5943,#5936,#2664,.T.);
#8315=EDGE_CURVE('',#5940,#5943,#2665,.T.);
#8316=EDGE_CURVE('',#5944,#5945,#4141,.T.);
#8317=EDGE_CURVE('',#5945,#5946,#2666,.T.);
#8318=EDGE_CURVE('',#5946,#5941,#2667,.T.);
#8319=EDGE_CURVE('',#5947,#5940,#2668,.T.);
#8320=EDGE_CURVE('',#5944,#5947,#2669,.T.);
#8321=EDGE_CURVE('',#5948,#5949,#4142,.T.);
#8322=EDGE_CURVE('',#5949,#5950,#2670,.T.);
#8323=EDGE_CURVE('',#5950,#5945,#2671,.T.);
#8324=EDGE_CURVE('',#5951,#5944,#2672,.T.);
#8325=EDGE_CURVE('',#5948,#5951,#2673,.T.);
#8326=EDGE_CURVE('',#5952,#5953,#4143,.T.);
#8327=EDGE_CURVE('',#5953,#5954,#2674,.T.);
#8328=EDGE_CURVE('',#5954,#5949,#2675,.T.);
#8329=EDGE_CURVE('',#5955,#5948,#2676,.T.);
#8330=EDGE_CURVE('',#5952,#5955,#2677,.T.);
#8331=EDGE_CURVE('',#5956,#5957,#4144,.T.);
#8332=EDGE_CURVE('',#5957,#5958,#2678,.T.);
#8333=EDGE_CURVE('',#5958,#5953,#2679,.T.);
#8334=EDGE_CURVE('',#5959,#5952,#2680,.T.);
#8335=EDGE_CURVE('',#5956,#5959,#2681,.T.);
#8336=EDGE_CURVE('',#5960,#5961,#4145,.T.);
#8337=EDGE_CURVE('',#5961,#5962,#2682,.T.);
#8338=EDGE_CURVE('',#5962,#5957,#2683,.T.);
#8339=EDGE_CURVE('',#5963,#5956,#2684,.T.);
#8340=EDGE_CURVE('',#5960,#5963,#2685,.T.);
#8341=EDGE_CURVE('',#5964,#5965,#4146,.T.);
#8342=EDGE_CURVE('',#5966,#5964,#2686,.T.);
#8343=EDGE_CURVE('',#5967,#5966,#2687,.T.);
#8344=EDGE_CURVE('',#5968,#5967,#1856,.T.);
#8345=EDGE_CURVE('',#5968,#5969,#2688,.T.);
#8346=EDGE_CURVE('',#5969,#5965,#2689,.T.);
#8347=EDGE_CURVE('',#5970,#5971,#4147,.T.);
#8348=EDGE_CURVE('',#5971,#5972,#2690,.T.);
#8349=EDGE_CURVE('',#5973,#5972,#1857,.T.);
#8350=EDGE_CURVE('',#5974,#5973,#2691,.T.);
#8351=EDGE_CURVE('',#5970,#5974,#2692,.T.);
#8352=EDGE_CURVE('',#5975,#5976,#4148,.T.);
#8353=EDGE_CURVE('',#5976,#5977,#2693,.T.);
#8354=EDGE_CURVE('',#5977,#5971,#2694,.T.);
#8355=EDGE_CURVE('',#5978,#5970,#2695,.T.);
#8356=EDGE_CURVE('',#5975,#5978,#2696,.T.);
#8357=EDGE_CURVE('',#5979,#5980,#4149,.T.);
#8358=EDGE_CURVE('',#5980,#5981,#2697,.T.);
#8359=EDGE_CURVE('',#5981,#5976,#2698,.T.);
#8360=EDGE_CURVE('',#5982,#5975,#2699,.T.);
#8361=EDGE_CURVE('',#5979,#5982,#2700,.T.);
#8362=EDGE_CURVE('',#5983,#5984,#4150,.T.);
#8363=EDGE_CURVE('',#5984,#5985,#2701,.T.);
#8364=EDGE_CURVE('',#5985,#5980,#2702,.T.);
#8365=EDGE_CURVE('',#5986,#5979,#2703,.T.);
#8366=EDGE_CURVE('',#5983,#5986,#2704,.T.);
#8367=EDGE_CURVE('',#5987,#5988,#4151,.T.);
#8368=EDGE_CURVE('',#5988,#5989,#2705,.T.);
#8369=EDGE_CURVE('',#5989,#5984,#2706,.T.);
#8370=EDGE_CURVE('',#5990,#5983,#2707,.T.);
#8371=EDGE_CURVE('',#5987,#5990,#2708,.T.);
#8372=EDGE_CURVE('',#5991,#5992,#4152,.T.);
#8373=EDGE_CURVE('',#5992,#5993,#2709,.T.);
#8374=EDGE_CURVE('',#5993,#5988,#2710,.T.);
#8375=EDGE_CURVE('',#5994,#5987,#2711,.T.);
#8376=EDGE_CURVE('',#5991,#5994,#2712,.T.);
#8377=EDGE_CURVE('',#5995,#5996,#4153,.T.);
#8378=EDGE_CURVE('',#5996,#5997,#2713,.T.);
#8379=EDGE_CURVE('',#5997,#5992,#2714,.T.);
#8380=EDGE_CURVE('',#5998,#5991,#2715,.T.);
#8381=EDGE_CURVE('',#5995,#5998,#2716,.T.);
#8382=EDGE_CURVE('',#5999,#6000,#4154,.T.);
#8383=EDGE_CURVE('',#6000,#6001,#2717,.T.);
#8384=EDGE_CURVE('',#6001,#5996,#2718,.T.);
#8385=EDGE_CURVE('',#6002,#5995,#2719,.T.);
#8386=EDGE_CURVE('',#5999,#6002,#2720,.T.);
#8387=EDGE_CURVE('',#6003,#6004,#4155,.T.);
#8388=EDGE_CURVE('',#6004,#6005,#2721,.T.);
#8389=EDGE_CURVE('',#6005,#6000,#2722,.T.);
#8390=EDGE_CURVE('',#6006,#5999,#2723,.T.);
#8391=EDGE_CURVE('',#6003,#6006,#2724,.T.);
#8392=EDGE_CURVE('',#6007,#6008,#4156,.T.);
#8393=EDGE_CURVE('',#6008,#6009,#2725,.T.);
#8394=EDGE_CURVE('',#6009,#6004,#2726,.T.);
#8395=EDGE_CURVE('',#6010,#6003,#2727,.T.);
#8396=EDGE_CURVE('',#6007,#6010,#2728,.T.);
#8397=EDGE_CURVE('',#6011,#6012,#4157,.T.);
#8398=EDGE_CURVE('',#6012,#6013,#2729,.T.);
#8399=EDGE_CURVE('',#6013,#6008,#2730,.T.);
#8400=EDGE_CURVE('',#6014,#6007,#2731,.T.);
#8401=EDGE_CURVE('',#6011,#6014,#2732,.T.);
#8402=EDGE_CURVE('',#6015,#6016,#4158,.T.);
#8403=EDGE_CURVE('',#6016,#6017,#2733,.T.);
#8404=EDGE_CURVE('',#6017,#6012,#2734,.T.);
#8405=EDGE_CURVE('',#6018,#6011,#2735,.T.);
#8406=EDGE_CURVE('',#6015,#6018,#2736,.T.);
#8407=EDGE_CURVE('',#6019,#6020,#4159,.T.);
#8408=EDGE_CURVE('',#6020,#6021,#2737,.T.);
#8409=EDGE_CURVE('',#6021,#6016,#2738,.T.);
#8410=EDGE_CURVE('',#6022,#6015,#2739,.T.);
#8411=EDGE_CURVE('',#6019,#6022,#2740,.T.);
#8412=EDGE_CURVE('',#6023,#6024,#4160,.T.);
#8413=EDGE_CURVE('',#6025,#6023,#2741,.T.);
#8414=EDGE_CURVE('',#6026,#6025,#2742,.T.);
#8415=EDGE_CURVE('',#6027,#6026,#1858,.T.);
#8416=EDGE_CURVE('',#6027,#6028,#2743,.T.);
#8417=EDGE_CURVE('',#6028,#6024,#2744,.T.);
#8418=EDGE_CURVE('',#6029,#6030,#4161,.T.);
#8419=EDGE_CURVE('',#6030,#6031,#2745,.T.);
#8420=EDGE_CURVE('',#6031,#6032,#1859,.F.);
#8421=EDGE_CURVE('',#6032,#6029,#2746,.T.);
#8422=EDGE_CURVE('',#6033,#6034,#4162,.T.);
#8423=EDGE_CURVE('',#6034,#6035,#2747,.T.);
#8424=EDGE_CURVE('',#6035,#6030,#2748,.T.);
#8425=EDGE_CURVE('',#6029,#6033,#2749,.T.);
#8426=EDGE_CURVE('',#6036,#6037,#4163,.T.);
#8427=EDGE_CURVE('',#6037,#6034,#2750,.T.);
#8428=EDGE_CURVE('',#6033,#6038,#2751,.T.);
#8429=EDGE_CURVE('',#6038,#6036,#2752,.T.);
#8430=EDGE_CURVE('',#6039,#6040,#4164,.T.);
#8431=EDGE_CURVE('',#6040,#6041,#2753,.T.);
#8432=EDGE_CURVE('',#6041,#6037,#2754,.T.);
#8433=EDGE_CURVE('',#6036,#6039,#2755,.T.);
#8434=EDGE_CURVE('',#6042,#6043,#4165,.T.);
#8435=EDGE_CURVE('',#6043,#6040,#2756,.T.);
#8436=EDGE_CURVE('',#6039,#6044,#2757,.T.);
#8437=EDGE_CURVE('',#6044,#6042,#2758,.T.);
#8438=EDGE_CURVE('',#6045,#6046,#4166,.T.);
#8439=EDGE_CURVE('',#6046,#6047,#2759,.T.);
#8440=EDGE_CURVE('',#6047,#6043,#2760,.T.);
#8441=EDGE_CURVE('',#6042,#6045,#2761,.T.);
#8442=EDGE_CURVE('',#6048,#6049,#4167,.T.);
#8443=EDGE_CURVE('',#6049,#6046,#2762,.T.);
#8444=EDGE_CURVE('',#6045,#6050,#2763,.T.);
#8445=EDGE_CURVE('',#6050,#6048,#2764,.T.);
#8446=EDGE_CURVE('',#6051,#6052,#4168,.T.);
#8447=EDGE_CURVE('',#6052,#6053,#2765,.T.);
#8448=EDGE_CURVE('',#6053,#6049,#2766,.T.);
#8449=EDGE_CURVE('',#6048,#6054,#2767,.T.);
#8450=EDGE_CURVE('',#6054,#6051,#2768,.T.);
#8451=EDGE_CURVE('',#6055,#6056,#4169,.T.);
#8452=EDGE_CURVE('',#6056,#6052,#2769,.T.);
#8453=EDGE_CURVE('',#6051,#6057,#2770,.T.);
#8454=EDGE_CURVE('',#6057,#6055,#2771,.T.);
#8455=EDGE_CURVE('',#6058,#6059,#4170,.T.);
#8456=EDGE_CURVE('',#6059,#6060,#2772,.T.);
#8457=EDGE_CURVE('',#6060,#6056,#2773,.T.);
#8458=EDGE_CURVE('',#6055,#6058,#2774,.T.);
#8459=EDGE_CURVE('',#6061,#6062,#4171,.T.);
#8460=EDGE_CURVE('',#6062,#6059,#2775,.T.);
#8461=EDGE_CURVE('',#6058,#6063,#2776,.T.);
#8462=EDGE_CURVE('',#6063,#6061,#2777,.T.);
#8463=EDGE_CURVE('',#6064,#6065,#4172,.T.);
#8464=EDGE_CURVE('',#6065,#6066,#2778,.T.);
#8465=EDGE_CURVE('',#6066,#6062,#2779,.T.);
#8466=EDGE_CURVE('',#6061,#6064,#2780,.T.);
#8467=EDGE_CURVE('',#6067,#6068,#4173,.T.);
#8468=EDGE_CURVE('',#6068,#6065,#2781,.T.);
#8469=EDGE_CURVE('',#6064,#6069,#2782,.T.);
#8470=EDGE_CURVE('',#6069,#6067,#2783,.T.);
#8471=EDGE_CURVE('',#6070,#6071,#4174,.T.);
#8472=EDGE_CURVE('',#6070,#6072,#2784,.T.);
#8473=EDGE_CURVE('',#6072,#6073,#2785,.T.);
#8474=EDGE_CURVE('',#6074,#6073,#1860,.T.);
#8475=EDGE_CURVE('',#6074,#6071,#2786,.T.);
#8476=EDGE_CURVE('',#6075,#6076,#4175,.T.);
#8477=EDGE_CURVE('',#6076,#6077,#2787,.T.);
#8478=EDGE_CURVE('',#6077,#6078,#1861,.F.);
#8479=EDGE_CURVE('',#6078,#6075,#2788,.T.);
#8480=EDGE_CURVE('',#6079,#6080,#4176,.T.);
#8481=EDGE_CURVE('',#6080,#6081,#2789,.T.);
#8482=EDGE_CURVE('',#6081,#6076,#2790,.T.);
#8483=EDGE_CURVE('',#6075,#6079,#2791,.T.);
#8484=EDGE_CURVE('',#6082,#6083,#4177,.T.);
#8485=EDGE_CURVE('',#6083,#6080,#2792,.T.);
#8486=EDGE_CURVE('',#6079,#6084,#2793,.T.);
#8487=EDGE_CURVE('',#6084,#6082,#2794,.T.);
#8488=EDGE_CURVE('',#6085,#6086,#4178,.T.);
#8489=EDGE_CURVE('',#6086,#6087,#2795,.T.);
#8490=EDGE_CURVE('',#6087,#6083,#2796,.T.);
#8491=EDGE_CURVE('',#6082,#6085,#2797,.T.);
#8492=EDGE_CURVE('',#6088,#6089,#4179,.T.);
#8493=EDGE_CURVE('',#6089,#6086,#2798,.T.);
#8494=EDGE_CURVE('',#6085,#6090,#2799,.T.);
#8495=EDGE_CURVE('',#6090,#6088,#2800,.T.);
#8496=EDGE_CURVE('',#6091,#6092,#4180,.T.);
#8497=EDGE_CURVE('',#6092,#6093,#2801,.T.);
#8498=EDGE_CURVE('',#6093,#6089,#2802,.T.);
#8499=EDGE_CURVE('',#6088,#6091,#2803,.T.);
#8500=EDGE_CURVE('',#6094,#6095,#4181,.T.);
#8501=EDGE_CURVE('',#6095,#6092,#2804,.T.);
#8502=EDGE_CURVE('',#6091,#6096,#2805,.T.);
#8503=EDGE_CURVE('',#6096,#6094,#2806,.T.);
#8504=EDGE_CURVE('',#6097,#6098,#4182,.T.);
#8505=EDGE_CURVE('',#6098,#6099,#2807,.T.);
#8506=EDGE_CURVE('',#6099,#6095,#2808,.T.);
#8507=EDGE_CURVE('',#6094,#6100,#2809,.T.);
#8508=EDGE_CURVE('',#6100,#6097,#2810,.T.);
#8509=EDGE_CURVE('',#6101,#6102,#4183,.T.);
#8510=EDGE_CURVE('',#6102,#6098,#2811,.T.);
#8511=EDGE_CURVE('',#6097,#6103,#2812,.T.);
#8512=EDGE_CURVE('',#6103,#6101,#2813,.T.);
#8513=EDGE_CURVE('',#6104,#6105,#4184,.T.);
#8514=EDGE_CURVE('',#6105,#6106,#2814,.T.);
#8515=EDGE_CURVE('',#6106,#6102,#2815,.T.);
#8516=EDGE_CURVE('',#6101,#6104,#2816,.T.);
#8517=EDGE_CURVE('',#6107,#6108,#4185,.T.);
#8518=EDGE_CURVE('',#6108,#6105,#2817,.T.);
#8519=EDGE_CURVE('',#6104,#6109,#2818,.T.);
#8520=EDGE_CURVE('',#6109,#6107,#2819,.T.);
#8521=EDGE_CURVE('',#6110,#6111,#4186,.T.);
#8522=EDGE_CURVE('',#6111,#6112,#2820,.T.);
#8523=EDGE_CURVE('',#6112,#6108,#2821,.T.);
#8524=EDGE_CURVE('',#6107,#6110,#2822,.T.);
#8525=EDGE_CURVE('',#6113,#6114,#4187,.T.);
#8526=EDGE_CURVE('',#6114,#6111,#2823,.T.);
#8527=EDGE_CURVE('',#6110,#6115,#2824,.T.);
#8528=EDGE_CURVE('',#6115,#6113,#2825,.T.);
#8529=EDGE_CURVE('',#6116,#6117,#4188,.T.);
#8530=EDGE_CURVE('',#6116,#6118,#2826,.T.);
#8531=EDGE_CURVE('',#6118,#6119,#2827,.T.);
#8532=EDGE_CURVE('',#6120,#6119,#1862,.T.);
#8533=EDGE_CURVE('',#6120,#6117,#2828,.T.);
#8534=EDGE_CURVE('',#6121,#6122,#4189,.T.);
#8535=EDGE_CURVE('',#6122,#6123,#2829,.T.);
#8536=EDGE_CURVE('',#6123,#6124,#1863,.F.);
#8537=EDGE_CURVE('',#6124,#6121,#2830,.T.);
#8538=EDGE_CURVE('',#6125,#6126,#4190,.T.);
#8539=EDGE_CURVE('',#6126,#6122,#2831,.T.);
#8540=EDGE_CURVE('',#6121,#6125,#2832,.T.);
#8541=EDGE_CURVE('',#6127,#6128,#4191,.T.);
#8542=EDGE_CURVE('',#6128,#6126,#2833,.T.);
#8543=EDGE_CURVE('',#6125,#6129,#2834,.T.);
#8544=EDGE_CURVE('',#6129,#6127,#2835,.T.);
#8545=EDGE_CURVE('',#6130,#6131,#4192,.T.);
#8546=EDGE_CURVE('',#6131,#6128,#2836,.T.);
#8547=EDGE_CURVE('',#6127,#6130,#2837,.T.);
#8548=EDGE_CURVE('',#6132,#6133,#4193,.T.);
#8549=EDGE_CURVE('',#6133,#6131,#2838,.T.);
#8550=EDGE_CURVE('',#6130,#6134,#2839,.T.);
#8551=EDGE_CURVE('',#6134,#6132,#2840,.T.);
#8552=EDGE_CURVE('',#6135,#6136,#4194,.T.);
#8553=EDGE_CURVE('',#6136,#6137,#2841,.T.);
#8554=EDGE_CURVE('',#6137,#6133,#2842,.T.);
#8555=EDGE_CURVE('',#6132,#6135,#2843,.T.);
#8556=EDGE_CURVE('',#6138,#6139,#4195,.T.);
#8557=EDGE_CURVE('',#6139,#6136,#2844,.T.);
#8558=EDGE_CURVE('',#6135,#6140,#2845,.T.);
#8559=EDGE_CURVE('',#6140,#6138,#2846,.T.);
#8560=EDGE_CURVE('',#6141,#6142,#4196,.T.);
#8561=EDGE_CURVE('',#6142,#6143,#2847,.T.);
#8562=EDGE_CURVE('',#6143,#6139,#2848,.T.);
#8563=EDGE_CURVE('',#6138,#6144,#2849,.T.);
#8564=EDGE_CURVE('',#6144,#6141,#2850,.T.);
#8565=EDGE_CURVE('',#6145,#6146,#4197,.T.);
#8566=EDGE_CURVE('',#6146,#6142,#2851,.T.);
#8567=EDGE_CURVE('',#6141,#6147,#2852,.T.);
#8568=EDGE_CURVE('',#6147,#6145,#2853,.T.);
#8569=EDGE_CURVE('',#6148,#6149,#4198,.T.);
#8570=EDGE_CURVE('',#6149,#6150,#2854,.T.);
#8571=EDGE_CURVE('',#6150,#6146,#2855,.T.);
#8572=EDGE_CURVE('',#6145,#6148,#2856,.T.);
#8573=EDGE_CURVE('',#6151,#6152,#4199,.T.);
#8574=EDGE_CURVE('',#6152,#6149,#2857,.T.);
#8575=EDGE_CURVE('',#6148,#6153,#2858,.T.);
#8576=EDGE_CURVE('',#6153,#6151,#2859,.T.);
#8577=EDGE_CURVE('',#6154,#6155,#4200,.T.);
#8578=EDGE_CURVE('',#6155,#6156,#2860,.T.);
#8579=EDGE_CURVE('',#6156,#6152,#2861,.T.);
#8580=EDGE_CURVE('',#6151,#6154,#2862,.T.);
#8581=EDGE_CURVE('',#6157,#6158,#4201,.T.);
#8582=EDGE_CURVE('',#6158,#6155,#2863,.T.);
#8583=EDGE_CURVE('',#6154,#6157,#2864,.T.);
#8584=EDGE_CURVE('',#6159,#6160,#4202,.T.);
#8585=EDGE_CURVE('',#6159,#6161,#2865,.T.);
#8586=EDGE_CURVE('',#6162,#6161,#1864,.T.);
#8587=EDGE_CURVE('',#6162,#6160,#2866,.T.);
#8588=EDGE_CURVE('',#6163,#6164,#4203,.T.);
#8589=EDGE_CURVE('',#6164,#6165,#2867,.T.);
#8590=EDGE_CURVE('',#6165,#6166,#1865,.F.);
#8591=EDGE_CURVE('',#6166,#6163,#2868,.T.);
#8592=EDGE_CURVE('',#6167,#6168,#4204,.T.);
#8593=EDGE_CURVE('',#6168,#6164,#2869,.T.);
#8594=EDGE_CURVE('',#6163,#6167,#2870,.T.);
#8595=EDGE_CURVE('',#6169,#6170,#4205,.T.);
#8596=EDGE_CURVE('',#6170,#6168,#2871,.T.);
#8597=EDGE_CURVE('',#6167,#6171,#2872,.T.);
#8598=EDGE_CURVE('',#6171,#6169,#2873,.T.);
#8599=EDGE_CURVE('',#6172,#6173,#4206,.T.);
#8600=EDGE_CURVE('',#6173,#6170,#2874,.T.);
#8601=EDGE_CURVE('',#6169,#6172,#2875,.T.);
#8602=EDGE_CURVE('',#6174,#6175,#4207,.T.);
#8603=EDGE_CURVE('',#6175,#6173,#2876,.T.);
#8604=EDGE_CURVE('',#6172,#6176,#2877,.T.);
#8605=EDGE_CURVE('',#6176,#6174,#2878,.T.);
#8606=EDGE_CURVE('',#6177,#6178,#4208,.T.);
#8607=EDGE_CURVE('',#6178,#6179,#2879,.T.);
#8608=EDGE_CURVE('',#6179,#6175,#2880,.T.);
#8609=EDGE_CURVE('',#6174,#6177,#2881,.T.);
#8610=EDGE_CURVE('',#6180,#6181,#4209,.T.);
#8611=EDGE_CURVE('',#6181,#6178,#2882,.T.);
#8612=EDGE_CURVE('',#6177,#6182,#2883,.T.);
#8613=EDGE_CURVE('',#6182,#6180,#2884,.T.);
#8614=EDGE_CURVE('',#6183,#6184,#4210,.T.);
#8615=EDGE_CURVE('',#6184,#6185,#2885,.T.);
#8616=EDGE_CURVE('',#6185,#6181,#2886,.T.);
#8617=EDGE_CURVE('',#6180,#6186,#2887,.T.);
#8618=EDGE_CURVE('',#6186,#6183,#2888,.T.);
#8619=EDGE_CURVE('',#6187,#6188,#4211,.T.);
#8620=EDGE_CURVE('',#6188,#6184,#2889,.T.);
#8621=EDGE_CURVE('',#6183,#6189,#2890,.T.);
#8622=EDGE_CURVE('',#6189,#6187,#2891,.T.);
#8623=EDGE_CURVE('',#6190,#6191,#4212,.T.);
#8624=EDGE_CURVE('',#6191,#6192,#2892,.T.);
#8625=EDGE_CURVE('',#6192,#6188,#2893,.T.);
#8626=EDGE_CURVE('',#6187,#6190,#2894,.T.);
#8627=EDGE_CURVE('',#6193,#6194,#4213,.T.);
#8628=EDGE_CURVE('',#6194,#6191,#2895,.T.);
#8629=EDGE_CURVE('',#6190,#6195,#2896,.T.);
#8630=EDGE_CURVE('',#6195,#6193,#2897,.T.);
#8631=EDGE_CURVE('',#6196,#6197,#4214,.T.);
#8632=EDGE_CURVE('',#6197,#6198,#2898,.T.);
#8633=EDGE_CURVE('',#6198,#6194,#2899,.T.);
#8634=EDGE_CURVE('',#6193,#6196,#2900,.T.);
#8635=EDGE_CURVE('',#6199,#6200,#4215,.T.);
#8636=EDGE_CURVE('',#6200,#6197,#2901,.T.);
#8637=EDGE_CURVE('',#6196,#6199,#2902,.T.);
#8638=EDGE_CURVE('',#6201,#6202,#4216,.T.);
#8639=EDGE_CURVE('',#6201,#6203,#2903,.T.);
#8640=EDGE_CURVE('',#6204,#6203,#1866,.T.);
#8641=EDGE_CURVE('',#6204,#6202,#2904,.T.);
#8642=EDGE_CURVE('',#6202,#6205,#2905,.T.);
#8643=EDGE_CURVE('',#6205,#6200,#2906,.T.);
#8644=EDGE_CURVE('',#6199,#6201,#2907,.T.);
#8645=EDGE_CURVE('',#6160,#6206,#2908,.T.);
#8646=EDGE_CURVE('',#6206,#6158,#2909,.T.);
#8647=EDGE_CURVE('',#6157,#6159,#2910,.T.);
#8648=EDGE_CURVE('',#6117,#6207,#2911,.T.);
#8649=EDGE_CURVE('',#6207,#6114,#2912,.T.);
#8650=EDGE_CURVE('',#6113,#6116,#2913,.T.);
#8651=EDGE_CURVE('',#6071,#6208,#2914,.T.);
#8652=EDGE_CURVE('',#6208,#6068,#2915,.T.);
#8653=EDGE_CURVE('',#6067,#6070,#2916,.T.);
#8654=EDGE_CURVE('',#6024,#6209,#2917,.T.);
#8655=EDGE_CURVE('',#6209,#6020,#2918,.T.);
#8656=EDGE_CURVE('',#6210,#6019,#2919,.T.);
#8657=EDGE_CURVE('',#6023,#6210,#2920,.T.);
#8658=EDGE_CURVE('',#5965,#6211,#2921,.T.);
#8659=EDGE_CURVE('',#6211,#5961,#2922,.T.);
#8660=EDGE_CURVE('',#6212,#5960,#2923,.T.);
#8661=EDGE_CURVE('',#5964,#6212,#2924,.T.);
#8662=EDGE_CURVE('',#5906,#6213,#2925,.T.);
#8663=EDGE_CURVE('',#6213,#5902,#2926,.T.);
#8664=EDGE_CURVE('',#6214,#5901,#2927,.T.);
#8665=EDGE_CURVE('',#5905,#6214,#2928,.T.);
#8666=EDGE_CURVE('',#5847,#6215,#2929,.T.);
#8667=EDGE_CURVE('',#6215,#5843,#2930,.T.);
#8668=EDGE_CURVE('',#6216,#5842,#2931,.T.);
#8669=EDGE_CURVE('',#5846,#6216,#2932,.T.);
#8670=EDGE_CURVE('',#5790,#6217,#2933,.T.);
#8671=EDGE_CURVE('',#6217,#5788,#2934,.T.);
#8672=EDGE_CURVE('',#5787,#5789,#2935,.T.);
#8673=EDGE_CURVE('',#5739,#6218,#2936,.T.);
#8674=EDGE_CURVE('',#6218,#5735,#2937,.T.);
#8675=EDGE_CURVE('',#6219,#5734,#2938,.T.);
#8676=EDGE_CURVE('',#5738,#6219,#2939,.T.);
#8677=EDGE_CURVE('',#5675,#6220,#2940,.T.);
#8678=EDGE_CURVE('',#6220,#5673,#2941,.T.);
#8679=EDGE_CURVE('',#5672,#5674,#2942,.T.);
#8680=EDGE_CURVE('',#5624,#6221,#2943,.T.);
#8681=EDGE_CURVE('',#6221,#5620,#2944,.T.);
#8682=EDGE_CURVE('',#6222,#5619,#2945,.T.);
#8683=EDGE_CURVE('',#5623,#6222,#2946,.T.);
#8684=EDGE_CURVE('',#5631,#5566,#2947,.T.);
#8685=EDGE_CURVE('',#5565,#5632,#2948,.T.);
#8686=EDGE_CURVE('',#5676,#5627,#2949,.T.);
#8687=EDGE_CURVE('',#6223,#5677,#2950,.T.);
#8688=EDGE_CURVE('',#5626,#6223,#2951,.T.);
#8689=EDGE_CURVE('',#5746,#5681,#2952,.T.);
#8690=EDGE_CURVE('',#5680,#5747,#2953,.T.);
#8691=EDGE_CURVE('',#5791,#5742,#2954,.T.);
#8692=EDGE_CURVE('',#6224,#5792,#2955,.T.);
#8693=EDGE_CURVE('',#5741,#6224,#2956,.T.);
#8694=EDGE_CURVE('',#6225,#6226,#4217,.T.);
#8695=EDGE_CURVE('',#6227,#6225,#4218,.T.);
#8696=EDGE_CURVE('',#6228,#6227,#4219,.T.);
#8697=EDGE_CURVE('',#6228,#6226,#4220,.T.);
#8698=EDGE_CURVE('',#6226,#6229,#1867,.T.);
#8699=EDGE_CURVE('',#6230,#6228,#4221,.T.);
#8700=EDGE_CURVE('',#6230,#6229,#4222,.T.);
#8701=EDGE_CURVE('',#6229,#6231,#4223,.T.);
#8702=EDGE_CURVE('',#6232,#6230,#4224,.T.);
#8703=EDGE_CURVE('',#6232,#6231,#4225,.T.);
#8704=EDGE_CURVE('',#6231,#6225,#1868,.T.);
#8705=EDGE_CURVE('',#6227,#6232,#4226,.T.);
#8706=EDGE_CURVE('',#6233,#6233,#1869,.T.);
#8707=EDGE_CURVE('',#6233,#6234,#4227,.T.);
#8708=EDGE_CURVE('',#6234,#6234,#1870,.T.);
#8709=EDGE_CURVE('',#6235,#6235,#1871,.T.);
#8710=EDGE_CURVE('',#6235,#6236,#4228,.T.);
#8711=EDGE_CURVE('',#6236,#6236,#1872,.T.);
#8712=EDGE_CURVE('',#6237,#6237,#1873,.T.);
#8713=EDGE_CURVE('',#6237,#6238,#4229,.T.);
#8714=EDGE_CURVE('',#6238,#6238,#1874,.T.);
#8715=EDGE_CURVE('',#6239,#6239,#1875,.T.);
#8716=EDGE_CURVE('',#6239,#6240,#4230,.T.);
#8717=EDGE_CURVE('',#6240,#6240,#1876,.T.);
#8718=EDGE_CURVE('',#5795,#6241,#2957,.T.);
#8719=EDGE_CURVE('',#6119,#5850,#2958,.T.);
#8720=EDGE_CURVE('',#6078,#6241,#2959,.T.);
#8721=EDGE_CURVE('',#6077,#5796,#2960,.T.);
#8722=EDGE_CURVE('',#6242,#6120,#2961,.T.);
#8723=EDGE_CURVE('',#5849,#6242,#2962,.T.);
#8724=EDGE_CURVE('',#5854,#6243,#2963,.T.);
#8725=EDGE_CURVE('',#6073,#5909,#2964,.T.);
#8726=EDGE_CURVE('',#6032,#6243,#2965,.T.);
#8727=EDGE_CURVE('',#6031,#5855,#2966,.T.);
#8728=EDGE_CURVE('',#6244,#6074,#2967,.T.);
#8729=EDGE_CURVE('',#5908,#6244,#2968,.T.);
#8730=EDGE_CURVE('',#5913,#6245,#2969,.T.);
#8731=EDGE_CURVE('',#6203,#5968,#2970,.T.);
#8732=EDGE_CURVE('',#6166,#6245,#2971,.T.);
#8733=EDGE_CURVE('',#6165,#5914,#2972,.T.);
#8734=EDGE_CURVE('',#6246,#6204,#2973,.T.);
#8735=EDGE_CURVE('',#5967,#6246,#2974,.T.);
#8736=EDGE_CURVE('',#5972,#6247,#2975,.T.);
#8737=EDGE_CURVE('',#6161,#6027,#2976,.T.);
#8738=EDGE_CURVE('',#6124,#6247,#2977,.T.);
#8739=EDGE_CURVE('',#6123,#5973,#2978,.T.);
#8740=EDGE_CURVE('',#6248,#6162,#2979,.T.);
#8741=EDGE_CURVE('',#6026,#6248,#2980,.T.);
#8742=EDGE_CURVE('',#6249,#6249,#1877,.T.);
#8743=EDGE_CURVE('',#6249,#6250,#4231,.T.);
#8744=EDGE_CURVE('',#6250,#6250,#1878,.T.);
#8745=EDGE_CURVE('',#6251,#6252,#4232,.T.);
#8746=EDGE_CURVE('',#6252,#6253,#4233,.T.);
#8747=EDGE_CURVE('',#6253,#6254,#4234,.T.);
#8748=EDGE_CURVE('',#6254,#6251,#4235,.T.);
#8749=EDGE_CURVE('',#6255,#6256,#4236,.T.);
#8750=EDGE_CURVE('',#6257,#6255,#4237,.T.);
#8751=EDGE_CURVE('',#6258,#6257,#4238,.T.);
#8752=EDGE_CURVE('',#6256,#6258,#4239,.T.);
#8753=EDGE_CURVE('',#6259,#6260,#4240,.T.);
#8754=EDGE_CURVE('',#6260,#6251,#4241,.T.);
#8755=EDGE_CURVE('',#6259,#6254,#4242,.T.);
#8756=EDGE_CURVE('',#6261,#6259,#4243,.T.);
#8757=EDGE_CURVE('',#6261,#6253,#4244,.T.);
#8758=EDGE_CURVE('',#6262,#6261,#4245,.T.);
#8759=EDGE_CURVE('',#6262,#6252,#4246,.T.);
#8760=EDGE_CURVE('',#6260,#6262,#4247,.T.);
#8761=EDGE_CURVE('',#6256,#6263,#4248,.T.);
#8762=EDGE_CURVE('',#6264,#6263,#4249,.T.);
#8763=EDGE_CURVE('',#6255,#6264,#4250,.T.);
#8764=EDGE_CURVE('',#6265,#6264,#4251,.T.);
#8765=EDGE_CURVE('',#6257,#6265,#4252,.T.);
#8766=EDGE_CURVE('',#6266,#6265,#4253,.T.);
#8767=EDGE_CURVE('',#6258,#6266,#4254,.T.);
#8768=EDGE_CURVE('',#6263,#6266,#4255,.T.);
#8769=EDGE_CURVE('',#6267,#6268,#4256,.T.);
#8770=EDGE_CURVE('',#6269,#6267,#4257,.T.);
#8771=EDGE_CURVE('',#6270,#6269,#4258,.T.);
#8772=EDGE_CURVE('',#6268,#6270,#4259,.T.);
#8773=EDGE_CURVE('',#6271,#6272,#4260,.T.);
#8774=EDGE_CURVE('',#6273,#6271,#4261,.T.);
#8775=EDGE_CURVE('',#6274,#6273,#4262,.T.);
#8776=EDGE_CURVE('',#6272,#6274,#4263,.T.);
#8777=EDGE_CURVE('',#6269,#6274,#1879,.T.);
#8778=EDGE_CURVE('',#6272,#6267,#1880,.T.);
#8779=EDGE_CURVE('',#6271,#6268,#1881,.T.);
#8780=EDGE_CURVE('',#6270,#6273,#1882,.T.);
#8781=EDGE_CURVE('',#6275,#6276,#4264,.T.);
#8782=EDGE_CURVE('',#6276,#6277,#2981,.T.);
#8783=EDGE_CURVE('',#6277,#6278,#1883,.T.);
#8784=EDGE_CURVE('',#6278,#6279,#4265,.T.);
#8785=EDGE_CURVE('',#6279,#6279,#1884,.F.);
#8786=EDGE_CURVE('',#6278,#6280,#1885,.T.);
#8787=EDGE_CURVE('',#6280,#6275,#2982,.T.);
#8788=EDGE_CURVE('',#6281,#6282,#4266,.T.);
#8789=EDGE_CURVE('',#6282,#6283,#2983,.T.);
#8790=EDGE_CURVE('',#6283,#6276,#2984,.T.);
#8791=EDGE_CURVE('',#6275,#6284,#2985,.T.);
#8792=EDGE_CURVE('',#6284,#6281,#2986,.T.);
#8793=EDGE_CURVE('',#6285,#6286,#4267,.T.);
#8794=EDGE_CURVE('',#6286,#6287,#2987,.T.);
#8795=EDGE_CURVE('',#6287,#6282,#2988,.T.);
#8796=EDGE_CURVE('',#6281,#6288,#2989,.T.);
#8797=EDGE_CURVE('',#6288,#6285,#2990,.T.);
#8798=EDGE_CURVE('',#6289,#6290,#4268,.T.);
#8799=EDGE_CURVE('',#6290,#6291,#2991,.T.);
#8800=EDGE_CURVE('',#6291,#6286,#2992,.T.);
#8801=EDGE_CURVE('',#6285,#6292,#2993,.T.);
#8802=EDGE_CURVE('',#6292,#6289,#2994,.T.);
#8803=EDGE_CURVE('',#6293,#6294,#4269,.T.);
#8804=EDGE_CURVE('',#6294,#6295,#2995,.T.);
#8805=EDGE_CURVE('',#6295,#6290,#2996,.T.);
#8806=EDGE_CURVE('',#6289,#6296,#2997,.T.);
#8807=EDGE_CURVE('',#6296,#6293,#2998,.T.);
#8808=EDGE_CURVE('',#6297,#6298,#4270,.T.);
#8809=EDGE_CURVE('',#6298,#6299,#2999,.T.);
#8810=EDGE_CURVE('',#6299,#6294,#3000,.T.);
#8811=EDGE_CURVE('',#6293,#6300,#3001,.T.);
#8812=EDGE_CURVE('',#6300,#6297,#3002,.T.);
#8813=EDGE_CURVE('',#6301,#6302,#4271,.T.);
#8814=EDGE_CURVE('',#6302,#6303,#3003,.T.);
#8815=EDGE_CURVE('',#6303,#6298,#3004,.T.);
#8816=EDGE_CURVE('',#6297,#6304,#3005,.T.);
#8817=EDGE_CURVE('',#6304,#6301,#3006,.T.);
#8818=EDGE_CURVE('',#6305,#6306,#4272,.T.);
#8819=EDGE_CURVE('',#6306,#6307,#3007,.T.);
#8820=EDGE_CURVE('',#6307,#6302,#3008,.T.);
#8821=EDGE_CURVE('',#6301,#6308,#3009,.T.);
#8822=EDGE_CURVE('',#6308,#6305,#3010,.T.);
#8823=EDGE_CURVE('',#6309,#6310,#4273,.T.);
#8824=EDGE_CURVE('',#6310,#6311,#3011,.T.);
#8825=EDGE_CURVE('',#6311,#6306,#3012,.T.);
#8826=EDGE_CURVE('',#6305,#6312,#3013,.T.);
#8827=EDGE_CURVE('',#6312,#6309,#3014,.T.);
#8828=EDGE_CURVE('',#6313,#6314,#4274,.T.);
#8829=EDGE_CURVE('',#6314,#6315,#3015,.T.);
#8830=EDGE_CURVE('',#6315,#6310,#3016,.T.);
#8831=EDGE_CURVE('',#6309,#6316,#3017,.T.);
#8832=EDGE_CURVE('',#6316,#6313,#3018,.T.);
#8833=EDGE_CURVE('',#6317,#6318,#4275,.T.);
#8834=EDGE_CURVE('',#6318,#6319,#3019,.T.);
#8835=EDGE_CURVE('',#6319,#6314,#3020,.T.);
#8836=EDGE_CURVE('',#6313,#6320,#3021,.T.);
#8837=EDGE_CURVE('',#6320,#6317,#3022,.T.);
#8838=EDGE_CURVE('',#6321,#6322,#4276,.T.);
#8839=EDGE_CURVE('',#6322,#6323,#3023,.T.);
#8840=EDGE_CURVE('',#6323,#6318,#3024,.T.);
#8841=EDGE_CURVE('',#6317,#6324,#3025,.T.);
#8842=EDGE_CURVE('',#6324,#6321,#3026,.T.);
#8843=EDGE_CURVE('',#6325,#6326,#4277,.T.);
#8844=EDGE_CURVE('',#6326,#6327,#3027,.T.);
#8845=EDGE_CURVE('',#6327,#6322,#3028,.T.);
#8846=EDGE_CURVE('',#6321,#6328,#3029,.T.);
#8847=EDGE_CURVE('',#6328,#6325,#3030,.T.);
#8848=EDGE_CURVE('',#6329,#6330,#4278,.T.);
#8849=EDGE_CURVE('',#6330,#6331,#3031,.T.);
#8850=EDGE_CURVE('',#6331,#6326,#3032,.T.);
#8851=EDGE_CURVE('',#6325,#6332,#3033,.T.);
#8852=EDGE_CURVE('',#6332,#6329,#3034,.T.);
#8853=EDGE_CURVE('',#6333,#6334,#4279,.T.);
#8854=EDGE_CURVE('',#6334,#6335,#3035,.T.);
#8855=EDGE_CURVE('',#6335,#6330,#3036,.T.);
#8856=EDGE_CURVE('',#6329,#6336,#3037,.T.);
#8857=EDGE_CURVE('',#6336,#6333,#3038,.T.);
#8858=EDGE_CURVE('',#6337,#6338,#4280,.T.);
#8859=EDGE_CURVE('',#6338,#6339,#3039,.T.);
#8860=EDGE_CURVE('',#6339,#6334,#3040,.T.);
#8861=EDGE_CURVE('',#6333,#6340,#3041,.T.);
#8862=EDGE_CURVE('',#6340,#6337,#3042,.T.);
#8863=EDGE_CURVE('',#6341,#6342,#4281,.T.);
#8864=EDGE_CURVE('',#6342,#6343,#3043,.T.);
#8865=EDGE_CURVE('',#6343,#6338,#3044,.T.);
#8866=EDGE_CURVE('',#6337,#6344,#3045,.T.);
#8867=EDGE_CURVE('',#6344,#6341,#3046,.T.);
#8868=EDGE_CURVE('',#6345,#6346,#4282,.T.);
#8869=EDGE_CURVE('',#6346,#6347,#3047,.T.);
#8870=EDGE_CURVE('',#6347,#6342,#3048,.T.);
#8871=EDGE_CURVE('',#6341,#6348,#3049,.T.);
#8872=EDGE_CURVE('',#6348,#6345,#3050,.T.);
#8873=EDGE_CURVE('',#6349,#6350,#4283,.T.);
#8874=EDGE_CURVE('',#6350,#6351,#3051,.T.);
#8875=EDGE_CURVE('',#6351,#6346,#3052,.T.);
#8876=EDGE_CURVE('',#6345,#6352,#3053,.T.);
#8877=EDGE_CURVE('',#6352,#6349,#3054,.T.);
#8878=EDGE_CURVE('',#6353,#6354,#4284,.T.);
#8879=EDGE_CURVE('',#6354,#6355,#3055,.T.);
#8880=EDGE_CURVE('',#6355,#6350,#3056,.T.);
#8881=EDGE_CURVE('',#6349,#6356,#3057,.T.);
#8882=EDGE_CURVE('',#6356,#6353,#3058,.T.);
#8883=EDGE_CURVE('',#6357,#6358,#4285,.T.);
#8884=EDGE_CURVE('',#6358,#6359,#3059,.T.);
#8885=EDGE_CURVE('',#6359,#6354,#3060,.T.);
#8886=EDGE_CURVE('',#6353,#6360,#3061,.T.);
#8887=EDGE_CURVE('',#6360,#6357,#3062,.T.);
#8888=EDGE_CURVE('',#6361,#6362,#4286,.T.);
#8889=EDGE_CURVE('',#6362,#6363,#3063,.T.);
#8890=EDGE_CURVE('',#6363,#6358,#3064,.T.);
#8891=EDGE_CURVE('',#6357,#6364,#3065,.T.);
#8892=EDGE_CURVE('',#6364,#6361,#3066,.T.);
#8893=EDGE_CURVE('',#6365,#6366,#4287,.T.);
#8894=EDGE_CURVE('',#6366,#6367,#3067,.T.);
#8895=EDGE_CURVE('',#6367,#6362,#3068,.T.);
#8896=EDGE_CURVE('',#6361,#6368,#3069,.T.);
#8897=EDGE_CURVE('',#6368,#6365,#3070,.T.);
#8898=EDGE_CURVE('',#6369,#6370,#4288,.T.);
#8899=EDGE_CURVE('',#6370,#6371,#3071,.T.);
#8900=EDGE_CURVE('',#6371,#6366,#3072,.T.);
#8901=EDGE_CURVE('',#6365,#6372,#3073,.T.);
#8902=EDGE_CURVE('',#6372,#6369,#3074,.T.);
#8903=EDGE_CURVE('',#6373,#6374,#4289,.T.);
#8904=EDGE_CURVE('',#6374,#6375,#3075,.T.);
#8905=EDGE_CURVE('',#6375,#6370,#3076,.T.);
#8906=EDGE_CURVE('',#6369,#6376,#3077,.T.);
#8907=EDGE_CURVE('',#6376,#6373,#3078,.T.);
#8908=EDGE_CURVE('',#6377,#6378,#4290,.T.);
#8909=EDGE_CURVE('',#6378,#6379,#3079,.T.);
#8910=EDGE_CURVE('',#6379,#6374,#3080,.T.);
#8911=EDGE_CURVE('',#6373,#6380,#3081,.T.);
#8912=EDGE_CURVE('',#6380,#6377,#3082,.T.);
#8913=EDGE_CURVE('',#6381,#6382,#4291,.T.);
#8914=EDGE_CURVE('',#6382,#6383,#3083,.T.);
#8915=EDGE_CURVE('',#6383,#6378,#3084,.T.);
#8916=EDGE_CURVE('',#6377,#6384,#3085,.T.);
#8917=EDGE_CURVE('',#6384,#6381,#3086,.T.);
#8918=EDGE_CURVE('',#6385,#6386,#4292,.T.);
#8919=EDGE_CURVE('',#6386,#6387,#3087,.T.);
#8920=EDGE_CURVE('',#6387,#6382,#3088,.T.);
#8921=EDGE_CURVE('',#6381,#6388,#3089,.T.);
#8922=EDGE_CURVE('',#6388,#6385,#3090,.T.);
#8923=EDGE_CURVE('',#6389,#6390,#4293,.T.);
#8924=EDGE_CURVE('',#6390,#6391,#3091,.T.);
#8925=EDGE_CURVE('',#6391,#6386,#3092,.T.);
#8926=EDGE_CURVE('',#6385,#6392,#3093,.T.);
#8927=EDGE_CURVE('',#6392,#6389,#3094,.T.);
#8928=EDGE_CURVE('',#6393,#6394,#4294,.T.);
#8929=EDGE_CURVE('',#6394,#6395,#3095,.T.);
#8930=EDGE_CURVE('',#6395,#6390,#3096,.T.);
#8931=EDGE_CURVE('',#6389,#6396,#3097,.T.);
#8932=EDGE_CURVE('',#6396,#6393,#3098,.T.);
#8933=EDGE_CURVE('',#6397,#6398,#4295,.T.);
#8934=EDGE_CURVE('',#6398,#6399,#3099,.T.);
#8935=EDGE_CURVE('',#6399,#6394,#3100,.T.);
#8936=EDGE_CURVE('',#6393,#6400,#3101,.T.);
#8937=EDGE_CURVE('',#6400,#6397,#3102,.T.);
#8938=EDGE_CURVE('',#6401,#6402,#4296,.T.);
#8939=EDGE_CURVE('',#6402,#6403,#3103,.T.);
#8940=EDGE_CURVE('',#6403,#6398,#3104,.T.);
#8941=EDGE_CURVE('',#6397,#6404,#3105,.T.);
#8942=EDGE_CURVE('',#6404,#6401,#3106,.T.);
#8943=EDGE_CURVE('',#6405,#6406,#4297,.T.);
#8944=EDGE_CURVE('',#6406,#6407,#3107,.T.);
#8945=EDGE_CURVE('',#6407,#6402,#3108,.T.);
#8946=EDGE_CURVE('',#6401,#6408,#3109,.T.);
#8947=EDGE_CURVE('',#6408,#6405,#3110,.T.);
#8948=EDGE_CURVE('',#6409,#6410,#4298,.T.);
#8949=EDGE_CURVE('',#6410,#6411,#3111,.T.);
#8950=EDGE_CURVE('',#6411,#6406,#3112,.T.);
#8951=EDGE_CURVE('',#6405,#6412,#3113,.T.);
#8952=EDGE_CURVE('',#6412,#6409,#3114,.T.);
#8953=EDGE_CURVE('',#6413,#6414,#4299,.T.);
#8954=EDGE_CURVE('',#6414,#6415,#3115,.T.);
#8955=EDGE_CURVE('',#6415,#6410,#3116,.T.);
#8956=EDGE_CURVE('',#6409,#6416,#3117,.T.);
#8957=EDGE_CURVE('',#6416,#6413,#3118,.T.);
#8958=EDGE_CURVE('',#6417,#6418,#4300,.T.);
#8959=EDGE_CURVE('',#6418,#6419,#3119,.T.);
#8960=EDGE_CURVE('',#6419,#6414,#3120,.T.);
#8961=EDGE_CURVE('',#6413,#6420,#3121,.T.);
#8962=EDGE_CURVE('',#6420,#6417,#3122,.T.);
#8963=EDGE_CURVE('',#6421,#6422,#4301,.T.);
#8964=EDGE_CURVE('',#6422,#6423,#3123,.T.);
#8965=EDGE_CURVE('',#6423,#6418,#3124,.T.);
#8966=EDGE_CURVE('',#6417,#6424,#3125,.T.);
#8967=EDGE_CURVE('',#6424,#6421,#3126,.T.);
#8968=EDGE_CURVE('',#6425,#6426,#4302,.T.);
#8969=EDGE_CURVE('',#6426,#6427,#3127,.T.);
#8970=EDGE_CURVE('',#6427,#6422,#3128,.T.);
#8971=EDGE_CURVE('',#6421,#6428,#3129,.T.);
#8972=EDGE_CURVE('',#6428,#6425,#3130,.T.);
#8973=EDGE_CURVE('',#6429,#6430,#4303,.T.);
#8974=EDGE_CURVE('',#6430,#6431,#3131,.T.);
#8975=EDGE_CURVE('',#6431,#6426,#3132,.T.);
#8976=EDGE_CURVE('',#6425,#6432,#3133,.T.);
#8977=EDGE_CURVE('',#6432,#6429,#3134,.T.);
#8978=EDGE_CURVE('',#6433,#6434,#4304,.T.);
#8979=EDGE_CURVE('',#6434,#6435,#3135,.T.);
#8980=EDGE_CURVE('',#6435,#6430,#3136,.T.);
#8981=EDGE_CURVE('',#6429,#6436,#3137,.T.);
#8982=EDGE_CURVE('',#6436,#6433,#3138,.T.);
#8983=EDGE_CURVE('',#6437,#6438,#4305,.T.);
#8984=EDGE_CURVE('',#6438,#6439,#3139,.T.);
#8985=EDGE_CURVE('',#6439,#6434,#3140,.T.);
#8986=EDGE_CURVE('',#6433,#6440,#3141,.T.);
#8987=EDGE_CURVE('',#6440,#6437,#3142,.T.);
#8988=EDGE_CURVE('',#6441,#6442,#4306,.T.);
#8989=EDGE_CURVE('',#6442,#6443,#3143,.T.);
#8990=EDGE_CURVE('',#6443,#6438,#3144,.T.);
#8991=EDGE_CURVE('',#6437,#6444,#3145,.T.);
#8992=EDGE_CURVE('',#6444,#6441,#3146,.T.);
#8993=EDGE_CURVE('',#6445,#6446,#4307,.T.);
#8994=EDGE_CURVE('',#6446,#6447,#3147,.T.);
#8995=EDGE_CURVE('',#6447,#6442,#3148,.T.);
#8996=EDGE_CURVE('',#6441,#6448,#3149,.T.);
#8997=EDGE_CURVE('',#6448,#6445,#3150,.T.);
#8998=EDGE_CURVE('',#6449,#6450,#4308,.T.);
#8999=EDGE_CURVE('',#6450,#6451,#3151,.T.);
#9000=EDGE_CURVE('',#6451,#6446,#3152,.T.);
#9001=EDGE_CURVE('',#6445,#6452,#3153,.T.);
#9002=EDGE_CURVE('',#6452,#6449,#3154,.T.);
#9003=EDGE_CURVE('',#6453,#6454,#4309,.T.);
#9004=EDGE_CURVE('',#6454,#6455,#3155,.T.);
#9005=EDGE_CURVE('',#6455,#6450,#3156,.T.);
#9006=EDGE_CURVE('',#6449,#6456,#3157,.T.);
#9007=EDGE_CURVE('',#6456,#6453,#3158,.T.);
#9008=EDGE_CURVE('',#6457,#6458,#4310,.T.);
#9009=EDGE_CURVE('',#6458,#6459,#3159,.T.);
#9010=EDGE_CURVE('',#6459,#6454,#3160,.T.);
#9011=EDGE_CURVE('',#6453,#6460,#3161,.T.);
#9012=EDGE_CURVE('',#6460,#6457,#3162,.T.);
#9013=EDGE_CURVE('',#6461,#6462,#4311,.T.);
#9014=EDGE_CURVE('',#6462,#6463,#3163,.T.);
#9015=EDGE_CURVE('',#6463,#6458,#3164,.T.);
#9016=EDGE_CURVE('',#6457,#6464,#3165,.T.);
#9017=EDGE_CURVE('',#6464,#6461,#3166,.T.);
#9018=EDGE_CURVE('',#6465,#6466,#4312,.T.);
#9019=EDGE_CURVE('',#6466,#6467,#3167,.T.);
#9020=EDGE_CURVE('',#6467,#6462,#3168,.T.);
#9021=EDGE_CURVE('',#6461,#6468,#3169,.T.);
#9022=EDGE_CURVE('',#6468,#6465,#3170,.T.);
#9023=EDGE_CURVE('',#6469,#6470,#4313,.T.);
#9024=EDGE_CURVE('',#6469,#6471,#3171,.T.);
#9025=EDGE_CURVE('',#6471,#6472,#3172,.T.);
#9026=EDGE_CURVE('',#6473,#6472,#1886,.F.);
#9027=EDGE_CURVE('',#6473,#6474,#3173,.T.);
#9028=EDGE_CURVE('',#6474,#6470,#3174,.T.);
#9029=EDGE_CURVE('',#6470,#6475,#3175,.T.);
#9030=EDGE_CURVE('',#6475,#6466,#3176,.T.);
#9031=EDGE_CURVE('',#6465,#6476,#3177,.T.);
#9032=EDGE_CURVE('',#6476,#6469,#3178,.T.);
#9033=EDGE_CURVE('',#6477,#6478,#3179,.T.);
#9034=EDGE_CURVE('',#6479,#6477,#1887,.T.);
#9035=EDGE_CURVE('',#6479,#6480,#3180,.T.);
#9036=EDGE_CURVE('',#6480,#6481,#3181,.T.);
#9037=EDGE_CURVE('',#6481,#6482,#3182,.T.);
#9038=EDGE_CURVE('',#6482,#6483,#3183,.T.);
#9039=EDGE_CURVE('',#6483,#6484,#3184,.T.);
#9040=EDGE_CURVE('',#6484,#6485,#3185,.T.);
#9041=EDGE_CURVE('',#6485,#6486,#3186,.T.);
#9042=EDGE_CURVE('',#6486,#6487,#3187,.T.);
#9043=EDGE_CURVE('',#6487,#6488,#3188,.T.);
#9044=EDGE_CURVE('',#6488,#6489,#3189,.T.);
#9045=EDGE_CURVE('',#6489,#6490,#3190,.T.);
#9046=EDGE_CURVE('',#6490,#6491,#3191,.T.);
#9047=EDGE_CURVE('',#6491,#6492,#3192,.T.);
#9048=EDGE_CURVE('',#6492,#6493,#3193,.T.);
#9049=EDGE_CURVE('',#6493,#6494,#3194,.T.);
#9050=EDGE_CURVE('',#6494,#6495,#3195,.T.);
#9051=EDGE_CURVE('',#6495,#6496,#3196,.T.);
#9052=EDGE_CURVE('',#6496,#6497,#3197,.T.);
#9053=EDGE_CURVE('',#6497,#6498,#3198,.T.);
#9054=EDGE_CURVE('',#6498,#6499,#3199,.T.);
#9055=EDGE_CURVE('',#6499,#6500,#3200,.T.);
#9056=EDGE_CURVE('',#6500,#6501,#3201,.T.);
#9057=EDGE_CURVE('',#6501,#6502,#3202,.T.);
#9058=EDGE_CURVE('',#6502,#6503,#3203,.T.);
#9059=EDGE_CURVE('',#6503,#6504,#3204,.T.);
#9060=EDGE_CURVE('',#6504,#6505,#3205,.T.);
#9061=EDGE_CURVE('',#6505,#6506,#3206,.T.);
#9062=EDGE_CURVE('',#6506,#6507,#3207,.T.);
#9063=EDGE_CURVE('',#6507,#6508,#3208,.T.);
#9064=EDGE_CURVE('',#6508,#6509,#3209,.T.);
#9065=EDGE_CURVE('',#6509,#6510,#3210,.T.);
#9066=EDGE_CURVE('',#6510,#6511,#3211,.T.);
#9067=EDGE_CURVE('',#6511,#6512,#3212,.T.);
#9068=EDGE_CURVE('',#6512,#6513,#3213,.T.);
#9069=EDGE_CURVE('',#6513,#6514,#3214,.T.);
#9070=EDGE_CURVE('',#6514,#6515,#3215,.T.);
#9071=EDGE_CURVE('',#6515,#6516,#3216,.T.);
#9072=EDGE_CURVE('',#6516,#6517,#3217,.T.);
#9073=EDGE_CURVE('',#6517,#6518,#3218,.T.);
#9074=EDGE_CURVE('',#6518,#6519,#3219,.T.);
#9075=EDGE_CURVE('',#6519,#6520,#3220,.T.);
#9076=EDGE_CURVE('',#6520,#6521,#3221,.T.);
#9077=EDGE_CURVE('',#6522,#6521,#1888,.T.);
#9078=EDGE_CURVE('',#6523,#6522,#3222,.T.);
#9079=EDGE_CURVE('',#6524,#6523,#3223,.T.);
#9080=EDGE_CURVE('',#6525,#6524,#3224,.F.);
#9081=EDGE_CURVE('',#6526,#6525,#3225,.F.);
#9082=EDGE_CURVE('',#6527,#6526,#3226,.F.);
#9083=EDGE_CURVE('',#6528,#6527,#3227,.T.);
#9084=EDGE_CURVE('',#6529,#6528,#3228,.T.);
#9085=EDGE_CURVE('',#6530,#6529,#3229,.T.);
#9086=EDGE_CURVE('',#6531,#6530,#3230,.T.);
#9087=EDGE_CURVE('',#6532,#6531,#3231,.T.);
#9088=EDGE_CURVE('',#6533,#6532,#3232,.T.);
#9089=EDGE_CURVE('',#6534,#6533,#3233,.F.);
#9090=EDGE_CURVE('',#6535,#6534,#3234,.F.);
#9091=EDGE_CURVE('',#6536,#6535,#3235,.F.);
#9092=EDGE_CURVE('',#6537,#6536,#3236,.T.);
#9093=EDGE_CURVE('',#6538,#6537,#3237,.T.);
#9094=EDGE_CURVE('',#6539,#6538,#3238,.T.);
#9095=EDGE_CURVE('',#6540,#6539,#3239,.T.);
#9096=EDGE_CURVE('',#6541,#6540,#3240,.T.);
#9097=EDGE_CURVE('',#6542,#6541,#3241,.T.);
#9098=EDGE_CURVE('',#6543,#6542,#3242,.T.);
#9099=EDGE_CURVE('',#6544,#6543,#3243,.F.);
#9100=EDGE_CURVE('',#6545,#6544,#3244,.T.);
#9101=EDGE_CURVE('',#6546,#6545,#3245,.F.);
#9102=EDGE_CURVE('',#6547,#6546,#3246,.T.);
#9103=EDGE_CURVE('',#6548,#6547,#3247,.T.);
#9104=EDGE_CURVE('',#6549,#6548,#3248,.T.);
#9105=EDGE_CURVE('',#6550,#6549,#3249,.T.);
#9106=EDGE_CURVE('',#6551,#6550,#3250,.T.);
#9107=EDGE_CURVE('',#6552,#6551,#3251,.T.);
#9108=EDGE_CURVE('',#6553,#6552,#3252,.T.);
#9109=EDGE_CURVE('',#6554,#6553,#3253,.T.);
#9110=EDGE_CURVE('',#6555,#6554,#3254,.T.);
#9111=EDGE_CURVE('',#6556,#6555,#3255,.T.);
#9112=EDGE_CURVE('',#6557,#6556,#3256,.T.);
#9113=EDGE_CURVE('',#6558,#6557,#3257,.T.);
#9114=EDGE_CURVE('',#6559,#6558,#3258,.T.);
#9115=EDGE_CURVE('',#6560,#6559,#3259,.T.);
#9116=EDGE_CURVE('',#6561,#6560,#3260,.F.);
#9117=EDGE_CURVE('',#6562,#6561,#3261,.T.);
#9118=EDGE_CURVE('',#6478,#6562,#3262,.T.);
#9119=EDGE_CURVE('',#6563,#6563,#1889,.T.);
#9120=EDGE_CURVE('',#6564,#6564,#1890,.T.);
#9121=EDGE_CURVE('',#6563,#6565,#4314,.T.);
#9122=EDGE_CURVE('',#6565,#6565,#1891,.T.);
#9123=EDGE_CURVE('',#6566,#6567,#4315,.T.);
#9124=EDGE_CURVE('',#6566,#6568,#4316,.T.);
#9125=EDGE_CURVE('',#6569,#6568,#4317,.T.);
#9126=EDGE_CURVE('',#6567,#6569,#4318,.T.);
#9127=EDGE_CURVE('',#6570,#6571,#4319,.T.);
#9128=EDGE_CURVE('',#6568,#6570,#4320,.T.);
#9129=EDGE_CURVE('',#6571,#6566,#4321,.T.);
#9130=EDGE_CURVE('',#6572,#6573,#4322,.T.);
#9131=EDGE_CURVE('',#6567,#6572,#4323,.T.);
#9132=EDGE_CURVE('',#6573,#6569,#4324,.T.);
#9133=EDGE_CURVE('',#6572,#6571,#1892,.T.);
#9134=EDGE_CURVE('',#6277,#6522,#3263,.T.);
#9135=EDGE_CURVE('',#6521,#6280,#3264,.T.);
#9136=EDGE_CURVE('',#6472,#6479,#3265,.T.);
#9137=EDGE_CURVE('',#6477,#6473,#3266,.T.);
#9138=EDGE_CURVE('',#6574,#6574,#1893,.T.);
#9139=EDGE_CURVE('',#6574,#6564,#4325,.T.);
#9140=EDGE_CURVE('',#6573,#6570,#1894,.T.);
#9141=EDGE_CURVE('',#6575,#6575,#1895,.T.);
#9142=EDGE_CURVE('',#6576,#6576,#1896,.T.);
#9143=EDGE_CURVE('',#6576,#6575,#4326,.T.);
#9144=EDGE_CURVE('',#6577,#6577,#1897,.T.);
#9145=EDGE_CURVE('',#6578,#6578,#1898,.T.);
#9146=EDGE_CURVE('',#6578,#6577,#4327,.T.);
#9147=EDGE_CURVE('',#6578,#6579,#4328,.T.);
#9148=EDGE_CURVE('',#6580,#6580,#1899,.T.);
#9149=EDGE_CURVE('',#6580,#6581,#4329,.T.);
#9150=EDGE_CURVE('',#6581,#6581,#1900,.T.);
#9151=EDGE_CURVE('',#6582,#6582,#1901,.T.);
#9152=EDGE_CURVE('',#6582,#6583,#4330,.T.);
#9153=EDGE_CURVE('',#6583,#6583,#1902,.T.);
#9154=EDGE_CURVE('',#6584,#6585,#4331,.T.);
#9155=EDGE_CURVE('',#6586,#6584,#4332,.T.);
#9156=EDGE_CURVE('',#6587,#6586,#4333,.T.);
#9157=EDGE_CURVE('',#6585,#6587,#4334,.T.);
#9158=EDGE_CURVE('',#6588,#6589,#4335,.T.);
#9159=EDGE_CURVE('',#6589,#6590,#4336,.T.);
#9160=EDGE_CURVE('',#6590,#6591,#4337,.T.);
#9161=EDGE_CURVE('',#6591,#6588,#4338,.T.);
#9162=EDGE_CURVE('',#6584,#6592,#4339,.T.);
#9163=EDGE_CURVE('',#6593,#6592,#4340,.T.);
#9164=EDGE_CURVE('',#6586,#6593,#4341,.T.);
#9165=EDGE_CURVE('',#6594,#6593,#4342,.T.);
#9166=EDGE_CURVE('',#6587,#6594,#4343,.T.);
#9167=EDGE_CURVE('',#6595,#6594,#4344,.T.);
#9168=EDGE_CURVE('',#6585,#6595,#4345,.T.);
#9169=EDGE_CURVE('',#6592,#6595,#4346,.T.);
#9170=EDGE_CURVE('',#6596,#6597,#4347,.T.);
#9171=EDGE_CURVE('',#6597,#6589,#4348,.T.);
#9172=EDGE_CURVE('',#6596,#6588,#4349,.T.);
#9173=EDGE_CURVE('',#6598,#6596,#4350,.T.);
#9174=EDGE_CURVE('',#6598,#6591,#4351,.T.);
#9175=EDGE_CURVE('',#6599,#6598,#4352,.T.);
#9176=EDGE_CURVE('',#6599,#6590,#4353,.T.);
#9177=EDGE_CURVE('',#6597,#6599,#4354,.T.);
#9178=EDGE_CURVE('',#6600,#6601,#4355,.T.);
#9179=EDGE_CURVE('',#6602,#6600,#4356,.T.);
#9180=EDGE_CURVE('',#6603,#6602,#4357,.T.);
#9181=EDGE_CURVE('',#6601,#6603,#4358,.T.);
#9182=EDGE_CURVE('',#6603,#6604,#4359,.T.);
#9183=EDGE_CURVE('',#6604,#6605,#4360,.T.);
#9184=EDGE_CURVE('',#6601,#6605,#4361,.T.);
#9185=EDGE_CURVE('',#6606,#6602,#4362,.T.);
#9186=EDGE_CURVE('',#6604,#6606,#4363,.T.);
#9187=EDGE_CURVE('',#6607,#6607,#1903,.T.);
#9188=EDGE_CURVE('',#6608,#6608,#1904,.T.);
#9189=EDGE_CURVE('',#6609,#6609,#1905,.T.);
#9190=EDGE_CURVE('',#6610,#6610,#1906,.T.);
#9191=EDGE_CURVE('',#6611,#6611,#1907,.T.);
#9192=EDGE_CURVE('',#6612,#6612,#1908,.T.);
#9193=EDGE_CURVE('',#6612,#6607,#4364,.T.);
#9194=EDGE_CURVE('',#6613,#6613,#1909,.T.);
#9195=EDGE_CURVE('',#6613,#6608,#4365,.T.);
#9196=EDGE_CURVE('',#6614,#6614,#1910,.T.);
#9197=EDGE_CURVE('',#6614,#6609,#4366,.T.);
#9198=EDGE_CURVE('',#6615,#6615,#1911,.T.);
#9199=EDGE_CURVE('',#6615,#6610,#4367,.T.);
#9200=EDGE_CURVE('',#6616,#6616,#1912,.T.);
#9201=EDGE_CURVE('',#6616,#6611,#4368,.T.);
#9202=EDGE_CURVE('',#6606,#6617,#4369,.T.);
#9203=EDGE_CURVE('',#6605,#6617,#4370,.T.);
#9204=EDGE_CURVE('',#6617,#6600,#4371,.T.);
#9205=EDGE_CURVE('',#6618,#6618,#1913,.T.);
#9206=EDGE_CURVE('',#6618,#6619,#4372,.T.);
#9207=EDGE_CURVE('',#6619,#6619,#1914,.T.);
#9208=EDGE_CURVE('',#6620,#6620,#1915,.T.);
#9209=EDGE_CURVE('',#6620,#6621,#4373,.T.);
#9210=EDGE_CURVE('',#6621,#6621,#1916,.T.);
#9211=EDGE_CURVE('',#6622,#6623,#4374,.T.);
#9212=EDGE_CURVE('',#6624,#6622,#3267,.T.);
#9213=EDGE_CURVE('',#6625,#6624,#1917,.T.);
#9214=EDGE_CURVE('',#6625,#6623,#3268,.T.);
#9215=EDGE_CURVE('',#6626,#6627,#4375,.T.);
#9216=EDGE_CURVE('',#6628,#6626,#3269,.T.);
#9217=EDGE_CURVE('',#6622,#6628,#3270,.T.);
#9218=EDGE_CURVE('',#6623,#6629,#3271,.T.);
#9219=EDGE_CURVE('',#6629,#6627,#3272,.T.);
#9220=EDGE_CURVE('',#6630,#6631,#4376,.T.);
#9221=EDGE_CURVE('',#6632,#6630,#3273,.T.);
#9222=EDGE_CURVE('',#6626,#6632,#3274,.T.);
#9223=EDGE_CURVE('',#6627,#6633,#3275,.T.);
#9224=EDGE_CURVE('',#6633,#6631,#3276,.T.);
#9225=EDGE_CURVE('',#6634,#6635,#4377,.T.);
#9226=EDGE_CURVE('',#6636,#6634,#3277,.T.);
#9227=EDGE_CURVE('',#6630,#6636,#3278,.T.);
#9228=EDGE_CURVE('',#6631,#6637,#3279,.T.);
#9229=EDGE_CURVE('',#6637,#6635,#3280,.T.);
#9230=EDGE_CURVE('',#6638,#6639,#4378,.T.);
#9231=EDGE_CURVE('',#6640,#6638,#3281,.T.);
#9232=EDGE_CURVE('',#6634,#6640,#3282,.T.);
#9233=EDGE_CURVE('',#6635,#6641,#3283,.T.);
#9234=EDGE_CURVE('',#6641,#6639,#3284,.T.);
#9235=EDGE_CURVE('',#6642,#6643,#4379,.T.);
#9236=EDGE_CURVE('',#6644,#6642,#3285,.T.);
#9237=EDGE_CURVE('',#6638,#6644,#3286,.T.);
#9238=EDGE_CURVE('',#6639,#6645,#3287,.T.);
#9239=EDGE_CURVE('',#6645,#6643,#3288,.T.);
#9240=EDGE_CURVE('',#6646,#6647,#4380,.T.);
#9241=EDGE_CURVE('',#6648,#6646,#3289,.T.);
#9242=EDGE_CURVE('',#6642,#6648,#3290,.T.);
#9243=EDGE_CURVE('',#6643,#6649,#3291,.T.);
#9244=EDGE_CURVE('',#6649,#6647,#3292,.T.);
#9245=EDGE_CURVE('',#6650,#6651,#4381,.T.);
#9246=EDGE_CURVE('',#6652,#6650,#3293,.T.);
#9247=EDGE_CURVE('',#6646,#6652,#3294,.T.);
#9248=EDGE_CURVE('',#6647,#6653,#3295,.T.);
#9249=EDGE_CURVE('',#6653,#6651,#3296,.T.);
#9250=EDGE_CURVE('',#6654,#6655,#4382,.T.);
#9251=EDGE_CURVE('',#6656,#6654,#3297,.T.);
#9252=EDGE_CURVE('',#6650,#6656,#3298,.T.);
#9253=EDGE_CURVE('',#6651,#6657,#3299,.T.);
#9254=EDGE_CURVE('',#6657,#6655,#3300,.T.);
#9255=EDGE_CURVE('',#6658,#6659,#4383,.T.);
#9256=EDGE_CURVE('',#6660,#6658,#3301,.T.);
#9257=EDGE_CURVE('',#6654,#6660,#3302,.T.);
#9258=EDGE_CURVE('',#6655,#6661,#3303,.T.);
#9259=EDGE_CURVE('',#6661,#6659,#3304,.T.);
#9260=EDGE_CURVE('',#6662,#6663,#4384,.T.);
#9261=EDGE_CURVE('',#6664,#6662,#3305,.T.);
#9262=EDGE_CURVE('',#6658,#6664,#3306,.T.);
#9263=EDGE_CURVE('',#6659,#6665,#3307,.T.);
#9264=EDGE_CURVE('',#6665,#6663,#3308,.T.);
#9265=EDGE_CURVE('',#6666,#6667,#4385,.T.);
#9266=EDGE_CURVE('',#6668,#6666,#3309,.T.);
#9267=EDGE_CURVE('',#6662,#6668,#3310,.T.);
#9268=EDGE_CURVE('',#6663,#6669,#3311,.T.);
#9269=EDGE_CURVE('',#6669,#6667,#3312,.T.);
#9270=EDGE_CURVE('',#6670,#6671,#4386,.T.);
#9271=EDGE_CURVE('',#6672,#6670,#3313,.T.);
#9272=EDGE_CURVE('',#6666,#6672,#3314,.T.);
#9273=EDGE_CURVE('',#6667,#6673,#3315,.T.);
#9274=EDGE_CURVE('',#6673,#6671,#3316,.T.);
#9275=EDGE_CURVE('',#6674,#6675,#4387,.T.);
#9276=EDGE_CURVE('',#6676,#6674,#3317,.T.);
#9277=EDGE_CURVE('',#6670,#6676,#3318,.T.);
#9278=EDGE_CURVE('',#6671,#6677,#3319,.T.);
#9279=EDGE_CURVE('',#6677,#6675,#3320,.T.);
#9280=EDGE_CURVE('',#6678,#6679,#4388,.T.);
#9281=EDGE_CURVE('',#6680,#6678,#3321,.T.);
#9282=EDGE_CURVE('',#6674,#6680,#3322,.T.);
#9283=EDGE_CURVE('',#6675,#6681,#3323,.T.);
#9284=EDGE_CURVE('',#6681,#6679,#3324,.T.);
#9285=EDGE_CURVE('',#6682,#6683,#4389,.T.);
#9286=EDGE_CURVE('',#6684,#6682,#3325,.T.);
#9287=EDGE_CURVE('',#6678,#6684,#3326,.T.);
#9288=EDGE_CURVE('',#6679,#6685,#3327,.T.);
#9289=EDGE_CURVE('',#6685,#6683,#3328,.T.);
#9290=EDGE_CURVE('',#6686,#6687,#4390,.T.);
#9291=EDGE_CURVE('',#6688,#6686,#3329,.T.);
#9292=EDGE_CURVE('',#6682,#6688,#3330,.T.);
#9293=EDGE_CURVE('',#6683,#6689,#3331,.T.);
#9294=EDGE_CURVE('',#6689,#6687,#3332,.T.);
#9295=EDGE_CURVE('',#6690,#6691,#4391,.T.);
#9296=EDGE_CURVE('',#6692,#6690,#3333,.T.);
#9297=EDGE_CURVE('',#6686,#6692,#3334,.T.);
#9298=EDGE_CURVE('',#6687,#6693,#3335,.T.);
#9299=EDGE_CURVE('',#6693,#6691,#3336,.T.);
#9300=EDGE_CURVE('',#6694,#6695,#4392,.T.);
#9301=EDGE_CURVE('',#6696,#6694,#3337,.T.);
#9302=EDGE_CURVE('',#6690,#6696,#3338,.T.);
#9303=EDGE_CURVE('',#6691,#6697,#3339,.T.);
#9304=EDGE_CURVE('',#6697,#6695,#3340,.T.);
#9305=EDGE_CURVE('',#6698,#6699,#4393,.T.);
#9306=EDGE_CURVE('',#6700,#6698,#3341,.T.);
#9307=EDGE_CURVE('',#6694,#6700,#3342,.T.);
#9308=EDGE_CURVE('',#6695,#6701,#3343,.T.);
#9309=EDGE_CURVE('',#6701,#6699,#3344,.T.);
#9310=EDGE_CURVE('',#6702,#6703,#4394,.T.);
#9311=EDGE_CURVE('',#6704,#6702,#3345,.T.);
#9312=EDGE_CURVE('',#6698,#6704,#3346,.T.);
#9313=EDGE_CURVE('',#6699,#6705,#3347,.T.);
#9314=EDGE_CURVE('',#6705,#6703,#3348,.T.);
#9315=EDGE_CURVE('',#6706,#6707,#4395,.T.);
#9316=EDGE_CURVE('',#6708,#6706,#3349,.T.);
#9317=EDGE_CURVE('',#6702,#6708,#3350,.T.);
#9318=EDGE_CURVE('',#6703,#6709,#3351,.T.);
#9319=EDGE_CURVE('',#6709,#6707,#3352,.T.);
#9320=EDGE_CURVE('',#6710,#6711,#4396,.T.);
#9321=EDGE_CURVE('',#6712,#6710,#3353,.T.);
#9322=EDGE_CURVE('',#6706,#6712,#3354,.T.);
#9323=EDGE_CURVE('',#6707,#6713,#3355,.T.);
#9324=EDGE_CURVE('',#6713,#6711,#3356,.T.);
#9325=EDGE_CURVE('',#6714,#6715,#4397,.T.);
#9326=EDGE_CURVE('',#6716,#6714,#3357,.T.);
#9327=EDGE_CURVE('',#6710,#6716,#3358,.T.);
#9328=EDGE_CURVE('',#6711,#6717,#3359,.T.);
#9329=EDGE_CURVE('',#6717,#6715,#3360,.T.);
#9330=EDGE_CURVE('',#6718,#6719,#4398,.T.);
#9331=EDGE_CURVE('',#6720,#6718,#3361,.T.);
#9332=EDGE_CURVE('',#6714,#6720,#3362,.T.);
#9333=EDGE_CURVE('',#6715,#6721,#3363,.T.);
#9334=EDGE_CURVE('',#6721,#6719,#3364,.T.);
#9335=EDGE_CURVE('',#6722,#6723,#4399,.T.);
#9336=EDGE_CURVE('',#6724,#6722,#3365,.T.);
#9337=EDGE_CURVE('',#6718,#6724,#3366,.T.);
#9338=EDGE_CURVE('',#6719,#6725,#3367,.T.);
#9339=EDGE_CURVE('',#6725,#6723,#3368,.T.);
#9340=EDGE_CURVE('',#6726,#6727,#4400,.T.);
#9341=EDGE_CURVE('',#6728,#6726,#3369,.T.);
#9342=EDGE_CURVE('',#6722,#6728,#3370,.T.);
#9343=EDGE_CURVE('',#6723,#6729,#3371,.T.);
#9344=EDGE_CURVE('',#6729,#6727,#3372,.T.);
#9345=EDGE_CURVE('',#6730,#6731,#4401,.T.);
#9346=EDGE_CURVE('',#6732,#6730,#3373,.T.);
#9347=EDGE_CURVE('',#6726,#6732,#3374,.T.);
#9348=EDGE_CURVE('',#6727,#6733,#3375,.T.);
#9349=EDGE_CURVE('',#6733,#6731,#3376,.T.);
#9350=EDGE_CURVE('',#6734,#6735,#4402,.T.);
#9351=EDGE_CURVE('',#6736,#6734,#3377,.T.);
#9352=EDGE_CURVE('',#6730,#6736,#3378,.T.);
#9353=EDGE_CURVE('',#6731,#6737,#3379,.T.);
#9354=EDGE_CURVE('',#6737,#6735,#3380,.T.);
#9355=EDGE_CURVE('',#6738,#6739,#4403,.T.);
#9356=EDGE_CURVE('',#6740,#6738,#3381,.T.);
#9357=EDGE_CURVE('',#6734,#6740,#3382,.T.);
#9358=EDGE_CURVE('',#6735,#6741,#3383,.T.);
#9359=EDGE_CURVE('',#6741,#6739,#3384,.T.);
#9360=EDGE_CURVE('',#6742,#6743,#4404,.T.);
#9361=EDGE_CURVE('',#6744,#6742,#3385,.T.);
#9362=EDGE_CURVE('',#6738,#6744,#3386,.T.);
#9363=EDGE_CURVE('',#6739,#6745,#3387,.T.);
#9364=EDGE_CURVE('',#6745,#6743,#3388,.T.);
#9365=EDGE_CURVE('',#6746,#6747,#4405,.T.);
#9366=EDGE_CURVE('',#6748,#6746,#3389,.T.);
#9367=EDGE_CURVE('',#6742,#6748,#3390,.T.);
#9368=EDGE_CURVE('',#6743,#6749,#3391,.T.);
#9369=EDGE_CURVE('',#6749,#6747,#3392,.T.);
#9370=EDGE_CURVE('',#6750,#6751,#4406,.T.);
#9371=EDGE_CURVE('',#6752,#6750,#3393,.T.);
#9372=EDGE_CURVE('',#6746,#6752,#3394,.T.);
#9373=EDGE_CURVE('',#6747,#6753,#3395,.T.);
#9374=EDGE_CURVE('',#6753,#6751,#3396,.T.);
#9375=EDGE_CURVE('',#6754,#6755,#4407,.T.);
#9376=EDGE_CURVE('',#6756,#6754,#3397,.T.);
#9377=EDGE_CURVE('',#6750,#6756,#3398,.T.);
#9378=EDGE_CURVE('',#6751,#6757,#3399,.T.);
#9379=EDGE_CURVE('',#6757,#6755,#3400,.T.);
#9380=EDGE_CURVE('',#6758,#6759,#4408,.T.);
#9381=EDGE_CURVE('',#6760,#6758,#3401,.T.);
#9382=EDGE_CURVE('',#6754,#6760,#3402,.T.);
#9383=EDGE_CURVE('',#6755,#6761,#3403,.T.);
#9384=EDGE_CURVE('',#6761,#6759,#3404,.T.);
#9385=EDGE_CURVE('',#6762,#6763,#4409,.T.);
#9386=EDGE_CURVE('',#6764,#6762,#3405,.T.);
#9387=EDGE_CURVE('',#6758,#6764,#3406,.T.);
#9388=EDGE_CURVE('',#6759,#6765,#3407,.T.);
#9389=EDGE_CURVE('',#6765,#6763,#3408,.T.);
#9390=EDGE_CURVE('',#6766,#6767,#4410,.T.);
#9391=EDGE_CURVE('',#6768,#6766,#3409,.T.);
#9392=EDGE_CURVE('',#6762,#6768,#3410,.T.);
#9393=EDGE_CURVE('',#6763,#6769,#3411,.T.);
#9394=EDGE_CURVE('',#6769,#6767,#3412,.T.);
#9395=EDGE_CURVE('',#6770,#6771,#4411,.T.);
#9396=EDGE_CURVE('',#6772,#6770,#3413,.T.);
#9397=EDGE_CURVE('',#6766,#6772,#3414,.T.);
#9398=EDGE_CURVE('',#6767,#6773,#3415,.T.);
#9399=EDGE_CURVE('',#6773,#6771,#3416,.T.);
#9400=EDGE_CURVE('',#6774,#6775,#4412,.T.);
#9401=EDGE_CURVE('',#6776,#6774,#3417,.T.);
#9402=EDGE_CURVE('',#6770,#6776,#3418,.T.);
#9403=EDGE_CURVE('',#6771,#6777,#3419,.T.);
#9404=EDGE_CURVE('',#6777,#6775,#3420,.T.);
#9405=EDGE_CURVE('',#6778,#6779,#4413,.T.);
#9406=EDGE_CURVE('',#6780,#6778,#3421,.T.);
#9407=EDGE_CURVE('',#6774,#6780,#3422,.T.);
#9408=EDGE_CURVE('',#6775,#6781,#3423,.T.);
#9409=EDGE_CURVE('',#6781,#6779,#3424,.T.);
#9410=EDGE_CURVE('',#6782,#6783,#4414,.T.);
#9411=EDGE_CURVE('',#6784,#6782,#3425,.T.);
#9412=EDGE_CURVE('',#6778,#6784,#3426,.T.);
#9413=EDGE_CURVE('',#6779,#6785,#3427,.T.);
#9414=EDGE_CURVE('',#6785,#6783,#3428,.T.);
#9415=EDGE_CURVE('',#6786,#6787,#4415,.T.);
#9416=EDGE_CURVE('',#6788,#6786,#3429,.T.);
#9417=EDGE_CURVE('',#6782,#6788,#3430,.T.);
#9418=EDGE_CURVE('',#6783,#6789,#3431,.T.);
#9419=EDGE_CURVE('',#6789,#6787,#3432,.T.);
#9420=EDGE_CURVE('',#6790,#6791,#4416,.T.);
#9421=EDGE_CURVE('',#6792,#6790,#3433,.T.);
#9422=EDGE_CURVE('',#6786,#6792,#3434,.T.);
#9423=EDGE_CURVE('',#6787,#6793,#3435,.T.);
#9424=EDGE_CURVE('',#6793,#6791,#3436,.T.);
#9425=EDGE_CURVE('',#6794,#6795,#4417,.T.);
#9426=EDGE_CURVE('',#6796,#6794,#3437,.T.);
#9427=EDGE_CURVE('',#6790,#6796,#3438,.T.);
#9428=EDGE_CURVE('',#6791,#6797,#3439,.T.);
#9429=EDGE_CURVE('',#6797,#6795,#3440,.T.);
#9430=EDGE_CURVE('',#6798,#6799,#4418,.T.);
#9431=EDGE_CURVE('',#6800,#6798,#3441,.T.);
#9432=EDGE_CURVE('',#6794,#6800,#3442,.T.);
#9433=EDGE_CURVE('',#6795,#6801,#3443,.T.);
#9434=EDGE_CURVE('',#6801,#6799,#3444,.T.);
#9435=EDGE_CURVE('',#6802,#6803,#4419,.T.);
#9436=EDGE_CURVE('',#6804,#6802,#3445,.T.);
#9437=EDGE_CURVE('',#6798,#6804,#3446,.T.);
#9438=EDGE_CURVE('',#6799,#6805,#3447,.T.);
#9439=EDGE_CURVE('',#6805,#6803,#3448,.T.);
#9440=EDGE_CURVE('',#6806,#6807,#4420,.T.);
#9441=EDGE_CURVE('',#6808,#6806,#3449,.T.);
#9442=EDGE_CURVE('',#6802,#6808,#3450,.T.);
#9443=EDGE_CURVE('',#6803,#6809,#3451,.T.);
#9444=EDGE_CURVE('',#6809,#6807,#3452,.T.);
#9445=EDGE_CURVE('',#6810,#6811,#4421,.T.);
#9446=EDGE_CURVE('',#6812,#6810,#3453,.T.);
#9447=EDGE_CURVE('',#6806,#6812,#3454,.T.);
#9448=EDGE_CURVE('',#6807,#6813,#3455,.T.);
#9449=EDGE_CURVE('',#6813,#6811,#3456,.T.);
#9450=EDGE_CURVE('',#6814,#6815,#4422,.T.);
#9451=EDGE_CURVE('',#6816,#6814,#3457,.T.);
#9452=EDGE_CURVE('',#6810,#6816,#3458,.T.);
#9453=EDGE_CURVE('',#6811,#6817,#3459,.T.);
#9454=EDGE_CURVE('',#6817,#6815,#3460,.T.);
#9455=EDGE_CURVE('',#6818,#6819,#4423,.T.);
#9456=EDGE_CURVE('',#6820,#6818,#3461,.T.);
#9457=EDGE_CURVE('',#6814,#6820,#3462,.T.);
#9458=EDGE_CURVE('',#6815,#6821,#3463,.T.);
#9459=EDGE_CURVE('',#6821,#6819,#3464,.T.);
#9460=EDGE_CURVE('',#6822,#6823,#4424,.T.);
#9461=EDGE_CURVE('',#6824,#6822,#3465,.T.);
#9462=EDGE_CURVE('',#6818,#6824,#3466,.T.);
#9463=EDGE_CURVE('',#6819,#6825,#3467,.T.);
#9464=EDGE_CURVE('',#6825,#6823,#3468,.T.);
#9465=EDGE_CURVE('',#6826,#6827,#4425,.T.);
#9466=EDGE_CURVE('',#6828,#6826,#3469,.T.);
#9467=EDGE_CURVE('',#6822,#6828,#3470,.T.);
#9468=EDGE_CURVE('',#6823,#6829,#3471,.T.);
#9469=EDGE_CURVE('',#6829,#6827,#3472,.T.);
#9470=EDGE_CURVE('',#6830,#6831,#4426,.T.);
#9471=EDGE_CURVE('',#6832,#6830,#3473,.T.);
#9472=EDGE_CURVE('',#6826,#6832,#3474,.T.);
#9473=EDGE_CURVE('',#6827,#6833,#3475,.T.);
#9474=EDGE_CURVE('',#6833,#6831,#3476,.T.);
#9475=EDGE_CURVE('',#6834,#6835,#4427,.T.);
#9476=EDGE_CURVE('',#6836,#6834,#3477,.T.);
#9477=EDGE_CURVE('',#6830,#6836,#3478,.T.);
#9478=EDGE_CURVE('',#6831,#6837,#3479,.T.);
#9479=EDGE_CURVE('',#6837,#6835,#3480,.T.);
#9480=EDGE_CURVE('',#6838,#6839,#4428,.T.);
#9481=EDGE_CURVE('',#6840,#6838,#3481,.T.);
#9482=EDGE_CURVE('',#6834,#6840,#3482,.T.);
#9483=EDGE_CURVE('',#6835,#6841,#3483,.T.);
#9484=EDGE_CURVE('',#6841,#6839,#3484,.T.);
#9485=EDGE_CURVE('',#6842,#6843,#4429,.T.);
#9486=EDGE_CURVE('',#6844,#6842,#3485,.T.);
#9487=EDGE_CURVE('',#6838,#6844,#3486,.T.);
#9488=EDGE_CURVE('',#6839,#6845,#3487,.T.);
#9489=EDGE_CURVE('',#6845,#6843,#3488,.T.);
#9490=EDGE_CURVE('',#6846,#6847,#4430,.T.);
#9491=EDGE_CURVE('',#6848,#6846,#3489,.T.);
#9492=EDGE_CURVE('',#6842,#6848,#3490,.T.);
#9493=EDGE_CURVE('',#6843,#6849,#3491,.T.);
#9494=EDGE_CURVE('',#6849,#6847,#3492,.T.);
#9495=EDGE_CURVE('',#6850,#6851,#4431,.T.);
#9496=EDGE_CURVE('',#6852,#6850,#3493,.T.);
#9497=EDGE_CURVE('',#6846,#6852,#3494,.T.);
#9498=EDGE_CURVE('',#6847,#6853,#3495,.T.);
#9499=EDGE_CURVE('',#6853,#6851,#3496,.T.);
#9500=EDGE_CURVE('',#6854,#6855,#4432,.T.);
#9501=EDGE_CURVE('',#6856,#6854,#3497,.T.);
#9502=EDGE_CURVE('',#6850,#6856,#3498,.T.);
#9503=EDGE_CURVE('',#6851,#6857,#3499,.T.);
#9504=EDGE_CURVE('',#6857,#6855,#3500,.T.);
#9505=EDGE_CURVE('',#6858,#6859,#4433,.T.);
#9506=EDGE_CURVE('',#6860,#6858,#3501,.T.);
#9507=EDGE_CURVE('',#6854,#6860,#3502,.T.);
#9508=EDGE_CURVE('',#6855,#6861,#3503,.T.);
#9509=EDGE_CURVE('',#6861,#6859,#3504,.T.);
#9510=EDGE_CURVE('',#6862,#6863,#4434,.T.);
#9511=EDGE_CURVE('',#6864,#6862,#3505,.T.);
#9512=EDGE_CURVE('',#6858,#6864,#3506,.T.);
#9513=EDGE_CURVE('',#6859,#6865,#3507,.T.);
#9514=EDGE_CURVE('',#6865,#6863,#3508,.T.);
#9515=EDGE_CURVE('',#6866,#6867,#4435,.T.);
#9516=EDGE_CURVE('',#6868,#6866,#3509,.T.);
#9517=EDGE_CURVE('',#6862,#6868,#3510,.T.);
#9518=EDGE_CURVE('',#6863,#6869,#3511,.T.);
#9519=EDGE_CURVE('',#6869,#6867,#3512,.T.);
#9520=EDGE_CURVE('',#6870,#6871,#4436,.T.);
#9521=EDGE_CURVE('',#6872,#6870,#3513,.T.);
#9522=EDGE_CURVE('',#6866,#6872,#3514,.T.);
#9523=EDGE_CURVE('',#6867,#6873,#3515,.T.);
#9524=EDGE_CURVE('',#6873,#6871,#3516,.T.);
#9525=EDGE_CURVE('',#6874,#6875,#4437,.T.);
#9526=EDGE_CURVE('',#6876,#6874,#3517,.T.);
#9527=EDGE_CURVE('',#6870,#6876,#3518,.T.);
#9528=EDGE_CURVE('',#6871,#6877,#3519,.T.);
#9529=EDGE_CURVE('',#6877,#6875,#3520,.T.);
#9530=EDGE_CURVE('',#6878,#6879,#4438,.T.);
#9531=EDGE_CURVE('',#6880,#6878,#3521,.T.);
#9532=EDGE_CURVE('',#6874,#6880,#3522,.T.);
#9533=EDGE_CURVE('',#6875,#6881,#3523,.T.);
#9534=EDGE_CURVE('',#6881,#6879,#3524,.T.);
#9535=EDGE_CURVE('',#6882,#6883,#3525,.T.);
#9536=EDGE_CURVE('',#6884,#6883,#1918,.T.);
#9537=EDGE_CURVE('',#6884,#6885,#3526,.T.);
#9538=EDGE_CURVE('',#6885,#6886,#3527,.T.);
#9539=EDGE_CURVE('',#6886,#6887,#3528,.T.);
#9540=EDGE_CURVE('',#6887,#6888,#3529,.T.);
#9541=EDGE_CURVE('',#6888,#6889,#3530,.T.);
#9542=EDGE_CURVE('',#6889,#6890,#3531,.T.);
#9543=EDGE_CURVE('',#6890,#6891,#3532,.T.);
#9544=EDGE_CURVE('',#6891,#6892,#3533,.T.);
#9545=EDGE_CURVE('',#6892,#6893,#3534,.T.);
#9546=EDGE_CURVE('',#6893,#6894,#3535,.T.);
#9547=EDGE_CURVE('',#6894,#6895,#3536,.T.);
#9548=EDGE_CURVE('',#6895,#6896,#3537,.T.);
#9549=EDGE_CURVE('',#6896,#6897,#3538,.T.);
#9550=EDGE_CURVE('',#6897,#6898,#3539,.T.);
#9551=EDGE_CURVE('',#6898,#6899,#3540,.T.);
#9552=EDGE_CURVE('',#6899,#6900,#3541,.T.);
#9553=EDGE_CURVE('',#6900,#6901,#3542,.T.);
#9554=EDGE_CURVE('',#6901,#6902,#3543,.T.);
#9555=EDGE_CURVE('',#6902,#6903,#3544,.T.);
#9556=EDGE_CURVE('',#6903,#6904,#3545,.T.);
#9557=EDGE_CURVE('',#6904,#6905,#3546,.T.);
#9558=EDGE_CURVE('',#6905,#6906,#3547,.T.);
#9559=EDGE_CURVE('',#6906,#6907,#3548,.T.);
#9560=EDGE_CURVE('',#6907,#6908,#3549,.T.);
#9561=EDGE_CURVE('',#6908,#6909,#3550,.T.);
#9562=EDGE_CURVE('',#6909,#6910,#3551,.T.);
#9563=EDGE_CURVE('',#6910,#6911,#3552,.T.);
#9564=EDGE_CURVE('',#6911,#6912,#3553,.T.);
#9565=EDGE_CURVE('',#6912,#6913,#3554,.T.);
#9566=EDGE_CURVE('',#6913,#6914,#3555,.T.);
#9567=EDGE_CURVE('',#6914,#6915,#3556,.T.);
#9568=EDGE_CURVE('',#6915,#6916,#3557,.T.);
#9569=EDGE_CURVE('',#6916,#6917,#3558,.T.);
#9570=EDGE_CURVE('',#6917,#6918,#3559,.T.);
#9571=EDGE_CURVE('',#6918,#6919,#3560,.T.);
#9572=EDGE_CURVE('',#6919,#6920,#3561,.T.);
#9573=EDGE_CURVE('',#6920,#6921,#3562,.T.);
#9574=EDGE_CURVE('',#6921,#6922,#3563,.T.);
#9575=EDGE_CURVE('',#6922,#6923,#3564,.T.);
#9576=EDGE_CURVE('',#6923,#6924,#3565,.T.);
#9577=EDGE_CURVE('',#6924,#6925,#3566,.T.);
#9578=EDGE_CURVE('',#6925,#6926,#3567,.T.);
#9579=EDGE_CURVE('',#6926,#6927,#3568,.T.);
#9580=EDGE_CURVE('',#6927,#6928,#3569,.T.);
#9581=EDGE_CURVE('',#6928,#6929,#3570,.T.);
#9582=EDGE_CURVE('',#6929,#6930,#3571,.T.);
#9583=EDGE_CURVE('',#6930,#6931,#3572,.T.);
#9584=EDGE_CURVE('',#6931,#6932,#3573,.T.);
#9585=EDGE_CURVE('',#6932,#6933,#3574,.T.);
#9586=EDGE_CURVE('',#6934,#6933,#1919,.F.);
#9587=EDGE_CURVE('',#6934,#6935,#3575,.T.);
#9588=EDGE_CURVE('',#6935,#6936,#3576,.T.);
#9589=EDGE_CURVE('',#6936,#6937,#3577,.T.);
#9590=EDGE_CURVE('',#6937,#6938,#3578,.T.);
#9591=EDGE_CURVE('',#6938,#6939,#3579,.T.);
#9592=EDGE_CURVE('',#6939,#6940,#3580,.T.);
#9593=EDGE_CURVE('',#6940,#6941,#3581,.T.);
#9594=EDGE_CURVE('',#6941,#6942,#3582,.T.);
#9595=EDGE_CURVE('',#6942,#6943,#3583,.T.);
#9596=EDGE_CURVE('',#6943,#6944,#3584,.T.);
#9597=EDGE_CURVE('',#6944,#6945,#3585,.T.);
#9598=EDGE_CURVE('',#6945,#6946,#3586,.T.);
#9599=EDGE_CURVE('',#6946,#6947,#3587,.T.);
#9600=EDGE_CURVE('',#6947,#6948,#3588,.T.);
#9601=EDGE_CURVE('',#6948,#6949,#3589,.T.);
#9602=EDGE_CURVE('',#6949,#6950,#3590,.T.);
#9603=EDGE_CURVE('',#6950,#6951,#3591,.T.);
#9604=EDGE_CURVE('',#6951,#6952,#3592,.T.);
#9605=EDGE_CURVE('',#6952,#6953,#3593,.T.);
#9606=EDGE_CURVE('',#6953,#6954,#3594,.T.);
#9607=EDGE_CURVE('',#6954,#6955,#3595,.T.);
#9608=EDGE_CURVE('',#6955,#6956,#3596,.T.);
#9609=EDGE_CURVE('',#6956,#6957,#3597,.T.);
#9610=EDGE_CURVE('',#6957,#6958,#3598,.T.);
#9611=EDGE_CURVE('',#6958,#6959,#3599,.T.);
#9612=EDGE_CURVE('',#6959,#6960,#3600,.T.);
#9613=EDGE_CURVE('',#6960,#6961,#3601,.T.);
#9614=EDGE_CURVE('',#6961,#6962,#3602,.T.);
#9615=EDGE_CURVE('',#6962,#6963,#3603,.T.);
#9616=EDGE_CURVE('',#6963,#6964,#3604,.T.);
#9617=EDGE_CURVE('',#6964,#6965,#3605,.T.);
#9618=EDGE_CURVE('',#6965,#6966,#3606,.T.);
#9619=EDGE_CURVE('',#6966,#6967,#3607,.T.);
#9620=EDGE_CURVE('',#6967,#6968,#3608,.T.);
#9621=EDGE_CURVE('',#6968,#6969,#3609,.T.);
#9622=EDGE_CURVE('',#6969,#6970,#3610,.T.);
#9623=EDGE_CURVE('',#6970,#6971,#3611,.T.);
#9624=EDGE_CURVE('',#6971,#6972,#3612,.T.);
#9625=EDGE_CURVE('',#6972,#6973,#3613,.T.);
#9626=EDGE_CURVE('',#6973,#6974,#3614,.T.);
#9627=EDGE_CURVE('',#6974,#6975,#3615,.T.);
#9628=EDGE_CURVE('',#6975,#6976,#3616,.T.);
#9629=EDGE_CURVE('',#6976,#6977,#3617,.T.);
#9630=EDGE_CURVE('',#6977,#6978,#3618,.T.);
#9631=EDGE_CURVE('',#6978,#6979,#3619,.T.);
#9632=EDGE_CURVE('',#6979,#6980,#3620,.T.);
#9633=EDGE_CURVE('',#6980,#6882,#3621,.T.);
#9634=EDGE_CURVE('',#6879,#6981,#3622,.T.);
#9635=EDGE_CURVE('',#6981,#6982,#3623,.T.);
#9636=EDGE_CURVE('',#6983,#6982,#1920,.T.);
#9637=EDGE_CURVE('',#6984,#6983,#3624,.T.);
#9638=EDGE_CURVE('',#6878,#6984,#3625,.T.);
#9639=EDGE_CURVE('',#6985,#6986,#3626,.T.);
#9640=EDGE_CURVE('',#6987,#6985,#3627,.T.);
#9641=EDGE_CURVE('',#6986,#6987,#3628,.T.);
#9642=EDGE_CURVE('',#6986,#6988,#4439,.T.);
#9643=EDGE_CURVE('',#6989,#6988,#3629,.T.);
#9644=EDGE_CURVE('',#6990,#6989,#3630,.T.);
#9645=EDGE_CURVE('',#6988,#6990,#3631,.T.);
#9646=EDGE_CURVE('',#6933,#6983,#3632,.T.);
#9647=EDGE_CURVE('',#6624,#6884,#3633,.T.);
#9648=EDGE_CURVE('',#6982,#6934,#3634,.T.);
#9649=EDGE_CURVE('',#6883,#6625,#3635,.T.);
#9650=EDGE_CURVE('',#6991,#6991,#1921,.T.);
#9651=EDGE_CURVE('',#6992,#6992,#1922,.T.);
#9652=EDGE_CURVE('',#6993,#6993,#1923,.T.);
#9653=EDGE_CURVE('',#6993,#6991,#4440,.T.);
#9654=EDGE_CURVE('',#6992,#6989,#4441,.T.);
#9655=EDGE_CURVE('',#6990,#6994,#4442,.T.);
#9656=EDGE_CURVE('',#6994,#6994,#1924,.T.);
#9657=EDGE_CURVE('',#6995,#6996,#3636,.T.);
#9658=EDGE_CURVE('',#6997,#6995,#3637,.T.);
#9659=EDGE_CURVE('',#6996,#6997,#3638,.T.);
#9660=EDGE_CURVE('',#6996,#6998,#4443,.T.);
#9661=EDGE_CURVE('',#6998,#6998,#3639,.T.);
#9662=EDGE_CURVE('',#6999,#7000,#3640,.T.);
#9663=EDGE_CURVE('',#7001,#6999,#3641,.T.);
#9664=EDGE_CURVE('',#7000,#7001,#3642,.T.);
#9665=EDGE_CURVE('',#7000,#7002,#4444,.T.);
#9666=EDGE_CURVE('',#7003,#7002,#3643,.T.);
#9667=EDGE_CURVE('',#7004,#7003,#3644,.T.);
#9668=EDGE_CURVE('',#7002,#7004,#3645,.T.);
#9669=EDGE_CURVE('',#7005,#7005,#1925,.T.);
#9670=EDGE_CURVE('',#7005,#7006,#4445,.T.);
#9671=EDGE_CURVE('',#7006,#7006,#1926,.T.);
#9672=EDGE_CURVE('',#7007,#7007,#1927,.T.);
#9673=EDGE_CURVE('',#7007,#7008,#4446,.T.);
#9674=EDGE_CURVE('',#7008,#7008,#1928,.T.);
#9675=EDGE_CURVE('',#7009,#7009,#1929,.T.);
#9676=EDGE_CURVE('',#7009,#7010,#4447,.T.);
#9677=EDGE_CURVE('',#7010,#7010,#1930,.T.);
#9678=EDGE_CURVE('',#7011,#7011,#1931,.T.);
#9679=EDGE_CURVE('',#7011,#7012,#4448,.T.);
#9680=EDGE_CURVE('',#7012,#7012,#1932,.T.);
#9681=EDGE_CURVE('',#7013,#7013,#1933,.T.);
#9682=EDGE_CURVE('',#7013,#7014,#4449,.T.);
#9683=EDGE_CURVE('',#7014,#7014,#1934,.T.);
#9684=EDGE_CURVE('',#7015,#7015,#1935,.T.);
#9685=EDGE_CURVE('',#7015,#7016,#4450,.T.);
#9686=EDGE_CURVE('',#7016,#7016,#1936,.T.);
#9687=EDGE_CURVE('',#7017,#7017,#1937,.T.);
#9688=EDGE_CURVE('',#7017,#7003,#4451,.T.);
#9689=EDGE_CURVE('',#7004,#7018,#4452,.T.);
#9690=EDGE_CURVE('',#7018,#7018,#1938,.T.);
#9691=EDGE_CURVE('',#7019,#7019,#1939,.T.);
#9692=EDGE_CURVE('',#7020,#7020,#1940,.T.);
#9693=EDGE_CURVE('',#7020,#6999,#4453,.T.);
#9694=EDGE_CURVE('',#7001,#7019,#4454,.T.);
#9695=EDGE_CURVE('',#7021,#7021,#1941,.F.);
#9696=EDGE_CURVE('',#7021,#7022,#4455,.T.);
#9697=EDGE_CURVE('',#7022,#7022,#1942,.F.);
#9698=EDGE_CURVE('',#7023,#7023,#1943,.T.);
#9699=EDGE_CURVE('',#7023,#7024,#4456,.T.);
#9700=EDGE_CURVE('',#7024,#7024,#1944,.T.);
#9701=EDGE_CURVE('',#7025,#7025,#1945,.T.);
#9702=EDGE_CURVE('',#7026,#7026,#1946,.T.);
#9703=EDGE_CURVE('',#7027,#7027,#1947,.T.);
#9704=EDGE_CURVE('',#7027,#7026,#4457,.T.);
#9705=EDGE_CURVE('',#7028,#7028,#1948,.T.);
#9706=EDGE_CURVE('',#7029,#7029,#1949,.T.);
#9707=EDGE_CURVE('',#7028,#7030,#4458,.T.);
#9708=EDGE_CURVE('',#7030,#7030,#1950,.T.);
#9709=EDGE_CURVE('',#7025,#7029,#4459,.T.);
#9710=EDGE_CURVE('',#7031,#7031,#1951,.T.);
#9711=EDGE_CURVE('',#7031,#7032,#4460,.T.);
#9712=EDGE_CURVE('',#7032,#7032,#1952,.T.);
#9713=EDGE_CURVE('',#7033,#7033,#1953,.T.);
#9714=EDGE_CURVE('',#7033,#7034,#4461,.T.);
#9715=EDGE_CURVE('',#7034,#7034,#1954,.T.);
#9716=EDGE_CURVE('',#7035,#7036,#4462,.T.);
#9717=EDGE_CURVE('',#7037,#7035,#4463,.T.);
#9718=EDGE_CURVE('',#7038,#7037,#4464,.T.);
#9719=EDGE_CURVE('',#7036,#7038,#4465,.T.);
#9720=EDGE_CURVE('',#7039,#7040,#4466,.T.);
#9721=EDGE_CURVE('',#7041,#7039,#4467,.T.);
#9722=EDGE_CURVE('',#7042,#7041,#4468,.T.);
#9723=EDGE_CURVE('',#7040,#7042,#4469,.T.);
#9724=EDGE_CURVE('',#7037,#7042,#1955,.T.);
#9725=EDGE_CURVE('',#7040,#7035,#1956,.T.);
#9726=EDGE_CURVE('',#7039,#7036,#1957,.T.);
#9727=EDGE_CURVE('',#7038,#7041,#1958,.T.);
#9728=EDGE_CURVE('',#7043,#7043,#1959,.T.);
#9729=EDGE_CURVE('',#7043,#7044,#4470,.T.);
#9730=EDGE_CURVE('',#7044,#7044,#1960,.T.);
#9731=EDGE_CURVE('',#7045,#7045,#1961,.T.);
#9732=EDGE_CURVE('',#7045,#7046,#4471,.T.);
#9733=EDGE_CURVE('',#7046,#7046,#1962,.T.);
#9734=EDGE_CURVE('',#7047,#7048,#4472,.T.);
#9735=EDGE_CURVE('',#7049,#7047,#1963,.T.);
#9736=EDGE_CURVE('',#7050,#7049,#3646,.T.);
#9737=EDGE_CURVE('',#7051,#7050,#1964,.T.);
#9738=EDGE_CURVE('',#7051,#7052,#4473,.T.);
#9739=EDGE_CURVE('',#7052,#7052,#1965,.T.);
#9740=EDGE_CURVE('',#7053,#7051,#1966,.T.);
#9741=EDGE_CURVE('',#7048,#7053,#3647,.T.);
#9742=EDGE_CURVE('',#7054,#7055,#4474,.T.);
#9743=EDGE_CURVE('',#7056,#7054,#3648,.T.);
#9744=EDGE_CURVE('',#7057,#7056,#1967,.T.);
#9745=EDGE_CURVE('',#7057,#7055,#3649,.T.);
#9746=EDGE_CURVE('',#7058,#7059,#4475,.T.);
#9747=EDGE_CURVE('',#7054,#7058,#3650,.F.);
#9748=EDGE_CURVE('',#7055,#7059,#3651,.T.);
#9749=EDGE_CURVE('',#7060,#7061,#4476,.T.);
#9750=EDGE_CURVE('',#7062,#7060,#3652,.F.);
#9751=EDGE_CURVE('',#7058,#7062,#3653,.F.);
#9752=EDGE_CURVE('',#7059,#7061,#3654,.T.);
#9753=EDGE_CURVE('',#7063,#7064,#4477,.T.);
#9754=EDGE_CURVE('',#7060,#7063,#3655,.F.);
#9755=EDGE_CURVE('',#7061,#7065,#3656,.T.);
#9756=EDGE_CURVE('',#7065,#7064,#3657,.T.);
#9757=EDGE_CURVE('',#7066,#7067,#4478,.T.);
#9758=EDGE_CURVE('',#7063,#7066,#3658,.F.);
#9759=EDGE_CURVE('',#7064,#7068,#3659,.T.);
#9760=EDGE_CURVE('',#7068,#7067,#3660,.T.);
#9761=EDGE_CURVE('',#7069,#7070,#4479,.T.);
#9762=EDGE_CURVE('',#7071,#7069,#3661,.F.);
#9763=EDGE_CURVE('',#7066,#7071,#3662,.F.);
#9764=EDGE_CURVE('',#7067,#7070,#3663,.T.);
#9765=EDGE_CURVE('',#7072,#7073,#4480,.T.);
#9766=EDGE_CURVE('',#7074,#7072,#3664,.F.);
#9767=EDGE_CURVE('',#7069,#7074,#3665,.F.);
#9768=EDGE_CURVE('',#7070,#7075,#3666,.T.);
#9769=EDGE_CURVE('',#7075,#7073,#3667,.T.);
#9770=EDGE_CURVE('',#7076,#7077,#4481,.T.);
#9771=EDGE_CURVE('',#7072,#7076,#3668,.F.);
#9772=EDGE_CURVE('',#7073,#7077,#3669,.T.);
#9773=EDGE_CURVE('',#7078,#7079,#4482,.T.);
#9774=EDGE_CURVE('',#7076,#7078,#3670,.F.);
#9775=EDGE_CURVE('',#7077,#7079,#3671,.T.);
#9776=EDGE_CURVE('',#7080,#7081,#4483,.T.);
#9777=EDGE_CURVE('',#7082,#7080,#3672,.F.);
#9778=EDGE_CURVE('',#7078,#7082,#3673,.F.);
#9779=EDGE_CURVE('',#7079,#7083,#3674,.T.);
#9780=EDGE_CURVE('',#7083,#7081,#3675,.T.);
#9781=EDGE_CURVE('',#7084,#7085,#4484,.T.);
#9782=EDGE_CURVE('',#7080,#7084,#3676,.F.);
#9783=EDGE_CURVE('',#7081,#7086,#3677,.T.);
#9784=EDGE_CURVE('',#7086,#7085,#3678,.T.);
#9785=EDGE_CURVE('',#7087,#7088,#4485,.T.);
#9786=EDGE_CURVE('',#7089,#7087,#3679,.F.);
#9787=EDGE_CURVE('',#7084,#7089,#3680,.F.);
#9788=EDGE_CURVE('',#7085,#7088,#3681,.T.);
#9789=EDGE_CURVE('',#7090,#7091,#4486,.T.);
#9790=EDGE_CURVE('',#7092,#7090,#3682,.F.);
#9791=EDGE_CURVE('',#7087,#7092,#3683,.F.);
#9792=EDGE_CURVE('',#7088,#7091,#3684,.T.);
#9793=EDGE_CURVE('',#7093,#7094,#4487,.T.);
#9794=EDGE_CURVE('',#7090,#7093,#3685,.F.);
#9795=EDGE_CURVE('',#7091,#7095,#3686,.T.);
#9796=EDGE_CURVE('',#7095,#7094,#3687,.T.);
#9797=EDGE_CURVE('',#7096,#7097,#4488,.T.);
#9798=EDGE_CURVE('',#7093,#7096,#3688,.F.);
#9799=EDGE_CURVE('',#7094,#7097,#3689,.T.);
#9800=EDGE_CURVE('',#7051,#7098,#4489,.T.);
#9801=EDGE_CURVE('',#7096,#7050,#3690,.T.);
#9802=EDGE_CURVE('',#7097,#7098,#3691,.T.);
#9803=EDGE_CURVE('',#7099,#7100,#3692,.T.);
#9804=EDGE_CURVE('',#7100,#7101,#1968,.F.);
#9805=EDGE_CURVE('',#7101,#7102,#3693,.T.);
#9806=EDGE_CURVE('',#7102,#7103,#3694,.T.);
#9807=EDGE_CURVE('',#7103,#7104,#3695,.T.);
#9808=EDGE_CURVE('',#7104,#7105,#3696,.T.);
#9809=EDGE_CURVE('',#7105,#7106,#3697,.T.);
#9810=EDGE_CURVE('',#7106,#7107,#3698,.T.);
#9811=EDGE_CURVE('',#7107,#7108,#3699,.T.);
#9812=EDGE_CURVE('',#7108,#7109,#3700,.T.);
#9813=EDGE_CURVE('',#7109,#7110,#3701,.T.);
#9814=EDGE_CURVE('',#7110,#7111,#3702,.T.);
#9815=EDGE_CURVE('',#7111,#7112,#3703,.T.);
#9816=EDGE_CURVE('',#7112,#7113,#3704,.T.);
#9817=EDGE_CURVE('',#7113,#7114,#3705,.T.);
#9818=EDGE_CURVE('',#7114,#7115,#3706,.T.);
#9819=EDGE_CURVE('',#7115,#7116,#3707,.T.);
#9820=EDGE_CURVE('',#7116,#7117,#3708,.T.);
#9821=EDGE_CURVE('',#7117,#7049,#3709,.T.);
#9822=EDGE_CURVE('',#7047,#7118,#1969,.T.);
#9823=EDGE_CURVE('',#7118,#7119,#3710,.T.);
#9824=EDGE_CURVE('',#7119,#7120,#3711,.T.);
#9825=EDGE_CURVE('',#7120,#7121,#3712,.T.);
#9826=EDGE_CURVE('',#7121,#7122,#3713,.T.);
#9827=EDGE_CURVE('',#7122,#7123,#3714,.T.);
#9828=EDGE_CURVE('',#7123,#7124,#3715,.T.);
#9829=EDGE_CURVE('',#7124,#7125,#3716,.T.);
#9830=EDGE_CURVE('',#7125,#7126,#3717,.T.);
#9831=EDGE_CURVE('',#7126,#7127,#3718,.T.);
#9832=EDGE_CURVE('',#7127,#7128,#3719,.T.);
#9833=EDGE_CURVE('',#7128,#7129,#3720,.T.);
#9834=EDGE_CURVE('',#7129,#7130,#3721,.T.);
#9835=EDGE_CURVE('',#7130,#7131,#3722,.T.);
#9836=EDGE_CURVE('',#7131,#7132,#3723,.T.);
#9837=EDGE_CURVE('',#7132,#7099,#3724,.T.);
#9838=EDGE_CURVE('',#7098,#7053,#3725,.T.);
#9839=EDGE_CURVE('',#7118,#7048,#3726,.T.);
#9840=EDGE_CURVE('',#7100,#7057,#3727,.T.);
#9841=EDGE_CURVE('',#7056,#7101,#3728,.T.);
#9842=EDGE_CURVE('',#7133,#7134,#4490,.T.);
#9843=EDGE_CURVE('',#7133,#7135,#4491,.T.);
#9844=EDGE_CURVE('',#7135,#7136,#4492,.T.);
#9845=EDGE_CURVE('',#7134,#7136,#4493,.T.);
#9846=EDGE_CURVE('',#7137,#7133,#4494,.T.);
#9847=EDGE_CURVE('',#7137,#7138,#4495,.T.);
#9848=EDGE_CURVE('',#7138,#7135,#4496,.T.);
#9849=EDGE_CURVE('',#7139,#7137,#4497,.T.);
#9850=EDGE_CURVE('',#7139,#7140,#4498,.T.);
#9851=EDGE_CURVE('',#7140,#7138,#4499,.T.);
#9852=EDGE_CURVE('',#7141,#7139,#4500,.T.);
#9853=EDGE_CURVE('',#7141,#7142,#4501,.T.);
#9854=EDGE_CURVE('',#7142,#7140,#4502,.T.);
#9855=EDGE_CURVE('',#7143,#7141,#4503,.T.);
#9856=EDGE_CURVE('',#7143,#7144,#4504,.T.);
#9857=EDGE_CURVE('',#7144,#7142,#4505,.T.);
#9858=EDGE_CURVE('',#7134,#7143,#4506,.T.);
#9859=EDGE_CURVE('',#7136,#7144,#4507,.T.);
#9860=EDGE_CURVE('',#7145,#7145,#1970,.T.);
#9861=EDGE_CURVE('',#7145,#7146,#4508,.T.);
#9862=EDGE_CURVE('',#7146,#7146,#1971,.T.);
#9863=EDGE_CURVE('',#7147,#7148,#4509,.T.);
#9864=EDGE_CURVE('',#7149,#7147,#1972,.T.);
#9865=EDGE_CURVE('',#7150,#7149,#3729,.T.);
#9866=EDGE_CURVE('',#7151,#7150,#1973,.T.);
#9867=EDGE_CURVE('',#7151,#7152,#4510,.T.);
#9868=EDGE_CURVE('',#7152,#7152,#1974,.T.);
#9869=EDGE_CURVE('',#7153,#7151,#1975,.T.);
#9870=EDGE_CURVE('',#7148,#7153,#3730,.T.);
#9871=EDGE_CURVE('',#7154,#7155,#4511,.T.);
#9872=EDGE_CURVE('',#7156,#7154,#3731,.T.);
#9873=EDGE_CURVE('',#7157,#7156,#1976,.T.);
#9874=EDGE_CURVE('',#7157,#7155,#3732,.T.);
#9875=EDGE_CURVE('',#7158,#7159,#4512,.T.);
#9876=EDGE_CURVE('',#7160,#7158,#3733,.F.);
#9877=EDGE_CURVE('',#7154,#7160,#3734,.T.);
#9878=EDGE_CURVE('',#7155,#7161,#3735,.T.);
#9879=EDGE_CURVE('',#7161,#7159,#3736,.T.);
#9880=EDGE_CURVE('',#7162,#7163,#4513,.T.);
#9881=EDGE_CURVE('',#7158,#7162,#3737,.F.);
#9882=EDGE_CURVE('',#7159,#7163,#3738,.T.);
#9883=EDGE_CURVE('',#7164,#7165,#4514,.T.);
#9884=EDGE_CURVE('',#7166,#7164,#3739,.F.);
#9885=EDGE_CURVE('',#7162,#7166,#3740,.F.);
#9886=EDGE_CURVE('',#7163,#7167,#3741,.T.);
#9887=EDGE_CURVE('',#7167,#7165,#3742,.T.);
#9888=EDGE_CURVE('',#7168,#7169,#4515,.T.);
#9889=EDGE_CURVE('',#7164,#7168,#3743,.F.);
#9890=EDGE_CURVE('',#7165,#7169,#3744,.T.);
#9891=EDGE_CURVE('',#7170,#7171,#4516,.T.);
#9892=EDGE_CURVE('',#7172,#7170,#3745,.F.);
#9893=EDGE_CURVE('',#7168,#7172,#3746,.F.);
#9894=EDGE_CURVE('',#7169,#7173,#3747,.T.);
#9895=EDGE_CURVE('',#7173,#7171,#3748,.T.);
#9896=EDGE_CURVE('',#7174,#7175,#4517,.T.);
#9897=EDGE_CURVE('',#7170,#7174,#3749,.F.);
#9898=EDGE_CURVE('',#7171,#7175,#3750,.T.);
#9899=EDGE_CURVE('',#7176,#7177,#4518,.T.);
#9900=EDGE_CURVE('',#7178,#7176,#3751,.F.);
#9901=EDGE_CURVE('',#7174,#7178,#3752,.F.);
#9902=EDGE_CURVE('',#7175,#7179,#3753,.T.);
#9903=EDGE_CURVE('',#7179,#7177,#3754,.T.);
#9904=EDGE_CURVE('',#7180,#7181,#4519,.T.);
#9905=EDGE_CURVE('',#7176,#7180,#3755,.F.);
#9906=EDGE_CURVE('',#7177,#7182,#3756,.T.);
#9907=EDGE_CURVE('',#7182,#7181,#3757,.T.);
#9908=EDGE_CURVE('',#7183,#7184,#4520,.T.);
#9909=EDGE_CURVE('',#7185,#7183,#3758,.T.);
#9910=EDGE_CURVE('',#7180,#7185,#3759,.F.);
#9911=EDGE_CURVE('',#7181,#7184,#3760,.T.);
#9912=EDGE_CURVE('',#7186,#7187,#4521,.T.);
#9913=EDGE_CURVE('',#7188,#7186,#3761,.F.);
#9914=EDGE_CURVE('',#7183,#7188,#3762,.T.);
#9915=EDGE_CURVE('',#7184,#7189,#3763,.T.);
#9916=EDGE_CURVE('',#7189,#7187,#3764,.T.);
#9917=EDGE_CURVE('',#7190,#7191,#4522,.T.);
#9918=EDGE_CURVE('',#7186,#7190,#3765,.F.);
#9919=EDGE_CURVE('',#7187,#7191,#3766,.T.);
#9920=EDGE_CURVE('',#7192,#7193,#4523,.T.);
#9921=EDGE_CURVE('',#7194,#7192,#3767,.T.);
#9922=EDGE_CURVE('',#7190,#7194,#3768,.F.);
#9923=EDGE_CURVE('',#7191,#7195,#3769,.T.);
#9924=EDGE_CURVE('',#7195,#7193,#3770,.T.);
#9925=EDGE_CURVE('',#7196,#7197,#4524,.T.);
#9926=EDGE_CURVE('',#7198,#7196,#3771,.F.);
#9927=EDGE_CURVE('',#7192,#7198,#3772,.T.);
#9928=EDGE_CURVE('',#7193,#7197,#3773,.T.);
#9929=EDGE_CURVE('',#7199,#7200,#4525,.T.);
#9930=EDGE_CURVE('',#7196,#7199,#3774,.F.);
#9931=EDGE_CURVE('',#7197,#7201,#3775,.T.);
#9932=EDGE_CURVE('',#7201,#7200,#3776,.T.);
#9933=EDGE_CURVE('',#7202,#7203,#4526,.T.);
#9934=EDGE_CURVE('',#7204,#7202,#3777,.F.);
#9935=EDGE_CURVE('',#7199,#7204,#3778,.F.);
#9936=EDGE_CURVE('',#7200,#7203,#3779,.T.);
#9937=EDGE_CURVE('',#7205,#7206,#4527,.T.);
#9938=EDGE_CURVE('',#7202,#7205,#3780,.F.);
#9939=EDGE_CURVE('',#7203,#7207,#3781,.T.);
#9940=EDGE_CURVE('',#7207,#7206,#3782,.T.);
#9941=EDGE_CURVE('',#7208,#7209,#4528,.T.);
#9942=EDGE_CURVE('',#7210,#7208,#3783,.F.);
#9943=EDGE_CURVE('',#7205,#7210,#3784,.F.);
#9944=EDGE_CURVE('',#7206,#7211,#3785,.T.);
#9945=EDGE_CURVE('',#7211,#7209,#3786,.T.);
#9946=EDGE_CURVE('',#7212,#7213,#4529,.T.);
#9947=EDGE_CURVE('',#7208,#7212,#3787,.F.);
#9948=EDGE_CURVE('',#7209,#7214,#3788,.T.);
#9949=EDGE_CURVE('',#7214,#7213,#3789,.T.);
#9950=EDGE_CURVE('',#7215,#7216,#4530,.T.);
#9951=EDGE_CURVE('',#7217,#7215,#3790,.F.);
#9952=EDGE_CURVE('',#7212,#7217,#3791,.F.);
#9953=EDGE_CURVE('',#7213,#7216,#3792,.T.);
#9954=EDGE_CURVE('',#7218,#7219,#4531,.T.);
#9955=EDGE_CURVE('',#7215,#7218,#3793,.F.);
#9956=EDGE_CURVE('',#7216,#7220,#3794,.T.);
#9957=EDGE_CURVE('',#7220,#7219,#3795,.T.);
#9958=EDGE_CURVE('',#7221,#7222,#4532,.T.);
#9959=EDGE_CURVE('',#7223,#7221,#3796,.F.);
#9960=EDGE_CURVE('',#7218,#7223,#3797,.F.);
#9961=EDGE_CURVE('',#7219,#7222,#3798,.T.);
#9962=EDGE_CURVE('',#7224,#7225,#4533,.T.);
#9963=EDGE_CURVE('',#7221,#7224,#3799,.F.);
#9964=EDGE_CURVE('',#7222,#7226,#3800,.T.);
#9965=EDGE_CURVE('',#7226,#7225,#3801,.T.);
#9966=EDGE_CURVE('',#7227,#7228,#4534,.T.);
#9967=EDGE_CURVE('',#7229,#7227,#3802,.F.);
#9968=EDGE_CURVE('',#7224,#7229,#3803,.F.);
#9969=EDGE_CURVE('',#7225,#7228,#3804,.T.);
#9970=EDGE_CURVE('',#7230,#7231,#4535,.T.);
#9971=EDGE_CURVE('',#7227,#7230,#3805,.F.);
#9972=EDGE_CURVE('',#7228,#7232,#3806,.T.);
#9973=EDGE_CURVE('',#7232,#7231,#3807,.T.);
#9974=EDGE_CURVE('',#7233,#7234,#4536,.T.);
#9975=EDGE_CURVE('',#7235,#7233,#3808,.F.);
#9976=EDGE_CURVE('',#7230,#7235,#3809,.F.);
#9977=EDGE_CURVE('',#7231,#7234,#3810,.T.);
#9978=EDGE_CURVE('',#7236,#7237,#4537,.T.);
#9979=EDGE_CURVE('',#7233,#7236,#3811,.F.);
#9980=EDGE_CURVE('',#7234,#7238,#3812,.T.);
#9981=EDGE_CURVE('',#7238,#7237,#3813,.T.);
#9982=EDGE_CURVE('',#7239,#7240,#4538,.T.);
#9983=EDGE_CURVE('',#7241,#7239,#3814,.T.);
#9984=EDGE_CURVE('',#7236,#7241,#3815,.F.);
#9985=EDGE_CURVE('',#7237,#7242,#3816,.T.);
#9986=EDGE_CURVE('',#7242,#7240,#3817,.T.);
#9987=EDGE_CURVE('',#7243,#7244,#3818,.T.);
#9988=EDGE_CURVE('',#7244,#7245,#1977,.F.);
#9989=EDGE_CURVE('',#7245,#7246,#3819,.T.);
#9990=EDGE_CURVE('',#7246,#7247,#3820,.T.);
#9991=EDGE_CURVE('',#7247,#7248,#3821,.T.);
#9992=EDGE_CURVE('',#7248,#7249,#3822,.T.);
#9993=EDGE_CURVE('',#7249,#7250,#3823,.T.);
#9994=EDGE_CURVE('',#7250,#7251,#3824,.T.);
#9995=EDGE_CURVE('',#7251,#7252,#3825,.T.);
#9996=EDGE_CURVE('',#7252,#7253,#3826,.T.);
#9997=EDGE_CURVE('',#7253,#7254,#3827,.T.);
#9998=EDGE_CURVE('',#7254,#7255,#3828,.T.);
#9999=EDGE_CURVE('',#7255,#7256,#3829,.T.);
#10000=EDGE_CURVE('',#7256,#7257,#3830,.T.);
#10001=EDGE_CURVE('',#7257,#7258,#3831,.T.);
#10002=EDGE_CURVE('',#7258,#7259,#3832,.T.);
#10003=EDGE_CURVE('',#7259,#7260,#3833,.T.);
#10004=EDGE_CURVE('',#7260,#7261,#3834,.T.);
#10005=EDGE_CURVE('',#7261,#7262,#3835,.T.);
#10006=EDGE_CURVE('',#7262,#7263,#3836,.T.);
#10007=EDGE_CURVE('',#7263,#7264,#3837,.T.);
#10008=EDGE_CURVE('',#7264,#7265,#3838,.T.);
#10009=EDGE_CURVE('',#7265,#7266,#3839,.T.);
#10010=EDGE_CURVE('',#7266,#7267,#3840,.T.);
#10011=EDGE_CURVE('',#7267,#7268,#3841,.T.);
#10012=EDGE_CURVE('',#7268,#7269,#3842,.T.);
#10013=EDGE_CURVE('',#7269,#7270,#3843,.T.);
#10014=EDGE_CURVE('',#7270,#7271,#3844,.T.);
#10015=EDGE_CURVE('',#7271,#7272,#3845,.T.);
#10016=EDGE_CURVE('',#7272,#7273,#3846,.T.);
#10017=EDGE_CURVE('',#7273,#7149,#1978,.T.);
#10018=EDGE_CURVE('',#7147,#7274,#1979,.T.);
#10019=EDGE_CURVE('',#7274,#7275,#3847,.T.);
#10020=EDGE_CURVE('',#7275,#7276,#3848,.T.);
#10021=EDGE_CURVE('',#7276,#7277,#3849,.T.);
#10022=EDGE_CURVE('',#7277,#7278,#3850,.T.);
#10023=EDGE_CURVE('',#7278,#7279,#3851,.T.);
#10024=EDGE_CURVE('',#7279,#7280,#3852,.T.);
#10025=EDGE_CURVE('',#7280,#7281,#3853,.T.);
#10026=EDGE_CURVE('',#7281,#7282,#3854,.T.);
#10027=EDGE_CURVE('',#7282,#7283,#3855,.T.);
#10028=EDGE_CURVE('',#7283,#7284,#3856,.T.);
#10029=EDGE_CURVE('',#7284,#7285,#3857,.T.);
#10030=EDGE_CURVE('',#7285,#7286,#3858,.T.);
#10031=EDGE_CURVE('',#7286,#7287,#3859,.T.);
#10032=EDGE_CURVE('',#7287,#7288,#3860,.T.);
#10033=EDGE_CURVE('',#7288,#7289,#3861,.T.);
#10034=EDGE_CURVE('',#7289,#7290,#3862,.T.);
#10035=EDGE_CURVE('',#7290,#7291,#3863,.T.);
#10036=EDGE_CURVE('',#7291,#7292,#3864,.T.);
#10037=EDGE_CURVE('',#7292,#7293,#3865,.T.);
#10038=EDGE_CURVE('',#7293,#7294,#3866,.T.);
#10039=EDGE_CURVE('',#7294,#7295,#3867,.T.);
#10040=EDGE_CURVE('',#7295,#7296,#3868,.T.);
#10041=EDGE_CURVE('',#7296,#7297,#3869,.T.);
#10042=EDGE_CURVE('',#7297,#7298,#3870,.T.);
#10043=EDGE_CURVE('',#7298,#7299,#3871,.T.);
#10044=EDGE_CURVE('',#7299,#7300,#3872,.T.);
#10045=EDGE_CURVE('',#7300,#7243,#3873,.T.);
#10046=EDGE_CURVE('',#7240,#7301,#3874,.T.);
#10047=EDGE_CURVE('',#7301,#7153,#3875,.T.);
#10048=EDGE_CURVE('',#7239,#7150,#3876,.T.);
#10049=EDGE_CURVE('',#7274,#7148,#3877,.T.);
#10050=EDGE_CURVE('',#7244,#7157,#3878,.T.);
#10051=EDGE_CURVE('',#7156,#7245,#3879,.T.);
#10052=EDGE_CURVE('',#7302,#7303,#4539,.T.);
#10053=EDGE_CURVE('',#7302,#7304,#4540,.T.);
#10054=EDGE_CURVE('',#7304,#7305,#4541,.T.);
#10055=EDGE_CURVE('',#7303,#7305,#4542,.T.);
#10056=EDGE_CURVE('',#7306,#7302,#4543,.T.);
#10057=EDGE_CURVE('',#7306,#7307,#4544,.T.);
#10058=EDGE_CURVE('',#7307,#7304,#4545,.T.);
#10059=EDGE_CURVE('',#7308,#7306,#4546,.T.);
#10060=EDGE_CURVE('',#7308,#7309,#4547,.T.);
#10061=EDGE_CURVE('',#7309,#7307,#4548,.T.);
#10062=EDGE_CURVE('',#7310,#7308,#4549,.T.);
#10063=EDGE_CURVE('',#7310,#7311,#4550,.T.);
#10064=EDGE_CURVE('',#7311,#7309,#4551,.T.);
#10065=EDGE_CURVE('',#7312,#7310,#4552,.T.);
#10066=EDGE_CURVE('',#7312,#7313,#4553,.T.);
#10067=EDGE_CURVE('',#7313,#7311,#4554,.T.);
#10068=EDGE_CURVE('',#7303,#7312,#4555,.T.);
#10069=EDGE_CURVE('',#7305,#7313,#4556,.T.);
#10070=EDGE_CURVE('',#7314,#7314,#1980,.T.);
#10071=EDGE_CURVE('',#7314,#7315,#4557,.T.);
#10072=EDGE_CURVE('',#7315,#7315,#1981,.T.);
#10073=EDGE_CURVE('',#7316,#7317,#3880,.T.);
#10074=EDGE_CURVE('',#7317,#7318,#1982,.F.);
#10075=EDGE_CURVE('',#7318,#7319,#3881,.T.);
#10076=EDGE_CURVE('',#7319,#7320,#3882,.T.);
#10077=EDGE_CURVE('',#7320,#7321,#3883,.T.);
#10078=EDGE_CURVE('',#7321,#7322,#3884,.T.);
#10079=EDGE_CURVE('',#7322,#7323,#3885,.T.);
#10080=EDGE_CURVE('',#7323,#7324,#3886,.T.);
#10081=EDGE_CURVE('',#7324,#7325,#3887,.T.);
#10082=EDGE_CURVE('',#7325,#7326,#3888,.T.);
#10083=EDGE_CURVE('',#7326,#7327,#3889,.T.);
#10084=EDGE_CURVE('',#7327,#7328,#3890,.T.);
#10085=EDGE_CURVE('',#7328,#7329,#3891,.T.);
#10086=EDGE_CURVE('',#7329,#7330,#3892,.T.);
#10087=EDGE_CURVE('',#7330,#7331,#3893,.T.);
#10088=EDGE_CURVE('',#7331,#7332,#3894,.T.);
#10089=EDGE_CURVE('',#7332,#7333,#3895,.T.);
#10090=EDGE_CURVE('',#7333,#7334,#3896,.T.);
#10091=EDGE_CURVE('',#7334,#7335,#3897,.T.);
#10092=EDGE_CURVE('',#7335,#7336,#1983,.T.);
#10093=EDGE_CURVE('',#7336,#7337,#3898,.T.);
#10094=EDGE_CURVE('',#7337,#7338,#3899,.T.);
#10095=EDGE_CURVE('',#7338,#7339,#3900,.T.);
#10096=EDGE_CURVE('',#7339,#7340,#3901,.T.);
#10097=EDGE_CURVE('',#7340,#7341,#3902,.T.);
#10098=EDGE_CURVE('',#7341,#7342,#3903,.T.);
#10099=EDGE_CURVE('',#7342,#7343,#3904,.T.);
#10100=EDGE_CURVE('',#7343,#7344,#3905,.T.);
#10101=EDGE_CURVE('',#7344,#7345,#3906,.T.);
#10102=EDGE_CURVE('',#7345,#7346,#3907,.T.);
#10103=EDGE_CURVE('',#7346,#7347,#3908,.T.);
#10104=EDGE_CURVE('',#7347,#7348,#3909,.T.);
#10105=EDGE_CURVE('',#7348,#7349,#3910,.T.);
#10106=EDGE_CURVE('',#7349,#7350,#3911,.T.);
#10107=EDGE_CURVE('',#7350,#7351,#3912,.T.);
#10108=EDGE_CURVE('',#7351,#7316,#3913,.T.);
#10109=EDGE_CURVE('',#7352,#7353,#3914,.T.);
#10110=EDGE_CURVE('',#7353,#7354,#1984,.T.);
#10111=EDGE_CURVE('',#7355,#7354,#3915,.T.);
#10112=EDGE_CURVE('',#7356,#7355,#3916,.F.);
#10113=EDGE_CURVE('',#7357,#7356,#3917,.F.);
#10114=EDGE_CURVE('',#7358,#7357,#3918,.T.);
#10115=EDGE_CURVE('',#7359,#7358,#3919,.F.);
#10116=EDGE_CURVE('',#7360,#7359,#3920,.T.);
#10117=EDGE_CURVE('',#7361,#7360,#3921,.F.);
#10118=EDGE_CURVE('',#7362,#7361,#3922,.T.);
#10119=EDGE_CURVE('',#7363,#7362,#3923,.F.);
#10120=EDGE_CURVE('',#7364,#7363,#3924,.F.);
#10121=EDGE_CURVE('',#7365,#7364,#3925,.T.);
#10122=EDGE_CURVE('',#7366,#7365,#1985,.T.);
#10123=EDGE_CURVE('',#7366,#7367,#3926,.T.);
#10124=EDGE_CURVE('',#7367,#7368,#3927,.T.);
#10125=EDGE_CURVE('',#7368,#7369,#3928,.T.);
#10126=EDGE_CURVE('',#7369,#7370,#3929,.T.);
#10127=EDGE_CURVE('',#7370,#7371,#3930,.T.);
#10128=EDGE_CURVE('',#7371,#7372,#3931,.T.);
#10129=EDGE_CURVE('',#7372,#7373,#3932,.T.);
#10130=EDGE_CURVE('',#7373,#7374,#3933,.T.);
#10131=EDGE_CURVE('',#7374,#7352,#3934,.T.);
#10132=EDGE_CURVE('',#7354,#7375,#3935,.T.);
#10133=EDGE_CURVE('',#7336,#7353,#3936,.T.);
#10134=EDGE_CURVE('',#7376,#7335,#3937,.T.);
#10135=EDGE_CURVE('',#7376,#7377,#4558,.T.);
#10136=EDGE_CURVE('',#7377,#7377,#1986,.T.);
#10137=EDGE_CURVE('',#7375,#7376,#3938,.T.);
#10138=EDGE_CURVE('',#7317,#7366,#3939,.T.);
#10139=EDGE_CURVE('',#7365,#7318,#3940,.T.);
#10140=EDGE_CURVE('',#7378,#7379,#4559,.T.);
#10141=EDGE_CURVE('',#7378,#7380,#4560,.T.);
#10142=EDGE_CURVE('',#7380,#7381,#4561,.T.);
#10143=EDGE_CURVE('',#7379,#7381,#4562,.T.);
#10144=EDGE_CURVE('',#7382,#7378,#4563,.T.);
#10145=EDGE_CURVE('',#7382,#7383,#4564,.T.);
#10146=EDGE_CURVE('',#7383,#7380,#4565,.T.);
#10147=EDGE_CURVE('',#7384,#7382,#4566,.T.);
#10148=EDGE_CURVE('',#7384,#7385,#4567,.T.);
#10149=EDGE_CURVE('',#7385,#7383,#4568,.T.);
#10150=EDGE_CURVE('',#7386,#7384,#4569,.T.);
#10151=EDGE_CURVE('',#7386,#7387,#4570,.T.);
#10152=EDGE_CURVE('',#7387,#7385,#4571,.T.);
#10153=EDGE_CURVE('',#7388,#7386,#4572,.T.);
#10154=EDGE_CURVE('',#7388,#7389,#4573,.T.);
#10155=EDGE_CURVE('',#7389,#7387,#4574,.T.);
#10156=EDGE_CURVE('',#7379,#7388,#4575,.T.);
#10157=EDGE_CURVE('',#7381,#7389,#4576,.T.);
#10158=EDGE_CURVE('',#7390,#7390,#1987,.T.);
#10159=EDGE_CURVE('',#7390,#7391,#4577,.T.);
#10160=EDGE_CURVE('',#7391,#7391,#1988,.T.);
#10161=ORIENTED_EDGE('',*,*,#7392,.T.);
#10162=ORIENTED_EDGE('',*,*,#7393,.T.);
#10163=ORIENTED_EDGE('',*,*,#7394,.T.);
#10164=ORIENTED_EDGE('',*,*,#7395,.F.);
#10165=ORIENTED_EDGE('',*,*,#7396,.F.);
#10166=ORIENTED_EDGE('',*,*,#7397,.F.);
#10167=ORIENTED_EDGE('',*,*,#7398,.T.);
#10168=ORIENTED_EDGE('',*,*,#7399,.T.);
#10169=ORIENTED_EDGE('',*,*,#7400,.T.);
#10170=ORIENTED_EDGE('',*,*,#7392,.F.);
#10171=ORIENTED_EDGE('',*,*,#7401,.F.);
#10172=ORIENTED_EDGE('',*,*,#7402,.F.);
#10173=ORIENTED_EDGE('',*,*,#7403,.T.);
#10174=ORIENTED_EDGE('',*,*,#7404,.T.);
#10175=ORIENTED_EDGE('',*,*,#7405,.T.);
#10176=ORIENTED_EDGE('',*,*,#7398,.F.);
#10177=ORIENTED_EDGE('',*,*,#7406,.F.);
#10178=ORIENTED_EDGE('',*,*,#7407,.F.);
#10179=ORIENTED_EDGE('',*,*,#7408,.T.);
#10180=ORIENTED_EDGE('',*,*,#7409,.T.);
#10181=ORIENTED_EDGE('',*,*,#7410,.T.);
#10182=ORIENTED_EDGE('',*,*,#7403,.F.);
#10183=ORIENTED_EDGE('',*,*,#7411,.F.);
#10184=ORIENTED_EDGE('',*,*,#7412,.F.);
#10185=ORIENTED_EDGE('',*,*,#7413,.T.);
#10186=ORIENTED_EDGE('',*,*,#7414,.T.);
#10187=ORIENTED_EDGE('',*,*,#7415,.T.);
#10188=ORIENTED_EDGE('',*,*,#7408,.F.);
#10189=ORIENTED_EDGE('',*,*,#7416,.F.);
#10190=ORIENTED_EDGE('',*,*,#7417,.F.);
#10191=ORIENTED_EDGE('',*,*,#7418,.T.);
#10192=ORIENTED_EDGE('',*,*,#7419,.T.);
#10193=ORIENTED_EDGE('',*,*,#7420,.T.);
#10194=ORIENTED_EDGE('',*,*,#7413,.F.);
#10195=ORIENTED_EDGE('',*,*,#7421,.F.);
#10196=ORIENTED_EDGE('',*,*,#7422,.F.);
#10197=ORIENTED_EDGE('',*,*,#7423,.T.);
#10198=ORIENTED_EDGE('',*,*,#7424,.T.);
#10199=ORIENTED_EDGE('',*,*,#7425,.T.);
#10200=ORIENTED_EDGE('',*,*,#7418,.F.);
#10201=ORIENTED_EDGE('',*,*,#7426,.F.);
#10202=ORIENTED_EDGE('',*,*,#7427,.F.);
#10203=ORIENTED_EDGE('',*,*,#7428,.T.);
#10204=ORIENTED_EDGE('',*,*,#7429,.T.);
#10205=ORIENTED_EDGE('',*,*,#7430,.T.);
#10206=ORIENTED_EDGE('',*,*,#7423,.F.);
#10207=ORIENTED_EDGE('',*,*,#7431,.F.);
#10208=ORIENTED_EDGE('',*,*,#7432,.F.);
#10209=ORIENTED_EDGE('',*,*,#7433,.T.);
#10210=ORIENTED_EDGE('',*,*,#7434,.T.);
#10211=ORIENTED_EDGE('',*,*,#7435,.T.);
#10212=ORIENTED_EDGE('',*,*,#7428,.F.);
#10213=ORIENTED_EDGE('',*,*,#7436,.F.);
#10214=ORIENTED_EDGE('',*,*,#7437,.F.);
#10215=ORIENTED_EDGE('',*,*,#7438,.F.);
#10216=ORIENTED_EDGE('',*,*,#7439,.F.);
#10217=ORIENTED_EDGE('',*,*,#7440,.F.);
#10218=ORIENTED_EDGE('',*,*,#7441,.F.);
#10219=ORIENTED_EDGE('',*,*,#7442,.T.);
#10220=ORIENTED_EDGE('',*,*,#7443,.T.);
#10221=ORIENTED_EDGE('',*,*,#7444,.T.);
#10222=ORIENTED_EDGE('',*,*,#7445,.T.);
#10223=ORIENTED_EDGE('',*,*,#7446,.T.);
#10224=ORIENTED_EDGE('',*,*,#7447,.T.);
#10225=ORIENTED_EDGE('',*,*,#7448,.T.);
#10226=ORIENTED_EDGE('',*,*,#7447,.F.);
#10227=ORIENTED_EDGE('',*,*,#7449,.T.);
#10228=ORIENTED_EDGE('',*,*,#7450,.T.);
#10229=ORIENTED_EDGE('',*,*,#7451,.T.);
#10230=ORIENTED_EDGE('',*,*,#7452,.T.);
#10231=ORIENTED_EDGE('',*,*,#7453,.T.);
#10232=ORIENTED_EDGE('',*,*,#7444,.F.);
#10233=ORIENTED_EDGE('',*,*,#7454,.T.);
#10234=ORIENTED_EDGE('',*,*,#7455,.T.);
#10235=ORIENTED_EDGE('',*,*,#7456,.T.);
#10236=ORIENTED_EDGE('',*,*,#7451,.F.);
#10237=ORIENTED_EDGE('',*,*,#7457,.T.);
#10238=ORIENTED_EDGE('',*,*,#7458,.T.);
#10239=ORIENTED_EDGE('',*,*,#7459,.T.);
#10240=ORIENTED_EDGE('',*,*,#7460,.T.);
#10241=ORIENTED_EDGE('',*,*,#7461,.T.);
#10242=ORIENTED_EDGE('',*,*,#7455,.F.);
#10243=ORIENTED_EDGE('',*,*,#7462,.T.);
#10244=ORIENTED_EDGE('',*,*,#7463,.T.);
#10245=ORIENTED_EDGE('',*,*,#7464,.T.);
#10246=ORIENTED_EDGE('',*,*,#7459,.F.);
#10247=ORIENTED_EDGE('',*,*,#7465,.T.);
#10248=ORIENTED_EDGE('',*,*,#7466,.T.);
#10249=ORIENTED_EDGE('',*,*,#7467,.T.);
#10250=ORIENTED_EDGE('',*,*,#7468,.T.);
#10251=ORIENTED_EDGE('',*,*,#7469,.T.);
#10252=ORIENTED_EDGE('',*,*,#7463,.F.);
#10253=ORIENTED_EDGE('',*,*,#7470,.T.);
#10254=ORIENTED_EDGE('',*,*,#7471,.T.);
#10255=ORIENTED_EDGE('',*,*,#7472,.T.);
#10256=ORIENTED_EDGE('',*,*,#7467,.F.);
#10257=ORIENTED_EDGE('',*,*,#7473,.T.);
#10258=ORIENTED_EDGE('',*,*,#7474,.T.);
#10259=ORIENTED_EDGE('',*,*,#7475,.T.);
#10260=ORIENTED_EDGE('',*,*,#7476,.T.);
#10261=ORIENTED_EDGE('',*,*,#7477,.T.);
#10262=ORIENTED_EDGE('',*,*,#7471,.F.);
#10263=ORIENTED_EDGE('',*,*,#7478,.T.);
#10264=ORIENTED_EDGE('',*,*,#7479,.T.);
#10265=ORIENTED_EDGE('',*,*,#7480,.T.);
#10266=ORIENTED_EDGE('',*,*,#7475,.F.);
#10267=ORIENTED_EDGE('',*,*,#7481,.T.);
#10268=ORIENTED_EDGE('',*,*,#7482,.T.);
#10269=ORIENTED_EDGE('',*,*,#7483,.F.);
#10270=ORIENTED_EDGE('',*,*,#7484,.T.);
#10271=ORIENTED_EDGE('',*,*,#7485,.F.);
#10272=ORIENTED_EDGE('',*,*,#7486,.T.);
#10273=ORIENTED_EDGE('',*,*,#7487,.T.);
#10274=ORIENTED_EDGE('',*,*,#7488,.T.);
#10275=ORIENTED_EDGE('',*,*,#7489,.T.);
#10276=ORIENTED_EDGE('',*,*,#7490,.F.);
#10277=ORIENTED_EDGE('',*,*,#7491,.F.);
#10278=ORIENTED_EDGE('',*,*,#7492,.F.);
#10279=ORIENTED_EDGE('',*,*,#7493,.T.);
#10280=ORIENTED_EDGE('',*,*,#7494,.T.);
#10281=ORIENTED_EDGE('',*,*,#7495,.T.);
#10282=ORIENTED_EDGE('',*,*,#7487,.F.);
#10283=ORIENTED_EDGE('',*,*,#7496,.F.);
#10284=ORIENTED_EDGE('',*,*,#7497,.F.);
#10285=ORIENTED_EDGE('',*,*,#7498,.T.);
#10286=ORIENTED_EDGE('',*,*,#7499,.T.);
#10287=ORIENTED_EDGE('',*,*,#7500,.T.);
#10288=ORIENTED_EDGE('',*,*,#7493,.F.);
#10289=ORIENTED_EDGE('',*,*,#7501,.F.);
#10290=ORIENTED_EDGE('',*,*,#7502,.F.);
#10291=ORIENTED_EDGE('',*,*,#7503,.T.);
#10292=ORIENTED_EDGE('',*,*,#7504,.T.);
#10293=ORIENTED_EDGE('',*,*,#7505,.T.);
#10294=ORIENTED_EDGE('',*,*,#7498,.F.);
#10295=ORIENTED_EDGE('',*,*,#7506,.F.);
#10296=ORIENTED_EDGE('',*,*,#7507,.F.);
#10297=ORIENTED_EDGE('',*,*,#7508,.T.);
#10298=ORIENTED_EDGE('',*,*,#7509,.T.);
#10299=ORIENTED_EDGE('',*,*,#7510,.T.);
#10300=ORIENTED_EDGE('',*,*,#7503,.F.);
#10301=ORIENTED_EDGE('',*,*,#7511,.F.);
#10302=ORIENTED_EDGE('',*,*,#7512,.F.);
#10303=ORIENTED_EDGE('',*,*,#7513,.T.);
#10304=ORIENTED_EDGE('',*,*,#7514,.T.);
#10305=ORIENTED_EDGE('',*,*,#7515,.T.);
#10306=ORIENTED_EDGE('',*,*,#7508,.F.);
#10307=ORIENTED_EDGE('',*,*,#7516,.F.);
#10308=ORIENTED_EDGE('',*,*,#7517,.F.);
#10309=ORIENTED_EDGE('',*,*,#7518,.T.);
#10310=ORIENTED_EDGE('',*,*,#7519,.T.);
#10311=ORIENTED_EDGE('',*,*,#7520,.T.);
#10312=ORIENTED_EDGE('',*,*,#7513,.F.);
#10313=ORIENTED_EDGE('',*,*,#7521,.F.);
#10314=ORIENTED_EDGE('',*,*,#7522,.F.);
#10315=ORIENTED_EDGE('',*,*,#7523,.T.);
#10316=ORIENTED_EDGE('',*,*,#7524,.T.);
#10317=ORIENTED_EDGE('',*,*,#7525,.T.);
#10318=ORIENTED_EDGE('',*,*,#7518,.F.);
#10319=ORIENTED_EDGE('',*,*,#7526,.F.);
#10320=ORIENTED_EDGE('',*,*,#7527,.F.);
#10321=ORIENTED_EDGE('',*,*,#7528,.T.);
#10322=ORIENTED_EDGE('',*,*,#7529,.T.);
#10323=ORIENTED_EDGE('',*,*,#7530,.T.);
#10324=ORIENTED_EDGE('',*,*,#7523,.F.);
#10325=ORIENTED_EDGE('',*,*,#7531,.F.);
#10326=ORIENTED_EDGE('',*,*,#7532,.F.);
#10327=ORIENTED_EDGE('',*,*,#7533,.F.);
#10328=ORIENTED_EDGE('',*,*,#7534,.F.);
#10329=ORIENTED_EDGE('',*,*,#7535,.F.);
#10330=ORIENTED_EDGE('',*,*,#7536,.F.);
#10331=ORIENTED_EDGE('',*,*,#7537,.T.);
#10332=ORIENTED_EDGE('',*,*,#7538,.T.);
#10333=ORIENTED_EDGE('',*,*,#7539,.T.);
#10334=ORIENTED_EDGE('',*,*,#7540,.T.);
#10335=ORIENTED_EDGE('',*,*,#7541,.T.);
#10336=ORIENTED_EDGE('',*,*,#7542,.T.);
#10337=ORIENTED_EDGE('',*,*,#7543,.T.);
#10338=ORIENTED_EDGE('',*,*,#7542,.F.);
#10339=ORIENTED_EDGE('',*,*,#7544,.T.);
#10340=ORIENTED_EDGE('',*,*,#7545,.T.);
#10341=ORIENTED_EDGE('',*,*,#7546,.T.);
#10342=ORIENTED_EDGE('',*,*,#7547,.T.);
#10343=ORIENTED_EDGE('',*,*,#7548,.T.);
#10344=ORIENTED_EDGE('',*,*,#7539,.F.);
#10345=ORIENTED_EDGE('',*,*,#7549,.T.);
#10346=ORIENTED_EDGE('',*,*,#7550,.T.);
#10347=ORIENTED_EDGE('',*,*,#7551,.T.);
#10348=ORIENTED_EDGE('',*,*,#7546,.F.);
#10349=ORIENTED_EDGE('',*,*,#7552,.T.);
#10350=ORIENTED_EDGE('',*,*,#7553,.T.);
#10351=ORIENTED_EDGE('',*,*,#7554,.T.);
#10352=ORIENTED_EDGE('',*,*,#7555,.T.);
#10353=ORIENTED_EDGE('',*,*,#7556,.T.);
#10354=ORIENTED_EDGE('',*,*,#7550,.F.);
#10355=ORIENTED_EDGE('',*,*,#7557,.T.);
#10356=ORIENTED_EDGE('',*,*,#7558,.T.);
#10357=ORIENTED_EDGE('',*,*,#7559,.T.);
#10358=ORIENTED_EDGE('',*,*,#7554,.F.);
#10359=ORIENTED_EDGE('',*,*,#7560,.T.);
#10360=ORIENTED_EDGE('',*,*,#7561,.T.);
#10361=ORIENTED_EDGE('',*,*,#7562,.T.);
#10362=ORIENTED_EDGE('',*,*,#7563,.T.);
#10363=ORIENTED_EDGE('',*,*,#7564,.T.);
#10364=ORIENTED_EDGE('',*,*,#7558,.F.);
#10365=ORIENTED_EDGE('',*,*,#7565,.T.);
#10366=ORIENTED_EDGE('',*,*,#7566,.T.);
#10367=ORIENTED_EDGE('',*,*,#7567,.T.);
#10368=ORIENTED_EDGE('',*,*,#7562,.F.);
#10369=ORIENTED_EDGE('',*,*,#7568,.T.);
#10370=ORIENTED_EDGE('',*,*,#7569,.T.);
#10371=ORIENTED_EDGE('',*,*,#7570,.T.);
#10372=ORIENTED_EDGE('',*,*,#7571,.T.);
#10373=ORIENTED_EDGE('',*,*,#7572,.T.);
#10374=ORIENTED_EDGE('',*,*,#7566,.F.);
#10375=ORIENTED_EDGE('',*,*,#7573,.T.);
#10376=ORIENTED_EDGE('',*,*,#7574,.T.);
#10377=ORIENTED_EDGE('',*,*,#7575,.T.);
#10378=ORIENTED_EDGE('',*,*,#7570,.F.);
#10379=ORIENTED_EDGE('',*,*,#7576,.T.);
#10380=ORIENTED_EDGE('',*,*,#7577,.T.);
#10381=ORIENTED_EDGE('',*,*,#7578,.F.);
#10382=ORIENTED_EDGE('',*,*,#7579,.T.);
#10383=ORIENTED_EDGE('',*,*,#7580,.F.);
#10384=ORIENTED_EDGE('',*,*,#7581,.T.);
#10385=ORIENTED_EDGE('',*,*,#7582,.T.);
#10386=ORIENTED_EDGE('',*,*,#7583,.T.);
#10387=ORIENTED_EDGE('',*,*,#7584,.T.);
#10388=ORIENTED_EDGE('',*,*,#7585,.F.);
#10389=ORIENTED_EDGE('',*,*,#7586,.F.);
#10390=ORIENTED_EDGE('',*,*,#7587,.F.);
#10391=ORIENTED_EDGE('',*,*,#7588,.T.);
#10392=ORIENTED_EDGE('',*,*,#7589,.T.);
#10393=ORIENTED_EDGE('',*,*,#7590,.T.);
#10394=ORIENTED_EDGE('',*,*,#7582,.F.);
#10395=ORIENTED_EDGE('',*,*,#7591,.F.);
#10396=ORIENTED_EDGE('',*,*,#7592,.F.);
#10397=ORIENTED_EDGE('',*,*,#7593,.T.);
#10398=ORIENTED_EDGE('',*,*,#7594,.T.);
#10399=ORIENTED_EDGE('',*,*,#7595,.T.);
#10400=ORIENTED_EDGE('',*,*,#7588,.F.);
#10401=ORIENTED_EDGE('',*,*,#7596,.F.);
#10402=ORIENTED_EDGE('',*,*,#7597,.F.);
#10403=ORIENTED_EDGE('',*,*,#7598,.T.);
#10404=ORIENTED_EDGE('',*,*,#7599,.T.);
#10405=ORIENTED_EDGE('',*,*,#7600,.T.);
#10406=ORIENTED_EDGE('',*,*,#7593,.F.);
#10407=ORIENTED_EDGE('',*,*,#7601,.F.);
#10408=ORIENTED_EDGE('',*,*,#7602,.F.);
#10409=ORIENTED_EDGE('',*,*,#7603,.T.);
#10410=ORIENTED_EDGE('',*,*,#7604,.T.);
#10411=ORIENTED_EDGE('',*,*,#7605,.T.);
#10412=ORIENTED_EDGE('',*,*,#7598,.F.);
#10413=ORIENTED_EDGE('',*,*,#7606,.F.);
#10414=ORIENTED_EDGE('',*,*,#7607,.F.);
#10415=ORIENTED_EDGE('',*,*,#7608,.T.);
#10416=ORIENTED_EDGE('',*,*,#7609,.T.);
#10417=ORIENTED_EDGE('',*,*,#7610,.T.);
#10418=ORIENTED_EDGE('',*,*,#7603,.F.);
#10419=ORIENTED_EDGE('',*,*,#7611,.F.);
#10420=ORIENTED_EDGE('',*,*,#7612,.F.);
#10421=ORIENTED_EDGE('',*,*,#7613,.T.);
#10422=ORIENTED_EDGE('',*,*,#7614,.T.);
#10423=ORIENTED_EDGE('',*,*,#7615,.T.);
#10424=ORIENTED_EDGE('',*,*,#7608,.F.);
#10425=ORIENTED_EDGE('',*,*,#7616,.F.);
#10426=ORIENTED_EDGE('',*,*,#7617,.F.);
#10427=ORIENTED_EDGE('',*,*,#7618,.T.);
#10428=ORIENTED_EDGE('',*,*,#7619,.T.);
#10429=ORIENTED_EDGE('',*,*,#7620,.T.);
#10430=ORIENTED_EDGE('',*,*,#7613,.F.);
#10431=ORIENTED_EDGE('',*,*,#7621,.F.);
#10432=ORIENTED_EDGE('',*,*,#7622,.F.);
#10433=ORIENTED_EDGE('',*,*,#7623,.T.);
#10434=ORIENTED_EDGE('',*,*,#7624,.T.);
#10435=ORIENTED_EDGE('',*,*,#7625,.T.);
#10436=ORIENTED_EDGE('',*,*,#7618,.F.);
#10437=ORIENTED_EDGE('',*,*,#7626,.F.);
#10438=ORIENTED_EDGE('',*,*,#7627,.F.);
#10439=ORIENTED_EDGE('',*,*,#7628,.F.);
#10440=ORIENTED_EDGE('',*,*,#7629,.F.);
#10441=ORIENTED_EDGE('',*,*,#7630,.F.);
#10442=ORIENTED_EDGE('',*,*,#7631,.F.);
#10443=ORIENTED_EDGE('',*,*,#7632,.T.);
#10444=ORIENTED_EDGE('',*,*,#7633,.T.);
#10445=ORIENTED_EDGE('',*,*,#7634,.T.);
#10446=ORIENTED_EDGE('',*,*,#7635,.T.);
#10447=ORIENTED_EDGE('',*,*,#7636,.T.);
#10448=ORIENTED_EDGE('',*,*,#7637,.T.);
#10449=ORIENTED_EDGE('',*,*,#7638,.T.);
#10450=ORIENTED_EDGE('',*,*,#7637,.F.);
#10451=ORIENTED_EDGE('',*,*,#7639,.T.);
#10452=ORIENTED_EDGE('',*,*,#7640,.T.);
#10453=ORIENTED_EDGE('',*,*,#7641,.T.);
#10454=ORIENTED_EDGE('',*,*,#7642,.T.);
#10455=ORIENTED_EDGE('',*,*,#7643,.T.);
#10456=ORIENTED_EDGE('',*,*,#7634,.F.);
#10457=ORIENTED_EDGE('',*,*,#7644,.T.);
#10458=ORIENTED_EDGE('',*,*,#7645,.T.);
#10459=ORIENTED_EDGE('',*,*,#7646,.T.);
#10460=ORIENTED_EDGE('',*,*,#7641,.F.);
#10461=ORIENTED_EDGE('',*,*,#7647,.T.);
#10462=ORIENTED_EDGE('',*,*,#7648,.T.);
#10463=ORIENTED_EDGE('',*,*,#7649,.T.);
#10464=ORIENTED_EDGE('',*,*,#7650,.T.);
#10465=ORIENTED_EDGE('',*,*,#7651,.T.);
#10466=ORIENTED_EDGE('',*,*,#7645,.F.);
#10467=ORIENTED_EDGE('',*,*,#7652,.T.);
#10468=ORIENTED_EDGE('',*,*,#7653,.T.);
#10469=ORIENTED_EDGE('',*,*,#7654,.T.);
#10470=ORIENTED_EDGE('',*,*,#7649,.F.);
#10471=ORIENTED_EDGE('',*,*,#7655,.T.);
#10472=ORIENTED_EDGE('',*,*,#7656,.T.);
#10473=ORIENTED_EDGE('',*,*,#7657,.T.);
#10474=ORIENTED_EDGE('',*,*,#7658,.T.);
#10475=ORIENTED_EDGE('',*,*,#7659,.T.);
#10476=ORIENTED_EDGE('',*,*,#7653,.F.);
#10477=ORIENTED_EDGE('',*,*,#7660,.T.);
#10478=ORIENTED_EDGE('',*,*,#7661,.T.);
#10479=ORIENTED_EDGE('',*,*,#7662,.T.);
#10480=ORIENTED_EDGE('',*,*,#7657,.F.);
#10481=ORIENTED_EDGE('',*,*,#7663,.T.);
#10482=ORIENTED_EDGE('',*,*,#7664,.T.);
#10483=ORIENTED_EDGE('',*,*,#7665,.T.);
#10484=ORIENTED_EDGE('',*,*,#7666,.T.);
#10485=ORIENTED_EDGE('',*,*,#7667,.T.);
#10486=ORIENTED_EDGE('',*,*,#7661,.F.);
#10487=ORIENTED_EDGE('',*,*,#7668,.T.);
#10488=ORIENTED_EDGE('',*,*,#7669,.T.);
#10489=ORIENTED_EDGE('',*,*,#7670,.T.);
#10490=ORIENTED_EDGE('',*,*,#7665,.F.);
#10491=ORIENTED_EDGE('',*,*,#7671,.T.);
#10492=ORIENTED_EDGE('',*,*,#7672,.T.);
#10493=ORIENTED_EDGE('',*,*,#7673,.F.);
#10494=ORIENTED_EDGE('',*,*,#7674,.T.);
#10495=ORIENTED_EDGE('',*,*,#7675,.F.);
#10496=ORIENTED_EDGE('',*,*,#7676,.T.);
#10497=ORIENTED_EDGE('',*,*,#7677,.T.);
#10498=ORIENTED_EDGE('',*,*,#7678,.T.);
#10499=ORIENTED_EDGE('',*,*,#7679,.T.);
#10500=ORIENTED_EDGE('',*,*,#7680,.F.);
#10501=ORIENTED_EDGE('',*,*,#7681,.F.);
#10502=ORIENTED_EDGE('',*,*,#7682,.F.);
#10503=ORIENTED_EDGE('',*,*,#7683,.T.);
#10504=ORIENTED_EDGE('',*,*,#7684,.T.);
#10505=ORIENTED_EDGE('',*,*,#7685,.T.);
#10506=ORIENTED_EDGE('',*,*,#7677,.F.);
#10507=ORIENTED_EDGE('',*,*,#7686,.F.);
#10508=ORIENTED_EDGE('',*,*,#7687,.F.);
#10509=ORIENTED_EDGE('',*,*,#7688,.T.);
#10510=ORIENTED_EDGE('',*,*,#7689,.T.);
#10511=ORIENTED_EDGE('',*,*,#7690,.T.);
#10512=ORIENTED_EDGE('',*,*,#7683,.F.);
#10513=ORIENTED_EDGE('',*,*,#7691,.F.);
#10514=ORIENTED_EDGE('',*,*,#7692,.F.);
#10515=ORIENTED_EDGE('',*,*,#7693,.T.);
#10516=ORIENTED_EDGE('',*,*,#7694,.T.);
#10517=ORIENTED_EDGE('',*,*,#7695,.T.);
#10518=ORIENTED_EDGE('',*,*,#7688,.F.);
#10519=ORIENTED_EDGE('',*,*,#7696,.F.);
#10520=ORIENTED_EDGE('',*,*,#7697,.F.);
#10521=ORIENTED_EDGE('',*,*,#7698,.T.);
#10522=ORIENTED_EDGE('',*,*,#7699,.T.);
#10523=ORIENTED_EDGE('',*,*,#7700,.T.);
#10524=ORIENTED_EDGE('',*,*,#7693,.F.);
#10525=ORIENTED_EDGE('',*,*,#7701,.F.);
#10526=ORIENTED_EDGE('',*,*,#7702,.F.);
#10527=ORIENTED_EDGE('',*,*,#7703,.T.);
#10528=ORIENTED_EDGE('',*,*,#7704,.T.);
#10529=ORIENTED_EDGE('',*,*,#7705,.T.);
#10530=ORIENTED_EDGE('',*,*,#7698,.F.);
#10531=ORIENTED_EDGE('',*,*,#7706,.F.);
#10532=ORIENTED_EDGE('',*,*,#7707,.F.);
#10533=ORIENTED_EDGE('',*,*,#7708,.T.);
#10534=ORIENTED_EDGE('',*,*,#7709,.T.);
#10535=ORIENTED_EDGE('',*,*,#7710,.T.);
#10536=ORIENTED_EDGE('',*,*,#7703,.F.);
#10537=ORIENTED_EDGE('',*,*,#7711,.F.);
#10538=ORIENTED_EDGE('',*,*,#7712,.F.);
#10539=ORIENTED_EDGE('',*,*,#7713,.T.);
#10540=ORIENTED_EDGE('',*,*,#7714,.T.);
#10541=ORIENTED_EDGE('',*,*,#7715,.T.);
#10542=ORIENTED_EDGE('',*,*,#7708,.F.);
#10543=ORIENTED_EDGE('',*,*,#7716,.F.);
#10544=ORIENTED_EDGE('',*,*,#7717,.F.);
#10545=ORIENTED_EDGE('',*,*,#7718,.T.);
#10546=ORIENTED_EDGE('',*,*,#7719,.T.);
#10547=ORIENTED_EDGE('',*,*,#7720,.T.);
#10548=ORIENTED_EDGE('',*,*,#7713,.F.);
#10549=ORIENTED_EDGE('',*,*,#7721,.F.);
#10550=ORIENTED_EDGE('',*,*,#7722,.F.);
#10551=ORIENTED_EDGE('',*,*,#7723,.F.);
#10552=ORIENTED_EDGE('',*,*,#7724,.F.);
#10553=ORIENTED_EDGE('',*,*,#7725,.F.);
#10554=ORIENTED_EDGE('',*,*,#7726,.F.);
#10555=ORIENTED_EDGE('',*,*,#7727,.T.);
#10556=ORIENTED_EDGE('',*,*,#7728,.T.);
#10557=ORIENTED_EDGE('',*,*,#7729,.T.);
#10558=ORIENTED_EDGE('',*,*,#7730,.T.);
#10559=ORIENTED_EDGE('',*,*,#7731,.T.);
#10560=ORIENTED_EDGE('',*,*,#7732,.T.);
#10561=ORIENTED_EDGE('',*,*,#7733,.T.);
#10562=ORIENTED_EDGE('',*,*,#7732,.F.);
#10563=ORIENTED_EDGE('',*,*,#7734,.T.);
#10564=ORIENTED_EDGE('',*,*,#7735,.T.);
#10565=ORIENTED_EDGE('',*,*,#7736,.T.);
#10566=ORIENTED_EDGE('',*,*,#7737,.T.);
#10567=ORIENTED_EDGE('',*,*,#7738,.T.);
#10568=ORIENTED_EDGE('',*,*,#7729,.F.);
#10569=ORIENTED_EDGE('',*,*,#7739,.T.);
#10570=ORIENTED_EDGE('',*,*,#7740,.T.);
#10571=ORIENTED_EDGE('',*,*,#7741,.T.);
#10572=ORIENTED_EDGE('',*,*,#7736,.F.);
#10573=ORIENTED_EDGE('',*,*,#7742,.T.);
#10574=ORIENTED_EDGE('',*,*,#7743,.T.);
#10575=ORIENTED_EDGE('',*,*,#7744,.T.);
#10576=ORIENTED_EDGE('',*,*,#7745,.T.);
#10577=ORIENTED_EDGE('',*,*,#7746,.T.);
#10578=ORIENTED_EDGE('',*,*,#7740,.F.);
#10579=ORIENTED_EDGE('',*,*,#7747,.T.);
#10580=ORIENTED_EDGE('',*,*,#7748,.T.);
#10581=ORIENTED_EDGE('',*,*,#7749,.T.);
#10582=ORIENTED_EDGE('',*,*,#7744,.F.);
#10583=ORIENTED_EDGE('',*,*,#7750,.T.);
#10584=ORIENTED_EDGE('',*,*,#7751,.T.);
#10585=ORIENTED_EDGE('',*,*,#7752,.T.);
#10586=ORIENTED_EDGE('',*,*,#7753,.T.);
#10587=ORIENTED_EDGE('',*,*,#7754,.T.);
#10588=ORIENTED_EDGE('',*,*,#7748,.F.);
#10589=ORIENTED_EDGE('',*,*,#7755,.T.);
#10590=ORIENTED_EDGE('',*,*,#7756,.T.);
#10591=ORIENTED_EDGE('',*,*,#7757,.T.);
#10592=ORIENTED_EDGE('',*,*,#7752,.F.);
#10593=ORIENTED_EDGE('',*,*,#7758,.T.);
#10594=ORIENTED_EDGE('',*,*,#7759,.T.);
#10595=ORIENTED_EDGE('',*,*,#7760,.T.);
#10596=ORIENTED_EDGE('',*,*,#7761,.T.);
#10597=ORIENTED_EDGE('',*,*,#7762,.T.);
#10598=ORIENTED_EDGE('',*,*,#7756,.F.);
#10599=ORIENTED_EDGE('',*,*,#7763,.T.);
#10600=ORIENTED_EDGE('',*,*,#7764,.T.);
#10601=ORIENTED_EDGE('',*,*,#7765,.T.);
#10602=ORIENTED_EDGE('',*,*,#7760,.F.);
#10603=ORIENTED_EDGE('',*,*,#7766,.T.);
#10604=ORIENTED_EDGE('',*,*,#7767,.T.);
#10605=ORIENTED_EDGE('',*,*,#7768,.F.);
#10606=ORIENTED_EDGE('',*,*,#7769,.T.);
#10607=ORIENTED_EDGE('',*,*,#7770,.F.);
#10608=ORIENTED_EDGE('',*,*,#7771,.T.);
#10609=ORIENTED_EDGE('',*,*,#7768,.T.);
#10610=ORIENTED_EDGE('',*,*,#7772,.T.);
#10611=ORIENTED_EDGE('',*,*,#7773,.T.);
#10612=ORIENTED_EDGE('',*,*,#7764,.F.);
#10613=ORIENTED_EDGE('',*,*,#7774,.T.);
#10614=ORIENTED_EDGE('',*,*,#7775,.T.);
#10615=ORIENTED_EDGE('',*,*,#7723,.T.);
#10616=ORIENTED_EDGE('',*,*,#7776,.T.);
#10617=ORIENTED_EDGE('',*,*,#7777,.T.);
#10618=ORIENTED_EDGE('',*,*,#7718,.F.);
#10619=ORIENTED_EDGE('',*,*,#7778,.F.);
#10620=ORIENTED_EDGE('',*,*,#7779,.F.);
#10621=ORIENTED_EDGE('',*,*,#7673,.T.);
#10622=ORIENTED_EDGE('',*,*,#7780,.T.);
#10623=ORIENTED_EDGE('',*,*,#7781,.T.);
#10624=ORIENTED_EDGE('',*,*,#7669,.F.);
#10625=ORIENTED_EDGE('',*,*,#7782,.T.);
#10626=ORIENTED_EDGE('',*,*,#7783,.T.);
#10627=ORIENTED_EDGE('',*,*,#7628,.T.);
#10628=ORIENTED_EDGE('',*,*,#7784,.T.);
#10629=ORIENTED_EDGE('',*,*,#7785,.T.);
#10630=ORIENTED_EDGE('',*,*,#7623,.F.);
#10631=ORIENTED_EDGE('',*,*,#7786,.F.);
#10632=ORIENTED_EDGE('',*,*,#7787,.F.);
#10633=ORIENTED_EDGE('',*,*,#7578,.T.);
#10634=ORIENTED_EDGE('',*,*,#7788,.T.);
#10635=ORIENTED_EDGE('',*,*,#7789,.T.);
#10636=ORIENTED_EDGE('',*,*,#7574,.F.);
#10637=ORIENTED_EDGE('',*,*,#7790,.T.);
#10638=ORIENTED_EDGE('',*,*,#7791,.T.);
#10639=ORIENTED_EDGE('',*,*,#7533,.T.);
#10640=ORIENTED_EDGE('',*,*,#7792,.T.);
#10641=ORIENTED_EDGE('',*,*,#7793,.T.);
#10642=ORIENTED_EDGE('',*,*,#7528,.F.);
#10643=ORIENTED_EDGE('',*,*,#7794,.F.);
#10644=ORIENTED_EDGE('',*,*,#7795,.F.);
#10645=ORIENTED_EDGE('',*,*,#7483,.T.);
#10646=ORIENTED_EDGE('',*,*,#7796,.T.);
#10647=ORIENTED_EDGE('',*,*,#7797,.T.);
#10648=ORIENTED_EDGE('',*,*,#7479,.F.);
#10649=ORIENTED_EDGE('',*,*,#7798,.T.);
#10650=ORIENTED_EDGE('',*,*,#7799,.T.);
#10651=ORIENTED_EDGE('',*,*,#7438,.T.);
#10652=ORIENTED_EDGE('',*,*,#7800,.T.);
#10653=ORIENTED_EDGE('',*,*,#7801,.T.);
#10654=ORIENTED_EDGE('',*,*,#7433,.F.);
#10655=ORIENTED_EDGE('',*,*,#7802,.F.);
#10656=ORIENTED_EDGE('',*,*,#7803,.F.);
#10657=ORIENTED_EDGE('',*,*,#7446,.F.);
#10658=ORIENTED_EDGE('',*,*,#7804,.T.);
#10659=ORIENTED_EDGE('',*,*,#7395,.T.);
#10660=ORIENTED_EDGE('',*,*,#7805,.T.);
#10661=ORIENTED_EDGE('',*,*,#7449,.F.);
#10662=ORIENTED_EDGE('',*,*,#7805,.F.);
#10663=ORIENTED_EDGE('',*,*,#7394,.F.);
#10664=ORIENTED_EDGE('',*,*,#7393,.F.);
#10665=ORIENTED_EDGE('',*,*,#7400,.F.);
#10666=ORIENTED_EDGE('',*,*,#7399,.F.);
#10667=ORIENTED_EDGE('',*,*,#7405,.F.);
#10668=ORIENTED_EDGE('',*,*,#7404,.F.);
#10669=ORIENTED_EDGE('',*,*,#7410,.F.);
#10670=ORIENTED_EDGE('',*,*,#7409,.F.);
#10671=ORIENTED_EDGE('',*,*,#7415,.F.);
#10672=ORIENTED_EDGE('',*,*,#7414,.F.);
#10673=ORIENTED_EDGE('',*,*,#7420,.F.);
#10674=ORIENTED_EDGE('',*,*,#7419,.F.);
#10675=ORIENTED_EDGE('',*,*,#7425,.F.);
#10676=ORIENTED_EDGE('',*,*,#7424,.F.);
#10677=ORIENTED_EDGE('',*,*,#7430,.F.);
#10678=ORIENTED_EDGE('',*,*,#7429,.F.);
#10679=ORIENTED_EDGE('',*,*,#7435,.F.);
#10680=ORIENTED_EDGE('',*,*,#7434,.F.);
#10681=ORIENTED_EDGE('',*,*,#7801,.F.);
#10682=ORIENTED_EDGE('',*,*,#7800,.F.);
#10683=ORIENTED_EDGE('',*,*,#7443,.F.);
#10684=ORIENTED_EDGE('',*,*,#7442,.F.);
#10685=ORIENTED_EDGE('',*,*,#7806,.F.);
#10686=ORIENTED_EDGE('',*,*,#7484,.F.);
#10687=ORIENTED_EDGE('',*,*,#7799,.F.);
#10688=ORIENTED_EDGE('',*,*,#7798,.F.);
#10689=ORIENTED_EDGE('',*,*,#7482,.F.);
#10690=ORIENTED_EDGE('',*,*,#7481,.F.);
#10691=ORIENTED_EDGE('',*,*,#7478,.F.);
#10692=ORIENTED_EDGE('',*,*,#7474,.F.);
#10693=ORIENTED_EDGE('',*,*,#7473,.F.);
#10694=ORIENTED_EDGE('',*,*,#7470,.F.);
#10695=ORIENTED_EDGE('',*,*,#7466,.F.);
#10696=ORIENTED_EDGE('',*,*,#7465,.F.);
#10697=ORIENTED_EDGE('',*,*,#7462,.F.);
#10698=ORIENTED_EDGE('',*,*,#7458,.F.);
#10699=ORIENTED_EDGE('',*,*,#7457,.F.);
#10700=ORIENTED_EDGE('',*,*,#7454,.F.);
#10701=ORIENTED_EDGE('',*,*,#7450,.F.);
#10702=ORIENTED_EDGE('',*,*,#7804,.F.);
#10703=ORIENTED_EDGE('',*,*,#7445,.F.);
#10704=ORIENTED_EDGE('',*,*,#7453,.F.);
#10705=ORIENTED_EDGE('',*,*,#7452,.F.);
#10706=ORIENTED_EDGE('',*,*,#7456,.F.);
#10707=ORIENTED_EDGE('',*,*,#7461,.F.);
#10708=ORIENTED_EDGE('',*,*,#7460,.F.);
#10709=ORIENTED_EDGE('',*,*,#7464,.F.);
#10710=ORIENTED_EDGE('',*,*,#7469,.F.);
#10711=ORIENTED_EDGE('',*,*,#7468,.F.);
#10712=ORIENTED_EDGE('',*,*,#7472,.F.);
#10713=ORIENTED_EDGE('',*,*,#7477,.F.);
#10714=ORIENTED_EDGE('',*,*,#7476,.F.);
#10715=ORIENTED_EDGE('',*,*,#7480,.F.);
#10716=ORIENTED_EDGE('',*,*,#7797,.F.);
#10717=ORIENTED_EDGE('',*,*,#7796,.F.);
#10718=ORIENTED_EDGE('',*,*,#7486,.F.);
#10719=ORIENTED_EDGE('',*,*,#7807,.F.);
#10720=ORIENTED_EDGE('',*,*,#7808,.F.);
#10721=ORIENTED_EDGE('',*,*,#7440,.T.);
#10722=ORIENTED_EDGE('',*,*,#7439,.T.);
#10723=ORIENTED_EDGE('',*,*,#7803,.T.);
#10724=ORIENTED_EDGE('',*,*,#7802,.T.);
#10725=ORIENTED_EDGE('',*,*,#7437,.T.);
#10726=ORIENTED_EDGE('',*,*,#7436,.T.);
#10727=ORIENTED_EDGE('',*,*,#7432,.T.);
#10728=ORIENTED_EDGE('',*,*,#7431,.T.);
#10729=ORIENTED_EDGE('',*,*,#7427,.T.);
#10730=ORIENTED_EDGE('',*,*,#7426,.T.);
#10731=ORIENTED_EDGE('',*,*,#7422,.T.);
#10732=ORIENTED_EDGE('',*,*,#7421,.T.);
#10733=ORIENTED_EDGE('',*,*,#7417,.T.);
#10734=ORIENTED_EDGE('',*,*,#7416,.T.);
#10735=ORIENTED_EDGE('',*,*,#7412,.T.);
#10736=ORIENTED_EDGE('',*,*,#7411,.T.);
#10737=ORIENTED_EDGE('',*,*,#7407,.T.);
#10738=ORIENTED_EDGE('',*,*,#7406,.T.);
#10739=ORIENTED_EDGE('',*,*,#7402,.T.);
#10740=ORIENTED_EDGE('',*,*,#7401,.T.);
#10741=ORIENTED_EDGE('',*,*,#7397,.T.);
#10742=ORIENTED_EDGE('',*,*,#7396,.T.);
#10743=ORIENTED_EDGE('',*,*,#7541,.F.);
#10744=ORIENTED_EDGE('',*,*,#7809,.T.);
#10745=ORIENTED_EDGE('',*,*,#7490,.T.);
#10746=ORIENTED_EDGE('',*,*,#7810,.T.);
#10747=ORIENTED_EDGE('',*,*,#7544,.F.);
#10748=ORIENTED_EDGE('',*,*,#7810,.F.);
#10749=ORIENTED_EDGE('',*,*,#7489,.F.);
#10750=ORIENTED_EDGE('',*,*,#7488,.F.);
#10751=ORIENTED_EDGE('',*,*,#7495,.F.);
#10752=ORIENTED_EDGE('',*,*,#7494,.F.);
#10753=ORIENTED_EDGE('',*,*,#7500,.F.);
#10754=ORIENTED_EDGE('',*,*,#7499,.F.);
#10755=ORIENTED_EDGE('',*,*,#7505,.F.);
#10756=ORIENTED_EDGE('',*,*,#7504,.F.);
#10757=ORIENTED_EDGE('',*,*,#7510,.F.);
#10758=ORIENTED_EDGE('',*,*,#7509,.F.);
#10759=ORIENTED_EDGE('',*,*,#7515,.F.);
#10760=ORIENTED_EDGE('',*,*,#7514,.F.);
#10761=ORIENTED_EDGE('',*,*,#7520,.F.);
#10762=ORIENTED_EDGE('',*,*,#7519,.F.);
#10763=ORIENTED_EDGE('',*,*,#7525,.F.);
#10764=ORIENTED_EDGE('',*,*,#7524,.F.);
#10765=ORIENTED_EDGE('',*,*,#7530,.F.);
#10766=ORIENTED_EDGE('',*,*,#7529,.F.);
#10767=ORIENTED_EDGE('',*,*,#7793,.F.);
#10768=ORIENTED_EDGE('',*,*,#7792,.F.);
#10769=ORIENTED_EDGE('',*,*,#7538,.F.);
#10770=ORIENTED_EDGE('',*,*,#7537,.F.);
#10771=ORIENTED_EDGE('',*,*,#7811,.F.);
#10772=ORIENTED_EDGE('',*,*,#7579,.F.);
#10773=ORIENTED_EDGE('',*,*,#7791,.F.);
#10774=ORIENTED_EDGE('',*,*,#7790,.F.);
#10775=ORIENTED_EDGE('',*,*,#7577,.F.);
#10776=ORIENTED_EDGE('',*,*,#7576,.F.);
#10777=ORIENTED_EDGE('',*,*,#7573,.F.);
#10778=ORIENTED_EDGE('',*,*,#7569,.F.);
#10779=ORIENTED_EDGE('',*,*,#7568,.F.);
#10780=ORIENTED_EDGE('',*,*,#7565,.F.);
#10781=ORIENTED_EDGE('',*,*,#7561,.F.);
#10782=ORIENTED_EDGE('',*,*,#7560,.F.);
#10783=ORIENTED_EDGE('',*,*,#7557,.F.);
#10784=ORIENTED_EDGE('',*,*,#7553,.F.);
#10785=ORIENTED_EDGE('',*,*,#7552,.F.);
#10786=ORIENTED_EDGE('',*,*,#7549,.F.);
#10787=ORIENTED_EDGE('',*,*,#7545,.F.);
#10788=ORIENTED_EDGE('',*,*,#7809,.F.);
#10789=ORIENTED_EDGE('',*,*,#7540,.F.);
#10790=ORIENTED_EDGE('',*,*,#7548,.F.);
#10791=ORIENTED_EDGE('',*,*,#7547,.F.);
#10792=ORIENTED_EDGE('',*,*,#7551,.F.);
#10793=ORIENTED_EDGE('',*,*,#7556,.F.);
#10794=ORIENTED_EDGE('',*,*,#7555,.F.);
#10795=ORIENTED_EDGE('',*,*,#7559,.F.);
#10796=ORIENTED_EDGE('',*,*,#7564,.F.);
#10797=ORIENTED_EDGE('',*,*,#7563,.F.);
#10798=ORIENTED_EDGE('',*,*,#7567,.F.);
#10799=ORIENTED_EDGE('',*,*,#7572,.F.);
#10800=ORIENTED_EDGE('',*,*,#7571,.F.);
#10801=ORIENTED_EDGE('',*,*,#7575,.F.);
#10802=ORIENTED_EDGE('',*,*,#7789,.F.);
#10803=ORIENTED_EDGE('',*,*,#7788,.F.);
#10804=ORIENTED_EDGE('',*,*,#7581,.F.);
#10805=ORIENTED_EDGE('',*,*,#7812,.F.);
#10806=ORIENTED_EDGE('',*,*,#7813,.F.);
#10807=ORIENTED_EDGE('',*,*,#7535,.T.);
#10808=ORIENTED_EDGE('',*,*,#7534,.T.);
#10809=ORIENTED_EDGE('',*,*,#7795,.T.);
#10810=ORIENTED_EDGE('',*,*,#7794,.T.);
#10811=ORIENTED_EDGE('',*,*,#7532,.T.);
#10812=ORIENTED_EDGE('',*,*,#7531,.T.);
#10813=ORIENTED_EDGE('',*,*,#7527,.T.);
#10814=ORIENTED_EDGE('',*,*,#7526,.T.);
#10815=ORIENTED_EDGE('',*,*,#7522,.T.);
#10816=ORIENTED_EDGE('',*,*,#7521,.T.);
#10817=ORIENTED_EDGE('',*,*,#7517,.T.);
#10818=ORIENTED_EDGE('',*,*,#7516,.T.);
#10819=ORIENTED_EDGE('',*,*,#7512,.T.);
#10820=ORIENTED_EDGE('',*,*,#7511,.T.);
#10821=ORIENTED_EDGE('',*,*,#7507,.T.);
#10822=ORIENTED_EDGE('',*,*,#7506,.T.);
#10823=ORIENTED_EDGE('',*,*,#7502,.T.);
#10824=ORIENTED_EDGE('',*,*,#7501,.T.);
#10825=ORIENTED_EDGE('',*,*,#7497,.T.);
#10826=ORIENTED_EDGE('',*,*,#7496,.T.);
#10827=ORIENTED_EDGE('',*,*,#7492,.T.);
#10828=ORIENTED_EDGE('',*,*,#7491,.T.);
#10829=ORIENTED_EDGE('',*,*,#7636,.F.);
#10830=ORIENTED_EDGE('',*,*,#7814,.T.);
#10831=ORIENTED_EDGE('',*,*,#7585,.T.);
#10832=ORIENTED_EDGE('',*,*,#7815,.T.);
#10833=ORIENTED_EDGE('',*,*,#7639,.F.);
#10834=ORIENTED_EDGE('',*,*,#7815,.F.);
#10835=ORIENTED_EDGE('',*,*,#7584,.F.);
#10836=ORIENTED_EDGE('',*,*,#7583,.F.);
#10837=ORIENTED_EDGE('',*,*,#7590,.F.);
#10838=ORIENTED_EDGE('',*,*,#7589,.F.);
#10839=ORIENTED_EDGE('',*,*,#7595,.F.);
#10840=ORIENTED_EDGE('',*,*,#7594,.F.);
#10841=ORIENTED_EDGE('',*,*,#7600,.F.);
#10842=ORIENTED_EDGE('',*,*,#7599,.F.);
#10843=ORIENTED_EDGE('',*,*,#7605,.F.);
#10844=ORIENTED_EDGE('',*,*,#7604,.F.);
#10845=ORIENTED_EDGE('',*,*,#7610,.F.);
#10846=ORIENTED_EDGE('',*,*,#7609,.F.);
#10847=ORIENTED_EDGE('',*,*,#7615,.F.);
#10848=ORIENTED_EDGE('',*,*,#7614,.F.);
#10849=ORIENTED_EDGE('',*,*,#7620,.F.);
#10850=ORIENTED_EDGE('',*,*,#7619,.F.);
#10851=ORIENTED_EDGE('',*,*,#7625,.F.);
#10852=ORIENTED_EDGE('',*,*,#7624,.F.);
#10853=ORIENTED_EDGE('',*,*,#7785,.F.);
#10854=ORIENTED_EDGE('',*,*,#7784,.F.);
#10855=ORIENTED_EDGE('',*,*,#7633,.F.);
#10856=ORIENTED_EDGE('',*,*,#7632,.F.);
#10857=ORIENTED_EDGE('',*,*,#7816,.F.);
#10858=ORIENTED_EDGE('',*,*,#7674,.F.);
#10859=ORIENTED_EDGE('',*,*,#7783,.F.);
#10860=ORIENTED_EDGE('',*,*,#7782,.F.);
#10861=ORIENTED_EDGE('',*,*,#7672,.F.);
#10862=ORIENTED_EDGE('',*,*,#7671,.F.);
#10863=ORIENTED_EDGE('',*,*,#7668,.F.);
#10864=ORIENTED_EDGE('',*,*,#7664,.F.);
#10865=ORIENTED_EDGE('',*,*,#7663,.F.);
#10866=ORIENTED_EDGE('',*,*,#7660,.F.);
#10867=ORIENTED_EDGE('',*,*,#7656,.F.);
#10868=ORIENTED_EDGE('',*,*,#7655,.F.);
#10869=ORIENTED_EDGE('',*,*,#7652,.F.);
#10870=ORIENTED_EDGE('',*,*,#7648,.F.);
#10871=ORIENTED_EDGE('',*,*,#7647,.F.);
#10872=ORIENTED_EDGE('',*,*,#7644,.F.);
#10873=ORIENTED_EDGE('',*,*,#7640,.F.);
#10874=ORIENTED_EDGE('',*,*,#7814,.F.);
#10875=ORIENTED_EDGE('',*,*,#7635,.F.);
#10876=ORIENTED_EDGE('',*,*,#7643,.F.);
#10877=ORIENTED_EDGE('',*,*,#7642,.F.);
#10878=ORIENTED_EDGE('',*,*,#7646,.F.);
#10879=ORIENTED_EDGE('',*,*,#7651,.F.);
#10880=ORIENTED_EDGE('',*,*,#7650,.F.);
#10881=ORIENTED_EDGE('',*,*,#7654,.F.);
#10882=ORIENTED_EDGE('',*,*,#7659,.F.);
#10883=ORIENTED_EDGE('',*,*,#7658,.F.);
#10884=ORIENTED_EDGE('',*,*,#7662,.F.);
#10885=ORIENTED_EDGE('',*,*,#7667,.F.);
#10886=ORIENTED_EDGE('',*,*,#7666,.F.);
#10887=ORIENTED_EDGE('',*,*,#7670,.F.);
#10888=ORIENTED_EDGE('',*,*,#7781,.F.);
#10889=ORIENTED_EDGE('',*,*,#7780,.F.);
#10890=ORIENTED_EDGE('',*,*,#7676,.F.);
#10891=ORIENTED_EDGE('',*,*,#7817,.F.);
#10892=ORIENTED_EDGE('',*,*,#7818,.F.);
#10893=ORIENTED_EDGE('',*,*,#7630,.T.);
#10894=ORIENTED_EDGE('',*,*,#7629,.T.);
#10895=ORIENTED_EDGE('',*,*,#7787,.T.);
#10896=ORIENTED_EDGE('',*,*,#7786,.T.);
#10897=ORIENTED_EDGE('',*,*,#7627,.T.);
#10898=ORIENTED_EDGE('',*,*,#7626,.T.);
#10899=ORIENTED_EDGE('',*,*,#7622,.T.);
#10900=ORIENTED_EDGE('',*,*,#7621,.T.);
#10901=ORIENTED_EDGE('',*,*,#7617,.T.);
#10902=ORIENTED_EDGE('',*,*,#7616,.T.);
#10903=ORIENTED_EDGE('',*,*,#7612,.T.);
#10904=ORIENTED_EDGE('',*,*,#7611,.T.);
#10905=ORIENTED_EDGE('',*,*,#7607,.T.);
#10906=ORIENTED_EDGE('',*,*,#7606,.T.);
#10907=ORIENTED_EDGE('',*,*,#7602,.T.);
#10908=ORIENTED_EDGE('',*,*,#7601,.T.);
#10909=ORIENTED_EDGE('',*,*,#7597,.T.);
#10910=ORIENTED_EDGE('',*,*,#7596,.T.);
#10911=ORIENTED_EDGE('',*,*,#7592,.T.);
#10912=ORIENTED_EDGE('',*,*,#7591,.T.);
#10913=ORIENTED_EDGE('',*,*,#7587,.T.);
#10914=ORIENTED_EDGE('',*,*,#7586,.T.);
#10915=ORIENTED_EDGE('',*,*,#7731,.F.);
#10916=ORIENTED_EDGE('',*,*,#7819,.T.);
#10917=ORIENTED_EDGE('',*,*,#7680,.T.);
#10918=ORIENTED_EDGE('',*,*,#7820,.T.);
#10919=ORIENTED_EDGE('',*,*,#7734,.F.);
#10920=ORIENTED_EDGE('',*,*,#7820,.F.);
#10921=ORIENTED_EDGE('',*,*,#7679,.F.);
#10922=ORIENTED_EDGE('',*,*,#7678,.F.);
#10923=ORIENTED_EDGE('',*,*,#7685,.F.);
#10924=ORIENTED_EDGE('',*,*,#7684,.F.);
#10925=ORIENTED_EDGE('',*,*,#7690,.F.);
#10926=ORIENTED_EDGE('',*,*,#7689,.F.);
#10927=ORIENTED_EDGE('',*,*,#7695,.F.);
#10928=ORIENTED_EDGE('',*,*,#7694,.F.);
#10929=ORIENTED_EDGE('',*,*,#7700,.F.);
#10930=ORIENTED_EDGE('',*,*,#7699,.F.);
#10931=ORIENTED_EDGE('',*,*,#7705,.F.);
#10932=ORIENTED_EDGE('',*,*,#7704,.F.);
#10933=ORIENTED_EDGE('',*,*,#7710,.F.);
#10934=ORIENTED_EDGE('',*,*,#7709,.F.);
#10935=ORIENTED_EDGE('',*,*,#7715,.F.);
#10936=ORIENTED_EDGE('',*,*,#7714,.F.);
#10937=ORIENTED_EDGE('',*,*,#7720,.F.);
#10938=ORIENTED_EDGE('',*,*,#7719,.F.);
#10939=ORIENTED_EDGE('',*,*,#7777,.F.);
#10940=ORIENTED_EDGE('',*,*,#7776,.F.);
#10941=ORIENTED_EDGE('',*,*,#7728,.F.);
#10942=ORIENTED_EDGE('',*,*,#7727,.F.);
#10943=ORIENTED_EDGE('',*,*,#7821,.F.);
#10944=ORIENTED_EDGE('',*,*,#7769,.F.);
#10945=ORIENTED_EDGE('',*,*,#7775,.F.);
#10946=ORIENTED_EDGE('',*,*,#7774,.F.);
#10947=ORIENTED_EDGE('',*,*,#7767,.F.);
#10948=ORIENTED_EDGE('',*,*,#7766,.F.);
#10949=ORIENTED_EDGE('',*,*,#7763,.F.);
#10950=ORIENTED_EDGE('',*,*,#7759,.F.);
#10951=ORIENTED_EDGE('',*,*,#7758,.F.);
#10952=ORIENTED_EDGE('',*,*,#7755,.F.);
#10953=ORIENTED_EDGE('',*,*,#7751,.F.);
#10954=ORIENTED_EDGE('',*,*,#7750,.F.);
#10955=ORIENTED_EDGE('',*,*,#7747,.F.);
#10956=ORIENTED_EDGE('',*,*,#7743,.F.);
#10957=ORIENTED_EDGE('',*,*,#7742,.F.);
#10958=ORIENTED_EDGE('',*,*,#7739,.F.);
#10959=ORIENTED_EDGE('',*,*,#7735,.F.);
#10960=ORIENTED_EDGE('',*,*,#7819,.F.);
#10961=ORIENTED_EDGE('',*,*,#7730,.F.);
#10962=ORIENTED_EDGE('',*,*,#7738,.F.);
#10963=ORIENTED_EDGE('',*,*,#7737,.F.);
#10964=ORIENTED_EDGE('',*,*,#7741,.F.);
#10965=ORIENTED_EDGE('',*,*,#7746,.F.);
#10966=ORIENTED_EDGE('',*,*,#7745,.F.);
#10967=ORIENTED_EDGE('',*,*,#7749,.F.);
#10968=ORIENTED_EDGE('',*,*,#7754,.F.);
#10969=ORIENTED_EDGE('',*,*,#7753,.F.);
#10970=ORIENTED_EDGE('',*,*,#7757,.F.);
#10971=ORIENTED_EDGE('',*,*,#7762,.F.);
#10972=ORIENTED_EDGE('',*,*,#7761,.F.);
#10973=ORIENTED_EDGE('',*,*,#7765,.F.);
#10974=ORIENTED_EDGE('',*,*,#7773,.F.);
#10975=ORIENTED_EDGE('',*,*,#7772,.F.);
#10976=ORIENTED_EDGE('',*,*,#7771,.F.);
#10977=ORIENTED_EDGE('',*,*,#7822,.F.);
#10978=ORIENTED_EDGE('',*,*,#7823,.F.);
#10979=ORIENTED_EDGE('',*,*,#7725,.T.);
#10980=ORIENTED_EDGE('',*,*,#7724,.T.);
#10981=ORIENTED_EDGE('',*,*,#7779,.T.);
#10982=ORIENTED_EDGE('',*,*,#7778,.T.);
#10983=ORIENTED_EDGE('',*,*,#7722,.T.);
#10984=ORIENTED_EDGE('',*,*,#7721,.T.);
#10985=ORIENTED_EDGE('',*,*,#7717,.T.);
#10986=ORIENTED_EDGE('',*,*,#7716,.T.);
#10987=ORIENTED_EDGE('',*,*,#7712,.T.);
#10988=ORIENTED_EDGE('',*,*,#7711,.T.);
#10989=ORIENTED_EDGE('',*,*,#7707,.T.);
#10990=ORIENTED_EDGE('',*,*,#7706,.T.);
#10991=ORIENTED_EDGE('',*,*,#7702,.T.);
#10992=ORIENTED_EDGE('',*,*,#7701,.T.);
#10993=ORIENTED_EDGE('',*,*,#7697,.T.);
#10994=ORIENTED_EDGE('',*,*,#7696,.T.);
#10995=ORIENTED_EDGE('',*,*,#7692,.T.);
#10996=ORIENTED_EDGE('',*,*,#7691,.T.);
#10997=ORIENTED_EDGE('',*,*,#7687,.T.);
#10998=ORIENTED_EDGE('',*,*,#7686,.T.);
#10999=ORIENTED_EDGE('',*,*,#7682,.T.);
#11000=ORIENTED_EDGE('',*,*,#7681,.T.);
#11001=ORIENTED_EDGE('',*,*,#7448,.F.);
#11002=ORIENTED_EDGE('',*,*,#7543,.F.);
#11003=ORIENTED_EDGE('',*,*,#7733,.F.);
#11004=ORIENTED_EDGE('',*,*,#7638,.F.);
#11005=ORIENTED_EDGE('',*,*,#7824,.F.);
#11006=ORIENTED_EDGE('',*,*,#7825,.T.);
#11007=ORIENTED_EDGE('',*,*,#7826,.F.);
#11008=ORIENTED_EDGE('',*,*,#7825,.F.);
#11009=ORIENTED_EDGE('',*,*,#7827,.F.);
#11010=ORIENTED_EDGE('',*,*,#7828,.T.);
#11011=ORIENTED_EDGE('',*,*,#7829,.F.);
#11012=ORIENTED_EDGE('',*,*,#7828,.F.);
#11013=ORIENTED_EDGE('',*,*,#7830,.F.);
#11014=ORIENTED_EDGE('',*,*,#7831,.T.);
#11015=ORIENTED_EDGE('',*,*,#7832,.F.);
#11016=ORIENTED_EDGE('',*,*,#7831,.F.);
#11017=ORIENTED_EDGE('',*,*,#7833,.F.);
#11018=ORIENTED_EDGE('',*,*,#7834,.T.);
#11019=ORIENTED_EDGE('',*,*,#7835,.F.);
#11020=ORIENTED_EDGE('',*,*,#7834,.F.);
#11021=ORIENTED_EDGE('',*,*,#7836,.T.);
#11022=ORIENTED_EDGE('',*,*,#7837,.T.);
#11023=ORIENTED_EDGE('',*,*,#7838,.F.);
#11024=ORIENTED_EDGE('',*,*,#7839,.F.);
#11025=ORIENTED_EDGE('',*,*,#7840,.T.);
#11026=ORIENTED_EDGE('',*,*,#7839,.T.);
#11027=ORIENTED_EDGE('',*,*,#7841,.F.);
#11028=ORIENTED_EDGE('',*,*,#7842,.F.);
#11029=ORIENTED_EDGE('',*,*,#7843,.T.);
#11030=ORIENTED_EDGE('',*,*,#7842,.T.);
#11031=ORIENTED_EDGE('',*,*,#7844,.F.);
#11032=ORIENTED_EDGE('',*,*,#7845,.F.);
#11033=ORIENTED_EDGE('',*,*,#7846,.T.);
#11034=ORIENTED_EDGE('',*,*,#7845,.T.);
#11035=ORIENTED_EDGE('',*,*,#7847,.F.);
#11036=ORIENTED_EDGE('',*,*,#7837,.F.);
#11037=ORIENTED_EDGE('',*,*,#7847,.T.);
#11038=ORIENTED_EDGE('',*,*,#7844,.T.);
#11039=ORIENTED_EDGE('',*,*,#7841,.T.);
#11040=ORIENTED_EDGE('',*,*,#7838,.T.);
#11041=ORIENTED_EDGE('',*,*,#7813,.T.);
#11042=ORIENTED_EDGE('',*,*,#7812,.T.);
#11043=ORIENTED_EDGE('',*,*,#7580,.T.);
#11044=ORIENTED_EDGE('',*,*,#7811,.T.);
#11045=ORIENTED_EDGE('',*,*,#7536,.T.);
#11046=ORIENTED_EDGE('',*,*,#7823,.T.);
#11047=ORIENTED_EDGE('',*,*,#7822,.T.);
#11048=ORIENTED_EDGE('',*,*,#7770,.T.);
#11049=ORIENTED_EDGE('',*,*,#7821,.T.);
#11050=ORIENTED_EDGE('',*,*,#7726,.T.);
#11051=ORIENTED_EDGE('',*,*,#7833,.T.);
#11052=ORIENTED_EDGE('',*,*,#7830,.T.);
#11053=ORIENTED_EDGE('',*,*,#7827,.T.);
#11054=ORIENTED_EDGE('',*,*,#7824,.T.);
#11055=ORIENTED_EDGE('',*,*,#7818,.T.);
#11056=ORIENTED_EDGE('',*,*,#7817,.T.);
#11057=ORIENTED_EDGE('',*,*,#7675,.T.);
#11058=ORIENTED_EDGE('',*,*,#7816,.T.);
#11059=ORIENTED_EDGE('',*,*,#7631,.T.);
#11060=ORIENTED_EDGE('',*,*,#7808,.T.);
#11061=ORIENTED_EDGE('',*,*,#7807,.T.);
#11062=ORIENTED_EDGE('',*,*,#7485,.T.);
#11063=ORIENTED_EDGE('',*,*,#7806,.T.);
#11064=ORIENTED_EDGE('',*,*,#7441,.T.);
#11065=ORIENTED_EDGE('',*,*,#7846,.F.);
#11066=ORIENTED_EDGE('',*,*,#7836,.F.);
#11067=ORIENTED_EDGE('',*,*,#7840,.F.);
#11068=ORIENTED_EDGE('',*,*,#7843,.F.);
#11069=ORIENTED_EDGE('',*,*,#7826,.T.);
#11070=ORIENTED_EDGE('',*,*,#7829,.T.);
#11071=ORIENTED_EDGE('',*,*,#7832,.T.);
#11072=ORIENTED_EDGE('',*,*,#7835,.T.);
#11073=ORIENTED_EDGE('',*,*,#7848,.T.);
#11074=ORIENTED_EDGE('',*,*,#7849,.T.);
#11075=ORIENTED_EDGE('',*,*,#7850,.F.);
#11076=ORIENTED_EDGE('',*,*,#7851,.F.);
#11077=ORIENTED_EDGE('',*,*,#7852,.T.);
#11078=ORIENTED_EDGE('',*,*,#7853,.T.);
#11079=ORIENTED_EDGE('',*,*,#7854,.T.);
#11080=ORIENTED_EDGE('',*,*,#7848,.F.);
#11081=ORIENTED_EDGE('',*,*,#7855,.F.);
#11082=ORIENTED_EDGE('',*,*,#7856,.F.);
#11083=ORIENTED_EDGE('',*,*,#7857,.T.);
#11084=ORIENTED_EDGE('',*,*,#7858,.T.);
#11085=ORIENTED_EDGE('',*,*,#7859,.T.);
#11086=ORIENTED_EDGE('',*,*,#7852,.F.);
#11087=ORIENTED_EDGE('',*,*,#7860,.F.);
#11088=ORIENTED_EDGE('',*,*,#7861,.F.);
#11089=ORIENTED_EDGE('',*,*,#7862,.T.);
#11090=ORIENTED_EDGE('',*,*,#7863,.T.);
#11091=ORIENTED_EDGE('',*,*,#7864,.T.);
#11092=ORIENTED_EDGE('',*,*,#7857,.F.);
#11093=ORIENTED_EDGE('',*,*,#7865,.F.);
#11094=ORIENTED_EDGE('',*,*,#7866,.F.);
#11095=ORIENTED_EDGE('',*,*,#7867,.T.);
#11096=ORIENTED_EDGE('',*,*,#7868,.T.);
#11097=ORIENTED_EDGE('',*,*,#7869,.T.);
#11098=ORIENTED_EDGE('',*,*,#7862,.F.);
#11099=ORIENTED_EDGE('',*,*,#7870,.F.);
#11100=ORIENTED_EDGE('',*,*,#7871,.F.);
#11101=ORIENTED_EDGE('',*,*,#7872,.T.);
#11102=ORIENTED_EDGE('',*,*,#7873,.T.);
#11103=ORIENTED_EDGE('',*,*,#7874,.T.);
#11104=ORIENTED_EDGE('',*,*,#7867,.F.);
#11105=ORIENTED_EDGE('',*,*,#7875,.F.);
#11106=ORIENTED_EDGE('',*,*,#7876,.F.);
#11107=ORIENTED_EDGE('',*,*,#7877,.T.);
#11108=ORIENTED_EDGE('',*,*,#7878,.T.);
#11109=ORIENTED_EDGE('',*,*,#7879,.T.);
#11110=ORIENTED_EDGE('',*,*,#7872,.F.);
#11111=ORIENTED_EDGE('',*,*,#7880,.F.);
#11112=ORIENTED_EDGE('',*,*,#7881,.F.);
#11113=ORIENTED_EDGE('',*,*,#7882,.T.);
#11114=ORIENTED_EDGE('',*,*,#7883,.T.);
#11115=ORIENTED_EDGE('',*,*,#7884,.T.);
#11116=ORIENTED_EDGE('',*,*,#7877,.F.);
#11117=ORIENTED_EDGE('',*,*,#7885,.F.);
#11118=ORIENTED_EDGE('',*,*,#7886,.F.);
#11119=ORIENTED_EDGE('',*,*,#7887,.T.);
#11120=ORIENTED_EDGE('',*,*,#7888,.T.);
#11121=ORIENTED_EDGE('',*,*,#7889,.T.);
#11122=ORIENTED_EDGE('',*,*,#7882,.F.);
#11123=ORIENTED_EDGE('',*,*,#7890,.F.);
#11124=ORIENTED_EDGE('',*,*,#7891,.F.);
#11125=ORIENTED_EDGE('',*,*,#7892,.T.);
#11126=ORIENTED_EDGE('',*,*,#7893,.T.);
#11127=ORIENTED_EDGE('',*,*,#7894,.T.);
#11128=ORIENTED_EDGE('',*,*,#7887,.F.);
#11129=ORIENTED_EDGE('',*,*,#7895,.F.);
#11130=ORIENTED_EDGE('',*,*,#7896,.F.);
#11131=ORIENTED_EDGE('',*,*,#7897,.T.);
#11132=ORIENTED_EDGE('',*,*,#7898,.T.);
#11133=ORIENTED_EDGE('',*,*,#7899,.T.);
#11134=ORIENTED_EDGE('',*,*,#7892,.F.);
#11135=ORIENTED_EDGE('',*,*,#7900,.F.);
#11136=ORIENTED_EDGE('',*,*,#7901,.F.);
#11137=ORIENTED_EDGE('',*,*,#7902,.T.);
#11138=ORIENTED_EDGE('',*,*,#7903,.T.);
#11139=ORIENTED_EDGE('',*,*,#7904,.T.);
#11140=ORIENTED_EDGE('',*,*,#7897,.F.);
#11141=ORIENTED_EDGE('',*,*,#7905,.F.);
#11142=ORIENTED_EDGE('',*,*,#7906,.F.);
#11143=ORIENTED_EDGE('',*,*,#7907,.T.);
#11144=ORIENTED_EDGE('',*,*,#7908,.T.);
#11145=ORIENTED_EDGE('',*,*,#7909,.T.);
#11146=ORIENTED_EDGE('',*,*,#7902,.F.);
#11147=ORIENTED_EDGE('',*,*,#7910,.F.);
#11148=ORIENTED_EDGE('',*,*,#7911,.F.);
#11149=ORIENTED_EDGE('',*,*,#7912,.T.);
#11150=ORIENTED_EDGE('',*,*,#7913,.T.);
#11151=ORIENTED_EDGE('',*,*,#7914,.T.);
#11152=ORIENTED_EDGE('',*,*,#7907,.F.);
#11153=ORIENTED_EDGE('',*,*,#7915,.F.);
#11154=ORIENTED_EDGE('',*,*,#7916,.F.);
#11155=ORIENTED_EDGE('',*,*,#7917,.T.);
#11156=ORIENTED_EDGE('',*,*,#7918,.T.);
#11157=ORIENTED_EDGE('',*,*,#7919,.T.);
#11158=ORIENTED_EDGE('',*,*,#7912,.F.);
#11159=ORIENTED_EDGE('',*,*,#7920,.F.);
#11160=ORIENTED_EDGE('',*,*,#7921,.F.);
#11161=ORIENTED_EDGE('',*,*,#7922,.F.);
#11162=ORIENTED_EDGE('',*,*,#7923,.F.);
#11163=ORIENTED_EDGE('',*,*,#7924,.F.);
#11164=ORIENTED_EDGE('',*,*,#7925,.F.);
#11165=ORIENTED_EDGE('',*,*,#7926,.T.);
#11166=ORIENTED_EDGE('',*,*,#7927,.T.);
#11167=ORIENTED_EDGE('',*,*,#7928,.T.);
#11168=ORIENTED_EDGE('',*,*,#7929,.T.);
#11169=ORIENTED_EDGE('',*,*,#7930,.T.);
#11170=ORIENTED_EDGE('',*,*,#7931,.T.);
#11171=ORIENTED_EDGE('',*,*,#7932,.T.);
#11172=ORIENTED_EDGE('',*,*,#7933,.T.);
#11173=ORIENTED_EDGE('',*,*,#7932,.F.);
#11174=ORIENTED_EDGE('',*,*,#7934,.T.);
#11175=ORIENTED_EDGE('',*,*,#7935,.T.);
#11176=ORIENTED_EDGE('',*,*,#7936,.T.);
#11177=ORIENTED_EDGE('',*,*,#7928,.F.);
#11178=ORIENTED_EDGE('',*,*,#7937,.T.);
#11179=ORIENTED_EDGE('',*,*,#7938,.T.);
#11180=ORIENTED_EDGE('',*,*,#7939,.T.);
#11181=ORIENTED_EDGE('',*,*,#7940,.T.);
#11182=ORIENTED_EDGE('',*,*,#7941,.T.);
#11183=ORIENTED_EDGE('',*,*,#7935,.F.);
#11184=ORIENTED_EDGE('',*,*,#7942,.T.);
#11185=ORIENTED_EDGE('',*,*,#7943,.T.);
#11186=ORIENTED_EDGE('',*,*,#7944,.T.);
#11187=ORIENTED_EDGE('',*,*,#7945,.T.);
#11188=ORIENTED_EDGE('',*,*,#7939,.F.);
#11189=ORIENTED_EDGE('',*,*,#7946,.T.);
#11190=ORIENTED_EDGE('',*,*,#7947,.T.);
#11191=ORIENTED_EDGE('',*,*,#7948,.T.);
#11192=ORIENTED_EDGE('',*,*,#7949,.T.);
#11193=ORIENTED_EDGE('',*,*,#7944,.F.);
#11194=ORIENTED_EDGE('',*,*,#7950,.T.);
#11195=ORIENTED_EDGE('',*,*,#7951,.T.);
#11196=ORIENTED_EDGE('',*,*,#7952,.T.);
#11197=ORIENTED_EDGE('',*,*,#7953,.T.);
#11198=ORIENTED_EDGE('',*,*,#7947,.F.);
#11199=ORIENTED_EDGE('',*,*,#7954,.T.);
#11200=ORIENTED_EDGE('',*,*,#7955,.T.);
#11201=ORIENTED_EDGE('',*,*,#7956,.T.);
#11202=ORIENTED_EDGE('',*,*,#7957,.T.);
#11203=ORIENTED_EDGE('',*,*,#7952,.F.);
#11204=ORIENTED_EDGE('',*,*,#7958,.T.);
#11205=ORIENTED_EDGE('',*,*,#7959,.T.);
#11206=ORIENTED_EDGE('',*,*,#7960,.T.);
#11207=ORIENTED_EDGE('',*,*,#7961,.T.);
#11208=ORIENTED_EDGE('',*,*,#7955,.F.);
#11209=ORIENTED_EDGE('',*,*,#7962,.T.);
#11210=ORIENTED_EDGE('',*,*,#7963,.T.);
#11211=ORIENTED_EDGE('',*,*,#7964,.T.);
#11212=ORIENTED_EDGE('',*,*,#7965,.T.);
#11213=ORIENTED_EDGE('',*,*,#7960,.F.);
#11214=ORIENTED_EDGE('',*,*,#7966,.T.);
#11215=ORIENTED_EDGE('',*,*,#7967,.T.);
#11216=ORIENTED_EDGE('',*,*,#7968,.T.);
#11217=ORIENTED_EDGE('',*,*,#7969,.T.);
#11218=ORIENTED_EDGE('',*,*,#7963,.F.);
#11219=ORIENTED_EDGE('',*,*,#7970,.T.);
#11220=ORIENTED_EDGE('',*,*,#7971,.T.);
#11221=ORIENTED_EDGE('',*,*,#7972,.T.);
#11222=ORIENTED_EDGE('',*,*,#7973,.T.);
#11223=ORIENTED_EDGE('',*,*,#7968,.F.);
#11224=ORIENTED_EDGE('',*,*,#7974,.T.);
#11225=ORIENTED_EDGE('',*,*,#7975,.T.);
#11226=ORIENTED_EDGE('',*,*,#7976,.T.);
#11227=ORIENTED_EDGE('',*,*,#7977,.T.);
#11228=ORIENTED_EDGE('',*,*,#7971,.F.);
#11229=ORIENTED_EDGE('',*,*,#7978,.T.);
#11230=ORIENTED_EDGE('',*,*,#7979,.T.);
#11231=ORIENTED_EDGE('',*,*,#7980,.T.);
#11232=ORIENTED_EDGE('',*,*,#7981,.T.);
#11233=ORIENTED_EDGE('',*,*,#7976,.F.);
#11234=ORIENTED_EDGE('',*,*,#7982,.T.);
#11235=ORIENTED_EDGE('',*,*,#7983,.T.);
#11236=ORIENTED_EDGE('',*,*,#7984,.T.);
#11237=ORIENTED_EDGE('',*,*,#7985,.T.);
#11238=ORIENTED_EDGE('',*,*,#7979,.F.);
#11239=ORIENTED_EDGE('',*,*,#7986,.T.);
#11240=ORIENTED_EDGE('',*,*,#7987,.F.);
#11241=ORIENTED_EDGE('',*,*,#7988,.T.);
#11242=ORIENTED_EDGE('',*,*,#7989,.F.);
#11243=ORIENTED_EDGE('',*,*,#7990,.T.);
#11244=ORIENTED_EDGE('',*,*,#7991,.T.);
#11245=ORIENTED_EDGE('',*,*,#7992,.T.);
#11246=ORIENTED_EDGE('',*,*,#7993,.F.);
#11247=ORIENTED_EDGE('',*,*,#7994,.F.);
#11248=ORIENTED_EDGE('',*,*,#7995,.T.);
#11249=ORIENTED_EDGE('',*,*,#7996,.T.);
#11250=ORIENTED_EDGE('',*,*,#7997,.T.);
#11251=ORIENTED_EDGE('',*,*,#7991,.F.);
#11252=ORIENTED_EDGE('',*,*,#7998,.F.);
#11253=ORIENTED_EDGE('',*,*,#7999,.F.);
#11254=ORIENTED_EDGE('',*,*,#8000,.T.);
#11255=ORIENTED_EDGE('',*,*,#8001,.T.);
#11256=ORIENTED_EDGE('',*,*,#8002,.T.);
#11257=ORIENTED_EDGE('',*,*,#7995,.F.);
#11258=ORIENTED_EDGE('',*,*,#8003,.F.);
#11259=ORIENTED_EDGE('',*,*,#8004,.F.);
#11260=ORIENTED_EDGE('',*,*,#8005,.T.);
#11261=ORIENTED_EDGE('',*,*,#8006,.T.);
#11262=ORIENTED_EDGE('',*,*,#8007,.T.);
#11263=ORIENTED_EDGE('',*,*,#8000,.F.);
#11264=ORIENTED_EDGE('',*,*,#8008,.F.);
#11265=ORIENTED_EDGE('',*,*,#8009,.F.);
#11266=ORIENTED_EDGE('',*,*,#8010,.T.);
#11267=ORIENTED_EDGE('',*,*,#8011,.T.);
#11268=ORIENTED_EDGE('',*,*,#8012,.T.);
#11269=ORIENTED_EDGE('',*,*,#8005,.F.);
#11270=ORIENTED_EDGE('',*,*,#8013,.F.);
#11271=ORIENTED_EDGE('',*,*,#8014,.F.);
#11272=ORIENTED_EDGE('',*,*,#8015,.T.);
#11273=ORIENTED_EDGE('',*,*,#8016,.T.);
#11274=ORIENTED_EDGE('',*,*,#8017,.T.);
#11275=ORIENTED_EDGE('',*,*,#8010,.F.);
#11276=ORIENTED_EDGE('',*,*,#8018,.F.);
#11277=ORIENTED_EDGE('',*,*,#8019,.F.);
#11278=ORIENTED_EDGE('',*,*,#8020,.T.);
#11279=ORIENTED_EDGE('',*,*,#8021,.T.);
#11280=ORIENTED_EDGE('',*,*,#8022,.T.);
#11281=ORIENTED_EDGE('',*,*,#8015,.F.);
#11282=ORIENTED_EDGE('',*,*,#8023,.F.);
#11283=ORIENTED_EDGE('',*,*,#8024,.F.);
#11284=ORIENTED_EDGE('',*,*,#8025,.T.);
#11285=ORIENTED_EDGE('',*,*,#8026,.T.);
#11286=ORIENTED_EDGE('',*,*,#8027,.T.);
#11287=ORIENTED_EDGE('',*,*,#8020,.F.);
#11288=ORIENTED_EDGE('',*,*,#8028,.F.);
#11289=ORIENTED_EDGE('',*,*,#8029,.F.);
#11290=ORIENTED_EDGE('',*,*,#8030,.T.);
#11291=ORIENTED_EDGE('',*,*,#8031,.T.);
#11292=ORIENTED_EDGE('',*,*,#8032,.T.);
#11293=ORIENTED_EDGE('',*,*,#8025,.F.);
#11294=ORIENTED_EDGE('',*,*,#8033,.F.);
#11295=ORIENTED_EDGE('',*,*,#8034,.F.);
#11296=ORIENTED_EDGE('',*,*,#8035,.T.);
#11297=ORIENTED_EDGE('',*,*,#8036,.T.);
#11298=ORIENTED_EDGE('',*,*,#8037,.T.);
#11299=ORIENTED_EDGE('',*,*,#8030,.F.);
#11300=ORIENTED_EDGE('',*,*,#8038,.F.);
#11301=ORIENTED_EDGE('',*,*,#8039,.F.);
#11302=ORIENTED_EDGE('',*,*,#8040,.T.);
#11303=ORIENTED_EDGE('',*,*,#8041,.T.);
#11304=ORIENTED_EDGE('',*,*,#8042,.T.);
#11305=ORIENTED_EDGE('',*,*,#8035,.F.);
#11306=ORIENTED_EDGE('',*,*,#8043,.F.);
#11307=ORIENTED_EDGE('',*,*,#8044,.F.);
#11308=ORIENTED_EDGE('',*,*,#8045,.T.);
#11309=ORIENTED_EDGE('',*,*,#8046,.T.);
#11310=ORIENTED_EDGE('',*,*,#8047,.T.);
#11311=ORIENTED_EDGE('',*,*,#8040,.F.);
#11312=ORIENTED_EDGE('',*,*,#8048,.F.);
#11313=ORIENTED_EDGE('',*,*,#8049,.F.);
#11314=ORIENTED_EDGE('',*,*,#8050,.T.);
#11315=ORIENTED_EDGE('',*,*,#8051,.T.);
#11316=ORIENTED_EDGE('',*,*,#8052,.T.);
#11317=ORIENTED_EDGE('',*,*,#8045,.F.);
#11318=ORIENTED_EDGE('',*,*,#8053,.F.);
#11319=ORIENTED_EDGE('',*,*,#8054,.F.);
#11320=ORIENTED_EDGE('',*,*,#8055,.T.);
#11321=ORIENTED_EDGE('',*,*,#8056,.T.);
#11322=ORIENTED_EDGE('',*,*,#8057,.T.);
#11323=ORIENTED_EDGE('',*,*,#8050,.F.);
#11324=ORIENTED_EDGE('',*,*,#8058,.F.);
#11325=ORIENTED_EDGE('',*,*,#8059,.F.);
#11326=ORIENTED_EDGE('',*,*,#8060,.T.);
#11327=ORIENTED_EDGE('',*,*,#8061,.T.);
#11328=ORIENTED_EDGE('',*,*,#8062,.T.);
#11329=ORIENTED_EDGE('',*,*,#8055,.F.);
#11330=ORIENTED_EDGE('',*,*,#8063,.F.);
#11331=ORIENTED_EDGE('',*,*,#8064,.F.);
#11332=ORIENTED_EDGE('',*,*,#8065,.F.);
#11333=ORIENTED_EDGE('',*,*,#8066,.F.);
#11334=ORIENTED_EDGE('',*,*,#8067,.F.);
#11335=ORIENTED_EDGE('',*,*,#8068,.F.);
#11336=ORIENTED_EDGE('',*,*,#8069,.T.);
#11337=ORIENTED_EDGE('',*,*,#8070,.T.);
#11338=ORIENTED_EDGE('',*,*,#8071,.T.);
#11339=ORIENTED_EDGE('',*,*,#8072,.T.);
#11340=ORIENTED_EDGE('',*,*,#8073,.T.);
#11341=ORIENTED_EDGE('',*,*,#8074,.T.);
#11342=ORIENTED_EDGE('',*,*,#8075,.T.);
#11343=ORIENTED_EDGE('',*,*,#8076,.T.);
#11344=ORIENTED_EDGE('',*,*,#8075,.F.);
#11345=ORIENTED_EDGE('',*,*,#8077,.T.);
#11346=ORIENTED_EDGE('',*,*,#8078,.T.);
#11347=ORIENTED_EDGE('',*,*,#8079,.T.);
#11348=ORIENTED_EDGE('',*,*,#8071,.F.);
#11349=ORIENTED_EDGE('',*,*,#8080,.T.);
#11350=ORIENTED_EDGE('',*,*,#8081,.T.);
#11351=ORIENTED_EDGE('',*,*,#8082,.T.);
#11352=ORIENTED_EDGE('',*,*,#8083,.T.);
#11353=ORIENTED_EDGE('',*,*,#8084,.T.);
#11354=ORIENTED_EDGE('',*,*,#8078,.F.);
#11355=ORIENTED_EDGE('',*,*,#8085,.T.);
#11356=ORIENTED_EDGE('',*,*,#8086,.T.);
#11357=ORIENTED_EDGE('',*,*,#8087,.T.);
#11358=ORIENTED_EDGE('',*,*,#8088,.T.);
#11359=ORIENTED_EDGE('',*,*,#8082,.F.);
#11360=ORIENTED_EDGE('',*,*,#8089,.T.);
#11361=ORIENTED_EDGE('',*,*,#8090,.T.);
#11362=ORIENTED_EDGE('',*,*,#8091,.T.);
#11363=ORIENTED_EDGE('',*,*,#8092,.T.);
#11364=ORIENTED_EDGE('',*,*,#8087,.F.);
#11365=ORIENTED_EDGE('',*,*,#8093,.T.);
#11366=ORIENTED_EDGE('',*,*,#8094,.T.);
#11367=ORIENTED_EDGE('',*,*,#8095,.T.);
#11368=ORIENTED_EDGE('',*,*,#8096,.T.);
#11369=ORIENTED_EDGE('',*,*,#8090,.F.);
#11370=ORIENTED_EDGE('',*,*,#8097,.T.);
#11371=ORIENTED_EDGE('',*,*,#8098,.T.);
#11372=ORIENTED_EDGE('',*,*,#8099,.T.);
#11373=ORIENTED_EDGE('',*,*,#8100,.T.);
#11374=ORIENTED_EDGE('',*,*,#8095,.F.);
#11375=ORIENTED_EDGE('',*,*,#8101,.T.);
#11376=ORIENTED_EDGE('',*,*,#8102,.T.);
#11377=ORIENTED_EDGE('',*,*,#8103,.T.);
#11378=ORIENTED_EDGE('',*,*,#8104,.T.);
#11379=ORIENTED_EDGE('',*,*,#8098,.F.);
#11380=ORIENTED_EDGE('',*,*,#8105,.T.);
#11381=ORIENTED_EDGE('',*,*,#8106,.T.);
#11382=ORIENTED_EDGE('',*,*,#8107,.T.);
#11383=ORIENTED_EDGE('',*,*,#8108,.T.);
#11384=ORIENTED_EDGE('',*,*,#8103,.F.);
#11385=ORIENTED_EDGE('',*,*,#8109,.T.);
#11386=ORIENTED_EDGE('',*,*,#8110,.T.);
#11387=ORIENTED_EDGE('',*,*,#8111,.T.);
#11388=ORIENTED_EDGE('',*,*,#8112,.T.);
#11389=ORIENTED_EDGE('',*,*,#8106,.F.);
#11390=ORIENTED_EDGE('',*,*,#8113,.T.);
#11391=ORIENTED_EDGE('',*,*,#8114,.T.);
#11392=ORIENTED_EDGE('',*,*,#8115,.T.);
#11393=ORIENTED_EDGE('',*,*,#8116,.T.);
#11394=ORIENTED_EDGE('',*,*,#8111,.F.);
#11395=ORIENTED_EDGE('',*,*,#8117,.T.);
#11396=ORIENTED_EDGE('',*,*,#8118,.T.);
#11397=ORIENTED_EDGE('',*,*,#8119,.T.);
#11398=ORIENTED_EDGE('',*,*,#8120,.T.);
#11399=ORIENTED_EDGE('',*,*,#8114,.F.);
#11400=ORIENTED_EDGE('',*,*,#8121,.T.);
#11401=ORIENTED_EDGE('',*,*,#8122,.T.);
#11402=ORIENTED_EDGE('',*,*,#8123,.T.);
#11403=ORIENTED_EDGE('',*,*,#8124,.T.);
#11404=ORIENTED_EDGE('',*,*,#8119,.F.);
#11405=ORIENTED_EDGE('',*,*,#8125,.T.);
#11406=ORIENTED_EDGE('',*,*,#8126,.T.);
#11407=ORIENTED_EDGE('',*,*,#8127,.T.);
#11408=ORIENTED_EDGE('',*,*,#8128,.T.);
#11409=ORIENTED_EDGE('',*,*,#8122,.F.);
#11410=ORIENTED_EDGE('',*,*,#8129,.T.);
#11411=ORIENTED_EDGE('',*,*,#8130,.F.);
#11412=ORIENTED_EDGE('',*,*,#8131,.T.);
#11413=ORIENTED_EDGE('',*,*,#8132,.F.);
#11414=ORIENTED_EDGE('',*,*,#8133,.T.);
#11415=ORIENTED_EDGE('',*,*,#8134,.T.);
#11416=ORIENTED_EDGE('',*,*,#8135,.T.);
#11417=ORIENTED_EDGE('',*,*,#8136,.F.);
#11418=ORIENTED_EDGE('',*,*,#8137,.F.);
#11419=ORIENTED_EDGE('',*,*,#8138,.F.);
#11420=ORIENTED_EDGE('',*,*,#8139,.T.);
#11421=ORIENTED_EDGE('',*,*,#8140,.T.);
#11422=ORIENTED_EDGE('',*,*,#8141,.T.);
#11423=ORIENTED_EDGE('',*,*,#8134,.F.);
#11424=ORIENTED_EDGE('',*,*,#8142,.F.);
#11425=ORIENTED_EDGE('',*,*,#8143,.F.);
#11426=ORIENTED_EDGE('',*,*,#8144,.T.);
#11427=ORIENTED_EDGE('',*,*,#8145,.T.);
#11428=ORIENTED_EDGE('',*,*,#8146,.T.);
#11429=ORIENTED_EDGE('',*,*,#8139,.F.);
#11430=ORIENTED_EDGE('',*,*,#8147,.F.);
#11431=ORIENTED_EDGE('',*,*,#8148,.F.);
#11432=ORIENTED_EDGE('',*,*,#8149,.T.);
#11433=ORIENTED_EDGE('',*,*,#8150,.T.);
#11434=ORIENTED_EDGE('',*,*,#8151,.T.);
#11435=ORIENTED_EDGE('',*,*,#8144,.F.);
#11436=ORIENTED_EDGE('',*,*,#8152,.F.);
#11437=ORIENTED_EDGE('',*,*,#8153,.F.);
#11438=ORIENTED_EDGE('',*,*,#8154,.T.);
#11439=ORIENTED_EDGE('',*,*,#8155,.T.);
#11440=ORIENTED_EDGE('',*,*,#8156,.T.);
#11441=ORIENTED_EDGE('',*,*,#8149,.F.);
#11442=ORIENTED_EDGE('',*,*,#8157,.F.);
#11443=ORIENTED_EDGE('',*,*,#8158,.F.);
#11444=ORIENTED_EDGE('',*,*,#8159,.T.);
#11445=ORIENTED_EDGE('',*,*,#8160,.T.);
#11446=ORIENTED_EDGE('',*,*,#8161,.T.);
#11447=ORIENTED_EDGE('',*,*,#8154,.F.);
#11448=ORIENTED_EDGE('',*,*,#8162,.F.);
#11449=ORIENTED_EDGE('',*,*,#8163,.F.);
#11450=ORIENTED_EDGE('',*,*,#8164,.T.);
#11451=ORIENTED_EDGE('',*,*,#8165,.T.);
#11452=ORIENTED_EDGE('',*,*,#8166,.T.);
#11453=ORIENTED_EDGE('',*,*,#8159,.F.);
#11454=ORIENTED_EDGE('',*,*,#8167,.F.);
#11455=ORIENTED_EDGE('',*,*,#8168,.F.);
#11456=ORIENTED_EDGE('',*,*,#8169,.T.);
#11457=ORIENTED_EDGE('',*,*,#8170,.T.);
#11458=ORIENTED_EDGE('',*,*,#8171,.T.);
#11459=ORIENTED_EDGE('',*,*,#8164,.F.);
#11460=ORIENTED_EDGE('',*,*,#8172,.F.);
#11461=ORIENTED_EDGE('',*,*,#8173,.F.);
#11462=ORIENTED_EDGE('',*,*,#8174,.T.);
#11463=ORIENTED_EDGE('',*,*,#8175,.T.);
#11464=ORIENTED_EDGE('',*,*,#8176,.T.);
#11465=ORIENTED_EDGE('',*,*,#8169,.F.);
#11466=ORIENTED_EDGE('',*,*,#8177,.F.);
#11467=ORIENTED_EDGE('',*,*,#8178,.F.);
#11468=ORIENTED_EDGE('',*,*,#8179,.T.);
#11469=ORIENTED_EDGE('',*,*,#8180,.T.);
#11470=ORIENTED_EDGE('',*,*,#8181,.T.);
#11471=ORIENTED_EDGE('',*,*,#8174,.F.);
#11472=ORIENTED_EDGE('',*,*,#8182,.F.);
#11473=ORIENTED_EDGE('',*,*,#8183,.F.);
#11474=ORIENTED_EDGE('',*,*,#8184,.T.);
#11475=ORIENTED_EDGE('',*,*,#8185,.T.);
#11476=ORIENTED_EDGE('',*,*,#8186,.T.);
#11477=ORIENTED_EDGE('',*,*,#8179,.F.);
#11478=ORIENTED_EDGE('',*,*,#8187,.F.);
#11479=ORIENTED_EDGE('',*,*,#8188,.F.);
#11480=ORIENTED_EDGE('',*,*,#8189,.T.);
#11481=ORIENTED_EDGE('',*,*,#8190,.T.);
#11482=ORIENTED_EDGE('',*,*,#8191,.T.);
#11483=ORIENTED_EDGE('',*,*,#8184,.F.);
#11484=ORIENTED_EDGE('',*,*,#8192,.F.);
#11485=ORIENTED_EDGE('',*,*,#8193,.F.);
#11486=ORIENTED_EDGE('',*,*,#8194,.T.);
#11487=ORIENTED_EDGE('',*,*,#8195,.T.);
#11488=ORIENTED_EDGE('',*,*,#8196,.T.);
#11489=ORIENTED_EDGE('',*,*,#8189,.F.);
#11490=ORIENTED_EDGE('',*,*,#8197,.F.);
#11491=ORIENTED_EDGE('',*,*,#8198,.F.);
#11492=ORIENTED_EDGE('',*,*,#8199,.F.);
#11493=ORIENTED_EDGE('',*,*,#8200,.F.);
#11494=ORIENTED_EDGE('',*,*,#8201,.F.);
#11495=ORIENTED_EDGE('',*,*,#8202,.F.);
#11496=ORIENTED_EDGE('',*,*,#8203,.T.);
#11497=ORIENTED_EDGE('',*,*,#8204,.T.);
#11498=ORIENTED_EDGE('',*,*,#8205,.T.);
#11499=ORIENTED_EDGE('',*,*,#8206,.T.);
#11500=ORIENTED_EDGE('',*,*,#8207,.F.);
#11501=ORIENTED_EDGE('',*,*,#8208,.F.);
#11502=ORIENTED_EDGE('',*,*,#8209,.F.);
#11503=ORIENTED_EDGE('',*,*,#8210,.T.);
#11504=ORIENTED_EDGE('',*,*,#8211,.T.);
#11505=ORIENTED_EDGE('',*,*,#8212,.T.);
#11506=ORIENTED_EDGE('',*,*,#8205,.F.);
#11507=ORIENTED_EDGE('',*,*,#8213,.F.);
#11508=ORIENTED_EDGE('',*,*,#8214,.F.);
#11509=ORIENTED_EDGE('',*,*,#8215,.T.);
#11510=ORIENTED_EDGE('',*,*,#8216,.T.);
#11511=ORIENTED_EDGE('',*,*,#8217,.T.);
#11512=ORIENTED_EDGE('',*,*,#8210,.F.);
#11513=ORIENTED_EDGE('',*,*,#8218,.F.);
#11514=ORIENTED_EDGE('',*,*,#8219,.F.);
#11515=ORIENTED_EDGE('',*,*,#8220,.T.);
#11516=ORIENTED_EDGE('',*,*,#8221,.T.);
#11517=ORIENTED_EDGE('',*,*,#8222,.T.);
#11518=ORIENTED_EDGE('',*,*,#8215,.F.);
#11519=ORIENTED_EDGE('',*,*,#8223,.F.);
#11520=ORIENTED_EDGE('',*,*,#8224,.F.);
#11521=ORIENTED_EDGE('',*,*,#8225,.T.);
#11522=ORIENTED_EDGE('',*,*,#8226,.T.);
#11523=ORIENTED_EDGE('',*,*,#8227,.T.);
#11524=ORIENTED_EDGE('',*,*,#8220,.F.);
#11525=ORIENTED_EDGE('',*,*,#8228,.F.);
#11526=ORIENTED_EDGE('',*,*,#8229,.F.);
#11527=ORIENTED_EDGE('',*,*,#8230,.T.);
#11528=ORIENTED_EDGE('',*,*,#8231,.T.);
#11529=ORIENTED_EDGE('',*,*,#8232,.T.);
#11530=ORIENTED_EDGE('',*,*,#8225,.F.);
#11531=ORIENTED_EDGE('',*,*,#8233,.F.);
#11532=ORIENTED_EDGE('',*,*,#8234,.F.);
#11533=ORIENTED_EDGE('',*,*,#8235,.T.);
#11534=ORIENTED_EDGE('',*,*,#8236,.T.);
#11535=ORIENTED_EDGE('',*,*,#8237,.T.);
#11536=ORIENTED_EDGE('',*,*,#8230,.F.);
#11537=ORIENTED_EDGE('',*,*,#8238,.F.);
#11538=ORIENTED_EDGE('',*,*,#8239,.F.);
#11539=ORIENTED_EDGE('',*,*,#8240,.T.);
#11540=ORIENTED_EDGE('',*,*,#8241,.T.);
#11541=ORIENTED_EDGE('',*,*,#8242,.T.);
#11542=ORIENTED_EDGE('',*,*,#8235,.F.);
#11543=ORIENTED_EDGE('',*,*,#8243,.F.);
#11544=ORIENTED_EDGE('',*,*,#8244,.F.);
#11545=ORIENTED_EDGE('',*,*,#8245,.T.);
#11546=ORIENTED_EDGE('',*,*,#8246,.T.);
#11547=ORIENTED_EDGE('',*,*,#8247,.T.);
#11548=ORIENTED_EDGE('',*,*,#8240,.F.);
#11549=ORIENTED_EDGE('',*,*,#8248,.F.);
#11550=ORIENTED_EDGE('',*,*,#8249,.F.);
#11551=ORIENTED_EDGE('',*,*,#8250,.T.);
#11552=ORIENTED_EDGE('',*,*,#8251,.T.);
#11553=ORIENTED_EDGE('',*,*,#8252,.T.);
#11554=ORIENTED_EDGE('',*,*,#8245,.F.);
#11555=ORIENTED_EDGE('',*,*,#8253,.F.);
#11556=ORIENTED_EDGE('',*,*,#8254,.F.);
#11557=ORIENTED_EDGE('',*,*,#8255,.T.);
#11558=ORIENTED_EDGE('',*,*,#8256,.T.);
#11559=ORIENTED_EDGE('',*,*,#8257,.T.);
#11560=ORIENTED_EDGE('',*,*,#8250,.F.);
#11561=ORIENTED_EDGE('',*,*,#8258,.F.);
#11562=ORIENTED_EDGE('',*,*,#8259,.F.);
#11563=ORIENTED_EDGE('',*,*,#8260,.T.);
#11564=ORIENTED_EDGE('',*,*,#8261,.T.);
#11565=ORIENTED_EDGE('',*,*,#8262,.T.);
#11566=ORIENTED_EDGE('',*,*,#8255,.F.);
#11567=ORIENTED_EDGE('',*,*,#8263,.F.);
#11568=ORIENTED_EDGE('',*,*,#8264,.F.);
#11569=ORIENTED_EDGE('',*,*,#8265,.T.);
#11570=ORIENTED_EDGE('',*,*,#8266,.T.);
#11571=ORIENTED_EDGE('',*,*,#8267,.T.);
#11572=ORIENTED_EDGE('',*,*,#8260,.F.);
#11573=ORIENTED_EDGE('',*,*,#8268,.F.);
#11574=ORIENTED_EDGE('',*,*,#8269,.F.);
#11575=ORIENTED_EDGE('',*,*,#8270,.F.);
#11576=ORIENTED_EDGE('',*,*,#8271,.F.);
#11577=ORIENTED_EDGE('',*,*,#8272,.F.);
#11578=ORIENTED_EDGE('',*,*,#8273,.F.);
#11579=ORIENTED_EDGE('',*,*,#8274,.T.);
#11580=ORIENTED_EDGE('',*,*,#8275,.T.);
#11581=ORIENTED_EDGE('',*,*,#8276,.T.);
#11582=ORIENTED_EDGE('',*,*,#8277,.T.);
#11583=ORIENTED_EDGE('',*,*,#8278,.F.);
#11584=ORIENTED_EDGE('',*,*,#8279,.F.);
#11585=ORIENTED_EDGE('',*,*,#8280,.F.);
#11586=ORIENTED_EDGE('',*,*,#8281,.T.);
#11587=ORIENTED_EDGE('',*,*,#8282,.T.);
#11588=ORIENTED_EDGE('',*,*,#8283,.T.);
#11589=ORIENTED_EDGE('',*,*,#8276,.F.);
#11590=ORIENTED_EDGE('',*,*,#8284,.F.);
#11591=ORIENTED_EDGE('',*,*,#8285,.F.);
#11592=ORIENTED_EDGE('',*,*,#8286,.T.);
#11593=ORIENTED_EDGE('',*,*,#8287,.T.);
#11594=ORIENTED_EDGE('',*,*,#8288,.T.);
#11595=ORIENTED_EDGE('',*,*,#8281,.F.);
#11596=ORIENTED_EDGE('',*,*,#8289,.F.);
#11597=ORIENTED_EDGE('',*,*,#8290,.F.);
#11598=ORIENTED_EDGE('',*,*,#8291,.T.);
#11599=ORIENTED_EDGE('',*,*,#8292,.T.);
#11600=ORIENTED_EDGE('',*,*,#8293,.T.);
#11601=ORIENTED_EDGE('',*,*,#8286,.F.);
#11602=ORIENTED_EDGE('',*,*,#8294,.F.);
#11603=ORIENTED_EDGE('',*,*,#8295,.F.);
#11604=ORIENTED_EDGE('',*,*,#8296,.T.);
#11605=ORIENTED_EDGE('',*,*,#8297,.T.);
#11606=ORIENTED_EDGE('',*,*,#8298,.T.);
#11607=ORIENTED_EDGE('',*,*,#8291,.F.);
#11608=ORIENTED_EDGE('',*,*,#8299,.F.);
#11609=ORIENTED_EDGE('',*,*,#8300,.F.);
#11610=ORIENTED_EDGE('',*,*,#8301,.T.);
#11611=ORIENTED_EDGE('',*,*,#8302,.T.);
#11612=ORIENTED_EDGE('',*,*,#8303,.T.);
#11613=ORIENTED_EDGE('',*,*,#8296,.F.);
#11614=ORIENTED_EDGE('',*,*,#8304,.F.);
#11615=ORIENTED_EDGE('',*,*,#8305,.F.);
#11616=ORIENTED_EDGE('',*,*,#8306,.T.);
#11617=ORIENTED_EDGE('',*,*,#8307,.T.);
#11618=ORIENTED_EDGE('',*,*,#8308,.T.);
#11619=ORIENTED_EDGE('',*,*,#8301,.F.);
#11620=ORIENTED_EDGE('',*,*,#8309,.F.);
#11621=ORIENTED_EDGE('',*,*,#8310,.F.);
#11622=ORIENTED_EDGE('',*,*,#8311,.T.);
#11623=ORIENTED_EDGE('',*,*,#8312,.T.);
#11624=ORIENTED_EDGE('',*,*,#8313,.T.);
#11625=ORIENTED_EDGE('',*,*,#8306,.F.);
#11626=ORIENTED_EDGE('',*,*,#8314,.F.);
#11627=ORIENTED_EDGE('',*,*,#8315,.F.);
#11628=ORIENTED_EDGE('',*,*,#8316,.T.);
#11629=ORIENTED_EDGE('',*,*,#8317,.T.);
#11630=ORIENTED_EDGE('',*,*,#8318,.T.);
#11631=ORIENTED_EDGE('',*,*,#8311,.F.);
#11632=ORIENTED_EDGE('',*,*,#8319,.F.);
#11633=ORIENTED_EDGE('',*,*,#8320,.F.);
#11634=ORIENTED_EDGE('',*,*,#8321,.T.);
#11635=ORIENTED_EDGE('',*,*,#8322,.T.);
#11636=ORIENTED_EDGE('',*,*,#8323,.T.);
#11637=ORIENTED_EDGE('',*,*,#8316,.F.);
#11638=ORIENTED_EDGE('',*,*,#8324,.F.);
#11639=ORIENTED_EDGE('',*,*,#8325,.F.);
#11640=ORIENTED_EDGE('',*,*,#8326,.T.);
#11641=ORIENTED_EDGE('',*,*,#8327,.T.);
#11642=ORIENTED_EDGE('',*,*,#8328,.T.);
#11643=ORIENTED_EDGE('',*,*,#8321,.F.);
#11644=ORIENTED_EDGE('',*,*,#8329,.F.);
#11645=ORIENTED_EDGE('',*,*,#8330,.F.);
#11646=ORIENTED_EDGE('',*,*,#8331,.T.);
#11647=ORIENTED_EDGE('',*,*,#8332,.T.);
#11648=ORIENTED_EDGE('',*,*,#8333,.T.);
#11649=ORIENTED_EDGE('',*,*,#8326,.F.);
#11650=ORIENTED_EDGE('',*,*,#8334,.F.);
#11651=ORIENTED_EDGE('',*,*,#8335,.F.);
#11652=ORIENTED_EDGE('',*,*,#8336,.T.);
#11653=ORIENTED_EDGE('',*,*,#8337,.T.);
#11654=ORIENTED_EDGE('',*,*,#8338,.T.);
#11655=ORIENTED_EDGE('',*,*,#8331,.F.);
#11656=ORIENTED_EDGE('',*,*,#8339,.F.);
#11657=ORIENTED_EDGE('',*,*,#8340,.F.);
#11658=ORIENTED_EDGE('',*,*,#8341,.F.);
#11659=ORIENTED_EDGE('',*,*,#8342,.F.);
#11660=ORIENTED_EDGE('',*,*,#8343,.F.);
#11661=ORIENTED_EDGE('',*,*,#8344,.F.);
#11662=ORIENTED_EDGE('',*,*,#8345,.T.);
#11663=ORIENTED_EDGE('',*,*,#8346,.T.);
#11664=ORIENTED_EDGE('',*,*,#8347,.T.);
#11665=ORIENTED_EDGE('',*,*,#8348,.T.);
#11666=ORIENTED_EDGE('',*,*,#8349,.F.);
#11667=ORIENTED_EDGE('',*,*,#8350,.F.);
#11668=ORIENTED_EDGE('',*,*,#8351,.F.);
#11669=ORIENTED_EDGE('',*,*,#8352,.T.);
#11670=ORIENTED_EDGE('',*,*,#8353,.T.);
#11671=ORIENTED_EDGE('',*,*,#8354,.T.);
#11672=ORIENTED_EDGE('',*,*,#8347,.F.);
#11673=ORIENTED_EDGE('',*,*,#8355,.F.);
#11674=ORIENTED_EDGE('',*,*,#8356,.F.);
#11675=ORIENTED_EDGE('',*,*,#8357,.T.);
#11676=ORIENTED_EDGE('',*,*,#8358,.T.);
#11677=ORIENTED_EDGE('',*,*,#8359,.T.);
#11678=ORIENTED_EDGE('',*,*,#8352,.F.);
#11679=ORIENTED_EDGE('',*,*,#8360,.F.);
#11680=ORIENTED_EDGE('',*,*,#8361,.F.);
#11681=ORIENTED_EDGE('',*,*,#8362,.T.);
#11682=ORIENTED_EDGE('',*,*,#8363,.T.);
#11683=ORIENTED_EDGE('',*,*,#8364,.T.);
#11684=ORIENTED_EDGE('',*,*,#8357,.F.);
#11685=ORIENTED_EDGE('',*,*,#8365,.F.);
#11686=ORIENTED_EDGE('',*,*,#8366,.F.);
#11687=ORIENTED_EDGE('',*,*,#8367,.T.);
#11688=ORIENTED_EDGE('',*,*,#8368,.T.);
#11689=ORIENTED_EDGE('',*,*,#8369,.T.);
#11690=ORIENTED_EDGE('',*,*,#8362,.F.);
#11691=ORIENTED_EDGE('',*,*,#8370,.F.);
#11692=ORIENTED_EDGE('',*,*,#8371,.F.);
#11693=ORIENTED_EDGE('',*,*,#8372,.T.);
#11694=ORIENTED_EDGE('',*,*,#8373,.T.);
#11695=ORIENTED_EDGE('',*,*,#8374,.T.);
#11696=ORIENTED_EDGE('',*,*,#8367,.F.);
#11697=ORIENTED_EDGE('',*,*,#8375,.F.);
#11698=ORIENTED_EDGE('',*,*,#8376,.F.);
#11699=ORIENTED_EDGE('',*,*,#8377,.T.);
#11700=ORIENTED_EDGE('',*,*,#8378,.T.);
#11701=ORIENTED_EDGE('',*,*,#8379,.T.);
#11702=ORIENTED_EDGE('',*,*,#8372,.F.);
#11703=ORIENTED_EDGE('',*,*,#8380,.F.);
#11704=ORIENTED_EDGE('',*,*,#8381,.F.);
#11705=ORIENTED_EDGE('',*,*,#8382,.T.);
#11706=ORIENTED_EDGE('',*,*,#8383,.T.);
#11707=ORIENTED_EDGE('',*,*,#8384,.T.);
#11708=ORIENTED_EDGE('',*,*,#8377,.F.);
#11709=ORIENTED_EDGE('',*,*,#8385,.F.);
#11710=ORIENTED_EDGE('',*,*,#8386,.F.);
#11711=ORIENTED_EDGE('',*,*,#8387,.T.);
#11712=ORIENTED_EDGE('',*,*,#8388,.T.);
#11713=ORIENTED_EDGE('',*,*,#8389,.T.);
#11714=ORIENTED_EDGE('',*,*,#8382,.F.);
#11715=ORIENTED_EDGE('',*,*,#8390,.F.);
#11716=ORIENTED_EDGE('',*,*,#8391,.F.);
#11717=ORIENTED_EDGE('',*,*,#8392,.T.);
#11718=ORIENTED_EDGE('',*,*,#8393,.T.);
#11719=ORIENTED_EDGE('',*,*,#8394,.T.);
#11720=ORIENTED_EDGE('',*,*,#8387,.F.);
#11721=ORIENTED_EDGE('',*,*,#8395,.F.);
#11722=ORIENTED_EDGE('',*,*,#8396,.F.);
#11723=ORIENTED_EDGE('',*,*,#8397,.T.);
#11724=ORIENTED_EDGE('',*,*,#8398,.T.);
#11725=ORIENTED_EDGE('',*,*,#8399,.T.);
#11726=ORIENTED_EDGE('',*,*,#8392,.F.);
#11727=ORIENTED_EDGE('',*,*,#8400,.F.);
#11728=ORIENTED_EDGE('',*,*,#8401,.F.);
#11729=ORIENTED_EDGE('',*,*,#8402,.T.);
#11730=ORIENTED_EDGE('',*,*,#8403,.T.);
#11731=ORIENTED_EDGE('',*,*,#8404,.T.);
#11732=ORIENTED_EDGE('',*,*,#8397,.F.);
#11733=ORIENTED_EDGE('',*,*,#8405,.F.);
#11734=ORIENTED_EDGE('',*,*,#8406,.F.);
#11735=ORIENTED_EDGE('',*,*,#8407,.T.);
#11736=ORIENTED_EDGE('',*,*,#8408,.T.);
#11737=ORIENTED_EDGE('',*,*,#8409,.T.);
#11738=ORIENTED_EDGE('',*,*,#8402,.F.);
#11739=ORIENTED_EDGE('',*,*,#8410,.F.);
#11740=ORIENTED_EDGE('',*,*,#8411,.F.);
#11741=ORIENTED_EDGE('',*,*,#8412,.F.);
#11742=ORIENTED_EDGE('',*,*,#8413,.F.);
#11743=ORIENTED_EDGE('',*,*,#8414,.F.);
#11744=ORIENTED_EDGE('',*,*,#8415,.F.);
#11745=ORIENTED_EDGE('',*,*,#8416,.T.);
#11746=ORIENTED_EDGE('',*,*,#8417,.T.);
#11747=ORIENTED_EDGE('',*,*,#8418,.T.);
#11748=ORIENTED_EDGE('',*,*,#8419,.T.);
#11749=ORIENTED_EDGE('',*,*,#8420,.T.);
#11750=ORIENTED_EDGE('',*,*,#8421,.T.);
#11751=ORIENTED_EDGE('',*,*,#8422,.T.);
#11752=ORIENTED_EDGE('',*,*,#8423,.T.);
#11753=ORIENTED_EDGE('',*,*,#8424,.T.);
#11754=ORIENTED_EDGE('',*,*,#8418,.F.);
#11755=ORIENTED_EDGE('',*,*,#8425,.T.);
#11756=ORIENTED_EDGE('',*,*,#8426,.T.);
#11757=ORIENTED_EDGE('',*,*,#8427,.T.);
#11758=ORIENTED_EDGE('',*,*,#8422,.F.);
#11759=ORIENTED_EDGE('',*,*,#8428,.T.);
#11760=ORIENTED_EDGE('',*,*,#8429,.T.);
#11761=ORIENTED_EDGE('',*,*,#8430,.T.);
#11762=ORIENTED_EDGE('',*,*,#8431,.T.);
#11763=ORIENTED_EDGE('',*,*,#8432,.T.);
#11764=ORIENTED_EDGE('',*,*,#8426,.F.);
#11765=ORIENTED_EDGE('',*,*,#8433,.T.);
#11766=ORIENTED_EDGE('',*,*,#8434,.T.);
#11767=ORIENTED_EDGE('',*,*,#8435,.T.);
#11768=ORIENTED_EDGE('',*,*,#8430,.F.);
#11769=ORIENTED_EDGE('',*,*,#8436,.T.);
#11770=ORIENTED_EDGE('',*,*,#8437,.T.);
#11771=ORIENTED_EDGE('',*,*,#8438,.T.);
#11772=ORIENTED_EDGE('',*,*,#8439,.T.);
#11773=ORIENTED_EDGE('',*,*,#8440,.T.);
#11774=ORIENTED_EDGE('',*,*,#8434,.F.);
#11775=ORIENTED_EDGE('',*,*,#8441,.T.);
#11776=ORIENTED_EDGE('',*,*,#8442,.T.);
#11777=ORIENTED_EDGE('',*,*,#8443,.T.);
#11778=ORIENTED_EDGE('',*,*,#8438,.F.);
#11779=ORIENTED_EDGE('',*,*,#8444,.T.);
#11780=ORIENTED_EDGE('',*,*,#8445,.T.);
#11781=ORIENTED_EDGE('',*,*,#8446,.T.);
#11782=ORIENTED_EDGE('',*,*,#8447,.T.);
#11783=ORIENTED_EDGE('',*,*,#8448,.T.);
#11784=ORIENTED_EDGE('',*,*,#8442,.F.);
#11785=ORIENTED_EDGE('',*,*,#8449,.T.);
#11786=ORIENTED_EDGE('',*,*,#8450,.T.);
#11787=ORIENTED_EDGE('',*,*,#8451,.T.);
#11788=ORIENTED_EDGE('',*,*,#8452,.T.);
#11789=ORIENTED_EDGE('',*,*,#8446,.F.);
#11790=ORIENTED_EDGE('',*,*,#8453,.T.);
#11791=ORIENTED_EDGE('',*,*,#8454,.T.);
#11792=ORIENTED_EDGE('',*,*,#8455,.T.);
#11793=ORIENTED_EDGE('',*,*,#8456,.T.);
#11794=ORIENTED_EDGE('',*,*,#8457,.T.);
#11795=ORIENTED_EDGE('',*,*,#8451,.F.);
#11796=ORIENTED_EDGE('',*,*,#8458,.T.);
#11797=ORIENTED_EDGE('',*,*,#8459,.T.);
#11798=ORIENTED_EDGE('',*,*,#8460,.T.);
#11799=ORIENTED_EDGE('',*,*,#8455,.F.);
#11800=ORIENTED_EDGE('',*,*,#8461,.T.);
#11801=ORIENTED_EDGE('',*,*,#8462,.T.);
#11802=ORIENTED_EDGE('',*,*,#8463,.T.);
#11803=ORIENTED_EDGE('',*,*,#8464,.T.);
#11804=ORIENTED_EDGE('',*,*,#8465,.T.);
#11805=ORIENTED_EDGE('',*,*,#8459,.F.);
#11806=ORIENTED_EDGE('',*,*,#8466,.T.);
#11807=ORIENTED_EDGE('',*,*,#8467,.T.);
#11808=ORIENTED_EDGE('',*,*,#8468,.T.);
#11809=ORIENTED_EDGE('',*,*,#8463,.F.);
#11810=ORIENTED_EDGE('',*,*,#8469,.T.);
#11811=ORIENTED_EDGE('',*,*,#8470,.T.);
#11812=ORIENTED_EDGE('',*,*,#8471,.F.);
#11813=ORIENTED_EDGE('',*,*,#8472,.T.);
#11814=ORIENTED_EDGE('',*,*,#8473,.T.);
#11815=ORIENTED_EDGE('',*,*,#8474,.F.);
#11816=ORIENTED_EDGE('',*,*,#8475,.T.);
#11817=ORIENTED_EDGE('',*,*,#8476,.T.);
#11818=ORIENTED_EDGE('',*,*,#8477,.T.);
#11819=ORIENTED_EDGE('',*,*,#8478,.T.);
#11820=ORIENTED_EDGE('',*,*,#8479,.T.);
#11821=ORIENTED_EDGE('',*,*,#8480,.T.);
#11822=ORIENTED_EDGE('',*,*,#8481,.T.);
#11823=ORIENTED_EDGE('',*,*,#8482,.T.);
#11824=ORIENTED_EDGE('',*,*,#8476,.F.);
#11825=ORIENTED_EDGE('',*,*,#8483,.T.);
#11826=ORIENTED_EDGE('',*,*,#8484,.T.);
#11827=ORIENTED_EDGE('',*,*,#8485,.T.);
#11828=ORIENTED_EDGE('',*,*,#8480,.F.);
#11829=ORIENTED_EDGE('',*,*,#8486,.T.);
#11830=ORIENTED_EDGE('',*,*,#8487,.T.);
#11831=ORIENTED_EDGE('',*,*,#8488,.T.);
#11832=ORIENTED_EDGE('',*,*,#8489,.T.);
#11833=ORIENTED_EDGE('',*,*,#8490,.T.);
#11834=ORIENTED_EDGE('',*,*,#8484,.F.);
#11835=ORIENTED_EDGE('',*,*,#8491,.T.);
#11836=ORIENTED_EDGE('',*,*,#8492,.T.);
#11837=ORIENTED_EDGE('',*,*,#8493,.T.);
#11838=ORIENTED_EDGE('',*,*,#8488,.F.);
#11839=ORIENTED_EDGE('',*,*,#8494,.T.);
#11840=ORIENTED_EDGE('',*,*,#8495,.T.);
#11841=ORIENTED_EDGE('',*,*,#8496,.T.);
#11842=ORIENTED_EDGE('',*,*,#8497,.T.);
#11843=ORIENTED_EDGE('',*,*,#8498,.T.);
#11844=ORIENTED_EDGE('',*,*,#8492,.F.);
#11845=ORIENTED_EDGE('',*,*,#8499,.T.);
#11846=ORIENTED_EDGE('',*,*,#8500,.T.);
#11847=ORIENTED_EDGE('',*,*,#8501,.T.);
#11848=ORIENTED_EDGE('',*,*,#8496,.F.);
#11849=ORIENTED_EDGE('',*,*,#8502,.T.);
#11850=ORIENTED_EDGE('',*,*,#8503,.T.);
#11851=ORIENTED_EDGE('',*,*,#8504,.T.);
#11852=ORIENTED_EDGE('',*,*,#8505,.T.);
#11853=ORIENTED_EDGE('',*,*,#8506,.T.);
#11854=ORIENTED_EDGE('',*,*,#8500,.F.);
#11855=ORIENTED_EDGE('',*,*,#8507,.T.);
#11856=ORIENTED_EDGE('',*,*,#8508,.T.);
#11857=ORIENTED_EDGE('',*,*,#8509,.T.);
#11858=ORIENTED_EDGE('',*,*,#8510,.T.);
#11859=ORIENTED_EDGE('',*,*,#8504,.F.);
#11860=ORIENTED_EDGE('',*,*,#8511,.T.);
#11861=ORIENTED_EDGE('',*,*,#8512,.T.);
#11862=ORIENTED_EDGE('',*,*,#8513,.T.);
#11863=ORIENTED_EDGE('',*,*,#8514,.T.);
#11864=ORIENTED_EDGE('',*,*,#8515,.T.);
#11865=ORIENTED_EDGE('',*,*,#8509,.F.);
#11866=ORIENTED_EDGE('',*,*,#8516,.T.);
#11867=ORIENTED_EDGE('',*,*,#8517,.T.);
#11868=ORIENTED_EDGE('',*,*,#8518,.T.);
#11869=ORIENTED_EDGE('',*,*,#8513,.F.);
#11870=ORIENTED_EDGE('',*,*,#8519,.T.);
#11871=ORIENTED_EDGE('',*,*,#8520,.T.);
#11872=ORIENTED_EDGE('',*,*,#8521,.T.);
#11873=ORIENTED_EDGE('',*,*,#8522,.T.);
#11874=ORIENTED_EDGE('',*,*,#8523,.T.);
#11875=ORIENTED_EDGE('',*,*,#8517,.F.);
#11876=ORIENTED_EDGE('',*,*,#8524,.T.);
#11877=ORIENTED_EDGE('',*,*,#8525,.T.);
#11878=ORIENTED_EDGE('',*,*,#8526,.T.);
#11879=ORIENTED_EDGE('',*,*,#8521,.F.);
#11880=ORIENTED_EDGE('',*,*,#8527,.T.);
#11881=ORIENTED_EDGE('',*,*,#8528,.T.);
#11882=ORIENTED_EDGE('',*,*,#8529,.F.);
#11883=ORIENTED_EDGE('',*,*,#8530,.T.);
#11884=ORIENTED_EDGE('',*,*,#8531,.T.);
#11885=ORIENTED_EDGE('',*,*,#8532,.F.);
#11886=ORIENTED_EDGE('',*,*,#8533,.T.);
#11887=ORIENTED_EDGE('',*,*,#8534,.T.);
#11888=ORIENTED_EDGE('',*,*,#8535,.T.);
#11889=ORIENTED_EDGE('',*,*,#8536,.T.);
#11890=ORIENTED_EDGE('',*,*,#8537,.T.);
#11891=ORIENTED_EDGE('',*,*,#8538,.T.);
#11892=ORIENTED_EDGE('',*,*,#8539,.T.);
#11893=ORIENTED_EDGE('',*,*,#8534,.F.);
#11894=ORIENTED_EDGE('',*,*,#8540,.T.);
#11895=ORIENTED_EDGE('',*,*,#8541,.T.);
#11896=ORIENTED_EDGE('',*,*,#8542,.T.);
#11897=ORIENTED_EDGE('',*,*,#8538,.F.);
#11898=ORIENTED_EDGE('',*,*,#8543,.T.);
#11899=ORIENTED_EDGE('',*,*,#8544,.T.);
#11900=ORIENTED_EDGE('',*,*,#8545,.T.);
#11901=ORIENTED_EDGE('',*,*,#8546,.T.);
#11902=ORIENTED_EDGE('',*,*,#8541,.F.);
#11903=ORIENTED_EDGE('',*,*,#8547,.T.);
#11904=ORIENTED_EDGE('',*,*,#8548,.T.);
#11905=ORIENTED_EDGE('',*,*,#8549,.T.);
#11906=ORIENTED_EDGE('',*,*,#8545,.F.);
#11907=ORIENTED_EDGE('',*,*,#8550,.T.);
#11908=ORIENTED_EDGE('',*,*,#8551,.T.);
#11909=ORIENTED_EDGE('',*,*,#8552,.T.);
#11910=ORIENTED_EDGE('',*,*,#8553,.T.);
#11911=ORIENTED_EDGE('',*,*,#8554,.T.);
#11912=ORIENTED_EDGE('',*,*,#8548,.F.);
#11913=ORIENTED_EDGE('',*,*,#8555,.T.);
#11914=ORIENTED_EDGE('',*,*,#8556,.T.);
#11915=ORIENTED_EDGE('',*,*,#8557,.T.);
#11916=ORIENTED_EDGE('',*,*,#8552,.F.);
#11917=ORIENTED_EDGE('',*,*,#8558,.T.);
#11918=ORIENTED_EDGE('',*,*,#8559,.T.);
#11919=ORIENTED_EDGE('',*,*,#8560,.T.);
#11920=ORIENTED_EDGE('',*,*,#8561,.T.);
#11921=ORIENTED_EDGE('',*,*,#8562,.T.);
#11922=ORIENTED_EDGE('',*,*,#8556,.F.);
#11923=ORIENTED_EDGE('',*,*,#8563,.T.);
#11924=ORIENTED_EDGE('',*,*,#8564,.T.);
#11925=ORIENTED_EDGE('',*,*,#8565,.T.);
#11926=ORIENTED_EDGE('',*,*,#8566,.T.);
#11927=ORIENTED_EDGE('',*,*,#8560,.F.);
#11928=ORIENTED_EDGE('',*,*,#8567,.T.);
#11929=ORIENTED_EDGE('',*,*,#8568,.T.);
#11930=ORIENTED_EDGE('',*,*,#8569,.T.);
#11931=ORIENTED_EDGE('',*,*,#8570,.T.);
#11932=ORIENTED_EDGE('',*,*,#8571,.T.);
#11933=ORIENTED_EDGE('',*,*,#8565,.F.);
#11934=ORIENTED_EDGE('',*,*,#8572,.T.);
#11935=ORIENTED_EDGE('',*,*,#8573,.T.);
#11936=ORIENTED_EDGE('',*,*,#8574,.T.);
#11937=ORIENTED_EDGE('',*,*,#8569,.F.);
#11938=ORIENTED_EDGE('',*,*,#8575,.T.);
#11939=ORIENTED_EDGE('',*,*,#8576,.T.);
#11940=ORIENTED_EDGE('',*,*,#8577,.T.);
#11941=ORIENTED_EDGE('',*,*,#8578,.T.);
#11942=ORIENTED_EDGE('',*,*,#8579,.T.);
#11943=ORIENTED_EDGE('',*,*,#8573,.F.);
#11944=ORIENTED_EDGE('',*,*,#8580,.T.);
#11945=ORIENTED_EDGE('',*,*,#8581,.T.);
#11946=ORIENTED_EDGE('',*,*,#8582,.T.);
#11947=ORIENTED_EDGE('',*,*,#8577,.F.);
#11948=ORIENTED_EDGE('',*,*,#8583,.T.);
#11949=ORIENTED_EDGE('',*,*,#8584,.F.);
#11950=ORIENTED_EDGE('',*,*,#8585,.T.);
#11951=ORIENTED_EDGE('',*,*,#8586,.F.);
#11952=ORIENTED_EDGE('',*,*,#8587,.T.);
#11953=ORIENTED_EDGE('',*,*,#8588,.T.);
#11954=ORIENTED_EDGE('',*,*,#8589,.T.);
#11955=ORIENTED_EDGE('',*,*,#8590,.T.);
#11956=ORIENTED_EDGE('',*,*,#8591,.T.);
#11957=ORIENTED_EDGE('',*,*,#8592,.T.);
#11958=ORIENTED_EDGE('',*,*,#8593,.T.);
#11959=ORIENTED_EDGE('',*,*,#8588,.F.);
#11960=ORIENTED_EDGE('',*,*,#8594,.T.);
#11961=ORIENTED_EDGE('',*,*,#8595,.T.);
#11962=ORIENTED_EDGE('',*,*,#8596,.T.);
#11963=ORIENTED_EDGE('',*,*,#8592,.F.);
#11964=ORIENTED_EDGE('',*,*,#8597,.T.);
#11965=ORIENTED_EDGE('',*,*,#8598,.T.);
#11966=ORIENTED_EDGE('',*,*,#8599,.T.);
#11967=ORIENTED_EDGE('',*,*,#8600,.T.);
#11968=ORIENTED_EDGE('',*,*,#8595,.F.);
#11969=ORIENTED_EDGE('',*,*,#8601,.T.);
#11970=ORIENTED_EDGE('',*,*,#8602,.T.);
#11971=ORIENTED_EDGE('',*,*,#8603,.T.);
#11972=ORIENTED_EDGE('',*,*,#8599,.F.);
#11973=ORIENTED_EDGE('',*,*,#8604,.T.);
#11974=ORIENTED_EDGE('',*,*,#8605,.T.);
#11975=ORIENTED_EDGE('',*,*,#8606,.T.);
#11976=ORIENTED_EDGE('',*,*,#8607,.T.);
#11977=ORIENTED_EDGE('',*,*,#8608,.T.);
#11978=ORIENTED_EDGE('',*,*,#8602,.F.);
#11979=ORIENTED_EDGE('',*,*,#8609,.T.);
#11980=ORIENTED_EDGE('',*,*,#8610,.T.);
#11981=ORIENTED_EDGE('',*,*,#8611,.T.);
#11982=ORIENTED_EDGE('',*,*,#8606,.F.);
#11983=ORIENTED_EDGE('',*,*,#8612,.T.);
#11984=ORIENTED_EDGE('',*,*,#8613,.T.);
#11985=ORIENTED_EDGE('',*,*,#8614,.T.);
#11986=ORIENTED_EDGE('',*,*,#8615,.T.);
#11987=ORIENTED_EDGE('',*,*,#8616,.T.);
#11988=ORIENTED_EDGE('',*,*,#8610,.F.);
#11989=ORIENTED_EDGE('',*,*,#8617,.T.);
#11990=ORIENTED_EDGE('',*,*,#8618,.T.);
#11991=ORIENTED_EDGE('',*,*,#8619,.T.);
#11992=ORIENTED_EDGE('',*,*,#8620,.T.);
#11993=ORIENTED_EDGE('',*,*,#8614,.F.);
#11994=ORIENTED_EDGE('',*,*,#8621,.T.);
#11995=ORIENTED_EDGE('',*,*,#8622,.T.);
#11996=ORIENTED_EDGE('',*,*,#8623,.T.);
#11997=ORIENTED_EDGE('',*,*,#8624,.T.);
#11998=ORIENTED_EDGE('',*,*,#8625,.T.);
#11999=ORIENTED_EDGE('',*,*,#8619,.F.);
#12000=ORIENTED_EDGE('',*,*,#8626,.T.);
#12001=ORIENTED_EDGE('',*,*,#8627,.T.);
#12002=ORIENTED_EDGE('',*,*,#8628,.T.);
#12003=ORIENTED_EDGE('',*,*,#8623,.F.);
#12004=ORIENTED_EDGE('',*,*,#8629,.T.);
#12005=ORIENTED_EDGE('',*,*,#8630,.T.);
#12006=ORIENTED_EDGE('',*,*,#8631,.T.);
#12007=ORIENTED_EDGE('',*,*,#8632,.T.);
#12008=ORIENTED_EDGE('',*,*,#8633,.T.);
#12009=ORIENTED_EDGE('',*,*,#8627,.F.);
#12010=ORIENTED_EDGE('',*,*,#8634,.T.);
#12011=ORIENTED_EDGE('',*,*,#8635,.T.);
#12012=ORIENTED_EDGE('',*,*,#8636,.T.);
#12013=ORIENTED_EDGE('',*,*,#8631,.F.);
#12014=ORIENTED_EDGE('',*,*,#8637,.T.);
#12015=ORIENTED_EDGE('',*,*,#8638,.F.);
#12016=ORIENTED_EDGE('',*,*,#8639,.T.);
#12017=ORIENTED_EDGE('',*,*,#8640,.F.);
#12018=ORIENTED_EDGE('',*,*,#8641,.T.);
#12019=ORIENTED_EDGE('',*,*,#8638,.T.);
#12020=ORIENTED_EDGE('',*,*,#8642,.T.);
#12021=ORIENTED_EDGE('',*,*,#8643,.T.);
#12022=ORIENTED_EDGE('',*,*,#8635,.F.);
#12023=ORIENTED_EDGE('',*,*,#8644,.T.);
#12024=ORIENTED_EDGE('',*,*,#8584,.T.);
#12025=ORIENTED_EDGE('',*,*,#8645,.T.);
#12026=ORIENTED_EDGE('',*,*,#8646,.T.);
#12027=ORIENTED_EDGE('',*,*,#8581,.F.);
#12028=ORIENTED_EDGE('',*,*,#8647,.T.);
#12029=ORIENTED_EDGE('',*,*,#8529,.T.);
#12030=ORIENTED_EDGE('',*,*,#8648,.T.);
#12031=ORIENTED_EDGE('',*,*,#8649,.T.);
#12032=ORIENTED_EDGE('',*,*,#8525,.F.);
#12033=ORIENTED_EDGE('',*,*,#8650,.T.);
#12034=ORIENTED_EDGE('',*,*,#8471,.T.);
#12035=ORIENTED_EDGE('',*,*,#8651,.T.);
#12036=ORIENTED_EDGE('',*,*,#8652,.T.);
#12037=ORIENTED_EDGE('',*,*,#8467,.F.);
#12038=ORIENTED_EDGE('',*,*,#8653,.T.);
#12039=ORIENTED_EDGE('',*,*,#8412,.T.);
#12040=ORIENTED_EDGE('',*,*,#8654,.T.);
#12041=ORIENTED_EDGE('',*,*,#8655,.T.);
#12042=ORIENTED_EDGE('',*,*,#8407,.F.);
#12043=ORIENTED_EDGE('',*,*,#8656,.F.);
#12044=ORIENTED_EDGE('',*,*,#8657,.F.);
#12045=ORIENTED_EDGE('',*,*,#8341,.T.);
#12046=ORIENTED_EDGE('',*,*,#8658,.T.);
#12047=ORIENTED_EDGE('',*,*,#8659,.T.);
#12048=ORIENTED_EDGE('',*,*,#8336,.F.);
#12049=ORIENTED_EDGE('',*,*,#8660,.F.);
#12050=ORIENTED_EDGE('',*,*,#8661,.F.);
#12051=ORIENTED_EDGE('',*,*,#8270,.T.);
#12052=ORIENTED_EDGE('',*,*,#8662,.T.);
#12053=ORIENTED_EDGE('',*,*,#8663,.T.);
#12054=ORIENTED_EDGE('',*,*,#8265,.F.);
#12055=ORIENTED_EDGE('',*,*,#8664,.F.);
#12056=ORIENTED_EDGE('',*,*,#8665,.F.);
#12057=ORIENTED_EDGE('',*,*,#8199,.T.);
#12058=ORIENTED_EDGE('',*,*,#8666,.T.);
#12059=ORIENTED_EDGE('',*,*,#8667,.T.);
#12060=ORIENTED_EDGE('',*,*,#8194,.F.);
#12061=ORIENTED_EDGE('',*,*,#8668,.F.);
#12062=ORIENTED_EDGE('',*,*,#8669,.F.);
#12063=ORIENTED_EDGE('',*,*,#8130,.T.);
#12064=ORIENTED_EDGE('',*,*,#8670,.T.);
#12065=ORIENTED_EDGE('',*,*,#8671,.T.);
#12066=ORIENTED_EDGE('',*,*,#8127,.F.);
#12067=ORIENTED_EDGE('',*,*,#8672,.T.);
#12068=ORIENTED_EDGE('',*,*,#8065,.T.);
#12069=ORIENTED_EDGE('',*,*,#8673,.T.);
#12070=ORIENTED_EDGE('',*,*,#8674,.T.);
#12071=ORIENTED_EDGE('',*,*,#8060,.F.);
#12072=ORIENTED_EDGE('',*,*,#8675,.F.);
#12073=ORIENTED_EDGE('',*,*,#8676,.F.);
#12074=ORIENTED_EDGE('',*,*,#7987,.T.);
#12075=ORIENTED_EDGE('',*,*,#8677,.T.);
#12076=ORIENTED_EDGE('',*,*,#8678,.T.);
#12077=ORIENTED_EDGE('',*,*,#7984,.F.);
#12078=ORIENTED_EDGE('',*,*,#8679,.T.);
#12079=ORIENTED_EDGE('',*,*,#7922,.T.);
#12080=ORIENTED_EDGE('',*,*,#8680,.T.);
#12081=ORIENTED_EDGE('',*,*,#8681,.T.);
#12082=ORIENTED_EDGE('',*,*,#7917,.F.);
#12083=ORIENTED_EDGE('',*,*,#8682,.F.);
#12084=ORIENTED_EDGE('',*,*,#8683,.F.);
#12085=ORIENTED_EDGE('',*,*,#7930,.F.);
#12086=ORIENTED_EDGE('',*,*,#8684,.T.);
#12087=ORIENTED_EDGE('',*,*,#7850,.T.);
#12088=ORIENTED_EDGE('',*,*,#8685,.T.);
#12089=ORIENTED_EDGE('',*,*,#8685,.F.);
#12090=ORIENTED_EDGE('',*,*,#7849,.F.);
#12091=ORIENTED_EDGE('',*,*,#7854,.F.);
#12092=ORIENTED_EDGE('',*,*,#7853,.F.);
#12093=ORIENTED_EDGE('',*,*,#7859,.F.);
#12094=ORIENTED_EDGE('',*,*,#7858,.F.);
#12095=ORIENTED_EDGE('',*,*,#7864,.F.);
#12096=ORIENTED_EDGE('',*,*,#7863,.F.);
#12097=ORIENTED_EDGE('',*,*,#7869,.F.);
#12098=ORIENTED_EDGE('',*,*,#7868,.F.);
#12099=ORIENTED_EDGE('',*,*,#7874,.F.);
#12100=ORIENTED_EDGE('',*,*,#7873,.F.);
#12101=ORIENTED_EDGE('',*,*,#7879,.F.);
#12102=ORIENTED_EDGE('',*,*,#7878,.F.);
#12103=ORIENTED_EDGE('',*,*,#7884,.F.);
#12104=ORIENTED_EDGE('',*,*,#7883,.F.);
#12105=ORIENTED_EDGE('',*,*,#7889,.F.);
#12106=ORIENTED_EDGE('',*,*,#7888,.F.);
#12107=ORIENTED_EDGE('',*,*,#7894,.F.);
#12108=ORIENTED_EDGE('',*,*,#7893,.F.);
#12109=ORIENTED_EDGE('',*,*,#7899,.F.);
#12110=ORIENTED_EDGE('',*,*,#7898,.F.);
#12111=ORIENTED_EDGE('',*,*,#7904,.F.);
#12112=ORIENTED_EDGE('',*,*,#7903,.F.);
#12113=ORIENTED_EDGE('',*,*,#7909,.F.);
#12114=ORIENTED_EDGE('',*,*,#7908,.F.);
#12115=ORIENTED_EDGE('',*,*,#7914,.F.);
#12116=ORIENTED_EDGE('',*,*,#7913,.F.);
#12117=ORIENTED_EDGE('',*,*,#7919,.F.);
#12118=ORIENTED_EDGE('',*,*,#7918,.F.);
#12119=ORIENTED_EDGE('',*,*,#8681,.F.);
#12120=ORIENTED_EDGE('',*,*,#8680,.F.);
#12121=ORIENTED_EDGE('',*,*,#7927,.F.);
#12122=ORIENTED_EDGE('',*,*,#7926,.F.);
#12123=ORIENTED_EDGE('',*,*,#8686,.F.);
#12124=ORIENTED_EDGE('',*,*,#7988,.F.);
#12125=ORIENTED_EDGE('',*,*,#8679,.F.);
#12126=ORIENTED_EDGE('',*,*,#7986,.F.);
#12127=ORIENTED_EDGE('',*,*,#7983,.F.);
#12128=ORIENTED_EDGE('',*,*,#7982,.F.);
#12129=ORIENTED_EDGE('',*,*,#7978,.F.);
#12130=ORIENTED_EDGE('',*,*,#7975,.F.);
#12131=ORIENTED_EDGE('',*,*,#7974,.F.);
#12132=ORIENTED_EDGE('',*,*,#7970,.F.);
#12133=ORIENTED_EDGE('',*,*,#7967,.F.);
#12134=ORIENTED_EDGE('',*,*,#7966,.F.);
#12135=ORIENTED_EDGE('',*,*,#7962,.F.);
#12136=ORIENTED_EDGE('',*,*,#7959,.F.);
#12137=ORIENTED_EDGE('',*,*,#7958,.F.);
#12138=ORIENTED_EDGE('',*,*,#7954,.F.);
#12139=ORIENTED_EDGE('',*,*,#7951,.F.);
#12140=ORIENTED_EDGE('',*,*,#7950,.F.);
#12141=ORIENTED_EDGE('',*,*,#7946,.F.);
#12142=ORIENTED_EDGE('',*,*,#7943,.F.);
#12143=ORIENTED_EDGE('',*,*,#7942,.F.);
#12144=ORIENTED_EDGE('',*,*,#7938,.F.);
#12145=ORIENTED_EDGE('',*,*,#7937,.F.);
#12146=ORIENTED_EDGE('',*,*,#7934,.F.);
#12147=ORIENTED_EDGE('',*,*,#7931,.F.);
#12148=ORIENTED_EDGE('',*,*,#8684,.F.);
#12149=ORIENTED_EDGE('',*,*,#7929,.F.);
#12150=ORIENTED_EDGE('',*,*,#7936,.F.);
#12151=ORIENTED_EDGE('',*,*,#7941,.F.);
#12152=ORIENTED_EDGE('',*,*,#7940,.F.);
#12153=ORIENTED_EDGE('',*,*,#7945,.F.);
#12154=ORIENTED_EDGE('',*,*,#7949,.F.);
#12155=ORIENTED_EDGE('',*,*,#7948,.F.);
#12156=ORIENTED_EDGE('',*,*,#7953,.F.);
#12157=ORIENTED_EDGE('',*,*,#7957,.F.);
#12158=ORIENTED_EDGE('',*,*,#7956,.F.);
#12159=ORIENTED_EDGE('',*,*,#7961,.F.);
#12160=ORIENTED_EDGE('',*,*,#7965,.F.);
#12161=ORIENTED_EDGE('',*,*,#7964,.F.);
#12162=ORIENTED_EDGE('',*,*,#7969,.F.);
#12163=ORIENTED_EDGE('',*,*,#7973,.F.);
#12164=ORIENTED_EDGE('',*,*,#7972,.F.);
#12165=ORIENTED_EDGE('',*,*,#7977,.F.);
#12166=ORIENTED_EDGE('',*,*,#7981,.F.);
#12167=ORIENTED_EDGE('',*,*,#7980,.F.);
#12168=ORIENTED_EDGE('',*,*,#7985,.F.);
#12169=ORIENTED_EDGE('',*,*,#8678,.F.);
#12170=ORIENTED_EDGE('',*,*,#8677,.F.);
#12171=ORIENTED_EDGE('',*,*,#7990,.F.);
#12172=ORIENTED_EDGE('',*,*,#8687,.F.);
#12173=ORIENTED_EDGE('',*,*,#8688,.F.);
#12174=ORIENTED_EDGE('',*,*,#7924,.T.);
#12175=ORIENTED_EDGE('',*,*,#7923,.T.);
#12176=ORIENTED_EDGE('',*,*,#8683,.T.);
#12177=ORIENTED_EDGE('',*,*,#8682,.T.);
#12178=ORIENTED_EDGE('',*,*,#7921,.T.);
#12179=ORIENTED_EDGE('',*,*,#7920,.T.);
#12180=ORIENTED_EDGE('',*,*,#7916,.T.);
#12181=ORIENTED_EDGE('',*,*,#7915,.T.);
#12182=ORIENTED_EDGE('',*,*,#7911,.T.);
#12183=ORIENTED_EDGE('',*,*,#7910,.T.);
#12184=ORIENTED_EDGE('',*,*,#7906,.T.);
#12185=ORIENTED_EDGE('',*,*,#7905,.T.);
#12186=ORIENTED_EDGE('',*,*,#7901,.T.);
#12187=ORIENTED_EDGE('',*,*,#7900,.T.);
#12188=ORIENTED_EDGE('',*,*,#7896,.T.);
#12189=ORIENTED_EDGE('',*,*,#7895,.T.);
#12190=ORIENTED_EDGE('',*,*,#7891,.T.);
#12191=ORIENTED_EDGE('',*,*,#7890,.T.);
#12192=ORIENTED_EDGE('',*,*,#7886,.T.);
#12193=ORIENTED_EDGE('',*,*,#7885,.T.);
#12194=ORIENTED_EDGE('',*,*,#7881,.T.);
#12195=ORIENTED_EDGE('',*,*,#7880,.T.);
#12196=ORIENTED_EDGE('',*,*,#7876,.T.);
#12197=ORIENTED_EDGE('',*,*,#7875,.T.);
#12198=ORIENTED_EDGE('',*,*,#7871,.T.);
#12199=ORIENTED_EDGE('',*,*,#7870,.T.);
#12200=ORIENTED_EDGE('',*,*,#7866,.T.);
#12201=ORIENTED_EDGE('',*,*,#7865,.T.);
#12202=ORIENTED_EDGE('',*,*,#7861,.T.);
#12203=ORIENTED_EDGE('',*,*,#7860,.T.);
#12204=ORIENTED_EDGE('',*,*,#7856,.T.);
#12205=ORIENTED_EDGE('',*,*,#7855,.T.);
#12206=ORIENTED_EDGE('',*,*,#7851,.T.);
#12207=ORIENTED_EDGE('',*,*,#8073,.F.);
#12208=ORIENTED_EDGE('',*,*,#8689,.T.);
#12209=ORIENTED_EDGE('',*,*,#7993,.T.);
#12210=ORIENTED_EDGE('',*,*,#8690,.T.);
#12211=ORIENTED_EDGE('',*,*,#8690,.F.);
#12212=ORIENTED_EDGE('',*,*,#7992,.F.);
#12213=ORIENTED_EDGE('',*,*,#7997,.F.);
#12214=ORIENTED_EDGE('',*,*,#7996,.F.);
#12215=ORIENTED_EDGE('',*,*,#8002,.F.);
#12216=ORIENTED_EDGE('',*,*,#8001,.F.);
#12217=ORIENTED_EDGE('',*,*,#8007,.F.);
#12218=ORIENTED_EDGE('',*,*,#8006,.F.);
#12219=ORIENTED_EDGE('',*,*,#8012,.F.);
#12220=ORIENTED_EDGE('',*,*,#8011,.F.);
#12221=ORIENTED_EDGE('',*,*,#8017,.F.);
#12222=ORIENTED_EDGE('',*,*,#8016,.F.);
#12223=ORIENTED_EDGE('',*,*,#8022,.F.);
#12224=ORIENTED_EDGE('',*,*,#8021,.F.);
#12225=ORIENTED_EDGE('',*,*,#8027,.F.);
#12226=ORIENTED_EDGE('',*,*,#8026,.F.);
#12227=ORIENTED_EDGE('',*,*,#8032,.F.);
#12228=ORIENTED_EDGE('',*,*,#8031,.F.);
#12229=ORIENTED_EDGE('',*,*,#8037,.F.);
#12230=ORIENTED_EDGE('',*,*,#8036,.F.);
#12231=ORIENTED_EDGE('',*,*,#8042,.F.);
#12232=ORIENTED_EDGE('',*,*,#8041,.F.);
#12233=ORIENTED_EDGE('',*,*,#8047,.F.);
#12234=ORIENTED_EDGE('',*,*,#8046,.F.);
#12235=ORIENTED_EDGE('',*,*,#8052,.F.);
#12236=ORIENTED_EDGE('',*,*,#8051,.F.);
#12237=ORIENTED_EDGE('',*,*,#8057,.F.);
#12238=ORIENTED_EDGE('',*,*,#8056,.F.);
#12239=ORIENTED_EDGE('',*,*,#8062,.F.);
#12240=ORIENTED_EDGE('',*,*,#8061,.F.);
#12241=ORIENTED_EDGE('',*,*,#8674,.F.);
#12242=ORIENTED_EDGE('',*,*,#8673,.F.);
#12243=ORIENTED_EDGE('',*,*,#8070,.F.);
#12244=ORIENTED_EDGE('',*,*,#8069,.F.);
#12245=ORIENTED_EDGE('',*,*,#8691,.F.);
#12246=ORIENTED_EDGE('',*,*,#8131,.F.);
#12247=ORIENTED_EDGE('',*,*,#8672,.F.);
#12248=ORIENTED_EDGE('',*,*,#8129,.F.);
#12249=ORIENTED_EDGE('',*,*,#8126,.F.);
#12250=ORIENTED_EDGE('',*,*,#8125,.F.);
#12251=ORIENTED_EDGE('',*,*,#8121,.F.);
#12252=ORIENTED_EDGE('',*,*,#8118,.F.);
#12253=ORIENTED_EDGE('',*,*,#8117,.F.);
#12254=ORIENTED_EDGE('',*,*,#8113,.F.);
#12255=ORIENTED_EDGE('',*,*,#8110,.F.);
#12256=ORIENTED_EDGE('',*,*,#8109,.F.);
#12257=ORIENTED_EDGE('',*,*,#8105,.F.);
#12258=ORIENTED_EDGE('',*,*,#8102,.F.);
#12259=ORIENTED_EDGE('',*,*,#8101,.F.);
#12260=ORIENTED_EDGE('',*,*,#8097,.F.);
#12261=ORIENTED_EDGE('',*,*,#8094,.F.);
#12262=ORIENTED_EDGE('',*,*,#8093,.F.);
#12263=ORIENTED_EDGE('',*,*,#8089,.F.);
#12264=ORIENTED_EDGE('',*,*,#8086,.F.);
#12265=ORIENTED_EDGE('',*,*,#8085,.F.);
#12266=ORIENTED_EDGE('',*,*,#8081,.F.);
#12267=ORIENTED_EDGE('',*,*,#8080,.F.);
#12268=ORIENTED_EDGE('',*,*,#8077,.F.);
#12269=ORIENTED_EDGE('',*,*,#8074,.F.);
#12270=ORIENTED_EDGE('',*,*,#8689,.F.);
#12271=ORIENTED_EDGE('',*,*,#8072,.F.);
#12272=ORIENTED_EDGE('',*,*,#8079,.F.);
#12273=ORIENTED_EDGE('',*,*,#8084,.F.);
#12274=ORIENTED_EDGE('',*,*,#8083,.F.);
#12275=ORIENTED_EDGE('',*,*,#8088,.F.);
#12276=ORIENTED_EDGE('',*,*,#8092,.F.);
#12277=ORIENTED_EDGE('',*,*,#8091,.F.);
#12278=ORIENTED_EDGE('',*,*,#8096,.F.);
#12279=ORIENTED_EDGE('',*,*,#8100,.F.);
#12280=ORIENTED_EDGE('',*,*,#8099,.F.);
#12281=ORIENTED_EDGE('',*,*,#8104,.F.);
#12282=ORIENTED_EDGE('',*,*,#8108,.F.);
#12283=ORIENTED_EDGE('',*,*,#8107,.F.);
#12284=ORIENTED_EDGE('',*,*,#8112,.F.);
#12285=ORIENTED_EDGE('',*,*,#8116,.F.);
#12286=ORIENTED_EDGE('',*,*,#8115,.F.);
#12287=ORIENTED_EDGE('',*,*,#8120,.F.);
#12288=ORIENTED_EDGE('',*,*,#8124,.F.);
#12289=ORIENTED_EDGE('',*,*,#8123,.F.);
#12290=ORIENTED_EDGE('',*,*,#8128,.F.);
#12291=ORIENTED_EDGE('',*,*,#8671,.F.);
#12292=ORIENTED_EDGE('',*,*,#8670,.F.);
#12293=ORIENTED_EDGE('',*,*,#8133,.F.);
#12294=ORIENTED_EDGE('',*,*,#8692,.F.);
#12295=ORIENTED_EDGE('',*,*,#8693,.F.);
#12296=ORIENTED_EDGE('',*,*,#8067,.T.);
#12297=ORIENTED_EDGE('',*,*,#8066,.T.);
#12298=ORIENTED_EDGE('',*,*,#8676,.T.);
#12299=ORIENTED_EDGE('',*,*,#8675,.T.);
#12300=ORIENTED_EDGE('',*,*,#8064,.T.);
#12301=ORIENTED_EDGE('',*,*,#8063,.T.);
#12302=ORIENTED_EDGE('',*,*,#8059,.T.);
#12303=ORIENTED_EDGE('',*,*,#8058,.T.);
#12304=ORIENTED_EDGE('',*,*,#8054,.T.);
#12305=ORIENTED_EDGE('',*,*,#8053,.T.);
#12306=ORIENTED_EDGE('',*,*,#8049,.T.);
#12307=ORIENTED_EDGE('',*,*,#8048,.T.);
#12308=ORIENTED_EDGE('',*,*,#8044,.T.);
#12309=ORIENTED_EDGE('',*,*,#8043,.T.);
#12310=ORIENTED_EDGE('',*,*,#8039,.T.);
#12311=ORIENTED_EDGE('',*,*,#8038,.T.);
#12312=ORIENTED_EDGE('',*,*,#8034,.T.);
#12313=ORIENTED_EDGE('',*,*,#8033,.T.);
#12314=ORIENTED_EDGE('',*,*,#8029,.T.);
#12315=ORIENTED_EDGE('',*,*,#8028,.T.);
#12316=ORIENTED_EDGE('',*,*,#8024,.T.);
#12317=ORIENTED_EDGE('',*,*,#8023,.T.);
#12318=ORIENTED_EDGE('',*,*,#8019,.T.);
#12319=ORIENTED_EDGE('',*,*,#8018,.T.);
#12320=ORIENTED_EDGE('',*,*,#8014,.T.);
#12321=ORIENTED_EDGE('',*,*,#8013,.T.);
#12322=ORIENTED_EDGE('',*,*,#8009,.T.);
#12323=ORIENTED_EDGE('',*,*,#8008,.T.);
#12324=ORIENTED_EDGE('',*,*,#8004,.T.);
#12325=ORIENTED_EDGE('',*,*,#8003,.T.);
#12326=ORIENTED_EDGE('',*,*,#7999,.T.);
#12327=ORIENTED_EDGE('',*,*,#7998,.T.);
#12328=ORIENTED_EDGE('',*,*,#7994,.T.);
#12329=ORIENTED_EDGE('',*,*,#8076,.F.);
#12330=ORIENTED_EDGE('',*,*,#7933,.F.);
#12331=ORIENTED_EDGE('',*,*,#8694,.F.);
#12332=ORIENTED_EDGE('',*,*,#8695,.F.);
#12333=ORIENTED_EDGE('',*,*,#8696,.F.);
#12334=ORIENTED_EDGE('',*,*,#8697,.T.);
#12335=ORIENTED_EDGE('',*,*,#8698,.F.);
#12336=ORIENTED_EDGE('',*,*,#8697,.F.);
#12337=ORIENTED_EDGE('',*,*,#8699,.F.);
#12338=ORIENTED_EDGE('',*,*,#8700,.T.);
#12339=ORIENTED_EDGE('',*,*,#8701,.F.);
#12340=ORIENTED_EDGE('',*,*,#8700,.F.);
#12341=ORIENTED_EDGE('',*,*,#8702,.F.);
#12342=ORIENTED_EDGE('',*,*,#8703,.T.);
#12343=ORIENTED_EDGE('',*,*,#8704,.F.);
#12344=ORIENTED_EDGE('',*,*,#8703,.F.);
#12345=ORIENTED_EDGE('',*,*,#8705,.F.);
#12346=ORIENTED_EDGE('',*,*,#8695,.T.);
#12347=ORIENTED_EDGE('',*,*,#8706,.F.);
#12348=ORIENTED_EDGE('',*,*,#8707,.T.);
#12349=ORIENTED_EDGE('',*,*,#8708,.F.);
#12350=ORIENTED_EDGE('',*,*,#8707,.F.);
#12351=ORIENTED_EDGE('',*,*,#8709,.F.);
#12352=ORIENTED_EDGE('',*,*,#8710,.T.);
#12353=ORIENTED_EDGE('',*,*,#8711,.F.);
#12354=ORIENTED_EDGE('',*,*,#8710,.F.);
#12355=ORIENTED_EDGE('',*,*,#8712,.F.);
#12356=ORIENTED_EDGE('',*,*,#8713,.T.);
#12357=ORIENTED_EDGE('',*,*,#8714,.F.);
#12358=ORIENTED_EDGE('',*,*,#8713,.F.);
#12359=ORIENTED_EDGE('',*,*,#8715,.F.);
#12360=ORIENTED_EDGE('',*,*,#8716,.T.);
#12361=ORIENTED_EDGE('',*,*,#8717,.F.);
#12362=ORIENTED_EDGE('',*,*,#8716,.F.);
#12363=ORIENTED_EDGE('',*,*,#8718,.F.);
#12364=ORIENTED_EDGE('',*,*,#8135,.F.);
#12365=ORIENTED_EDGE('',*,*,#8141,.F.);
#12366=ORIENTED_EDGE('',*,*,#8140,.F.);
#12367=ORIENTED_EDGE('',*,*,#8146,.F.);
#12368=ORIENTED_EDGE('',*,*,#8145,.F.);
#12369=ORIENTED_EDGE('',*,*,#8151,.F.);
#12370=ORIENTED_EDGE('',*,*,#8150,.F.);
#12371=ORIENTED_EDGE('',*,*,#8156,.F.);
#12372=ORIENTED_EDGE('',*,*,#8155,.F.);
#12373=ORIENTED_EDGE('',*,*,#8161,.F.);
#12374=ORIENTED_EDGE('',*,*,#8160,.F.);
#12375=ORIENTED_EDGE('',*,*,#8166,.F.);
#12376=ORIENTED_EDGE('',*,*,#8165,.F.);
#12377=ORIENTED_EDGE('',*,*,#8171,.F.);
#12378=ORIENTED_EDGE('',*,*,#8170,.F.);
#12379=ORIENTED_EDGE('',*,*,#8176,.F.);
#12380=ORIENTED_EDGE('',*,*,#8175,.F.);
#12381=ORIENTED_EDGE('',*,*,#8181,.F.);
#12382=ORIENTED_EDGE('',*,*,#8180,.F.);
#12383=ORIENTED_EDGE('',*,*,#8186,.F.);
#12384=ORIENTED_EDGE('',*,*,#8185,.F.);
#12385=ORIENTED_EDGE('',*,*,#8191,.F.);
#12386=ORIENTED_EDGE('',*,*,#8190,.F.);
#12387=ORIENTED_EDGE('',*,*,#8196,.F.);
#12388=ORIENTED_EDGE('',*,*,#8195,.F.);
#12389=ORIENTED_EDGE('',*,*,#8667,.F.);
#12390=ORIENTED_EDGE('',*,*,#8666,.F.);
#12391=ORIENTED_EDGE('',*,*,#8204,.F.);
#12392=ORIENTED_EDGE('',*,*,#8203,.F.);
#12393=ORIENTED_EDGE('',*,*,#8719,.F.);
#12394=ORIENTED_EDGE('',*,*,#8531,.F.);
#12395=ORIENTED_EDGE('',*,*,#8530,.F.);
#12396=ORIENTED_EDGE('',*,*,#8650,.F.);
#12397=ORIENTED_EDGE('',*,*,#8528,.F.);
#12398=ORIENTED_EDGE('',*,*,#8527,.F.);
#12399=ORIENTED_EDGE('',*,*,#8524,.F.);
#12400=ORIENTED_EDGE('',*,*,#8520,.F.);
#12401=ORIENTED_EDGE('',*,*,#8519,.F.);
#12402=ORIENTED_EDGE('',*,*,#8516,.F.);
#12403=ORIENTED_EDGE('',*,*,#8512,.F.);
#12404=ORIENTED_EDGE('',*,*,#8511,.F.);
#12405=ORIENTED_EDGE('',*,*,#8508,.F.);
#12406=ORIENTED_EDGE('',*,*,#8507,.F.);
#12407=ORIENTED_EDGE('',*,*,#8503,.F.);
#12408=ORIENTED_EDGE('',*,*,#8502,.F.);
#12409=ORIENTED_EDGE('',*,*,#8499,.F.);
#12410=ORIENTED_EDGE('',*,*,#8495,.F.);
#12411=ORIENTED_EDGE('',*,*,#8494,.F.);
#12412=ORIENTED_EDGE('',*,*,#8491,.F.);
#12413=ORIENTED_EDGE('',*,*,#8487,.F.);
#12414=ORIENTED_EDGE('',*,*,#8486,.F.);
#12415=ORIENTED_EDGE('',*,*,#8483,.F.);
#12416=ORIENTED_EDGE('',*,*,#8479,.F.);
#12417=ORIENTED_EDGE('',*,*,#8720,.T.);
#12418=ORIENTED_EDGE('',*,*,#8721,.F.);
#12419=ORIENTED_EDGE('',*,*,#8477,.F.);
#12420=ORIENTED_EDGE('',*,*,#8482,.F.);
#12421=ORIENTED_EDGE('',*,*,#8481,.F.);
#12422=ORIENTED_EDGE('',*,*,#8485,.F.);
#12423=ORIENTED_EDGE('',*,*,#8490,.F.);
#12424=ORIENTED_EDGE('',*,*,#8489,.F.);
#12425=ORIENTED_EDGE('',*,*,#8493,.F.);
#12426=ORIENTED_EDGE('',*,*,#8498,.F.);
#12427=ORIENTED_EDGE('',*,*,#8497,.F.);
#12428=ORIENTED_EDGE('',*,*,#8501,.F.);
#12429=ORIENTED_EDGE('',*,*,#8506,.F.);
#12430=ORIENTED_EDGE('',*,*,#8505,.F.);
#12431=ORIENTED_EDGE('',*,*,#8510,.F.);
#12432=ORIENTED_EDGE('',*,*,#8515,.F.);
#12433=ORIENTED_EDGE('',*,*,#8514,.F.);
#12434=ORIENTED_EDGE('',*,*,#8518,.F.);
#12435=ORIENTED_EDGE('',*,*,#8523,.F.);
#12436=ORIENTED_EDGE('',*,*,#8522,.F.);
#12437=ORIENTED_EDGE('',*,*,#8526,.F.);
#12438=ORIENTED_EDGE('',*,*,#8649,.F.);
#12439=ORIENTED_EDGE('',*,*,#8648,.F.);
#12440=ORIENTED_EDGE('',*,*,#8533,.F.);
#12441=ORIENTED_EDGE('',*,*,#8722,.F.);
#12442=ORIENTED_EDGE('',*,*,#8723,.F.);
#12443=ORIENTED_EDGE('',*,*,#8201,.T.);
#12444=ORIENTED_EDGE('',*,*,#8200,.T.);
#12445=ORIENTED_EDGE('',*,*,#8669,.T.);
#12446=ORIENTED_EDGE('',*,*,#8668,.T.);
#12447=ORIENTED_EDGE('',*,*,#8198,.T.);
#12448=ORIENTED_EDGE('',*,*,#8197,.T.);
#12449=ORIENTED_EDGE('',*,*,#8193,.T.);
#12450=ORIENTED_EDGE('',*,*,#8192,.T.);
#12451=ORIENTED_EDGE('',*,*,#8188,.T.);
#12452=ORIENTED_EDGE('',*,*,#8187,.T.);
#12453=ORIENTED_EDGE('',*,*,#8183,.T.);
#12454=ORIENTED_EDGE('',*,*,#8182,.T.);
#12455=ORIENTED_EDGE('',*,*,#8178,.T.);
#12456=ORIENTED_EDGE('',*,*,#8177,.T.);
#12457=ORIENTED_EDGE('',*,*,#8173,.T.);
#12458=ORIENTED_EDGE('',*,*,#8172,.T.);
#12459=ORIENTED_EDGE('',*,*,#8168,.T.);
#12460=ORIENTED_EDGE('',*,*,#8167,.T.);
#12461=ORIENTED_EDGE('',*,*,#8163,.T.);
#12462=ORIENTED_EDGE('',*,*,#8162,.T.);
#12463=ORIENTED_EDGE('',*,*,#8158,.T.);
#12464=ORIENTED_EDGE('',*,*,#8157,.T.);
#12465=ORIENTED_EDGE('',*,*,#8153,.T.);
#12466=ORIENTED_EDGE('',*,*,#8152,.T.);
#12467=ORIENTED_EDGE('',*,*,#8148,.T.);
#12468=ORIENTED_EDGE('',*,*,#8147,.T.);
#12469=ORIENTED_EDGE('',*,*,#8143,.T.);
#12470=ORIENTED_EDGE('',*,*,#8142,.T.);
#12471=ORIENTED_EDGE('',*,*,#8138,.T.);
#12472=ORIENTED_EDGE('',*,*,#8137,.T.);
#12473=ORIENTED_EDGE('',*,*,#8724,.F.);
#12474=ORIENTED_EDGE('',*,*,#8206,.F.);
#12475=ORIENTED_EDGE('',*,*,#8212,.F.);
#12476=ORIENTED_EDGE('',*,*,#8211,.F.);
#12477=ORIENTED_EDGE('',*,*,#8217,.F.);
#12478=ORIENTED_EDGE('',*,*,#8216,.F.);
#12479=ORIENTED_EDGE('',*,*,#8222,.F.);
#12480=ORIENTED_EDGE('',*,*,#8221,.F.);
#12481=ORIENTED_EDGE('',*,*,#8227,.F.);
#12482=ORIENTED_EDGE('',*,*,#8226,.F.);
#12483=ORIENTED_EDGE('',*,*,#8232,.F.);
#12484=ORIENTED_EDGE('',*,*,#8231,.F.);
#12485=ORIENTED_EDGE('',*,*,#8237,.F.);
#12486=ORIENTED_EDGE('',*,*,#8236,.F.);
#12487=ORIENTED_EDGE('',*,*,#8242,.F.);
#12488=ORIENTED_EDGE('',*,*,#8241,.F.);
#12489=ORIENTED_EDGE('',*,*,#8247,.F.);
#12490=ORIENTED_EDGE('',*,*,#8246,.F.);
#12491=ORIENTED_EDGE('',*,*,#8252,.F.);
#12492=ORIENTED_EDGE('',*,*,#8251,.F.);
#12493=ORIENTED_EDGE('',*,*,#8257,.F.);
#12494=ORIENTED_EDGE('',*,*,#8256,.F.);
#12495=ORIENTED_EDGE('',*,*,#8262,.F.);
#12496=ORIENTED_EDGE('',*,*,#8261,.F.);
#12497=ORIENTED_EDGE('',*,*,#8267,.F.);
#12498=ORIENTED_EDGE('',*,*,#8266,.F.);
#12499=ORIENTED_EDGE('',*,*,#8663,.F.);
#12500=ORIENTED_EDGE('',*,*,#8662,.F.);
#12501=ORIENTED_EDGE('',*,*,#8275,.F.);
#12502=ORIENTED_EDGE('',*,*,#8274,.F.);
#12503=ORIENTED_EDGE('',*,*,#8725,.F.);
#12504=ORIENTED_EDGE('',*,*,#8473,.F.);
#12505=ORIENTED_EDGE('',*,*,#8472,.F.);
#12506=ORIENTED_EDGE('',*,*,#8653,.F.);
#12507=ORIENTED_EDGE('',*,*,#8470,.F.);
#12508=ORIENTED_EDGE('',*,*,#8469,.F.);
#12509=ORIENTED_EDGE('',*,*,#8466,.F.);
#12510=ORIENTED_EDGE('',*,*,#8462,.F.);
#12511=ORIENTED_EDGE('',*,*,#8461,.F.);
#12512=ORIENTED_EDGE('',*,*,#8458,.F.);
#12513=ORIENTED_EDGE('',*,*,#8454,.F.);
#12514=ORIENTED_EDGE('',*,*,#8453,.F.);
#12515=ORIENTED_EDGE('',*,*,#8450,.F.);
#12516=ORIENTED_EDGE('',*,*,#8449,.F.);
#12517=ORIENTED_EDGE('',*,*,#8445,.F.);
#12518=ORIENTED_EDGE('',*,*,#8444,.F.);
#12519=ORIENTED_EDGE('',*,*,#8441,.F.);
#12520=ORIENTED_EDGE('',*,*,#8437,.F.);
#12521=ORIENTED_EDGE('',*,*,#8436,.F.);
#12522=ORIENTED_EDGE('',*,*,#8433,.F.);
#12523=ORIENTED_EDGE('',*,*,#8429,.F.);
#12524=ORIENTED_EDGE('',*,*,#8428,.F.);
#12525=ORIENTED_EDGE('',*,*,#8425,.F.);
#12526=ORIENTED_EDGE('',*,*,#8421,.F.);
#12527=ORIENTED_EDGE('',*,*,#8726,.T.);
#12528=ORIENTED_EDGE('',*,*,#8727,.F.);
#12529=ORIENTED_EDGE('',*,*,#8419,.F.);
#12530=ORIENTED_EDGE('',*,*,#8424,.F.);
#12531=ORIENTED_EDGE('',*,*,#8423,.F.);
#12532=ORIENTED_EDGE('',*,*,#8427,.F.);
#12533=ORIENTED_EDGE('',*,*,#8432,.F.);
#12534=ORIENTED_EDGE('',*,*,#8431,.F.);
#12535=ORIENTED_EDGE('',*,*,#8435,.F.);
#12536=ORIENTED_EDGE('',*,*,#8440,.F.);
#12537=ORIENTED_EDGE('',*,*,#8439,.F.);
#12538=ORIENTED_EDGE('',*,*,#8443,.F.);
#12539=ORIENTED_EDGE('',*,*,#8448,.F.);
#12540=ORIENTED_EDGE('',*,*,#8447,.F.);
#12541=ORIENTED_EDGE('',*,*,#8452,.F.);
#12542=ORIENTED_EDGE('',*,*,#8457,.F.);
#12543=ORIENTED_EDGE('',*,*,#8456,.F.);
#12544=ORIENTED_EDGE('',*,*,#8460,.F.);
#12545=ORIENTED_EDGE('',*,*,#8465,.F.);
#12546=ORIENTED_EDGE('',*,*,#8464,.F.);
#12547=ORIENTED_EDGE('',*,*,#8468,.F.);
#12548=ORIENTED_EDGE('',*,*,#8652,.F.);
#12549=ORIENTED_EDGE('',*,*,#8651,.F.);
#12550=ORIENTED_EDGE('',*,*,#8475,.F.);
#12551=ORIENTED_EDGE('',*,*,#8728,.F.);
#12552=ORIENTED_EDGE('',*,*,#8729,.F.);
#12553=ORIENTED_EDGE('',*,*,#8272,.T.);
#12554=ORIENTED_EDGE('',*,*,#8271,.T.);
#12555=ORIENTED_EDGE('',*,*,#8665,.T.);
#12556=ORIENTED_EDGE('',*,*,#8664,.T.);
#12557=ORIENTED_EDGE('',*,*,#8269,.T.);
#12558=ORIENTED_EDGE('',*,*,#8268,.T.);
#12559=ORIENTED_EDGE('',*,*,#8264,.T.);
#12560=ORIENTED_EDGE('',*,*,#8263,.T.);
#12561=ORIENTED_EDGE('',*,*,#8259,.T.);
#12562=ORIENTED_EDGE('',*,*,#8258,.T.);
#12563=ORIENTED_EDGE('',*,*,#8254,.T.);
#12564=ORIENTED_EDGE('',*,*,#8253,.T.);
#12565=ORIENTED_EDGE('',*,*,#8249,.T.);
#12566=ORIENTED_EDGE('',*,*,#8248,.T.);
#12567=ORIENTED_EDGE('',*,*,#8244,.T.);
#12568=ORIENTED_EDGE('',*,*,#8243,.T.);
#12569=ORIENTED_EDGE('',*,*,#8239,.T.);
#12570=ORIENTED_EDGE('',*,*,#8238,.T.);
#12571=ORIENTED_EDGE('',*,*,#8234,.T.);
#12572=ORIENTED_EDGE('',*,*,#8233,.T.);
#12573=ORIENTED_EDGE('',*,*,#8229,.T.);
#12574=ORIENTED_EDGE('',*,*,#8228,.T.);
#12575=ORIENTED_EDGE('',*,*,#8224,.T.);
#12576=ORIENTED_EDGE('',*,*,#8223,.T.);
#12577=ORIENTED_EDGE('',*,*,#8219,.T.);
#12578=ORIENTED_EDGE('',*,*,#8218,.T.);
#12579=ORIENTED_EDGE('',*,*,#8214,.T.);
#12580=ORIENTED_EDGE('',*,*,#8213,.T.);
#12581=ORIENTED_EDGE('',*,*,#8209,.T.);
#12582=ORIENTED_EDGE('',*,*,#8208,.T.);
#12583=ORIENTED_EDGE('',*,*,#8730,.F.);
#12584=ORIENTED_EDGE('',*,*,#8277,.F.);
#12585=ORIENTED_EDGE('',*,*,#8283,.F.);
#12586=ORIENTED_EDGE('',*,*,#8282,.F.);
#12587=ORIENTED_EDGE('',*,*,#8288,.F.);
#12588=ORIENTED_EDGE('',*,*,#8287,.F.);
#12589=ORIENTED_EDGE('',*,*,#8293,.F.);
#12590=ORIENTED_EDGE('',*,*,#8292,.F.);
#12591=ORIENTED_EDGE('',*,*,#8298,.F.);
#12592=ORIENTED_EDGE('',*,*,#8297,.F.);
#12593=ORIENTED_EDGE('',*,*,#8303,.F.);
#12594=ORIENTED_EDGE('',*,*,#8302,.F.);
#12595=ORIENTED_EDGE('',*,*,#8308,.F.);
#12596=ORIENTED_EDGE('',*,*,#8307,.F.);
#12597=ORIENTED_EDGE('',*,*,#8313,.F.);
#12598=ORIENTED_EDGE('',*,*,#8312,.F.);
#12599=ORIENTED_EDGE('',*,*,#8318,.F.);
#12600=ORIENTED_EDGE('',*,*,#8317,.F.);
#12601=ORIENTED_EDGE('',*,*,#8323,.F.);
#12602=ORIENTED_EDGE('',*,*,#8322,.F.);
#12603=ORIENTED_EDGE('',*,*,#8328,.F.);
#12604=ORIENTED_EDGE('',*,*,#8327,.F.);
#12605=ORIENTED_EDGE('',*,*,#8333,.F.);
#12606=ORIENTED_EDGE('',*,*,#8332,.F.);
#12607=ORIENTED_EDGE('',*,*,#8338,.F.);
#12608=ORIENTED_EDGE('',*,*,#8337,.F.);
#12609=ORIENTED_EDGE('',*,*,#8659,.F.);
#12610=ORIENTED_EDGE('',*,*,#8658,.F.);
#12611=ORIENTED_EDGE('',*,*,#8346,.F.);
#12612=ORIENTED_EDGE('',*,*,#8345,.F.);
#12613=ORIENTED_EDGE('',*,*,#8731,.F.);
#12614=ORIENTED_EDGE('',*,*,#8639,.F.);
#12615=ORIENTED_EDGE('',*,*,#8644,.F.);
#12616=ORIENTED_EDGE('',*,*,#8637,.F.);
#12617=ORIENTED_EDGE('',*,*,#8634,.F.);
#12618=ORIENTED_EDGE('',*,*,#8630,.F.);
#12619=ORIENTED_EDGE('',*,*,#8629,.F.);
#12620=ORIENTED_EDGE('',*,*,#8626,.F.);
#12621=ORIENTED_EDGE('',*,*,#8622,.F.);
#12622=ORIENTED_EDGE('',*,*,#8621,.F.);
#12623=ORIENTED_EDGE('',*,*,#8618,.F.);
#12624=ORIENTED_EDGE('',*,*,#8617,.F.);
#12625=ORIENTED_EDGE('',*,*,#8613,.F.);
#12626=ORIENTED_EDGE('',*,*,#8612,.F.);
#12627=ORIENTED_EDGE('',*,*,#8609,.F.);
#12628=ORIENTED_EDGE('',*,*,#8605,.F.);
#12629=ORIENTED_EDGE('',*,*,#8604,.F.);
#12630=ORIENTED_EDGE('',*,*,#8601,.F.);
#12631=ORIENTED_EDGE('',*,*,#8598,.F.);
#12632=ORIENTED_EDGE('',*,*,#8597,.F.);
#12633=ORIENTED_EDGE('',*,*,#8594,.F.);
#12634=ORIENTED_EDGE('',*,*,#8591,.F.);
#12635=ORIENTED_EDGE('',*,*,#8732,.T.);
#12636=ORIENTED_EDGE('',*,*,#8733,.F.);
#12637=ORIENTED_EDGE('',*,*,#8589,.F.);
#12638=ORIENTED_EDGE('',*,*,#8593,.F.);
#12639=ORIENTED_EDGE('',*,*,#8596,.F.);
#12640=ORIENTED_EDGE('',*,*,#8600,.F.);
#12641=ORIENTED_EDGE('',*,*,#8603,.F.);
#12642=ORIENTED_EDGE('',*,*,#8608,.F.);
#12643=ORIENTED_EDGE('',*,*,#8607,.F.);
#12644=ORIENTED_EDGE('',*,*,#8611,.F.);
#12645=ORIENTED_EDGE('',*,*,#8616,.F.);
#12646=ORIENTED_EDGE('',*,*,#8615,.F.);
#12647=ORIENTED_EDGE('',*,*,#8620,.F.);
#12648=ORIENTED_EDGE('',*,*,#8625,.F.);
#12649=ORIENTED_EDGE('',*,*,#8624,.F.);
#12650=ORIENTED_EDGE('',*,*,#8628,.F.);
#12651=ORIENTED_EDGE('',*,*,#8633,.F.);
#12652=ORIENTED_EDGE('',*,*,#8632,.F.);
#12653=ORIENTED_EDGE('',*,*,#8636,.F.);
#12654=ORIENTED_EDGE('',*,*,#8643,.F.);
#12655=ORIENTED_EDGE('',*,*,#8642,.F.);
#12656=ORIENTED_EDGE('',*,*,#8641,.F.);
#12657=ORIENTED_EDGE('',*,*,#8734,.F.);
#12658=ORIENTED_EDGE('',*,*,#8735,.F.);
#12659=ORIENTED_EDGE('',*,*,#8343,.T.);
#12660=ORIENTED_EDGE('',*,*,#8342,.T.);
#12661=ORIENTED_EDGE('',*,*,#8661,.T.);
#12662=ORIENTED_EDGE('',*,*,#8660,.T.);
#12663=ORIENTED_EDGE('',*,*,#8340,.T.);
#12664=ORIENTED_EDGE('',*,*,#8339,.T.);
#12665=ORIENTED_EDGE('',*,*,#8335,.T.);
#12666=ORIENTED_EDGE('',*,*,#8334,.T.);
#12667=ORIENTED_EDGE('',*,*,#8330,.T.);
#12668=ORIENTED_EDGE('',*,*,#8329,.T.);
#12669=ORIENTED_EDGE('',*,*,#8325,.T.);
#12670=ORIENTED_EDGE('',*,*,#8324,.T.);
#12671=ORIENTED_EDGE('',*,*,#8320,.T.);
#12672=ORIENTED_EDGE('',*,*,#8319,.T.);
#12673=ORIENTED_EDGE('',*,*,#8315,.T.);
#12674=ORIENTED_EDGE('',*,*,#8314,.T.);
#12675=ORIENTED_EDGE('',*,*,#8310,.T.);
#12676=ORIENTED_EDGE('',*,*,#8309,.T.);
#12677=ORIENTED_EDGE('',*,*,#8305,.T.);
#12678=ORIENTED_EDGE('',*,*,#8304,.T.);
#12679=ORIENTED_EDGE('',*,*,#8300,.T.);
#12680=ORIENTED_EDGE('',*,*,#8299,.T.);
#12681=ORIENTED_EDGE('',*,*,#8295,.T.);
#12682=ORIENTED_EDGE('',*,*,#8294,.T.);
#12683=ORIENTED_EDGE('',*,*,#8290,.T.);
#12684=ORIENTED_EDGE('',*,*,#8289,.T.);
#12685=ORIENTED_EDGE('',*,*,#8285,.T.);
#12686=ORIENTED_EDGE('',*,*,#8284,.T.);
#12687=ORIENTED_EDGE('',*,*,#8280,.T.);
#12688=ORIENTED_EDGE('',*,*,#8279,.T.);
#12689=ORIENTED_EDGE('',*,*,#8736,.F.);
#12690=ORIENTED_EDGE('',*,*,#8348,.F.);
#12691=ORIENTED_EDGE('',*,*,#8354,.F.);
#12692=ORIENTED_EDGE('',*,*,#8353,.F.);
#12693=ORIENTED_EDGE('',*,*,#8359,.F.);
#12694=ORIENTED_EDGE('',*,*,#8358,.F.);
#12695=ORIENTED_EDGE('',*,*,#8364,.F.);
#12696=ORIENTED_EDGE('',*,*,#8363,.F.);
#12697=ORIENTED_EDGE('',*,*,#8369,.F.);
#12698=ORIENTED_EDGE('',*,*,#8368,.F.);
#12699=ORIENTED_EDGE('',*,*,#8374,.F.);
#12700=ORIENTED_EDGE('',*,*,#8373,.F.);
#12701=ORIENTED_EDGE('',*,*,#8379,.F.);
#12702=ORIENTED_EDGE('',*,*,#8378,.F.);
#12703=ORIENTED_EDGE('',*,*,#8384,.F.);
#12704=ORIENTED_EDGE('',*,*,#8383,.F.);
#12705=ORIENTED_EDGE('',*,*,#8389,.F.);
#12706=ORIENTED_EDGE('',*,*,#8388,.F.);
#12707=ORIENTED_EDGE('',*,*,#8394,.F.);
#12708=ORIENTED_EDGE('',*,*,#8393,.F.);
#12709=ORIENTED_EDGE('',*,*,#8399,.F.);
#12710=ORIENTED_EDGE('',*,*,#8398,.F.);
#12711=ORIENTED_EDGE('',*,*,#8404,.F.);
#12712=ORIENTED_EDGE('',*,*,#8403,.F.);
#12713=ORIENTED_EDGE('',*,*,#8409,.F.);
#12714=ORIENTED_EDGE('',*,*,#8408,.F.);
#12715=ORIENTED_EDGE('',*,*,#8655,.F.);
#12716=ORIENTED_EDGE('',*,*,#8654,.F.);
#12717=ORIENTED_EDGE('',*,*,#8417,.F.);
#12718=ORIENTED_EDGE('',*,*,#8416,.F.);
#12719=ORIENTED_EDGE('',*,*,#8737,.F.);
#12720=ORIENTED_EDGE('',*,*,#8585,.F.);
#12721=ORIENTED_EDGE('',*,*,#8647,.F.);
#12722=ORIENTED_EDGE('',*,*,#8583,.F.);
#12723=ORIENTED_EDGE('',*,*,#8580,.F.);
#12724=ORIENTED_EDGE('',*,*,#8576,.F.);
#12725=ORIENTED_EDGE('',*,*,#8575,.F.);
#12726=ORIENTED_EDGE('',*,*,#8572,.F.);
#12727=ORIENTED_EDGE('',*,*,#8568,.F.);
#12728=ORIENTED_EDGE('',*,*,#8567,.F.);
#12729=ORIENTED_EDGE('',*,*,#8564,.F.);
#12730=ORIENTED_EDGE('',*,*,#8563,.F.);
#12731=ORIENTED_EDGE('',*,*,#8559,.F.);
#12732=ORIENTED_EDGE('',*,*,#8558,.F.);
#12733=ORIENTED_EDGE('',*,*,#8555,.F.);
#12734=ORIENTED_EDGE('',*,*,#8551,.F.);
#12735=ORIENTED_EDGE('',*,*,#8550,.F.);
#12736=ORIENTED_EDGE('',*,*,#8547,.F.);
#12737=ORIENTED_EDGE('',*,*,#8544,.F.);
#12738=ORIENTED_EDGE('',*,*,#8543,.F.);
#12739=ORIENTED_EDGE('',*,*,#8540,.F.);
#12740=ORIENTED_EDGE('',*,*,#8537,.F.);
#12741=ORIENTED_EDGE('',*,*,#8738,.T.);
#12742=ORIENTED_EDGE('',*,*,#8739,.F.);
#12743=ORIENTED_EDGE('',*,*,#8535,.F.);
#12744=ORIENTED_EDGE('',*,*,#8539,.F.);
#12745=ORIENTED_EDGE('',*,*,#8542,.F.);
#12746=ORIENTED_EDGE('',*,*,#8546,.F.);
#12747=ORIENTED_EDGE('',*,*,#8549,.F.);
#12748=ORIENTED_EDGE('',*,*,#8554,.F.);
#12749=ORIENTED_EDGE('',*,*,#8553,.F.);
#12750=ORIENTED_EDGE('',*,*,#8557,.F.);
#12751=ORIENTED_EDGE('',*,*,#8562,.F.);
#12752=ORIENTED_EDGE('',*,*,#8561,.F.);
#12753=ORIENTED_EDGE('',*,*,#8566,.F.);
#12754=ORIENTED_EDGE('',*,*,#8571,.F.);
#12755=ORIENTED_EDGE('',*,*,#8570,.F.);
#12756=ORIENTED_EDGE('',*,*,#8574,.F.);
#12757=ORIENTED_EDGE('',*,*,#8579,.F.);
#12758=ORIENTED_EDGE('',*,*,#8578,.F.);
#12759=ORIENTED_EDGE('',*,*,#8582,.F.);
#12760=ORIENTED_EDGE('',*,*,#8646,.F.);
#12761=ORIENTED_EDGE('',*,*,#8645,.F.);
#12762=ORIENTED_EDGE('',*,*,#8587,.F.);
#12763=ORIENTED_EDGE('',*,*,#8740,.F.);
#12764=ORIENTED_EDGE('',*,*,#8741,.F.);
#12765=ORIENTED_EDGE('',*,*,#8414,.T.);
#12766=ORIENTED_EDGE('',*,*,#8413,.T.);
#12767=ORIENTED_EDGE('',*,*,#8657,.T.);
#12768=ORIENTED_EDGE('',*,*,#8656,.T.);
#12769=ORIENTED_EDGE('',*,*,#8411,.T.);
#12770=ORIENTED_EDGE('',*,*,#8410,.T.);
#12771=ORIENTED_EDGE('',*,*,#8406,.T.);
#12772=ORIENTED_EDGE('',*,*,#8405,.T.);
#12773=ORIENTED_EDGE('',*,*,#8401,.T.);
#12774=ORIENTED_EDGE('',*,*,#8400,.T.);
#12775=ORIENTED_EDGE('',*,*,#8396,.T.);
#12776=ORIENTED_EDGE('',*,*,#8395,.T.);
#12777=ORIENTED_EDGE('',*,*,#8391,.T.);
#12778=ORIENTED_EDGE('',*,*,#8390,.T.);
#12779=ORIENTED_EDGE('',*,*,#8386,.T.);
#12780=ORIENTED_EDGE('',*,*,#8385,.T.);
#12781=ORIENTED_EDGE('',*,*,#8381,.T.);
#12782=ORIENTED_EDGE('',*,*,#8380,.T.);
#12783=ORIENTED_EDGE('',*,*,#8376,.T.);
#12784=ORIENTED_EDGE('',*,*,#8375,.T.);
#12785=ORIENTED_EDGE('',*,*,#8371,.T.);
#12786=ORIENTED_EDGE('',*,*,#8370,.T.);
#12787=ORIENTED_EDGE('',*,*,#8366,.T.);
#12788=ORIENTED_EDGE('',*,*,#8365,.T.);
#12789=ORIENTED_EDGE('',*,*,#8361,.T.);
#12790=ORIENTED_EDGE('',*,*,#8360,.T.);
#12791=ORIENTED_EDGE('',*,*,#8356,.T.);
#12792=ORIENTED_EDGE('',*,*,#8355,.T.);
#12793=ORIENTED_EDGE('',*,*,#8351,.T.);
#12794=ORIENTED_EDGE('',*,*,#8350,.T.);
#12795=ORIENTED_EDGE('',*,*,#8727,.T.);
#12796=ORIENTED_EDGE('',*,*,#8207,.T.);
#12797=ORIENTED_EDGE('',*,*,#8724,.T.);
#12798=ORIENTED_EDGE('',*,*,#8726,.F.);
#12799=ORIENTED_EDGE('',*,*,#8420,.F.);
#12800=ORIENTED_EDGE('',*,*,#8721,.T.);
#12801=ORIENTED_EDGE('',*,*,#8136,.T.);
#12802=ORIENTED_EDGE('',*,*,#8718,.T.);
#12803=ORIENTED_EDGE('',*,*,#8720,.F.);
#12804=ORIENTED_EDGE('',*,*,#8478,.F.);
#12805=ORIENTED_EDGE('',*,*,#8739,.T.);
#12806=ORIENTED_EDGE('',*,*,#8349,.T.);
#12807=ORIENTED_EDGE('',*,*,#8736,.T.);
#12808=ORIENTED_EDGE('',*,*,#8738,.F.);
#12809=ORIENTED_EDGE('',*,*,#8536,.F.);
#12810=ORIENTED_EDGE('',*,*,#8733,.T.);
#12811=ORIENTED_EDGE('',*,*,#8278,.T.);
#12812=ORIENTED_EDGE('',*,*,#8730,.T.);
#12813=ORIENTED_EDGE('',*,*,#8732,.F.);
#12814=ORIENTED_EDGE('',*,*,#8590,.F.);
#12815=ORIENTED_EDGE('',*,*,#8742,.F.);
#12816=ORIENTED_EDGE('',*,*,#8743,.T.);
#12817=ORIENTED_EDGE('',*,*,#8744,.F.);
#12818=ORIENTED_EDGE('',*,*,#8743,.F.);
#12819=ORIENTED_EDGE('',*,*,#8701,.T.);
#12820=ORIENTED_EDGE('',*,*,#8704,.T.);
#12821=ORIENTED_EDGE('',*,*,#8694,.T.);
#12822=ORIENTED_EDGE('',*,*,#8698,.T.);
#12823=ORIENTED_EDGE('',*,*,#8745,.T.);
#12824=ORIENTED_EDGE('',*,*,#8746,.T.);
#12825=ORIENTED_EDGE('',*,*,#8747,.T.);
#12826=ORIENTED_EDGE('',*,*,#8748,.T.);
#12827=ORIENTED_EDGE('',*,*,#8749,.F.);
#12828=ORIENTED_EDGE('',*,*,#8750,.F.);
#12829=ORIENTED_EDGE('',*,*,#8751,.F.);
#12830=ORIENTED_EDGE('',*,*,#8752,.F.);
#12831=ORIENTED_EDGE('',*,*,#8715,.T.);
#12832=ORIENTED_EDGE('',*,*,#8712,.T.);
#12833=ORIENTED_EDGE('',*,*,#8709,.T.);
#12834=ORIENTED_EDGE('',*,*,#8706,.T.);
#12835=ORIENTED_EDGE('',*,*,#8753,.T.);
#12836=ORIENTED_EDGE('',*,*,#8754,.T.);
#12837=ORIENTED_EDGE('',*,*,#8748,.F.);
#12838=ORIENTED_EDGE('',*,*,#8755,.F.);
#12839=ORIENTED_EDGE('',*,*,#8756,.T.);
#12840=ORIENTED_EDGE('',*,*,#8755,.T.);
#12841=ORIENTED_EDGE('',*,*,#8747,.F.);
#12842=ORIENTED_EDGE('',*,*,#8757,.F.);
#12843=ORIENTED_EDGE('',*,*,#8758,.T.);
#12844=ORIENTED_EDGE('',*,*,#8757,.T.);
#12845=ORIENTED_EDGE('',*,*,#8746,.F.);
#12846=ORIENTED_EDGE('',*,*,#8759,.F.);
#12847=ORIENTED_EDGE('',*,*,#8760,.T.);
#12848=ORIENTED_EDGE('',*,*,#8759,.T.);
#12849=ORIENTED_EDGE('',*,*,#8745,.F.);
#12850=ORIENTED_EDGE('',*,*,#8754,.F.);
#12851=ORIENTED_EDGE('',*,*,#8760,.F.);
#12852=ORIENTED_EDGE('',*,*,#8753,.F.);
#12853=ORIENTED_EDGE('',*,*,#8756,.F.);
#12854=ORIENTED_EDGE('',*,*,#8758,.F.);
#12855=ORIENTED_EDGE('',*,*,#8708,.T.);
#12856=ORIENTED_EDGE('',*,*,#8711,.T.);
#12857=ORIENTED_EDGE('',*,*,#8714,.T.);
#12858=ORIENTED_EDGE('',*,*,#8717,.T.);
#12859=ORIENTED_EDGE('',*,*,#8749,.T.);
#12860=ORIENTED_EDGE('',*,*,#8761,.T.);
#12861=ORIENTED_EDGE('',*,*,#8762,.F.);
#12862=ORIENTED_EDGE('',*,*,#8763,.F.);
#12863=ORIENTED_EDGE('',*,*,#8750,.T.);
#12864=ORIENTED_EDGE('',*,*,#8763,.T.);
#12865=ORIENTED_EDGE('',*,*,#8764,.F.);
#12866=ORIENTED_EDGE('',*,*,#8765,.F.);
#12867=ORIENTED_EDGE('',*,*,#8742,.T.);
#12868=ORIENTED_EDGE('',*,*,#8751,.T.);
#12869=ORIENTED_EDGE('',*,*,#8765,.T.);
#12870=ORIENTED_EDGE('',*,*,#8766,.F.);
#12871=ORIENTED_EDGE('',*,*,#8767,.F.);
#12872=ORIENTED_EDGE('',*,*,#8752,.T.);
#12873=ORIENTED_EDGE('',*,*,#8767,.T.);
#12874=ORIENTED_EDGE('',*,*,#8768,.F.);
#12875=ORIENTED_EDGE('',*,*,#8761,.F.);
#12876=ORIENTED_EDGE('',*,*,#8723,.T.);
#12877=ORIENTED_EDGE('',*,*,#8722,.T.);
#12878=ORIENTED_EDGE('',*,*,#8532,.T.);
#12879=ORIENTED_EDGE('',*,*,#8719,.T.);
#12880=ORIENTED_EDGE('',*,*,#8202,.T.);
#12881=ORIENTED_EDGE('',*,*,#8729,.T.);
#12882=ORIENTED_EDGE('',*,*,#8728,.T.);
#12883=ORIENTED_EDGE('',*,*,#8474,.T.);
#12884=ORIENTED_EDGE('',*,*,#8725,.T.);
#12885=ORIENTED_EDGE('',*,*,#8273,.T.);
#12886=ORIENTED_EDGE('',*,*,#8735,.T.);
#12887=ORIENTED_EDGE('',*,*,#8734,.T.);
#12888=ORIENTED_EDGE('',*,*,#8640,.T.);
#12889=ORIENTED_EDGE('',*,*,#8731,.T.);
#12890=ORIENTED_EDGE('',*,*,#8344,.T.);
#12891=ORIENTED_EDGE('',*,*,#8741,.T.);
#12892=ORIENTED_EDGE('',*,*,#8740,.T.);
#12893=ORIENTED_EDGE('',*,*,#8586,.T.);
#12894=ORIENTED_EDGE('',*,*,#8737,.T.);
#12895=ORIENTED_EDGE('',*,*,#8415,.T.);
#12896=ORIENTED_EDGE('',*,*,#8744,.T.);
#12897=ORIENTED_EDGE('',*,*,#8768,.T.);
#12898=ORIENTED_EDGE('',*,*,#8766,.T.);
#12899=ORIENTED_EDGE('',*,*,#8764,.T.);
#12900=ORIENTED_EDGE('',*,*,#8762,.T.);
#12901=ORIENTED_EDGE('',*,*,#8688,.T.);
#12902=ORIENTED_EDGE('',*,*,#8687,.T.);
#12903=ORIENTED_EDGE('',*,*,#7989,.T.);
#12904=ORIENTED_EDGE('',*,*,#8686,.T.);
#12905=ORIENTED_EDGE('',*,*,#7925,.T.);
#12906=ORIENTED_EDGE('',*,*,#8693,.T.);
#12907=ORIENTED_EDGE('',*,*,#8692,.T.);
#12908=ORIENTED_EDGE('',*,*,#8132,.T.);
#12909=ORIENTED_EDGE('',*,*,#8691,.T.);
#12910=ORIENTED_EDGE('',*,*,#8068,.T.);
#12911=ORIENTED_EDGE('',*,*,#8702,.T.);
#12912=ORIENTED_EDGE('',*,*,#8699,.T.);
#12913=ORIENTED_EDGE('',*,*,#8696,.T.);
#12914=ORIENTED_EDGE('',*,*,#8705,.T.);
#12915=ORIENTED_EDGE('',*,*,#8769,.F.);
#12916=ORIENTED_EDGE('',*,*,#8770,.F.);
#12917=ORIENTED_EDGE('',*,*,#8771,.F.);
#12918=ORIENTED_EDGE('',*,*,#8772,.F.);
#12919=ORIENTED_EDGE('',*,*,#8773,.F.);
#12920=ORIENTED_EDGE('',*,*,#8774,.F.);
#12921=ORIENTED_EDGE('',*,*,#8775,.F.);
#12922=ORIENTED_EDGE('',*,*,#8776,.F.);
#12923=ORIENTED_EDGE('',*,*,#8776,.T.);
#12924=ORIENTED_EDGE('',*,*,#8777,.F.);
#12925=ORIENTED_EDGE('',*,*,#8770,.T.);
#12926=ORIENTED_EDGE('',*,*,#8778,.F.);
#12927=ORIENTED_EDGE('',*,*,#8773,.T.);
#12928=ORIENTED_EDGE('',*,*,#8778,.T.);
#12929=ORIENTED_EDGE('',*,*,#8769,.T.);
#12930=ORIENTED_EDGE('',*,*,#8779,.F.);
#12931=ORIENTED_EDGE('',*,*,#8775,.T.);
#12932=ORIENTED_EDGE('',*,*,#8780,.F.);
#12933=ORIENTED_EDGE('',*,*,#8771,.T.);
#12934=ORIENTED_EDGE('',*,*,#8777,.T.);
#12935=ORIENTED_EDGE('',*,*,#8774,.T.);
#12936=ORIENTED_EDGE('',*,*,#8779,.T.);
#12937=ORIENTED_EDGE('',*,*,#8772,.T.);
#12938=ORIENTED_EDGE('',*,*,#8780,.T.);
#12939=ORIENTED_EDGE('',*,*,#8781,.T.);
#12940=ORIENTED_EDGE('',*,*,#8782,.T.);
#12941=ORIENTED_EDGE('',*,*,#8783,.T.);
#12942=ORIENTED_EDGE('',*,*,#8784,.T.);
#12943=ORIENTED_EDGE('',*,*,#8785,.T.);
#12944=ORIENTED_EDGE('',*,*,#8784,.F.);
#12945=ORIENTED_EDGE('',*,*,#8786,.T.);
#12946=ORIENTED_EDGE('',*,*,#8787,.T.);
#12947=ORIENTED_EDGE('',*,*,#8788,.T.);
#12948=ORIENTED_EDGE('',*,*,#8789,.T.);
#12949=ORIENTED_EDGE('',*,*,#8790,.T.);
#12950=ORIENTED_EDGE('',*,*,#8781,.F.);
#12951=ORIENTED_EDGE('',*,*,#8791,.T.);
#12952=ORIENTED_EDGE('',*,*,#8792,.T.);
#12953=ORIENTED_EDGE('',*,*,#8793,.T.);
#12954=ORIENTED_EDGE('',*,*,#8794,.T.);
#12955=ORIENTED_EDGE('',*,*,#8795,.T.);
#12956=ORIENTED_EDGE('',*,*,#8788,.F.);
#12957=ORIENTED_EDGE('',*,*,#8796,.T.);
#12958=ORIENTED_EDGE('',*,*,#8797,.T.);
#12959=ORIENTED_EDGE('',*,*,#8798,.T.);
#12960=ORIENTED_EDGE('',*,*,#8799,.T.);
#12961=ORIENTED_EDGE('',*,*,#8800,.T.);
#12962=ORIENTED_EDGE('',*,*,#8793,.F.);
#12963=ORIENTED_EDGE('',*,*,#8801,.T.);
#12964=ORIENTED_EDGE('',*,*,#8802,.T.);
#12965=ORIENTED_EDGE('',*,*,#8803,.T.);
#12966=ORIENTED_EDGE('',*,*,#8804,.T.);
#12967=ORIENTED_EDGE('',*,*,#8805,.T.);
#12968=ORIENTED_EDGE('',*,*,#8798,.F.);
#12969=ORIENTED_EDGE('',*,*,#8806,.T.);
#12970=ORIENTED_EDGE('',*,*,#8807,.T.);
#12971=ORIENTED_EDGE('',*,*,#8808,.T.);
#12972=ORIENTED_EDGE('',*,*,#8809,.T.);
#12973=ORIENTED_EDGE('',*,*,#8810,.T.);
#12974=ORIENTED_EDGE('',*,*,#8803,.F.);
#12975=ORIENTED_EDGE('',*,*,#8811,.T.);
#12976=ORIENTED_EDGE('',*,*,#8812,.T.);
#12977=ORIENTED_EDGE('',*,*,#8813,.T.);
#12978=ORIENTED_EDGE('',*,*,#8814,.T.);
#12979=ORIENTED_EDGE('',*,*,#8815,.T.);
#12980=ORIENTED_EDGE('',*,*,#8808,.F.);
#12981=ORIENTED_EDGE('',*,*,#8816,.T.);
#12982=ORIENTED_EDGE('',*,*,#8817,.T.);
#12983=ORIENTED_EDGE('',*,*,#8818,.T.);
#12984=ORIENTED_EDGE('',*,*,#8819,.T.);
#12985=ORIENTED_EDGE('',*,*,#8820,.T.);
#12986=ORIENTED_EDGE('',*,*,#8813,.F.);
#12987=ORIENTED_EDGE('',*,*,#8821,.T.);
#12988=ORIENTED_EDGE('',*,*,#8822,.T.);
#12989=ORIENTED_EDGE('',*,*,#8823,.T.);
#12990=ORIENTED_EDGE('',*,*,#8824,.T.);
#12991=ORIENTED_EDGE('',*,*,#8825,.T.);
#12992=ORIENTED_EDGE('',*,*,#8818,.F.);
#12993=ORIENTED_EDGE('',*,*,#8826,.T.);
#12994=ORIENTED_EDGE('',*,*,#8827,.T.);
#12995=ORIENTED_EDGE('',*,*,#8828,.T.);
#12996=ORIENTED_EDGE('',*,*,#8829,.T.);
#12997=ORIENTED_EDGE('',*,*,#8830,.T.);
#12998=ORIENTED_EDGE('',*,*,#8823,.F.);
#12999=ORIENTED_EDGE('',*,*,#8831,.T.);
#13000=ORIENTED_EDGE('',*,*,#8832,.T.);
#13001=ORIENTED_EDGE('',*,*,#8833,.T.);
#13002=ORIENTED_EDGE('',*,*,#8834,.T.);
#13003=ORIENTED_EDGE('',*,*,#8835,.T.);
#13004=ORIENTED_EDGE('',*,*,#8828,.F.);
#13005=ORIENTED_EDGE('',*,*,#8836,.T.);
#13006=ORIENTED_EDGE('',*,*,#8837,.T.);
#13007=ORIENTED_EDGE('',*,*,#8838,.T.);
#13008=ORIENTED_EDGE('',*,*,#8839,.T.);
#13009=ORIENTED_EDGE('',*,*,#8840,.T.);
#13010=ORIENTED_EDGE('',*,*,#8833,.F.);
#13011=ORIENTED_EDGE('',*,*,#8841,.T.);
#13012=ORIENTED_EDGE('',*,*,#8842,.T.);
#13013=ORIENTED_EDGE('',*,*,#8843,.T.);
#13014=ORIENTED_EDGE('',*,*,#8844,.T.);
#13015=ORIENTED_EDGE('',*,*,#8845,.T.);
#13016=ORIENTED_EDGE('',*,*,#8838,.F.);
#13017=ORIENTED_EDGE('',*,*,#8846,.T.);
#13018=ORIENTED_EDGE('',*,*,#8847,.T.);
#13019=ORIENTED_EDGE('',*,*,#8848,.T.);
#13020=ORIENTED_EDGE('',*,*,#8849,.T.);
#13021=ORIENTED_EDGE('',*,*,#8850,.T.);
#13022=ORIENTED_EDGE('',*,*,#8843,.F.);
#13023=ORIENTED_EDGE('',*,*,#8851,.T.);
#13024=ORIENTED_EDGE('',*,*,#8852,.T.);
#13025=ORIENTED_EDGE('',*,*,#8853,.T.);
#13026=ORIENTED_EDGE('',*,*,#8854,.T.);
#13027=ORIENTED_EDGE('',*,*,#8855,.T.);
#13028=ORIENTED_EDGE('',*,*,#8848,.F.);
#13029=ORIENTED_EDGE('',*,*,#8856,.T.);
#13030=ORIENTED_EDGE('',*,*,#8857,.T.);
#13031=ORIENTED_EDGE('',*,*,#8858,.T.);
#13032=ORIENTED_EDGE('',*,*,#8859,.T.);
#13033=ORIENTED_EDGE('',*,*,#8860,.T.);
#13034=ORIENTED_EDGE('',*,*,#8853,.F.);
#13035=ORIENTED_EDGE('',*,*,#8861,.T.);
#13036=ORIENTED_EDGE('',*,*,#8862,.T.);
#13037=ORIENTED_EDGE('',*,*,#8863,.T.);
#13038=ORIENTED_EDGE('',*,*,#8864,.T.);
#13039=ORIENTED_EDGE('',*,*,#8865,.T.);
#13040=ORIENTED_EDGE('',*,*,#8858,.F.);
#13041=ORIENTED_EDGE('',*,*,#8866,.T.);
#13042=ORIENTED_EDGE('',*,*,#8867,.T.);
#13043=ORIENTED_EDGE('',*,*,#8868,.T.);
#13044=ORIENTED_EDGE('',*,*,#8869,.T.);
#13045=ORIENTED_EDGE('',*,*,#8870,.T.);
#13046=ORIENTED_EDGE('',*,*,#8863,.F.);
#13047=ORIENTED_EDGE('',*,*,#8871,.T.);
#13048=ORIENTED_EDGE('',*,*,#8872,.T.);
#13049=ORIENTED_EDGE('',*,*,#8873,.T.);
#13050=ORIENTED_EDGE('',*,*,#8874,.T.);
#13051=ORIENTED_EDGE('',*,*,#8875,.T.);
#13052=ORIENTED_EDGE('',*,*,#8868,.F.);
#13053=ORIENTED_EDGE('',*,*,#8876,.T.);
#13054=ORIENTED_EDGE('',*,*,#8877,.T.);
#13055=ORIENTED_EDGE('',*,*,#8878,.T.);
#13056=ORIENTED_EDGE('',*,*,#8879,.T.);
#13057=ORIENTED_EDGE('',*,*,#8880,.T.);
#13058=ORIENTED_EDGE('',*,*,#8873,.F.);
#13059=ORIENTED_EDGE('',*,*,#8881,.T.);
#13060=ORIENTED_EDGE('',*,*,#8882,.T.);
#13061=ORIENTED_EDGE('',*,*,#8883,.T.);
#13062=ORIENTED_EDGE('',*,*,#8884,.T.);
#13063=ORIENTED_EDGE('',*,*,#8885,.T.);
#13064=ORIENTED_EDGE('',*,*,#8878,.F.);
#13065=ORIENTED_EDGE('',*,*,#8886,.T.);
#13066=ORIENTED_EDGE('',*,*,#8887,.T.);
#13067=ORIENTED_EDGE('',*,*,#8888,.T.);
#13068=ORIENTED_EDGE('',*,*,#8889,.T.);
#13069=ORIENTED_EDGE('',*,*,#8890,.T.);
#13070=ORIENTED_EDGE('',*,*,#8883,.F.);
#13071=ORIENTED_EDGE('',*,*,#8891,.T.);
#13072=ORIENTED_EDGE('',*,*,#8892,.T.);
#13073=ORIENTED_EDGE('',*,*,#8893,.T.);
#13074=ORIENTED_EDGE('',*,*,#8894,.T.);
#13075=ORIENTED_EDGE('',*,*,#8895,.T.);
#13076=ORIENTED_EDGE('',*,*,#8888,.F.);
#13077=ORIENTED_EDGE('',*,*,#8896,.T.);
#13078=ORIENTED_EDGE('',*,*,#8897,.T.);
#13079=ORIENTED_EDGE('',*,*,#8898,.T.);
#13080=ORIENTED_EDGE('',*,*,#8899,.T.);
#13081=ORIENTED_EDGE('',*,*,#8900,.T.);
#13082=ORIENTED_EDGE('',*,*,#8893,.F.);
#13083=ORIENTED_EDGE('',*,*,#8901,.T.);
#13084=ORIENTED_EDGE('',*,*,#8902,.T.);
#13085=ORIENTED_EDGE('',*,*,#8903,.T.);
#13086=ORIENTED_EDGE('',*,*,#8904,.T.);
#13087=ORIENTED_EDGE('',*,*,#8905,.T.);
#13088=ORIENTED_EDGE('',*,*,#8898,.F.);
#13089=ORIENTED_EDGE('',*,*,#8906,.T.);
#13090=ORIENTED_EDGE('',*,*,#8907,.T.);
#13091=ORIENTED_EDGE('',*,*,#8908,.T.);
#13092=ORIENTED_EDGE('',*,*,#8909,.T.);
#13093=ORIENTED_EDGE('',*,*,#8910,.T.);
#13094=ORIENTED_EDGE('',*,*,#8903,.F.);
#13095=ORIENTED_EDGE('',*,*,#8911,.T.);
#13096=ORIENTED_EDGE('',*,*,#8912,.T.);
#13097=ORIENTED_EDGE('',*,*,#8913,.T.);
#13098=ORIENTED_EDGE('',*,*,#8914,.T.);
#13099=ORIENTED_EDGE('',*,*,#8915,.T.);
#13100=ORIENTED_EDGE('',*,*,#8908,.F.);
#13101=ORIENTED_EDGE('',*,*,#8916,.T.);
#13102=ORIENTED_EDGE('',*,*,#8917,.T.);
#13103=ORIENTED_EDGE('',*,*,#8918,.T.);
#13104=ORIENTED_EDGE('',*,*,#8919,.T.);
#13105=ORIENTED_EDGE('',*,*,#8920,.T.);
#13106=ORIENTED_EDGE('',*,*,#8913,.F.);
#13107=ORIENTED_EDGE('',*,*,#8921,.T.);
#13108=ORIENTED_EDGE('',*,*,#8922,.T.);
#13109=ORIENTED_EDGE('',*,*,#8923,.T.);
#13110=ORIENTED_EDGE('',*,*,#8924,.T.);
#13111=ORIENTED_EDGE('',*,*,#8925,.T.);
#13112=ORIENTED_EDGE('',*,*,#8918,.F.);
#13113=ORIENTED_EDGE('',*,*,#8926,.T.);
#13114=ORIENTED_EDGE('',*,*,#8927,.T.);
#13115=ORIENTED_EDGE('',*,*,#8928,.T.);
#13116=ORIENTED_EDGE('',*,*,#8929,.T.);
#13117=ORIENTED_EDGE('',*,*,#8930,.T.);
#13118=ORIENTED_EDGE('',*,*,#8923,.F.);
#13119=ORIENTED_EDGE('',*,*,#8931,.T.);
#13120=ORIENTED_EDGE('',*,*,#8932,.T.);
#13121=ORIENTED_EDGE('',*,*,#8933,.T.);
#13122=ORIENTED_EDGE('',*,*,#8934,.T.);
#13123=ORIENTED_EDGE('',*,*,#8935,.T.);
#13124=ORIENTED_EDGE('',*,*,#8928,.F.);
#13125=ORIENTED_EDGE('',*,*,#8936,.T.);
#13126=ORIENTED_EDGE('',*,*,#8937,.T.);
#13127=ORIENTED_EDGE('',*,*,#8938,.T.);
#13128=ORIENTED_EDGE('',*,*,#8939,.T.);
#13129=ORIENTED_EDGE('',*,*,#8940,.T.);
#13130=ORIENTED_EDGE('',*,*,#8933,.F.);
#13131=ORIENTED_EDGE('',*,*,#8941,.T.);
#13132=ORIENTED_EDGE('',*,*,#8942,.T.);
#13133=ORIENTED_EDGE('',*,*,#8943,.T.);
#13134=ORIENTED_EDGE('',*,*,#8944,.T.);
#13135=ORIENTED_EDGE('',*,*,#8945,.T.);
#13136=ORIENTED_EDGE('',*,*,#8938,.F.);
#13137=ORIENTED_EDGE('',*,*,#8946,.T.);
#13138=ORIENTED_EDGE('',*,*,#8947,.T.);
#13139=ORIENTED_EDGE('',*,*,#8948,.T.);
#13140=ORIENTED_EDGE('',*,*,#8949,.T.);
#13141=ORIENTED_EDGE('',*,*,#8950,.T.);
#13142=ORIENTED_EDGE('',*,*,#8943,.F.);
#13143=ORIENTED_EDGE('',*,*,#8951,.T.);
#13144=ORIENTED_EDGE('',*,*,#8952,.T.);
#13145=ORIENTED_EDGE('',*,*,#8953,.T.);
#13146=ORIENTED_EDGE('',*,*,#8954,.T.);
#13147=ORIENTED_EDGE('',*,*,#8955,.T.);
#13148=ORIENTED_EDGE('',*,*,#8948,.F.);
#13149=ORIENTED_EDGE('',*,*,#8956,.T.);
#13150=ORIENTED_EDGE('',*,*,#8957,.T.);
#13151=ORIENTED_EDGE('',*,*,#8958,.T.);
#13152=ORIENTED_EDGE('',*,*,#8959,.T.);
#13153=ORIENTED_EDGE('',*,*,#8960,.T.);
#13154=ORIENTED_EDGE('',*,*,#8953,.F.);
#13155=ORIENTED_EDGE('',*,*,#8961,.T.);
#13156=ORIENTED_EDGE('',*,*,#8962,.T.);
#13157=ORIENTED_EDGE('',*,*,#8963,.T.);
#13158=ORIENTED_EDGE('',*,*,#8964,.T.);
#13159=ORIENTED_EDGE('',*,*,#8965,.T.);
#13160=ORIENTED_EDGE('',*,*,#8958,.F.);
#13161=ORIENTED_EDGE('',*,*,#8966,.T.);
#13162=ORIENTED_EDGE('',*,*,#8967,.T.);
#13163=ORIENTED_EDGE('',*,*,#8968,.T.);
#13164=ORIENTED_EDGE('',*,*,#8969,.T.);
#13165=ORIENTED_EDGE('',*,*,#8970,.T.);
#13166=ORIENTED_EDGE('',*,*,#8963,.F.);
#13167=ORIENTED_EDGE('',*,*,#8971,.T.);
#13168=ORIENTED_EDGE('',*,*,#8972,.T.);
#13169=ORIENTED_EDGE('',*,*,#8973,.T.);
#13170=ORIENTED_EDGE('',*,*,#8974,.T.);
#13171=ORIENTED_EDGE('',*,*,#8975,.T.);
#13172=ORIENTED_EDGE('',*,*,#8968,.F.);
#13173=ORIENTED_EDGE('',*,*,#8976,.T.);
#13174=ORIENTED_EDGE('',*,*,#8977,.T.);
#13175=ORIENTED_EDGE('',*,*,#8978,.T.);
#13176=ORIENTED_EDGE('',*,*,#8979,.T.);
#13177=ORIENTED_EDGE('',*,*,#8980,.T.);
#13178=ORIENTED_EDGE('',*,*,#8973,.F.);
#13179=ORIENTED_EDGE('',*,*,#8981,.T.);
#13180=ORIENTED_EDGE('',*,*,#8982,.T.);
#13181=ORIENTED_EDGE('',*,*,#8983,.T.);
#13182=ORIENTED_EDGE('',*,*,#8984,.T.);
#13183=ORIENTED_EDGE('',*,*,#8985,.T.);
#13184=ORIENTED_EDGE('',*,*,#8978,.F.);
#13185=ORIENTED_EDGE('',*,*,#8986,.T.);
#13186=ORIENTED_EDGE('',*,*,#8987,.T.);
#13187=ORIENTED_EDGE('',*,*,#8988,.T.);
#13188=ORIENTED_EDGE('',*,*,#8989,.T.);
#13189=ORIENTED_EDGE('',*,*,#8990,.T.);
#13190=ORIENTED_EDGE('',*,*,#8983,.F.);
#13191=ORIENTED_EDGE('',*,*,#8991,.T.);
#13192=ORIENTED_EDGE('',*,*,#8992,.T.);
#13193=ORIENTED_EDGE('',*,*,#8993,.T.);
#13194=ORIENTED_EDGE('',*,*,#8994,.T.);
#13195=ORIENTED_EDGE('',*,*,#8995,.T.);
#13196=ORIENTED_EDGE('',*,*,#8988,.F.);
#13197=ORIENTED_EDGE('',*,*,#8996,.T.);
#13198=ORIENTED_EDGE('',*,*,#8997,.T.);
#13199=ORIENTED_EDGE('',*,*,#8998,.T.);
#13200=ORIENTED_EDGE('',*,*,#8999,.T.);
#13201=ORIENTED_EDGE('',*,*,#9000,.T.);
#13202=ORIENTED_EDGE('',*,*,#8993,.F.);
#13203=ORIENTED_EDGE('',*,*,#9001,.T.);
#13204=ORIENTED_EDGE('',*,*,#9002,.T.);
#13205=ORIENTED_EDGE('',*,*,#9003,.T.);
#13206=ORIENTED_EDGE('',*,*,#9004,.T.);
#13207=ORIENTED_EDGE('',*,*,#9005,.T.);
#13208=ORIENTED_EDGE('',*,*,#8998,.F.);
#13209=ORIENTED_EDGE('',*,*,#9006,.T.);
#13210=ORIENTED_EDGE('',*,*,#9007,.T.);
#13211=ORIENTED_EDGE('',*,*,#9008,.T.);
#13212=ORIENTED_EDGE('',*,*,#9009,.T.);
#13213=ORIENTED_EDGE('',*,*,#9010,.T.);
#13214=ORIENTED_EDGE('',*,*,#9003,.F.);
#13215=ORIENTED_EDGE('',*,*,#9011,.T.);
#13216=ORIENTED_EDGE('',*,*,#9012,.T.);
#13217=ORIENTED_EDGE('',*,*,#9013,.T.);
#13218=ORIENTED_EDGE('',*,*,#9014,.T.);
#13219=ORIENTED_EDGE('',*,*,#9015,.T.);
#13220=ORIENTED_EDGE('',*,*,#9008,.F.);
#13221=ORIENTED_EDGE('',*,*,#9016,.T.);
#13222=ORIENTED_EDGE('',*,*,#9017,.T.);
#13223=ORIENTED_EDGE('',*,*,#9018,.T.);
#13224=ORIENTED_EDGE('',*,*,#9019,.T.);
#13225=ORIENTED_EDGE('',*,*,#9020,.T.);
#13226=ORIENTED_EDGE('',*,*,#9013,.F.);
#13227=ORIENTED_EDGE('',*,*,#9021,.T.);
#13228=ORIENTED_EDGE('',*,*,#9022,.T.);
#13229=ORIENTED_EDGE('',*,*,#9023,.F.);
#13230=ORIENTED_EDGE('',*,*,#9024,.T.);
#13231=ORIENTED_EDGE('',*,*,#9025,.T.);
#13232=ORIENTED_EDGE('',*,*,#9026,.F.);
#13233=ORIENTED_EDGE('',*,*,#9027,.T.);
#13234=ORIENTED_EDGE('',*,*,#9028,.T.);
#13235=ORIENTED_EDGE('',*,*,#9023,.T.);
#13236=ORIENTED_EDGE('',*,*,#9029,.T.);
#13237=ORIENTED_EDGE('',*,*,#9030,.T.);
#13238=ORIENTED_EDGE('',*,*,#9018,.F.);
#13239=ORIENTED_EDGE('',*,*,#9031,.T.);
#13240=ORIENTED_EDGE('',*,*,#9032,.T.);
#13241=ORIENTED_EDGE('',*,*,#9033,.F.);
#13242=ORIENTED_EDGE('',*,*,#9034,.F.);
#13243=ORIENTED_EDGE('',*,*,#9035,.T.);
#13244=ORIENTED_EDGE('',*,*,#9036,.T.);
#13245=ORIENTED_EDGE('',*,*,#9037,.T.);
#13246=ORIENTED_EDGE('',*,*,#9038,.T.);
#13247=ORIENTED_EDGE('',*,*,#9039,.T.);
#13248=ORIENTED_EDGE('',*,*,#9040,.T.);
#13249=ORIENTED_EDGE('',*,*,#9041,.T.);
#13250=ORIENTED_EDGE('',*,*,#9042,.T.);
#13251=ORIENTED_EDGE('',*,*,#9043,.T.);
#13252=ORIENTED_EDGE('',*,*,#9044,.T.);
#13253=ORIENTED_EDGE('',*,*,#9045,.T.);
#13254=ORIENTED_EDGE('',*,*,#9046,.T.);
#13255=ORIENTED_EDGE('',*,*,#9047,.T.);
#13256=ORIENTED_EDGE('',*,*,#9048,.T.);
#13257=ORIENTED_EDGE('',*,*,#9049,.T.);
#13258=ORIENTED_EDGE('',*,*,#9050,.T.);
#13259=ORIENTED_EDGE('',*,*,#9051,.T.);
#13260=ORIENTED_EDGE('',*,*,#9052,.T.);
#13261=ORIENTED_EDGE('',*,*,#9053,.T.);
#13262=ORIENTED_EDGE('',*,*,#9054,.T.);
#13263=ORIENTED_EDGE('',*,*,#9055,.T.);
#13264=ORIENTED_EDGE('',*,*,#9056,.T.);
#13265=ORIENTED_EDGE('',*,*,#9057,.T.);
#13266=ORIENTED_EDGE('',*,*,#9058,.T.);
#13267=ORIENTED_EDGE('',*,*,#9059,.T.);
#13268=ORIENTED_EDGE('',*,*,#9060,.T.);
#13269=ORIENTED_EDGE('',*,*,#9061,.T.);
#13270=ORIENTED_EDGE('',*,*,#9062,.T.);
#13271=ORIENTED_EDGE('',*,*,#9063,.T.);
#13272=ORIENTED_EDGE('',*,*,#9064,.T.);
#13273=ORIENTED_EDGE('',*,*,#9065,.T.);
#13274=ORIENTED_EDGE('',*,*,#9066,.T.);
#13275=ORIENTED_EDGE('',*,*,#9067,.T.);
#13276=ORIENTED_EDGE('',*,*,#9068,.T.);
#13277=ORIENTED_EDGE('',*,*,#9069,.T.);
#13278=ORIENTED_EDGE('',*,*,#9070,.T.);
#13279=ORIENTED_EDGE('',*,*,#9071,.T.);
#13280=ORIENTED_EDGE('',*,*,#9072,.T.);
#13281=ORIENTED_EDGE('',*,*,#9073,.T.);
#13282=ORIENTED_EDGE('',*,*,#9074,.T.);
#13283=ORIENTED_EDGE('',*,*,#9075,.T.);
#13284=ORIENTED_EDGE('',*,*,#9076,.T.);
#13285=ORIENTED_EDGE('',*,*,#9077,.F.);
#13286=ORIENTED_EDGE('',*,*,#9078,.F.);
#13287=ORIENTED_EDGE('',*,*,#9079,.F.);
#13288=ORIENTED_EDGE('',*,*,#9080,.F.);
#13289=ORIENTED_EDGE('',*,*,#9081,.F.);
#13290=ORIENTED_EDGE('',*,*,#9082,.F.);
#13291=ORIENTED_EDGE('',*,*,#9083,.F.);
#13292=ORIENTED_EDGE('',*,*,#9084,.F.);
#13293=ORIENTED_EDGE('',*,*,#9085,.F.);
#13294=ORIENTED_EDGE('',*,*,#9086,.F.);
#13295=ORIENTED_EDGE('',*,*,#9087,.F.);
#13296=ORIENTED_EDGE('',*,*,#9088,.F.);
#13297=ORIENTED_EDGE('',*,*,#9089,.F.);
#13298=ORIENTED_EDGE('',*,*,#9090,.F.);
#13299=ORIENTED_EDGE('',*,*,#9091,.F.);
#13300=ORIENTED_EDGE('',*,*,#9092,.F.);
#13301=ORIENTED_EDGE('',*,*,#9093,.F.);
#13302=ORIENTED_EDGE('',*,*,#9094,.F.);
#13303=ORIENTED_EDGE('',*,*,#9095,.F.);
#13304=ORIENTED_EDGE('',*,*,#9096,.F.);
#13305=ORIENTED_EDGE('',*,*,#9097,.F.);
#13306=ORIENTED_EDGE('',*,*,#9098,.F.);
#13307=ORIENTED_EDGE('',*,*,#9099,.F.);
#13308=ORIENTED_EDGE('',*,*,#9100,.F.);
#13309=ORIENTED_EDGE('',*,*,#9101,.F.);
#13310=ORIENTED_EDGE('',*,*,#9102,.F.);
#13311=ORIENTED_EDGE('',*,*,#9103,.F.);
#13312=ORIENTED_EDGE('',*,*,#9104,.F.);
#13313=ORIENTED_EDGE('',*,*,#9105,.F.);
#13314=ORIENTED_EDGE('',*,*,#9106,.F.);
#13315=ORIENTED_EDGE('',*,*,#9107,.F.);
#13316=ORIENTED_EDGE('',*,*,#9108,.F.);
#13317=ORIENTED_EDGE('',*,*,#9109,.F.);
#13318=ORIENTED_EDGE('',*,*,#9110,.F.);
#13319=ORIENTED_EDGE('',*,*,#9111,.F.);
#13320=ORIENTED_EDGE('',*,*,#9112,.F.);
#13321=ORIENTED_EDGE('',*,*,#9113,.F.);
#13322=ORIENTED_EDGE('',*,*,#9114,.F.);
#13323=ORIENTED_EDGE('',*,*,#9115,.F.);
#13324=ORIENTED_EDGE('',*,*,#9116,.F.);
#13325=ORIENTED_EDGE('',*,*,#9117,.F.);
#13326=ORIENTED_EDGE('',*,*,#9118,.F.);
#13327=ORIENTED_EDGE('',*,*,#9119,.T.);
#13328=ORIENTED_EDGE('',*,*,#9120,.F.);
#13329=ORIENTED_EDGE('',*,*,#9119,.F.);
#13330=ORIENTED_EDGE('',*,*,#9121,.T.);
#13331=ORIENTED_EDGE('',*,*,#9122,.F.);
#13332=ORIENTED_EDGE('',*,*,#9121,.F.);
#13333=ORIENTED_EDGE('',*,*,#9123,.F.);
#13334=ORIENTED_EDGE('',*,*,#9124,.T.);
#13335=ORIENTED_EDGE('',*,*,#9125,.F.);
#13336=ORIENTED_EDGE('',*,*,#9126,.F.);
#13337=ORIENTED_EDGE('',*,*,#9127,.F.);
#13338=ORIENTED_EDGE('',*,*,#9128,.F.);
#13339=ORIENTED_EDGE('',*,*,#9124,.F.);
#13340=ORIENTED_EDGE('',*,*,#9129,.F.);
#13341=ORIENTED_EDGE('',*,*,#9130,.F.);
#13342=ORIENTED_EDGE('',*,*,#9131,.F.);
#13343=ORIENTED_EDGE('',*,*,#9126,.T.);
#13344=ORIENTED_EDGE('',*,*,#9132,.F.);
#13345=ORIENTED_EDGE('',*,*,#9129,.T.);
#13346=ORIENTED_EDGE('',*,*,#9123,.T.);
#13347=ORIENTED_EDGE('',*,*,#9131,.T.);
#13348=ORIENTED_EDGE('',*,*,#9133,.T.);
#13349=ORIENTED_EDGE('',*,*,#9122,.T.);
#13350=ORIENTED_EDGE('',*,*,#8783,.F.);
#13351=ORIENTED_EDGE('',*,*,#9134,.T.);
#13352=ORIENTED_EDGE('',*,*,#9077,.T.);
#13353=ORIENTED_EDGE('',*,*,#9135,.T.);
#13354=ORIENTED_EDGE('',*,*,#8786,.F.);
#13355=ORIENTED_EDGE('',*,*,#9135,.F.);
#13356=ORIENTED_EDGE('',*,*,#9076,.F.);
#13357=ORIENTED_EDGE('',*,*,#9075,.F.);
#13358=ORIENTED_EDGE('',*,*,#9074,.F.);
#13359=ORIENTED_EDGE('',*,*,#9073,.F.);
#13360=ORIENTED_EDGE('',*,*,#9072,.F.);
#13361=ORIENTED_EDGE('',*,*,#9071,.F.);
#13362=ORIENTED_EDGE('',*,*,#9070,.F.);
#13363=ORIENTED_EDGE('',*,*,#9069,.F.);
#13364=ORIENTED_EDGE('',*,*,#9068,.F.);
#13365=ORIENTED_EDGE('',*,*,#9067,.F.);
#13366=ORIENTED_EDGE('',*,*,#9066,.F.);
#13367=ORIENTED_EDGE('',*,*,#9065,.F.);
#13368=ORIENTED_EDGE('',*,*,#9064,.F.);
#13369=ORIENTED_EDGE('',*,*,#9063,.F.);
#13370=ORIENTED_EDGE('',*,*,#9062,.F.);
#13371=ORIENTED_EDGE('',*,*,#9061,.F.);
#13372=ORIENTED_EDGE('',*,*,#9060,.F.);
#13373=ORIENTED_EDGE('',*,*,#9059,.F.);
#13374=ORIENTED_EDGE('',*,*,#9058,.F.);
#13375=ORIENTED_EDGE('',*,*,#9057,.F.);
#13376=ORIENTED_EDGE('',*,*,#9056,.F.);
#13377=ORIENTED_EDGE('',*,*,#9055,.F.);
#13378=ORIENTED_EDGE('',*,*,#9054,.F.);
#13379=ORIENTED_EDGE('',*,*,#9053,.F.);
#13380=ORIENTED_EDGE('',*,*,#9052,.F.);
#13381=ORIENTED_EDGE('',*,*,#9051,.F.);
#13382=ORIENTED_EDGE('',*,*,#9050,.F.);
#13383=ORIENTED_EDGE('',*,*,#9049,.F.);
#13384=ORIENTED_EDGE('',*,*,#9048,.F.);
#13385=ORIENTED_EDGE('',*,*,#9047,.F.);
#13386=ORIENTED_EDGE('',*,*,#9046,.F.);
#13387=ORIENTED_EDGE('',*,*,#9045,.F.);
#13388=ORIENTED_EDGE('',*,*,#9044,.F.);
#13389=ORIENTED_EDGE('',*,*,#9043,.F.);
#13390=ORIENTED_EDGE('',*,*,#9042,.F.);
#13391=ORIENTED_EDGE('',*,*,#9041,.F.);
#13392=ORIENTED_EDGE('',*,*,#9040,.F.);
#13393=ORIENTED_EDGE('',*,*,#9039,.F.);
#13394=ORIENTED_EDGE('',*,*,#9038,.F.);
#13395=ORIENTED_EDGE('',*,*,#9037,.F.);
#13396=ORIENTED_EDGE('',*,*,#9036,.F.);
#13397=ORIENTED_EDGE('',*,*,#9035,.F.);
#13398=ORIENTED_EDGE('',*,*,#9136,.F.);
#13399=ORIENTED_EDGE('',*,*,#9025,.F.);
#13400=ORIENTED_EDGE('',*,*,#9024,.F.);
#13401=ORIENTED_EDGE('',*,*,#9032,.F.);
#13402=ORIENTED_EDGE('',*,*,#9031,.F.);
#13403=ORIENTED_EDGE('',*,*,#9022,.F.);
#13404=ORIENTED_EDGE('',*,*,#9021,.F.);
#13405=ORIENTED_EDGE('',*,*,#9017,.F.);
#13406=ORIENTED_EDGE('',*,*,#9016,.F.);
#13407=ORIENTED_EDGE('',*,*,#9012,.F.);
#13408=ORIENTED_EDGE('',*,*,#9011,.F.);
#13409=ORIENTED_EDGE('',*,*,#9007,.F.);
#13410=ORIENTED_EDGE('',*,*,#9006,.F.);
#13411=ORIENTED_EDGE('',*,*,#9002,.F.);
#13412=ORIENTED_EDGE('',*,*,#9001,.F.);
#13413=ORIENTED_EDGE('',*,*,#8997,.F.);
#13414=ORIENTED_EDGE('',*,*,#8996,.F.);
#13415=ORIENTED_EDGE('',*,*,#8992,.F.);
#13416=ORIENTED_EDGE('',*,*,#8991,.F.);
#13417=ORIENTED_EDGE('',*,*,#8987,.F.);
#13418=ORIENTED_EDGE('',*,*,#8986,.F.);
#13419=ORIENTED_EDGE('',*,*,#8982,.F.);
#13420=ORIENTED_EDGE('',*,*,#8981,.F.);
#13421=ORIENTED_EDGE('',*,*,#8977,.F.);
#13422=ORIENTED_EDGE('',*,*,#8976,.F.);
#13423=ORIENTED_EDGE('',*,*,#8972,.F.);
#13424=ORIENTED_EDGE('',*,*,#8971,.F.);
#13425=ORIENTED_EDGE('',*,*,#8967,.F.);
#13426=ORIENTED_EDGE('',*,*,#8966,.F.);
#13427=ORIENTED_EDGE('',*,*,#8962,.F.);
#13428=ORIENTED_EDGE('',*,*,#8961,.F.);
#13429=ORIENTED_EDGE('',*,*,#8957,.F.);
#13430=ORIENTED_EDGE('',*,*,#8956,.F.);
#13431=ORIENTED_EDGE('',*,*,#8952,.F.);
#13432=ORIENTED_EDGE('',*,*,#8951,.F.);
#13433=ORIENTED_EDGE('',*,*,#8947,.F.);
#13434=ORIENTED_EDGE('',*,*,#8946,.F.);
#13435=ORIENTED_EDGE('',*,*,#8942,.F.);
#13436=ORIENTED_EDGE('',*,*,#8941,.F.);
#13437=ORIENTED_EDGE('',*,*,#8937,.F.);
#13438=ORIENTED_EDGE('',*,*,#8936,.F.);
#13439=ORIENTED_EDGE('',*,*,#8932,.F.);
#13440=ORIENTED_EDGE('',*,*,#8931,.F.);
#13441=ORIENTED_EDGE('',*,*,#8927,.F.);
#13442=ORIENTED_EDGE('',*,*,#8926,.F.);
#13443=ORIENTED_EDGE('',*,*,#8922,.F.);
#13444=ORIENTED_EDGE('',*,*,#8921,.F.);
#13445=ORIENTED_EDGE('',*,*,#8917,.F.);
#13446=ORIENTED_EDGE('',*,*,#8916,.F.);
#13447=ORIENTED_EDGE('',*,*,#8912,.F.);
#13448=ORIENTED_EDGE('',*,*,#8911,.F.);
#13449=ORIENTED_EDGE('',*,*,#8907,.F.);
#13450=ORIENTED_EDGE('',*,*,#8906,.F.);
#13451=ORIENTED_EDGE('',*,*,#8902,.F.);
#13452=ORIENTED_EDGE('',*,*,#8901,.F.);
#13453=ORIENTED_EDGE('',*,*,#8897,.F.);
#13454=ORIENTED_EDGE('',*,*,#8896,.F.);
#13455=ORIENTED_EDGE('',*,*,#8892,.F.);
#13456=ORIENTED_EDGE('',*,*,#8891,.F.);
#13457=ORIENTED_EDGE('',*,*,#8887,.F.);
#13458=ORIENTED_EDGE('',*,*,#8886,.F.);
#13459=ORIENTED_EDGE('',*,*,#8882,.F.);
#13460=ORIENTED_EDGE('',*,*,#8881,.F.);
#13461=ORIENTED_EDGE('',*,*,#8877,.F.);
#13462=ORIENTED_EDGE('',*,*,#8876,.F.);
#13463=ORIENTED_EDGE('',*,*,#8872,.F.);
#13464=ORIENTED_EDGE('',*,*,#8871,.F.);
#13465=ORIENTED_EDGE('',*,*,#8867,.F.);
#13466=ORIENTED_EDGE('',*,*,#8866,.F.);
#13467=ORIENTED_EDGE('',*,*,#8862,.F.);
#13468=ORIENTED_EDGE('',*,*,#8861,.F.);
#13469=ORIENTED_EDGE('',*,*,#8857,.F.);
#13470=ORIENTED_EDGE('',*,*,#8856,.F.);
#13471=ORIENTED_EDGE('',*,*,#8852,.F.);
#13472=ORIENTED_EDGE('',*,*,#8851,.F.);
#13473=ORIENTED_EDGE('',*,*,#8847,.F.);
#13474=ORIENTED_EDGE('',*,*,#8846,.F.);
#13475=ORIENTED_EDGE('',*,*,#8842,.F.);
#13476=ORIENTED_EDGE('',*,*,#8841,.F.);
#13477=ORIENTED_EDGE('',*,*,#8837,.F.);
#13478=ORIENTED_EDGE('',*,*,#8836,.F.);
#13479=ORIENTED_EDGE('',*,*,#8832,.F.);
#13480=ORIENTED_EDGE('',*,*,#8831,.F.);
#13481=ORIENTED_EDGE('',*,*,#8827,.F.);
#13482=ORIENTED_EDGE('',*,*,#8826,.F.);
#13483=ORIENTED_EDGE('',*,*,#8822,.F.);
#13484=ORIENTED_EDGE('',*,*,#8821,.F.);
#13485=ORIENTED_EDGE('',*,*,#8817,.F.);
#13486=ORIENTED_EDGE('',*,*,#8816,.F.);
#13487=ORIENTED_EDGE('',*,*,#8812,.F.);
#13488=ORIENTED_EDGE('',*,*,#8811,.F.);
#13489=ORIENTED_EDGE('',*,*,#8807,.F.);
#13490=ORIENTED_EDGE('',*,*,#8806,.F.);
#13491=ORIENTED_EDGE('',*,*,#8802,.F.);
#13492=ORIENTED_EDGE('',*,*,#8801,.F.);
#13493=ORIENTED_EDGE('',*,*,#8797,.F.);
#13494=ORIENTED_EDGE('',*,*,#8796,.F.);
#13495=ORIENTED_EDGE('',*,*,#8792,.F.);
#13496=ORIENTED_EDGE('',*,*,#8791,.F.);
#13497=ORIENTED_EDGE('',*,*,#8787,.F.);
#13498=ORIENTED_EDGE('',*,*,#9134,.F.);
#13499=ORIENTED_EDGE('',*,*,#8782,.F.);
#13500=ORIENTED_EDGE('',*,*,#8790,.F.);
#13501=ORIENTED_EDGE('',*,*,#8789,.F.);
#13502=ORIENTED_EDGE('',*,*,#8795,.F.);
#13503=ORIENTED_EDGE('',*,*,#8794,.F.);
#13504=ORIENTED_EDGE('',*,*,#8800,.F.);
#13505=ORIENTED_EDGE('',*,*,#8799,.F.);
#13506=ORIENTED_EDGE('',*,*,#8805,.F.);
#13507=ORIENTED_EDGE('',*,*,#8804,.F.);
#13508=ORIENTED_EDGE('',*,*,#8810,.F.);
#13509=ORIENTED_EDGE('',*,*,#8809,.F.);
#13510=ORIENTED_EDGE('',*,*,#8815,.F.);
#13511=ORIENTED_EDGE('',*,*,#8814,.F.);
#13512=ORIENTED_EDGE('',*,*,#8820,.F.);
#13513=ORIENTED_EDGE('',*,*,#8819,.F.);
#13514=ORIENTED_EDGE('',*,*,#8825,.F.);
#13515=ORIENTED_EDGE('',*,*,#8824,.F.);
#13516=ORIENTED_EDGE('',*,*,#8830,.F.);
#13517=ORIENTED_EDGE('',*,*,#8829,.F.);
#13518=ORIENTED_EDGE('',*,*,#8835,.F.);
#13519=ORIENTED_EDGE('',*,*,#8834,.F.);
#13520=ORIENTED_EDGE('',*,*,#8840,.F.);
#13521=ORIENTED_EDGE('',*,*,#8839,.F.);
#13522=ORIENTED_EDGE('',*,*,#8845,.F.);
#13523=ORIENTED_EDGE('',*,*,#8844,.F.);
#13524=ORIENTED_EDGE('',*,*,#8850,.F.);
#13525=ORIENTED_EDGE('',*,*,#8849,.F.);
#13526=ORIENTED_EDGE('',*,*,#8855,.F.);
#13527=ORIENTED_EDGE('',*,*,#8854,.F.);
#13528=ORIENTED_EDGE('',*,*,#8860,.F.);
#13529=ORIENTED_EDGE('',*,*,#8859,.F.);
#13530=ORIENTED_EDGE('',*,*,#8865,.F.);
#13531=ORIENTED_EDGE('',*,*,#8864,.F.);
#13532=ORIENTED_EDGE('',*,*,#8870,.F.);
#13533=ORIENTED_EDGE('',*,*,#8869,.F.);
#13534=ORIENTED_EDGE('',*,*,#8875,.F.);
#13535=ORIENTED_EDGE('',*,*,#8874,.F.);
#13536=ORIENTED_EDGE('',*,*,#8880,.F.);
#13537=ORIENTED_EDGE('',*,*,#8879,.F.);
#13538=ORIENTED_EDGE('',*,*,#8885,.F.);
#13539=ORIENTED_EDGE('',*,*,#8884,.F.);
#13540=ORIENTED_EDGE('',*,*,#8890,.F.);
#13541=ORIENTED_EDGE('',*,*,#8889,.F.);
#13542=ORIENTED_EDGE('',*,*,#8895,.F.);
#13543=ORIENTED_EDGE('',*,*,#8894,.F.);
#13544=ORIENTED_EDGE('',*,*,#8900,.F.);
#13545=ORIENTED_EDGE('',*,*,#8899,.F.);
#13546=ORIENTED_EDGE('',*,*,#8905,.F.);
#13547=ORIENTED_EDGE('',*,*,#8904,.F.);
#13548=ORIENTED_EDGE('',*,*,#8910,.F.);
#13549=ORIENTED_EDGE('',*,*,#8909,.F.);
#13550=ORIENTED_EDGE('',*,*,#8915,.F.);
#13551=ORIENTED_EDGE('',*,*,#8914,.F.);
#13552=ORIENTED_EDGE('',*,*,#8920,.F.);
#13553=ORIENTED_EDGE('',*,*,#8919,.F.);
#13554=ORIENTED_EDGE('',*,*,#8925,.F.);
#13555=ORIENTED_EDGE('',*,*,#8924,.F.);
#13556=ORIENTED_EDGE('',*,*,#8930,.F.);
#13557=ORIENTED_EDGE('',*,*,#8929,.F.);
#13558=ORIENTED_EDGE('',*,*,#8935,.F.);
#13559=ORIENTED_EDGE('',*,*,#8934,.F.);
#13560=ORIENTED_EDGE('',*,*,#8940,.F.);
#13561=ORIENTED_EDGE('',*,*,#8939,.F.);
#13562=ORIENTED_EDGE('',*,*,#8945,.F.);
#13563=ORIENTED_EDGE('',*,*,#8944,.F.);
#13564=ORIENTED_EDGE('',*,*,#8950,.F.);
#13565=ORIENTED_EDGE('',*,*,#8949,.F.);
#13566=ORIENTED_EDGE('',*,*,#8955,.F.);
#13567=ORIENTED_EDGE('',*,*,#8954,.F.);
#13568=ORIENTED_EDGE('',*,*,#8960,.F.);
#13569=ORIENTED_EDGE('',*,*,#8959,.F.);
#13570=ORIENTED_EDGE('',*,*,#8965,.F.);
#13571=ORIENTED_EDGE('',*,*,#8964,.F.);
#13572=ORIENTED_EDGE('',*,*,#8970,.F.);
#13573=ORIENTED_EDGE('',*,*,#8969,.F.);
#13574=ORIENTED_EDGE('',*,*,#8975,.F.);
#13575=ORIENTED_EDGE('',*,*,#8974,.F.);
#13576=ORIENTED_EDGE('',*,*,#8980,.F.);
#13577=ORIENTED_EDGE('',*,*,#8979,.F.);
#13578=ORIENTED_EDGE('',*,*,#8985,.F.);
#13579=ORIENTED_EDGE('',*,*,#8984,.F.);
#13580=ORIENTED_EDGE('',*,*,#8990,.F.);
#13581=ORIENTED_EDGE('',*,*,#8989,.F.);
#13582=ORIENTED_EDGE('',*,*,#8995,.F.);
#13583=ORIENTED_EDGE('',*,*,#8994,.F.);
#13584=ORIENTED_EDGE('',*,*,#9000,.F.);
#13585=ORIENTED_EDGE('',*,*,#8999,.F.);
#13586=ORIENTED_EDGE('',*,*,#9005,.F.);
#13587=ORIENTED_EDGE('',*,*,#9004,.F.);
#13588=ORIENTED_EDGE('',*,*,#9010,.F.);
#13589=ORIENTED_EDGE('',*,*,#9009,.F.);
#13590=ORIENTED_EDGE('',*,*,#9015,.F.);
#13591=ORIENTED_EDGE('',*,*,#9014,.F.);
#13592=ORIENTED_EDGE('',*,*,#9020,.F.);
#13593=ORIENTED_EDGE('',*,*,#9019,.F.);
#13594=ORIENTED_EDGE('',*,*,#9030,.F.);
#13595=ORIENTED_EDGE('',*,*,#9029,.F.);
#13596=ORIENTED_EDGE('',*,*,#9028,.F.);
#13597=ORIENTED_EDGE('',*,*,#9027,.F.);
#13598=ORIENTED_EDGE('',*,*,#9137,.F.);
#13599=ORIENTED_EDGE('',*,*,#9033,.T.);
#13600=ORIENTED_EDGE('',*,*,#9118,.T.);
#13601=ORIENTED_EDGE('',*,*,#9117,.T.);
#13602=ORIENTED_EDGE('',*,*,#9116,.T.);
#13603=ORIENTED_EDGE('',*,*,#9115,.T.);
#13604=ORIENTED_EDGE('',*,*,#9114,.T.);
#13605=ORIENTED_EDGE('',*,*,#9113,.T.);
#13606=ORIENTED_EDGE('',*,*,#9112,.T.);
#13607=ORIENTED_EDGE('',*,*,#9111,.T.);
#13608=ORIENTED_EDGE('',*,*,#9110,.T.);
#13609=ORIENTED_EDGE('',*,*,#9109,.T.);
#13610=ORIENTED_EDGE('',*,*,#9108,.T.);
#13611=ORIENTED_EDGE('',*,*,#9107,.T.);
#13612=ORIENTED_EDGE('',*,*,#9106,.T.);
#13613=ORIENTED_EDGE('',*,*,#9105,.T.);
#13614=ORIENTED_EDGE('',*,*,#9104,.T.);
#13615=ORIENTED_EDGE('',*,*,#9103,.T.);
#13616=ORIENTED_EDGE('',*,*,#9102,.T.);
#13617=ORIENTED_EDGE('',*,*,#9101,.T.);
#13618=ORIENTED_EDGE('',*,*,#9100,.T.);
#13619=ORIENTED_EDGE('',*,*,#9099,.T.);
#13620=ORIENTED_EDGE('',*,*,#9098,.T.);
#13621=ORIENTED_EDGE('',*,*,#9097,.T.);
#13622=ORIENTED_EDGE('',*,*,#9096,.T.);
#13623=ORIENTED_EDGE('',*,*,#9095,.T.);
#13624=ORIENTED_EDGE('',*,*,#9094,.T.);
#13625=ORIENTED_EDGE('',*,*,#9093,.T.);
#13626=ORIENTED_EDGE('',*,*,#9092,.T.);
#13627=ORIENTED_EDGE('',*,*,#9091,.T.);
#13628=ORIENTED_EDGE('',*,*,#9090,.T.);
#13629=ORIENTED_EDGE('',*,*,#9089,.T.);
#13630=ORIENTED_EDGE('',*,*,#9088,.T.);
#13631=ORIENTED_EDGE('',*,*,#9087,.T.);
#13632=ORIENTED_EDGE('',*,*,#9086,.T.);
#13633=ORIENTED_EDGE('',*,*,#9085,.T.);
#13634=ORIENTED_EDGE('',*,*,#9084,.T.);
#13635=ORIENTED_EDGE('',*,*,#9083,.T.);
#13636=ORIENTED_EDGE('',*,*,#9082,.T.);
#13637=ORIENTED_EDGE('',*,*,#9081,.T.);
#13638=ORIENTED_EDGE('',*,*,#9080,.T.);
#13639=ORIENTED_EDGE('',*,*,#9079,.T.);
#13640=ORIENTED_EDGE('',*,*,#9078,.T.);
#13641=ORIENTED_EDGE('',*,*,#8785,.F.);
#13642=ORIENTED_EDGE('',*,*,#9138,.F.);
#13643=ORIENTED_EDGE('',*,*,#9138,.T.);
#13644=ORIENTED_EDGE('',*,*,#9139,.T.);
#13645=ORIENTED_EDGE('',*,*,#9120,.T.);
#13646=ORIENTED_EDGE('',*,*,#9139,.F.);
#13647=ORIENTED_EDGE('',*,*,#9127,.T.);
#13648=ORIENTED_EDGE('',*,*,#9133,.F.);
#13649=ORIENTED_EDGE('',*,*,#9130,.T.);
#13650=ORIENTED_EDGE('',*,*,#9140,.T.);
#13651=ORIENTED_EDGE('',*,*,#9128,.T.);
#13652=ORIENTED_EDGE('',*,*,#9140,.F.);
#13653=ORIENTED_EDGE('',*,*,#9132,.T.);
#13654=ORIENTED_EDGE('',*,*,#9125,.T.);
#13655=ORIENTED_EDGE('',*,*,#9137,.T.);
#13656=ORIENTED_EDGE('',*,*,#9026,.T.);
#13657=ORIENTED_EDGE('',*,*,#9136,.T.);
#13658=ORIENTED_EDGE('',*,*,#9034,.T.);
#13659=ORIENTED_EDGE('',*,*,#9141,.F.);
#13660=ORIENTED_EDGE('',*,*,#9142,.F.);
#13661=ORIENTED_EDGE('',*,*,#9143,.T.);
#13662=ORIENTED_EDGE('',*,*,#9141,.T.);
#13663=ORIENTED_EDGE('',*,*,#9143,.F.);
#13664=ORIENTED_EDGE('',*,*,#9144,.F.);
#13665=ORIENTED_EDGE('',*,*,#9142,.T.);
#13666=ORIENTED_EDGE('',*,*,#9145,.F.);
#13667=ORIENTED_EDGE('',*,*,#9146,.T.);
#13668=ORIENTED_EDGE('',*,*,#9144,.T.);
#13669=ORIENTED_EDGE('',*,*,#9146,.F.);
#13670=ORIENTED_EDGE('',*,*,#9145,.T.);
#13671=ORIENTED_EDGE('',*,*,#9147,.T.);
#13672=ORIENTED_EDGE('',*,*,#9147,.F.);
#13673=ORIENTED_EDGE('',*,*,#9148,.F.);
#13674=ORIENTED_EDGE('',*,*,#9149,.T.);
#13675=ORIENTED_EDGE('',*,*,#9150,.F.);
#13676=ORIENTED_EDGE('',*,*,#9149,.F.);
#13677=ORIENTED_EDGE('',*,*,#9151,.F.);
#13678=ORIENTED_EDGE('',*,*,#9152,.T.);
#13679=ORIENTED_EDGE('',*,*,#9153,.F.);
#13680=ORIENTED_EDGE('',*,*,#9152,.F.);
#13681=ORIENTED_EDGE('',*,*,#9154,.F.);
#13682=ORIENTED_EDGE('',*,*,#9155,.F.);
#13683=ORIENTED_EDGE('',*,*,#9156,.F.);
#13684=ORIENTED_EDGE('',*,*,#9157,.F.);
#13685=ORIENTED_EDGE('',*,*,#9150,.T.);
#13686=ORIENTED_EDGE('',*,*,#9153,.T.);
#13687=ORIENTED_EDGE('',*,*,#9158,.T.);
#13688=ORIENTED_EDGE('',*,*,#9159,.T.);
#13689=ORIENTED_EDGE('',*,*,#9160,.T.);
#13690=ORIENTED_EDGE('',*,*,#9161,.T.);
#13691=ORIENTED_EDGE('',*,*,#9155,.T.);
#13692=ORIENTED_EDGE('',*,*,#9162,.T.);
#13693=ORIENTED_EDGE('',*,*,#9163,.F.);
#13694=ORIENTED_EDGE('',*,*,#9164,.F.);
#13695=ORIENTED_EDGE('',*,*,#9156,.T.);
#13696=ORIENTED_EDGE('',*,*,#9164,.T.);
#13697=ORIENTED_EDGE('',*,*,#9165,.F.);
#13698=ORIENTED_EDGE('',*,*,#9166,.F.);
#13699=ORIENTED_EDGE('',*,*,#9157,.T.);
#13700=ORIENTED_EDGE('',*,*,#9166,.T.);
#13701=ORIENTED_EDGE('',*,*,#9167,.F.);
#13702=ORIENTED_EDGE('',*,*,#9168,.F.);
#13703=ORIENTED_EDGE('',*,*,#9154,.T.);
#13704=ORIENTED_EDGE('',*,*,#9168,.T.);
#13705=ORIENTED_EDGE('',*,*,#9169,.F.);
#13706=ORIENTED_EDGE('',*,*,#9162,.F.);
#13707=ORIENTED_EDGE('',*,*,#9169,.T.);
#13708=ORIENTED_EDGE('',*,*,#9167,.T.);
#13709=ORIENTED_EDGE('',*,*,#9165,.T.);
#13710=ORIENTED_EDGE('',*,*,#9163,.T.);
#13711=ORIENTED_EDGE('',*,*,#9148,.T.);
#13712=ORIENTED_EDGE('',*,*,#9151,.T.);
#13713=ORIENTED_EDGE('',*,*,#9170,.T.);
#13714=ORIENTED_EDGE('',*,*,#9171,.T.);
#13715=ORIENTED_EDGE('',*,*,#9158,.F.);
#13716=ORIENTED_EDGE('',*,*,#9172,.F.);
#13717=ORIENTED_EDGE('',*,*,#9173,.T.);
#13718=ORIENTED_EDGE('',*,*,#9172,.T.);
#13719=ORIENTED_EDGE('',*,*,#9161,.F.);
#13720=ORIENTED_EDGE('',*,*,#9174,.F.);
#13721=ORIENTED_EDGE('',*,*,#9175,.T.);
#13722=ORIENTED_EDGE('',*,*,#9174,.T.);
#13723=ORIENTED_EDGE('',*,*,#9160,.F.);
#13724=ORIENTED_EDGE('',*,*,#9176,.F.);
#13725=ORIENTED_EDGE('',*,*,#9177,.T.);
#13726=ORIENTED_EDGE('',*,*,#9176,.T.);
#13727=ORIENTED_EDGE('',*,*,#9159,.F.);
#13728=ORIENTED_EDGE('',*,*,#9171,.F.);
#13729=ORIENTED_EDGE('',*,*,#9177,.F.);
#13730=ORIENTED_EDGE('',*,*,#9170,.F.);
#13731=ORIENTED_EDGE('',*,*,#9173,.F.);
#13732=ORIENTED_EDGE('',*,*,#9175,.F.);
#13733=ORIENTED_EDGE('',*,*,#9178,.F.);
#13734=ORIENTED_EDGE('',*,*,#9179,.F.);
#13735=ORIENTED_EDGE('',*,*,#9180,.F.);
#13736=ORIENTED_EDGE('',*,*,#9181,.F.);
#13737=ORIENTED_EDGE('',*,*,#9181,.T.);
#13738=ORIENTED_EDGE('',*,*,#9182,.T.);
#13739=ORIENTED_EDGE('',*,*,#9183,.T.);
#13740=ORIENTED_EDGE('',*,*,#9184,.F.);
#13741=ORIENTED_EDGE('',*,*,#9180,.T.);
#13742=ORIENTED_EDGE('',*,*,#9185,.F.);
#13743=ORIENTED_EDGE('',*,*,#9186,.F.);
#13744=ORIENTED_EDGE('',*,*,#9182,.F.);
#13745=ORIENTED_EDGE('',*,*,#9187,.T.);
#13746=ORIENTED_EDGE('',*,*,#9188,.T.);
#13747=ORIENTED_EDGE('',*,*,#9189,.T.);
#13748=ORIENTED_EDGE('',*,*,#9190,.T.);
#13749=ORIENTED_EDGE('',*,*,#9191,.T.);
#13750=ORIENTED_EDGE('',*,*,#9192,.F.);
#13751=ORIENTED_EDGE('',*,*,#9193,.T.);
#13752=ORIENTED_EDGE('',*,*,#9187,.F.);
#13753=ORIENTED_EDGE('',*,*,#9193,.F.);
#13754=ORIENTED_EDGE('',*,*,#9194,.F.);
#13755=ORIENTED_EDGE('',*,*,#9195,.T.);
#13756=ORIENTED_EDGE('',*,*,#9188,.F.);
#13757=ORIENTED_EDGE('',*,*,#9195,.F.);
#13758=ORIENTED_EDGE('',*,*,#9196,.F.);
#13759=ORIENTED_EDGE('',*,*,#9197,.T.);
#13760=ORIENTED_EDGE('',*,*,#9189,.F.);
#13761=ORIENTED_EDGE('',*,*,#9197,.F.);
#13762=ORIENTED_EDGE('',*,*,#9198,.F.);
#13763=ORIENTED_EDGE('',*,*,#9199,.T.);
#13764=ORIENTED_EDGE('',*,*,#9190,.F.);
#13765=ORIENTED_EDGE('',*,*,#9199,.F.);
#13766=ORIENTED_EDGE('',*,*,#9200,.F.);
#13767=ORIENTED_EDGE('',*,*,#9201,.T.);
#13768=ORIENTED_EDGE('',*,*,#9191,.F.);
#13769=ORIENTED_EDGE('',*,*,#9201,.F.);
#13770=ORIENTED_EDGE('',*,*,#9186,.T.);
#13771=ORIENTED_EDGE('',*,*,#9202,.T.);
#13772=ORIENTED_EDGE('',*,*,#9203,.F.);
#13773=ORIENTED_EDGE('',*,*,#9183,.F.);
#13774=ORIENTED_EDGE('',*,*,#9179,.T.);
#13775=ORIENTED_EDGE('',*,*,#9204,.F.);
#13776=ORIENTED_EDGE('',*,*,#9202,.F.);
#13777=ORIENTED_EDGE('',*,*,#9185,.T.);
#13778=ORIENTED_EDGE('',*,*,#9178,.T.);
#13779=ORIENTED_EDGE('',*,*,#9184,.T.);
#13780=ORIENTED_EDGE('',*,*,#9203,.T.);
#13781=ORIENTED_EDGE('',*,*,#9204,.T.);
#13782=ORIENTED_EDGE('',*,*,#9200,.T.);
#13783=ORIENTED_EDGE('',*,*,#9198,.T.);
#13784=ORIENTED_EDGE('',*,*,#9196,.T.);
#13785=ORIENTED_EDGE('',*,*,#9194,.T.);
#13786=ORIENTED_EDGE('',*,*,#9192,.T.);
#13787=ORIENTED_EDGE('',*,*,#9205,.T.);
#13788=ORIENTED_EDGE('',*,*,#9206,.T.);
#13789=ORIENTED_EDGE('',*,*,#9207,.F.);
#13790=ORIENTED_EDGE('',*,*,#9206,.F.);
#13791=ORIENTED_EDGE('',*,*,#9208,.F.);
#13792=ORIENTED_EDGE('',*,*,#9209,.T.);
#13793=ORIENTED_EDGE('',*,*,#9210,.T.);
#13794=ORIENTED_EDGE('',*,*,#9209,.F.);
#13795=ORIENTED_EDGE('',*,*,#9208,.T.);
#13796=ORIENTED_EDGE('',*,*,#9207,.T.);
#13797=ORIENTED_EDGE('',*,*,#9210,.F.);
#13798=ORIENTED_EDGE('',*,*,#9205,.F.);
#13799=ORIENTED_EDGE('',*,*,#9211,.F.);
#13800=ORIENTED_EDGE('',*,*,#9212,.F.);
#13801=ORIENTED_EDGE('',*,*,#9213,.F.);
#13802=ORIENTED_EDGE('',*,*,#9214,.T.);
#13803=ORIENTED_EDGE('',*,*,#9215,.F.);
#13804=ORIENTED_EDGE('',*,*,#9216,.F.);
#13805=ORIENTED_EDGE('',*,*,#9217,.F.);
#13806=ORIENTED_EDGE('',*,*,#9211,.T.);
#13807=ORIENTED_EDGE('',*,*,#9218,.T.);
#13808=ORIENTED_EDGE('',*,*,#9219,.T.);
#13809=ORIENTED_EDGE('',*,*,#9220,.F.);
#13810=ORIENTED_EDGE('',*,*,#9221,.F.);
#13811=ORIENTED_EDGE('',*,*,#9222,.F.);
#13812=ORIENTED_EDGE('',*,*,#9215,.T.);
#13813=ORIENTED_EDGE('',*,*,#9223,.T.);
#13814=ORIENTED_EDGE('',*,*,#9224,.T.);
#13815=ORIENTED_EDGE('',*,*,#9225,.F.);
#13816=ORIENTED_EDGE('',*,*,#9226,.F.);
#13817=ORIENTED_EDGE('',*,*,#9227,.F.);
#13818=ORIENTED_EDGE('',*,*,#9220,.T.);
#13819=ORIENTED_EDGE('',*,*,#9228,.T.);
#13820=ORIENTED_EDGE('',*,*,#9229,.T.);
#13821=ORIENTED_EDGE('',*,*,#9230,.F.);
#13822=ORIENTED_EDGE('',*,*,#9231,.F.);
#13823=ORIENTED_EDGE('',*,*,#9232,.F.);
#13824=ORIENTED_EDGE('',*,*,#9225,.T.);
#13825=ORIENTED_EDGE('',*,*,#9233,.T.);
#13826=ORIENTED_EDGE('',*,*,#9234,.T.);
#13827=ORIENTED_EDGE('',*,*,#9235,.F.);
#13828=ORIENTED_EDGE('',*,*,#9236,.F.);
#13829=ORIENTED_EDGE('',*,*,#9237,.F.);
#13830=ORIENTED_EDGE('',*,*,#9230,.T.);
#13831=ORIENTED_EDGE('',*,*,#9238,.T.);
#13832=ORIENTED_EDGE('',*,*,#9239,.T.);
#13833=ORIENTED_EDGE('',*,*,#9240,.F.);
#13834=ORIENTED_EDGE('',*,*,#9241,.F.);
#13835=ORIENTED_EDGE('',*,*,#9242,.F.);
#13836=ORIENTED_EDGE('',*,*,#9235,.T.);
#13837=ORIENTED_EDGE('',*,*,#9243,.T.);
#13838=ORIENTED_EDGE('',*,*,#9244,.T.);
#13839=ORIENTED_EDGE('',*,*,#9245,.F.);
#13840=ORIENTED_EDGE('',*,*,#9246,.F.);
#13841=ORIENTED_EDGE('',*,*,#9247,.F.);
#13842=ORIENTED_EDGE('',*,*,#9240,.T.);
#13843=ORIENTED_EDGE('',*,*,#9248,.T.);
#13844=ORIENTED_EDGE('',*,*,#9249,.T.);
#13845=ORIENTED_EDGE('',*,*,#9250,.F.);
#13846=ORIENTED_EDGE('',*,*,#9251,.F.);
#13847=ORIENTED_EDGE('',*,*,#9252,.F.);
#13848=ORIENTED_EDGE('',*,*,#9245,.T.);
#13849=ORIENTED_EDGE('',*,*,#9253,.T.);
#13850=ORIENTED_EDGE('',*,*,#9254,.T.);
#13851=ORIENTED_EDGE('',*,*,#9255,.F.);
#13852=ORIENTED_EDGE('',*,*,#9256,.F.);
#13853=ORIENTED_EDGE('',*,*,#9257,.F.);
#13854=ORIENTED_EDGE('',*,*,#9250,.T.);
#13855=ORIENTED_EDGE('',*,*,#9258,.T.);
#13856=ORIENTED_EDGE('',*,*,#9259,.T.);
#13857=ORIENTED_EDGE('',*,*,#9260,.F.);
#13858=ORIENTED_EDGE('',*,*,#9261,.F.);
#13859=ORIENTED_EDGE('',*,*,#9262,.F.);
#13860=ORIENTED_EDGE('',*,*,#9255,.T.);
#13861=ORIENTED_EDGE('',*,*,#9263,.T.);
#13862=ORIENTED_EDGE('',*,*,#9264,.T.);
#13863=ORIENTED_EDGE('',*,*,#9265,.F.);
#13864=ORIENTED_EDGE('',*,*,#9266,.F.);
#13865=ORIENTED_EDGE('',*,*,#9267,.F.);
#13866=ORIENTED_EDGE('',*,*,#9260,.T.);
#13867=ORIENTED_EDGE('',*,*,#9268,.T.);
#13868=ORIENTED_EDGE('',*,*,#9269,.T.);
#13869=ORIENTED_EDGE('',*,*,#9270,.F.);
#13870=ORIENTED_EDGE('',*,*,#9271,.F.);
#13871=ORIENTED_EDGE('',*,*,#9272,.F.);
#13872=ORIENTED_EDGE('',*,*,#9265,.T.);
#13873=ORIENTED_EDGE('',*,*,#9273,.T.);
#13874=ORIENTED_EDGE('',*,*,#9274,.T.);
#13875=ORIENTED_EDGE('',*,*,#9275,.F.);
#13876=ORIENTED_EDGE('',*,*,#9276,.F.);
#13877=ORIENTED_EDGE('',*,*,#9277,.F.);
#13878=ORIENTED_EDGE('',*,*,#9270,.T.);
#13879=ORIENTED_EDGE('',*,*,#9278,.T.);
#13880=ORIENTED_EDGE('',*,*,#9279,.T.);
#13881=ORIENTED_EDGE('',*,*,#9280,.F.);
#13882=ORIENTED_EDGE('',*,*,#9281,.F.);
#13883=ORIENTED_EDGE('',*,*,#9282,.F.);
#13884=ORIENTED_EDGE('',*,*,#9275,.T.);
#13885=ORIENTED_EDGE('',*,*,#9283,.T.);
#13886=ORIENTED_EDGE('',*,*,#9284,.T.);
#13887=ORIENTED_EDGE('',*,*,#9285,.F.);
#13888=ORIENTED_EDGE('',*,*,#9286,.F.);
#13889=ORIENTED_EDGE('',*,*,#9287,.F.);
#13890=ORIENTED_EDGE('',*,*,#9280,.T.);
#13891=ORIENTED_EDGE('',*,*,#9288,.T.);
#13892=ORIENTED_EDGE('',*,*,#9289,.T.);
#13893=ORIENTED_EDGE('',*,*,#9290,.F.);
#13894=ORIENTED_EDGE('',*,*,#9291,.F.);
#13895=ORIENTED_EDGE('',*,*,#9292,.F.);
#13896=ORIENTED_EDGE('',*,*,#9285,.T.);
#13897=ORIENTED_EDGE('',*,*,#9293,.T.);
#13898=ORIENTED_EDGE('',*,*,#9294,.T.);
#13899=ORIENTED_EDGE('',*,*,#9295,.F.);
#13900=ORIENTED_EDGE('',*,*,#9296,.F.);
#13901=ORIENTED_EDGE('',*,*,#9297,.F.);
#13902=ORIENTED_EDGE('',*,*,#9290,.T.);
#13903=ORIENTED_EDGE('',*,*,#9298,.T.);
#13904=ORIENTED_EDGE('',*,*,#9299,.T.);
#13905=ORIENTED_EDGE('',*,*,#9300,.F.);
#13906=ORIENTED_EDGE('',*,*,#9301,.F.);
#13907=ORIENTED_EDGE('',*,*,#9302,.F.);
#13908=ORIENTED_EDGE('',*,*,#9295,.T.);
#13909=ORIENTED_EDGE('',*,*,#9303,.T.);
#13910=ORIENTED_EDGE('',*,*,#9304,.T.);
#13911=ORIENTED_EDGE('',*,*,#9305,.F.);
#13912=ORIENTED_EDGE('',*,*,#9306,.F.);
#13913=ORIENTED_EDGE('',*,*,#9307,.F.);
#13914=ORIENTED_EDGE('',*,*,#9300,.T.);
#13915=ORIENTED_EDGE('',*,*,#9308,.T.);
#13916=ORIENTED_EDGE('',*,*,#9309,.T.);
#13917=ORIENTED_EDGE('',*,*,#9310,.F.);
#13918=ORIENTED_EDGE('',*,*,#9311,.F.);
#13919=ORIENTED_EDGE('',*,*,#9312,.F.);
#13920=ORIENTED_EDGE('',*,*,#9305,.T.);
#13921=ORIENTED_EDGE('',*,*,#9313,.T.);
#13922=ORIENTED_EDGE('',*,*,#9314,.T.);
#13923=ORIENTED_EDGE('',*,*,#9315,.F.);
#13924=ORIENTED_EDGE('',*,*,#9316,.F.);
#13925=ORIENTED_EDGE('',*,*,#9317,.F.);
#13926=ORIENTED_EDGE('',*,*,#9310,.T.);
#13927=ORIENTED_EDGE('',*,*,#9318,.T.);
#13928=ORIENTED_EDGE('',*,*,#9319,.T.);
#13929=ORIENTED_EDGE('',*,*,#9320,.F.);
#13930=ORIENTED_EDGE('',*,*,#9321,.F.);
#13931=ORIENTED_EDGE('',*,*,#9322,.F.);
#13932=ORIENTED_EDGE('',*,*,#9315,.T.);
#13933=ORIENTED_EDGE('',*,*,#9323,.T.);
#13934=ORIENTED_EDGE('',*,*,#9324,.T.);
#13935=ORIENTED_EDGE('',*,*,#9325,.F.);
#13936=ORIENTED_EDGE('',*,*,#9326,.F.);
#13937=ORIENTED_EDGE('',*,*,#9327,.F.);
#13938=ORIENTED_EDGE('',*,*,#9320,.T.);
#13939=ORIENTED_EDGE('',*,*,#9328,.T.);
#13940=ORIENTED_EDGE('',*,*,#9329,.T.);
#13941=ORIENTED_EDGE('',*,*,#9330,.F.);
#13942=ORIENTED_EDGE('',*,*,#9331,.F.);
#13943=ORIENTED_EDGE('',*,*,#9332,.F.);
#13944=ORIENTED_EDGE('',*,*,#9325,.T.);
#13945=ORIENTED_EDGE('',*,*,#9333,.T.);
#13946=ORIENTED_EDGE('',*,*,#9334,.T.);
#13947=ORIENTED_EDGE('',*,*,#9335,.F.);
#13948=ORIENTED_EDGE('',*,*,#9336,.F.);
#13949=ORIENTED_EDGE('',*,*,#9337,.F.);
#13950=ORIENTED_EDGE('',*,*,#9330,.T.);
#13951=ORIENTED_EDGE('',*,*,#9338,.T.);
#13952=ORIENTED_EDGE('',*,*,#9339,.T.);
#13953=ORIENTED_EDGE('',*,*,#9340,.F.);
#13954=ORIENTED_EDGE('',*,*,#9341,.F.);
#13955=ORIENTED_EDGE('',*,*,#9342,.F.);
#13956=ORIENTED_EDGE('',*,*,#9335,.T.);
#13957=ORIENTED_EDGE('',*,*,#9343,.T.);
#13958=ORIENTED_EDGE('',*,*,#9344,.T.);
#13959=ORIENTED_EDGE('',*,*,#9345,.F.);
#13960=ORIENTED_EDGE('',*,*,#9346,.F.);
#13961=ORIENTED_EDGE('',*,*,#9347,.F.);
#13962=ORIENTED_EDGE('',*,*,#9340,.T.);
#13963=ORIENTED_EDGE('',*,*,#9348,.T.);
#13964=ORIENTED_EDGE('',*,*,#9349,.T.);
#13965=ORIENTED_EDGE('',*,*,#9350,.F.);
#13966=ORIENTED_EDGE('',*,*,#9351,.F.);
#13967=ORIENTED_EDGE('',*,*,#9352,.F.);
#13968=ORIENTED_EDGE('',*,*,#9345,.T.);
#13969=ORIENTED_EDGE('',*,*,#9353,.T.);
#13970=ORIENTED_EDGE('',*,*,#9354,.T.);
#13971=ORIENTED_EDGE('',*,*,#9355,.F.);
#13972=ORIENTED_EDGE('',*,*,#9356,.F.);
#13973=ORIENTED_EDGE('',*,*,#9357,.F.);
#13974=ORIENTED_EDGE('',*,*,#9350,.T.);
#13975=ORIENTED_EDGE('',*,*,#9358,.T.);
#13976=ORIENTED_EDGE('',*,*,#9359,.T.);
#13977=ORIENTED_EDGE('',*,*,#9360,.F.);
#13978=ORIENTED_EDGE('',*,*,#9361,.F.);
#13979=ORIENTED_EDGE('',*,*,#9362,.F.);
#13980=ORIENTED_EDGE('',*,*,#9355,.T.);
#13981=ORIENTED_EDGE('',*,*,#9363,.T.);
#13982=ORIENTED_EDGE('',*,*,#9364,.T.);
#13983=ORIENTED_EDGE('',*,*,#9365,.F.);
#13984=ORIENTED_EDGE('',*,*,#9366,.F.);
#13985=ORIENTED_EDGE('',*,*,#9367,.F.);
#13986=ORIENTED_EDGE('',*,*,#9360,.T.);
#13987=ORIENTED_EDGE('',*,*,#9368,.T.);
#13988=ORIENTED_EDGE('',*,*,#9369,.T.);
#13989=ORIENTED_EDGE('',*,*,#9370,.F.);
#13990=ORIENTED_EDGE('',*,*,#9371,.F.);
#13991=ORIENTED_EDGE('',*,*,#9372,.F.);
#13992=ORIENTED_EDGE('',*,*,#9365,.T.);
#13993=ORIENTED_EDGE('',*,*,#9373,.T.);
#13994=ORIENTED_EDGE('',*,*,#9374,.T.);
#13995=ORIENTED_EDGE('',*,*,#9375,.F.);
#13996=ORIENTED_EDGE('',*,*,#9376,.F.);
#13997=ORIENTED_EDGE('',*,*,#9377,.F.);
#13998=ORIENTED_EDGE('',*,*,#9370,.T.);
#13999=ORIENTED_EDGE('',*,*,#9378,.T.);
#14000=ORIENTED_EDGE('',*,*,#9379,.T.);
#14001=ORIENTED_EDGE('',*,*,#9380,.F.);
#14002=ORIENTED_EDGE('',*,*,#9381,.F.);
#14003=ORIENTED_EDGE('',*,*,#9382,.F.);
#14004=ORIENTED_EDGE('',*,*,#9375,.T.);
#14005=ORIENTED_EDGE('',*,*,#9383,.T.);
#14006=ORIENTED_EDGE('',*,*,#9384,.T.);
#14007=ORIENTED_EDGE('',*,*,#9385,.F.);
#14008=ORIENTED_EDGE('',*,*,#9386,.F.);
#14009=ORIENTED_EDGE('',*,*,#9387,.F.);
#14010=ORIENTED_EDGE('',*,*,#9380,.T.);
#14011=ORIENTED_EDGE('',*,*,#9388,.T.);
#14012=ORIENTED_EDGE('',*,*,#9389,.T.);
#14013=ORIENTED_EDGE('',*,*,#9390,.F.);
#14014=ORIENTED_EDGE('',*,*,#9391,.F.);
#14015=ORIENTED_EDGE('',*,*,#9392,.F.);
#14016=ORIENTED_EDGE('',*,*,#9385,.T.);
#14017=ORIENTED_EDGE('',*,*,#9393,.T.);
#14018=ORIENTED_EDGE('',*,*,#9394,.T.);
#14019=ORIENTED_EDGE('',*,*,#9395,.F.);
#14020=ORIENTED_EDGE('',*,*,#9396,.F.);
#14021=ORIENTED_EDGE('',*,*,#9397,.F.);
#14022=ORIENTED_EDGE('',*,*,#9390,.T.);
#14023=ORIENTED_EDGE('',*,*,#9398,.T.);
#14024=ORIENTED_EDGE('',*,*,#9399,.T.);
#14025=ORIENTED_EDGE('',*,*,#9400,.F.);
#14026=ORIENTED_EDGE('',*,*,#9401,.F.);
#14027=ORIENTED_EDGE('',*,*,#9402,.F.);
#14028=ORIENTED_EDGE('',*,*,#9395,.T.);
#14029=ORIENTED_EDGE('',*,*,#9403,.T.);
#14030=ORIENTED_EDGE('',*,*,#9404,.T.);
#14031=ORIENTED_EDGE('',*,*,#9405,.F.);
#14032=ORIENTED_EDGE('',*,*,#9406,.F.);
#14033=ORIENTED_EDGE('',*,*,#9407,.F.);
#14034=ORIENTED_EDGE('',*,*,#9400,.T.);
#14035=ORIENTED_EDGE('',*,*,#9408,.T.);
#14036=ORIENTED_EDGE('',*,*,#9409,.T.);
#14037=ORIENTED_EDGE('',*,*,#9410,.F.);
#14038=ORIENTED_EDGE('',*,*,#9411,.F.);
#14039=ORIENTED_EDGE('',*,*,#9412,.F.);
#14040=ORIENTED_EDGE('',*,*,#9405,.T.);
#14041=ORIENTED_EDGE('',*,*,#9413,.T.);
#14042=ORIENTED_EDGE('',*,*,#9414,.T.);
#14043=ORIENTED_EDGE('',*,*,#9415,.F.);
#14044=ORIENTED_EDGE('',*,*,#9416,.F.);
#14045=ORIENTED_EDGE('',*,*,#9417,.F.);
#14046=ORIENTED_EDGE('',*,*,#9410,.T.);
#14047=ORIENTED_EDGE('',*,*,#9418,.T.);
#14048=ORIENTED_EDGE('',*,*,#9419,.T.);
#14049=ORIENTED_EDGE('',*,*,#9420,.F.);
#14050=ORIENTED_EDGE('',*,*,#9421,.F.);
#14051=ORIENTED_EDGE('',*,*,#9422,.F.);
#14052=ORIENTED_EDGE('',*,*,#9415,.T.);
#14053=ORIENTED_EDGE('',*,*,#9423,.T.);
#14054=ORIENTED_EDGE('',*,*,#9424,.T.);
#14055=ORIENTED_EDGE('',*,*,#9425,.F.);
#14056=ORIENTED_EDGE('',*,*,#9426,.F.);
#14057=ORIENTED_EDGE('',*,*,#9427,.F.);
#14058=ORIENTED_EDGE('',*,*,#9420,.T.);
#14059=ORIENTED_EDGE('',*,*,#9428,.T.);
#14060=ORIENTED_EDGE('',*,*,#9429,.T.);
#14061=ORIENTED_EDGE('',*,*,#9430,.F.);
#14062=ORIENTED_EDGE('',*,*,#9431,.F.);
#14063=ORIENTED_EDGE('',*,*,#9432,.F.);
#14064=ORIENTED_EDGE('',*,*,#9425,.T.);
#14065=ORIENTED_EDGE('',*,*,#9433,.T.);
#14066=ORIENTED_EDGE('',*,*,#9434,.T.);
#14067=ORIENTED_EDGE('',*,*,#9435,.F.);
#14068=ORIENTED_EDGE('',*,*,#9436,.F.);
#14069=ORIENTED_EDGE('',*,*,#9437,.F.);
#14070=ORIENTED_EDGE('',*,*,#9430,.T.);
#14071=ORIENTED_EDGE('',*,*,#9438,.T.);
#14072=ORIENTED_EDGE('',*,*,#9439,.T.);
#14073=ORIENTED_EDGE('',*,*,#9440,.F.);
#14074=ORIENTED_EDGE('',*,*,#9441,.F.);
#14075=ORIENTED_EDGE('',*,*,#9442,.F.);
#14076=ORIENTED_EDGE('',*,*,#9435,.T.);
#14077=ORIENTED_EDGE('',*,*,#9443,.T.);
#14078=ORIENTED_EDGE('',*,*,#9444,.T.);
#14079=ORIENTED_EDGE('',*,*,#9445,.F.);
#14080=ORIENTED_EDGE('',*,*,#9446,.F.);
#14081=ORIENTED_EDGE('',*,*,#9447,.F.);
#14082=ORIENTED_EDGE('',*,*,#9440,.T.);
#14083=ORIENTED_EDGE('',*,*,#9448,.T.);
#14084=ORIENTED_EDGE('',*,*,#9449,.T.);
#14085=ORIENTED_EDGE('',*,*,#9450,.F.);
#14086=ORIENTED_EDGE('',*,*,#9451,.F.);
#14087=ORIENTED_EDGE('',*,*,#9452,.F.);
#14088=ORIENTED_EDGE('',*,*,#9445,.T.);
#14089=ORIENTED_EDGE('',*,*,#9453,.T.);
#14090=ORIENTED_EDGE('',*,*,#9454,.T.);
#14091=ORIENTED_EDGE('',*,*,#9455,.F.);
#14092=ORIENTED_EDGE('',*,*,#9456,.F.);
#14093=ORIENTED_EDGE('',*,*,#9457,.F.);
#14094=ORIENTED_EDGE('',*,*,#9450,.T.);
#14095=ORIENTED_EDGE('',*,*,#9458,.T.);
#14096=ORIENTED_EDGE('',*,*,#9459,.T.);
#14097=ORIENTED_EDGE('',*,*,#9460,.F.);
#14098=ORIENTED_EDGE('',*,*,#9461,.F.);
#14099=ORIENTED_EDGE('',*,*,#9462,.F.);
#14100=ORIENTED_EDGE('',*,*,#9455,.T.);
#14101=ORIENTED_EDGE('',*,*,#9463,.T.);
#14102=ORIENTED_EDGE('',*,*,#9464,.T.);
#14103=ORIENTED_EDGE('',*,*,#9465,.F.);
#14104=ORIENTED_EDGE('',*,*,#9466,.F.);
#14105=ORIENTED_EDGE('',*,*,#9467,.F.);
#14106=ORIENTED_EDGE('',*,*,#9460,.T.);
#14107=ORIENTED_EDGE('',*,*,#9468,.T.);
#14108=ORIENTED_EDGE('',*,*,#9469,.T.);
#14109=ORIENTED_EDGE('',*,*,#9470,.F.);
#14110=ORIENTED_EDGE('',*,*,#9471,.F.);
#14111=ORIENTED_EDGE('',*,*,#9472,.F.);
#14112=ORIENTED_EDGE('',*,*,#9465,.T.);
#14113=ORIENTED_EDGE('',*,*,#9473,.T.);
#14114=ORIENTED_EDGE('',*,*,#9474,.T.);
#14115=ORIENTED_EDGE('',*,*,#9475,.F.);
#14116=ORIENTED_EDGE('',*,*,#9476,.F.);
#14117=ORIENTED_EDGE('',*,*,#9477,.F.);
#14118=ORIENTED_EDGE('',*,*,#9470,.T.);
#14119=ORIENTED_EDGE('',*,*,#9478,.T.);
#14120=ORIENTED_EDGE('',*,*,#9479,.T.);
#14121=ORIENTED_EDGE('',*,*,#9480,.F.);
#14122=ORIENTED_EDGE('',*,*,#9481,.F.);
#14123=ORIENTED_EDGE('',*,*,#9482,.F.);
#14124=ORIENTED_EDGE('',*,*,#9475,.T.);
#14125=ORIENTED_EDGE('',*,*,#9483,.T.);
#14126=ORIENTED_EDGE('',*,*,#9484,.T.);
#14127=ORIENTED_EDGE('',*,*,#9485,.F.);
#14128=ORIENTED_EDGE('',*,*,#9486,.F.);
#14129=ORIENTED_EDGE('',*,*,#9487,.F.);
#14130=ORIENTED_EDGE('',*,*,#9480,.T.);
#14131=ORIENTED_EDGE('',*,*,#9488,.T.);
#14132=ORIENTED_EDGE('',*,*,#9489,.T.);
#14133=ORIENTED_EDGE('',*,*,#9490,.F.);
#14134=ORIENTED_EDGE('',*,*,#9491,.F.);
#14135=ORIENTED_EDGE('',*,*,#9492,.F.);
#14136=ORIENTED_EDGE('',*,*,#9485,.T.);
#14137=ORIENTED_EDGE('',*,*,#9493,.T.);
#14138=ORIENTED_EDGE('',*,*,#9494,.T.);
#14139=ORIENTED_EDGE('',*,*,#9495,.F.);
#14140=ORIENTED_EDGE('',*,*,#9496,.F.);
#14141=ORIENTED_EDGE('',*,*,#9497,.F.);
#14142=ORIENTED_EDGE('',*,*,#9490,.T.);
#14143=ORIENTED_EDGE('',*,*,#9498,.T.);
#14144=ORIENTED_EDGE('',*,*,#9499,.T.);
#14145=ORIENTED_EDGE('',*,*,#9500,.F.);
#14146=ORIENTED_EDGE('',*,*,#9501,.F.);
#14147=ORIENTED_EDGE('',*,*,#9502,.F.);
#14148=ORIENTED_EDGE('',*,*,#9495,.T.);
#14149=ORIENTED_EDGE('',*,*,#9503,.T.);
#14150=ORIENTED_EDGE('',*,*,#9504,.T.);
#14151=ORIENTED_EDGE('',*,*,#9505,.F.);
#14152=ORIENTED_EDGE('',*,*,#9506,.F.);
#14153=ORIENTED_EDGE('',*,*,#9507,.F.);
#14154=ORIENTED_EDGE('',*,*,#9500,.T.);
#14155=ORIENTED_EDGE('',*,*,#9508,.T.);
#14156=ORIENTED_EDGE('',*,*,#9509,.T.);
#14157=ORIENTED_EDGE('',*,*,#9510,.F.);
#14158=ORIENTED_EDGE('',*,*,#9511,.F.);
#14159=ORIENTED_EDGE('',*,*,#9512,.F.);
#14160=ORIENTED_EDGE('',*,*,#9505,.T.);
#14161=ORIENTED_EDGE('',*,*,#9513,.T.);
#14162=ORIENTED_EDGE('',*,*,#9514,.T.);
#14163=ORIENTED_EDGE('',*,*,#9515,.F.);
#14164=ORIENTED_EDGE('',*,*,#9516,.F.);
#14165=ORIENTED_EDGE('',*,*,#9517,.F.);
#14166=ORIENTED_EDGE('',*,*,#9510,.T.);
#14167=ORIENTED_EDGE('',*,*,#9518,.T.);
#14168=ORIENTED_EDGE('',*,*,#9519,.T.);
#14169=ORIENTED_EDGE('',*,*,#9520,.F.);
#14170=ORIENTED_EDGE('',*,*,#9521,.F.);
#14171=ORIENTED_EDGE('',*,*,#9522,.F.);
#14172=ORIENTED_EDGE('',*,*,#9515,.T.);
#14173=ORIENTED_EDGE('',*,*,#9523,.T.);
#14174=ORIENTED_EDGE('',*,*,#9524,.T.);
#14175=ORIENTED_EDGE('',*,*,#9525,.F.);
#14176=ORIENTED_EDGE('',*,*,#9526,.F.);
#14177=ORIENTED_EDGE('',*,*,#9527,.F.);
#14178=ORIENTED_EDGE('',*,*,#9520,.T.);
#14179=ORIENTED_EDGE('',*,*,#9528,.T.);
#14180=ORIENTED_EDGE('',*,*,#9529,.T.);
#14181=ORIENTED_EDGE('',*,*,#9530,.F.);
#14182=ORIENTED_EDGE('',*,*,#9531,.F.);
#14183=ORIENTED_EDGE('',*,*,#9532,.F.);
#14184=ORIENTED_EDGE('',*,*,#9525,.T.);
#14185=ORIENTED_EDGE('',*,*,#9533,.T.);
#14186=ORIENTED_EDGE('',*,*,#9534,.T.);
#14187=ORIENTED_EDGE('',*,*,#9535,.T.);
#14188=ORIENTED_EDGE('',*,*,#9536,.F.);
#14189=ORIENTED_EDGE('',*,*,#9537,.T.);
#14190=ORIENTED_EDGE('',*,*,#9538,.T.);
#14191=ORIENTED_EDGE('',*,*,#9539,.T.);
#14192=ORIENTED_EDGE('',*,*,#9540,.T.);
#14193=ORIENTED_EDGE('',*,*,#9541,.T.);
#14194=ORIENTED_EDGE('',*,*,#9542,.T.);
#14195=ORIENTED_EDGE('',*,*,#9543,.T.);
#14196=ORIENTED_EDGE('',*,*,#9544,.T.);
#14197=ORIENTED_EDGE('',*,*,#9545,.T.);
#14198=ORIENTED_EDGE('',*,*,#9546,.T.);
#14199=ORIENTED_EDGE('',*,*,#9547,.T.);
#14200=ORIENTED_EDGE('',*,*,#9548,.T.);
#14201=ORIENTED_EDGE('',*,*,#9549,.T.);
#14202=ORIENTED_EDGE('',*,*,#9550,.T.);
#14203=ORIENTED_EDGE('',*,*,#9551,.T.);
#14204=ORIENTED_EDGE('',*,*,#9552,.T.);
#14205=ORIENTED_EDGE('',*,*,#9553,.T.);
#14206=ORIENTED_EDGE('',*,*,#9554,.T.);
#14207=ORIENTED_EDGE('',*,*,#9555,.T.);
#14208=ORIENTED_EDGE('',*,*,#9556,.T.);
#14209=ORIENTED_EDGE('',*,*,#9557,.T.);
#14210=ORIENTED_EDGE('',*,*,#9558,.T.);
#14211=ORIENTED_EDGE('',*,*,#9559,.T.);
#14212=ORIENTED_EDGE('',*,*,#9560,.T.);
#14213=ORIENTED_EDGE('',*,*,#9561,.T.);
#14214=ORIENTED_EDGE('',*,*,#9562,.T.);
#14215=ORIENTED_EDGE('',*,*,#9563,.T.);
#14216=ORIENTED_EDGE('',*,*,#9564,.T.);
#14217=ORIENTED_EDGE('',*,*,#9565,.T.);
#14218=ORIENTED_EDGE('',*,*,#9566,.T.);
#14219=ORIENTED_EDGE('',*,*,#9567,.T.);
#14220=ORIENTED_EDGE('',*,*,#9568,.T.);
#14221=ORIENTED_EDGE('',*,*,#9569,.T.);
#14222=ORIENTED_EDGE('',*,*,#9570,.T.);
#14223=ORIENTED_EDGE('',*,*,#9571,.T.);
#14224=ORIENTED_EDGE('',*,*,#9572,.T.);
#14225=ORIENTED_EDGE('',*,*,#9573,.T.);
#14226=ORIENTED_EDGE('',*,*,#9574,.T.);
#14227=ORIENTED_EDGE('',*,*,#9575,.T.);
#14228=ORIENTED_EDGE('',*,*,#9576,.T.);
#14229=ORIENTED_EDGE('',*,*,#9577,.T.);
#14230=ORIENTED_EDGE('',*,*,#9578,.T.);
#14231=ORIENTED_EDGE('',*,*,#9579,.T.);
#14232=ORIENTED_EDGE('',*,*,#9580,.T.);
#14233=ORIENTED_EDGE('',*,*,#9581,.T.);
#14234=ORIENTED_EDGE('',*,*,#9582,.T.);
#14235=ORIENTED_EDGE('',*,*,#9583,.T.);
#14236=ORIENTED_EDGE('',*,*,#9584,.T.);
#14237=ORIENTED_EDGE('',*,*,#9585,.T.);
#14238=ORIENTED_EDGE('',*,*,#9586,.F.);
#14239=ORIENTED_EDGE('',*,*,#9587,.T.);
#14240=ORIENTED_EDGE('',*,*,#9588,.T.);
#14241=ORIENTED_EDGE('',*,*,#9589,.T.);
#14242=ORIENTED_EDGE('',*,*,#9590,.T.);
#14243=ORIENTED_EDGE('',*,*,#9591,.T.);
#14244=ORIENTED_EDGE('',*,*,#9592,.T.);
#14245=ORIENTED_EDGE('',*,*,#9593,.T.);
#14246=ORIENTED_EDGE('',*,*,#9594,.T.);
#14247=ORIENTED_EDGE('',*,*,#9595,.T.);
#14248=ORIENTED_EDGE('',*,*,#9596,.T.);
#14249=ORIENTED_EDGE('',*,*,#9597,.T.);
#14250=ORIENTED_EDGE('',*,*,#9598,.T.);
#14251=ORIENTED_EDGE('',*,*,#9599,.T.);
#14252=ORIENTED_EDGE('',*,*,#9600,.T.);
#14253=ORIENTED_EDGE('',*,*,#9601,.T.);
#14254=ORIENTED_EDGE('',*,*,#9602,.T.);
#14255=ORIENTED_EDGE('',*,*,#9603,.T.);
#14256=ORIENTED_EDGE('',*,*,#9604,.T.);
#14257=ORIENTED_EDGE('',*,*,#9605,.T.);
#14258=ORIENTED_EDGE('',*,*,#9606,.T.);
#14259=ORIENTED_EDGE('',*,*,#9607,.T.);
#14260=ORIENTED_EDGE('',*,*,#9608,.T.);
#14261=ORIENTED_EDGE('',*,*,#9609,.T.);
#14262=ORIENTED_EDGE('',*,*,#9610,.T.);
#14263=ORIENTED_EDGE('',*,*,#9611,.T.);
#14264=ORIENTED_EDGE('',*,*,#9612,.T.);
#14265=ORIENTED_EDGE('',*,*,#9613,.T.);
#14266=ORIENTED_EDGE('',*,*,#9614,.T.);
#14267=ORIENTED_EDGE('',*,*,#9615,.T.);
#14268=ORIENTED_EDGE('',*,*,#9616,.T.);
#14269=ORIENTED_EDGE('',*,*,#9617,.T.);
#14270=ORIENTED_EDGE('',*,*,#9618,.T.);
#14271=ORIENTED_EDGE('',*,*,#9619,.T.);
#14272=ORIENTED_EDGE('',*,*,#9620,.T.);
#14273=ORIENTED_EDGE('',*,*,#9621,.T.);
#14274=ORIENTED_EDGE('',*,*,#9622,.T.);
#14275=ORIENTED_EDGE('',*,*,#9623,.T.);
#14276=ORIENTED_EDGE('',*,*,#9624,.T.);
#14277=ORIENTED_EDGE('',*,*,#9625,.T.);
#14278=ORIENTED_EDGE('',*,*,#9626,.T.);
#14279=ORIENTED_EDGE('',*,*,#9627,.T.);
#14280=ORIENTED_EDGE('',*,*,#9628,.T.);
#14281=ORIENTED_EDGE('',*,*,#9629,.T.);
#14282=ORIENTED_EDGE('',*,*,#9630,.T.);
#14283=ORIENTED_EDGE('',*,*,#9631,.T.);
#14284=ORIENTED_EDGE('',*,*,#9632,.T.);
#14285=ORIENTED_EDGE('',*,*,#9633,.T.);
#14286=ORIENTED_EDGE('',*,*,#9530,.T.);
#14287=ORIENTED_EDGE('',*,*,#9634,.T.);
#14288=ORIENTED_EDGE('',*,*,#9635,.T.);
#14289=ORIENTED_EDGE('',*,*,#9636,.F.);
#14290=ORIENTED_EDGE('',*,*,#9637,.F.);
#14291=ORIENTED_EDGE('',*,*,#9638,.F.);
#14292=ORIENTED_EDGE('',*,*,#9639,.F.);
#14293=ORIENTED_EDGE('',*,*,#9640,.F.);
#14294=ORIENTED_EDGE('',*,*,#9641,.F.);
#14295=ORIENTED_EDGE('',*,*,#9642,.T.);
#14296=ORIENTED_EDGE('',*,*,#9643,.F.);
#14297=ORIENTED_EDGE('',*,*,#9644,.F.);
#14298=ORIENTED_EDGE('',*,*,#9645,.F.);
#14299=ORIENTED_EDGE('',*,*,#9642,.F.);
#14300=ORIENTED_EDGE('',*,*,#9646,.F.);
#14301=ORIENTED_EDGE('',*,*,#9585,.F.);
#14302=ORIENTED_EDGE('',*,*,#9584,.F.);
#14303=ORIENTED_EDGE('',*,*,#9583,.F.);
#14304=ORIENTED_EDGE('',*,*,#9582,.F.);
#14305=ORIENTED_EDGE('',*,*,#9581,.F.);
#14306=ORIENTED_EDGE('',*,*,#9580,.F.);
#14307=ORIENTED_EDGE('',*,*,#9579,.F.);
#14308=ORIENTED_EDGE('',*,*,#9578,.F.);
#14309=ORIENTED_EDGE('',*,*,#9577,.F.);
#14310=ORIENTED_EDGE('',*,*,#9576,.F.);
#14311=ORIENTED_EDGE('',*,*,#9575,.F.);
#14312=ORIENTED_EDGE('',*,*,#9574,.F.);
#14313=ORIENTED_EDGE('',*,*,#9573,.F.);
#14314=ORIENTED_EDGE('',*,*,#9572,.F.);
#14315=ORIENTED_EDGE('',*,*,#9571,.F.);
#14316=ORIENTED_EDGE('',*,*,#9570,.F.);
#14317=ORIENTED_EDGE('',*,*,#9569,.F.);
#14318=ORIENTED_EDGE('',*,*,#9568,.F.);
#14319=ORIENTED_EDGE('',*,*,#9567,.F.);
#14320=ORIENTED_EDGE('',*,*,#9566,.F.);
#14321=ORIENTED_EDGE('',*,*,#9565,.F.);
#14322=ORIENTED_EDGE('',*,*,#9564,.F.);
#14323=ORIENTED_EDGE('',*,*,#9563,.F.);
#14324=ORIENTED_EDGE('',*,*,#9562,.F.);
#14325=ORIENTED_EDGE('',*,*,#9561,.F.);
#14326=ORIENTED_EDGE('',*,*,#9560,.F.);
#14327=ORIENTED_EDGE('',*,*,#9559,.F.);
#14328=ORIENTED_EDGE('',*,*,#9558,.F.);
#14329=ORIENTED_EDGE('',*,*,#9557,.F.);
#14330=ORIENTED_EDGE('',*,*,#9556,.F.);
#14331=ORIENTED_EDGE('',*,*,#9555,.F.);
#14332=ORIENTED_EDGE('',*,*,#9554,.F.);
#14333=ORIENTED_EDGE('',*,*,#9553,.F.);
#14334=ORIENTED_EDGE('',*,*,#9552,.F.);
#14335=ORIENTED_EDGE('',*,*,#9551,.F.);
#14336=ORIENTED_EDGE('',*,*,#9550,.F.);
#14337=ORIENTED_EDGE('',*,*,#9549,.F.);
#14338=ORIENTED_EDGE('',*,*,#9548,.F.);
#14339=ORIENTED_EDGE('',*,*,#9547,.F.);
#14340=ORIENTED_EDGE('',*,*,#9546,.F.);
#14341=ORIENTED_EDGE('',*,*,#9545,.F.);
#14342=ORIENTED_EDGE('',*,*,#9544,.F.);
#14343=ORIENTED_EDGE('',*,*,#9543,.F.);
#14344=ORIENTED_EDGE('',*,*,#9542,.F.);
#14345=ORIENTED_EDGE('',*,*,#9541,.F.);
#14346=ORIENTED_EDGE('',*,*,#9540,.F.);
#14347=ORIENTED_EDGE('',*,*,#9539,.F.);
#14348=ORIENTED_EDGE('',*,*,#9538,.F.);
#14349=ORIENTED_EDGE('',*,*,#9537,.F.);
#14350=ORIENTED_EDGE('',*,*,#9647,.F.);
#14351=ORIENTED_EDGE('',*,*,#9212,.T.);
#14352=ORIENTED_EDGE('',*,*,#9217,.T.);
#14353=ORIENTED_EDGE('',*,*,#9216,.T.);
#14354=ORIENTED_EDGE('',*,*,#9222,.T.);
#14355=ORIENTED_EDGE('',*,*,#9221,.T.);
#14356=ORIENTED_EDGE('',*,*,#9227,.T.);
#14357=ORIENTED_EDGE('',*,*,#9226,.T.);
#14358=ORIENTED_EDGE('',*,*,#9232,.T.);
#14359=ORIENTED_EDGE('',*,*,#9231,.T.);
#14360=ORIENTED_EDGE('',*,*,#9237,.T.);
#14361=ORIENTED_EDGE('',*,*,#9236,.T.);
#14362=ORIENTED_EDGE('',*,*,#9242,.T.);
#14363=ORIENTED_EDGE('',*,*,#9241,.T.);
#14364=ORIENTED_EDGE('',*,*,#9247,.T.);
#14365=ORIENTED_EDGE('',*,*,#9246,.T.);
#14366=ORIENTED_EDGE('',*,*,#9252,.T.);
#14367=ORIENTED_EDGE('',*,*,#9251,.T.);
#14368=ORIENTED_EDGE('',*,*,#9257,.T.);
#14369=ORIENTED_EDGE('',*,*,#9256,.T.);
#14370=ORIENTED_EDGE('',*,*,#9262,.T.);
#14371=ORIENTED_EDGE('',*,*,#9261,.T.);
#14372=ORIENTED_EDGE('',*,*,#9267,.T.);
#14373=ORIENTED_EDGE('',*,*,#9266,.T.);
#14374=ORIENTED_EDGE('',*,*,#9272,.T.);
#14375=ORIENTED_EDGE('',*,*,#9271,.T.);
#14376=ORIENTED_EDGE('',*,*,#9277,.T.);
#14377=ORIENTED_EDGE('',*,*,#9276,.T.);
#14378=ORIENTED_EDGE('',*,*,#9282,.T.);
#14379=ORIENTED_EDGE('',*,*,#9281,.T.);
#14380=ORIENTED_EDGE('',*,*,#9287,.T.);
#14381=ORIENTED_EDGE('',*,*,#9286,.T.);
#14382=ORIENTED_EDGE('',*,*,#9292,.T.);
#14383=ORIENTED_EDGE('',*,*,#9291,.T.);
#14384=ORIENTED_EDGE('',*,*,#9297,.T.);
#14385=ORIENTED_EDGE('',*,*,#9296,.T.);
#14386=ORIENTED_EDGE('',*,*,#9302,.T.);
#14387=ORIENTED_EDGE('',*,*,#9301,.T.);
#14388=ORIENTED_EDGE('',*,*,#9307,.T.);
#14389=ORIENTED_EDGE('',*,*,#9306,.T.);
#14390=ORIENTED_EDGE('',*,*,#9312,.T.);
#14391=ORIENTED_EDGE('',*,*,#9311,.T.);
#14392=ORIENTED_EDGE('',*,*,#9317,.T.);
#14393=ORIENTED_EDGE('',*,*,#9316,.T.);
#14394=ORIENTED_EDGE('',*,*,#9322,.T.);
#14395=ORIENTED_EDGE('',*,*,#9321,.T.);
#14396=ORIENTED_EDGE('',*,*,#9327,.T.);
#14397=ORIENTED_EDGE('',*,*,#9326,.T.);
#14398=ORIENTED_EDGE('',*,*,#9332,.T.);
#14399=ORIENTED_EDGE('',*,*,#9331,.T.);
#14400=ORIENTED_EDGE('',*,*,#9337,.T.);
#14401=ORIENTED_EDGE('',*,*,#9336,.T.);
#14402=ORIENTED_EDGE('',*,*,#9342,.T.);
#14403=ORIENTED_EDGE('',*,*,#9341,.T.);
#14404=ORIENTED_EDGE('',*,*,#9347,.T.);
#14405=ORIENTED_EDGE('',*,*,#9346,.T.);
#14406=ORIENTED_EDGE('',*,*,#9352,.T.);
#14407=ORIENTED_EDGE('',*,*,#9351,.T.);
#14408=ORIENTED_EDGE('',*,*,#9357,.T.);
#14409=ORIENTED_EDGE('',*,*,#9356,.T.);
#14410=ORIENTED_EDGE('',*,*,#9362,.T.);
#14411=ORIENTED_EDGE('',*,*,#9361,.T.);
#14412=ORIENTED_EDGE('',*,*,#9367,.T.);
#14413=ORIENTED_EDGE('',*,*,#9366,.T.);
#14414=ORIENTED_EDGE('',*,*,#9372,.T.);
#14415=ORIENTED_EDGE('',*,*,#9371,.T.);
#14416=ORIENTED_EDGE('',*,*,#9377,.T.);
#14417=ORIENTED_EDGE('',*,*,#9376,.T.);
#14418=ORIENTED_EDGE('',*,*,#9382,.T.);
#14419=ORIENTED_EDGE('',*,*,#9381,.T.);
#14420=ORIENTED_EDGE('',*,*,#9387,.T.);
#14421=ORIENTED_EDGE('',*,*,#9386,.T.);
#14422=ORIENTED_EDGE('',*,*,#9392,.T.);
#14423=ORIENTED_EDGE('',*,*,#9391,.T.);
#14424=ORIENTED_EDGE('',*,*,#9397,.T.);
#14425=ORIENTED_EDGE('',*,*,#9396,.T.);
#14426=ORIENTED_EDGE('',*,*,#9402,.T.);
#14427=ORIENTED_EDGE('',*,*,#9401,.T.);
#14428=ORIENTED_EDGE('',*,*,#9407,.T.);
#14429=ORIENTED_EDGE('',*,*,#9406,.T.);
#14430=ORIENTED_EDGE('',*,*,#9412,.T.);
#14431=ORIENTED_EDGE('',*,*,#9411,.T.);
#14432=ORIENTED_EDGE('',*,*,#9417,.T.);
#14433=ORIENTED_EDGE('',*,*,#9416,.T.);
#14434=ORIENTED_EDGE('',*,*,#9422,.T.);
#14435=ORIENTED_EDGE('',*,*,#9421,.T.);
#14436=ORIENTED_EDGE('',*,*,#9427,.T.);
#14437=ORIENTED_EDGE('',*,*,#9426,.T.);
#14438=ORIENTED_EDGE('',*,*,#9432,.T.);
#14439=ORIENTED_EDGE('',*,*,#9431,.T.);
#14440=ORIENTED_EDGE('',*,*,#9437,.T.);
#14441=ORIENTED_EDGE('',*,*,#9436,.T.);
#14442=ORIENTED_EDGE('',*,*,#9442,.T.);
#14443=ORIENTED_EDGE('',*,*,#9441,.T.);
#14444=ORIENTED_EDGE('',*,*,#9447,.T.);
#14445=ORIENTED_EDGE('',*,*,#9446,.T.);
#14446=ORIENTED_EDGE('',*,*,#9452,.T.);
#14447=ORIENTED_EDGE('',*,*,#9451,.T.);
#14448=ORIENTED_EDGE('',*,*,#9457,.T.);
#14449=ORIENTED_EDGE('',*,*,#9456,.T.);
#14450=ORIENTED_EDGE('',*,*,#9462,.T.);
#14451=ORIENTED_EDGE('',*,*,#9461,.T.);
#14452=ORIENTED_EDGE('',*,*,#9467,.T.);
#14453=ORIENTED_EDGE('',*,*,#9466,.T.);
#14454=ORIENTED_EDGE('',*,*,#9472,.T.);
#14455=ORIENTED_EDGE('',*,*,#9471,.T.);
#14456=ORIENTED_EDGE('',*,*,#9477,.T.);
#14457=ORIENTED_EDGE('',*,*,#9476,.T.);
#14458=ORIENTED_EDGE('',*,*,#9482,.T.);
#14459=ORIENTED_EDGE('',*,*,#9481,.T.);
#14460=ORIENTED_EDGE('',*,*,#9487,.T.);
#14461=ORIENTED_EDGE('',*,*,#9486,.T.);
#14462=ORIENTED_EDGE('',*,*,#9492,.T.);
#14463=ORIENTED_EDGE('',*,*,#9491,.T.);
#14464=ORIENTED_EDGE('',*,*,#9497,.T.);
#14465=ORIENTED_EDGE('',*,*,#9496,.T.);
#14466=ORIENTED_EDGE('',*,*,#9502,.T.);
#14467=ORIENTED_EDGE('',*,*,#9501,.T.);
#14468=ORIENTED_EDGE('',*,*,#9507,.T.);
#14469=ORIENTED_EDGE('',*,*,#9506,.T.);
#14470=ORIENTED_EDGE('',*,*,#9512,.T.);
#14471=ORIENTED_EDGE('',*,*,#9511,.T.);
#14472=ORIENTED_EDGE('',*,*,#9517,.T.);
#14473=ORIENTED_EDGE('',*,*,#9516,.T.);
#14474=ORIENTED_EDGE('',*,*,#9522,.T.);
#14475=ORIENTED_EDGE('',*,*,#9521,.T.);
#14476=ORIENTED_EDGE('',*,*,#9527,.T.);
#14477=ORIENTED_EDGE('',*,*,#9526,.T.);
#14478=ORIENTED_EDGE('',*,*,#9532,.T.);
#14479=ORIENTED_EDGE('',*,*,#9531,.T.);
#14480=ORIENTED_EDGE('',*,*,#9638,.T.);
#14481=ORIENTED_EDGE('',*,*,#9637,.T.);
#14482=ORIENTED_EDGE('',*,*,#9648,.F.);
#14483=ORIENTED_EDGE('',*,*,#9635,.F.);
#14484=ORIENTED_EDGE('',*,*,#9634,.F.);
#14485=ORIENTED_EDGE('',*,*,#9534,.F.);
#14486=ORIENTED_EDGE('',*,*,#9533,.F.);
#14487=ORIENTED_EDGE('',*,*,#9529,.F.);
#14488=ORIENTED_EDGE('',*,*,#9528,.F.);
#14489=ORIENTED_EDGE('',*,*,#9524,.F.);
#14490=ORIENTED_EDGE('',*,*,#9523,.F.);
#14491=ORIENTED_EDGE('',*,*,#9519,.F.);
#14492=ORIENTED_EDGE('',*,*,#9518,.F.);
#14493=ORIENTED_EDGE('',*,*,#9514,.F.);
#14494=ORIENTED_EDGE('',*,*,#9513,.F.);
#14495=ORIENTED_EDGE('',*,*,#9509,.F.);
#14496=ORIENTED_EDGE('',*,*,#9508,.F.);
#14497=ORIENTED_EDGE('',*,*,#9504,.F.);
#14498=ORIENTED_EDGE('',*,*,#9503,.F.);
#14499=ORIENTED_EDGE('',*,*,#9499,.F.);
#14500=ORIENTED_EDGE('',*,*,#9498,.F.);
#14501=ORIENTED_EDGE('',*,*,#9494,.F.);
#14502=ORIENTED_EDGE('',*,*,#9493,.F.);
#14503=ORIENTED_EDGE('',*,*,#9489,.F.);
#14504=ORIENTED_EDGE('',*,*,#9488,.F.);
#14505=ORIENTED_EDGE('',*,*,#9484,.F.);
#14506=ORIENTED_EDGE('',*,*,#9483,.F.);
#14507=ORIENTED_EDGE('',*,*,#9479,.F.);
#14508=ORIENTED_EDGE('',*,*,#9478,.F.);
#14509=ORIENTED_EDGE('',*,*,#9474,.F.);
#14510=ORIENTED_EDGE('',*,*,#9473,.F.);
#14511=ORIENTED_EDGE('',*,*,#9469,.F.);
#14512=ORIENTED_EDGE('',*,*,#9468,.F.);
#14513=ORIENTED_EDGE('',*,*,#9464,.F.);
#14514=ORIENTED_EDGE('',*,*,#9463,.F.);
#14515=ORIENTED_EDGE('',*,*,#9459,.F.);
#14516=ORIENTED_EDGE('',*,*,#9458,.F.);
#14517=ORIENTED_EDGE('',*,*,#9454,.F.);
#14518=ORIENTED_EDGE('',*,*,#9453,.F.);
#14519=ORIENTED_EDGE('',*,*,#9449,.F.);
#14520=ORIENTED_EDGE('',*,*,#9448,.F.);
#14521=ORIENTED_EDGE('',*,*,#9444,.F.);
#14522=ORIENTED_EDGE('',*,*,#9443,.F.);
#14523=ORIENTED_EDGE('',*,*,#9439,.F.);
#14524=ORIENTED_EDGE('',*,*,#9438,.F.);
#14525=ORIENTED_EDGE('',*,*,#9434,.F.);
#14526=ORIENTED_EDGE('',*,*,#9433,.F.);
#14527=ORIENTED_EDGE('',*,*,#9429,.F.);
#14528=ORIENTED_EDGE('',*,*,#9428,.F.);
#14529=ORIENTED_EDGE('',*,*,#9424,.F.);
#14530=ORIENTED_EDGE('',*,*,#9423,.F.);
#14531=ORIENTED_EDGE('',*,*,#9419,.F.);
#14532=ORIENTED_EDGE('',*,*,#9418,.F.);
#14533=ORIENTED_EDGE('',*,*,#9414,.F.);
#14534=ORIENTED_EDGE('',*,*,#9413,.F.);
#14535=ORIENTED_EDGE('',*,*,#9409,.F.);
#14536=ORIENTED_EDGE('',*,*,#9408,.F.);
#14537=ORIENTED_EDGE('',*,*,#9404,.F.);
#14538=ORIENTED_EDGE('',*,*,#9403,.F.);
#14539=ORIENTED_EDGE('',*,*,#9399,.F.);
#14540=ORIENTED_EDGE('',*,*,#9398,.F.);
#14541=ORIENTED_EDGE('',*,*,#9394,.F.);
#14542=ORIENTED_EDGE('',*,*,#9393,.F.);
#14543=ORIENTED_EDGE('',*,*,#9389,.F.);
#14544=ORIENTED_EDGE('',*,*,#9388,.F.);
#14545=ORIENTED_EDGE('',*,*,#9384,.F.);
#14546=ORIENTED_EDGE('',*,*,#9383,.F.);
#14547=ORIENTED_EDGE('',*,*,#9379,.F.);
#14548=ORIENTED_EDGE('',*,*,#9378,.F.);
#14549=ORIENTED_EDGE('',*,*,#9374,.F.);
#14550=ORIENTED_EDGE('',*,*,#9373,.F.);
#14551=ORIENTED_EDGE('',*,*,#9369,.F.);
#14552=ORIENTED_EDGE('',*,*,#9368,.F.);
#14553=ORIENTED_EDGE('',*,*,#9364,.F.);
#14554=ORIENTED_EDGE('',*,*,#9363,.F.);
#14555=ORIENTED_EDGE('',*,*,#9359,.F.);
#14556=ORIENTED_EDGE('',*,*,#9358,.F.);
#14557=ORIENTED_EDGE('',*,*,#9354,.F.);
#14558=ORIENTED_EDGE('',*,*,#9353,.F.);
#14559=ORIENTED_EDGE('',*,*,#9349,.F.);
#14560=ORIENTED_EDGE('',*,*,#9348,.F.);
#14561=ORIENTED_EDGE('',*,*,#9344,.F.);
#14562=ORIENTED_EDGE('',*,*,#9343,.F.);
#14563=ORIENTED_EDGE('',*,*,#9339,.F.);
#14564=ORIENTED_EDGE('',*,*,#9338,.F.);
#14565=ORIENTED_EDGE('',*,*,#9334,.F.);
#14566=ORIENTED_EDGE('',*,*,#9333,.F.);
#14567=ORIENTED_EDGE('',*,*,#9329,.F.);
#14568=ORIENTED_EDGE('',*,*,#9328,.F.);
#14569=ORIENTED_EDGE('',*,*,#9324,.F.);
#14570=ORIENTED_EDGE('',*,*,#9323,.F.);
#14571=ORIENTED_EDGE('',*,*,#9319,.F.);
#14572=ORIENTED_EDGE('',*,*,#9318,.F.);
#14573=ORIENTED_EDGE('',*,*,#9314,.F.);
#14574=ORIENTED_EDGE('',*,*,#9313,.F.);
#14575=ORIENTED_EDGE('',*,*,#9309,.F.);
#14576=ORIENTED_EDGE('',*,*,#9308,.F.);
#14577=ORIENTED_EDGE('',*,*,#9304,.F.);
#14578=ORIENTED_EDGE('',*,*,#9303,.F.);
#14579=ORIENTED_EDGE('',*,*,#9299,.F.);
#14580=ORIENTED_EDGE('',*,*,#9298,.F.);
#14581=ORIENTED_EDGE('',*,*,#9294,.F.);
#14582=ORIENTED_EDGE('',*,*,#9293,.F.);
#14583=ORIENTED_EDGE('',*,*,#9289,.F.);
#14584=ORIENTED_EDGE('',*,*,#9288,.F.);
#14585=ORIENTED_EDGE('',*,*,#9284,.F.);
#14586=ORIENTED_EDGE('',*,*,#9283,.F.);
#14587=ORIENTED_EDGE('',*,*,#9279,.F.);
#14588=ORIENTED_EDGE('',*,*,#9278,.F.);
#14589=ORIENTED_EDGE('',*,*,#9274,.F.);
#14590=ORIENTED_EDGE('',*,*,#9273,.F.);
#14591=ORIENTED_EDGE('',*,*,#9269,.F.);
#14592=ORIENTED_EDGE('',*,*,#9268,.F.);
#14593=ORIENTED_EDGE('',*,*,#9264,.F.);
#14594=ORIENTED_EDGE('',*,*,#9263,.F.);
#14595=ORIENTED_EDGE('',*,*,#9259,.F.);
#14596=ORIENTED_EDGE('',*,*,#9258,.F.);
#14597=ORIENTED_EDGE('',*,*,#9254,.F.);
#14598=ORIENTED_EDGE('',*,*,#9253,.F.);
#14599=ORIENTED_EDGE('',*,*,#9249,.F.);
#14600=ORIENTED_EDGE('',*,*,#9248,.F.);
#14601=ORIENTED_EDGE('',*,*,#9244,.F.);
#14602=ORIENTED_EDGE('',*,*,#9243,.F.);
#14603=ORIENTED_EDGE('',*,*,#9239,.F.);
#14604=ORIENTED_EDGE('',*,*,#9238,.F.);
#14605=ORIENTED_EDGE('',*,*,#9234,.F.);
#14606=ORIENTED_EDGE('',*,*,#9233,.F.);
#14607=ORIENTED_EDGE('',*,*,#9229,.F.);
#14608=ORIENTED_EDGE('',*,*,#9228,.F.);
#14609=ORIENTED_EDGE('',*,*,#9224,.F.);
#14610=ORIENTED_EDGE('',*,*,#9223,.F.);
#14611=ORIENTED_EDGE('',*,*,#9219,.F.);
#14612=ORIENTED_EDGE('',*,*,#9218,.F.);
#14613=ORIENTED_EDGE('',*,*,#9214,.F.);
#14614=ORIENTED_EDGE('',*,*,#9649,.F.);
#14615=ORIENTED_EDGE('',*,*,#9535,.F.);
#14616=ORIENTED_EDGE('',*,*,#9633,.F.);
#14617=ORIENTED_EDGE('',*,*,#9632,.F.);
#14618=ORIENTED_EDGE('',*,*,#9631,.F.);
#14619=ORIENTED_EDGE('',*,*,#9630,.F.);
#14620=ORIENTED_EDGE('',*,*,#9629,.F.);
#14621=ORIENTED_EDGE('',*,*,#9628,.F.);
#14622=ORIENTED_EDGE('',*,*,#9627,.F.);
#14623=ORIENTED_EDGE('',*,*,#9626,.F.);
#14624=ORIENTED_EDGE('',*,*,#9625,.F.);
#14625=ORIENTED_EDGE('',*,*,#9624,.F.);
#14626=ORIENTED_EDGE('',*,*,#9623,.F.);
#14627=ORIENTED_EDGE('',*,*,#9622,.F.);
#14628=ORIENTED_EDGE('',*,*,#9621,.F.);
#14629=ORIENTED_EDGE('',*,*,#9620,.F.);
#14630=ORIENTED_EDGE('',*,*,#9619,.F.);
#14631=ORIENTED_EDGE('',*,*,#9618,.F.);
#14632=ORIENTED_EDGE('',*,*,#9617,.F.);
#14633=ORIENTED_EDGE('',*,*,#9616,.F.);
#14634=ORIENTED_EDGE('',*,*,#9615,.F.);
#14635=ORIENTED_EDGE('',*,*,#9614,.F.);
#14636=ORIENTED_EDGE('',*,*,#9613,.F.);
#14637=ORIENTED_EDGE('',*,*,#9612,.F.);
#14638=ORIENTED_EDGE('',*,*,#9611,.F.);
#14639=ORIENTED_EDGE('',*,*,#9610,.F.);
#14640=ORIENTED_EDGE('',*,*,#9609,.F.);
#14641=ORIENTED_EDGE('',*,*,#9608,.F.);
#14642=ORIENTED_EDGE('',*,*,#9607,.F.);
#14643=ORIENTED_EDGE('',*,*,#9606,.F.);
#14644=ORIENTED_EDGE('',*,*,#9605,.F.);
#14645=ORIENTED_EDGE('',*,*,#9604,.F.);
#14646=ORIENTED_EDGE('',*,*,#9603,.F.);
#14647=ORIENTED_EDGE('',*,*,#9602,.F.);
#14648=ORIENTED_EDGE('',*,*,#9601,.F.);
#14649=ORIENTED_EDGE('',*,*,#9600,.F.);
#14650=ORIENTED_EDGE('',*,*,#9599,.F.);
#14651=ORIENTED_EDGE('',*,*,#9598,.F.);
#14652=ORIENTED_EDGE('',*,*,#9597,.F.);
#14653=ORIENTED_EDGE('',*,*,#9596,.F.);
#14654=ORIENTED_EDGE('',*,*,#9595,.F.);
#14655=ORIENTED_EDGE('',*,*,#9594,.F.);
#14656=ORIENTED_EDGE('',*,*,#9593,.F.);
#14657=ORIENTED_EDGE('',*,*,#9592,.F.);
#14658=ORIENTED_EDGE('',*,*,#9591,.F.);
#14659=ORIENTED_EDGE('',*,*,#9590,.F.);
#14660=ORIENTED_EDGE('',*,*,#9589,.F.);
#14661=ORIENTED_EDGE('',*,*,#9588,.F.);
#14662=ORIENTED_EDGE('',*,*,#9587,.F.);
#14663=ORIENTED_EDGE('',*,*,#9648,.T.);
#14664=ORIENTED_EDGE('',*,*,#9586,.T.);
#14665=ORIENTED_EDGE('',*,*,#9646,.T.);
#14666=ORIENTED_EDGE('',*,*,#9636,.T.);
#14667=ORIENTED_EDGE('',*,*,#9650,.F.);
#14668=ORIENTED_EDGE('',*,*,#9651,.F.);
#14669=ORIENTED_EDGE('',*,*,#9652,.F.);
#14670=ORIENTED_EDGE('',*,*,#9653,.T.);
#14671=ORIENTED_EDGE('',*,*,#9650,.T.);
#14672=ORIENTED_EDGE('',*,*,#9653,.F.);
#14673=ORIENTED_EDGE('',*,*,#9651,.T.);
#14674=ORIENTED_EDGE('',*,*,#9654,.T.);
#14675=ORIENTED_EDGE('',*,*,#9643,.T.);
#14676=ORIENTED_EDGE('',*,*,#9645,.T.);
#14677=ORIENTED_EDGE('',*,*,#9655,.T.);
#14678=ORIENTED_EDGE('',*,*,#9656,.T.);
#14679=ORIENTED_EDGE('',*,*,#9655,.F.);
#14680=ORIENTED_EDGE('',*,*,#9644,.T.);
#14681=ORIENTED_EDGE('',*,*,#9654,.F.);
#14682=ORIENTED_EDGE('',*,*,#9640,.T.);
#14683=ORIENTED_EDGE('',*,*,#9639,.T.);
#14684=ORIENTED_EDGE('',*,*,#9641,.T.);
#14685=ORIENTED_EDGE('',*,*,#9652,.T.);
#14686=ORIENTED_EDGE('',*,*,#9536,.T.);
#14687=ORIENTED_EDGE('',*,*,#9649,.T.);
#14688=ORIENTED_EDGE('',*,*,#9213,.T.);
#14689=ORIENTED_EDGE('',*,*,#9647,.T.);
#14690=ORIENTED_EDGE('',*,*,#9656,.F.);
#14691=ORIENTED_EDGE('',*,*,#9657,.F.);
#14692=ORIENTED_EDGE('',*,*,#9658,.F.);
#14693=ORIENTED_EDGE('',*,*,#9659,.F.);
#14694=ORIENTED_EDGE('',*,*,#9660,.T.);
#14695=ORIENTED_EDGE('',*,*,#9661,.F.);
#14696=ORIENTED_EDGE('',*,*,#9660,.F.);
#14697=ORIENTED_EDGE('',*,*,#9662,.F.);
#14698=ORIENTED_EDGE('',*,*,#9663,.F.);
#14699=ORIENTED_EDGE('',*,*,#9664,.F.);
#14700=ORIENTED_EDGE('',*,*,#9665,.T.);
#14701=ORIENTED_EDGE('',*,*,#9666,.F.);
#14702=ORIENTED_EDGE('',*,*,#9667,.F.);
#14703=ORIENTED_EDGE('',*,*,#9668,.F.);
#14704=ORIENTED_EDGE('',*,*,#9665,.F.);
#14705=ORIENTED_EDGE('',*,*,#9669,.F.);
#14706=ORIENTED_EDGE('',*,*,#9670,.T.);
#14707=ORIENTED_EDGE('',*,*,#9671,.F.);
#14708=ORIENTED_EDGE('',*,*,#9670,.F.);
#14709=ORIENTED_EDGE('',*,*,#9672,.F.);
#14710=ORIENTED_EDGE('',*,*,#9673,.T.);
#14711=ORIENTED_EDGE('',*,*,#9674,.F.);
#14712=ORIENTED_EDGE('',*,*,#9673,.F.);
#14713=ORIENTED_EDGE('',*,*,#9675,.F.);
#14714=ORIENTED_EDGE('',*,*,#9676,.T.);
#14715=ORIENTED_EDGE('',*,*,#9677,.F.);
#14716=ORIENTED_EDGE('',*,*,#9676,.F.);
#14717=ORIENTED_EDGE('',*,*,#9678,.F.);
#14718=ORIENTED_EDGE('',*,*,#9679,.T.);
#14719=ORIENTED_EDGE('',*,*,#9680,.F.);
#14720=ORIENTED_EDGE('',*,*,#9679,.F.);
#14721=ORIENTED_EDGE('',*,*,#9681,.F.);
#14722=ORIENTED_EDGE('',*,*,#9682,.T.);
#14723=ORIENTED_EDGE('',*,*,#9683,.F.);
#14724=ORIENTED_EDGE('',*,*,#9682,.F.);
#14725=ORIENTED_EDGE('',*,*,#9684,.F.);
#14726=ORIENTED_EDGE('',*,*,#9685,.T.);
#14727=ORIENTED_EDGE('',*,*,#9686,.F.);
#14728=ORIENTED_EDGE('',*,*,#9685,.F.);
#14729=ORIENTED_EDGE('',*,*,#9687,.F.);
#14730=ORIENTED_EDGE('',*,*,#9688,.T.);
#14731=ORIENTED_EDGE('',*,*,#9666,.T.);
#14732=ORIENTED_EDGE('',*,*,#9668,.T.);
#14733=ORIENTED_EDGE('',*,*,#9689,.T.);
#14734=ORIENTED_EDGE('',*,*,#9690,.F.);
#14735=ORIENTED_EDGE('',*,*,#9689,.F.);
#14736=ORIENTED_EDGE('',*,*,#9667,.T.);
#14737=ORIENTED_EDGE('',*,*,#9688,.F.);
#14738=ORIENTED_EDGE('',*,*,#9658,.T.);
#14739=ORIENTED_EDGE('',*,*,#9657,.T.);
#14740=ORIENTED_EDGE('',*,*,#9659,.T.);
#14741=ORIENTED_EDGE('',*,*,#9687,.T.);
#14742=ORIENTED_EDGE('',*,*,#9691,.T.);
#14743=ORIENTED_EDGE('',*,*,#9692,.T.);
#14744=ORIENTED_EDGE('',*,*,#9693,.T.);
#14745=ORIENTED_EDGE('',*,*,#9662,.T.);
#14746=ORIENTED_EDGE('',*,*,#9664,.T.);
#14747=ORIENTED_EDGE('',*,*,#9694,.T.);
#14748=ORIENTED_EDGE('',*,*,#9691,.F.);
#14749=ORIENTED_EDGE('',*,*,#9694,.F.);
#14750=ORIENTED_EDGE('',*,*,#9663,.T.);
#14751=ORIENTED_EDGE('',*,*,#9693,.F.);
#14752=ORIENTED_EDGE('',*,*,#9661,.T.);
#14753=ORIENTED_EDGE('',*,*,#9695,.F.);
#14754=ORIENTED_EDGE('',*,*,#9696,.T.);
#14755=ORIENTED_EDGE('',*,*,#9697,.T.);
#14756=ORIENTED_EDGE('',*,*,#9696,.F.);
#14757=ORIENTED_EDGE('',*,*,#9695,.T.);
#14758=ORIENTED_EDGE('',*,*,#9690,.T.);
#14759=ORIENTED_EDGE('',*,*,#9684,.T.);
#14760=ORIENTED_EDGE('',*,*,#9681,.T.);
#14761=ORIENTED_EDGE('',*,*,#9678,.T.);
#14762=ORIENTED_EDGE('',*,*,#9675,.T.);
#14763=ORIENTED_EDGE('',*,*,#9672,.T.);
#14764=ORIENTED_EDGE('',*,*,#9669,.T.);
#14765=ORIENTED_EDGE('',*,*,#9697,.F.);
#14766=ORIENTED_EDGE('',*,*,#9692,.F.);
#14767=ORIENTED_EDGE('',*,*,#9686,.T.);
#14768=ORIENTED_EDGE('',*,*,#9683,.T.);
#14769=ORIENTED_EDGE('',*,*,#9680,.T.);
#14770=ORIENTED_EDGE('',*,*,#9677,.T.);
#14771=ORIENTED_EDGE('',*,*,#9674,.T.);
#14772=ORIENTED_EDGE('',*,*,#9671,.T.);
#14773=ORIENTED_EDGE('',*,*,#9698,.F.);
#14774=ORIENTED_EDGE('',*,*,#9699,.T.);
#14775=ORIENTED_EDGE('',*,*,#9700,.T.);
#14776=ORIENTED_EDGE('',*,*,#9699,.F.);
#14777=ORIENTED_EDGE('',*,*,#9701,.F.);
#14778=ORIENTED_EDGE('',*,*,#9700,.F.);
#14779=ORIENTED_EDGE('',*,*,#9702,.F.);
#14780=ORIENTED_EDGE('',*,*,#9698,.T.);
#14781=ORIENTED_EDGE('',*,*,#9703,.F.);
#14782=ORIENTED_EDGE('',*,*,#9704,.T.);
#14783=ORIENTED_EDGE('',*,*,#9702,.T.);
#14784=ORIENTED_EDGE('',*,*,#9704,.F.);
#14785=ORIENTED_EDGE('',*,*,#9705,.T.);
#14786=ORIENTED_EDGE('',*,*,#9706,.F.);
#14787=ORIENTED_EDGE('',*,*,#9705,.F.);
#14788=ORIENTED_EDGE('',*,*,#9707,.T.);
#14789=ORIENTED_EDGE('',*,*,#9708,.T.);
#14790=ORIENTED_EDGE('',*,*,#9707,.F.);
#14791=ORIENTED_EDGE('',*,*,#9708,.F.);
#14792=ORIENTED_EDGE('',*,*,#9701,.T.);
#14793=ORIENTED_EDGE('',*,*,#9709,.T.);
#14794=ORIENTED_EDGE('',*,*,#9706,.T.);
#14795=ORIENTED_EDGE('',*,*,#9709,.F.);
#14796=ORIENTED_EDGE('',*,*,#9703,.T.);
#14797=ORIENTED_EDGE('',*,*,#9710,.T.);
#14798=ORIENTED_EDGE('',*,*,#9711,.T.);
#14799=ORIENTED_EDGE('',*,*,#9712,.F.);
#14800=ORIENTED_EDGE('',*,*,#9711,.F.);
#14801=ORIENTED_EDGE('',*,*,#9713,.F.);
#14802=ORIENTED_EDGE('',*,*,#9714,.T.);
#14803=ORIENTED_EDGE('',*,*,#9715,.T.);
#14804=ORIENTED_EDGE('',*,*,#9714,.F.);
#14805=ORIENTED_EDGE('',*,*,#9713,.T.);
#14806=ORIENTED_EDGE('',*,*,#9712,.T.);
#14807=ORIENTED_EDGE('',*,*,#9715,.F.);
#14808=ORIENTED_EDGE('',*,*,#9710,.F.);
#14809=ORIENTED_EDGE('',*,*,#9716,.F.);
#14810=ORIENTED_EDGE('',*,*,#9717,.F.);
#14811=ORIENTED_EDGE('',*,*,#9718,.F.);
#14812=ORIENTED_EDGE('',*,*,#9719,.F.);
#14813=ORIENTED_EDGE('',*,*,#9720,.F.);
#14814=ORIENTED_EDGE('',*,*,#9721,.F.);
#14815=ORIENTED_EDGE('',*,*,#9722,.F.);
#14816=ORIENTED_EDGE('',*,*,#9723,.F.);
#14817=ORIENTED_EDGE('',*,*,#9723,.T.);
#14818=ORIENTED_EDGE('',*,*,#9724,.F.);
#14819=ORIENTED_EDGE('',*,*,#9717,.T.);
#14820=ORIENTED_EDGE('',*,*,#9725,.F.);
#14821=ORIENTED_EDGE('',*,*,#9720,.T.);
#14822=ORIENTED_EDGE('',*,*,#9725,.T.);
#14823=ORIENTED_EDGE('',*,*,#9716,.T.);
#14824=ORIENTED_EDGE('',*,*,#9726,.F.);
#14825=ORIENTED_EDGE('',*,*,#9722,.T.);
#14826=ORIENTED_EDGE('',*,*,#9727,.F.);
#14827=ORIENTED_EDGE('',*,*,#9718,.T.);
#14828=ORIENTED_EDGE('',*,*,#9724,.T.);
#14829=ORIENTED_EDGE('',*,*,#9721,.T.);
#14830=ORIENTED_EDGE('',*,*,#9726,.T.);
#14831=ORIENTED_EDGE('',*,*,#9719,.T.);
#14832=ORIENTED_EDGE('',*,*,#9727,.T.);
#14833=ORIENTED_EDGE('',*,*,#9728,.T.);
#14834=ORIENTED_EDGE('',*,*,#9729,.T.);
#14835=ORIENTED_EDGE('',*,*,#9730,.F.);
#14836=ORIENTED_EDGE('',*,*,#9729,.F.);
#14837=ORIENTED_EDGE('',*,*,#9731,.F.);
#14838=ORIENTED_EDGE('',*,*,#9732,.T.);
#14839=ORIENTED_EDGE('',*,*,#9733,.T.);
#14840=ORIENTED_EDGE('',*,*,#9732,.F.);
#14841=ORIENTED_EDGE('',*,*,#9731,.T.);
#14842=ORIENTED_EDGE('',*,*,#9730,.T.);
#14843=ORIENTED_EDGE('',*,*,#9733,.F.);
#14844=ORIENTED_EDGE('',*,*,#9728,.F.);
#14845=ORIENTED_EDGE('',*,*,#9734,.F.);
#14846=ORIENTED_EDGE('',*,*,#9735,.F.);
#14847=ORIENTED_EDGE('',*,*,#9736,.F.);
#14848=ORIENTED_EDGE('',*,*,#9737,.F.);
#14849=ORIENTED_EDGE('',*,*,#9738,.T.);
#14850=ORIENTED_EDGE('',*,*,#9739,.F.);
#14851=ORIENTED_EDGE('',*,*,#9738,.F.);
#14852=ORIENTED_EDGE('',*,*,#9740,.F.);
#14853=ORIENTED_EDGE('',*,*,#9741,.F.);
#14854=ORIENTED_EDGE('',*,*,#9742,.F.);
#14855=ORIENTED_EDGE('',*,*,#9743,.F.);
#14856=ORIENTED_EDGE('',*,*,#9744,.F.);
#14857=ORIENTED_EDGE('',*,*,#9745,.T.);
#14858=ORIENTED_EDGE('',*,*,#9746,.F.);
#14859=ORIENTED_EDGE('',*,*,#9747,.F.);
#14860=ORIENTED_EDGE('',*,*,#9742,.T.);
#14861=ORIENTED_EDGE('',*,*,#9748,.T.);
#14862=ORIENTED_EDGE('',*,*,#9749,.F.);
#14863=ORIENTED_EDGE('',*,*,#9750,.F.);
#14864=ORIENTED_EDGE('',*,*,#9751,.F.);
#14865=ORIENTED_EDGE('',*,*,#9746,.T.);
#14866=ORIENTED_EDGE('',*,*,#9752,.T.);
#14867=ORIENTED_EDGE('',*,*,#9753,.F.);
#14868=ORIENTED_EDGE('',*,*,#9754,.F.);
#14869=ORIENTED_EDGE('',*,*,#9749,.T.);
#14870=ORIENTED_EDGE('',*,*,#9755,.T.);
#14871=ORIENTED_EDGE('',*,*,#9756,.T.);
#14872=ORIENTED_EDGE('',*,*,#9757,.F.);
#14873=ORIENTED_EDGE('',*,*,#9758,.F.);
#14874=ORIENTED_EDGE('',*,*,#9753,.T.);
#14875=ORIENTED_EDGE('',*,*,#9759,.T.);
#14876=ORIENTED_EDGE('',*,*,#9760,.T.);
#14877=ORIENTED_EDGE('',*,*,#9761,.F.);
#14878=ORIENTED_EDGE('',*,*,#9762,.F.);
#14879=ORIENTED_EDGE('',*,*,#9763,.F.);
#14880=ORIENTED_EDGE('',*,*,#9757,.T.);
#14881=ORIENTED_EDGE('',*,*,#9764,.T.);
#14882=ORIENTED_EDGE('',*,*,#9765,.F.);
#14883=ORIENTED_EDGE('',*,*,#9766,.F.);
#14884=ORIENTED_EDGE('',*,*,#9767,.F.);
#14885=ORIENTED_EDGE('',*,*,#9761,.T.);
#14886=ORIENTED_EDGE('',*,*,#9768,.T.);
#14887=ORIENTED_EDGE('',*,*,#9769,.T.);
#14888=ORIENTED_EDGE('',*,*,#9770,.F.);
#14889=ORIENTED_EDGE('',*,*,#9771,.F.);
#14890=ORIENTED_EDGE('',*,*,#9765,.T.);
#14891=ORIENTED_EDGE('',*,*,#9772,.T.);
#14892=ORIENTED_EDGE('',*,*,#9773,.F.);
#14893=ORIENTED_EDGE('',*,*,#9774,.F.);
#14894=ORIENTED_EDGE('',*,*,#9770,.T.);
#14895=ORIENTED_EDGE('',*,*,#9775,.T.);
#14896=ORIENTED_EDGE('',*,*,#9776,.F.);
#14897=ORIENTED_EDGE('',*,*,#9777,.F.);
#14898=ORIENTED_EDGE('',*,*,#9778,.F.);
#14899=ORIENTED_EDGE('',*,*,#9773,.T.);
#14900=ORIENTED_EDGE('',*,*,#9779,.T.);
#14901=ORIENTED_EDGE('',*,*,#9780,.T.);
#14902=ORIENTED_EDGE('',*,*,#9781,.F.);
#14903=ORIENTED_EDGE('',*,*,#9782,.F.);
#14904=ORIENTED_EDGE('',*,*,#9776,.T.);
#14905=ORIENTED_EDGE('',*,*,#9783,.T.);
#14906=ORIENTED_EDGE('',*,*,#9784,.T.);
#14907=ORIENTED_EDGE('',*,*,#9785,.F.);
#14908=ORIENTED_EDGE('',*,*,#9786,.F.);
#14909=ORIENTED_EDGE('',*,*,#9787,.F.);
#14910=ORIENTED_EDGE('',*,*,#9781,.T.);
#14911=ORIENTED_EDGE('',*,*,#9788,.T.);
#14912=ORIENTED_EDGE('',*,*,#9789,.F.);
#14913=ORIENTED_EDGE('',*,*,#9790,.F.);
#14914=ORIENTED_EDGE('',*,*,#9791,.F.);
#14915=ORIENTED_EDGE('',*,*,#9785,.T.);
#14916=ORIENTED_EDGE('',*,*,#9792,.T.);
#14917=ORIENTED_EDGE('',*,*,#9793,.F.);
#14918=ORIENTED_EDGE('',*,*,#9794,.F.);
#14919=ORIENTED_EDGE('',*,*,#9789,.T.);
#14920=ORIENTED_EDGE('',*,*,#9795,.T.);
#14921=ORIENTED_EDGE('',*,*,#9796,.T.);
#14922=ORIENTED_EDGE('',*,*,#9797,.F.);
#14923=ORIENTED_EDGE('',*,*,#9798,.F.);
#14924=ORIENTED_EDGE('',*,*,#9793,.T.);
#14925=ORIENTED_EDGE('',*,*,#9799,.T.);
#14926=ORIENTED_EDGE('',*,*,#9800,.F.);
#14927=ORIENTED_EDGE('',*,*,#9737,.T.);
#14928=ORIENTED_EDGE('',*,*,#9801,.F.);
#14929=ORIENTED_EDGE('',*,*,#9797,.T.);
#14930=ORIENTED_EDGE('',*,*,#9802,.T.);
#14931=ORIENTED_EDGE('',*,*,#9803,.T.);
#14932=ORIENTED_EDGE('',*,*,#9804,.T.);
#14933=ORIENTED_EDGE('',*,*,#9805,.T.);
#14934=ORIENTED_EDGE('',*,*,#9806,.T.);
#14935=ORIENTED_EDGE('',*,*,#9807,.T.);
#14936=ORIENTED_EDGE('',*,*,#9808,.T.);
#14937=ORIENTED_EDGE('',*,*,#9809,.T.);
#14938=ORIENTED_EDGE('',*,*,#9810,.T.);
#14939=ORIENTED_EDGE('',*,*,#9811,.T.);
#14940=ORIENTED_EDGE('',*,*,#9812,.T.);
#14941=ORIENTED_EDGE('',*,*,#9813,.T.);
#14942=ORIENTED_EDGE('',*,*,#9814,.T.);
#14943=ORIENTED_EDGE('',*,*,#9815,.T.);
#14944=ORIENTED_EDGE('',*,*,#9816,.T.);
#14945=ORIENTED_EDGE('',*,*,#9817,.T.);
#14946=ORIENTED_EDGE('',*,*,#9818,.T.);
#14947=ORIENTED_EDGE('',*,*,#9819,.T.);
#14948=ORIENTED_EDGE('',*,*,#9820,.T.);
#14949=ORIENTED_EDGE('',*,*,#9821,.T.);
#14950=ORIENTED_EDGE('',*,*,#9735,.T.);
#14951=ORIENTED_EDGE('',*,*,#9822,.T.);
#14952=ORIENTED_EDGE('',*,*,#9823,.T.);
#14953=ORIENTED_EDGE('',*,*,#9824,.T.);
#14954=ORIENTED_EDGE('',*,*,#9825,.T.);
#14955=ORIENTED_EDGE('',*,*,#9826,.T.);
#14956=ORIENTED_EDGE('',*,*,#9827,.T.);
#14957=ORIENTED_EDGE('',*,*,#9828,.T.);
#14958=ORIENTED_EDGE('',*,*,#9829,.T.);
#14959=ORIENTED_EDGE('',*,*,#9830,.T.);
#14960=ORIENTED_EDGE('',*,*,#9831,.T.);
#14961=ORIENTED_EDGE('',*,*,#9832,.T.);
#14962=ORIENTED_EDGE('',*,*,#9833,.T.);
#14963=ORIENTED_EDGE('',*,*,#9834,.T.);
#14964=ORIENTED_EDGE('',*,*,#9835,.T.);
#14965=ORIENTED_EDGE('',*,*,#9836,.T.);
#14966=ORIENTED_EDGE('',*,*,#9837,.T.);
#14967=ORIENTED_EDGE('',*,*,#9800,.T.);
#14968=ORIENTED_EDGE('',*,*,#9838,.T.);
#14969=ORIENTED_EDGE('',*,*,#9740,.T.);
#14970=ORIENTED_EDGE('',*,*,#9734,.T.);
#14971=ORIENTED_EDGE('',*,*,#9839,.F.);
#14972=ORIENTED_EDGE('',*,*,#9822,.F.);
#14973=ORIENTED_EDGE('',*,*,#9839,.T.);
#14974=ORIENTED_EDGE('',*,*,#9741,.T.);
#14975=ORIENTED_EDGE('',*,*,#9838,.F.);
#14976=ORIENTED_EDGE('',*,*,#9802,.F.);
#14977=ORIENTED_EDGE('',*,*,#9799,.F.);
#14978=ORIENTED_EDGE('',*,*,#9796,.F.);
#14979=ORIENTED_EDGE('',*,*,#9795,.F.);
#14980=ORIENTED_EDGE('',*,*,#9792,.F.);
#14981=ORIENTED_EDGE('',*,*,#9788,.F.);
#14982=ORIENTED_EDGE('',*,*,#9784,.F.);
#14983=ORIENTED_EDGE('',*,*,#9783,.F.);
#14984=ORIENTED_EDGE('',*,*,#9780,.F.);
#14985=ORIENTED_EDGE('',*,*,#9779,.F.);
#14986=ORIENTED_EDGE('',*,*,#9775,.F.);
#14987=ORIENTED_EDGE('',*,*,#9772,.F.);
#14988=ORIENTED_EDGE('',*,*,#9769,.F.);
#14989=ORIENTED_EDGE('',*,*,#9768,.F.);
#14990=ORIENTED_EDGE('',*,*,#9764,.F.);
#14991=ORIENTED_EDGE('',*,*,#9760,.F.);
#14992=ORIENTED_EDGE('',*,*,#9759,.F.);
#14993=ORIENTED_EDGE('',*,*,#9756,.F.);
#14994=ORIENTED_EDGE('',*,*,#9755,.F.);
#14995=ORIENTED_EDGE('',*,*,#9752,.F.);
#14996=ORIENTED_EDGE('',*,*,#9748,.F.);
#14997=ORIENTED_EDGE('',*,*,#9745,.F.);
#14998=ORIENTED_EDGE('',*,*,#9840,.F.);
#14999=ORIENTED_EDGE('',*,*,#9803,.F.);
#15000=ORIENTED_EDGE('',*,*,#9837,.F.);
#15001=ORIENTED_EDGE('',*,*,#9836,.F.);
#15002=ORIENTED_EDGE('',*,*,#9835,.F.);
#15003=ORIENTED_EDGE('',*,*,#9834,.F.);
#15004=ORIENTED_EDGE('',*,*,#9833,.F.);
#15005=ORIENTED_EDGE('',*,*,#9832,.F.);
#15006=ORIENTED_EDGE('',*,*,#9831,.F.);
#15007=ORIENTED_EDGE('',*,*,#9830,.F.);
#15008=ORIENTED_EDGE('',*,*,#9829,.F.);
#15009=ORIENTED_EDGE('',*,*,#9828,.F.);
#15010=ORIENTED_EDGE('',*,*,#9827,.F.);
#15011=ORIENTED_EDGE('',*,*,#9826,.F.);
#15012=ORIENTED_EDGE('',*,*,#9825,.F.);
#15013=ORIENTED_EDGE('',*,*,#9824,.F.);
#15014=ORIENTED_EDGE('',*,*,#9823,.F.);
#15015=ORIENTED_EDGE('',*,*,#9736,.T.);
#15016=ORIENTED_EDGE('',*,*,#9821,.F.);
#15017=ORIENTED_EDGE('',*,*,#9820,.F.);
#15018=ORIENTED_EDGE('',*,*,#9819,.F.);
#15019=ORIENTED_EDGE('',*,*,#9818,.F.);
#15020=ORIENTED_EDGE('',*,*,#9817,.F.);
#15021=ORIENTED_EDGE('',*,*,#9816,.F.);
#15022=ORIENTED_EDGE('',*,*,#9815,.F.);
#15023=ORIENTED_EDGE('',*,*,#9814,.F.);
#15024=ORIENTED_EDGE('',*,*,#9813,.F.);
#15025=ORIENTED_EDGE('',*,*,#9812,.F.);
#15026=ORIENTED_EDGE('',*,*,#9811,.F.);
#15027=ORIENTED_EDGE('',*,*,#9810,.F.);
#15028=ORIENTED_EDGE('',*,*,#9809,.F.);
#15029=ORIENTED_EDGE('',*,*,#9808,.F.);
#15030=ORIENTED_EDGE('',*,*,#9807,.F.);
#15031=ORIENTED_EDGE('',*,*,#9806,.F.);
#15032=ORIENTED_EDGE('',*,*,#9805,.F.);
#15033=ORIENTED_EDGE('',*,*,#9841,.F.);
#15034=ORIENTED_EDGE('',*,*,#9743,.T.);
#15035=ORIENTED_EDGE('',*,*,#9747,.T.);
#15036=ORIENTED_EDGE('',*,*,#9751,.T.);
#15037=ORIENTED_EDGE('',*,*,#9750,.T.);
#15038=ORIENTED_EDGE('',*,*,#9754,.T.);
#15039=ORIENTED_EDGE('',*,*,#9758,.T.);
#15040=ORIENTED_EDGE('',*,*,#9763,.T.);
#15041=ORIENTED_EDGE('',*,*,#9762,.T.);
#15042=ORIENTED_EDGE('',*,*,#9767,.T.);
#15043=ORIENTED_EDGE('',*,*,#9766,.T.);
#15044=ORIENTED_EDGE('',*,*,#9771,.T.);
#15045=ORIENTED_EDGE('',*,*,#9774,.T.);
#15046=ORIENTED_EDGE('',*,*,#9778,.T.);
#15047=ORIENTED_EDGE('',*,*,#9777,.T.);
#15048=ORIENTED_EDGE('',*,*,#9782,.T.);
#15049=ORIENTED_EDGE('',*,*,#9787,.T.);
#15050=ORIENTED_EDGE('',*,*,#9786,.T.);
#15051=ORIENTED_EDGE('',*,*,#9791,.T.);
#15052=ORIENTED_EDGE('',*,*,#9790,.T.);
#15053=ORIENTED_EDGE('',*,*,#9794,.T.);
#15054=ORIENTED_EDGE('',*,*,#9798,.T.);
#15055=ORIENTED_EDGE('',*,*,#9801,.T.);
#15056=ORIENTED_EDGE('',*,*,#9842,.F.);
#15057=ORIENTED_EDGE('',*,*,#9843,.T.);
#15058=ORIENTED_EDGE('',*,*,#9844,.T.);
#15059=ORIENTED_EDGE('',*,*,#9845,.F.);
#15060=ORIENTED_EDGE('',*,*,#9846,.F.);
#15061=ORIENTED_EDGE('',*,*,#9847,.T.);
#15062=ORIENTED_EDGE('',*,*,#9848,.T.);
#15063=ORIENTED_EDGE('',*,*,#9843,.F.);
#15064=ORIENTED_EDGE('',*,*,#9849,.F.);
#15065=ORIENTED_EDGE('',*,*,#9850,.T.);
#15066=ORIENTED_EDGE('',*,*,#9851,.T.);
#15067=ORIENTED_EDGE('',*,*,#9847,.F.);
#15068=ORIENTED_EDGE('',*,*,#9852,.F.);
#15069=ORIENTED_EDGE('',*,*,#9853,.T.);
#15070=ORIENTED_EDGE('',*,*,#9854,.T.);
#15071=ORIENTED_EDGE('',*,*,#9850,.F.);
#15072=ORIENTED_EDGE('',*,*,#9855,.F.);
#15073=ORIENTED_EDGE('',*,*,#9856,.T.);
#15074=ORIENTED_EDGE('',*,*,#9857,.T.);
#15075=ORIENTED_EDGE('',*,*,#9853,.F.);
#15076=ORIENTED_EDGE('',*,*,#9858,.F.);
#15077=ORIENTED_EDGE('',*,*,#9845,.T.);
#15078=ORIENTED_EDGE('',*,*,#9859,.T.);
#15079=ORIENTED_EDGE('',*,*,#9856,.F.);
#15080=ORIENTED_EDGE('',*,*,#9859,.F.);
#15081=ORIENTED_EDGE('',*,*,#9844,.F.);
#15082=ORIENTED_EDGE('',*,*,#9848,.F.);
#15083=ORIENTED_EDGE('',*,*,#9851,.F.);
#15084=ORIENTED_EDGE('',*,*,#9854,.F.);
#15085=ORIENTED_EDGE('',*,*,#9857,.F.);
#15086=ORIENTED_EDGE('',*,*,#9860,.T.);
#15087=ORIENTED_EDGE('',*,*,#9840,.T.);
#15088=ORIENTED_EDGE('',*,*,#9744,.T.);
#15089=ORIENTED_EDGE('',*,*,#9841,.T.);
#15090=ORIENTED_EDGE('',*,*,#9804,.F.);
#15091=ORIENTED_EDGE('',*,*,#9860,.F.);
#15092=ORIENTED_EDGE('',*,*,#9861,.T.);
#15093=ORIENTED_EDGE('',*,*,#9862,.T.);
#15094=ORIENTED_EDGE('',*,*,#9861,.F.);
#15095=ORIENTED_EDGE('',*,*,#9862,.F.);
#15096=ORIENTED_EDGE('',*,*,#9842,.T.);
#15097=ORIENTED_EDGE('',*,*,#9858,.T.);
#15098=ORIENTED_EDGE('',*,*,#9855,.T.);
#15099=ORIENTED_EDGE('',*,*,#9852,.T.);
#15100=ORIENTED_EDGE('',*,*,#9849,.T.);
#15101=ORIENTED_EDGE('',*,*,#9846,.T.);
#15102=ORIENTED_EDGE('',*,*,#9739,.T.);
#15103=ORIENTED_EDGE('',*,*,#9863,.F.);
#15104=ORIENTED_EDGE('',*,*,#9864,.F.);
#15105=ORIENTED_EDGE('',*,*,#9865,.F.);
#15106=ORIENTED_EDGE('',*,*,#9866,.F.);
#15107=ORIENTED_EDGE('',*,*,#9867,.T.);
#15108=ORIENTED_EDGE('',*,*,#9868,.F.);
#15109=ORIENTED_EDGE('',*,*,#9867,.F.);
#15110=ORIENTED_EDGE('',*,*,#9869,.F.);
#15111=ORIENTED_EDGE('',*,*,#9870,.F.);
#15112=ORIENTED_EDGE('',*,*,#9871,.F.);
#15113=ORIENTED_EDGE('',*,*,#9872,.F.);
#15114=ORIENTED_EDGE('',*,*,#9873,.F.);
#15115=ORIENTED_EDGE('',*,*,#9874,.T.);
#15116=ORIENTED_EDGE('',*,*,#9875,.F.);
#15117=ORIENTED_EDGE('',*,*,#9876,.F.);
#15118=ORIENTED_EDGE('',*,*,#9877,.F.);
#15119=ORIENTED_EDGE('',*,*,#9871,.T.);
#15120=ORIENTED_EDGE('',*,*,#9878,.T.);
#15121=ORIENTED_EDGE('',*,*,#9879,.T.);
#15122=ORIENTED_EDGE('',*,*,#9880,.F.);
#15123=ORIENTED_EDGE('',*,*,#9881,.F.);
#15124=ORIENTED_EDGE('',*,*,#9875,.T.);
#15125=ORIENTED_EDGE('',*,*,#9882,.T.);
#15126=ORIENTED_EDGE('',*,*,#9883,.F.);
#15127=ORIENTED_EDGE('',*,*,#9884,.F.);
#15128=ORIENTED_EDGE('',*,*,#9885,.F.);
#15129=ORIENTED_EDGE('',*,*,#9880,.T.);
#15130=ORIENTED_EDGE('',*,*,#9886,.T.);
#15131=ORIENTED_EDGE('',*,*,#9887,.T.);
#15132=ORIENTED_EDGE('',*,*,#9888,.F.);
#15133=ORIENTED_EDGE('',*,*,#9889,.F.);
#15134=ORIENTED_EDGE('',*,*,#9883,.T.);
#15135=ORIENTED_EDGE('',*,*,#9890,.T.);
#15136=ORIENTED_EDGE('',*,*,#9891,.F.);
#15137=ORIENTED_EDGE('',*,*,#9892,.F.);
#15138=ORIENTED_EDGE('',*,*,#9893,.F.);
#15139=ORIENTED_EDGE('',*,*,#9888,.T.);
#15140=ORIENTED_EDGE('',*,*,#9894,.T.);
#15141=ORIENTED_EDGE('',*,*,#9895,.T.);
#15142=ORIENTED_EDGE('',*,*,#9896,.F.);
#15143=ORIENTED_EDGE('',*,*,#9897,.F.);
#15144=ORIENTED_EDGE('',*,*,#9891,.T.);
#15145=ORIENTED_EDGE('',*,*,#9898,.T.);
#15146=ORIENTED_EDGE('',*,*,#9899,.F.);
#15147=ORIENTED_EDGE('',*,*,#9900,.F.);
#15148=ORIENTED_EDGE('',*,*,#9901,.F.);
#15149=ORIENTED_EDGE('',*,*,#9896,.T.);
#15150=ORIENTED_EDGE('',*,*,#9902,.T.);
#15151=ORIENTED_EDGE('',*,*,#9903,.T.);
#15152=ORIENTED_EDGE('',*,*,#9904,.F.);
#15153=ORIENTED_EDGE('',*,*,#9905,.F.);
#15154=ORIENTED_EDGE('',*,*,#9899,.T.);
#15155=ORIENTED_EDGE('',*,*,#9906,.T.);
#15156=ORIENTED_EDGE('',*,*,#9907,.T.);
#15157=ORIENTED_EDGE('',*,*,#9908,.F.);
#15158=ORIENTED_EDGE('',*,*,#9909,.F.);
#15159=ORIENTED_EDGE('',*,*,#9910,.F.);
#15160=ORIENTED_EDGE('',*,*,#9904,.T.);
#15161=ORIENTED_EDGE('',*,*,#9911,.T.);
#15162=ORIENTED_EDGE('',*,*,#9912,.F.);
#15163=ORIENTED_EDGE('',*,*,#9913,.F.);
#15164=ORIENTED_EDGE('',*,*,#9914,.F.);
#15165=ORIENTED_EDGE('',*,*,#9908,.T.);
#15166=ORIENTED_EDGE('',*,*,#9915,.T.);
#15167=ORIENTED_EDGE('',*,*,#9916,.T.);
#15168=ORIENTED_EDGE('',*,*,#9917,.F.);
#15169=ORIENTED_EDGE('',*,*,#9918,.F.);
#15170=ORIENTED_EDGE('',*,*,#9912,.T.);
#15171=ORIENTED_EDGE('',*,*,#9919,.T.);
#15172=ORIENTED_EDGE('',*,*,#9920,.F.);
#15173=ORIENTED_EDGE('',*,*,#9921,.F.);
#15174=ORIENTED_EDGE('',*,*,#9922,.F.);
#15175=ORIENTED_EDGE('',*,*,#9917,.T.);
#15176=ORIENTED_EDGE('',*,*,#9923,.T.);
#15177=ORIENTED_EDGE('',*,*,#9924,.T.);
#15178=ORIENTED_EDGE('',*,*,#9925,.F.);
#15179=ORIENTED_EDGE('',*,*,#9926,.F.);
#15180=ORIENTED_EDGE('',*,*,#9927,.F.);
#15181=ORIENTED_EDGE('',*,*,#9920,.T.);
#15182=ORIENTED_EDGE('',*,*,#9928,.T.);
#15183=ORIENTED_EDGE('',*,*,#9929,.F.);
#15184=ORIENTED_EDGE('',*,*,#9930,.F.);
#15185=ORIENTED_EDGE('',*,*,#9925,.T.);
#15186=ORIENTED_EDGE('',*,*,#9931,.T.);
#15187=ORIENTED_EDGE('',*,*,#9932,.T.);
#15188=ORIENTED_EDGE('',*,*,#9933,.F.);
#15189=ORIENTED_EDGE('',*,*,#9934,.F.);
#15190=ORIENTED_EDGE('',*,*,#9935,.F.);
#15191=ORIENTED_EDGE('',*,*,#9929,.T.);
#15192=ORIENTED_EDGE('',*,*,#9936,.T.);
#15193=ORIENTED_EDGE('',*,*,#9937,.F.);
#15194=ORIENTED_EDGE('',*,*,#9938,.F.);
#15195=ORIENTED_EDGE('',*,*,#9933,.T.);
#15196=ORIENTED_EDGE('',*,*,#9939,.T.);
#15197=ORIENTED_EDGE('',*,*,#9940,.T.);
#15198=ORIENTED_EDGE('',*,*,#9941,.F.);
#15199=ORIENTED_EDGE('',*,*,#9942,.F.);
#15200=ORIENTED_EDGE('',*,*,#9943,.F.);
#15201=ORIENTED_EDGE('',*,*,#9937,.T.);
#15202=ORIENTED_EDGE('',*,*,#9944,.T.);
#15203=ORIENTED_EDGE('',*,*,#9945,.T.);
#15204=ORIENTED_EDGE('',*,*,#9946,.F.);
#15205=ORIENTED_EDGE('',*,*,#9947,.F.);
#15206=ORIENTED_EDGE('',*,*,#9941,.T.);
#15207=ORIENTED_EDGE('',*,*,#9948,.T.);
#15208=ORIENTED_EDGE('',*,*,#9949,.T.);
#15209=ORIENTED_EDGE('',*,*,#9950,.F.);
#15210=ORIENTED_EDGE('',*,*,#9951,.F.);
#15211=ORIENTED_EDGE('',*,*,#9952,.F.);
#15212=ORIENTED_EDGE('',*,*,#9946,.T.);
#15213=ORIENTED_EDGE('',*,*,#9953,.T.);
#15214=ORIENTED_EDGE('',*,*,#9954,.F.);
#15215=ORIENTED_EDGE('',*,*,#9955,.F.);
#15216=ORIENTED_EDGE('',*,*,#9950,.T.);
#15217=ORIENTED_EDGE('',*,*,#9956,.T.);
#15218=ORIENTED_EDGE('',*,*,#9957,.T.);
#15219=ORIENTED_EDGE('',*,*,#9958,.F.);
#15220=ORIENTED_EDGE('',*,*,#9959,.F.);
#15221=ORIENTED_EDGE('',*,*,#9960,.F.);
#15222=ORIENTED_EDGE('',*,*,#9954,.T.);
#15223=ORIENTED_EDGE('',*,*,#9961,.T.);
#15224=ORIENTED_EDGE('',*,*,#9962,.F.);
#15225=ORIENTED_EDGE('',*,*,#9963,.F.);
#15226=ORIENTED_EDGE('',*,*,#9958,.T.);
#15227=ORIENTED_EDGE('',*,*,#9964,.T.);
#15228=ORIENTED_EDGE('',*,*,#9965,.T.);
#15229=ORIENTED_EDGE('',*,*,#9966,.F.);
#15230=ORIENTED_EDGE('',*,*,#9967,.F.);
#15231=ORIENTED_EDGE('',*,*,#9968,.F.);
#15232=ORIENTED_EDGE('',*,*,#9962,.T.);
#15233=ORIENTED_EDGE('',*,*,#9969,.T.);
#15234=ORIENTED_EDGE('',*,*,#9970,.F.);
#15235=ORIENTED_EDGE('',*,*,#9971,.F.);
#15236=ORIENTED_EDGE('',*,*,#9966,.T.);
#15237=ORIENTED_EDGE('',*,*,#9972,.T.);
#15238=ORIENTED_EDGE('',*,*,#9973,.T.);
#15239=ORIENTED_EDGE('',*,*,#9974,.F.);
#15240=ORIENTED_EDGE('',*,*,#9975,.F.);
#15241=ORIENTED_EDGE('',*,*,#9976,.F.);
#15242=ORIENTED_EDGE('',*,*,#9970,.T.);
#15243=ORIENTED_EDGE('',*,*,#9977,.T.);
#15244=ORIENTED_EDGE('',*,*,#9978,.F.);
#15245=ORIENTED_EDGE('',*,*,#9979,.F.);
#15246=ORIENTED_EDGE('',*,*,#9974,.T.);
#15247=ORIENTED_EDGE('',*,*,#9980,.T.);
#15248=ORIENTED_EDGE('',*,*,#9981,.T.);
#15249=ORIENTED_EDGE('',*,*,#9982,.F.);
#15250=ORIENTED_EDGE('',*,*,#9983,.F.);
#15251=ORIENTED_EDGE('',*,*,#9984,.F.);
#15252=ORIENTED_EDGE('',*,*,#9978,.T.);
#15253=ORIENTED_EDGE('',*,*,#9985,.T.);
#15254=ORIENTED_EDGE('',*,*,#9986,.T.);
#15255=ORIENTED_EDGE('',*,*,#9987,.T.);
#15256=ORIENTED_EDGE('',*,*,#9988,.T.);
#15257=ORIENTED_EDGE('',*,*,#9989,.T.);
#15258=ORIENTED_EDGE('',*,*,#9990,.T.);
#15259=ORIENTED_EDGE('',*,*,#9991,.T.);
#15260=ORIENTED_EDGE('',*,*,#9992,.T.);
#15261=ORIENTED_EDGE('',*,*,#9993,.T.);
#15262=ORIENTED_EDGE('',*,*,#9994,.T.);
#15263=ORIENTED_EDGE('',*,*,#9995,.T.);
#15264=ORIENTED_EDGE('',*,*,#9996,.T.);
#15265=ORIENTED_EDGE('',*,*,#9997,.T.);
#15266=ORIENTED_EDGE('',*,*,#9998,.T.);
#15267=ORIENTED_EDGE('',*,*,#9999,.T.);
#15268=ORIENTED_EDGE('',*,*,#10000,.T.);
#15269=ORIENTED_EDGE('',*,*,#10001,.T.);
#15270=ORIENTED_EDGE('',*,*,#10002,.T.);
#15271=ORIENTED_EDGE('',*,*,#10003,.T.);
#15272=ORIENTED_EDGE('',*,*,#10004,.T.);
#15273=ORIENTED_EDGE('',*,*,#10005,.T.);
#15274=ORIENTED_EDGE('',*,*,#10006,.T.);
#15275=ORIENTED_EDGE('',*,*,#10007,.T.);
#15276=ORIENTED_EDGE('',*,*,#10008,.T.);
#15277=ORIENTED_EDGE('',*,*,#10009,.T.);
#15278=ORIENTED_EDGE('',*,*,#10010,.T.);
#15279=ORIENTED_EDGE('',*,*,#10011,.T.);
#15280=ORIENTED_EDGE('',*,*,#10012,.T.);
#15281=ORIENTED_EDGE('',*,*,#10013,.T.);
#15282=ORIENTED_EDGE('',*,*,#10014,.T.);
#15283=ORIENTED_EDGE('',*,*,#10015,.T.);
#15284=ORIENTED_EDGE('',*,*,#10016,.T.);
#15285=ORIENTED_EDGE('',*,*,#10017,.T.);
#15286=ORIENTED_EDGE('',*,*,#9864,.T.);
#15287=ORIENTED_EDGE('',*,*,#10018,.T.);
#15288=ORIENTED_EDGE('',*,*,#10019,.T.);
#15289=ORIENTED_EDGE('',*,*,#10020,.T.);
#15290=ORIENTED_EDGE('',*,*,#10021,.T.);
#15291=ORIENTED_EDGE('',*,*,#10022,.T.);
#15292=ORIENTED_EDGE('',*,*,#10023,.T.);
#15293=ORIENTED_EDGE('',*,*,#10024,.T.);
#15294=ORIENTED_EDGE('',*,*,#10025,.T.);
#15295=ORIENTED_EDGE('',*,*,#10026,.T.);
#15296=ORIENTED_EDGE('',*,*,#10027,.T.);
#15297=ORIENTED_EDGE('',*,*,#10028,.T.);
#15298=ORIENTED_EDGE('',*,*,#10029,.T.);
#15299=ORIENTED_EDGE('',*,*,#10030,.T.);
#15300=ORIENTED_EDGE('',*,*,#10031,.T.);
#15301=ORIENTED_EDGE('',*,*,#10032,.T.);
#15302=ORIENTED_EDGE('',*,*,#10033,.T.);
#15303=ORIENTED_EDGE('',*,*,#10034,.T.);
#15304=ORIENTED_EDGE('',*,*,#10035,.T.);
#15305=ORIENTED_EDGE('',*,*,#10036,.T.);
#15306=ORIENTED_EDGE('',*,*,#10037,.T.);
#15307=ORIENTED_EDGE('',*,*,#10038,.T.);
#15308=ORIENTED_EDGE('',*,*,#10039,.T.);
#15309=ORIENTED_EDGE('',*,*,#10040,.T.);
#15310=ORIENTED_EDGE('',*,*,#10041,.T.);
#15311=ORIENTED_EDGE('',*,*,#10042,.T.);
#15312=ORIENTED_EDGE('',*,*,#10043,.T.);
#15313=ORIENTED_EDGE('',*,*,#10044,.T.);
#15314=ORIENTED_EDGE('',*,*,#10045,.T.);
#15315=ORIENTED_EDGE('',*,*,#9982,.T.);
#15316=ORIENTED_EDGE('',*,*,#10046,.T.);
#15317=ORIENTED_EDGE('',*,*,#10047,.T.);
#15318=ORIENTED_EDGE('',*,*,#9869,.T.);
#15319=ORIENTED_EDGE('',*,*,#9866,.T.);
#15320=ORIENTED_EDGE('',*,*,#10048,.F.);
#15321=ORIENTED_EDGE('',*,*,#9863,.T.);
#15322=ORIENTED_EDGE('',*,*,#10049,.F.);
#15323=ORIENTED_EDGE('',*,*,#10018,.F.);
#15324=ORIENTED_EDGE('',*,*,#10049,.T.);
#15325=ORIENTED_EDGE('',*,*,#9870,.T.);
#15326=ORIENTED_EDGE('',*,*,#10047,.F.);
#15327=ORIENTED_EDGE('',*,*,#10046,.F.);
#15328=ORIENTED_EDGE('',*,*,#9986,.F.);
#15329=ORIENTED_EDGE('',*,*,#9985,.F.);
#15330=ORIENTED_EDGE('',*,*,#9981,.F.);
#15331=ORIENTED_EDGE('',*,*,#9980,.F.);
#15332=ORIENTED_EDGE('',*,*,#9977,.F.);
#15333=ORIENTED_EDGE('',*,*,#9973,.F.);
#15334=ORIENTED_EDGE('',*,*,#9972,.F.);
#15335=ORIENTED_EDGE('',*,*,#9969,.F.);
#15336=ORIENTED_EDGE('',*,*,#9965,.F.);
#15337=ORIENTED_EDGE('',*,*,#9964,.F.);
#15338=ORIENTED_EDGE('',*,*,#9961,.F.);
#15339=ORIENTED_EDGE('',*,*,#9957,.F.);
#15340=ORIENTED_EDGE('',*,*,#9956,.F.);
#15341=ORIENTED_EDGE('',*,*,#9953,.F.);
#15342=ORIENTED_EDGE('',*,*,#9949,.F.);
#15343=ORIENTED_EDGE('',*,*,#9948,.F.);
#15344=ORIENTED_EDGE('',*,*,#9945,.F.);
#15345=ORIENTED_EDGE('',*,*,#9944,.F.);
#15346=ORIENTED_EDGE('',*,*,#9940,.F.);
#15347=ORIENTED_EDGE('',*,*,#9939,.F.);
#15348=ORIENTED_EDGE('',*,*,#9936,.F.);
#15349=ORIENTED_EDGE('',*,*,#9932,.F.);
#15350=ORIENTED_EDGE('',*,*,#9931,.F.);
#15351=ORIENTED_EDGE('',*,*,#9928,.F.);
#15352=ORIENTED_EDGE('',*,*,#9924,.F.);
#15353=ORIENTED_EDGE('',*,*,#9923,.F.);
#15354=ORIENTED_EDGE('',*,*,#9919,.F.);
#15355=ORIENTED_EDGE('',*,*,#9916,.F.);
#15356=ORIENTED_EDGE('',*,*,#9915,.F.);
#15357=ORIENTED_EDGE('',*,*,#9911,.F.);
#15358=ORIENTED_EDGE('',*,*,#9907,.F.);
#15359=ORIENTED_EDGE('',*,*,#9906,.F.);
#15360=ORIENTED_EDGE('',*,*,#9903,.F.);
#15361=ORIENTED_EDGE('',*,*,#9902,.F.);
#15362=ORIENTED_EDGE('',*,*,#9898,.F.);
#15363=ORIENTED_EDGE('',*,*,#9895,.F.);
#15364=ORIENTED_EDGE('',*,*,#9894,.F.);
#15365=ORIENTED_EDGE('',*,*,#9890,.F.);
#15366=ORIENTED_EDGE('',*,*,#9887,.F.);
#15367=ORIENTED_EDGE('',*,*,#9886,.F.);
#15368=ORIENTED_EDGE('',*,*,#9882,.F.);
#15369=ORIENTED_EDGE('',*,*,#9879,.F.);
#15370=ORIENTED_EDGE('',*,*,#9878,.F.);
#15371=ORIENTED_EDGE('',*,*,#9874,.F.);
#15372=ORIENTED_EDGE('',*,*,#10050,.F.);
#15373=ORIENTED_EDGE('',*,*,#9987,.F.);
#15374=ORIENTED_EDGE('',*,*,#10045,.F.);
#15375=ORIENTED_EDGE('',*,*,#10044,.F.);
#15376=ORIENTED_EDGE('',*,*,#10043,.F.);
#15377=ORIENTED_EDGE('',*,*,#10042,.F.);
#15378=ORIENTED_EDGE('',*,*,#10041,.F.);
#15379=ORIENTED_EDGE('',*,*,#10040,.F.);
#15380=ORIENTED_EDGE('',*,*,#10039,.F.);
#15381=ORIENTED_EDGE('',*,*,#10038,.F.);
#15382=ORIENTED_EDGE('',*,*,#10037,.F.);
#15383=ORIENTED_EDGE('',*,*,#10036,.F.);
#15384=ORIENTED_EDGE('',*,*,#10035,.F.);
#15385=ORIENTED_EDGE('',*,*,#10034,.F.);
#15386=ORIENTED_EDGE('',*,*,#10033,.F.);
#15387=ORIENTED_EDGE('',*,*,#10032,.F.);
#15388=ORIENTED_EDGE('',*,*,#10031,.F.);
#15389=ORIENTED_EDGE('',*,*,#10030,.F.);
#15390=ORIENTED_EDGE('',*,*,#10029,.F.);
#15391=ORIENTED_EDGE('',*,*,#10028,.F.);
#15392=ORIENTED_EDGE('',*,*,#10027,.F.);
#15393=ORIENTED_EDGE('',*,*,#10026,.F.);
#15394=ORIENTED_EDGE('',*,*,#10025,.F.);
#15395=ORIENTED_EDGE('',*,*,#10024,.F.);
#15396=ORIENTED_EDGE('',*,*,#10023,.F.);
#15397=ORIENTED_EDGE('',*,*,#10022,.F.);
#15398=ORIENTED_EDGE('',*,*,#10021,.F.);
#15399=ORIENTED_EDGE('',*,*,#10020,.F.);
#15400=ORIENTED_EDGE('',*,*,#10019,.F.);
#15401=ORIENTED_EDGE('',*,*,#9865,.T.);
#15402=ORIENTED_EDGE('',*,*,#10017,.F.);
#15403=ORIENTED_EDGE('',*,*,#10016,.F.);
#15404=ORIENTED_EDGE('',*,*,#10015,.F.);
#15405=ORIENTED_EDGE('',*,*,#10014,.F.);
#15406=ORIENTED_EDGE('',*,*,#10013,.F.);
#15407=ORIENTED_EDGE('',*,*,#10012,.F.);
#15408=ORIENTED_EDGE('',*,*,#10011,.F.);
#15409=ORIENTED_EDGE('',*,*,#10010,.F.);
#15410=ORIENTED_EDGE('',*,*,#10009,.F.);
#15411=ORIENTED_EDGE('',*,*,#10008,.F.);
#15412=ORIENTED_EDGE('',*,*,#10007,.F.);
#15413=ORIENTED_EDGE('',*,*,#10006,.F.);
#15414=ORIENTED_EDGE('',*,*,#10005,.F.);
#15415=ORIENTED_EDGE('',*,*,#10004,.F.);
#15416=ORIENTED_EDGE('',*,*,#10003,.F.);
#15417=ORIENTED_EDGE('',*,*,#10002,.F.);
#15418=ORIENTED_EDGE('',*,*,#10001,.F.);
#15419=ORIENTED_EDGE('',*,*,#10000,.F.);
#15420=ORIENTED_EDGE('',*,*,#9999,.F.);
#15421=ORIENTED_EDGE('',*,*,#9998,.F.);
#15422=ORIENTED_EDGE('',*,*,#9997,.F.);
#15423=ORIENTED_EDGE('',*,*,#9996,.F.);
#15424=ORIENTED_EDGE('',*,*,#9995,.F.);
#15425=ORIENTED_EDGE('',*,*,#9994,.F.);
#15426=ORIENTED_EDGE('',*,*,#9993,.F.);
#15427=ORIENTED_EDGE('',*,*,#9992,.F.);
#15428=ORIENTED_EDGE('',*,*,#9991,.F.);
#15429=ORIENTED_EDGE('',*,*,#9990,.F.);
#15430=ORIENTED_EDGE('',*,*,#9989,.F.);
#15431=ORIENTED_EDGE('',*,*,#10051,.F.);
#15432=ORIENTED_EDGE('',*,*,#9872,.T.);
#15433=ORIENTED_EDGE('',*,*,#9877,.T.);
#15434=ORIENTED_EDGE('',*,*,#9876,.T.);
#15435=ORIENTED_EDGE('',*,*,#9881,.T.);
#15436=ORIENTED_EDGE('',*,*,#9885,.T.);
#15437=ORIENTED_EDGE('',*,*,#9884,.T.);
#15438=ORIENTED_EDGE('',*,*,#9889,.T.);
#15439=ORIENTED_EDGE('',*,*,#9893,.T.);
#15440=ORIENTED_EDGE('',*,*,#9892,.T.);
#15441=ORIENTED_EDGE('',*,*,#9897,.T.);
#15442=ORIENTED_EDGE('',*,*,#9901,.T.);
#15443=ORIENTED_EDGE('',*,*,#9900,.T.);
#15444=ORIENTED_EDGE('',*,*,#9905,.T.);
#15445=ORIENTED_EDGE('',*,*,#9910,.T.);
#15446=ORIENTED_EDGE('',*,*,#9909,.T.);
#15447=ORIENTED_EDGE('',*,*,#9914,.T.);
#15448=ORIENTED_EDGE('',*,*,#9913,.T.);
#15449=ORIENTED_EDGE('',*,*,#9918,.T.);
#15450=ORIENTED_EDGE('',*,*,#9922,.T.);
#15451=ORIENTED_EDGE('',*,*,#9921,.T.);
#15452=ORIENTED_EDGE('',*,*,#9927,.T.);
#15453=ORIENTED_EDGE('',*,*,#9926,.T.);
#15454=ORIENTED_EDGE('',*,*,#9930,.T.);
#15455=ORIENTED_EDGE('',*,*,#9935,.T.);
#15456=ORIENTED_EDGE('',*,*,#9934,.T.);
#15457=ORIENTED_EDGE('',*,*,#9938,.T.);
#15458=ORIENTED_EDGE('',*,*,#9943,.T.);
#15459=ORIENTED_EDGE('',*,*,#9942,.T.);
#15460=ORIENTED_EDGE('',*,*,#9947,.T.);
#15461=ORIENTED_EDGE('',*,*,#9952,.T.);
#15462=ORIENTED_EDGE('',*,*,#9951,.T.);
#15463=ORIENTED_EDGE('',*,*,#9955,.T.);
#15464=ORIENTED_EDGE('',*,*,#9960,.T.);
#15465=ORIENTED_EDGE('',*,*,#9959,.T.);
#15466=ORIENTED_EDGE('',*,*,#9963,.T.);
#15467=ORIENTED_EDGE('',*,*,#9968,.T.);
#15468=ORIENTED_EDGE('',*,*,#9967,.T.);
#15469=ORIENTED_EDGE('',*,*,#9971,.T.);
#15470=ORIENTED_EDGE('',*,*,#9976,.T.);
#15471=ORIENTED_EDGE('',*,*,#9975,.T.);
#15472=ORIENTED_EDGE('',*,*,#9979,.T.);
#15473=ORIENTED_EDGE('',*,*,#9984,.T.);
#15474=ORIENTED_EDGE('',*,*,#9983,.T.);
#15475=ORIENTED_EDGE('',*,*,#10048,.T.);
#15476=ORIENTED_EDGE('',*,*,#10052,.F.);
#15477=ORIENTED_EDGE('',*,*,#10053,.T.);
#15478=ORIENTED_EDGE('',*,*,#10054,.T.);
#15479=ORIENTED_EDGE('',*,*,#10055,.F.);
#15480=ORIENTED_EDGE('',*,*,#10056,.F.);
#15481=ORIENTED_EDGE('',*,*,#10057,.T.);
#15482=ORIENTED_EDGE('',*,*,#10058,.T.);
#15483=ORIENTED_EDGE('',*,*,#10053,.F.);
#15484=ORIENTED_EDGE('',*,*,#10059,.F.);
#15485=ORIENTED_EDGE('',*,*,#10060,.T.);
#15486=ORIENTED_EDGE('',*,*,#10061,.T.);
#15487=ORIENTED_EDGE('',*,*,#10057,.F.);
#15488=ORIENTED_EDGE('',*,*,#10062,.F.);
#15489=ORIENTED_EDGE('',*,*,#10063,.T.);
#15490=ORIENTED_EDGE('',*,*,#10064,.T.);
#15491=ORIENTED_EDGE('',*,*,#10060,.F.);
#15492=ORIENTED_EDGE('',*,*,#10065,.F.);
#15493=ORIENTED_EDGE('',*,*,#10066,.T.);
#15494=ORIENTED_EDGE('',*,*,#10067,.T.);
#15495=ORIENTED_EDGE('',*,*,#10063,.F.);
#15496=ORIENTED_EDGE('',*,*,#10068,.F.);
#15497=ORIENTED_EDGE('',*,*,#10055,.T.);
#15498=ORIENTED_EDGE('',*,*,#10069,.T.);
#15499=ORIENTED_EDGE('',*,*,#10066,.F.);
#15500=ORIENTED_EDGE('',*,*,#10069,.F.);
#15501=ORIENTED_EDGE('',*,*,#10054,.F.);
#15502=ORIENTED_EDGE('',*,*,#10058,.F.);
#15503=ORIENTED_EDGE('',*,*,#10061,.F.);
#15504=ORIENTED_EDGE('',*,*,#10064,.F.);
#15505=ORIENTED_EDGE('',*,*,#10067,.F.);
#15506=ORIENTED_EDGE('',*,*,#10070,.T.);
#15507=ORIENTED_EDGE('',*,*,#10050,.T.);
#15508=ORIENTED_EDGE('',*,*,#9873,.T.);
#15509=ORIENTED_EDGE('',*,*,#10051,.T.);
#15510=ORIENTED_EDGE('',*,*,#9988,.F.);
#15511=ORIENTED_EDGE('',*,*,#10070,.F.);
#15512=ORIENTED_EDGE('',*,*,#10071,.T.);
#15513=ORIENTED_EDGE('',*,*,#10072,.T.);
#15514=ORIENTED_EDGE('',*,*,#10071,.F.);
#15515=ORIENTED_EDGE('',*,*,#10072,.F.);
#15516=ORIENTED_EDGE('',*,*,#10052,.T.);
#15517=ORIENTED_EDGE('',*,*,#10068,.T.);
#15518=ORIENTED_EDGE('',*,*,#10065,.T.);
#15519=ORIENTED_EDGE('',*,*,#10062,.T.);
#15520=ORIENTED_EDGE('',*,*,#10059,.T.);
#15521=ORIENTED_EDGE('',*,*,#10056,.T.);
#15522=ORIENTED_EDGE('',*,*,#9868,.T.);
#15523=ORIENTED_EDGE('',*,*,#10073,.T.);
#15524=ORIENTED_EDGE('',*,*,#10074,.T.);
#15525=ORIENTED_EDGE('',*,*,#10075,.T.);
#15526=ORIENTED_EDGE('',*,*,#10076,.T.);
#15527=ORIENTED_EDGE('',*,*,#10077,.T.);
#15528=ORIENTED_EDGE('',*,*,#10078,.T.);
#15529=ORIENTED_EDGE('',*,*,#10079,.T.);
#15530=ORIENTED_EDGE('',*,*,#10080,.T.);
#15531=ORIENTED_EDGE('',*,*,#10081,.T.);
#15532=ORIENTED_EDGE('',*,*,#10082,.T.);
#15533=ORIENTED_EDGE('',*,*,#10083,.T.);
#15534=ORIENTED_EDGE('',*,*,#10084,.T.);
#15535=ORIENTED_EDGE('',*,*,#10085,.T.);
#15536=ORIENTED_EDGE('',*,*,#10086,.T.);
#15537=ORIENTED_EDGE('',*,*,#10087,.T.);
#15538=ORIENTED_EDGE('',*,*,#10088,.T.);
#15539=ORIENTED_EDGE('',*,*,#10089,.T.);
#15540=ORIENTED_EDGE('',*,*,#10090,.T.);
#15541=ORIENTED_EDGE('',*,*,#10091,.T.);
#15542=ORIENTED_EDGE('',*,*,#10092,.T.);
#15543=ORIENTED_EDGE('',*,*,#10093,.T.);
#15544=ORIENTED_EDGE('',*,*,#10094,.T.);
#15545=ORIENTED_EDGE('',*,*,#10095,.T.);
#15546=ORIENTED_EDGE('',*,*,#10096,.T.);
#15547=ORIENTED_EDGE('',*,*,#10097,.T.);
#15548=ORIENTED_EDGE('',*,*,#10098,.T.);
#15549=ORIENTED_EDGE('',*,*,#10099,.T.);
#15550=ORIENTED_EDGE('',*,*,#10100,.T.);
#15551=ORIENTED_EDGE('',*,*,#10101,.T.);
#15552=ORIENTED_EDGE('',*,*,#10102,.T.);
#15553=ORIENTED_EDGE('',*,*,#10103,.T.);
#15554=ORIENTED_EDGE('',*,*,#10104,.T.);
#15555=ORIENTED_EDGE('',*,*,#10105,.T.);
#15556=ORIENTED_EDGE('',*,*,#10106,.T.);
#15557=ORIENTED_EDGE('',*,*,#10107,.T.);
#15558=ORIENTED_EDGE('',*,*,#10108,.T.);
#15559=ORIENTED_EDGE('',*,*,#10109,.T.);
#15560=ORIENTED_EDGE('',*,*,#10110,.T.);
#15561=ORIENTED_EDGE('',*,*,#10111,.F.);
#15562=ORIENTED_EDGE('',*,*,#10112,.F.);
#15563=ORIENTED_EDGE('',*,*,#10113,.F.);
#15564=ORIENTED_EDGE('',*,*,#10114,.F.);
#15565=ORIENTED_EDGE('',*,*,#10115,.F.);
#15566=ORIENTED_EDGE('',*,*,#10116,.F.);
#15567=ORIENTED_EDGE('',*,*,#10117,.F.);
#15568=ORIENTED_EDGE('',*,*,#10118,.F.);
#15569=ORIENTED_EDGE('',*,*,#10119,.F.);
#15570=ORIENTED_EDGE('',*,*,#10120,.F.);
#15571=ORIENTED_EDGE('',*,*,#10121,.F.);
#15572=ORIENTED_EDGE('',*,*,#10122,.F.);
#15573=ORIENTED_EDGE('',*,*,#10123,.T.);
#15574=ORIENTED_EDGE('',*,*,#10124,.T.);
#15575=ORIENTED_EDGE('',*,*,#10125,.T.);
#15576=ORIENTED_EDGE('',*,*,#10126,.T.);
#15577=ORIENTED_EDGE('',*,*,#10127,.T.);
#15578=ORIENTED_EDGE('',*,*,#10128,.T.);
#15579=ORIENTED_EDGE('',*,*,#10129,.T.);
#15580=ORIENTED_EDGE('',*,*,#10130,.T.);
#15581=ORIENTED_EDGE('',*,*,#10131,.T.);
#15582=ORIENTED_EDGE('',*,*,#10132,.F.);
#15583=ORIENTED_EDGE('',*,*,#10110,.F.);
#15584=ORIENTED_EDGE('',*,*,#10133,.F.);
#15585=ORIENTED_EDGE('',*,*,#10092,.F.);
#15586=ORIENTED_EDGE('',*,*,#10134,.F.);
#15587=ORIENTED_EDGE('',*,*,#10135,.T.);
#15588=ORIENTED_EDGE('',*,*,#10136,.F.);
#15589=ORIENTED_EDGE('',*,*,#10135,.F.);
#15590=ORIENTED_EDGE('',*,*,#10137,.F.);
#15591=ORIENTED_EDGE('',*,*,#10133,.T.);
#15592=ORIENTED_EDGE('',*,*,#10109,.F.);
#15593=ORIENTED_EDGE('',*,*,#10131,.F.);
#15594=ORIENTED_EDGE('',*,*,#10130,.F.);
#15595=ORIENTED_EDGE('',*,*,#10129,.F.);
#15596=ORIENTED_EDGE('',*,*,#10128,.F.);
#15597=ORIENTED_EDGE('',*,*,#10127,.F.);
#15598=ORIENTED_EDGE('',*,*,#10126,.F.);
#15599=ORIENTED_EDGE('',*,*,#10125,.F.);
#15600=ORIENTED_EDGE('',*,*,#10124,.F.);
#15601=ORIENTED_EDGE('',*,*,#10123,.F.);
#15602=ORIENTED_EDGE('',*,*,#10138,.F.);
#15603=ORIENTED_EDGE('',*,*,#10073,.F.);
#15604=ORIENTED_EDGE('',*,*,#10108,.F.);
#15605=ORIENTED_EDGE('',*,*,#10107,.F.);
#15606=ORIENTED_EDGE('',*,*,#10106,.F.);
#15607=ORIENTED_EDGE('',*,*,#10105,.F.);
#15608=ORIENTED_EDGE('',*,*,#10104,.F.);
#15609=ORIENTED_EDGE('',*,*,#10103,.F.);
#15610=ORIENTED_EDGE('',*,*,#10102,.F.);
#15611=ORIENTED_EDGE('',*,*,#10101,.F.);
#15612=ORIENTED_EDGE('',*,*,#10100,.F.);
#15613=ORIENTED_EDGE('',*,*,#10099,.F.);
#15614=ORIENTED_EDGE('',*,*,#10098,.F.);
#15615=ORIENTED_EDGE('',*,*,#10097,.F.);
#15616=ORIENTED_EDGE('',*,*,#10096,.F.);
#15617=ORIENTED_EDGE('',*,*,#10095,.F.);
#15618=ORIENTED_EDGE('',*,*,#10094,.F.);
#15619=ORIENTED_EDGE('',*,*,#10093,.F.);
#15620=ORIENTED_EDGE('',*,*,#10132,.T.);
#15621=ORIENTED_EDGE('',*,*,#10137,.T.);
#15622=ORIENTED_EDGE('',*,*,#10134,.T.);
#15623=ORIENTED_EDGE('',*,*,#10091,.F.);
#15624=ORIENTED_EDGE('',*,*,#10090,.F.);
#15625=ORIENTED_EDGE('',*,*,#10089,.F.);
#15626=ORIENTED_EDGE('',*,*,#10088,.F.);
#15627=ORIENTED_EDGE('',*,*,#10087,.F.);
#15628=ORIENTED_EDGE('',*,*,#10086,.F.);
#15629=ORIENTED_EDGE('',*,*,#10085,.F.);
#15630=ORIENTED_EDGE('',*,*,#10084,.F.);
#15631=ORIENTED_EDGE('',*,*,#10083,.F.);
#15632=ORIENTED_EDGE('',*,*,#10082,.F.);
#15633=ORIENTED_EDGE('',*,*,#10081,.F.);
#15634=ORIENTED_EDGE('',*,*,#10080,.F.);
#15635=ORIENTED_EDGE('',*,*,#10079,.F.);
#15636=ORIENTED_EDGE('',*,*,#10078,.F.);
#15637=ORIENTED_EDGE('',*,*,#10077,.F.);
#15638=ORIENTED_EDGE('',*,*,#10076,.F.);
#15639=ORIENTED_EDGE('',*,*,#10075,.F.);
#15640=ORIENTED_EDGE('',*,*,#10139,.F.);
#15641=ORIENTED_EDGE('',*,*,#10121,.T.);
#15642=ORIENTED_EDGE('',*,*,#10120,.T.);
#15643=ORIENTED_EDGE('',*,*,#10119,.T.);
#15644=ORIENTED_EDGE('',*,*,#10118,.T.);
#15645=ORIENTED_EDGE('',*,*,#10117,.T.);
#15646=ORIENTED_EDGE('',*,*,#10116,.T.);
#15647=ORIENTED_EDGE('',*,*,#10115,.T.);
#15648=ORIENTED_EDGE('',*,*,#10114,.T.);
#15649=ORIENTED_EDGE('',*,*,#10113,.T.);
#15650=ORIENTED_EDGE('',*,*,#10112,.T.);
#15651=ORIENTED_EDGE('',*,*,#10111,.T.);
#15652=ORIENTED_EDGE('',*,*,#10140,.F.);
#15653=ORIENTED_EDGE('',*,*,#10141,.T.);
#15654=ORIENTED_EDGE('',*,*,#10142,.T.);
#15655=ORIENTED_EDGE('',*,*,#10143,.F.);
#15656=ORIENTED_EDGE('',*,*,#10144,.F.);
#15657=ORIENTED_EDGE('',*,*,#10145,.T.);
#15658=ORIENTED_EDGE('',*,*,#10146,.T.);
#15659=ORIENTED_EDGE('',*,*,#10141,.F.);
#15660=ORIENTED_EDGE('',*,*,#10147,.F.);
#15661=ORIENTED_EDGE('',*,*,#10148,.T.);
#15662=ORIENTED_EDGE('',*,*,#10149,.T.);
#15663=ORIENTED_EDGE('',*,*,#10145,.F.);
#15664=ORIENTED_EDGE('',*,*,#10150,.F.);
#15665=ORIENTED_EDGE('',*,*,#10151,.T.);
#15666=ORIENTED_EDGE('',*,*,#10152,.T.);
#15667=ORIENTED_EDGE('',*,*,#10148,.F.);
#15668=ORIENTED_EDGE('',*,*,#10153,.F.);
#15669=ORIENTED_EDGE('',*,*,#10154,.T.);
#15670=ORIENTED_EDGE('',*,*,#10155,.T.);
#15671=ORIENTED_EDGE('',*,*,#10151,.F.);
#15672=ORIENTED_EDGE('',*,*,#10156,.F.);
#15673=ORIENTED_EDGE('',*,*,#10143,.T.);
#15674=ORIENTED_EDGE('',*,*,#10157,.T.);
#15675=ORIENTED_EDGE('',*,*,#10154,.F.);
#15676=ORIENTED_EDGE('',*,*,#10157,.F.);
#15677=ORIENTED_EDGE('',*,*,#10142,.F.);
#15678=ORIENTED_EDGE('',*,*,#10146,.F.);
#15679=ORIENTED_EDGE('',*,*,#10149,.F.);
#15680=ORIENTED_EDGE('',*,*,#10152,.F.);
#15681=ORIENTED_EDGE('',*,*,#10155,.F.);
#15682=ORIENTED_EDGE('',*,*,#10158,.T.);
#15683=ORIENTED_EDGE('',*,*,#10138,.T.);
#15684=ORIENTED_EDGE('',*,*,#10122,.T.);
#15685=ORIENTED_EDGE('',*,*,#10139,.T.);
#15686=ORIENTED_EDGE('',*,*,#10074,.F.);
#15687=ORIENTED_EDGE('',*,*,#10158,.F.);
#15688=ORIENTED_EDGE('',*,*,#10159,.T.);
#15689=ORIENTED_EDGE('',*,*,#10160,.T.);
#15690=ORIENTED_EDGE('',*,*,#10159,.F.);
#15691=ORIENTED_EDGE('',*,*,#10160,.F.);
#15692=ORIENTED_EDGE('',*,*,#10140,.T.);
#15693=ORIENTED_EDGE('',*,*,#10156,.T.);
#15694=ORIENTED_EDGE('',*,*,#10153,.T.);
#15695=ORIENTED_EDGE('',*,*,#10150,.T.);
#15696=ORIENTED_EDGE('',*,*,#10147,.T.);
#15697=ORIENTED_EDGE('',*,*,#10144,.T.);
#15698=ORIENTED_EDGE('',*,*,#10136,.T.);
#15699=CYLINDRICAL_SURFACE('',#17048,4.085);
#15700=CYLINDRICAL_SURFACE('',#17050,4.085);
#15701=CYLINDRICAL_SURFACE('',#17051,4.085);
#15702=CYLINDRICAL_SURFACE('',#17052,4.085);
#15703=CYLINDRICAL_SURFACE('',#17053,4.085);
#15704=CYLINDRICAL_SURFACE('',#17054,4.085);
#15705=CYLINDRICAL_SURFACE('',#17055,4.085);
#15706=CYLINDRICAL_SURFACE('',#17056,4.085);
#15707=CYLINDRICAL_SURFACE('',#17057,4.085);
#15708=CYLINDRICAL_SURFACE('',#17058,4.085);
#15709=CYLINDRICAL_SURFACE('',#17060,3.38975);
#15710=CYLINDRICAL_SURFACE('',#17064,3.38975);
#15711=CYLINDRICAL_SURFACE('',#17065,3.38975);
#15712=CYLINDRICAL_SURFACE('',#17066,3.38975);
#15713=CYLINDRICAL_SURFACE('',#17067,3.38975);
#15714=CYLINDRICAL_SURFACE('',#17068,3.38975);
#15715=CYLINDRICAL_SURFACE('',#17069,3.38975);
#15716=CYLINDRICAL_SURFACE('',#17070,3.38975);
#15717=CYLINDRICAL_SURFACE('',#17071,3.38975);
#15718=CYLINDRICAL_SURFACE('',#17072,3.38975);
#15719=CYLINDRICAL_SURFACE('',#17074,4.085);
#15720=CYLINDRICAL_SURFACE('',#17076,4.085);
#15721=CYLINDRICAL_SURFACE('',#17077,4.085);
#15722=CYLINDRICAL_SURFACE('',#17078,4.085);
#15723=CYLINDRICAL_SURFACE('',#17079,4.085);
#15724=CYLINDRICAL_SURFACE('',#17080,4.085);
#15725=CYLINDRICAL_SURFACE('',#17081,4.085);
#15726=CYLINDRICAL_SURFACE('',#17082,4.085);
#15727=CYLINDRICAL_SURFACE('',#17083,4.085);
#15728=CYLINDRICAL_SURFACE('',#17084,4.085);
#15729=CYLINDRICAL_SURFACE('',#17086,3.38975);
#15730=CYLINDRICAL_SURFACE('',#17090,3.38975);
#15731=CYLINDRICAL_SURFACE('',#17091,3.38975);
#15732=CYLINDRICAL_SURFACE('',#17092,3.38975);
#15733=CYLINDRICAL_SURFACE('',#17093,3.38975);
#15734=CYLINDRICAL_SURFACE('',#17094,3.38975);
#15735=CYLINDRICAL_SURFACE('',#17095,3.38975);
#15736=CYLINDRICAL_SURFACE('',#17096,3.38975);
#15737=CYLINDRICAL_SURFACE('',#17097,3.38975);
#15738=CYLINDRICAL_SURFACE('',#17098,3.38975);
#15739=CYLINDRICAL_SURFACE('',#17100,4.085);
#15740=CYLINDRICAL_SURFACE('',#17102,4.085);
#15741=CYLINDRICAL_SURFACE('',#17103,4.085);
#15742=CYLINDRICAL_SURFACE('',#17104,4.085);
#15743=CYLINDRICAL_SURFACE('',#17105,4.085);
#15744=CYLINDRICAL_SURFACE('',#17106,4.085);
#15745=CYLINDRICAL_SURFACE('',#17107,4.085);
#15746=CYLINDRICAL_SURFACE('',#17108,4.085);
#15747=CYLINDRICAL_SURFACE('',#17109,4.085);
#15748=CYLINDRICAL_SURFACE('',#17110,4.085);
#15749=CYLINDRICAL_SURFACE('',#17112,3.38975);
#15750=CYLINDRICAL_SURFACE('',#17116,3.38975);
#15751=CYLINDRICAL_SURFACE('',#17117,3.38975);
#15752=CYLINDRICAL_SURFACE('',#17118,3.38975);
#15753=CYLINDRICAL_SURFACE('',#17119,3.38975);
#15754=CYLINDRICAL_SURFACE('',#17120,3.38975);
#15755=CYLINDRICAL_SURFACE('',#17121,3.38975);
#15756=CYLINDRICAL_SURFACE('',#17122,3.38975);
#15757=CYLINDRICAL_SURFACE('',#17123,3.38975);
#15758=CYLINDRICAL_SURFACE('',#17124,3.38975);
#15759=CYLINDRICAL_SURFACE('',#17126,4.085);
#15760=CYLINDRICAL_SURFACE('',#17128,4.085);
#15761=CYLINDRICAL_SURFACE('',#17129,4.085);
#15762=CYLINDRICAL_SURFACE('',#17130,4.085);
#15763=CYLINDRICAL_SURFACE('',#17131,4.085);
#15764=CYLINDRICAL_SURFACE('',#17132,4.085);
#15765=CYLINDRICAL_SURFACE('',#17133,4.085);
#15766=CYLINDRICAL_SURFACE('',#17134,4.085);
#15767=CYLINDRICAL_SURFACE('',#17135,4.085);
#15768=CYLINDRICAL_SURFACE('',#17136,4.085);
#15769=CYLINDRICAL_SURFACE('',#17138,3.38975);
#15770=CYLINDRICAL_SURFACE('',#17142,3.38975);
#15771=CYLINDRICAL_SURFACE('',#17143,3.38975);
#15772=CYLINDRICAL_SURFACE('',#17144,3.38975);
#15773=CYLINDRICAL_SURFACE('',#17145,3.38975);
#15774=CYLINDRICAL_SURFACE('',#17146,3.38975);
#15775=CYLINDRICAL_SURFACE('',#17147,3.38975);
#15776=CYLINDRICAL_SURFACE('',#17148,3.38975);
#15777=CYLINDRICAL_SURFACE('',#17149,3.38975);
#15778=CYLINDRICAL_SURFACE('',#17150,3.38975);
#15779=CYLINDRICAL_SURFACE('',#17152,3.38975);
#15780=CYLINDRICAL_SURFACE('',#17153,4.085);
#15781=CYLINDRICAL_SURFACE('',#17154,3.38975);
#15782=CYLINDRICAL_SURFACE('',#17155,4.085);
#15783=CYLINDRICAL_SURFACE('',#17156,3.38975);
#15784=CYLINDRICAL_SURFACE('',#17157,4.085);
#15785=CYLINDRICAL_SURFACE('',#17158,3.38975);
#15786=CYLINDRICAL_SURFACE('',#17159,4.085);
#15787=CYLINDRICAL_SURFACE('',#17168,4.5);
#15788=CYLINDRICAL_SURFACE('',#17171,4.5);
#15789=CYLINDRICAL_SURFACE('',#17174,4.5);
#15790=CYLINDRICAL_SURFACE('',#17177,4.5);
#15791=CYLINDRICAL_SURFACE('',#17187,2.05475);
#15792=CYLINDRICAL_SURFACE('',#17189,2.05475);
#15793=CYLINDRICAL_SURFACE('',#17190,2.05475);
#15794=CYLINDRICAL_SURFACE('',#17191,2.05475);
#15795=CYLINDRICAL_SURFACE('',#17192,2.05475);
#15796=CYLINDRICAL_SURFACE('',#17193,2.05475);
#15797=CYLINDRICAL_SURFACE('',#17194,2.05475);
#15798=CYLINDRICAL_SURFACE('',#17195,2.05475);
#15799=CYLINDRICAL_SURFACE('',#17196,2.05475);
#15800=CYLINDRICAL_SURFACE('',#17197,2.05475);
#15801=CYLINDRICAL_SURFACE('',#17198,2.05475);
#15802=CYLINDRICAL_SURFACE('',#17199,2.05475);
#15803=CYLINDRICAL_SURFACE('',#17200,2.05475);
#15804=CYLINDRICAL_SURFACE('',#17201,2.05475);
#15805=CYLINDRICAL_SURFACE('',#17202,2.05475);
#15806=CYLINDRICAL_SURFACE('',#17203,2.05475);
#15807=CYLINDRICAL_SURFACE('',#17205,1.666);
#15808=CYLINDRICAL_SURFACE('',#17208,1.666);
#15809=CYLINDRICAL_SURFACE('',#17209,1.666);
#15810=CYLINDRICAL_SURFACE('',#17210,1.666);
#15811=CYLINDRICAL_SURFACE('',#17211,1.666);
#15812=CYLINDRICAL_SURFACE('',#17212,1.666);
#15813=CYLINDRICAL_SURFACE('',#17213,1.666);
#15814=CYLINDRICAL_SURFACE('',#17214,1.666);
#15815=CYLINDRICAL_SURFACE('',#17215,1.666);
#15816=CYLINDRICAL_SURFACE('',#17216,1.666);
#15817=CYLINDRICAL_SURFACE('',#17217,1.666);
#15818=CYLINDRICAL_SURFACE('',#17218,1.666);
#15819=CYLINDRICAL_SURFACE('',#17219,1.666);
#15820=CYLINDRICAL_SURFACE('',#17220,1.666);
#15821=CYLINDRICAL_SURFACE('',#17221,1.666);
#15822=CYLINDRICAL_SURFACE('',#17223,2.05475);
#15823=CYLINDRICAL_SURFACE('',#17225,2.05475);
#15824=CYLINDRICAL_SURFACE('',#17226,2.05475);
#15825=CYLINDRICAL_SURFACE('',#17227,2.05475);
#15826=CYLINDRICAL_SURFACE('',#17228,2.05475);
#15827=CYLINDRICAL_SURFACE('',#17229,2.05475);
#15828=CYLINDRICAL_SURFACE('',#17230,2.05475);
#15829=CYLINDRICAL_SURFACE('',#17231,2.05475);
#15830=CYLINDRICAL_SURFACE('',#17232,2.05475);
#15831=CYLINDRICAL_SURFACE('',#17233,2.05475);
#15832=CYLINDRICAL_SURFACE('',#17234,2.05475);
#15833=CYLINDRICAL_SURFACE('',#17235,2.05475);
#15834=CYLINDRICAL_SURFACE('',#17236,2.05475);
#15835=CYLINDRICAL_SURFACE('',#17237,2.05475);
#15836=CYLINDRICAL_SURFACE('',#17238,2.05475);
#15837=CYLINDRICAL_SURFACE('',#17239,2.05475);
#15838=CYLINDRICAL_SURFACE('',#17241,1.666);
#15839=CYLINDRICAL_SURFACE('',#17244,1.666);
#15840=CYLINDRICAL_SURFACE('',#17245,1.666);
#15841=CYLINDRICAL_SURFACE('',#17246,1.666);
#15842=CYLINDRICAL_SURFACE('',#17247,1.666);
#15843=CYLINDRICAL_SURFACE('',#17248,1.666);
#15844=CYLINDRICAL_SURFACE('',#17249,1.666);
#15845=CYLINDRICAL_SURFACE('',#17250,1.666);
#15846=CYLINDRICAL_SURFACE('',#17251,1.666);
#15847=CYLINDRICAL_SURFACE('',#17252,1.666);
#15848=CYLINDRICAL_SURFACE('',#17253,1.666);
#15849=CYLINDRICAL_SURFACE('',#17254,1.666);
#15850=CYLINDRICAL_SURFACE('',#17255,1.666);
#15851=CYLINDRICAL_SURFACE('',#17256,1.666);
#15852=CYLINDRICAL_SURFACE('',#17257,1.666);
#15853=CYLINDRICAL_SURFACE('',#17259,2.05475);
#15854=CYLINDRICAL_SURFACE('',#17261,2.05475);
#15855=CYLINDRICAL_SURFACE('',#17262,2.05475);
#15856=CYLINDRICAL_SURFACE('',#17263,2.05475);
#15857=CYLINDRICAL_SURFACE('',#17264,2.05475);
#15858=CYLINDRICAL_SURFACE('',#17265,2.05475);
#15859=CYLINDRICAL_SURFACE('',#17266,2.05475);
#15860=CYLINDRICAL_SURFACE('',#17267,2.05475);
#15861=CYLINDRICAL_SURFACE('',#17268,2.05475);
#15862=CYLINDRICAL_SURFACE('',#17269,2.05475);
#15863=CYLINDRICAL_SURFACE('',#17270,2.05475);
#15864=CYLINDRICAL_SURFACE('',#17271,2.05475);
#15865=CYLINDRICAL_SURFACE('',#17272,2.05475);
#15866=CYLINDRICAL_SURFACE('',#17273,2.05475);
#15867=CYLINDRICAL_SURFACE('',#17275,2.05475);
#15868=CYLINDRICAL_SURFACE('',#17277,2.05475);
#15869=CYLINDRICAL_SURFACE('',#17278,2.05475);
#15870=CYLINDRICAL_SURFACE('',#17279,2.05475);
#15871=CYLINDRICAL_SURFACE('',#17280,2.05475);
#15872=CYLINDRICAL_SURFACE('',#17281,2.05475);
#15873=CYLINDRICAL_SURFACE('',#17282,2.05475);
#15874=CYLINDRICAL_SURFACE('',#17283,2.05475);
#15875=CYLINDRICAL_SURFACE('',#17284,2.05475);
#15876=CYLINDRICAL_SURFACE('',#17285,2.05475);
#15877=CYLINDRICAL_SURFACE('',#17286,2.05475);
#15878=CYLINDRICAL_SURFACE('',#17287,2.05475);
#15879=CYLINDRICAL_SURFACE('',#17288,2.05475);
#15880=CYLINDRICAL_SURFACE('',#17289,2.05475);
#15881=CYLINDRICAL_SURFACE('',#17291,2.05475);
#15882=CYLINDRICAL_SURFACE('',#17293,2.05475);
#15883=CYLINDRICAL_SURFACE('',#17294,2.05475);
#15884=CYLINDRICAL_SURFACE('',#17295,2.05475);
#15885=CYLINDRICAL_SURFACE('',#17296,2.05475);
#15886=CYLINDRICAL_SURFACE('',#17297,2.05475);
#15887=CYLINDRICAL_SURFACE('',#17298,2.05475);
#15888=CYLINDRICAL_SURFACE('',#17299,2.05475);
#15889=CYLINDRICAL_SURFACE('',#17300,2.05475);
#15890=CYLINDRICAL_SURFACE('',#17301,2.05475);
#15891=CYLINDRICAL_SURFACE('',#17302,2.05475);
#15892=CYLINDRICAL_SURFACE('',#17303,2.05475);
#15893=CYLINDRICAL_SURFACE('',#17304,2.05475);
#15894=CYLINDRICAL_SURFACE('',#17305,2.05475);
#15895=CYLINDRICAL_SURFACE('',#17307,2.05475);
#15896=CYLINDRICAL_SURFACE('',#17309,2.05475);
#15897=CYLINDRICAL_SURFACE('',#17310,2.05475);
#15898=CYLINDRICAL_SURFACE('',#17311,2.05475);
#15899=CYLINDRICAL_SURFACE('',#17312,2.05475);
#15900=CYLINDRICAL_SURFACE('',#17313,2.05475);
#15901=CYLINDRICAL_SURFACE('',#17314,2.05475);
#15902=CYLINDRICAL_SURFACE('',#17315,2.05475);
#15903=CYLINDRICAL_SURFACE('',#17316,2.05475);
#15904=CYLINDRICAL_SURFACE('',#17317,2.05475);
#15905=CYLINDRICAL_SURFACE('',#17318,2.05475);
#15906=CYLINDRICAL_SURFACE('',#17319,2.05475);
#15907=CYLINDRICAL_SURFACE('',#17320,2.05475);
#15908=CYLINDRICAL_SURFACE('',#17321,2.05475);
#15909=CYLINDRICAL_SURFACE('',#17323,1.666);
#15910=CYLINDRICAL_SURFACE('',#17325,1.666);
#15911=CYLINDRICAL_SURFACE('',#17326,1.666);
#15912=CYLINDRICAL_SURFACE('',#17327,1.666);
#15913=CYLINDRICAL_SURFACE('',#17328,1.666);
#15914=CYLINDRICAL_SURFACE('',#17329,1.666);
#15915=CYLINDRICAL_SURFACE('',#17330,1.666);
#15916=CYLINDRICAL_SURFACE('',#17331,1.666);
#15917=CYLINDRICAL_SURFACE('',#17332,1.666);
#15918=CYLINDRICAL_SURFACE('',#17333,1.666);
#15919=CYLINDRICAL_SURFACE('',#17334,1.666);
#15920=CYLINDRICAL_SURFACE('',#17335,1.666);
#15921=CYLINDRICAL_SURFACE('',#17336,1.666);
#15922=CYLINDRICAL_SURFACE('',#17337,1.666);
#15923=CYLINDRICAL_SURFACE('',#17339,1.666);
#15924=CYLINDRICAL_SURFACE('',#17341,1.666);
#15925=CYLINDRICAL_SURFACE('',#17342,1.666);
#15926=CYLINDRICAL_SURFACE('',#17343,1.666);
#15927=CYLINDRICAL_SURFACE('',#17344,1.666);
#15928=CYLINDRICAL_SURFACE('',#17345,1.666);
#15929=CYLINDRICAL_SURFACE('',#17346,1.666);
#15930=CYLINDRICAL_SURFACE('',#17347,1.666);
#15931=CYLINDRICAL_SURFACE('',#17348,1.666);
#15932=CYLINDRICAL_SURFACE('',#17349,1.666);
#15933=CYLINDRICAL_SURFACE('',#17350,1.666);
#15934=CYLINDRICAL_SURFACE('',#17351,1.666);
#15935=CYLINDRICAL_SURFACE('',#17352,1.666);
#15936=CYLINDRICAL_SURFACE('',#17353,1.666);
#15937=CYLINDRICAL_SURFACE('',#17355,1.666);
#15938=CYLINDRICAL_SURFACE('',#17357,1.666);
#15939=CYLINDRICAL_SURFACE('',#17358,1.666);
#15940=CYLINDRICAL_SURFACE('',#17359,1.666);
#15941=CYLINDRICAL_SURFACE('',#17360,1.666);
#15942=CYLINDRICAL_SURFACE('',#17361,1.666);
#15943=CYLINDRICAL_SURFACE('',#17362,1.666);
#15944=CYLINDRICAL_SURFACE('',#17363,1.666);
#15945=CYLINDRICAL_SURFACE('',#17364,1.666);
#15946=CYLINDRICAL_SURFACE('',#17365,1.666);
#15947=CYLINDRICAL_SURFACE('',#17366,1.666);
#15948=CYLINDRICAL_SURFACE('',#17367,1.666);
#15949=CYLINDRICAL_SURFACE('',#17368,1.666);
#15950=CYLINDRICAL_SURFACE('',#17369,1.666);
#15951=CYLINDRICAL_SURFACE('',#17371,1.666);
#15952=CYLINDRICAL_SURFACE('',#17373,1.666);
#15953=CYLINDRICAL_SURFACE('',#17374,1.666);
#15954=CYLINDRICAL_SURFACE('',#17375,1.666);
#15955=CYLINDRICAL_SURFACE('',#17376,1.666);
#15956=CYLINDRICAL_SURFACE('',#17377,1.666);
#15957=CYLINDRICAL_SURFACE('',#17378,1.666);
#15958=CYLINDRICAL_SURFACE('',#17379,1.666);
#15959=CYLINDRICAL_SURFACE('',#17380,1.666);
#15960=CYLINDRICAL_SURFACE('',#17381,1.666);
#15961=CYLINDRICAL_SURFACE('',#17382,1.666);
#15962=CYLINDRICAL_SURFACE('',#17383,1.666);
#15963=CYLINDRICAL_SURFACE('',#17384,1.666);
#15964=CYLINDRICAL_SURFACE('',#17385,1.666);
#15965=CYLINDRICAL_SURFACE('',#17387,1.666);
#15966=CYLINDRICAL_SURFACE('',#17388,1.666);
#15967=CYLINDRICAL_SURFACE('',#17389,1.666);
#15968=CYLINDRICAL_SURFACE('',#17390,1.666);
#15969=CYLINDRICAL_SURFACE('',#17391,2.05475);
#15970=CYLINDRICAL_SURFACE('',#17392,2.05475);
#15971=CYLINDRICAL_SURFACE('',#17393,2.05475);
#15972=CYLINDRICAL_SURFACE('',#17394,2.05475);
#15973=CYLINDRICAL_SURFACE('',#17395,1.666);
#15974=CYLINDRICAL_SURFACE('',#17396,2.05475);
#15975=CYLINDRICAL_SURFACE('',#17397,1.666);
#15976=CYLINDRICAL_SURFACE('',#17398,2.05475);
#15977=CYLINDRICAL_SURFACE('',#17409,4.5);
#15978=CYLINDRICAL_SURFACE('',#17412,4.5);
#15979=CYLINDRICAL_SURFACE('',#17415,4.5);
#15980=CYLINDRICAL_SURFACE('',#17418,4.5);
#15981=CYLINDRICAL_SURFACE('',#17425,22.);
#15982=CYLINDRICAL_SURFACE('',#17445,20.);
#15983=CYLINDRICAL_SURFACE('',#17447,22.);
#15984=CYLINDRICAL_SURFACE('',#17451,7.01125);
#15985=CYLINDRICAL_SURFACE('',#17455,7.01125);
#15986=CYLINDRICAL_SURFACE('',#17456,7.01125);
#15987=CYLINDRICAL_SURFACE('',#17457,7.01125);
#15988=CYLINDRICAL_SURFACE('',#17458,7.01125);
#15989=CYLINDRICAL_SURFACE('',#17459,7.01125);
#15990=CYLINDRICAL_SURFACE('',#17460,7.01125);
#15991=CYLINDRICAL_SURFACE('',#17461,7.01125);
#15992=CYLINDRICAL_SURFACE('',#17462,7.01125);
#15993=CYLINDRICAL_SURFACE('',#17463,7.01125);
#15994=CYLINDRICAL_SURFACE('',#17464,7.01125);
#15995=CYLINDRICAL_SURFACE('',#17465,7.01125);
#15996=CYLINDRICAL_SURFACE('',#17466,7.01125);
#15997=CYLINDRICAL_SURFACE('',#17467,7.01125);
#15998=CYLINDRICAL_SURFACE('',#17468,7.01125);
#15999=CYLINDRICAL_SURFACE('',#17469,7.01125);
#16000=CYLINDRICAL_SURFACE('',#17470,7.01125);
#16001=CYLINDRICAL_SURFACE('',#17471,7.01125);
#16002=CYLINDRICAL_SURFACE('',#17472,7.01125);
#16003=CYLINDRICAL_SURFACE('',#17473,7.01125);
#16004=CYLINDRICAL_SURFACE('',#17474,7.01125);
#16005=CYLINDRICAL_SURFACE('',#17475,7.01125);
#16006=CYLINDRICAL_SURFACE('',#17476,7.01125);
#16007=CYLINDRICAL_SURFACE('',#17477,7.01125);
#16008=CYLINDRICAL_SURFACE('',#17478,7.01125);
#16009=CYLINDRICAL_SURFACE('',#17479,7.01125);
#16010=CYLINDRICAL_SURFACE('',#17480,7.01125);
#16011=CYLINDRICAL_SURFACE('',#17481,7.01125);
#16012=CYLINDRICAL_SURFACE('',#17482,7.01125);
#16013=CYLINDRICAL_SURFACE('',#17483,7.01125);
#16014=CYLINDRICAL_SURFACE('',#17484,7.01125);
#16015=CYLINDRICAL_SURFACE('',#17485,7.01125);
#16016=CYLINDRICAL_SURFACE('',#17486,7.01125);
#16017=CYLINDRICAL_SURFACE('',#17487,7.01125);
#16018=CYLINDRICAL_SURFACE('',#17488,7.01125);
#16019=CYLINDRICAL_SURFACE('',#17489,7.01125);
#16020=CYLINDRICAL_SURFACE('',#17490,7.01125);
#16021=CYLINDRICAL_SURFACE('',#17491,7.01125);
#16022=CYLINDRICAL_SURFACE('',#17492,7.01125);
#16023=CYLINDRICAL_SURFACE('',#17493,7.01125);
#16024=CYLINDRICAL_SURFACE('',#17494,7.01125);
#16025=CYLINDRICAL_SURFACE('',#17495,7.01125);
#16026=CYLINDRICAL_SURFACE('',#17496,7.01125);
#16027=CYLINDRICAL_SURFACE('',#17497,7.01125);
#16028=CYLINDRICAL_SURFACE('',#17498,7.01125);
#16029=CYLINDRICAL_SURFACE('',#17499,7.01125);
#16030=CYLINDRICAL_SURFACE('',#17500,7.01125);
#16031=CYLINDRICAL_SURFACE('',#17501,7.01125);
#16032=CYLINDRICAL_SURFACE('',#17502,7.01125);
#16033=CYLINDRICAL_SURFACE('',#17504,7.01125);
#16034=CYLINDRICAL_SURFACE('',#17505,8.12525);
#16035=CYLINDRICAL_SURFACE('',#17521,4.);
#16036=CYLINDRICAL_SURFACE('',#17522,20.);
#16037=CYLINDRICAL_SURFACE('',#17532,13.);
#16038=CYLINDRICAL_SURFACE('',#17536,2.5);
#16039=CYLINDRICAL_SURFACE('',#17539,2.5);
#16040=CYLINDRICAL_SURFACE('',#17562,2.5);
#16041=CYLINDRICAL_SURFACE('',#17564,2.5);
#16042=CYLINDRICAL_SURFACE('',#17566,2.5);
#16043=CYLINDRICAL_SURFACE('',#17568,2.5);
#16044=CYLINDRICAL_SURFACE('',#17570,7.);
#16045=CYLINDRICAL_SURFACE('',#17576,6.);
#16046=CYLINDRICAL_SURFACE('',#17579,7.);
#16047=CYLINDRICAL_SURFACE('',#17585,6.767);
#16048=CYLINDRICAL_SURFACE('',#17587,6.767);
#16049=CYLINDRICAL_SURFACE('',#17588,6.767);
#16050=CYLINDRICAL_SURFACE('',#17589,6.767);
#16051=CYLINDRICAL_SURFACE('',#17590,6.767);
#16052=CYLINDRICAL_SURFACE('',#17591,6.767);
#16053=CYLINDRICAL_SURFACE('',#17592,6.767);
#16054=CYLINDRICAL_SURFACE('',#17593,6.767);
#16055=CYLINDRICAL_SURFACE('',#17594,6.767);
#16056=CYLINDRICAL_SURFACE('',#17595,6.767);
#16057=CYLINDRICAL_SURFACE('',#17596,6.767);
#16058=CYLINDRICAL_SURFACE('',#17597,6.767);
#16059=CYLINDRICAL_SURFACE('',#17598,6.767);
#16060=CYLINDRICAL_SURFACE('',#17599,6.767);
#16061=CYLINDRICAL_SURFACE('',#17600,6.767);
#16062=CYLINDRICAL_SURFACE('',#17601,6.767);
#16063=CYLINDRICAL_SURFACE('',#17602,6.767);
#16064=CYLINDRICAL_SURFACE('',#17603,6.767);
#16065=CYLINDRICAL_SURFACE('',#17604,6.767);
#16066=CYLINDRICAL_SURFACE('',#17605,6.767);
#16067=CYLINDRICAL_SURFACE('',#17606,6.767);
#16068=CYLINDRICAL_SURFACE('',#17607,6.767);
#16069=CYLINDRICAL_SURFACE('',#17608,6.767);
#16070=CYLINDRICAL_SURFACE('',#17609,6.767);
#16071=CYLINDRICAL_SURFACE('',#17610,6.767);
#16072=CYLINDRICAL_SURFACE('',#17611,6.767);
#16073=CYLINDRICAL_SURFACE('',#17612,6.767);
#16074=CYLINDRICAL_SURFACE('',#17613,6.767);
#16075=CYLINDRICAL_SURFACE('',#17614,6.767);
#16076=CYLINDRICAL_SURFACE('',#17615,6.767);
#16077=CYLINDRICAL_SURFACE('',#17616,6.767);
#16078=CYLINDRICAL_SURFACE('',#17617,6.767);
#16079=CYLINDRICAL_SURFACE('',#17618,6.767);
#16080=CYLINDRICAL_SURFACE('',#17619,6.767);
#16081=CYLINDRICAL_SURFACE('',#17620,6.767);
#16082=CYLINDRICAL_SURFACE('',#17621,6.767);
#16083=CYLINDRICAL_SURFACE('',#17622,6.767);
#16084=CYLINDRICAL_SURFACE('',#17623,6.767);
#16085=CYLINDRICAL_SURFACE('',#17624,6.767);
#16086=CYLINDRICAL_SURFACE('',#17625,6.767);
#16087=CYLINDRICAL_SURFACE('',#17626,6.767);
#16088=CYLINDRICAL_SURFACE('',#17627,6.767);
#16089=CYLINDRICAL_SURFACE('',#17628,6.767);
#16090=CYLINDRICAL_SURFACE('',#17629,6.767);
#16091=CYLINDRICAL_SURFACE('',#17630,6.767);
#16092=CYLINDRICAL_SURFACE('',#17631,6.767);
#16093=CYLINDRICAL_SURFACE('',#17632,6.767);
#16094=CYLINDRICAL_SURFACE('',#17633,6.767);
#16095=CYLINDRICAL_SURFACE('',#17634,6.767);
#16096=CYLINDRICAL_SURFACE('',#17635,6.767);
#16097=CYLINDRICAL_SURFACE('',#17636,6.767);
#16098=CYLINDRICAL_SURFACE('',#17637,6.767);
#16099=CYLINDRICAL_SURFACE('',#17638,6.767);
#16100=CYLINDRICAL_SURFACE('',#17639,6.767);
#16101=CYLINDRICAL_SURFACE('',#17640,6.767);
#16102=CYLINDRICAL_SURFACE('',#17641,6.767);
#16103=CYLINDRICAL_SURFACE('',#17642,6.767);
#16104=CYLINDRICAL_SURFACE('',#17643,6.767);
#16105=CYLINDRICAL_SURFACE('',#17644,6.767);
#16106=CYLINDRICAL_SURFACE('',#17645,6.767);
#16107=CYLINDRICAL_SURFACE('',#17646,6.767);
#16108=CYLINDRICAL_SURFACE('',#17647,6.767);
#16109=CYLINDRICAL_SURFACE('',#17648,6.767);
#16110=CYLINDRICAL_SURFACE('',#17649,6.767);
#16111=CYLINDRICAL_SURFACE('',#17650,6.767);
#16112=CYLINDRICAL_SURFACE('',#17651,7.911);
#16113=CYLINDRICAL_SURFACE('',#17654,6.767);
#16114=CYLINDRICAL_SURFACE('',#17656,2.);
#16115=CYLINDRICAL_SURFACE('',#17661,10.);
#16116=CYLINDRICAL_SURFACE('',#17663,6.);
#16117=CYLINDRICAL_SURFACE('',#17668,2.);
#16118=CYLINDRICAL_SURFACE('',#17669,2.);
#16119=CYLINDRICAL_SURFACE('',#17670,8.);
#16120=CYLINDRICAL_SURFACE('',#17673,8.);
#16121=CYLINDRICAL_SURFACE('',#17676,8.);
#16122=CYLINDRICAL_SURFACE('',#17679,8.);
#16123=CYLINDRICAL_SURFACE('',#17682,8.);
#16124=CYLINDRICAL_SURFACE('',#17685,8.);
#16125=CYLINDRICAL_SURFACE('',#17688,14.);
#16126=CYLINDRICAL_SURFACE('',#17693,6.);
#16127=CYLINDRICAL_SURFACE('',#17695,45.);
#16128=CYLINDRICAL_SURFACE('',#17701,1.5);
#16129=CYLINDRICAL_SURFACE('',#17708,2.);
#16130=CYLINDRICAL_SURFACE('',#17713,3.5);
#16131=CYLINDRICAL_SURFACE('',#17716,2.);
#16132=CYLINDRICAL_SURFACE('',#17719,2.);
#16133=CYLINDRICAL_SURFACE('',#17722,3.5);
#16134=CYLINDRICAL_SURFACE('',#17733,1.5);
#16135=CYLINDRICAL_SURFACE('',#17735,3.5);
#16136=CYLINDRICAL_SURFACE('',#17739,6.);
#16137=CYLINDRICAL_SURFACE('',#17742,12.);
#16138=CYLINDRICAL_SURFACE('',#17753,3.22275);
#16139=CYLINDRICAL_SURFACE('',#17755,3.22275);
#16140=CYLINDRICAL_SURFACE('',#17756,3.22275);
#16141=CYLINDRICAL_SURFACE('',#17757,3.22275);
#16142=CYLINDRICAL_SURFACE('',#17758,3.22275);
#16143=CYLINDRICAL_SURFACE('',#17759,3.22275);
#16144=CYLINDRICAL_SURFACE('',#17760,3.22275);
#16145=CYLINDRICAL_SURFACE('',#17761,3.22275);
#16146=CYLINDRICAL_SURFACE('',#17762,3.22275);
#16147=CYLINDRICAL_SURFACE('',#17763,3.22275);
#16148=CYLINDRICAL_SURFACE('',#17764,3.22275);
#16149=CYLINDRICAL_SURFACE('',#17765,3.22275);
#16150=CYLINDRICAL_SURFACE('',#17766,3.22275);
#16151=CYLINDRICAL_SURFACE('',#17767,3.22275);
#16152=CYLINDRICAL_SURFACE('',#17768,3.22275);
#16153=CYLINDRICAL_SURFACE('',#17769,3.22275);
#16154=CYLINDRICAL_SURFACE('',#17770,3.933);
#16155=CYLINDRICAL_SURFACE('',#17773,3.22275);
#16156=CYLINDRICAL_SURFACE('',#17784,6.5);
#16157=CYLINDRICAL_SURFACE('',#17794,1.5555);
#16158=CYLINDRICAL_SURFACE('',#17796,1.5555);
#16159=CYLINDRICAL_SURFACE('',#17797,1.5555);
#16160=CYLINDRICAL_SURFACE('',#17798,1.5555);
#16161=CYLINDRICAL_SURFACE('',#17799,1.5555);
#16162=CYLINDRICAL_SURFACE('',#17800,1.5555);
#16163=CYLINDRICAL_SURFACE('',#17801,1.5555);
#16164=CYLINDRICAL_SURFACE('',#17802,1.5555);
#16165=CYLINDRICAL_SURFACE('',#17803,1.5555);
#16166=CYLINDRICAL_SURFACE('',#17804,1.5555);
#16167=CYLINDRICAL_SURFACE('',#17805,1.5555);
#16168=CYLINDRICAL_SURFACE('',#17806,1.5555);
#16169=CYLINDRICAL_SURFACE('',#17807,1.5555);
#16170=CYLINDRICAL_SURFACE('',#17808,1.5555);
#16171=CYLINDRICAL_SURFACE('',#17809,1.5555);
#16172=CYLINDRICAL_SURFACE('',#17810,1.5555);
#16173=CYLINDRICAL_SURFACE('',#17811,1.5555);
#16174=CYLINDRICAL_SURFACE('',#17812,1.5555);
#16175=CYLINDRICAL_SURFACE('',#17813,1.5555);
#16176=CYLINDRICAL_SURFACE('',#17814,1.5555);
#16177=CYLINDRICAL_SURFACE('',#17815,1.5555);
#16178=CYLINDRICAL_SURFACE('',#17816,1.5555);
#16179=CYLINDRICAL_SURFACE('',#17817,1.5555);
#16180=CYLINDRICAL_SURFACE('',#17818,1.5555);
#16181=CYLINDRICAL_SURFACE('',#17819,1.5555);
#16182=CYLINDRICAL_SURFACE('',#17820,1.5555);
#16183=CYLINDRICAL_SURFACE('',#17821,1.5555);
#16184=CYLINDRICAL_SURFACE('',#17822,1.5555);
#16185=CYLINDRICAL_SURFACE('',#17823,1.954);
#16186=CYLINDRICAL_SURFACE('',#17827,1.5555);
#16187=CYLINDRICAL_SURFACE('',#17838,3.5);
#16188=CYLINDRICAL_SURFACE('',#17843,1.954);
#16189=CYLINDRICAL_SURFACE('',#17846,1.5555);
#16190=CYLINDRICAL_SURFACE('',#17860,3.5);
#16191=ADVANCED_FACE('',(#423),#15699,.F.);
#16192=ADVANCED_FACE('',(#424),#15700,.F.);
#16193=ADVANCED_FACE('',(#425),#15701,.F.);
#16194=ADVANCED_FACE('',(#426),#15702,.F.);
#16195=ADVANCED_FACE('',(#427),#15703,.F.);
#16196=ADVANCED_FACE('',(#428),#15704,.F.);
#16197=ADVANCED_FACE('',(#429),#15705,.F.);
#16198=ADVANCED_FACE('',(#430),#15706,.F.);
#16199=ADVANCED_FACE('',(#431),#15707,.F.);
#16200=ADVANCED_FACE('',(#432),#15708,.F.);
#16201=ADVANCED_FACE('',(#433),#15709,.F.);
#16202=ADVANCED_FACE('',(#434),#15710,.F.);
#16203=ADVANCED_FACE('',(#435),#15711,.F.);
#16204=ADVANCED_FACE('',(#436),#15712,.F.);
#16205=ADVANCED_FACE('',(#437),#15713,.F.);
#16206=ADVANCED_FACE('',(#438),#15714,.F.);
#16207=ADVANCED_FACE('',(#439),#15715,.F.);
#16208=ADVANCED_FACE('',(#440),#15716,.F.);
#16209=ADVANCED_FACE('',(#441),#15717,.F.);
#16210=ADVANCED_FACE('',(#442),#15718,.F.);
#16211=ADVANCED_FACE('',(#443),#15719,.F.);
#16212=ADVANCED_FACE('',(#444),#15720,.F.);
#16213=ADVANCED_FACE('',(#445),#15721,.F.);
#16214=ADVANCED_FACE('',(#446),#15722,.F.);
#16215=ADVANCED_FACE('',(#447),#15723,.F.);
#16216=ADVANCED_FACE('',(#448),#15724,.F.);
#16217=ADVANCED_FACE('',(#449),#15725,.F.);
#16218=ADVANCED_FACE('',(#450),#15726,.F.);
#16219=ADVANCED_FACE('',(#451),#15727,.F.);
#16220=ADVANCED_FACE('',(#452),#15728,.F.);
#16221=ADVANCED_FACE('',(#453),#15729,.F.);
#16222=ADVANCED_FACE('',(#454),#15730,.F.);
#16223=ADVANCED_FACE('',(#455),#15731,.F.);
#16224=ADVANCED_FACE('',(#456),#15732,.F.);
#16225=ADVANCED_FACE('',(#457),#15733,.F.);
#16226=ADVANCED_FACE('',(#458),#15734,.F.);
#16227=ADVANCED_FACE('',(#459),#15735,.F.);
#16228=ADVANCED_FACE('',(#460),#15736,.F.);
#16229=ADVANCED_FACE('',(#461),#15737,.F.);
#16230=ADVANCED_FACE('',(#462),#15738,.F.);
#16231=ADVANCED_FACE('',(#463),#15739,.F.);
#16232=ADVANCED_FACE('',(#464),#15740,.F.);
#16233=ADVANCED_FACE('',(#465),#15741,.F.);
#16234=ADVANCED_FACE('',(#466),#15742,.F.);
#16235=ADVANCED_FACE('',(#467),#15743,.F.);
#16236=ADVANCED_FACE('',(#468),#15744,.F.);
#16237=ADVANCED_FACE('',(#469),#15745,.F.);
#16238=ADVANCED_FACE('',(#470),#15746,.F.);
#16239=ADVANCED_FACE('',(#471),#15747,.F.);
#16240=ADVANCED_FACE('',(#472),#15748,.F.);
#16241=ADVANCED_FACE('',(#473),#15749,.F.);
#16242=ADVANCED_FACE('',(#474),#15750,.F.);
#16243=ADVANCED_FACE('',(#475),#15751,.F.);
#16244=ADVANCED_FACE('',(#476),#15752,.F.);
#16245=ADVANCED_FACE('',(#477),#15753,.F.);
#16246=ADVANCED_FACE('',(#478),#15754,.F.);
#16247=ADVANCED_FACE('',(#479),#15755,.F.);
#16248=ADVANCED_FACE('',(#480),#15756,.F.);
#16249=ADVANCED_FACE('',(#481),#15757,.F.);
#16250=ADVANCED_FACE('',(#482),#15758,.F.);
#16251=ADVANCED_FACE('',(#483),#15759,.F.);
#16252=ADVANCED_FACE('',(#484),#15760,.F.);
#16253=ADVANCED_FACE('',(#485),#15761,.F.);
#16254=ADVANCED_FACE('',(#486),#15762,.F.);
#16255=ADVANCED_FACE('',(#487),#15763,.F.);
#16256=ADVANCED_FACE('',(#488),#15764,.F.);
#16257=ADVANCED_FACE('',(#489),#15765,.F.);
#16258=ADVANCED_FACE('',(#490),#15766,.F.);
#16259=ADVANCED_FACE('',(#491),#15767,.F.);
#16260=ADVANCED_FACE('',(#492),#15768,.F.);
#16261=ADVANCED_FACE('',(#493),#15769,.F.);
#16262=ADVANCED_FACE('',(#494),#15770,.F.);
#16263=ADVANCED_FACE('',(#495),#15771,.F.);
#16264=ADVANCED_FACE('',(#496),#15772,.F.);
#16265=ADVANCED_FACE('',(#497),#15773,.F.);
#16266=ADVANCED_FACE('',(#498),#15774,.F.);
#16267=ADVANCED_FACE('',(#499),#15775,.F.);
#16268=ADVANCED_FACE('',(#500),#15776,.F.);
#16269=ADVANCED_FACE('',(#501),#15777,.F.);
#16270=ADVANCED_FACE('',(#502),#15778,.F.);
#16271=ADVANCED_FACE('',(#503),#15779,.F.);
#16272=ADVANCED_FACE('',(#504),#15780,.F.);
#16273=ADVANCED_FACE('',(#505),#15781,.F.);
#16274=ADVANCED_FACE('',(#506),#15782,.F.);
#16275=ADVANCED_FACE('',(#507),#15783,.F.);
#16276=ADVANCED_FACE('',(#508),#15784,.F.);
#16277=ADVANCED_FACE('',(#509),#15785,.F.);
#16278=ADVANCED_FACE('',(#510),#15786,.F.);
#16279=ADVANCED_FACE('',(#511),#303,.T.);
#16280=ADVANCED_FACE('',(#512),#273,.F.);
#16281=ADVANCED_FACE('',(#513),#274,.F.);
#16282=ADVANCED_FACE('',(#514),#304,.T.);
#16283=ADVANCED_FACE('',(#515),#275,.F.);
#16284=ADVANCED_FACE('',(#516),#276,.F.);
#16285=ADVANCED_FACE('',(#517),#305,.T.);
#16286=ADVANCED_FACE('',(#518),#277,.F.);
#16287=ADVANCED_FACE('',(#519),#278,.F.);
#16288=ADVANCED_FACE('',(#520),#306,.T.);
#16289=ADVANCED_FACE('',(#521),#279,.F.);
#16290=ADVANCED_FACE('',(#522),#280,.F.);
#16291=ADVANCED_FACE('',(#523),#307,.F.);
#16292=ADVANCED_FACE('',(#524),#308,.F.);
#16293=ADVANCED_FACE('',(#525),#309,.F.);
#16294=ADVANCED_FACE('',(#526),#310,.F.);
#16295=ADVANCED_FACE('',(#527),#15787,.F.);
#16296=ADVANCED_FACE('',(#528),#15788,.F.);
#16297=ADVANCED_FACE('',(#529),#15789,.F.);
#16298=ADVANCED_FACE('',(#530),#15790,.F.);
#16299=ADVANCED_FACE('',(#531),#311,.T.);
#16300=ADVANCED_FACE('',(#532),#312,.T.);
#16301=ADVANCED_FACE('',(#533),#313,.T.);
#16302=ADVANCED_FACE('',(#534),#314,.T.);
#16303=ADVANCED_FACE('',(#535,#187,#188,#189,#190,#191,#192,#193,#194),
#315,.T.);
#16304=ADVANCED_FACE('',(#536,#195,#196,#197,#198),#316,.F.);
#16305=ADVANCED_FACE('',(#537),#15791,.F.);
#16306=ADVANCED_FACE('',(#538),#15792,.F.);
#16307=ADVANCED_FACE('',(#539),#15793,.F.);
#16308=ADVANCED_FACE('',(#540),#15794,.F.);
#16309=ADVANCED_FACE('',(#541),#15795,.F.);
#16310=ADVANCED_FACE('',(#542),#15796,.F.);
#16311=ADVANCED_FACE('',(#543),#15797,.F.);
#16312=ADVANCED_FACE('',(#544),#15798,.F.);
#16313=ADVANCED_FACE('',(#545),#15799,.F.);
#16314=ADVANCED_FACE('',(#546),#15800,.F.);
#16315=ADVANCED_FACE('',(#547),#15801,.F.);
#16316=ADVANCED_FACE('',(#548),#15802,.F.);
#16317=ADVANCED_FACE('',(#549),#15803,.F.);
#16318=ADVANCED_FACE('',(#550),#15804,.F.);
#16319=ADVANCED_FACE('',(#551),#15805,.F.);
#16320=ADVANCED_FACE('',(#552),#15806,.F.);
#16321=ADVANCED_FACE('',(#553),#15807,.F.);
#16322=ADVANCED_FACE('',(#554),#15808,.F.);
#16323=ADVANCED_FACE('',(#555),#15809,.F.);
#16324=ADVANCED_FACE('',(#556),#15810,.F.);
#16325=ADVANCED_FACE('',(#557),#15811,.F.);
#16326=ADVANCED_FACE('',(#558),#15812,.F.);
#16327=ADVANCED_FACE('',(#559),#15813,.F.);
#16328=ADVANCED_FACE('',(#560),#15814,.F.);
#16329=ADVANCED_FACE('',(#561),#15815,.F.);
#16330=ADVANCED_FACE('',(#562),#15816,.F.);
#16331=ADVANCED_FACE('',(#563),#15817,.F.);
#16332=ADVANCED_FACE('',(#564),#15818,.F.);
#16333=ADVANCED_FACE('',(#565),#15819,.F.);
#16334=ADVANCED_FACE('',(#566),#15820,.F.);
#16335=ADVANCED_FACE('',(#567),#15821,.F.);
#16336=ADVANCED_FACE('',(#568),#15822,.F.);
#16337=ADVANCED_FACE('',(#569),#15823,.F.);
#16338=ADVANCED_FACE('',(#570),#15824,.F.);
#16339=ADVANCED_FACE('',(#571),#15825,.F.);
#16340=ADVANCED_FACE('',(#572),#15826,.F.);
#16341=ADVANCED_FACE('',(#573),#15827,.F.);
#16342=ADVANCED_FACE('',(#574),#15828,.F.);
#16343=ADVANCED_FACE('',(#575),#15829,.F.);
#16344=ADVANCED_FACE('',(#576),#15830,.F.);
#16345=ADVANCED_FACE('',(#577),#15831,.F.);
#16346=ADVANCED_FACE('',(#578),#15832,.F.);
#16347=ADVANCED_FACE('',(#579),#15833,.F.);
#16348=ADVANCED_FACE('',(#580),#15834,.F.);
#16349=ADVANCED_FACE('',(#581),#15835,.F.);
#16350=ADVANCED_FACE('',(#582),#15836,.F.);
#16351=ADVANCED_FACE('',(#583),#15837,.F.);
#16352=ADVANCED_FACE('',(#584),#15838,.F.);
#16353=ADVANCED_FACE('',(#585),#15839,.F.);
#16354=ADVANCED_FACE('',(#586),#15840,.F.);
#16355=ADVANCED_FACE('',(#587),#15841,.F.);
#16356=ADVANCED_FACE('',(#588),#15842,.F.);
#16357=ADVANCED_FACE('',(#589),#15843,.F.);
#16358=ADVANCED_FACE('',(#590),#15844,.F.);
#16359=ADVANCED_FACE('',(#591),#15845,.F.);
#16360=ADVANCED_FACE('',(#592),#15846,.F.);
#16361=ADVANCED_FACE('',(#593),#15847,.F.);
#16362=ADVANCED_FACE('',(#594),#15848,.F.);
#16363=ADVANCED_FACE('',(#595),#15849,.F.);
#16364=ADVANCED_FACE('',(#596),#15850,.F.);
#16365=ADVANCED_FACE('',(#597),#15851,.F.);
#16366=ADVANCED_FACE('',(#598),#15852,.F.);
#16367=ADVANCED_FACE('',(#599),#15853,.F.);
#16368=ADVANCED_FACE('',(#600),#15854,.F.);
#16369=ADVANCED_FACE('',(#601),#15855,.F.);
#16370=ADVANCED_FACE('',(#602),#15856,.F.);
#16371=ADVANCED_FACE('',(#603),#15857,.F.);
#16372=ADVANCED_FACE('',(#604),#15858,.F.);
#16373=ADVANCED_FACE('',(#605),#15859,.F.);
#16374=ADVANCED_FACE('',(#606),#15860,.F.);
#16375=ADVANCED_FACE('',(#607),#15861,.F.);
#16376=ADVANCED_FACE('',(#608),#15862,.F.);
#16377=ADVANCED_FACE('',(#609),#15863,.F.);
#16378=ADVANCED_FACE('',(#610),#15864,.F.);
#16379=ADVANCED_FACE('',(#611),#15865,.F.);
#16380=ADVANCED_FACE('',(#612),#15866,.F.);
#16381=ADVANCED_FACE('',(#613),#15867,.F.);
#16382=ADVANCED_FACE('',(#614),#15868,.F.);
#16383=ADVANCED_FACE('',(#615),#15869,.F.);
#16384=ADVANCED_FACE('',(#616),#15870,.F.);
#16385=ADVANCED_FACE('',(#617),#15871,.F.);
#16386=ADVANCED_FACE('',(#618),#15872,.F.);
#16387=ADVANCED_FACE('',(#619),#15873,.F.);
#16388=ADVANCED_FACE('',(#620),#15874,.F.);
#16389=ADVANCED_FACE('',(#621),#15875,.F.);
#16390=ADVANCED_FACE('',(#622),#15876,.F.);
#16391=ADVANCED_FACE('',(#623),#15877,.F.);
#16392=ADVANCED_FACE('',(#624),#15878,.F.);
#16393=ADVANCED_FACE('',(#625),#15879,.F.);
#16394=ADVANCED_FACE('',(#626),#15880,.F.);
#16395=ADVANCED_FACE('',(#627),#15881,.F.);
#16396=ADVANCED_FACE('',(#628),#15882,.F.);
#16397=ADVANCED_FACE('',(#629),#15883,.F.);
#16398=ADVANCED_FACE('',(#630),#15884,.F.);
#16399=ADVANCED_FACE('',(#631),#15885,.F.);
#16400=ADVANCED_FACE('',(#632),#15886,.F.);
#16401=ADVANCED_FACE('',(#633),#15887,.F.);
#16402=ADVANCED_FACE('',(#634),#15888,.F.);
#16403=ADVANCED_FACE('',(#635),#15889,.F.);
#16404=ADVANCED_FACE('',(#636),#15890,.F.);
#16405=ADVANCED_FACE('',(#637),#15891,.F.);
#16406=ADVANCED_FACE('',(#638),#15892,.F.);
#16407=ADVANCED_FACE('',(#639),#15893,.F.);
#16408=ADVANCED_FACE('',(#640),#15894,.F.);
#16409=ADVANCED_FACE('',(#641),#15895,.F.);
#16410=ADVANCED_FACE('',(#642),#15896,.F.);
#16411=ADVANCED_FACE('',(#643),#15897,.F.);
#16412=ADVANCED_FACE('',(#644),#15898,.F.);
#16413=ADVANCED_FACE('',(#645),#15899,.F.);
#16414=ADVANCED_FACE('',(#646),#15900,.F.);
#16415=ADVANCED_FACE('',(#647),#15901,.F.);
#16416=ADVANCED_FACE('',(#648),#15902,.F.);
#16417=ADVANCED_FACE('',(#649),#15903,.F.);
#16418=ADVANCED_FACE('',(#650),#15904,.F.);
#16419=ADVANCED_FACE('',(#651),#15905,.F.);
#16420=ADVANCED_FACE('',(#652),#15906,.F.);
#16421=ADVANCED_FACE('',(#653),#15907,.F.);
#16422=ADVANCED_FACE('',(#654),#15908,.F.);
#16423=ADVANCED_FACE('',(#655),#15909,.F.);
#16424=ADVANCED_FACE('',(#656),#15910,.F.);
#16425=ADVANCED_FACE('',(#657),#15911,.F.);
#16426=ADVANCED_FACE('',(#658),#15912,.F.);
#16427=ADVANCED_FACE('',(#659),#15913,.F.);
#16428=ADVANCED_FACE('',(#660),#15914,.F.);
#16429=ADVANCED_FACE('',(#661),#15915,.F.);
#16430=ADVANCED_FACE('',(#662),#15916,.F.);
#16431=ADVANCED_FACE('',(#663),#15917,.F.);
#16432=ADVANCED_FACE('',(#664),#15918,.F.);
#16433=ADVANCED_FACE('',(#665),#15919,.F.);
#16434=ADVANCED_FACE('',(#666),#15920,.F.);
#16435=ADVANCED_FACE('',(#667),#15921,.F.);
#16436=ADVANCED_FACE('',(#668),#15922,.F.);
#16437=ADVANCED_FACE('',(#669),#15923,.F.);
#16438=ADVANCED_FACE('',(#670),#15924,.F.);
#16439=ADVANCED_FACE('',(#671),#15925,.F.);
#16440=ADVANCED_FACE('',(#672),#15926,.F.);
#16441=ADVANCED_FACE('',(#673),#15927,.F.);
#16442=ADVANCED_FACE('',(#674),#15928,.F.);
#16443=ADVANCED_FACE('',(#675),#15929,.F.);
#16444=ADVANCED_FACE('',(#676),#15930,.F.);
#16445=ADVANCED_FACE('',(#677),#15931,.F.);
#16446=ADVANCED_FACE('',(#678),#15932,.F.);
#16447=ADVANCED_FACE('',(#679),#15933,.F.);
#16448=ADVANCED_FACE('',(#680),#15934,.F.);
#16449=ADVANCED_FACE('',(#681),#15935,.F.);
#16450=ADVANCED_FACE('',(#682),#15936,.F.);
#16451=ADVANCED_FACE('',(#683),#15937,.F.);
#16452=ADVANCED_FACE('',(#684),#15938,.F.);
#16453=ADVANCED_FACE('',(#685),#15939,.F.);
#16454=ADVANCED_FACE('',(#686),#15940,.F.);
#16455=ADVANCED_FACE('',(#687),#15941,.F.);
#16456=ADVANCED_FACE('',(#688),#15942,.F.);
#16457=ADVANCED_FACE('',(#689),#15943,.F.);
#16458=ADVANCED_FACE('',(#690),#15944,.F.);
#16459=ADVANCED_FACE('',(#691),#15945,.F.);
#16460=ADVANCED_FACE('',(#692),#15946,.F.);
#16461=ADVANCED_FACE('',(#693),#15947,.F.);
#16462=ADVANCED_FACE('',(#694),#15948,.F.);
#16463=ADVANCED_FACE('',(#695),#15949,.F.);
#16464=ADVANCED_FACE('',(#696),#15950,.F.);
#16465=ADVANCED_FACE('',(#697),#15951,.F.);
#16466=ADVANCED_FACE('',(#698),#15952,.F.);
#16467=ADVANCED_FACE('',(#699),#15953,.F.);
#16468=ADVANCED_FACE('',(#700),#15954,.F.);
#16469=ADVANCED_FACE('',(#701),#15955,.F.);
#16470=ADVANCED_FACE('',(#702),#15956,.F.);
#16471=ADVANCED_FACE('',(#703),#15957,.F.);
#16472=ADVANCED_FACE('',(#704),#15958,.F.);
#16473=ADVANCED_FACE('',(#705),#15959,.F.);
#16474=ADVANCED_FACE('',(#706),#15960,.F.);
#16475=ADVANCED_FACE('',(#707),#15961,.F.);
#16476=ADVANCED_FACE('',(#708),#15962,.F.);
#16477=ADVANCED_FACE('',(#709),#15963,.F.);
#16478=ADVANCED_FACE('',(#710),#15964,.F.);
#16479=ADVANCED_FACE('',(#711),#15965,.F.);
#16480=ADVANCED_FACE('',(#712),#15966,.F.);
#16481=ADVANCED_FACE('',(#713),#15967,.F.);
#16482=ADVANCED_FACE('',(#714),#15968,.F.);
#16483=ADVANCED_FACE('',(#715),#15969,.F.);
#16484=ADVANCED_FACE('',(#716),#15970,.F.);
#16485=ADVANCED_FACE('',(#717),#15971,.F.);
#16486=ADVANCED_FACE('',(#718),#15972,.F.);
#16487=ADVANCED_FACE('',(#719),#15973,.F.);
#16488=ADVANCED_FACE('',(#720),#15974,.F.);
#16489=ADVANCED_FACE('',(#721),#15975,.F.);
#16490=ADVANCED_FACE('',(#722),#15976,.F.);
#16491=ADVANCED_FACE('',(#723),#317,.T.);
#16492=ADVANCED_FACE('',(#724),#281,.F.);
#16493=ADVANCED_FACE('',(#725),#282,.F.);
#16494=ADVANCED_FACE('',(#726),#318,.T.);
#16495=ADVANCED_FACE('',(#727),#283,.F.);
#16496=ADVANCED_FACE('',(#728),#284,.F.);
#16497=ADVANCED_FACE('',(#729),#319,.F.);
#16498=ADVANCED_FACE('',(#730),#320,.F.);
#16499=ADVANCED_FACE('',(#731),#321,.F.);
#16500=ADVANCED_FACE('',(#732),#322,.F.);
#16501=ADVANCED_FACE('',(#733),#323,.F.);
#16502=ADVANCED_FACE('',(#734),#324,.F.);
#16503=ADVANCED_FACE('',(#735),#15977,.F.);
#16504=ADVANCED_FACE('',(#736),#15978,.F.);
#16505=ADVANCED_FACE('',(#737),#15979,.F.);
#16506=ADVANCED_FACE('',(#738),#15980,.F.);
#16507=ADVANCED_FACE('',(#739),#285,.F.);
#16508=ADVANCED_FACE('',(#740),#286,.F.);
#16509=ADVANCED_FACE('',(#741),#287,.F.);
#16510=ADVANCED_FACE('',(#742),#288,.F.);
#16511=ADVANCED_FACE('',(#743),#289,.F.);
#16512=ADVANCED_FACE('',(#744),#290,.F.);
#16513=ADVANCED_FACE('',(#745),#291,.F.);
#16514=ADVANCED_FACE('',(#746),#292,.F.);
#16515=ADVANCED_FACE('',(#747),#325,.F.);
#16516=ADVANCED_FACE('',(#748),#326,.F.);
#16517=ADVANCED_FACE('',(#749),#327,.F.);
#16518=ADVANCED_FACE('',(#750),#328,.F.);
#16519=ADVANCED_FACE('',(#751,#199),#15981,.F.);
#16520=ADVANCED_FACE('',(#752,#200,#201,#202,#203,#204),#329,.T.);
#16521=ADVANCED_FACE('',(#753),#330,.T.);
#16522=ADVANCED_FACE('',(#754),#331,.T.);
#16523=ADVANCED_FACE('',(#755),#332,.T.);
#16524=ADVANCED_FACE('',(#756),#333,.T.);
#16525=ADVANCED_FACE('',(#757,#205,#206,#207,#208),#334,.F.);
#16526=ADVANCED_FACE('',(#758),#335,.T.);
#16527=ADVANCED_FACE('',(#759,#209),#336,.T.);
#16528=ADVANCED_FACE('',(#760),#337,.T.);
#16529=ADVANCED_FACE('',(#761,#210,#211,#212,#213,#214),#338,.T.);
#16530=ADVANCED_FACE('',(#762,#215,#216,#217),#339,.T.);
#16531=ADVANCED_FACE('',(#763),#340,.F.);
#16532=ADVANCED_FACE('',(#764),#341,.F.);
#16533=ADVANCED_FACE('',(#765),#342,.F.);
#16534=ADVANCED_FACE('',(#766),#15982,.F.);
#16535=ADVANCED_FACE('',(#767),#15983,.T.);
#16536=ADVANCED_FACE('',(#768),#343,.T.);
#16537=ADVANCED_FACE('',(#769),#15984,.F.);
#16538=ADVANCED_FACE('',(#770),#15985,.F.);
#16539=ADVANCED_FACE('',(#771),#15986,.F.);
#16540=ADVANCED_FACE('',(#772),#15987,.F.);
#16541=ADVANCED_FACE('',(#773),#15988,.F.);
#16542=ADVANCED_FACE('',(#774),#15989,.F.);
#16543=ADVANCED_FACE('',(#775),#15990,.F.);
#16544=ADVANCED_FACE('',(#776),#15991,.F.);
#16545=ADVANCED_FACE('',(#777),#15992,.F.);
#16546=ADVANCED_FACE('',(#778),#15993,.F.);
#16547=ADVANCED_FACE('',(#779),#15994,.F.);
#16548=ADVANCED_FACE('',(#780),#15995,.F.);
#16549=ADVANCED_FACE('',(#781),#15996,.F.);
#16550=ADVANCED_FACE('',(#782),#15997,.F.);
#16551=ADVANCED_FACE('',(#783),#15998,.F.);
#16552=ADVANCED_FACE('',(#784),#15999,.F.);
#16553=ADVANCED_FACE('',(#785),#16000,.F.);
#16554=ADVANCED_FACE('',(#786),#16001,.F.);
#16555=ADVANCED_FACE('',(#787),#16002,.F.);
#16556=ADVANCED_FACE('',(#788),#16003,.F.);
#16557=ADVANCED_FACE('',(#789),#16004,.F.);
#16558=ADVANCED_FACE('',(#790),#16005,.F.);
#16559=ADVANCED_FACE('',(#791),#16006,.F.);
#16560=ADVANCED_FACE('',(#792),#16007,.F.);
#16561=ADVANCED_FACE('',(#793),#16008,.F.);
#16562=ADVANCED_FACE('',(#794),#16009,.F.);
#16563=ADVANCED_FACE('',(#795),#16010,.F.);
#16564=ADVANCED_FACE('',(#796),#16011,.F.);
#16565=ADVANCED_FACE('',(#797),#16012,.F.);
#16566=ADVANCED_FACE('',(#798),#16013,.F.);
#16567=ADVANCED_FACE('',(#799),#16014,.F.);
#16568=ADVANCED_FACE('',(#800),#16015,.F.);
#16569=ADVANCED_FACE('',(#801),#16016,.F.);
#16570=ADVANCED_FACE('',(#802),#16017,.F.);
#16571=ADVANCED_FACE('',(#803),#16018,.F.);
#16572=ADVANCED_FACE('',(#804),#16019,.F.);
#16573=ADVANCED_FACE('',(#805),#16020,.F.);
#16574=ADVANCED_FACE('',(#806),#16021,.F.);
#16575=ADVANCED_FACE('',(#807),#16022,.F.);
#16576=ADVANCED_FACE('',(#808),#16023,.F.);
#16577=ADVANCED_FACE('',(#809),#16024,.F.);
#16578=ADVANCED_FACE('',(#810),#16025,.F.);
#16579=ADVANCED_FACE('',(#811),#16026,.F.);
#16580=ADVANCED_FACE('',(#812),#16027,.F.);
#16581=ADVANCED_FACE('',(#813),#16028,.F.);
#16582=ADVANCED_FACE('',(#814),#16029,.F.);
#16583=ADVANCED_FACE('',(#815),#16030,.F.);
#16584=ADVANCED_FACE('',(#816),#16031,.F.);
#16585=ADVANCED_FACE('',(#817),#16032,.F.);
#16586=ADVANCED_FACE('',(#818),#16033,.F.);
#16587=ADVANCED_FACE('',(#819),#16034,.F.);
#16588=ADVANCED_FACE('',(#820,#218),#344,.F.);
#16589=ADVANCED_FACE('',(#821),#111,.F.);
#16590=ADVANCED_FACE('',(#822),#345,.F.);
#16591=ADVANCED_FACE('',(#823),#346,.F.);
#16592=ADVANCED_FACE('',(#824),#347,.F.);
#16593=ADVANCED_FACE('',(#825,#219),#348,.T.);
#16594=ADVANCED_FACE('',(#826),#349,.F.);
#16595=ADVANCED_FACE('',(#827),#293,.F.);
#16596=ADVANCED_FACE('',(#828),#294,.F.);
#16597=ADVANCED_FACE('',(#829,#220),#350,.F.);
#16598=ADVANCED_FACE('',(#830),#16035,.F.);
#16599=ADVANCED_FACE('',(#831),#16036,.T.);
#16600=ADVANCED_FACE('',(#832,#221),#351,.F.);
#16601=ADVANCED_FACE('',(#833),#352,.T.);
#16602=ADVANCED_FACE('',(#834),#112,.T.);
#16603=ADVANCED_FACE('',(#835,#222),#353,.T.);
#16604=ADVANCED_FACE('',(#836),#16037,.T.);
#16605=ADVANCED_FACE('',(#837),#113,.T.);
#16606=ADVANCED_FACE('',(#838),#16038,.F.);
#16607=ADVANCED_FACE('',(#839),#16039,.F.);
#16608=ADVANCED_FACE('',(#840,#223,#224,#225),#354,.F.);
#16609=ADVANCED_FACE('',(#841),#355,.T.);
#16610=ADVANCED_FACE('',(#842),#356,.T.);
#16611=ADVANCED_FACE('',(#843),#357,.T.);
#16612=ADVANCED_FACE('',(#844),#358,.T.);
#16613=ADVANCED_FACE('',(#845,#226,#227),#359,.T.);
#16614=ADVANCED_FACE('',(#846),#360,.T.);
#16615=ADVANCED_FACE('',(#847),#361,.T.);
#16616=ADVANCED_FACE('',(#848),#362,.T.);
#16617=ADVANCED_FACE('',(#849),#363,.T.);
#16618=ADVANCED_FACE('',(#850),#364,.F.);
#16619=ADVANCED_FACE('',(#851),#365,.F.);
#16620=ADVANCED_FACE('',(#852),#366,.T.);
#16621=ADVANCED_FACE('',(#853,#228,#229,#230,#231,#232),#367,.F.);
#16622=ADVANCED_FACE('',(#854),#16040,.F.);
#16623=ADVANCED_FACE('',(#855),#16041,.F.);
#16624=ADVANCED_FACE('',(#856),#16042,.F.);
#16625=ADVANCED_FACE('',(#857),#16043,.F.);
#16626=ADVANCED_FACE('',(#858),#16044,.F.);
#16627=ADVANCED_FACE('',(#859),#368,.T.);
#16628=ADVANCED_FACE('',(#860),#369,.T.);
#16629=ADVANCED_FACE('',(#861,#233,#234,#235,#236,#237),#370,.T.);
#16630=ADVANCED_FACE('',(#862),#16045,.F.);
#16631=ADVANCED_FACE('',(#863),#16046,.T.);
#16632=ADVANCED_FACE('',(#864,#238),#371,.T.);
#16633=ADVANCED_FACE('',(#865,#239),#372,.F.);
#16634=ADVANCED_FACE('',(#866),#16047,.T.);
#16635=ADVANCED_FACE('',(#867),#16048,.T.);
#16636=ADVANCED_FACE('',(#868),#16049,.T.);
#16637=ADVANCED_FACE('',(#869),#16050,.T.);
#16638=ADVANCED_FACE('',(#870),#16051,.T.);
#16639=ADVANCED_FACE('',(#871),#16052,.T.);
#16640=ADVANCED_FACE('',(#872),#16053,.T.);
#16641=ADVANCED_FACE('',(#873),#16054,.T.);
#16642=ADVANCED_FACE('',(#874),#16055,.T.);
#16643=ADVANCED_FACE('',(#875),#16056,.T.);
#16644=ADVANCED_FACE('',(#876),#16057,.T.);
#16645=ADVANCED_FACE('',(#877),#16058,.T.);
#16646=ADVANCED_FACE('',(#878),#16059,.T.);
#16647=ADVANCED_FACE('',(#879),#16060,.T.);
#16648=ADVANCED_FACE('',(#880),#16061,.T.);
#16649=ADVANCED_FACE('',(#881),#16062,.T.);
#16650=ADVANCED_FACE('',(#882),#16063,.T.);
#16651=ADVANCED_FACE('',(#883),#16064,.T.);
#16652=ADVANCED_FACE('',(#884),#16065,.T.);
#16653=ADVANCED_FACE('',(#885),#16066,.T.);
#16654=ADVANCED_FACE('',(#886),#16067,.T.);
#16655=ADVANCED_FACE('',(#887),#16068,.T.);
#16656=ADVANCED_FACE('',(#888),#16069,.T.);
#16657=ADVANCED_FACE('',(#889),#16070,.T.);
#16658=ADVANCED_FACE('',(#890),#16071,.T.);
#16659=ADVANCED_FACE('',(#891),#16072,.T.);
#16660=ADVANCED_FACE('',(#892),#16073,.T.);
#16661=ADVANCED_FACE('',(#893),#16074,.T.);
#16662=ADVANCED_FACE('',(#894),#16075,.T.);
#16663=ADVANCED_FACE('',(#895),#16076,.T.);
#16664=ADVANCED_FACE('',(#896),#16077,.T.);
#16665=ADVANCED_FACE('',(#897),#16078,.T.);
#16666=ADVANCED_FACE('',(#898),#16079,.T.);
#16667=ADVANCED_FACE('',(#899),#16080,.T.);
#16668=ADVANCED_FACE('',(#900),#16081,.T.);
#16669=ADVANCED_FACE('',(#901),#16082,.T.);
#16670=ADVANCED_FACE('',(#902),#16083,.T.);
#16671=ADVANCED_FACE('',(#903),#16084,.T.);
#16672=ADVANCED_FACE('',(#904),#16085,.T.);
#16673=ADVANCED_FACE('',(#905),#16086,.T.);
#16674=ADVANCED_FACE('',(#906),#16087,.T.);
#16675=ADVANCED_FACE('',(#907),#16088,.T.);
#16676=ADVANCED_FACE('',(#908),#16089,.T.);
#16677=ADVANCED_FACE('',(#909),#16090,.T.);
#16678=ADVANCED_FACE('',(#910),#16091,.T.);
#16679=ADVANCED_FACE('',(#911),#16092,.T.);
#16680=ADVANCED_FACE('',(#912),#16093,.T.);
#16681=ADVANCED_FACE('',(#913),#16094,.T.);
#16682=ADVANCED_FACE('',(#914),#16095,.T.);
#16683=ADVANCED_FACE('',(#915),#16096,.T.);
#16684=ADVANCED_FACE('',(#916),#16097,.T.);
#16685=ADVANCED_FACE('',(#917),#16098,.T.);
#16686=ADVANCED_FACE('',(#918),#16099,.T.);
#16687=ADVANCED_FACE('',(#919),#16100,.T.);
#16688=ADVANCED_FACE('',(#920),#16101,.T.);
#16689=ADVANCED_FACE('',(#921),#16102,.T.);
#16690=ADVANCED_FACE('',(#922),#16103,.T.);
#16691=ADVANCED_FACE('',(#923),#16104,.T.);
#16692=ADVANCED_FACE('',(#924),#16105,.T.);
#16693=ADVANCED_FACE('',(#925),#16106,.T.);
#16694=ADVANCED_FACE('',(#926),#16107,.T.);
#16695=ADVANCED_FACE('',(#927),#16108,.T.);
#16696=ADVANCED_FACE('',(#928),#16109,.T.);
#16697=ADVANCED_FACE('',(#929),#16110,.T.);
#16698=ADVANCED_FACE('',(#930),#16111,.T.);
#16699=ADVANCED_FACE('',(#931),#16112,.T.);
#16700=ADVANCED_FACE('',(#932),#16113,.T.);
#16701=ADVANCED_FACE('',(#933),#16114,.F.);
#16702=ADVANCED_FACE('',(#934),#295,.F.);
#16703=ADVANCED_FACE('',(#935),#296,.F.);
#16704=ADVANCED_FACE('',(#936),#373,.T.);
#16705=ADVANCED_FACE('',(#937,#240),#374,.F.);
#16706=ADVANCED_FACE('',(#938),#16115,.T.);
#16707=ADVANCED_FACE('',(#939,#241),#16116,.T.);
#16708=ADVANCED_FACE('',(#940,#242),#375,.T.);
#16709=ADVANCED_FACE('',(#941),#376,.F.);
#16710=ADVANCED_FACE('',(#942),#16117,.F.);
#16711=ADVANCED_FACE('',(#943),#16118,.F.);
#16712=ADVANCED_FACE('',(#944),#16119,.F.);
#16713=ADVANCED_FACE('',(#945),#16120,.F.);
#16714=ADVANCED_FACE('',(#946),#16121,.F.);
#16715=ADVANCED_FACE('',(#947),#16122,.F.);
#16716=ADVANCED_FACE('',(#948),#16123,.F.);
#16717=ADVANCED_FACE('',(#949),#16124,.F.);
#16718=ADVANCED_FACE('',(#950,#243),#16125,.T.);
#16719=ADVANCED_FACE('',(#951,#244),#377,.T.);
#16720=ADVANCED_FACE('',(#952,#245),#16126,.F.);
#16721=ADVANCED_FACE('',(#953),#16127,.T.);
#16722=ADVANCED_FACE('',(#954,#246,#247,#248,#249,#250,#251,#252),#378,
 .T.);
#16723=ADVANCED_FACE('',(#955,#253,#254,#255,#256,#257,#258,#259),#379,
 .F.);
#16724=ADVANCED_FACE('',(#956),#16128,.T.);
#16725=ADVANCED_FACE('',(#957,#260),#380,.F.);
#16726=ADVANCED_FACE('',(#958,#261),#381,.F.);
#16727=ADVANCED_FACE('',(#959),#16129,.T.);
#16728=ADVANCED_FACE('',(#960,#262),#382,.T.);
#16729=ADVANCED_FACE('',(#961),#16130,.T.);
#16730=ADVANCED_FACE('',(#962),#383,.F.);
#16731=ADVANCED_FACE('',(#963),#16131,.T.);
#16732=ADVANCED_FACE('',(#964),#384,.T.);
#16733=ADVANCED_FACE('',(#965),#16132,.F.);
#16734=ADVANCED_FACE('',(#966),#16133,.T.);
#16735=ADVANCED_FACE('',(#967,#263),#385,.T.);
#16736=ADVANCED_FACE('',(#968,#264),#386,.F.);
#16737=ADVANCED_FACE('',(#969),#387,.F.);
#16738=ADVANCED_FACE('',(#970),#388,.F.);
#16739=ADVANCED_FACE('',(#971),#389,.F.);
#16740=ADVANCED_FACE('',(#972),#16134,.F.);
#16741=ADVANCED_FACE('',(#973),#16135,.T.);
#16742=ADVANCED_FACE('',(#974),#390,.T.);
#16743=ADVANCED_FACE('',(#975),#16136,.F.);
#16744=ADVANCED_FACE('',(#976),#16137,.T.);
#16745=ADVANCED_FACE('',(#977,#265),#391,.T.);
#16746=ADVANCED_FACE('',(#978,#266),#392,.F.);
#16747=ADVANCED_FACE('',(#979),#114,.T.);
#16748=ADVANCED_FACE('',(#980),#16138,.T.);
#16749=ADVANCED_FACE('',(#981),#16139,.T.);
#16750=ADVANCED_FACE('',(#982),#16140,.T.);
#16751=ADVANCED_FACE('',(#983),#16141,.T.);
#16752=ADVANCED_FACE('',(#984),#16142,.T.);
#16753=ADVANCED_FACE('',(#985),#16143,.T.);
#16754=ADVANCED_FACE('',(#986),#16144,.T.);
#16755=ADVANCED_FACE('',(#987),#16145,.T.);
#16756=ADVANCED_FACE('',(#988),#16146,.T.);
#16757=ADVANCED_FACE('',(#989),#16147,.T.);
#16758=ADVANCED_FACE('',(#990),#16148,.T.);
#16759=ADVANCED_FACE('',(#991),#16149,.T.);
#16760=ADVANCED_FACE('',(#992),#16150,.T.);
#16761=ADVANCED_FACE('',(#993),#16151,.T.);
#16762=ADVANCED_FACE('',(#994),#16152,.T.);
#16763=ADVANCED_FACE('',(#995),#16153,.T.);
#16764=ADVANCED_FACE('',(#996),#16154,.T.);
#16765=ADVANCED_FACE('',(#997),#16155,.T.);
#16766=ADVANCED_FACE('',(#998),#115,.T.);
#16767=ADVANCED_FACE('',(#999),#297,.F.);
#16768=ADVANCED_FACE('',(#1000),#298,.F.);
#16769=ADVANCED_FACE('',(#1001),#393,.F.);
#16770=ADVANCED_FACE('',(#1002),#394,.F.);
#16771=ADVANCED_FACE('',(#1003),#395,.F.);
#16772=ADVANCED_FACE('',(#1004),#396,.F.);
#16773=ADVANCED_FACE('',(#1005),#397,.F.);
#16774=ADVANCED_FACE('',(#1006),#398,.F.);
#16775=ADVANCED_FACE('',(#1007),#399,.F.);
#16776=ADVANCED_FACE('',(#1008,#267),#400,.T.);
#16777=ADVANCED_FACE('',(#1009),#16156,.T.);
#16778=ADVANCED_FACE('',(#1010,#268),#401,.F.);
#16779=ADVANCED_FACE('',(#1011),#402,.T.);
#16780=ADVANCED_FACE('',(#1012),#116,.T.);
#16781=ADVANCED_FACE('',(#1013),#16157,.T.);
#16782=ADVANCED_FACE('',(#1014),#16158,.T.);
#16783=ADVANCED_FACE('',(#1015),#16159,.T.);
#16784=ADVANCED_FACE('',(#1016),#16160,.T.);
#16785=ADVANCED_FACE('',(#1017),#16161,.T.);
#16786=ADVANCED_FACE('',(#1018),#16162,.T.);
#16787=ADVANCED_FACE('',(#1019),#16163,.T.);
#16788=ADVANCED_FACE('',(#1020),#16164,.T.);
#16789=ADVANCED_FACE('',(#1021),#16165,.T.);
#16790=ADVANCED_FACE('',(#1022),#16166,.T.);
#16791=ADVANCED_FACE('',(#1023),#16167,.T.);
#16792=ADVANCED_FACE('',(#1024),#16168,.T.);
#16793=ADVANCED_FACE('',(#1025),#16169,.T.);
#16794=ADVANCED_FACE('',(#1026),#16170,.T.);
#16795=ADVANCED_FACE('',(#1027),#16171,.T.);
#16796=ADVANCED_FACE('',(#1028),#16172,.T.);
#16797=ADVANCED_FACE('',(#1029),#16173,.T.);
#16798=ADVANCED_FACE('',(#1030),#16174,.T.);
#16799=ADVANCED_FACE('',(#1031),#16175,.T.);
#16800=ADVANCED_FACE('',(#1032),#16176,.T.);
#16801=ADVANCED_FACE('',(#1033),#16177,.T.);
#16802=ADVANCED_FACE('',(#1034),#16178,.T.);
#16803=ADVANCED_FACE('',(#1035),#16179,.T.);
#16804=ADVANCED_FACE('',(#1036),#16180,.T.);
#16805=ADVANCED_FACE('',(#1037),#16181,.T.);
#16806=ADVANCED_FACE('',(#1038),#16182,.T.);
#16807=ADVANCED_FACE('',(#1039),#16183,.T.);
#16808=ADVANCED_FACE('',(#1040),#16184,.T.);
#16809=ADVANCED_FACE('',(#1041),#16185,.T.);
#16810=ADVANCED_FACE('',(#1042),#16186,.T.);
#16811=ADVANCED_FACE('',(#1043),#117,.T.);
#16812=ADVANCED_FACE('',(#1044),#299,.F.);
#16813=ADVANCED_FACE('',(#1045),#300,.F.);
#16814=ADVANCED_FACE('',(#1046),#403,.F.);
#16815=ADVANCED_FACE('',(#1047),#404,.F.);
#16816=ADVANCED_FACE('',(#1048),#405,.F.);
#16817=ADVANCED_FACE('',(#1049),#406,.F.);
#16818=ADVANCED_FACE('',(#1050),#407,.F.);
#16819=ADVANCED_FACE('',(#1051),#408,.F.);
#16820=ADVANCED_FACE('',(#1052),#409,.F.);
#16821=ADVANCED_FACE('',(#1053,#269),#410,.T.);
#16822=ADVANCED_FACE('',(#1054),#16187,.T.);
#16823=ADVANCED_FACE('',(#1055,#270),#411,.F.);
#16824=ADVANCED_FACE('',(#1056),#412,.T.);
#16825=ADVANCED_FACE('',(#1057),#16188,.T.);
#16826=ADVANCED_FACE('',(#1058),#16189,.T.);
#16827=ADVANCED_FACE('',(#1059),#118,.T.);
#16828=ADVANCED_FACE('',(#1060),#301,.F.);
#16829=ADVANCED_FACE('',(#1061),#302,.F.);
#16830=ADVANCED_FACE('',(#1062),#413,.F.);
#16831=ADVANCED_FACE('',(#1063),#414,.F.);
#16832=ADVANCED_FACE('',(#1064),#415,.F.);
#16833=ADVANCED_FACE('',(#1065),#416,.F.);
#16834=ADVANCED_FACE('',(#1066),#417,.F.);
#16835=ADVANCED_FACE('',(#1067),#418,.F.);
#16836=ADVANCED_FACE('',(#1068),#419,.F.);
#16837=ADVANCED_FACE('',(#1069,#271),#420,.T.);
#16838=ADVANCED_FACE('',(#1070),#16190,.T.);
#16839=ADVANCED_FACE('',(#1071,#272),#421,.F.);
#16840=ADVANCED_FACE('',(#1072),#422,.T.);
#16841=CLOSED_SHELL('',(#16191,#16192,#16193,#16194,#16195,#16196,#16197,
#16198,#16199,#16200,#16201,#16202,#16203,#16204,#16205,#16206,#16207,#16208,
#16209,#16210,#16211,#16212,#16213,#16214,#16215,#16216,#16217,#16218,#16219,
#16220,#16221,#16222,#16223,#16224,#16225,#16226,#16227,#16228,#16229,#16230,
#16231,#16232,#16233,#16234,#16235,#16236,#16237,#16238,#16239,#16240,#16241,
#16242,#16243,#16244,#16245,#16246,#16247,#16248,#16249,#16250,#16251,#16252,
#16253,#16254,#16255,#16256,#16257,#16258,#16259,#16260,#16261,#16262,#16263,
#16264,#16265,#16266,#16267,#16268,#16269,#16270,#16271,#16272,#16273,#16274,
#16275,#16276,#16277,#16278,#16279,#16280,#16281,#16282,#16283,#16284,#16285,
#16286,#16287,#16288,#16289,#16290,#16291,#16292,#16293,#16294,#16295,#16296,
#16297,#16298,#16299,#16300,#16301,#16302,#16303,#16304));
#16842=CLOSED_SHELL('',(#16305,#16306,#16307,#16308,#16309,#16310,#16311,
#16312,#16313,#16314,#16315,#16316,#16317,#16318,#16319,#16320,#16321,#16322,
#16323,#16324,#16325,#16326,#16327,#16328,#16329,#16330,#16331,#16332,#16333,
#16334,#16335,#16336,#16337,#16338,#16339,#16340,#16341,#16342,#16343,#16344,
#16345,#16346,#16347,#16348,#16349,#16350,#16351,#16352,#16353,#16354,#16355,
#16356,#16357,#16358,#16359,#16360,#16361,#16362,#16363,#16364,#16365,#16366,
#16367,#16368,#16369,#16370,#16371,#16372,#16373,#16374,#16375,#16376,#16377,
#16378,#16379,#16380,#16381,#16382,#16383,#16384,#16385,#16386,#16387,#16388,
#16389,#16390,#16391,#16392,#16393,#16394,#16395,#16396,#16397,#16398,#16399,
#16400,#16401,#16402,#16403,#16404,#16405,#16406,#16407,#16408,#16409,#16410,
#16411,#16412,#16413,#16414,#16415,#16416,#16417,#16418,#16419,#16420,#16421,
#16422,#16423,#16424,#16425,#16426,#16427,#16428,#16429,#16430,#16431,#16432,
#16433,#16434,#16435,#16436,#16437,#16438,#16439,#16440,#16441,#16442,#16443,
#16444,#16445,#16446,#16447,#16448,#16449,#16450,#16451,#16452,#16453,#16454,
#16455,#16456,#16457,#16458,#16459,#16460,#16461,#16462,#16463,#16464,#16465,
#16466,#16467,#16468,#16469,#16470,#16471,#16472,#16473,#16474,#16475,#16476,
#16477,#16478,#16479,#16480,#16481,#16482,#16483,#16484,#16485,#16486,#16487,
#16488,#16489,#16490,#16491,#16492,#16493,#16494,#16495,#16496,#16497,#16498,
#16499,#16500,#16501,#16502,#16503,#16504,#16505,#16506,#16507,#16508,#16509,
#16510,#16511,#16512,#16513,#16514,#16515,#16516,#16517,#16518,#16519,#16520,
#16521,#16522,#16523,#16524,#16525,#16526,#16527,#16528,#16529,#16530));
#16843=CLOSED_SHELL('',(#16531,#16532,#16533,#16534,#16535,#16536));
#16844=CLOSED_SHELL('',(#16537,#16538,#16539,#16540,#16541,#16542,#16543,
#16544,#16545,#16546,#16547,#16548,#16549,#16550,#16551,#16552,#16553,#16554,
#16555,#16556,#16557,#16558,#16559,#16560,#16561,#16562,#16563,#16564,#16565,
#16566,#16567,#16568,#16569,#16570,#16571,#16572,#16573,#16574,#16575,#16576,
#16577,#16578,#16579,#16580,#16581,#16582,#16583,#16584,#16585,#16586,#16587,
#16588,#16589,#16590,#16591,#16592,#16593,#16594,#16595,#16596,#16597,#16598,
#16599,#16600));
#16845=CLOSED_SHELL('',(#16601,#16602,#16603,#16604,#16605));
#16846=CLOSED_SHELL('',(#16606,#16607,#16608,#16609,#16610,#16611,#16612,
#16613,#16614,#16615,#16616,#16617,#16618));
#16847=CLOSED_SHELL('',(#16619,#16620,#16621,#16622,#16623,#16624,#16625,
#16626,#16627,#16628,#16629));
#16848=CLOSED_SHELL('',(#16630,#16631,#16632,#16633));
#16849=CLOSED_SHELL('',(#16634,#16635,#16636,#16637,#16638,#16639,#16640,
#16641,#16642,#16643,#16644,#16645,#16646,#16647,#16648,#16649,#16650,#16651,
#16652,#16653,#16654,#16655,#16656,#16657,#16658,#16659,#16660,#16661,#16662,
#16663,#16664,#16665,#16666,#16667,#16668,#16669,#16670,#16671,#16672,#16673,
#16674,#16675,#16676,#16677,#16678,#16679,#16680,#16681,#16682,#16683,#16684,
#16685,#16686,#16687,#16688,#16689,#16690,#16691,#16692,#16693,#16694,#16695,
#16696,#16697,#16698,#16699,#16700,#16701,#16702,#16703,#16704,#16705,#16706,
#16707,#16708,#16709));
#16850=CLOSED_SHELL('',(#16710,#16711,#16712,#16713,#16714,#16715,#16716,
#16717,#16718,#16719,#16720,#16721,#16722,#16723));
#16851=CLOSED_SHELL('',(#16724,#16725,#16726,#16727,#16728,#16729,#16730,
#16731,#16732));
#16852=CLOSED_SHELL('',(#16733,#16734,#16735,#16736));
#16853=CLOSED_SHELL('',(#16737,#16738,#16739,#16740,#16741,#16742));
#16854=CLOSED_SHELL('',(#16743,#16744,#16745,#16746));
#16855=CLOSED_SHELL('',(#16747,#16748,#16749,#16750,#16751,#16752,#16753,
#16754,#16755,#16756,#16757,#16758,#16759,#16760,#16761,#16762,#16763,#16764,
#16765,#16766,#16767,#16768,#16769,#16770,#16771,#16772,#16773,#16774,#16775,
#16776,#16777,#16778,#16779));
#16856=CLOSED_SHELL('',(#16780,#16781,#16782,#16783,#16784,#16785,#16786,
#16787,#16788,#16789,#16790,#16791,#16792,#16793,#16794,#16795,#16796,#16797,
#16798,#16799,#16800,#16801,#16802,#16803,#16804,#16805,#16806,#16807,#16808,
#16809,#16810,#16811,#16812,#16813,#16814,#16815,#16816,#16817,#16818,#16819,
#16820,#16821,#16822,#16823,#16824));
#16857=CLOSED_SHELL('',(#16825,#16826,#16827,#16828,#16829,#16830,#16831,
#16832,#16833,#16834,#16835,#16836,#16837,#16838,#16839,#16840));
#16858=DERIVED_UNIT_ELEMENT(#16892,1.);
#16859=DERIVED_UNIT_ELEMENT(#289389,-3.);
#16860=DERIVED_UNIT_ELEMENT(#16892,1.);
#16861=DERIVED_UNIT_ELEMENT(#289389,-3.);
#16862=DERIVED_UNIT_ELEMENT(#16892,1.);
#16863=DERIVED_UNIT_ELEMENT(#289389,-3.);
#16864=DERIVED_UNIT_ELEMENT(#16892,1.);
#16865=DERIVED_UNIT_ELEMENT(#289389,-3.);
#16866=DERIVED_UNIT_ELEMENT(#16892,1.);
#16867=DERIVED_UNIT_ELEMENT(#289389,-3.);
#16868=DERIVED_UNIT_ELEMENT(#16892,1.);
#16869=DERIVED_UNIT_ELEMENT(#289389,-3.);
#16870=DERIVED_UNIT_ELEMENT(#16892,1.);
#16871=DERIVED_UNIT_ELEMENT(#289389,-3.);
#16872=DERIVED_UNIT_ELEMENT(#16892,1.);
#16873=DERIVED_UNIT_ELEMENT(#289389,-3.);
#16874=DERIVED_UNIT_ELEMENT(#16892,1.);
#16875=DERIVED_UNIT_ELEMENT(#289389,-3.);
#16876=DERIVED_UNIT_ELEMENT(#16892,1.);
#16877=DERIVED_UNIT_ELEMENT(#289389,-3.);
#16878=DERIVED_UNIT_ELEMENT(#16892,1.);
#16879=DERIVED_UNIT_ELEMENT(#289389,-3.);
#16880=DERIVED_UNIT_ELEMENT(#16892,1.);
#16881=DERIVED_UNIT_ELEMENT(#289389,-3.);
#16882=DERIVED_UNIT_ELEMENT(#16892,1.);
#16883=DERIVED_UNIT_ELEMENT(#289389,-3.);
#16884=DERIVED_UNIT_ELEMENT(#16892,1.);
#16885=DERIVED_UNIT_ELEMENT(#289389,-3.);
#16886=DERIVED_UNIT_ELEMENT(#16892,1.);
#16887=DERIVED_UNIT_ELEMENT(#289389,-3.);
#16888=DERIVED_UNIT_ELEMENT(#16892,1.);
#16889=DERIVED_UNIT_ELEMENT(#289389,-3.);
#16890=DERIVED_UNIT_ELEMENT(#16892,1.);
#16891=DERIVED_UNIT_ELEMENT(#289389,-3.);
#16892=(
MASS_UNIT()
NAMED_UNIT(*)
SI_UNIT(.KILO.,.GRAM.)
);
#16893=DERIVED_UNIT((#16858,#16859));
#16894=DERIVED_UNIT((#16860,#16861));
#16895=DERIVED_UNIT((#16862,#16863));
#16896=DERIVED_UNIT((#16864,#16865));
#16897=DERIVED_UNIT((#16866,#16867));
#16898=DERIVED_UNIT((#16868,#16869));
#16899=DERIVED_UNIT((#16870,#16871));
#16900=DERIVED_UNIT((#16872,#16873));
#16901=DERIVED_UNIT((#16874,#16875));
#16902=DERIVED_UNIT((#16876,#16877));
#16903=DERIVED_UNIT((#16878,#16879));
#16904=DERIVED_UNIT((#16880,#16881));
#16905=DERIVED_UNIT((#16882,#16883));
#16906=DERIVED_UNIT((#16884,#16885));
#16907=DERIVED_UNIT((#16886,#16887));
#16908=DERIVED_UNIT((#16888,#16889));
#16909=DERIVED_UNIT((#16890,#16891));
#16910=MEASURE_REPRESENTATION_ITEM('density measure',
POSITIVE_RATIO_MEASURE(7850.),#16893);
#16911=MEASURE_REPRESENTATION_ITEM('density measure',
POSITIVE_RATIO_MEASURE(7850.),#16894);
#16912=MEASURE_REPRESENTATION_ITEM('density measure',
POSITIVE_RATIO_MEASURE(8920.),#16895);
#16913=MEASURE_REPRESENTATION_ITEM('density measure',
POSITIVE_RATIO_MEASURE(7850.),#16896);
#16914=MEASURE_REPRESENTATION_ITEM('density measure',
POSITIVE_RATIO_MEASURE(7850.),#16897);
#16915=MEASURE_REPRESENTATION_ITEM('density measure',
POSITIVE_RATIO_MEASURE(7850.),#16898);
#16916=MEASURE_REPRESENTATION_ITEM('density measure',
POSITIVE_RATIO_MEASURE(7850.),#16899);
#16917=MEASURE_REPRESENTATION_ITEM('density measure',
POSITIVE_RATIO_MEASURE(8920.),#16900);
#16918=MEASURE_REPRESENTATION_ITEM('density measure',
POSITIVE_RATIO_MEASURE(7850.),#16901);
#16919=MEASURE_REPRESENTATION_ITEM('density measure',
POSITIVE_RATIO_MEASURE(7850.),#16902);
#16920=MEASURE_REPRESENTATION_ITEM('density measure',
POSITIVE_RATIO_MEASURE(7850.),#16903);
#16921=MEASURE_REPRESENTATION_ITEM('density measure',
POSITIVE_RATIO_MEASURE(7850.),#16904);
#16922=MEASURE_REPRESENTATION_ITEM('density measure',
POSITIVE_RATIO_MEASURE(7850.),#16905);
#16923=MEASURE_REPRESENTATION_ITEM('density measure',
POSITIVE_RATIO_MEASURE(8920.),#16906);
#16924=MEASURE_REPRESENTATION_ITEM('density measure',
POSITIVE_RATIO_MEASURE(7850.),#16907);
#16925=MEASURE_REPRESENTATION_ITEM('density measure',
POSITIVE_RATIO_MEASURE(7850.),#16908);
#16926=MEASURE_REPRESENTATION_ITEM('density measure',
POSITIVE_RATIO_MEASURE(7850.),#16909);
#16927=PROPERTY_DEFINITION_REPRESENTATION(#17012,#16961);
#16928=PROPERTY_DEFINITION_REPRESENTATION(#17013,#16962);
#16929=PROPERTY_DEFINITION_REPRESENTATION(#17014,#16963);
#16930=PROPERTY_DEFINITION_REPRESENTATION(#17015,#16964);
#16931=PROPERTY_DEFINITION_REPRESENTATION(#17016,#16965);
#16932=PROPERTY_DEFINITION_REPRESENTATION(#17017,#16966);
#16933=PROPERTY_DEFINITION_REPRESENTATION(#17018,#16967);
#16934=PROPERTY_DEFINITION_REPRESENTATION(#17019,#16968);
#16935=PROPERTY_DEFINITION_REPRESENTATION(#17020,#16969);
#16936=PROPERTY_DEFINITION_REPRESENTATION(#17021,#16970);
#16937=PROPERTY_DEFINITION_REPRESENTATION(#17022,#16971);
#16938=PROPERTY_DEFINITION_REPRESENTATION(#17023,#16972);
#16939=PROPERTY_DEFINITION_REPRESENTATION(#17024,#16973);
#16940=PROPERTY_DEFINITION_REPRESENTATION(#17025,#16974);
#16941=PROPERTY_DEFINITION_REPRESENTATION(#17026,#16975);
#16942=PROPERTY_DEFINITION_REPRESENTATION(#17027,#16976);
#16943=PROPERTY_DEFINITION_REPRESENTATION(#17028,#16977);
#16944=PROPERTY_DEFINITION_REPRESENTATION(#17029,#16978);
#16945=PROPERTY_DEFINITION_REPRESENTATION(#17030,#16979);
#16946=PROPERTY_DEFINITION_REPRESENTATION(#17031,#16980);
#16947=PROPERTY_DEFINITION_REPRESENTATION(#17032,#16981);
#16948=PROPERTY_DEFINITION_REPRESENTATION(#17033,#16982);
#16949=PROPERTY_DEFINITION_REPRESENTATION(#17034,#16983);
#16950=PROPERTY_DEFINITION_REPRESENTATION(#17035,#16984);
#16951=PROPERTY_DEFINITION_REPRESENTATION(#17036,#16985);
#16952=PROPERTY_DEFINITION_REPRESENTATION(#17037,#16986);
#16953=PROPERTY_DEFINITION_REPRESENTATION(#17038,#16987);
#16954=PROPERTY_DEFINITION_REPRESENTATION(#17039,#16988);
#16955=PROPERTY_DEFINITION_REPRESENTATION(#17040,#16989);
#16956=PROPERTY_DEFINITION_REPRESENTATION(#17041,#16990);
#16957=PROPERTY_DEFINITION_REPRESENTATION(#17042,#16991);
#16958=PROPERTY_DEFINITION_REPRESENTATION(#17043,#16992);
#16959=PROPERTY_DEFINITION_REPRESENTATION(#17044,#16993);
#16960=PROPERTY_DEFINITION_REPRESENTATION(#17045,#16994);
#16961=REPRESENTATION('material name',(#16995),#289370);
#16962=REPRESENTATION('density',(#16910),#289370);
#16963=REPRESENTATION('material name',(#16996),#289371);
#16964=REPRESENTATION('density',(#16911),#289371);
#16965=REPRESENTATION('material name',(#16997),#289372);
#16966=REPRESENTATION('density',(#16912),#289372);
#16967=REPRESENTATION('material name',(#16998),#289373);
#16968=REPRESENTATION('density',(#16913),#289373);
#16969=REPRESENTATION('material name',(#16999),#289374);
#16970=REPRESENTATION('density',(#16914),#289374);
#16971=REPRESENTATION('material name',(#17000),#289375);
#16972=REPRESENTATION('density',(#16915),#289375);
#16973=REPRESENTATION('material name',(#17001),#289376);
#16974=REPRESENTATION('density',(#16916),#289376);
#16975=REPRESENTATION('material name',(#17002),#289377);
#16976=REPRESENTATION('density',(#16917),#289377);
#16977=REPRESENTATION('material name',(#17003),#289378);
#16978=REPRESENTATION('density',(#16918),#289378);
#16979=REPRESENTATION('material name',(#17004),#289379);
#16980=REPRESENTATION('density',(#16919),#289379);
#16981=REPRESENTATION('material name',(#17005),#289380);
#16982=REPRESENTATION('density',(#16920),#289380);
#16983=REPRESENTATION('material name',(#17006),#289381);
#16984=REPRESENTATION('density',(#16921),#289381);
#16985=REPRESENTATION('material name',(#17007),#289382);
#16986=REPRESENTATION('density',(#16922),#289382);
#16987=REPRESENTATION('material name',(#17008),#289383);
#16988=REPRESENTATION('density',(#16923),#289383);
#16989=REPRESENTATION('material name',(#17009),#289384);
#16990=REPRESENTATION('density',(#16924),#289384);
#16991=REPRESENTATION('material name',(#17010),#289385);
#16992=REPRESENTATION('density',(#16925),#289385);
#16993=REPRESENTATION('material name',(#17011),#289386);
#16994=REPRESENTATION('density',(#16926),#289386);
#16995=DESCRIPTIVE_REPRESENTATION_ITEM('Steel','Steel');
#16996=DESCRIPTIVE_REPRESENTATION_ITEM('Steel','Steel');
#16997=DESCRIPTIVE_REPRESENTATION_ITEM('Copper, Alloy','Copper, Alloy');
#16998=DESCRIPTIVE_REPRESENTATION_ITEM('Steel','Steel');
#16999=DESCRIPTIVE_REPRESENTATION_ITEM('Steel','Steel');
#17000=DESCRIPTIVE_REPRESENTATION_ITEM('Steel','Steel');
#17001=DESCRIPTIVE_REPRESENTATION_ITEM('Steel','Steel');
#17002=DESCRIPTIVE_REPRESENTATION_ITEM('Copper, Alloy','Copper, Alloy');
#17003=DESCRIPTIVE_REPRESENTATION_ITEM('Steel','Steel');
#17004=DESCRIPTIVE_REPRESENTATION_ITEM('Steel','Steel');
#17005=DESCRIPTIVE_REPRESENTATION_ITEM('Steel','Steel');
#17006=DESCRIPTIVE_REPRESENTATION_ITEM('Steel','Steel');
#17007=DESCRIPTIVE_REPRESENTATION_ITEM('Steel','Steel');
#17008=DESCRIPTIVE_REPRESENTATION_ITEM('Copper, Alloy','Copper, Alloy');
#17009=DESCRIPTIVE_REPRESENTATION_ITEM('Steel','Steel');
#17010=DESCRIPTIVE_REPRESENTATION_ITEM('Steel','Steel');
#17011=DESCRIPTIVE_REPRESENTATION_ITEM('Steel','Steel');
#17012=PROPERTY_DEFINITION('material property','material name',#289473);
#17013=PROPERTY_DEFINITION('material property','density of part',#289473);
#17014=PROPERTY_DEFINITION('material property','material name',#289474);
#17015=PROPERTY_DEFINITION('material property','density of part',#289474);
#17016=PROPERTY_DEFINITION('material property','material name',#289475);
#17017=PROPERTY_DEFINITION('material property','density of part',#289475);
#17018=PROPERTY_DEFINITION('material property','material name',#289476);
#17019=PROPERTY_DEFINITION('material property','density of part',#289476);
#17020=PROPERTY_DEFINITION('material property','material name',#289477);
#17021=PROPERTY_DEFINITION('material property','density of part',#289477);
#17022=PROPERTY_DEFINITION('material property','material name',#289478);
#17023=PROPERTY_DEFINITION('material property','density of part',#289478);
#17024=PROPERTY_DEFINITION('material property','material name',#289479);
#17025=PROPERTY_DEFINITION('material property','density of part',#289479);
#17026=PROPERTY_DEFINITION('material property','material name',#289480);
#17027=PROPERTY_DEFINITION('material property','density of part',#289480);
#17028=PROPERTY_DEFINITION('material property','material name',#289481);
#17029=PROPERTY_DEFINITION('material property','density of part',#289481);
#17030=PROPERTY_DEFINITION('material property','material name',#289482);
#17031=PROPERTY_DEFINITION('material property','density of part',#289482);
#17032=PROPERTY_DEFINITION('material property','material name',#289483);
#17033=PROPERTY_DEFINITION('material property','density of part',#289483);
#17034=PROPERTY_DEFINITION('material property','material name',#289484);
#17035=PROPERTY_DEFINITION('material property','density of part',#289484);
#17036=PROPERTY_DEFINITION('material property','material name',#289485);
#17037=PROPERTY_DEFINITION('material property','density of part',#289485);
#17038=PROPERTY_DEFINITION('material property','material name',#289486);
#17039=PROPERTY_DEFINITION('material property','density of part',#289486);
#17040=PROPERTY_DEFINITION('material property','material name',#289487);
#17041=PROPERTY_DEFINITION('material property','density of part',#289487);
#17042=PROPERTY_DEFINITION('material property','material name',#289488);
#17043=PROPERTY_DEFINITION('material property','density of part',#289488);
#17044=PROPERTY_DEFINITION('material property','material name',#289489);
#17045=PROPERTY_DEFINITION('material property','density of part',#289489);
#17046=AXIS2_PLACEMENT_3D('',#20212,#17889,#17890);
#17047=AXIS2_PLACEMENT_3D('',#20213,#17891,#17892);
#17048=AXIS2_PLACEMENT_3D('',#20214,#17893,#17894);
#17049=AXIS2_PLACEMENT_3D('',#20370,#17896,#17897);
#17050=AXIS2_PLACEMENT_3D('',#20563,#17898,#17899);
#17051=AXIS2_PLACEMENT_3D('',#21032,#17901,#17902);
#17052=AXIS2_PLACEMENT_3D('',#21498,#17904,#17905);
#17053=AXIS2_PLACEMENT_3D('',#21961,#17907,#17908);
#17054=AXIS2_PLACEMENT_3D('',#22424,#17910,#17911);
#17055=AXIS2_PLACEMENT_3D('',#22890,#17913,#17914);
#17056=AXIS2_PLACEMENT_3D('',#23353,#17916,#17917);
#17057=AXIS2_PLACEMENT_3D('',#23819,#17919,#17920);
#17058=AXIS2_PLACEMENT_3D('',#24288,#17922,#17923);
#17059=AXIS2_PLACEMENT_3D('',#24382,#17925,#17926);
#17060=AXIS2_PLACEMENT_3D('',#24530,#17927,#17928);
#17061=AXIS2_PLACEMENT_3D('',#24633,#17930,#17931);
#17062=AXIS2_PLACEMENT_3D('',#24636,#17933,#17934);
#17063=AXIS2_PLACEMENT_3D('',#24638,#17935,#17936);
#17064=AXIS2_PLACEMENT_3D('',#24773,#17937,#17938);
#17065=AXIS2_PLACEMENT_3D('',#25164,#17940,#17941);
#17066=AXIS2_PLACEMENT_3D('',#25551,#17943,#17944);
#17067=AXIS2_PLACEMENT_3D('',#25936,#17946,#17947);
#17068=AXIS2_PLACEMENT_3D('',#26327,#17949,#17950);
#17069=AXIS2_PLACEMENT_3D('',#26714,#17952,#17953);
#17070=AXIS2_PLACEMENT_3D('',#27095,#17955,#17956);
#17071=AXIS2_PLACEMENT_3D('',#27488,#17958,#17959);
#17072=AXIS2_PLACEMENT_3D('',#27894,#17961,#17962);
#17073=AXIS2_PLACEMENT_3D('',#28026,#17964,#17965);
#17074=AXIS2_PLACEMENT_3D('',#28205,#17966,#17967);
#17075=AXIS2_PLACEMENT_3D('',#28361,#17969,#17970);
#17076=AXIS2_PLACEMENT_3D('',#28554,#17971,#17972);
#17077=AXIS2_PLACEMENT_3D('',#29023,#17974,#17975);
#17078=AXIS2_PLACEMENT_3D('',#29489,#17977,#17978);
#17079=AXIS2_PLACEMENT_3D('',#29952,#17980,#17981);
#17080=AXIS2_PLACEMENT_3D('',#30415,#17983,#17984);
#17081=AXIS2_PLACEMENT_3D('',#30881,#17986,#17987);
#17082=AXIS2_PLACEMENT_3D('',#31344,#17989,#17990);
#17083=AXIS2_PLACEMENT_3D('',#31810,#17992,#17993);
#17084=AXIS2_PLACEMENT_3D('',#32279,#17995,#17996);
#17085=AXIS2_PLACEMENT_3D('',#32373,#17998,#17999);
#17086=AXIS2_PLACEMENT_3D('',#32521,#18000,#18001);
#17087=AXIS2_PLACEMENT_3D('',#32624,#18003,#18004);
#17088=AXIS2_PLACEMENT_3D('',#32627,#18006,#18007);
#17089=AXIS2_PLACEMENT_3D('',#32629,#18008,#18009);
#17090=AXIS2_PLACEMENT_3D('',#32768,#18010,#18011);
#17091=AXIS2_PLACEMENT_3D('',#33161,#18013,#18014);
#17092=AXIS2_PLACEMENT_3D('',#33540,#18016,#18017);
#17093=AXIS2_PLACEMENT_3D('',#33923,#18019,#18020);
#17094=AXIS2_PLACEMENT_3D('',#34310,#18022,#18023);
#17095=AXIS2_PLACEMENT_3D('',#34705,#18025,#18026);
#17096=AXIS2_PLACEMENT_3D('',#35086,#18028,#18029);
#17097=AXIS2_PLACEMENT_3D('',#35481,#18031,#18032);
#17098=AXIS2_PLACEMENT_3D('',#35887,#18034,#18035);
#17099=AXIS2_PLACEMENT_3D('',#36021,#18037,#18038);
#17100=AXIS2_PLACEMENT_3D('',#36200,#18039,#18040);
#17101=AXIS2_PLACEMENT_3D('',#36356,#18042,#18043);
#17102=AXIS2_PLACEMENT_3D('',#36549,#18044,#18045);
#17103=AXIS2_PLACEMENT_3D('',#37018,#18047,#18048);
#17104=AXIS2_PLACEMENT_3D('',#37484,#18050,#18051);
#17105=AXIS2_PLACEMENT_3D('',#37947,#18053,#18054);
#17106=AXIS2_PLACEMENT_3D('',#38410,#18056,#18057);
#17107=AXIS2_PLACEMENT_3D('',#38876,#18059,#18060);
#17108=AXIS2_PLACEMENT_3D('',#39339,#18062,#18063);
#17109=AXIS2_PLACEMENT_3D('',#39805,#18065,#18066);
#17110=AXIS2_PLACEMENT_3D('',#40274,#18068,#18069);
#17111=AXIS2_PLACEMENT_3D('',#40368,#18071,#18072);
#17112=AXIS2_PLACEMENT_3D('',#40516,#18073,#18074);
#17113=AXIS2_PLACEMENT_3D('',#40619,#18076,#18077);
#17114=AXIS2_PLACEMENT_3D('',#40622,#18079,#18080);
#17115=AXIS2_PLACEMENT_3D('',#40624,#18081,#18082);
#17116=AXIS2_PLACEMENT_3D('',#40763,#18083,#18084);
#17117=AXIS2_PLACEMENT_3D('',#41156,#18086,#18087);
#17118=AXIS2_PLACEMENT_3D('',#41547,#18089,#18090);
#17119=AXIS2_PLACEMENT_3D('',#41932,#18092,#18093);
#17120=AXIS2_PLACEMENT_3D('',#42325,#18095,#18096);
#17121=AXIS2_PLACEMENT_3D('',#42716,#18098,#18099);
#17122=AXIS2_PLACEMENT_3D('',#43101,#18101,#18102);
#17123=AXIS2_PLACEMENT_3D('',#43496,#18104,#18105);
#17124=AXIS2_PLACEMENT_3D('',#43900,#18107,#18108);
#17125=AXIS2_PLACEMENT_3D('',#44034,#18110,#18111);
#17126=AXIS2_PLACEMENT_3D('',#44211,#18112,#18113);
#17127=AXIS2_PLACEMENT_3D('',#44367,#18115,#18116);
#17128=AXIS2_PLACEMENT_3D('',#44560,#18117,#18118);
#17129=AXIS2_PLACEMENT_3D('',#45029,#18120,#18121);
#17130=AXIS2_PLACEMENT_3D('',#45495,#18123,#18124);
#17131=AXIS2_PLACEMENT_3D('',#45958,#18126,#18127);
#17132=AXIS2_PLACEMENT_3D('',#46421,#18129,#18130);
#17133=AXIS2_PLACEMENT_3D('',#46887,#18132,#18133);
#17134=AXIS2_PLACEMENT_3D('',#47350,#18135,#18136);
#17135=AXIS2_PLACEMENT_3D('',#47816,#18138,#18139);
#17136=AXIS2_PLACEMENT_3D('',#48285,#18141,#18142);
#17137=AXIS2_PLACEMENT_3D('',#48379,#18144,#18145);
#17138=AXIS2_PLACEMENT_3D('',#48527,#18146,#18147);
#17139=AXIS2_PLACEMENT_3D('',#48630,#18149,#18150);
#17140=AXIS2_PLACEMENT_3D('',#48633,#18152,#18153);
#17141=AXIS2_PLACEMENT_3D('',#48635,#18154,#18155);
#17142=AXIS2_PLACEMENT_3D('',#48774,#18156,#18157);
#17143=AXIS2_PLACEMENT_3D('',#49163,#18159,#18160);
#17144=AXIS2_PLACEMENT_3D('',#49550,#18162,#18163);
#17145=AXIS2_PLACEMENT_3D('',#49931,#18165,#18166);
#17146=AXIS2_PLACEMENT_3D('',#50324,#18168,#18169);
#17147=AXIS2_PLACEMENT_3D('',#50719,#18171,#18172);
#17148=AXIS2_PLACEMENT_3D('',#51102,#18174,#18175);
#17149=AXIS2_PLACEMENT_3D('',#51499,#18177,#18178);
#17150=AXIS2_PLACEMENT_3D('',#51905,#18180,#18181);
#17151=AXIS2_PLACEMENT_3D('',#52039,#18183,#18184);
#17152=AXIS2_PLACEMENT_3D('',#52220,#18185,#18186);
#17153=AXIS2_PLACEMENT_3D('',#52602,#18187,#18188);
#17154=AXIS2_PLACEMENT_3D('',#53062,#18189,#18190);
#17155=AXIS2_PLACEMENT_3D('',#53444,#18191,#18192);
#17156=AXIS2_PLACEMENT_3D('',#53904,#18193,#18194);
#17157=AXIS2_PLACEMENT_3D('',#54282,#18195,#18196);
#17158=AXIS2_PLACEMENT_3D('',#54742,#18197,#18198);
#17159=AXIS2_PLACEMENT_3D('',#55124,#18199,#18200);
#17160=AXIS2_PLACEMENT_3D('',#55584,#18201,#18202);
#17161=AXIS2_PLACEMENT_3D('',#56549,#18203,#18204);
#17162=AXIS2_PLACEMENT_3D('',#57514,#18205,#18206);
#17163=AXIS2_PLACEMENT_3D('',#58479,#18207,#18208);
#17164=AXIS2_PLACEMENT_3D('',#59441,#18209,#18210);
#17165=AXIS2_PLACEMENT_3D('',#59442,#18211,#18212);
#17166=AXIS2_PLACEMENT_3D('',#59443,#18213,#18214);
#17167=AXIS2_PLACEMENT_3D('',#59444,#18215,#18216);
#17168=AXIS2_PLACEMENT_3D('',#59445,#18217,#18218);
#17169=AXIS2_PLACEMENT_3D('',#59447,#18219,#18220);
#17170=AXIS2_PLACEMENT_3D('',#59450,#18222,#18223);
#17171=AXIS2_PLACEMENT_3D('',#59451,#18224,#18225);
#17172=AXIS2_PLACEMENT_3D('',#59453,#18226,#18227);
#17173=AXIS2_PLACEMENT_3D('',#59456,#18229,#18230);
#17174=AXIS2_PLACEMENT_3D('',#59457,#18231,#18232);
#17175=AXIS2_PLACEMENT_3D('',#59459,#18233,#18234);
#17176=AXIS2_PLACEMENT_3D('',#59462,#18236,#18237);
#17177=AXIS2_PLACEMENT_3D('',#59463,#18238,#18239);
#17178=AXIS2_PLACEMENT_3D('',#59465,#18240,#18241);
#17179=AXIS2_PLACEMENT_3D('',#59468,#18243,#18244);
#17180=AXIS2_PLACEMENT_3D('',#59469,#18245,#18246);
#17181=AXIS2_PLACEMENT_3D('',#59478,#18251,#18252);
#17182=AXIS2_PLACEMENT_3D('',#59484,#18256,#18257);
#17183=AXIS2_PLACEMENT_3D('',#59490,#18261,#18262);
#17184=AXIS2_PLACEMENT_3D('',#59493,#18265,#18266);
#17185=AXIS2_PLACEMENT_3D('',#59494,#18267,#18268);
#17186=AXIS2_PLACEMENT_3D('',#59495,#18269,#18270);
#17187=AXIS2_PLACEMENT_3D('',#59496,#18271,#18272);
#17188=AXIS2_PLACEMENT_3D('',#59506,#18274,#18275);
#17189=AXIS2_PLACEMENT_3D('',#59538,#18276,#18277);
#17190=AXIS2_PLACEMENT_3D('',#59865,#18279,#18280);
#17191=AXIS2_PLACEMENT_3D('',#60259,#18282,#18283);
#17192=AXIS2_PLACEMENT_3D('',#60650,#18285,#18286);
#17193=AXIS2_PLACEMENT_3D('',#61041,#18288,#18289);
#17194=AXIS2_PLACEMENT_3D('',#61429,#18291,#18292);
#17195=AXIS2_PLACEMENT_3D('',#61820,#18294,#18295);
#17196=AXIS2_PLACEMENT_3D('',#62211,#18297,#18298);
#17197=AXIS2_PLACEMENT_3D('',#62599,#18300,#18301);
#17198=AXIS2_PLACEMENT_3D('',#62993,#18303,#18304);
#17199=AXIS2_PLACEMENT_3D('',#63384,#18306,#18307);
#17200=AXIS2_PLACEMENT_3D('',#63775,#18309,#18310);
#17201=AXIS2_PLACEMENT_3D('',#64169,#18312,#18313);
#17202=AXIS2_PLACEMENT_3D('',#64560,#18315,#18316);
#17203=AXIS2_PLACEMENT_3D('',#64948,#18318,#18319);
#17204=AXIS2_PLACEMENT_3D('',#65030,#18321,#18322);
#17205=AXIS2_PLACEMENT_3D('',#65157,#18323,#18324);
#17206=AXIS2_PLACEMENT_3D('',#65323,#18326,#18327);
#17207=AXIS2_PLACEMENT_3D('',#65337,#18329,#18330);
#17208=AXIS2_PLACEMENT_3D('',#65584,#18331,#18332);
#17209=AXIS2_PLACEMENT_3D('',#65814,#18334,#18335);
#17210=AXIS2_PLACEMENT_3D('',#66227,#18337,#18338);
#17211=AXIS2_PLACEMENT_3D('',#66673,#18340,#18341);
#17212=AXIS2_PLACEMENT_3D('',#67129,#18343,#18344);
#17213=AXIS2_PLACEMENT_3D('',#67561,#18346,#18347);
#17214=AXIS2_PLACEMENT_3D('',#67993,#18349,#18350);
#17215=AXIS2_PLACEMENT_3D('',#68393,#18352,#18353);
#17216=AXIS2_PLACEMENT_3D('',#68847,#18355,#18356);
#17217=AXIS2_PLACEMENT_3D('',#69283,#18358,#18359);
#17218=AXIS2_PLACEMENT_3D('',#69711,#18361,#18362);
#17219=AXIS2_PLACEMENT_3D('',#70123,#18364,#18365);
#17220=AXIS2_PLACEMENT_3D('',#70551,#18367,#18368);
#17221=AXIS2_PLACEMENT_3D('',#70967,#18370,#18371);
#17222=AXIS2_PLACEMENT_3D('',#71107,#18373,#18374);
#17223=AXIS2_PLACEMENT_3D('',#71310,#18375,#18376);
#17224=AXIS2_PLACEMENT_3D('',#71320,#18378,#18379);
#17225=AXIS2_PLACEMENT_3D('',#71352,#18380,#18381);
#17226=AXIS2_PLACEMENT_3D('',#71679,#18383,#18384);
#17227=AXIS2_PLACEMENT_3D('',#72073,#18386,#18387);
#17228=AXIS2_PLACEMENT_3D('',#72464,#18389,#18390);
#17229=AXIS2_PLACEMENT_3D('',#72855,#18392,#18393);
#17230=AXIS2_PLACEMENT_3D('',#73243,#18395,#18396);
#17231=AXIS2_PLACEMENT_3D('',#73634,#18398,#18399);
#17232=AXIS2_PLACEMENT_3D('',#74025,#18401,#18402);
#17233=AXIS2_PLACEMENT_3D('',#74413,#18404,#18405);
#17234=AXIS2_PLACEMENT_3D('',#74807,#18407,#18408);
#17235=AXIS2_PLACEMENT_3D('',#75198,#18410,#18411);
#17236=AXIS2_PLACEMENT_3D('',#75589,#18413,#18414);
#17237=AXIS2_PLACEMENT_3D('',#75983,#18416,#18417);
#17238=AXIS2_PLACEMENT_3D('',#76374,#18419,#18420);
#17239=AXIS2_PLACEMENT_3D('',#76762,#18422,#18423);
#17240=AXIS2_PLACEMENT_3D('',#76844,#18425,#18426);
#17241=AXIS2_PLACEMENT_3D('',#76971,#18427,#18428);
#17242=AXIS2_PLACEMENT_3D('',#77137,#18430,#18431);
#17243=AXIS2_PLACEMENT_3D('',#77153,#18433,#18434);
#17244=AXIS2_PLACEMENT_3D('',#77446,#18435,#18436);
#17245=AXIS2_PLACEMENT_3D('',#77680,#18438,#18439);
#17246=AXIS2_PLACEMENT_3D('',#78091,#18441,#18442);
#17247=AXIS2_PLACEMENT_3D('',#78507,#18444,#18445);
#17248=AXIS2_PLACEMENT_3D('',#78965,#18447,#18448);
#17249=AXIS2_PLACEMENT_3D('',#79393,#18450,#18451);
#17250=AXIS2_PLACEMENT_3D('',#79803,#18453,#18454);
#17251=AXIS2_PLACEMENT_3D('',#80231,#18456,#18457);
#17252=AXIS2_PLACEMENT_3D('',#80683,#18459,#18460);
#17253=AXIS2_PLACEMENT_3D('',#81127,#18462,#18463);
#17254=AXIS2_PLACEMENT_3D('',#81555,#18465,#18466);
#17255=AXIS2_PLACEMENT_3D('',#81967,#18468,#18469);
#17256=AXIS2_PLACEMENT_3D('',#82391,#18471,#18472);
#17257=AXIS2_PLACEMENT_3D('',#82817,#18474,#18475);
#17258=AXIS2_PLACEMENT_3D('',#82967,#18477,#18478);
#17259=AXIS2_PLACEMENT_3D('',#83174,#18479,#18480);
#17260=AXIS2_PLACEMENT_3D('',#83188,#18482,#18483);
#17261=AXIS2_PLACEMENT_3D('',#83330,#18484,#18485);
#17262=AXIS2_PLACEMENT_3D('',#83660,#18487,#18488);
#17263=AXIS2_PLACEMENT_3D('',#84051,#18490,#18491);
#17264=AXIS2_PLACEMENT_3D('',#84439,#18493,#18494);
#17265=AXIS2_PLACEMENT_3D('',#84830,#18496,#18497);
#17266=AXIS2_PLACEMENT_3D('',#85221,#18499,#18500);
#17267=AXIS2_PLACEMENT_3D('',#85609,#18502,#18503);
#17268=AXIS2_PLACEMENT_3D('',#86000,#18505,#18506);
#17269=AXIS2_PLACEMENT_3D('',#86391,#18508,#18509);
#17270=AXIS2_PLACEMENT_3D('',#86782,#18511,#18512);
#17271=AXIS2_PLACEMENT_3D('',#87176,#18514,#18515);
#17272=AXIS2_PLACEMENT_3D('',#87451,#18517,#18518);
#17273=AXIS2_PLACEMENT_3D('',#87778,#18520,#18521);
#17274=AXIS2_PLACEMENT_3D('',#87860,#18523,#18524);
#17275=AXIS2_PLACEMENT_3D('',#87987,#18525,#18526);
#17276=AXIS2_PLACEMENT_3D('',#88001,#18528,#18529);
#17277=AXIS2_PLACEMENT_3D('',#88143,#18530,#18531);
#17278=AXIS2_PLACEMENT_3D('',#88473,#18533,#18534);
#17279=AXIS2_PLACEMENT_3D('',#88864,#18536,#18537);
#17280=AXIS2_PLACEMENT_3D('',#89252,#18539,#18540);
#17281=AXIS2_PLACEMENT_3D('',#89643,#18542,#18543);
#17282=AXIS2_PLACEMENT_3D('',#90034,#18545,#18546);
#17283=AXIS2_PLACEMENT_3D('',#90422,#18548,#18549);
#17284=AXIS2_PLACEMENT_3D('',#90813,#18551,#18552);
#17285=AXIS2_PLACEMENT_3D('',#91204,#18554,#18555);
#17286=AXIS2_PLACEMENT_3D('',#91595,#18557,#18558);
#17287=AXIS2_PLACEMENT_3D('',#91989,#18560,#18561);
#17288=AXIS2_PLACEMENT_3D('',#92264,#18563,#18564);
#17289=AXIS2_PLACEMENT_3D('',#92591,#18566,#18567);
#17290=AXIS2_PLACEMENT_3D('',#92673,#18569,#18570);
#17291=AXIS2_PLACEMENT_3D('',#92800,#18571,#18572);
#17292=AXIS2_PLACEMENT_3D('',#92814,#18574,#18575);
#17293=AXIS2_PLACEMENT_3D('',#92956,#18576,#18577);
#17294=AXIS2_PLACEMENT_3D('',#93286,#18579,#18580);
#17295=AXIS2_PLACEMENT_3D('',#93677,#18582,#18583);
#17296=AXIS2_PLACEMENT_3D('',#94065,#18585,#18586);
#17297=AXIS2_PLACEMENT_3D('',#94456,#18588,#18589);
#17298=AXIS2_PLACEMENT_3D('',#94847,#18591,#18592);
#17299=AXIS2_PLACEMENT_3D('',#95235,#18594,#18595);
#17300=AXIS2_PLACEMENT_3D('',#95626,#18597,#18598);
#17301=AXIS2_PLACEMENT_3D('',#96017,#18600,#18601);
#17302=AXIS2_PLACEMENT_3D('',#96408,#18603,#18604);
#17303=AXIS2_PLACEMENT_3D('',#96802,#18606,#18607);
#17304=AXIS2_PLACEMENT_3D('',#97193,#18609,#18610);
#17305=AXIS2_PLACEMENT_3D('',#97581,#18612,#18613);
#17306=AXIS2_PLACEMENT_3D('',#97663,#18615,#18616);
#17307=AXIS2_PLACEMENT_3D('',#97790,#18617,#18618);
#17308=AXIS2_PLACEMENT_3D('',#97804,#18620,#18621);
#17309=AXIS2_PLACEMENT_3D('',#97946,#18622,#18623);
#17310=AXIS2_PLACEMENT_3D('',#98276,#18625,#18626);
#17311=AXIS2_PLACEMENT_3D('',#98667,#18628,#18629);
#17312=AXIS2_PLACEMENT_3D('',#99055,#18631,#18632);
#17313=AXIS2_PLACEMENT_3D('',#99446,#18634,#18635);
#17314=AXIS2_PLACEMENT_3D('',#99837,#18637,#18638);
#17315=AXIS2_PLACEMENT_3D('',#100225,#18640,#18641);
#17316=AXIS2_PLACEMENT_3D('',#100616,#18643,#18644);
#17317=AXIS2_PLACEMENT_3D('',#101007,#18646,#18647);
#17318=AXIS2_PLACEMENT_3D('',#101398,#18649,#18650);
#17319=AXIS2_PLACEMENT_3D('',#101792,#18652,#18653);
#17320=AXIS2_PLACEMENT_3D('',#102183,#18655,#18656);
#17321=AXIS2_PLACEMENT_3D('',#102571,#18658,#18659);
#17322=AXIS2_PLACEMENT_3D('',#102653,#18661,#18662);
#17323=AXIS2_PLACEMENT_3D('',#102780,#18663,#18664);
#17324=AXIS2_PLACEMENT_3D('',#102850,#18666,#18667);
#17325=AXIS2_PLACEMENT_3D('',#102971,#18668,#18669);
#17326=AXIS2_PLACEMENT_3D('',#103400,#18671,#18672);
#17327=AXIS2_PLACEMENT_3D('',#103833,#18674,#18675);
#17328=AXIS2_PLACEMENT_3D('',#104270,#18677,#18678);
#17329=AXIS2_PLACEMENT_3D('',#104755,#18680,#18681);
#17330=AXIS2_PLACEMENT_3D('',#105198,#18683,#18684);
#17331=AXIS2_PLACEMENT_3D('',#105618,#18686,#18687);
#17332=AXIS2_PLACEMENT_3D('',#105868,#18689,#18690);
#17333=AXIS2_PLACEMENT_3D('',#106272,#18692,#18693);
#17334=AXIS2_PLACEMENT_3D('',#106707,#18695,#18696);
#17335=AXIS2_PLACEMENT_3D('',#107116,#18698,#18699);
#17336=AXIS2_PLACEMENT_3D('',#107517,#18701,#18702);
#17337=AXIS2_PLACEMENT_3D('',#107934,#18704,#18705);
#17338=AXIS2_PLACEMENT_3D('',#108070,#18707,#18708);
#17339=AXIS2_PLACEMENT_3D('',#108251,#18709,#18710);
#17340=AXIS2_PLACEMENT_3D('',#108321,#18712,#18713);
#17341=AXIS2_PLACEMENT_3D('',#108440,#18714,#18715);
#17342=AXIS2_PLACEMENT_3D('',#108857,#18717,#18718);
#17343=AXIS2_PLACEMENT_3D('',#109290,#18720,#18721);
#17344=AXIS2_PLACEMENT_3D('',#109727,#18723,#18724);
#17345=AXIS2_PLACEMENT_3D('',#110220,#18726,#18727);
#17346=AXIS2_PLACEMENT_3D('',#110663,#18729,#18730);
#17347=AXIS2_PLACEMENT_3D('',#111085,#18732,#18733);
#17348=AXIS2_PLACEMENT_3D('',#111335,#18735,#18736);
#17349=AXIS2_PLACEMENT_3D('',#111733,#18738,#18739);
#17350=AXIS2_PLACEMENT_3D('',#112166,#18741,#18742);
#17351=AXIS2_PLACEMENT_3D('',#112579,#18744,#18745);
#17352=AXIS2_PLACEMENT_3D('',#112996,#18747,#18748);
#17353=AXIS2_PLACEMENT_3D('',#113417,#18750,#18751);
#17354=AXIS2_PLACEMENT_3D('',#113553,#18753,#18754);
#17355=AXIS2_PLACEMENT_3D('',#113728,#18755,#18756);
#17356=AXIS2_PLACEMENT_3D('',#113806,#18758,#18759);
#17357=AXIS2_PLACEMENT_3D('',#113927,#18760,#18761);
#17358=AXIS2_PLACEMENT_3D('',#114353,#18763,#18764);
#17359=AXIS2_PLACEMENT_3D('',#114778,#18766,#18767);
#17360=AXIS2_PLACEMENT_3D('',#115190,#18769,#18770);
#17361=AXIS2_PLACEMENT_3D('',#115679,#18772,#18773);
#17362=AXIS2_PLACEMENT_3D('',#116108,#18775,#18776);
#17363=AXIS2_PLACEMENT_3D('',#116522,#18778,#18779);
#17364=AXIS2_PLACEMENT_3D('',#116772,#18781,#18782);
#17365=AXIS2_PLACEMENT_3D('',#117186,#18784,#18785);
#17366=AXIS2_PLACEMENT_3D('',#117619,#18787,#18788);
#17367=AXIS2_PLACEMENT_3D('',#118018,#18790,#18791);
#17368=AXIS2_PLACEMENT_3D('',#118411,#18793,#18794);
#17369=AXIS2_PLACEMENT_3D('',#118831,#18796,#18797);
#17370=AXIS2_PLACEMENT_3D('',#118967,#18799,#18800);
#17371=AXIS2_PLACEMENT_3D('',#119156,#18801,#18802);
#17372=AXIS2_PLACEMENT_3D('',#119236,#18804,#18805);
#17373=AXIS2_PLACEMENT_3D('',#119359,#18806,#18807);
#17374=AXIS2_PLACEMENT_3D('',#119785,#18809,#18810);
#17375=AXIS2_PLACEMENT_3D('',#120208,#18812,#18813);
#17376=AXIS2_PLACEMENT_3D('',#120624,#18815,#18816);
#17377=AXIS2_PLACEMENT_3D('',#121121,#18818,#18819);
#17378=AXIS2_PLACEMENT_3D('',#121570,#18821,#18822);
#17379=AXIS2_PLACEMENT_3D('',#121976,#18824,#18825);
#17380=AXIS2_PLACEMENT_3D('',#122228,#18827,#18828);
#17381=AXIS2_PLACEMENT_3D('',#122644,#18830,#18831);
#17382=AXIS2_PLACEMENT_3D('',#123077,#18833,#18834);
#17383=AXIS2_PLACEMENT_3D('',#123496,#18836,#18837);
#17384=AXIS2_PLACEMENT_3D('',#123903,#18839,#18840);
#17385=AXIS2_PLACEMENT_3D('',#124323,#18842,#18843);
#17386=AXIS2_PLACEMENT_3D('',#124461,#18845,#18846);
#17387=AXIS2_PLACEMENT_3D('',#124650,#18847,#18848);
#17388=AXIS2_PLACEMENT_3D('',#125148,#18849,#18850);
#17389=AXIS2_PLACEMENT_3D('',#125646,#18851,#18852);
#17390=AXIS2_PLACEMENT_3D('',#126058,#18853,#18854);
#17391=AXIS2_PLACEMENT_3D('',#126460,#18855,#18856);
#17392=AXIS2_PLACEMENT_3D('',#126845,#18857,#18858);
#17393=AXIS2_PLACEMENT_3D('',#127230,#18859,#18860);
#17394=AXIS2_PLACEMENT_3D('',#127615,#18861,#18862);
#17395=AXIS2_PLACEMENT_3D('',#128000,#18863,#18864);
#17396=AXIS2_PLACEMENT_3D('',#128414,#18865,#18866);
#17397=AXIS2_PLACEMENT_3D('',#128799,#18867,#18868);
#17398=AXIS2_PLACEMENT_3D('',#129217,#18869,#18870);
#17399=AXIS2_PLACEMENT_3D('',#129602,#18871,#18872);
#17400=AXIS2_PLACEMENT_3D('',#130783,#18873,#18874);
#17401=AXIS2_PLACEMENT_3D('',#131961,#18875,#18876);
#17402=AXIS2_PLACEMENT_3D('',#131962,#18877,#18878);
#17403=AXIS2_PLACEMENT_3D('',#131963,#18879,#18880);
#17404=AXIS2_PLACEMENT_3D('',#131972,#18885,#18886);
#17405=AXIS2_PLACEMENT_3D('',#131974,#18887,#18888);
#17406=AXIS2_PLACEMENT_3D('',#131978,#18891,#18892);
#17407=AXIS2_PLACEMENT_3D('',#131984,#18896,#18897);
#17408=AXIS2_PLACEMENT_3D('',#131985,#18898,#18899);
#17409=AXIS2_PLACEMENT_3D('',#131987,#18901,#18902);
#17410=AXIS2_PLACEMENT_3D('',#131989,#18903,#18904);
#17411=AXIS2_PLACEMENT_3D('',#131992,#18906,#18907);
#17412=AXIS2_PLACEMENT_3D('',#131993,#18908,#18909);
#17413=AXIS2_PLACEMENT_3D('',#131995,#18910,#18911);
#17414=AXIS2_PLACEMENT_3D('',#131998,#18913,#18914);
#17415=AXIS2_PLACEMENT_3D('',#131999,#18915,#18916);
#17416=AXIS2_PLACEMENT_3D('',#132001,#18917,#18918);
#17417=AXIS2_PLACEMENT_3D('',#132004,#18920,#18921);
#17418=AXIS2_PLACEMENT_3D('',#132005,#18922,#18923);
#17419=AXIS2_PLACEMENT_3D('',#132007,#18924,#18925);
#17420=AXIS2_PLACEMENT_3D('',#132010,#18927,#18928);
#17421=AXIS2_PLACEMENT_3D('',#136451,#18929,#18930);
#17422=AXIS2_PLACEMENT_3D('',#136452,#18931,#18932);
#17423=AXIS2_PLACEMENT_3D('',#136453,#18933,#18934);
#17424=AXIS2_PLACEMENT_3D('',#136454,#18935,#18936);
#17425=AXIS2_PLACEMENT_3D('',#136455,#18937,#18938);
#17426=AXIS2_PLACEMENT_3D('',#136457,#18939,#18940);
#17427=AXIS2_PLACEMENT_3D('',#136460,#18942,#18943);
#17428=AXIS2_PLACEMENT_3D('',#136461,#18944,#18945);
#17429=AXIS2_PLACEMENT_3D('',#136478,#18954,#18955);
#17430=AXIS2_PLACEMENT_3D('',#136484,#18959,#18960);
#17431=AXIS2_PLACEMENT_3D('',#136488,#18963,#18964);
#17432=AXIS2_PLACEMENT_3D('',#136492,#18967,#18968);
#17433=AXIS2_PLACEMENT_3D('',#136494,#18970,#18971);
#17434=AXIS2_PLACEMENT_3D('',#136495,#18972,#18973);
#17435=AXIS2_PLACEMENT_3D('',#136501,#18977,#18978);
#17436=AXIS2_PLACEMENT_3D('',#136505,#18981,#18982);
#17437=AXIS2_PLACEMENT_3D('',#136509,#18985,#18986);
#17438=AXIS2_PLACEMENT_3D('',#136511,#18988,#18989);
#17439=AXIS2_PLACEMENT_3D('',#136512,#18990,#18991);
#17440=AXIS2_PLACEMENT_3D('',#136513,#18992,#18993);
#17441=AXIS2_PLACEMENT_3D('',#136522,#18998,#18999);
#17442=AXIS2_PLACEMENT_3D('',#136531,#19004,#19005);
#17443=AXIS2_PLACEMENT_3D('',#136532,#19006,#19007);
#17444=AXIS2_PLACEMENT_3D('',#136533,#19008,#19009);
#17445=AXIS2_PLACEMENT_3D('',#136534,#19010,#19011);
#17446=AXIS2_PLACEMENT_3D('',#136535,#19012,#19013);
#17447=AXIS2_PLACEMENT_3D('',#136536,#19014,#19015);
#17448=AXIS2_PLACEMENT_3D('',#136537,#19016,#19017);
#17449=AXIS2_PLACEMENT_3D('',#136538,#19018,#19019);
#17450=AXIS2_PLACEMENT_3D('',#136539,#19020,#19021);
#17451=AXIS2_PLACEMENT_3D('',#136540,#19022,#19023);
#17452=AXIS2_PLACEMENT_3D('',#136685,#19025,#19026);
#17453=AXIS2_PLACEMENT_3D('',#136688,#19028,#19029);
#17454=AXIS2_PLACEMENT_3D('',#136690,#19030,#19031);
#17455=AXIS2_PLACEMENT_3D('',#136899,#19032,#19033);
#17456=AXIS2_PLACEMENT_3D('',#137407,#19035,#19036);
#17457=AXIS2_PLACEMENT_3D('',#137918,#19038,#19039);
#17458=AXIS2_PLACEMENT_3D('',#138411,#19041,#19042);
#17459=AXIS2_PLACEMENT_3D('',#138919,#19044,#19045);
#17460=AXIS2_PLACEMENT_3D('',#139430,#19047,#19048);
#17461=AXIS2_PLACEMENT_3D('',#139938,#19050,#19051);
#17462=AXIS2_PLACEMENT_3D('',#140449,#19053,#19054);
#17463=AXIS2_PLACEMENT_3D('',#140957,#19056,#19057);
#17464=AXIS2_PLACEMENT_3D('',#141471,#19059,#19060);
#17465=AXIS2_PLACEMENT_3D('',#141964,#19062,#19063);
#17466=AXIS2_PLACEMENT_3D('',#142472,#19065,#19066);
#17467=AXIS2_PLACEMENT_3D('',#142980,#19068,#19069);
#17468=AXIS2_PLACEMENT_3D('',#143476,#19071,#19072);
#17469=AXIS2_PLACEMENT_3D('',#143990,#19074,#19075);
#17470=AXIS2_PLACEMENT_3D('',#144498,#19077,#19078);
#17471=AXIS2_PLACEMENT_3D('',#145012,#19080,#19081);
#17472=AXIS2_PLACEMENT_3D('',#145523,#19083,#19084);
#17473=AXIS2_PLACEMENT_3D('',#146031,#19086,#19087);
#17474=AXIS2_PLACEMENT_3D('',#146545,#19089,#19090);
#17475=AXIS2_PLACEMENT_3D('',#147035,#19092,#19093);
#17476=AXIS2_PLACEMENT_3D('',#147546,#19095,#19096);
#17477=AXIS2_PLACEMENT_3D('',#148057,#19098,#19099);
#17478=AXIS2_PLACEMENT_3D('',#148547,#19101,#19102);
#17479=AXIS2_PLACEMENT_3D('',#149046,#19104,#19105);
#17480=AXIS2_PLACEMENT_3D('',#149563,#19107,#19108);
#17481=AXIS2_PLACEMENT_3D('',#150056,#19110,#19111);
#17482=AXIS2_PLACEMENT_3D('',#150570,#19113,#19114);
#17483=AXIS2_PLACEMENT_3D('',#151081,#19116,#19117);
#17484=AXIS2_PLACEMENT_3D('',#151580,#19119,#19120);
#17485=AXIS2_PLACEMENT_3D('',#152085,#19122,#19123);
#17486=AXIS2_PLACEMENT_3D('',#152593,#19125,#19126);
#17487=AXIS2_PLACEMENT_3D('',#153107,#19128,#19129);
#17488=AXIS2_PLACEMENT_3D('',#153621,#19131,#19132);
#17489=AXIS2_PLACEMENT_3D('',#154135,#19134,#19135);
#17490=AXIS2_PLACEMENT_3D('',#154637,#19137,#19138);
#17491=AXIS2_PLACEMENT_3D('',#155130,#19140,#19141);
#17492=AXIS2_PLACEMENT_3D('',#155641,#19143,#19144);
#17493=AXIS2_PLACEMENT_3D('',#156152,#19146,#19147);
#17494=AXIS2_PLACEMENT_3D('',#156645,#19149,#19150);
#17495=AXIS2_PLACEMENT_3D('',#157150,#19152,#19153);
#17496=AXIS2_PLACEMENT_3D('',#157664,#19155,#19156);
#17497=AXIS2_PLACEMENT_3D('',#158178,#19158,#19159);
#17498=AXIS2_PLACEMENT_3D('',#158689,#19161,#19162);
#17499=AXIS2_PLACEMENT_3D('',#159200,#19164,#19165);
#17500=AXIS2_PLACEMENT_3D('',#159708,#19167,#19168);
#17501=AXIS2_PLACEMENT_3D('',#160201,#19170,#19171);
#17502=AXIS2_PLACEMENT_3D('',#160709,#19173,#19174);
#17503=AXIS2_PLACEMENT_3D('',#160883,#19176,#19177);
#17504=AXIS2_PLACEMENT_3D('',#161121,#19178,#19179);
#17505=AXIS2_PLACEMENT_3D('',#161629,#19180,#19181);
#17506=AXIS2_PLACEMENT_3D('',#161688,#19182,#19183);
#17507=AXIS2_PLACEMENT_3D('',#170989,#19184,#19185);
#17508=AXIS2_PLACEMENT_3D('',#180353,#19186,#19187);
#17509=AXIS2_PLACEMENT_3D('',#180355,#19188,#19189);
#17510=AXIS2_PLACEMENT_3D('',#180357,#19190,#19191);
#17511=AXIS2_PLACEMENT_3D('',#180358,#19192,#19193);
#17512=AXIS2_PLACEMENT_3D('',#180361,#19195,#19196);
#17513=AXIS2_PLACEMENT_3D('',#180362,#19197,#19198);
#17514=AXIS2_PLACEMENT_3D('',#180371,#19203,#19204);
#17515=AXIS2_PLACEMENT_3D('',#180377,#19208,#19209);
#17516=AXIS2_PLACEMENT_3D('',#180383,#19213,#19214);
#17517=AXIS2_PLACEMENT_3D('',#180384,#19215,#19216);
#17518=AXIS2_PLACEMENT_3D('',#180385,#19217,#19218);
#17519=AXIS2_PLACEMENT_3D('',#185138,#19219,#19220);
#17520=AXIS2_PLACEMENT_3D('',#185140,#19221,#19222);
#17521=AXIS2_PLACEMENT_3D('',#185141,#19223,#19224);
#17522=AXIS2_PLACEMENT_3D('',#185143,#19226,#19227);
#17523=AXIS2_PLACEMENT_3D('',#185144,#19228,#19229);
#17524=AXIS2_PLACEMENT_3D('',#185145,#19230,#19231);
#17525=AXIS2_PLACEMENT_3D('',#185146,#19232,#19233);
#17526=AXIS2_PLACEMENT_3D('',#185147,#19234,#19235);
#17527=AXIS2_PLACEMENT_3D('',#185149,#19236,#19237);
#17528=AXIS2_PLACEMENT_3D('',#185150,#19238,#19239);
#17529=AXIS2_PLACEMENT_3D('',#185152,#19240,#19241);
#17530=AXIS2_PLACEMENT_3D('',#185154,#19243,#19244);
#17531=AXIS2_PLACEMENT_3D('',#185156,#19245,#19246);
#17532=AXIS2_PLACEMENT_3D('',#185157,#19247,#19248);
#17533=AXIS2_PLACEMENT_3D('',#185159,#19249,#19250);
#17534=AXIS2_PLACEMENT_3D('',#185161,#19252,#19253);
#17535=AXIS2_PLACEMENT_3D('',#185164,#19255,#19256);
#17536=AXIS2_PLACEMENT_3D('',#185165,#19257,#19258);
#17537=AXIS2_PLACEMENT_3D('',#185167,#19259,#19260);
#17538=AXIS2_PLACEMENT_3D('',#185170,#19262,#19263);
#17539=AXIS2_PLACEMENT_3D('',#185171,#19264,#19265);
#17540=AXIS2_PLACEMENT_3D('',#185173,#19266,#19267);
#17541=AXIS2_PLACEMENT_3D('',#185176,#19269,#19270);
#17542=AXIS2_PLACEMENT_3D('',#185177,#19271,#19272);
#17543=AXIS2_PLACEMENT_3D('',#185194,#19281,#19282);
#17544=AXIS2_PLACEMENT_3D('',#185200,#19286,#19287);
#17545=AXIS2_PLACEMENT_3D('',#185204,#19290,#19291);
#17546=AXIS2_PLACEMENT_3D('',#185208,#19294,#19295);
#17547=AXIS2_PLACEMENT_3D('',#185210,#19297,#19298);
#17548=AXIS2_PLACEMENT_3D('',#185211,#19299,#19300);
#17549=AXIS2_PLACEMENT_3D('',#185217,#19304,#19305);
#17550=AXIS2_PLACEMENT_3D('',#185221,#19308,#19309);
#17551=AXIS2_PLACEMENT_3D('',#185225,#19312,#19313);
#17552=AXIS2_PLACEMENT_3D('',#185227,#19315,#19316);
#17553=AXIS2_PLACEMENT_3D('',#185228,#19317,#19318);
#17554=AXIS2_PLACEMENT_3D('',#185229,#19319,#19320);
#17555=AXIS2_PLACEMENT_3D('',#185238,#19325,#19326);
#17556=AXIS2_PLACEMENT_3D('',#185244,#19330,#19331);
#17557=AXIS2_PLACEMENT_3D('',#185249,#19334,#19335);
#17558=AXIS2_PLACEMENT_3D('',#185251,#19336,#19337);
#17559=AXIS2_PLACEMENT_3D('',#185253,#19338,#19339);
#17560=AXIS2_PLACEMENT_3D('',#185255,#19340,#19341);
#17561=AXIS2_PLACEMENT_3D('',#185257,#19342,#19343);
#17562=AXIS2_PLACEMENT_3D('',#185258,#19344,#19345);
#17563=AXIS2_PLACEMENT_3D('',#185260,#19346,#19347);
#17564=AXIS2_PLACEMENT_3D('',#185262,#19349,#19350);
#17565=AXIS2_PLACEMENT_3D('',#185264,#19351,#19352);
#17566=AXIS2_PLACEMENT_3D('',#185266,#19354,#19355);
#17567=AXIS2_PLACEMENT_3D('',#185268,#19356,#19357);
#17568=AXIS2_PLACEMENT_3D('',#185270,#19359,#19360);
#17569=AXIS2_PLACEMENT_3D('',#185272,#19361,#19362);
#17570=AXIS2_PLACEMENT_3D('',#185274,#19364,#19365);
#17571=AXIS2_PLACEMENT_3D('',#185276,#19366,#19367);
#17572=AXIS2_PLACEMENT_3D('',#185278,#19369,#19370);
#17573=AXIS2_PLACEMENT_3D('',#185282,#19373,#19374);
#17574=AXIS2_PLACEMENT_3D('',#185284,#19376,#19377);
#17575=AXIS2_PLACEMENT_3D('',#185285,#19378,#19379);
#17576=AXIS2_PLACEMENT_3D('',#185286,#19380,#19381);
#17577=AXIS2_PLACEMENT_3D('',#185288,#19382,#19383);
#17578=AXIS2_PLACEMENT_3D('',#185291,#19385,#19386);
#17579=AXIS2_PLACEMENT_3D('',#185292,#19387,#19388);
#17580=AXIS2_PLACEMENT_3D('',#185294,#19389,#19390);
#17581=AXIS2_PLACEMENT_3D('',#185297,#19392,#19393);
#17582=AXIS2_PLACEMENT_3D('',#185298,#19394,#19395);
#17583=AXIS2_PLACEMENT_3D('',#185299,#19396,#19397);
#17584=AXIS2_PLACEMENT_3D('',#185300,#19398,#19399);
#17585=AXIS2_PLACEMENT_3D('',#185301,#19400,#19401);
#17586=AXIS2_PLACEMENT_3D('',#185440,#19403,#19404);
#17587=AXIS2_PLACEMENT_3D('',#185523,#19405,#19406);
#17588=AXIS2_PLACEMENT_3D('',#186022,#19408,#19409);
#17589=AXIS2_PLACEMENT_3D('',#186518,#19411,#19412);
#17590=AXIS2_PLACEMENT_3D('',#187029,#19414,#19415);
#17591=AXIS2_PLACEMENT_3D('',#187537,#19417,#19418);
#17592=AXIS2_PLACEMENT_3D('',#188030,#19420,#19421);
#17593=AXIS2_PLACEMENT_3D('',#188532,#19423,#19424);
#17594=AXIS2_PLACEMENT_3D('',#189025,#19426,#19427);
#17595=AXIS2_PLACEMENT_3D('',#189527,#19429,#19430);
#17596=AXIS2_PLACEMENT_3D('',#190038,#19432,#19433);
#17597=AXIS2_PLACEMENT_3D('',#190549,#19435,#19436);
#17598=AXIS2_PLACEMENT_3D('',#191048,#19438,#19439);
#17599=AXIS2_PLACEMENT_3D('',#191550,#19441,#19442);
#17600=AXIS2_PLACEMENT_3D('',#192055,#19444,#19445);
#17601=AXIS2_PLACEMENT_3D('',#192563,#19447,#19448);
#17602=AXIS2_PLACEMENT_3D('',#193065,#19450,#19451);
#17603=AXIS2_PLACEMENT_3D('',#193555,#19453,#19454);
#17604=AXIS2_PLACEMENT_3D('',#194042,#19456,#19457);
#17605=AXIS2_PLACEMENT_3D('',#194544,#19459,#19460);
#17606=AXIS2_PLACEMENT_3D('',#195052,#19462,#19463);
#17607=AXIS2_PLACEMENT_3D('',#195566,#19465,#19466);
#17608=AXIS2_PLACEMENT_3D('',#196059,#19468,#19469);
#17609=AXIS2_PLACEMENT_3D('',#196555,#19471,#19472);
#17610=AXIS2_PLACEMENT_3D('',#197060,#19474,#19475);
#17611=AXIS2_PLACEMENT_3D('',#197571,#19477,#19478);
#17612=AXIS2_PLACEMENT_3D('',#198070,#19480,#19481);
#17613=AXIS2_PLACEMENT_3D('',#198557,#19483,#19484);
#17614=AXIS2_PLACEMENT_3D('',#199062,#19486,#19487);
#17615=AXIS2_PLACEMENT_3D('',#199573,#19489,#19490);
#17616=AXIS2_PLACEMENT_3D('',#200084,#19492,#19493);
#17617=AXIS2_PLACEMENT_3D('',#200583,#19495,#19496);
#17618=AXIS2_PLACEMENT_3D('',#201082,#19498,#19499);
#17619=AXIS2_PLACEMENT_3D('',#201575,#19501,#19502);
#17620=AXIS2_PLACEMENT_3D('',#202050,#19504,#19505);
#17621=AXIS2_PLACEMENT_3D('',#202534,#19507,#19508);
#17622=AXIS2_PLACEMENT_3D('',#203030,#19510,#19511);
#17623=AXIS2_PLACEMENT_3D('',#203529,#19513,#19514);
#17624=AXIS2_PLACEMENT_3D('',#204034,#19516,#19517);
#17625=AXIS2_PLACEMENT_3D('',#204533,#19519,#19520);
#17626=AXIS2_PLACEMENT_3D('',#205026,#19522,#19523);
#17627=AXIS2_PLACEMENT_3D('',#205516,#19525,#19526);
#17628=AXIS2_PLACEMENT_3D('',#206015,#19528,#19529);
#17629=AXIS2_PLACEMENT_3D('',#206517,#19531,#19532);
#17630=AXIS2_PLACEMENT_3D('',#207019,#19534,#19535);
#17631=AXIS2_PLACEMENT_3D('',#207515,#19537,#19538);
#17632=AXIS2_PLACEMENT_3D('',#208005,#19540,#19541);
#17633=AXIS2_PLACEMENT_3D('',#208507,#19543,#19544);
#17634=AXIS2_PLACEMENT_3D('',#209000,#19546,#19547);
#17635=AXIS2_PLACEMENT_3D('',#209490,#19549,#19550);
#17636=AXIS2_PLACEMENT_3D('',#209980,#19552,#19553);
#17637=AXIS2_PLACEMENT_3D('',#210467,#19555,#19556);
#17638=AXIS2_PLACEMENT_3D('',#210810,#19558,#19559);
#17639=AXIS2_PLACEMENT_3D('',#211227,#19561,#19562);
#17640=AXIS2_PLACEMENT_3D('',#211732,#19564,#19565);
#17641=AXIS2_PLACEMENT_3D('',#212231,#19567,#19568);
#17642=AXIS2_PLACEMENT_3D('',#212730,#19570,#19571);
#17643=AXIS2_PLACEMENT_3D('',#213238,#19573,#19574);
#17644=AXIS2_PLACEMENT_3D('',#213734,#19576,#19577);
#17645=AXIS2_PLACEMENT_3D('',#214227,#19579,#19580);
#17646=AXIS2_PLACEMENT_3D('',#214705,#19582,#19583);
#17647=AXIS2_PLACEMENT_3D('',#215189,#19585,#19586);
#17648=AXIS2_PLACEMENT_3D('',#215691,#19588,#19589);
#17649=AXIS2_PLACEMENT_3D('',#216199,#19591,#19592);
#17650=AXIS2_PLACEMENT_3D('',#216695,#19594,#19595);
#17651=AXIS2_PLACEMENT_3D('',#217176,#19597,#19598);
#17652=AXIS2_PLACEMENT_3D('',#217188,#19599,#19600);
#17653=AXIS2_PLACEMENT_3D('',#229073,#19601,#19602);
#17654=AXIS2_PLACEMENT_3D('',#241498,#19603,#19604);
#17655=AXIS2_PLACEMENT_3D('',#241666,#19605,#19606);
#17656=AXIS2_PLACEMENT_3D('',#241781,#19607,#19608);
#17657=AXIS2_PLACEMENT_3D('',#247022,#19610,#19611);
#17658=AXIS2_PLACEMENT_3D('',#247023,#19612,#19613);
#17659=AXIS2_PLACEMENT_3D('',#247025,#19614,#19615);
#17660=AXIS2_PLACEMENT_3D('',#247027,#19616,#19617);
#17661=AXIS2_PLACEMENT_3D('',#247028,#19618,#19619);
#17662=AXIS2_PLACEMENT_3D('',#247030,#19620,#19621);
#17663=AXIS2_PLACEMENT_3D('',#247032,#19623,#19624);
#17664=AXIS2_PLACEMENT_3D('',#247036,#19627,#19628);
#17665=AXIS2_PLACEMENT_3D('',#247037,#19629,#19630);
#17666=AXIS2_PLACEMENT_3D('',#247038,#19631,#19632);
#17667=AXIS2_PLACEMENT_3D('',#247039,#19633,#19634);
#17668=AXIS2_PLACEMENT_3D('',#247040,#19635,#19636);
#17669=AXIS2_PLACEMENT_3D('',#247118,#19638,#19639);
#17670=AXIS2_PLACEMENT_3D('',#247202,#19641,#19642);
#17671=AXIS2_PLACEMENT_3D('',#247204,#19643,#19644);
#17672=AXIS2_PLACEMENT_3D('',#247207,#19646,#19647);
#17673=AXIS2_PLACEMENT_3D('',#247208,#19648,#19649);
#17674=AXIS2_PLACEMENT_3D('',#247210,#19650,#19651);
#17675=AXIS2_PLACEMENT_3D('',#247213,#19653,#19654);
#17676=AXIS2_PLACEMENT_3D('',#247214,#19655,#19656);
#17677=AXIS2_PLACEMENT_3D('',#247216,#19657,#19658);
#17678=AXIS2_PLACEMENT_3D('',#247219,#19660,#19661);
#17679=AXIS2_PLACEMENT_3D('',#247220,#19662,#19663);
#17680=AXIS2_PLACEMENT_3D('',#247222,#19664,#19665);
#17681=AXIS2_PLACEMENT_3D('',#247225,#19667,#19668);
#17682=AXIS2_PLACEMENT_3D('',#247226,#19669,#19670);
#17683=AXIS2_PLACEMENT_3D('',#247228,#19671,#19672);
#17684=AXIS2_PLACEMENT_3D('',#247231,#19674,#19675);
#17685=AXIS2_PLACEMENT_3D('',#247232,#19676,#19677);
#17686=AXIS2_PLACEMENT_3D('',#247234,#19678,#19679);
#17687=AXIS2_PLACEMENT_3D('',#247237,#19681,#19682);
#17688=AXIS2_PLACEMENT_3D('',#247238,#19683,#19684);
#17689=AXIS2_PLACEMENT_3D('',#247240,#19685,#19686);
#17690=AXIS2_PLACEMENT_3D('',#247244,#19689,#19690);
#17691=AXIS2_PLACEMENT_3D('',#247245,#19691,#19692);
#17692=AXIS2_PLACEMENT_3D('',#247247,#19693,#19694);
#17693=AXIS2_PLACEMENT_3D('',#247248,#19695,#19696);
#17694=AXIS2_PLACEMENT_3D('',#247250,#19697,#19698);
#17695=AXIS2_PLACEMENT_3D('',#247253,#19701,#19702);
#17696=AXIS2_PLACEMENT_3D('',#247255,#19703,#19704);
#17697=AXIS2_PLACEMENT_3D('',#247258,#19706,#19707);
#17698=AXIS2_PLACEMENT_3D('',#247259,#19708,#19709);
#17699=AXIS2_PLACEMENT_3D('',#247260,#19710,#19711);
#17700=AXIS2_PLACEMENT_3D('',#247261,#19712,#19713);
#17701=AXIS2_PLACEMENT_3D('',#247262,#19714,#19715);
#17702=AXIS2_PLACEMENT_3D('',#247264,#19716,#19717);
#17703=AXIS2_PLACEMENT_3D('',#247267,#19719,#19720);
#17704=AXIS2_PLACEMENT_3D('',#247268,#19721,#19722);
#17705=AXIS2_PLACEMENT_3D('',#247270,#19723,#19724);
#17706=AXIS2_PLACEMENT_3D('',#247271,#19725,#19726);
#17707=AXIS2_PLACEMENT_3D('',#247273,#19727,#19728);
#17708=AXIS2_PLACEMENT_3D('',#247274,#19729,#19730);
#17709=AXIS2_PLACEMENT_3D('',#247276,#19731,#19732);
#17710=AXIS2_PLACEMENT_3D('',#247278,#19734,#19735);
#17711=AXIS2_PLACEMENT_3D('',#247280,#19736,#19737);
#17712=AXIS2_PLACEMENT_3D('',#247282,#19738,#19739);
#17713=AXIS2_PLACEMENT_3D('',#247283,#19740,#19741);
#17714=AXIS2_PLACEMENT_3D('',#247286,#19743,#19744);
#17715=AXIS2_PLACEMENT_3D('',#247287,#19745,#19746);
#17716=AXIS2_PLACEMENT_3D('',#247288,#19747,#19748);
#17717=AXIS2_PLACEMENT_3D('',#247290,#19750,#19751);
#17718=AXIS2_PLACEMENT_3D('',#247291,#19752,#19753);
#17719=AXIS2_PLACEMENT_3D('',#247292,#19754,#19755);
#17720=AXIS2_PLACEMENT_3D('',#247294,#19756,#19757);
#17721=AXIS2_PLACEMENT_3D('',#247297,#19759,#19760);
#17722=AXIS2_PLACEMENT_3D('',#247298,#19761,#19762);
#17723=AXIS2_PLACEMENT_3D('',#247300,#19763,#19764);
#17724=AXIS2_PLACEMENT_3D('',#247303,#19766,#19767);
#17725=AXIS2_PLACEMENT_3D('',#247304,#19768,#19769);
#17726=AXIS2_PLACEMENT_3D('',#247305,#19770,#19771);
#17727=AXIS2_PLACEMENT_3D('',#247306,#19772,#19773);
#17728=AXIS2_PLACEMENT_3D('',#247307,#19774,#19775);
#17729=AXIS2_PLACEMENT_3D('',#247316,#19780,#19781);
#17730=AXIS2_PLACEMENT_3D('',#247325,#19786,#19787);
#17731=AXIS2_PLACEMENT_3D('',#247326,#19788,#19789);
#17732=AXIS2_PLACEMENT_3D('',#247327,#19790,#19791);
#17733=AXIS2_PLACEMENT_3D('',#247328,#19792,#19793);
#17734=AXIS2_PLACEMENT_3D('',#247329,#19794,#19795);
#17735=AXIS2_PLACEMENT_3D('',#247330,#19796,#19797);
#17736=AXIS2_PLACEMENT_3D('',#247331,#19798,#19799);
#17737=AXIS2_PLACEMENT_3D('',#247332,#19800,#19801);
#17738=AXIS2_PLACEMENT_3D('',#247333,#19802,#19803);
#17739=AXIS2_PLACEMENT_3D('',#247334,#19804,#19805);
#17740=AXIS2_PLACEMENT_3D('',#247336,#19806,#19807);
#17741=AXIS2_PLACEMENT_3D('',#247339,#19809,#19810);
#17742=AXIS2_PLACEMENT_3D('',#247340,#19811,#19812);
#17743=AXIS2_PLACEMENT_3D('',#247342,#19813,#19814);
#17744=AXIS2_PLACEMENT_3D('',#247345,#19816,#19817);
#17745=AXIS2_PLACEMENT_3D('',#247346,#19818,#19819);
#17746=AXIS2_PLACEMENT_3D('',#247347,#19820,#19821);
#17747=AXIS2_PLACEMENT_3D('',#247348,#19822,#19823);
#17748=AXIS2_PLACEMENT_3D('',#247349,#19824,#19825);
#17749=AXIS2_PLACEMENT_3D('',#247354,#19827,#19828);
#17750=AXIS2_PLACEMENT_3D('',#247631,#19829,#19830);
#17751=AXIS2_PLACEMENT_3D('',#247634,#19832,#19833);
#17752=AXIS2_PLACEMENT_3D('',#247636,#19834,#19835);
#17753=AXIS2_PLACEMENT_3D('',#247686,#19836,#19837);
#17754=AXIS2_PLACEMENT_3D('',#247870,#19839,#19840);
#17755=AXIS2_PLACEMENT_3D('',#248007,#19841,#19842);
#17756=AXIS2_PLACEMENT_3D('',#248427,#19844,#19845);
#17757=AXIS2_PLACEMENT_3D('',#248860,#19847,#19848);
#17758=AXIS2_PLACEMENT_3D('',#249357,#19850,#19851);
#17759=AXIS2_PLACEMENT_3D('',#249792,#19853,#19854);
#17760=AXIS2_PLACEMENT_3D('',#250221,#19856,#19857);
#17761=AXIS2_PLACEMENT_3D('',#250651,#19859,#19860);
#17762=AXIS2_PLACEMENT_3D('',#251091,#19862,#19863);
#17763=AXIS2_PLACEMENT_3D('',#251555,#19865,#19866);
#17764=AXIS2_PLACEMENT_3D('',#251995,#19868,#19869);
#17765=AXIS2_PLACEMENT_3D('',#252422,#19871,#19872);
#17766=AXIS2_PLACEMENT_3D('',#252855,#19874,#19875);
#17767=AXIS2_PLACEMENT_3D('',#253362,#19877,#19878);
#17768=AXIS2_PLACEMENT_3D('',#253785,#19880,#19881);
#17769=AXIS2_PLACEMENT_3D('',#254215,#19883,#19884);
#17770=AXIS2_PLACEMENT_3D('',#254628,#19886,#19887);
#17771=AXIS2_PLACEMENT_3D('',#254638,#19888,#19889);
#17772=AXIS2_PLACEMENT_3D('',#258091,#19890,#19891);
#17773=AXIS2_PLACEMENT_3D('',#259546,#19892,#19893);
#17774=AXIS2_PLACEMENT_3D('',#259584,#19894,#19895);
#17775=AXIS2_PLACEMENT_3D('',#260627,#19896,#19897);
#17776=AXIS2_PLACEMENT_3D('',#260636,#19902,#19903);
#17777=AXIS2_PLACEMENT_3D('',#260642,#19907,#19908);
#17778=AXIS2_PLACEMENT_3D('',#260648,#19912,#19913);
#17779=AXIS2_PLACEMENT_3D('',#260654,#19917,#19918);
#17780=AXIS2_PLACEMENT_3D('',#260660,#19922,#19923);
#17781=AXIS2_PLACEMENT_3D('',#260663,#19926,#19927);
#17782=AXIS2_PLACEMENT_3D('',#260664,#19928,#19929);
#17783=AXIS2_PLACEMENT_3D('',#260666,#19930,#19931);
#17784=AXIS2_PLACEMENT_3D('',#260667,#19932,#19933);
#17785=AXIS2_PLACEMENT_3D('',#260670,#19935,#19936);
#17786=AXIS2_PLACEMENT_3D('',#260671,#19937,#19938);
#17787=AXIS2_PLACEMENT_3D('',#260672,#19939,#19940);
#17788=AXIS2_PLACEMENT_3D('',#260673,#19941,#19942);
#17789=AXIS2_PLACEMENT_3D('',#260674,#19943,#19944);
#17790=AXIS2_PLACEMENT_3D('',#260679,#19946,#19947);
#17791=AXIS2_PLACEMENT_3D('',#260920,#19948,#19949);
#17792=AXIS2_PLACEMENT_3D('',#260923,#19951,#19952);
#17793=AXIS2_PLACEMENT_3D('',#260925,#19953,#19954);
#17794=AXIS2_PLACEMENT_3D('',#260960,#19955,#19956);
#17795=AXIS2_PLACEMENT_3D('',#261039,#19958,#19959);
#17796=AXIS2_PLACEMENT_3D('',#261080,#19960,#19961);
#17797=AXIS2_PLACEMENT_3D('',#261482,#19963,#19964);
#17798=AXIS2_PLACEMENT_3D('',#261916,#19966,#19967);
#17799=AXIS2_PLACEMENT_3D('',#262374,#19969,#19970);
#17800=AXIS2_PLACEMENT_3D('',#262800,#19972,#19973);
#17801=AXIS2_PLACEMENT_3D('',#263312,#19975,#19976);
#17802=AXIS2_PLACEMENT_3D('',#263734,#19978,#19979);
#17803=AXIS2_PLACEMENT_3D('',#264070,#19981,#19982);
#17804=AXIS2_PLACEMENT_3D('',#264422,#19984,#19985);
#17805=AXIS2_PLACEMENT_3D('',#264741,#19987,#19988);
#17806=AXIS2_PLACEMENT_3D('',#265104,#19990,#19991);
#17807=AXIS2_PLACEMENT_3D('',#265532,#19993,#19994);
#17808=AXIS2_PLACEMENT_3D('',#265874,#19996,#19997);
#17809=AXIS2_PLACEMENT_3D('',#266237,#19999,#20000);
#17810=AXIS2_PLACEMENT_3D('',#266672,#20002,#20003);
#17811=AXIS2_PLACEMENT_3D('',#267129,#20005,#20006);
#17812=AXIS2_PLACEMENT_3D('',#267558,#20008,#20009);
#17813=AXIS2_PLACEMENT_3D('',#267885,#20011,#20012);
#17814=AXIS2_PLACEMENT_3D('',#268249,#20014,#20015);
#17815=AXIS2_PLACEMENT_3D('',#268692,#20017,#20018);
#17816=AXIS2_PLACEMENT_3D('',#269143,#20020,#20021);
#17817=AXIS2_PLACEMENT_3D('',#269592,#20023,#20024);
#17818=AXIS2_PLACEMENT_3D('',#270055,#20026,#20027);
#17819=AXIS2_PLACEMENT_3D('',#270492,#20029,#20030);
#17820=AXIS2_PLACEMENT_3D('',#270941,#20032,#20033);
#17821=AXIS2_PLACEMENT_3D('',#271392,#20035,#20036);
#17822=AXIS2_PLACEMENT_3D('',#271811,#20038,#20039);
#17823=AXIS2_PLACEMENT_3D('',#272283,#20041,#20042);
#17824=AXIS2_PLACEMENT_3D('',#272348,#20043,#20044);
#17825=AXIS2_PLACEMENT_3D('',#274664,#20045,#20046);
#17826=AXIS2_PLACEMENT_3D('',#274666,#20047,#20048);
#17827=AXIS2_PLACEMENT_3D('',#277291,#20049,#20050);
#17828=AXIS2_PLACEMENT_3D('',#277455,#20051,#20052);
#17829=AXIS2_PLACEMENT_3D('',#279083,#20053,#20054);
#17830=AXIS2_PLACEMENT_3D('',#279092,#20059,#20060);
#17831=AXIS2_PLACEMENT_3D('',#279098,#20064,#20065);
#17832=AXIS2_PLACEMENT_3D('',#279104,#20069,#20070);
#17833=AXIS2_PLACEMENT_3D('',#279110,#20074,#20075);
#17834=AXIS2_PLACEMENT_3D('',#279116,#20079,#20080);
#17835=AXIS2_PLACEMENT_3D('',#279119,#20083,#20084);
#17836=AXIS2_PLACEMENT_3D('',#279120,#20085,#20086);
#17837=AXIS2_PLACEMENT_3D('',#279122,#20087,#20088);
#17838=AXIS2_PLACEMENT_3D('',#279123,#20089,#20090);
#17839=AXIS2_PLACEMENT_3D('',#279126,#20092,#20093);
#17840=AXIS2_PLACEMENT_3D('',#279127,#20094,#20095);
#17841=AXIS2_PLACEMENT_3D('',#279128,#20096,#20097);
#17842=AXIS2_PLACEMENT_3D('',#279129,#20098,#20099);
#17843=AXIS2_PLACEMENT_3D('',#279130,#20100,#20101);
#17844=AXIS2_PLACEMENT_3D('',#279195,#20102,#20103);
#17845=AXIS2_PLACEMENT_3D('',#280671,#20104,#20105);
#17846=AXIS2_PLACEMENT_3D('',#282191,#20106,#20107);
#17847=AXIS2_PLACEMENT_3D('',#282316,#20108,#20109);
#17848=AXIS2_PLACEMENT_3D('',#285072,#20110,#20111);
#17849=AXIS2_PLACEMENT_3D('',#288060,#20112,#20113);
#17850=AXIS2_PLACEMENT_3D('',#288254,#20115,#20116);
#17851=AXIS2_PLACEMENT_3D('',#289279,#20117,#20118);
#17852=AXIS2_PLACEMENT_3D('',#289288,#20123,#20124);
#17853=AXIS2_PLACEMENT_3D('',#289294,#20128,#20129);
#17854=AXIS2_PLACEMENT_3D('',#289300,#20133,#20134);
#17855=AXIS2_PLACEMENT_3D('',#289306,#20138,#20139);
#17856=AXIS2_PLACEMENT_3D('',#289312,#20143,#20144);
#17857=AXIS2_PLACEMENT_3D('',#289315,#20147,#20148);
#17858=AXIS2_PLACEMENT_3D('',#289316,#20149,#20150);
#17859=AXIS2_PLACEMENT_3D('',#289318,#20151,#20152);
#17860=AXIS2_PLACEMENT_3D('',#289319,#20153,#20154);
#17861=AXIS2_PLACEMENT_3D('',#289322,#20156,#20157);
#17862=AXIS2_PLACEMENT_3D('',#289323,#20158,#20159);
#17863=AXIS2_PLACEMENT_3D('',#289324,#20160,#20161);
#17864=AXIS2_PLACEMENT_3D('',#289325,#20162,#20163);
#17865=AXIS2_PLACEMENT_3D('',#289326,#20164,#20165);
#17866=AXIS2_PLACEMENT_3D('',#289327,#20166,#20167);
#17867=AXIS2_PLACEMENT_3D('',#289328,#20168,#20169);
#17868=AXIS2_PLACEMENT_3D('',#289329,#20170,#20171);
#17869=AXIS2_PLACEMENT_3D('',#289330,#20172,#20173);
#17870=AXIS2_PLACEMENT_3D('',#289331,#20174,#20175);
#17871=AXIS2_PLACEMENT_3D('',#289332,#20176,#20177);
#17872=AXIS2_PLACEMENT_3D('',#289333,#20178,#20179);
#17873=AXIS2_PLACEMENT_3D('',#289334,#20180,#20181);
#17874=AXIS2_PLACEMENT_3D('',#289335,#20182,#20183);
#17875=AXIS2_PLACEMENT_3D('',#289336,#20184,#20185);
#17876=AXIS2_PLACEMENT_3D('',#289337,#20186,#20187);
#17877=AXIS2_PLACEMENT_3D('',#289338,#20188,#20189);
#17878=AXIS2_PLACEMENT_3D('',#289339,#20190,#20191);
#17879=AXIS2_PLACEMENT_3D('',#289340,#20192,#20193);
#17880=AXIS2_PLACEMENT_3D('',#289341,#20194,#20195);
#17881=AXIS2_PLACEMENT_3D('',#289342,#20196,#20197);
#17882=AXIS2_PLACEMENT_3D('',#289343,#20198,#20199);
#17883=AXIS2_PLACEMENT_3D('',#289344,#20200,#20201);
#17884=AXIS2_PLACEMENT_3D('',#289345,#20202,#20203);
#17885=AXIS2_PLACEMENT_3D('',#289346,#20204,#20205);
#17886=AXIS2_PLACEMENT_3D('',#289347,#20206,#20207);
#17887=AXIS2_PLACEMENT_3D('',#289348,#20208,#20209);
#17888=AXIS2_PLACEMENT_3D('',#289349,#20210,#20211);
#17889=DIRECTION('axis',(0.,0.,1.));
#17890=DIRECTION('refdir',(1.,0.,0.));
#17891=DIRECTION('axis',(0.,0.,1.));
#17892=DIRECTION('refdir',(1.,0.,0.));
#17893=DIRECTION('center_axis',(0.,0.,-1.));
#17894=DIRECTION('ref_axis',(-0.608852061413682,-0.79328378737518,0.));
#17895=DIRECTION('',(0.,0.,-1.));
#17896=DIRECTION('center_axis',(0.,0.,1.));
#17897=DIRECTION('ref_axis',(1.,-4.78333543045355E-14,0.));
#17898=DIRECTION('center_axis',(0.,0.,-1.));
#17899=DIRECTION('ref_axis',(-0.608852061413682,-0.79328378737518,0.));
#17900=DIRECTION('',(0.,0.,-1.));
#17901=DIRECTION('center_axis',(0.,0.,-1.));
#17902=DIRECTION('ref_axis',(-0.608852061413682,-0.79328378737518,0.));
#17903=DIRECTION('',(0.,0.,-1.));
#17904=DIRECTION('center_axis',(0.,0.,-1.));
#17905=DIRECTION('ref_axis',(-0.608852061413682,-0.79328378737518,0.));
#17906=DIRECTION('',(0.,0.,-1.));
#17907=DIRECTION('center_axis',(0.,0.,-1.));
#17908=DIRECTION('ref_axis',(-0.608852061413682,-0.79328378737518,0.));
#17909=DIRECTION('',(0.,0.,-1.));
#17910=DIRECTION('center_axis',(0.,0.,-1.));
#17911=DIRECTION('ref_axis',(-0.608852061413682,-0.79328378737518,0.));
#17912=DIRECTION('',(0.,0.,-1.));
#17913=DIRECTION('center_axis',(0.,0.,-1.));
#17914=DIRECTION('ref_axis',(-0.608852061413682,-0.79328378737518,0.));
#17915=DIRECTION('',(0.,0.,-1.));
#17916=DIRECTION('center_axis',(0.,0.,-1.));
#17917=DIRECTION('ref_axis',(-0.608852061413682,-0.79328378737518,0.));
#17918=DIRECTION('',(0.,0.,-1.));
#17919=DIRECTION('center_axis',(0.,0.,-1.));
#17920=DIRECTION('ref_axis',(-0.608852061413682,-0.79328378737518,0.));
#17921=DIRECTION('',(0.,0.,-1.));
#17922=DIRECTION('center_axis',(0.,0.,-1.));
#17923=DIRECTION('ref_axis',(-0.608852061413682,-0.79328378737518,0.));
#17924=DIRECTION('',(0.,0.,-1.));
#17925=DIRECTION('center_axis',(0.,0.,-1.));
#17926=DIRECTION('ref_axis',(1.,-4.78333543045355E-14,0.));
#17927=DIRECTION('center_axis',(0.,0.,-1.));
#17928=DIRECTION('ref_axis',(0.937755906520935,-0.347295061561634,0.));
#17929=DIRECTION('',(0.,0.,-1.));
#17930=DIRECTION('center_axis',(0.,0.,1.));
#17931=DIRECTION('ref_axis',(1.,0.,0.));
#17932=DIRECTION('',(0.,0.,-1.));
#17933=DIRECTION('center_axis',(0.,0.,1.));
#17934=DIRECTION('ref_axis',(1.,0.,0.));
#17935=DIRECTION('center_axis',(0.,0.,1.));
#17936=DIRECTION('ref_axis',(1.,0.,0.));
#17937=DIRECTION('center_axis',(0.,0.,-1.));
#17938=DIRECTION('ref_axis',(0.937755906520935,-0.347295061561634,0.));
#17939=DIRECTION('',(0.,0.,-1.));
#17940=DIRECTION('center_axis',(0.,0.,-1.));
#17941=DIRECTION('ref_axis',(0.937755906520935,-0.347295061561634,0.));
#17942=DIRECTION('',(0.,0.,-1.));
#17943=DIRECTION('center_axis',(0.,0.,-1.));
#17944=DIRECTION('ref_axis',(0.937755906520935,-0.347295061561634,0.));
#17945=DIRECTION('',(0.,0.,-1.));
#17946=DIRECTION('center_axis',(0.,0.,-1.));
#17947=DIRECTION('ref_axis',(0.937755906520935,-0.347295061561634,0.));
#17948=DIRECTION('',(0.,0.,-1.));
#17949=DIRECTION('center_axis',(0.,0.,-1.));
#17950=DIRECTION('ref_axis',(0.937755906520935,-0.347295061561634,0.));
#17951=DIRECTION('',(0.,0.,-1.));
#17952=DIRECTION('center_axis',(0.,0.,-1.));
#17953=DIRECTION('ref_axis',(0.937755906520935,-0.347295061561634,0.));
#17954=DIRECTION('',(0.,0.,-1.));
#17955=DIRECTION('center_axis',(0.,0.,-1.));
#17956=DIRECTION('ref_axis',(0.937755906520935,-0.347295061561634,0.));
#17957=DIRECTION('',(0.,0.,-1.));
#17958=DIRECTION('center_axis',(0.,0.,-1.));
#17959=DIRECTION('ref_axis',(0.937755906520935,-0.347295061561634,0.));
#17960=DIRECTION('',(0.,0.,-1.));
#17961=DIRECTION('center_axis',(0.,0.,-1.));
#17962=DIRECTION('ref_axis',(0.857775286865319,-0.514024860530227,0.));
#17963=DIRECTION('',(0.,0.,-1.));
#17964=DIRECTION('center_axis',(0.,0.,-1.));
#17965=DIRECTION('ref_axis',(1.,0.,0.));
#17966=DIRECTION('center_axis',(0.,0.,-1.));
#17967=DIRECTION('ref_axis',(-0.608854967610821,-0.793281556835671,0.));
#17968=DIRECTION('',(0.,0.,-1.));
#17969=DIRECTION('center_axis',(0.,0.,1.));
#17970=DIRECTION('ref_axis',(1.,-4.56591109270566E-14,0.));
#17971=DIRECTION('center_axis',(0.,0.,-1.));
#17972=DIRECTION('ref_axis',(-0.608854967610821,-0.793281556835671,0.));
#17973=DIRECTION('',(0.,0.,-1.));
#17974=DIRECTION('center_axis',(0.,0.,-1.));
#17975=DIRECTION('ref_axis',(-0.608854967610821,-0.793281556835671,0.));
#17976=DIRECTION('',(0.,0.,-1.));
#17977=DIRECTION('center_axis',(0.,0.,-1.));
#17978=DIRECTION('ref_axis',(-0.608854967610821,-0.793281556835671,0.));
#17979=DIRECTION('',(0.,0.,-1.));
#17980=DIRECTION('center_axis',(0.,0.,-1.));
#17981=DIRECTION('ref_axis',(-0.608854967610821,-0.793281556835671,0.));
#17982=DIRECTION('',(0.,0.,-1.));
#17983=DIRECTION('center_axis',(0.,0.,-1.));
#17984=DIRECTION('ref_axis',(-0.608854967610821,-0.793281556835671,0.));
#17985=DIRECTION('',(0.,0.,-1.));
#17986=DIRECTION('center_axis',(0.,0.,-1.));
#17987=DIRECTION('ref_axis',(-0.608854967610821,-0.793281556835671,0.));
#17988=DIRECTION('',(0.,0.,-1.));
#17989=DIRECTION('center_axis',(0.,0.,-1.));
#17990=DIRECTION('ref_axis',(-0.608854967610821,-0.793281556835671,0.));
#17991=DIRECTION('',(0.,0.,-1.));
#17992=DIRECTION('center_axis',(0.,0.,-1.));
#17993=DIRECTION('ref_axis',(-0.608854967610821,-0.793281556835671,0.));
#17994=DIRECTION('',(0.,0.,-1.));
#17995=DIRECTION('center_axis',(0.,0.,-1.));
#17996=DIRECTION('ref_axis',(-0.608854967610821,-0.793281556835671,0.));
#17997=DIRECTION('',(0.,0.,-1.));
#17998=DIRECTION('center_axis',(0.,0.,-1.));
#17999=DIRECTION('ref_axis',(1.,-4.56591109270566E-14,0.));
#18000=DIRECTION('center_axis',(0.,0.,-1.));
#18001=DIRECTION('ref_axis',(0.937753558233112,-0.347301402273498,0.));
#18002=DIRECTION('',(0.,0.,-1.));
#18003=DIRECTION('center_axis',(0.,0.,1.));
#18004=DIRECTION('ref_axis',(1.,0.,0.));
#18005=DIRECTION('',(0.,0.,-1.));
#18006=DIRECTION('center_axis',(0.,0.,1.));
#18007=DIRECTION('ref_axis',(1.,0.,0.));
#18008=DIRECTION('center_axis',(0.,0.,1.));
#18009=DIRECTION('ref_axis',(1.,0.,0.));
#18010=DIRECTION('center_axis',(0.,0.,-1.));
#18011=DIRECTION('ref_axis',(0.937753558233112,-0.347301402273498,0.));
#18012=DIRECTION('',(0.,0.,-1.));
#18013=DIRECTION('center_axis',(0.,0.,-1.));
#18014=DIRECTION('ref_axis',(0.937753558233112,-0.347301402273498,0.));
#18015=DIRECTION('',(0.,0.,-1.));
#18016=DIRECTION('center_axis',(0.,0.,-1.));
#18017=DIRECTION('ref_axis',(0.937753558233112,-0.347301402273498,0.));
#18018=DIRECTION('',(0.,0.,-1.));
#18019=DIRECTION('center_axis',(0.,0.,-1.));
#18020=DIRECTION('ref_axis',(0.937753558233112,-0.347301402273498,0.));
#18021=DIRECTION('',(0.,0.,-1.));
#18022=DIRECTION('center_axis',(0.,0.,-1.));
#18023=DIRECTION('ref_axis',(0.937753558233112,-0.347301402273498,0.));
#18024=DIRECTION('',(0.,0.,-1.));
#18025=DIRECTION('center_axis',(0.,0.,-1.));
#18026=DIRECTION('ref_axis',(0.937753558233112,-0.347301402273498,0.));
#18027=DIRECTION('',(0.,0.,-1.));
#18028=DIRECTION('center_axis',(0.,0.,-1.));
#18029=DIRECTION('ref_axis',(0.937753558233112,-0.347301402273498,0.));
#18030=DIRECTION('',(0.,0.,-1.));
#18031=DIRECTION('center_axis',(0.,0.,-1.));
#18032=DIRECTION('ref_axis',(0.937753558233112,-0.347301402273498,0.));
#18033=DIRECTION('',(0.,0.,-1.));
#18034=DIRECTION('center_axis',(0.,0.,-1.));
#18035=DIRECTION('ref_axis',(0.85779647863907,-0.51398949525687,0.));
#18036=DIRECTION('',(0.,0.,-1.));
#18037=DIRECTION('center_axis',(0.,0.,-1.));
#18038=DIRECTION('ref_axis',(1.,0.,0.));
#18039=DIRECTION('center_axis',(0.,0.,-1.));
#18040=DIRECTION('ref_axis',(-0.608852066092606,-0.793283783784066,0.));
#18041=DIRECTION('',(0.,0.,-1.));
#18042=DIRECTION('center_axis',(0.,0.,1.));
#18043=DIRECTION('ref_axis',(1.,-4.78333543045355E-14,0.));
#18044=DIRECTION('center_axis',(0.,0.,-1.));
#18045=DIRECTION('ref_axis',(-0.608852066092606,-0.793283783784066,0.));
#18046=DIRECTION('',(0.,0.,-1.));
#18047=DIRECTION('center_axis',(0.,0.,-1.));
#18048=DIRECTION('ref_axis',(-0.608852066092606,-0.793283783784066,0.));
#18049=DIRECTION('',(0.,0.,-1.));
#18050=DIRECTION('center_axis',(0.,0.,-1.));
#18051=DIRECTION('ref_axis',(-0.608852066092606,-0.793283783784066,0.));
#18052=DIRECTION('',(0.,0.,-1.));
#18053=DIRECTION('center_axis',(0.,0.,-1.));
#18054=DIRECTION('ref_axis',(-0.608852066092606,-0.793283783784066,0.));
#18055=DIRECTION('',(0.,0.,-1.));
#18056=DIRECTION('center_axis',(0.,0.,-1.));
#18057=DIRECTION('ref_axis',(-0.608852066092606,-0.793283783784066,0.));
#18058=DIRECTION('',(0.,0.,-1.));
#18059=DIRECTION('center_axis',(0.,0.,-1.));
#18060=DIRECTION('ref_axis',(-0.608852066092606,-0.793283783784066,0.));
#18061=DIRECTION('',(0.,0.,-1.));
#18062=DIRECTION('center_axis',(0.,0.,-1.));
#18063=DIRECTION('ref_axis',(-0.608852066092606,-0.793283783784066,0.));
#18064=DIRECTION('',(0.,0.,-1.));
#18065=DIRECTION('center_axis',(0.,0.,-1.));
#18066=DIRECTION('ref_axis',(-0.608852066092606,-0.793283783784066,0.));
#18067=DIRECTION('',(0.,0.,-1.));
#18068=DIRECTION('center_axis',(0.,0.,-1.));
#18069=DIRECTION('ref_axis',(-0.608852066092606,-0.793283783784066,0.));
#18070=DIRECTION('',(0.,0.,-1.));
#18071=DIRECTION('center_axis',(0.,0.,-1.));
#18072=DIRECTION('ref_axis',(1.,-4.78333543045355E-14,0.));
#18073=DIRECTION('center_axis',(0.,0.,-1.));
#18074=DIRECTION('ref_axis',(0.937755905787258,-0.347295063542687,0.));
#18075=DIRECTION('',(0.,0.,-1.));
#18076=DIRECTION('center_axis',(0.,0.,1.));
#18077=DIRECTION('ref_axis',(1.,0.,0.));
#18078=DIRECTION('',(0.,0.,-1.));
#18079=DIRECTION('center_axis',(0.,0.,1.));
#18080=DIRECTION('ref_axis',(1.,0.,0.));
#18081=DIRECTION('center_axis',(0.,0.,1.));
#18082=DIRECTION('ref_axis',(1.,0.,0.));
#18083=DIRECTION('center_axis',(0.,0.,-1.));
#18084=DIRECTION('ref_axis',(0.937755905787258,-0.347295063542687,0.));
#18085=DIRECTION('',(0.,0.,-1.));
#18086=DIRECTION('center_axis',(0.,0.,-1.));
#18087=DIRECTION('ref_axis',(0.937755905787258,-0.347295063542687,0.));
#18088=DIRECTION('',(0.,0.,-1.));
#18089=DIRECTION('center_axis',(0.,0.,-1.));
#18090=DIRECTION('ref_axis',(0.937755905787258,-0.347295063542687,0.));
#18091=DIRECTION('',(0.,0.,-1.));
#18092=DIRECTION('center_axis',(0.,0.,-1.));
#18093=DIRECTION('ref_axis',(0.937755905787258,-0.347295063542687,0.));
#18094=DIRECTION('',(0.,0.,-1.));
#18095=DIRECTION('center_axis',(0.,0.,-1.));
#18096=DIRECTION('ref_axis',(0.937755905787258,-0.347295063542687,0.));
#18097=DIRECTION('',(0.,0.,-1.));
#18098=DIRECTION('center_axis',(0.,0.,-1.));
#18099=DIRECTION('ref_axis',(0.937755905787258,-0.347295063542687,0.));
#18100=DIRECTION('',(0.,0.,-1.));
#18101=DIRECTION('center_axis',(0.,0.,-1.));
#18102=DIRECTION('ref_axis',(0.937755905787258,-0.347295063542687,0.));
#18103=DIRECTION('',(0.,0.,-1.));
#18104=DIRECTION('center_axis',(0.,0.,-1.));
#18105=DIRECTION('ref_axis',(0.937755905787258,-0.347295063542687,0.));
#18106=DIRECTION('',(0.,0.,-1.));
#18107=DIRECTION('center_axis',(0.,0.,-1.));
#18108=DIRECTION('ref_axis',(0.857775134428094,-0.514025114908664,0.));
#18109=DIRECTION('',(0.,0.,-1.));
#18110=DIRECTION('center_axis',(0.,0.,-1.));
#18111=DIRECTION('ref_axis',(1.,0.,0.));
#18112=DIRECTION('center_axis',(0.,0.,-1.));
#18113=DIRECTION('ref_axis',(-0.60885499756405,-0.793281533846138,0.));
#18114=DIRECTION('',(0.,0.,-1.));
#18115=DIRECTION('center_axis',(0.,0.,1.));
#18116=DIRECTION('ref_axis',(1.,-4.78333543045355E-14,0.));
#18117=DIRECTION('center_axis',(0.,0.,-1.));
#18118=DIRECTION('ref_axis',(-0.60885499756405,-0.793281533846138,0.));
#18119=DIRECTION('',(0.,0.,-1.));
#18120=DIRECTION('center_axis',(0.,0.,-1.));
#18121=DIRECTION('ref_axis',(-0.60885499756405,-0.793281533846138,0.));
#18122=DIRECTION('',(0.,0.,-1.));
#18123=DIRECTION('center_axis',(0.,0.,-1.));
#18124=DIRECTION('ref_axis',(-0.60885499756405,-0.793281533846138,0.));
#18125=DIRECTION('',(0.,0.,-1.));
#18126=DIRECTION('center_axis',(0.,0.,-1.));
#18127=DIRECTION('ref_axis',(-0.60885499756405,-0.793281533846138,0.));
#18128=DIRECTION('',(0.,0.,-1.));
#18129=DIRECTION('center_axis',(0.,0.,-1.));
#18130=DIRECTION('ref_axis',(-0.60885499756405,-0.793281533846138,0.));
#18131=DIRECTION('',(0.,0.,-1.));
#18132=DIRECTION('center_axis',(0.,0.,-1.));
#18133=DIRECTION('ref_axis',(-0.60885499756405,-0.793281533846138,0.));
#18134=DIRECTION('',(0.,0.,-1.));
#18135=DIRECTION('center_axis',(0.,0.,-1.));
#18136=DIRECTION('ref_axis',(-0.60885499756405,-0.793281533846138,0.));
#18137=DIRECTION('',(0.,0.,-1.));
#18138=DIRECTION('center_axis',(0.,0.,-1.));
#18139=DIRECTION('ref_axis',(-0.60885499756405,-0.793281533846138,0.));
#18140=DIRECTION('',(0.,0.,-1.));
#18141=DIRECTION('center_axis',(0.,0.,-1.));
#18142=DIRECTION('ref_axis',(-0.60885499756405,-0.793281533846138,0.));
#18143=DIRECTION('',(0.,0.,-1.));
#18144=DIRECTION('center_axis',(0.,0.,-1.));
#18145=DIRECTION('ref_axis',(1.,-4.78333543045355E-14,0.));
#18146=DIRECTION('center_axis',(0.,0.,-1.));
#18147=DIRECTION('ref_axis',(0.93775354145692,-0.347301447571133,0.));
#18148=DIRECTION('',(0.,0.,-1.));
#18149=DIRECTION('center_axis',(0.,0.,1.));
#18150=DIRECTION('ref_axis',(1.,0.,0.));
#18151=DIRECTION('',(0.,0.,-1.));
#18152=DIRECTION('center_axis',(0.,0.,1.));
#18153=DIRECTION('ref_axis',(1.,0.,0.));
#18154=DIRECTION('center_axis',(0.,0.,1.));
#18155=DIRECTION('ref_axis',(1.,0.,0.));
#18156=DIRECTION('center_axis',(0.,0.,-1.));
#18157=DIRECTION('ref_axis',(0.93775354145692,-0.347301447571133,0.));
#18158=DIRECTION('',(0.,0.,-1.));
#18159=DIRECTION('center_axis',(0.,0.,-1.));
#18160=DIRECTION('ref_axis',(0.93775354145692,-0.347301447571133,0.));
#18161=DIRECTION('',(0.,0.,-1.));
#18162=DIRECTION('center_axis',(0.,0.,-1.));
#18163=DIRECTION('ref_axis',(0.93775354145692,-0.347301447571133,0.));
#18164=DIRECTION('',(0.,0.,-1.));
#18165=DIRECTION('center_axis',(0.,0.,-1.));
#18166=DIRECTION('ref_axis',(0.93775354145692,-0.347301447571133,0.));
#18167=DIRECTION('',(0.,0.,-1.));
#18168=DIRECTION('center_axis',(0.,0.,-1.));
#18169=DIRECTION('ref_axis',(0.93775354145692,-0.347301447571133,0.));
#18170=DIRECTION('',(0.,0.,-1.));
#18171=DIRECTION('center_axis',(0.,0.,-1.));
#18172=DIRECTION('ref_axis',(0.93775354145692,-0.347301447571133,0.));
#18173=DIRECTION('',(0.,0.,-1.));
#18174=DIRECTION('center_axis',(0.,0.,-1.));
#18175=DIRECTION('ref_axis',(0.93775354145692,-0.347301447571133,0.));
#18176=DIRECTION('',(0.,0.,-1.));
#18177=DIRECTION('center_axis',(0.,0.,-1.));
#18178=DIRECTION('ref_axis',(0.93775354145692,-0.347301447571133,0.));
#18179=DIRECTION('',(0.,0.,-1.));
#18180=DIRECTION('center_axis',(0.,0.,-1.));
#18181=DIRECTION('ref_axis',(0.857796441547725,-0.513989557158567,0.));
#18182=DIRECTION('',(0.,0.,-1.));
#18183=DIRECTION('center_axis',(0.,0.,-1.));
#18184=DIRECTION('ref_axis',(1.,0.,0.));
#18185=DIRECTION('center_axis',(0.,0.,-1.));
#18186=DIRECTION('ref_axis',(0.93775354145692,-0.347301447571133,0.));
#18187=DIRECTION('center_axis',(0.,0.,-1.));
#18188=DIRECTION('ref_axis',(-0.60885499756405,-0.793281533846138,0.));
#18189=DIRECTION('center_axis',(0.,0.,-1.));
#18190=DIRECTION('ref_axis',(0.937755905787258,-0.347295063542687,0.));
#18191=DIRECTION('center_axis',(0.,0.,-1.));
#18192=DIRECTION('ref_axis',(-0.608852066092606,-0.793283783784066,0.));
#18193=DIRECTION('center_axis',(0.,0.,-1.));
#18194=DIRECTION('ref_axis',(0.937753558233112,-0.347301402273498,0.));
#18195=DIRECTION('center_axis',(0.,0.,-1.));
#18196=DIRECTION('ref_axis',(-0.608854967610821,-0.793281556835671,0.));
#18197=DIRECTION('center_axis',(0.,0.,-1.));
#18198=DIRECTION('ref_axis',(0.937755906520935,-0.347295061561634,0.));
#18199=DIRECTION('center_axis',(0.,0.,-1.));
#18200=DIRECTION('ref_axis',(-0.608852061413682,-0.79328378737518,0.));
#18201=DIRECTION('center_axis',(0.,0.,1.));
#18202=DIRECTION('ref_axis',(1.,0.,0.));
#18203=DIRECTION('center_axis',(0.,0.,1.));
#18204=DIRECTION('ref_axis',(1.,0.,0.));
#18205=DIRECTION('center_axis',(0.,0.,1.));
#18206=DIRECTION('ref_axis',(1.,0.,0.));
#18207=DIRECTION('center_axis',(0.,0.,1.));
#18208=DIRECTION('ref_axis',(1.,0.,0.));
#18209=DIRECTION('center_axis',(0.,0.,-1.));
#18210=DIRECTION('ref_axis',(1.,0.,0.));
#18211=DIRECTION('center_axis',(0.,0.,-1.));
#18212=DIRECTION('ref_axis',(1.,0.,0.));
#18213=DIRECTION('center_axis',(0.,0.,-1.));
#18214=DIRECTION('ref_axis',(1.,0.,0.));
#18215=DIRECTION('center_axis',(0.,0.,-1.));
#18216=DIRECTION('ref_axis',(1.,0.,0.));
#18217=DIRECTION('center_axis',(0.,0.,-1.));
#18218=DIRECTION('ref_axis',(1.,0.,0.));
#18219=DIRECTION('center_axis',(0.,0.,-1.));
#18220=DIRECTION('ref_axis',(1.,0.,0.));
#18221=DIRECTION('',(0.,0.,-1.));
#18222=DIRECTION('center_axis',(0.,0.,1.));
#18223=DIRECTION('ref_axis',(1.,0.,0.));
#18224=DIRECTION('center_axis',(0.,0.,-1.));
#18225=DIRECTION('ref_axis',(1.,0.,0.));
#18226=DIRECTION('center_axis',(0.,0.,-1.));
#18227=DIRECTION('ref_axis',(1.,0.,0.));
#18228=DIRECTION('',(0.,0.,-1.));
#18229=DIRECTION('center_axis',(0.,0.,1.));
#18230=DIRECTION('ref_axis',(1.,0.,0.));
#18231=DIRECTION('center_axis',(0.,0.,-1.));
#18232=DIRECTION('ref_axis',(1.,0.,0.));
#18233=DIRECTION('center_axis',(0.,0.,-1.));
#18234=DIRECTION('ref_axis',(1.,0.,0.));
#18235=DIRECTION('',(0.,0.,-1.));
#18236=DIRECTION('center_axis',(0.,0.,1.));
#18237=DIRECTION('ref_axis',(1.,0.,0.));
#18238=DIRECTION('center_axis',(0.,0.,-1.));
#18239=DIRECTION('ref_axis',(1.,0.,0.));
#18240=DIRECTION('center_axis',(0.,0.,-1.));
#18241=DIRECTION('ref_axis',(1.,0.,0.));
#18242=DIRECTION('',(0.,0.,-1.));
#18243=DIRECTION('center_axis',(0.,0.,1.));
#18244=DIRECTION('ref_axis',(1.,0.,0.));
#18245=DIRECTION('center_axis',(0.,1.,0.));
#18246=DIRECTION('ref_axis',(-1.,0.,0.));
#18247=DIRECTION('',(1.,0.,0.));
#18248=DIRECTION('',(0.,0.,1.));
#18249=DIRECTION('',(1.,0.,0.));
#18250=DIRECTION('',(0.,0.,1.));
#18251=DIRECTION('center_axis',(1.,0.,0.));
#18252=DIRECTION('ref_axis',(0.,1.,0.));
#18253=DIRECTION('',(0.,-1.,0.));
#18254=DIRECTION('',(0.,-1.,0.));
#18255=DIRECTION('',(0.,0.,-1.));
#18256=DIRECTION('center_axis',(0.,-1.,0.));
#18257=DIRECTION('ref_axis',(1.,0.,0.));
#18258=DIRECTION('',(-1.,0.,0.));
#18259=DIRECTION('',(-1.,0.,0.));
#18260=DIRECTION('',(0.,0.,-1.));
#18261=DIRECTION('center_axis',(-1.,0.,0.));
#18262=DIRECTION('ref_axis',(0.,-1.,0.));
#18263=DIRECTION('',(0.,1.,0.));
#18264=DIRECTION('',(0.,1.,0.));
#18265=DIRECTION('center_axis',(0.,0.,1.));
#18266=DIRECTION('ref_axis',(1.,0.,0.));
#18267=DIRECTION('center_axis',(0.,0.,1.));
#18268=DIRECTION('ref_axis',(1.,0.,0.));
#18269=DIRECTION('axis',(0.,0.,1.));
#18270=DIRECTION('refdir',(1.,0.,0.));
#18271=DIRECTION('center_axis',(0.,0.,-1.));
#18272=DIRECTION('ref_axis',(-0.609338902105852,-0.792909895499126,0.));
#18273=DIRECTION('',(0.,0.,-1.));
#18274=DIRECTION('center_axis',(0.,0.,1.));
#18275=DIRECTION('ref_axis',(1.,-8.10480368384347E-14,0.));
#18276=DIRECTION('center_axis',(0.,0.,-1.));
#18277=DIRECTION('ref_axis',(-0.609338902105852,-0.792909895499126,0.));
#18278=DIRECTION('',(0.,0.,-1.));
#18279=DIRECTION('center_axis',(0.,0.,-1.));
#18280=DIRECTION('ref_axis',(-0.609338902105852,-0.792909895499126,0.));
#18281=DIRECTION('',(0.,0.,-1.));
#18282=DIRECTION('center_axis',(0.,0.,-1.));
#18283=DIRECTION('ref_axis',(-0.609338902105852,-0.792909895499126,0.));
#18284=DIRECTION('',(0.,0.,-1.));
#18285=DIRECTION('center_axis',(0.,0.,-1.));
#18286=DIRECTION('ref_axis',(-0.609338902105852,-0.792909895499126,0.));
#18287=DIRECTION('',(0.,0.,-1.));
#18288=DIRECTION('center_axis',(0.,0.,-1.));
#18289=DIRECTION('ref_axis',(-0.609338902105852,-0.792909895499126,0.));
#18290=DIRECTION('',(0.,0.,-1.));
#18291=DIRECTION('center_axis',(0.,0.,-1.));
#18292=DIRECTION('ref_axis',(-0.609338902105852,-0.792909895499126,0.));
#18293=DIRECTION('',(0.,0.,-1.));
#18294=DIRECTION('center_axis',(0.,0.,-1.));
#18295=DIRECTION('ref_axis',(-0.609338902105852,-0.792909895499126,0.));
#18296=DIRECTION('',(0.,0.,-1.));
#18297=DIRECTION('center_axis',(0.,0.,-1.));
#18298=DIRECTION('ref_axis',(-0.609338902105852,-0.792909895499126,0.));
#18299=DIRECTION('',(0.,0.,-1.));
#18300=DIRECTION('center_axis',(0.,0.,-1.));
#18301=DIRECTION('ref_axis',(-0.609338902105852,-0.792909895499126,0.));
#18302=DIRECTION('',(0.,0.,-1.));
#18303=DIRECTION('center_axis',(0.,0.,-1.));
#18304=DIRECTION('ref_axis',(-0.609338902105852,-0.792909895499126,0.));
#18305=DIRECTION('',(0.,0.,-1.));
#18306=DIRECTION('center_axis',(0.,0.,-1.));
#18307=DIRECTION('ref_axis',(-0.609338902105852,-0.792909895499126,0.));
#18308=DIRECTION('',(0.,0.,-1.));
#18309=DIRECTION('center_axis',(0.,0.,-1.));
#18310=DIRECTION('ref_axis',(-0.609338902105852,-0.792909895499126,0.));
#18311=DIRECTION('',(0.,0.,-1.));
#18312=DIRECTION('center_axis',(0.,0.,-1.));
#18313=DIRECTION('ref_axis',(-0.609338902105852,-0.792909895499126,0.));
#18314=DIRECTION('',(0.,0.,-1.));
#18315=DIRECTION('center_axis',(0.,0.,-1.));
#18316=DIRECTION('ref_axis',(-0.609338902105852,-0.792909895499126,0.));
#18317=DIRECTION('',(0.,0.,-1.));
#18318=DIRECTION('center_axis',(0.,0.,-1.));
#18319=DIRECTION('ref_axis',(-0.609338902105852,-0.792909895499126,0.));
#18320=DIRECTION('',(0.,0.,-1.));
#18321=DIRECTION('center_axis',(0.,0.,-1.));
#18322=DIRECTION('ref_axis',(1.,-8.10480368384347E-14,0.));
#18323=DIRECTION('center_axis',(0.,0.,-1.));
#18324=DIRECTION('ref_axis',(0.938439751642368,-0.345442951205277,0.));
#18325=DIRECTION('',(0.,0.,-1.));
#18326=DIRECTION('center_axis',(0.,0.,1.));
#18327=DIRECTION('ref_axis',(1.,0.,0.));
#18328=DIRECTION('',(0.,0.,-1.));
#18329=DIRECTION('center_axis',(0.,0.,1.));
#18330=DIRECTION('ref_axis',(1.,0.,0.));
#18331=DIRECTION('center_axis',(0.,0.,-1.));
#18332=DIRECTION('ref_axis',(0.938439751642368,-0.345442951205277,0.));
#18333=DIRECTION('',(0.,0.,-1.));
#18334=DIRECTION('center_axis',(0.,0.,-1.));
#18335=DIRECTION('ref_axis',(0.938439751642368,-0.345442951205277,0.));
#18336=DIRECTION('',(0.,0.,-1.));
#18337=DIRECTION('center_axis',(0.,0.,-1.));
#18338=DIRECTION('ref_axis',(0.938439751642368,-0.345442951205277,0.));
#18339=DIRECTION('',(0.,0.,-1.));
#18340=DIRECTION('center_axis',(0.,0.,-1.));
#18341=DIRECTION('ref_axis',(0.938439751642368,-0.345442951205277,0.));
#18342=DIRECTION('',(0.,0.,-1.));
#18343=DIRECTION('center_axis',(0.,0.,-1.));
#18344=DIRECTION('ref_axis',(0.938439751642368,-0.345442951205277,0.));
#18345=DIRECTION('',(0.,0.,-1.));
#18346=DIRECTION('center_axis',(0.,0.,-1.));
#18347=DIRECTION('ref_axis',(0.938439751642368,-0.345442951205277,0.));
#18348=DIRECTION('',(0.,0.,-1.));
#18349=DIRECTION('center_axis',(0.,0.,-1.));
#18350=DIRECTION('ref_axis',(0.938439751642368,-0.345442951205277,0.));
#18351=DIRECTION('',(0.,0.,-1.));
#18352=DIRECTION('center_axis',(0.,0.,-1.));
#18353=DIRECTION('ref_axis',(0.938439751642368,-0.345442951205277,0.));
#18354=DIRECTION('',(0.,0.,-1.));
#18355=DIRECTION('center_axis',(0.,0.,-1.));
#18356=DIRECTION('ref_axis',(0.938439751642368,-0.345442951205277,0.));
#18357=DIRECTION('',(0.,0.,-1.));
#18358=DIRECTION('center_axis',(0.,0.,-1.));
#18359=DIRECTION('ref_axis',(0.938439751642368,-0.345442951205277,0.));
#18360=DIRECTION('',(0.,0.,-1.));
#18361=DIRECTION('center_axis',(0.,0.,-1.));
#18362=DIRECTION('ref_axis',(0.938439751642368,-0.345442951205277,0.));
#18363=DIRECTION('',(0.,0.,-1.));
#18364=DIRECTION('center_axis',(0.,0.,-1.));
#18365=DIRECTION('ref_axis',(0.938439751642368,-0.345442951205277,0.));
#18366=DIRECTION('',(0.,0.,-1.));
#18367=DIRECTION('center_axis',(0.,0.,-1.));
#18368=DIRECTION('ref_axis',(0.938439751642368,-0.345442951205277,0.));
#18369=DIRECTION('',(0.,0.,-1.));
#18370=DIRECTION('center_axis',(0.,0.,-1.));
#18371=DIRECTION('ref_axis',(0.938439751642368,-0.345442951205277,0.));
#18372=DIRECTION('',(0.,0.,-1.));
#18373=DIRECTION('center_axis',(0.,0.,-1.));
#18374=DIRECTION('ref_axis',(1.,0.,0.));
#18375=DIRECTION('center_axis',(0.,0.,-1.));
#18376=DIRECTION('ref_axis',(-0.609338902889834,-0.792909894896648,0.));
#18377=DIRECTION('',(0.,0.,-1.));
#18378=DIRECTION('center_axis',(0.,0.,1.));
#18379=DIRECTION('ref_axis',(1.,-8.10480368384347E-14,0.));
#18380=DIRECTION('center_axis',(0.,0.,-1.));
#18381=DIRECTION('ref_axis',(-0.609338902889834,-0.792909894896648,0.));
#18382=DIRECTION('',(0.,0.,-1.));
#18383=DIRECTION('center_axis',(0.,0.,-1.));
#18384=DIRECTION('ref_axis',(-0.609338902889834,-0.792909894896648,0.));
#18385=DIRECTION('',(0.,0.,-1.));
#18386=DIRECTION('center_axis',(0.,0.,-1.));
#18387=DIRECTION('ref_axis',(-0.609338902889834,-0.792909894896648,0.));
#18388=DIRECTION('',(0.,0.,-1.));
#18389=DIRECTION('center_axis',(0.,0.,-1.));
#18390=DIRECTION('ref_axis',(-0.609338902889834,-0.792909894896648,0.));
#18391=DIRECTION('',(0.,0.,-1.));
#18392=DIRECTION('center_axis',(0.,0.,-1.));
#18393=DIRECTION('ref_axis',(-0.609338902889834,-0.792909894896648,0.));
#18394=DIRECTION('',(0.,0.,-1.));
#18395=DIRECTION('center_axis',(0.,0.,-1.));
#18396=DIRECTION('ref_axis',(-0.609338902889834,-0.792909894896648,0.));
#18397=DIRECTION('',(0.,0.,-1.));
#18398=DIRECTION('center_axis',(0.,0.,-1.));
#18399=DIRECTION('ref_axis',(-0.609338902889834,-0.792909894896648,0.));
#18400=DIRECTION('',(0.,0.,-1.));
#18401=DIRECTION('center_axis',(0.,0.,-1.));
#18402=DIRECTION('ref_axis',(-0.609338902889834,-0.792909894896648,0.));
#18403=DIRECTION('',(0.,0.,-1.));
#18404=DIRECTION('center_axis',(0.,0.,-1.));
#18405=DIRECTION('ref_axis',(-0.609338902889834,-0.792909894896648,0.));
#18406=DIRECTION('',(0.,0.,-1.));
#18407=DIRECTION('center_axis',(0.,0.,-1.));
#18408=DIRECTION('ref_axis',(-0.609338902889834,-0.792909894896648,0.));
#18409=DIRECTION('',(0.,0.,-1.));
#18410=DIRECTION('center_axis',(0.,0.,-1.));
#18411=DIRECTION('ref_axis',(-0.609338902889834,-0.792909894896648,0.));
#18412=DIRECTION('',(0.,0.,-1.));
#18413=DIRECTION('center_axis',(0.,0.,-1.));
#18414=DIRECTION('ref_axis',(-0.609338902889834,-0.792909894896648,0.));
#18415=DIRECTION('',(0.,0.,-1.));
#18416=DIRECTION('center_axis',(0.,0.,-1.));
#18417=DIRECTION('ref_axis',(-0.609338902889834,-0.792909894896648,0.));
#18418=DIRECTION('',(0.,0.,-1.));
#18419=DIRECTION('center_axis',(0.,0.,-1.));
#18420=DIRECTION('ref_axis',(-0.609338902889834,-0.792909894896648,0.));
#18421=DIRECTION('',(0.,0.,-1.));
#18422=DIRECTION('center_axis',(0.,0.,-1.));
#18423=DIRECTION('ref_axis',(-0.609338902889834,-0.792909894896648,0.));
#18424=DIRECTION('',(0.,0.,-1.));
#18425=DIRECTION('center_axis',(0.,0.,-1.));
#18426=DIRECTION('ref_axis',(1.,-8.10480368384347E-14,0.));
#18427=DIRECTION('center_axis',(0.,0.,-1.));
#18428=DIRECTION('ref_axis',(0.938439750900799,-0.345442953219843,0.));
#18429=DIRECTION('',(0.,0.,-1.));
#18430=DIRECTION('center_axis',(0.,0.,1.));
#18431=DIRECTION('ref_axis',(1.,0.,0.));
#18432=DIRECTION('',(0.,0.,-1.));
#18433=DIRECTION('center_axis',(0.,0.,1.));
#18434=DIRECTION('ref_axis',(1.,0.,0.));
#18435=DIRECTION('center_axis',(0.,0.,-1.));
#18436=DIRECTION('ref_axis',(0.938439750900799,-0.345442953219843,0.));
#18437=DIRECTION('',(0.,0.,-1.));
#18438=DIRECTION('center_axis',(0.,0.,-1.));
#18439=DIRECTION('ref_axis',(0.938439750900799,-0.345442953219843,0.));
#18440=DIRECTION('',(0.,0.,-1.));
#18441=DIRECTION('center_axis',(0.,0.,-1.));
#18442=DIRECTION('ref_axis',(0.938439750900799,-0.345442953219843,0.));
#18443=DIRECTION('',(0.,0.,-1.));
#18444=DIRECTION('center_axis',(0.,0.,-1.));
#18445=DIRECTION('ref_axis',(0.938439750900799,-0.345442953219843,0.));
#18446=DIRECTION('',(0.,0.,-1.));
#18447=DIRECTION('center_axis',(0.,0.,-1.));
#18448=DIRECTION('ref_axis',(0.938439750900799,-0.345442953219843,0.));
#18449=DIRECTION('',(0.,0.,-1.));
#18450=DIRECTION('center_axis',(0.,0.,-1.));
#18451=DIRECTION('ref_axis',(0.938439750900799,-0.345442953219843,0.));
#18452=DIRECTION('',(0.,0.,-1.));
#18453=DIRECTION('center_axis',(0.,0.,-1.));
#18454=DIRECTION('ref_axis',(0.938439750900799,-0.345442953219843,0.));
#18455=DIRECTION('',(0.,0.,-1.));
#18456=DIRECTION('center_axis',(0.,0.,-1.));
#18457=DIRECTION('ref_axis',(0.938439750900799,-0.345442953219843,0.));
#18458=DIRECTION('',(0.,0.,-1.));
#18459=DIRECTION('center_axis',(0.,0.,-1.));
#18460=DIRECTION('ref_axis',(0.938439750900799,-0.345442953219843,0.));
#18461=DIRECTION('',(0.,0.,-1.));
#18462=DIRECTION('center_axis',(0.,0.,-1.));
#18463=DIRECTION('ref_axis',(0.938439750900799,-0.345442953219843,0.));
#18464=DIRECTION('',(0.,0.,-1.));
#18465=DIRECTION('center_axis',(0.,0.,-1.));
#18466=DIRECTION('ref_axis',(0.938439750900799,-0.345442953219843,0.));
#18467=DIRECTION('',(0.,0.,-1.));
#18468=DIRECTION('center_axis',(0.,0.,-1.));
#18469=DIRECTION('ref_axis',(0.938439750900799,-0.345442953219843,0.));
#18470=DIRECTION('',(0.,0.,-1.));
#18471=DIRECTION('center_axis',(0.,0.,-1.));
#18472=DIRECTION('ref_axis',(0.938439750900799,-0.345442953219843,0.));
#18473=DIRECTION('',(0.,0.,-1.));
#18474=DIRECTION('center_axis',(0.,0.,-1.));
#18475=DIRECTION('ref_axis',(0.859566642449979,-0.511023665975726,0.));
#18476=DIRECTION('',(0.,0.,-1.));
#18477=DIRECTION('center_axis',(0.,0.,-1.));
#18478=DIRECTION('ref_axis',(1.,0.,0.));
#18479=DIRECTION('center_axis',(1.,0.,0.));
#18480=DIRECTION('ref_axis',(0.,0.609343021033316,-0.792906730150521));
#18481=DIRECTION('',(1.,0.,0.));
#18482=DIRECTION('center_axis',(-1.,0.,0.));
#18483=DIRECTION('ref_axis',(0.,-1.,-7.34835534001807E-14));
#18484=DIRECTION('center_axis',(1.,0.,0.));
#18485=DIRECTION('ref_axis',(0.,0.609343021033316,-0.792906730150521));
#18486=DIRECTION('',(1.,0.,0.));
#18487=DIRECTION('center_axis',(1.,0.,0.));
#18488=DIRECTION('ref_axis',(0.,0.609343021033316,-0.792906730150521));
#18489=DIRECTION('',(1.,0.,0.));
#18490=DIRECTION('center_axis',(1.,0.,0.));
#18491=DIRECTION('ref_axis',(0.,0.609343021033316,-0.792906730150521));
#18492=DIRECTION('',(1.,0.,0.));
#18493=DIRECTION('center_axis',(1.,0.,0.));
#18494=DIRECTION('ref_axis',(0.,0.609343021033316,-0.792906730150521));
#18495=DIRECTION('',(1.,0.,0.));
#18496=DIRECTION('center_axis',(1.,0.,0.));
#18497=DIRECTION('ref_axis',(0.,0.609343021033316,-0.792906730150521));
#18498=DIRECTION('',(1.,0.,0.));
#18499=DIRECTION('center_axis',(1.,0.,0.));
#18500=DIRECTION('ref_axis',(0.,0.609343021033316,-0.792906730150521));
#18501=DIRECTION('',(1.,0.,0.));
#18502=DIRECTION('center_axis',(1.,0.,0.));
#18503=DIRECTION('ref_axis',(0.,0.609343021033316,-0.792906730150521));
#18504=DIRECTION('',(1.,0.,0.));
#18505=DIRECTION('center_axis',(1.,0.,0.));
#18506=DIRECTION('ref_axis',(0.,0.609343021033316,-0.792906730150521));
#18507=DIRECTION('',(1.,0.,0.));
#18508=DIRECTION('center_axis',(1.,0.,0.));
#18509=DIRECTION('ref_axis',(0.,0.609343021033316,-0.792906730150521));
#18510=DIRECTION('',(1.,0.,0.));
#18511=DIRECTION('center_axis',(1.,0.,0.));
#18512=DIRECTION('ref_axis',(0.,0.609343021033316,-0.792906730150521));
#18513=DIRECTION('',(1.,0.,0.));
#18514=DIRECTION('center_axis',(1.,0.,0.));
#18515=DIRECTION('ref_axis',(0.,0.609343021033316,-0.792906730150521));
#18516=DIRECTION('',(1.,0.,0.));
#18517=DIRECTION('center_axis',(1.,0.,0.));
#18518=DIRECTION('ref_axis',(0.,0.609343021033316,-0.792906730150521));
#18519=DIRECTION('',(1.,0.,0.));
#18520=DIRECTION('center_axis',(1.,0.,0.));
#18521=DIRECTION('ref_axis',(0.,0.609343021033316,-0.792906730150521));
#18522=DIRECTION('',(1.,0.,0.));
#18523=DIRECTION('center_axis',(1.,0.,0.));
#18524=DIRECTION('ref_axis',(0.,-1.,-7.34835534001808E-14));
#18525=DIRECTION('center_axis',(1.,0.,0.));
#18526=DIRECTION('ref_axis',(0.,0.609343031978545,-0.792906721739193));
#18527=DIRECTION('',(1.,0.,0.));
#18528=DIRECTION('center_axis',(-1.,0.,0.));
#18529=DIRECTION('ref_axis',(0.,-1.,-7.78061153648973E-14));
#18530=DIRECTION('center_axis',(1.,0.,0.));
#18531=DIRECTION('ref_axis',(0.,0.609343031978545,-0.792906721739193));
#18532=DIRECTION('',(1.,0.,0.));
#18533=DIRECTION('center_axis',(1.,0.,0.));
#18534=DIRECTION('ref_axis',(0.,0.609343031978545,-0.792906721739193));
#18535=DIRECTION('',(1.,0.,0.));
#18536=DIRECTION('center_axis',(1.,0.,0.));
#18537=DIRECTION('ref_axis',(0.,0.609343031978545,-0.792906721739193));
#18538=DIRECTION('',(1.,0.,0.));
#18539=DIRECTION('center_axis',(1.,0.,0.));
#18540=DIRECTION('ref_axis',(0.,0.609343031978545,-0.792906721739193));
#18541=DIRECTION('',(1.,0.,0.));
#18542=DIRECTION('center_axis',(1.,0.,0.));
#18543=DIRECTION('ref_axis',(0.,0.609343031978545,-0.792906721739193));
#18544=DIRECTION('',(1.,0.,0.));
#18545=DIRECTION('center_axis',(1.,0.,0.));
#18546=DIRECTION('ref_axis',(0.,0.609343031978545,-0.792906721739193));
#18547=DIRECTION('',(1.,0.,0.));
#18548=DIRECTION('center_axis',(1.,0.,0.));
#18549=DIRECTION('ref_axis',(0.,0.609343031978545,-0.792906721739193));
#18550=DIRECTION('',(1.,0.,0.));
#18551=DIRECTION('center_axis',(1.,0.,0.));
#18552=DIRECTION('ref_axis',(0.,0.609343031978545,-0.792906721739193));
#18553=DIRECTION('',(1.,0.,0.));
#18554=DIRECTION('center_axis',(1.,0.,0.));
#18555=DIRECTION('ref_axis',(0.,0.609343031978545,-0.792906721739193));
#18556=DIRECTION('',(1.,0.,0.));
#18557=DIRECTION('center_axis',(1.,0.,0.));
#18558=DIRECTION('ref_axis',(0.,0.609343031978545,-0.792906721739193));
#18559=DIRECTION('',(1.,0.,0.));
#18560=DIRECTION('center_axis',(1.,0.,0.));
#18561=DIRECTION('ref_axis',(0.,0.609343031978545,-0.792906721739193));
#18562=DIRECTION('',(1.,0.,0.));
#18563=DIRECTION('center_axis',(1.,0.,0.));
#18564=DIRECTION('ref_axis',(0.,0.609343031978545,-0.792906721739193));
#18565=DIRECTION('',(1.,0.,0.));
#18566=DIRECTION('center_axis',(1.,0.,0.));
#18567=DIRECTION('ref_axis',(0.,0.609343031978545,-0.792906721739193));
#18568=DIRECTION('',(1.,0.,0.));
#18569=DIRECTION('center_axis',(1.,0.,0.));
#18570=DIRECTION('ref_axis',(0.,-1.,-7.78061153648973E-14));
#18571=DIRECTION('center_axis',(1.,0.,0.));
#18572=DIRECTION('ref_axis',(0.,0.609339783037272,-0.792909218516275));
#18573=DIRECTION('',(1.,0.,0.));
#18574=DIRECTION('center_axis',(-1.,0.,0.));
#18575=DIRECTION('ref_axis',(0.,-1.,-7.78061153648971E-14));
#18576=DIRECTION('center_axis',(1.,0.,0.));
#18577=DIRECTION('ref_axis',(0.,0.609339783037272,-0.792909218516275));
#18578=DIRECTION('',(1.,0.,0.));
#18579=DIRECTION('center_axis',(1.,0.,0.));
#18580=DIRECTION('ref_axis',(0.,0.609339783037272,-0.792909218516275));
#18581=DIRECTION('',(1.,0.,0.));
#18582=DIRECTION('center_axis',(1.,0.,0.));
#18583=DIRECTION('ref_axis',(0.,0.609339783037272,-0.792909218516275));
#18584=DIRECTION('',(1.,0.,0.));
#18585=DIRECTION('center_axis',(1.,0.,0.));
#18586=DIRECTION('ref_axis',(0.,0.609339783037272,-0.792909218516275));
#18587=DIRECTION('',(1.,0.,0.));
#18588=DIRECTION('center_axis',(1.,0.,0.));
#18589=DIRECTION('ref_axis',(0.,0.609339783037272,-0.792909218516275));
#18590=DIRECTION('',(1.,0.,0.));
#18591=DIRECTION('center_axis',(1.,0.,0.));
#18592=DIRECTION('ref_axis',(0.,0.609339783037272,-0.792909218516275));
#18593=DIRECTION('',(1.,0.,0.));
#18594=DIRECTION('center_axis',(1.,0.,0.));
#18595=DIRECTION('ref_axis',(0.,0.609339783037272,-0.792909218516275));
#18596=DIRECTION('',(1.,0.,0.));
#18597=DIRECTION('center_axis',(1.,0.,0.));
#18598=DIRECTION('ref_axis',(0.,0.609339783037272,-0.792909218516275));
#18599=DIRECTION('',(1.,0.,0.));
#18600=DIRECTION('center_axis',(1.,0.,0.));
#18601=DIRECTION('ref_axis',(0.,0.609339783037272,-0.792909218516275));
#18602=DIRECTION('',(1.,0.,0.));
#18603=DIRECTION('center_axis',(1.,0.,0.));
#18604=DIRECTION('ref_axis',(0.,0.609339783037272,-0.792909218516275));
#18605=DIRECTION('',(1.,0.,0.));
#18606=DIRECTION('center_axis',(1.,0.,0.));
#18607=DIRECTION('ref_axis',(0.,0.609339783037272,-0.792909218516275));
#18608=DIRECTION('',(1.,0.,0.));
#18609=DIRECTION('center_axis',(1.,0.,0.));
#18610=DIRECTION('ref_axis',(0.,0.609339783037272,-0.792909218516275));
#18611=DIRECTION('',(1.,0.,0.));
#18612=DIRECTION('center_axis',(1.,0.,0.));
#18613=DIRECTION('ref_axis',(0.,0.609339783037272,-0.792909218516275));
#18614=DIRECTION('',(1.,0.,0.));
#18615=DIRECTION('center_axis',(1.,0.,0.));
#18616=DIRECTION('ref_axis',(0.,-1.,-7.78061153648971E-14));
#18617=DIRECTION('center_axis',(1.,0.,0.));
#18618=DIRECTION('ref_axis',(0.,0.609339779193897,-0.792909221469856));
#18619=DIRECTION('',(1.,0.,0.));
#18620=DIRECTION('center_axis',(-1.,0.,0.));
#18621=DIRECTION('ref_axis',(0.,-1.,-6.91609914354641E-14));
#18622=DIRECTION('center_axis',(1.,0.,0.));
#18623=DIRECTION('ref_axis',(0.,0.609339779193897,-0.792909221469856));
#18624=DIRECTION('',(1.,0.,0.));
#18625=DIRECTION('center_axis',(1.,0.,0.));
#18626=DIRECTION('ref_axis',(0.,0.609339779193897,-0.792909221469856));
#18627=DIRECTION('',(1.,0.,0.));
#18628=DIRECTION('center_axis',(1.,0.,0.));
#18629=DIRECTION('ref_axis',(0.,0.609339779193897,-0.792909221469856));
#18630=DIRECTION('',(1.,0.,0.));
#18631=DIRECTION('center_axis',(1.,0.,0.));
#18632=DIRECTION('ref_axis',(0.,0.609339779193897,-0.792909221469856));
#18633=DIRECTION('',(1.,0.,0.));
#18634=DIRECTION('center_axis',(1.,0.,0.));
#18635=DIRECTION('ref_axis',(0.,0.609339779193897,-0.792909221469856));
#18636=DIRECTION('',(1.,0.,0.));
#18637=DIRECTION('center_axis',(1.,0.,0.));
#18638=DIRECTION('ref_axis',(0.,0.609339779193897,-0.792909221469856));
#18639=DIRECTION('',(1.,0.,0.));
#18640=DIRECTION('center_axis',(1.,0.,0.));
#18641=DIRECTION('ref_axis',(0.,0.609339779193897,-0.792909221469856));
#18642=DIRECTION('',(1.,0.,0.));
#18643=DIRECTION('center_axis',(1.,0.,0.));
#18644=DIRECTION('ref_axis',(0.,0.609339779193897,-0.792909221469856));
#18645=DIRECTION('',(1.,0.,0.));
#18646=DIRECTION('center_axis',(1.,0.,0.));
#18647=DIRECTION('ref_axis',(0.,0.609339779193897,-0.792909221469856));
#18648=DIRECTION('',(1.,0.,0.));
#18649=DIRECTION('center_axis',(1.,0.,0.));
#18650=DIRECTION('ref_axis',(0.,0.609339779193897,-0.792909221469856));
#18651=DIRECTION('',(1.,0.,0.));
#18652=DIRECTION('center_axis',(1.,0.,0.));
#18653=DIRECTION('ref_axis',(0.,0.609339779193897,-0.792909221469856));
#18654=DIRECTION('',(1.,0.,0.));
#18655=DIRECTION('center_axis',(1.,0.,0.));
#18656=DIRECTION('ref_axis',(0.,0.609339779193897,-0.792909221469856));
#18657=DIRECTION('',(1.,0.,0.));
#18658=DIRECTION('center_axis',(1.,0.,0.));
#18659=DIRECTION('ref_axis',(0.,0.609339779193897,-0.792909221469856));
#18660=DIRECTION('',(1.,0.,0.));
#18661=DIRECTION('center_axis',(1.,0.,0.));
#18662=DIRECTION('ref_axis',(0.,-1.,-6.91609914354641E-14));
#18663=DIRECTION('center_axis',(1.,0.,0.));
#18664=DIRECTION('ref_axis',(0.,-0.938437982150219,-0.345447758217975));
#18665=DIRECTION('',(1.,0.,0.));
#18666=DIRECTION('center_axis',(-1.,0.,0.));
#18667=DIRECTION('ref_axis',(0.,-1.,0.));
#18668=DIRECTION('center_axis',(1.,0.,0.));
#18669=DIRECTION('ref_axis',(0.,-0.938437982150219,-0.345447758217975));
#18670=DIRECTION('',(1.,0.,0.));
#18671=DIRECTION('center_axis',(1.,0.,0.));
#18672=DIRECTION('ref_axis',(0.,-0.938437982150219,-0.345447758217975));
#18673=DIRECTION('',(1.,0.,0.));
#18674=DIRECTION('center_axis',(1.,0.,0.));
#18675=DIRECTION('ref_axis',(0.,-0.938437982150219,-0.345447758217975));
#18676=DIRECTION('',(1.,0.,0.));
#18677=DIRECTION('center_axis',(1.,0.,0.));
#18678=DIRECTION('ref_axis',(0.,-0.938437982150219,-0.345447758217975));
#18679=DIRECTION('',(1.,0.,0.));
#18680=DIRECTION('center_axis',(1.,0.,0.));
#18681=DIRECTION('ref_axis',(0.,-0.938437982150219,-0.345447758217975));
#18682=DIRECTION('',(1.,0.,0.));
#18683=DIRECTION('center_axis',(1.,0.,0.));
#18684=DIRECTION('ref_axis',(0.,-0.938437982150219,-0.345447758217975));
#18685=DIRECTION('',(1.,0.,0.));
#18686=DIRECTION('center_axis',(1.,0.,0.));
#18687=DIRECTION('ref_axis',(0.,-0.938437982150219,-0.345447758217975));
#18688=DIRECTION('',(1.,0.,0.));
#18689=DIRECTION('center_axis',(1.,0.,0.));
#18690=DIRECTION('ref_axis',(0.,-0.938437982150219,-0.345447758217975));
#18691=DIRECTION('',(1.,0.,0.));
#18692=DIRECTION('center_axis',(1.,0.,0.));
#18693=DIRECTION('ref_axis',(0.,-0.938437982150219,-0.345447758217975));
#18694=DIRECTION('',(1.,0.,0.));
#18695=DIRECTION('center_axis',(1.,0.,0.));
#18696=DIRECTION('ref_axis',(0.,-0.938437982150219,-0.345447758217975));
#18697=DIRECTION('',(1.,0.,0.));
#18698=DIRECTION('center_axis',(1.,0.,0.));
#18699=DIRECTION('ref_axis',(0.,-0.938437982150219,-0.345447758217975));
#18700=DIRECTION('',(1.,0.,0.));
#18701=DIRECTION('center_axis',(1.,0.,0.));
#18702=DIRECTION('ref_axis',(0.,-0.938437982150219,-0.345447758217975));
#18703=DIRECTION('',(1.,0.,0.));
#18704=DIRECTION('center_axis',(1.,0.,0.));
#18705=DIRECTION('ref_axis',(0.,-0.938437982150219,-0.345447758217975));
#18706=DIRECTION('',(1.,0.,0.));
#18707=DIRECTION('center_axis',(1.,0.,0.));
#18708=DIRECTION('ref_axis',(0.,-1.,0.));
#18709=DIRECTION('center_axis',(1.,0.,0.));
#18710=DIRECTION('ref_axis',(0.,-0.938437989074542,-0.345447739407467));
#18711=DIRECTION('',(1.,0.,0.));
#18712=DIRECTION('center_axis',(-1.,0.,0.));
#18713=DIRECTION('ref_axis',(0.,-1.,0.));
#18714=DIRECTION('center_axis',(1.,0.,0.));
#18715=DIRECTION('ref_axis',(0.,-0.938437989074542,-0.345447739407467));
#18716=DIRECTION('',(1.,0.,0.));
#18717=DIRECTION('center_axis',(1.,0.,0.));
#18718=DIRECTION('ref_axis',(0.,-0.938437989074542,-0.345447739407467));
#18719=DIRECTION('',(1.,0.,0.));
#18720=DIRECTION('center_axis',(1.,0.,0.));
#18721=DIRECTION('ref_axis',(0.,-0.938437989074542,-0.345447739407467));
#18722=DIRECTION('',(1.,0.,0.));
#18723=DIRECTION('center_axis',(1.,0.,0.));
#18724=DIRECTION('ref_axis',(0.,-0.938437989074542,-0.345447739407467));
#18725=DIRECTION('',(1.,0.,0.));
#18726=DIRECTION('center_axis',(1.,0.,0.));
#18727=DIRECTION('ref_axis',(0.,-0.938437989074542,-0.345447739407467));
#18728=DIRECTION('',(1.,0.,0.));
#18729=DIRECTION('center_axis',(1.,0.,0.));
#18730=DIRECTION('ref_axis',(0.,-0.938437989074542,-0.345447739407467));
#18731=DIRECTION('',(1.,0.,0.));
#18732=DIRECTION('center_axis',(1.,0.,0.));
#18733=DIRECTION('ref_axis',(0.,-0.938437989074542,-0.345447739407467));
#18734=DIRECTION('',(1.,0.,0.));
#18735=DIRECTION('center_axis',(1.,0.,0.));
#18736=DIRECTION('ref_axis',(0.,-0.938437989074542,-0.345447739407467));
#18737=DIRECTION('',(1.,0.,0.));
#18738=DIRECTION('center_axis',(1.,0.,0.));
#18739=DIRECTION('ref_axis',(0.,-0.938437989074542,-0.345447739407467));
#18740=DIRECTION('',(1.,0.,0.));
#18741=DIRECTION('center_axis',(1.,0.,0.));
#18742=DIRECTION('ref_axis',(0.,-0.938437989074542,-0.345447739407467));
#18743=DIRECTION('',(1.,0.,0.));
#18744=DIRECTION('center_axis',(1.,0.,0.));
#18745=DIRECTION('ref_axis',(0.,-0.938437989074542,-0.345447739407467));
#18746=DIRECTION('',(1.,0.,0.));
#18747=DIRECTION('center_axis',(1.,0.,0.));
#18748=DIRECTION('ref_axis',(0.,-0.938437989074542,-0.345447739407467));
#18749=DIRECTION('',(1.,0.,0.));
#18750=DIRECTION('center_axis',(1.,0.,0.));
#18751=DIRECTION('ref_axis',(0.,-0.938437989074542,-0.345447739407467));
#18752=DIRECTION('',(1.,0.,0.));
#18753=DIRECTION('center_axis',(1.,0.,0.));
#18754=DIRECTION('ref_axis',(0.,-1.,0.));
#18755=DIRECTION('center_axis',(1.,0.,0.));
#18756=DIRECTION('ref_axis',(0.,-0.938439385487086,-0.345443945911084));
#18757=DIRECTION('',(1.,0.,0.));
#18758=DIRECTION('center_axis',(-1.,0.,0.));
#18759=DIRECTION('ref_axis',(0.,-1.,0.));
#18760=DIRECTION('center_axis',(1.,0.,0.));
#18761=DIRECTION('ref_axis',(0.,-0.938439385487086,-0.345443945911084));
#18762=DIRECTION('',(1.,0.,0.));
#18763=DIRECTION('center_axis',(1.,0.,0.));
#18764=DIRECTION('ref_axis',(0.,-0.938439385487086,-0.345443945911084));
#18765=DIRECTION('',(1.,0.,0.));
#18766=DIRECTION('center_axis',(1.,0.,0.));
#18767=DIRECTION('ref_axis',(0.,-0.938439385487086,-0.345443945911084));
#18768=DIRECTION('',(1.,0.,0.));
#18769=DIRECTION('center_axis',(1.,0.,0.));
#18770=DIRECTION('ref_axis',(0.,-0.938439385487086,-0.345443945911084));
#18771=DIRECTION('',(1.,0.,0.));
#18772=DIRECTION('center_axis',(1.,0.,0.));
#18773=DIRECTION('ref_axis',(0.,-0.938439385487086,-0.345443945911084));
#18774=DIRECTION('',(1.,0.,0.));
#18775=DIRECTION('center_axis',(1.,0.,0.));
#18776=DIRECTION('ref_axis',(0.,-0.938439385487086,-0.345443945911084));
#18777=DIRECTION('',(1.,0.,0.));
#18778=DIRECTION('center_axis',(1.,0.,0.));
#18779=DIRECTION('ref_axis',(0.,-0.938439385487086,-0.345443945911084));
#18780=DIRECTION('',(1.,0.,0.));
#18781=DIRECTION('center_axis',(1.,0.,0.));
#18782=DIRECTION('ref_axis',(0.,-0.938439385487086,-0.345443945911084));
#18783=DIRECTION('',(1.,0.,0.));
#18784=DIRECTION('center_axis',(1.,0.,0.));
#18785=DIRECTION('ref_axis',(0.,-0.938439385487086,-0.345443945911084));
#18786=DIRECTION('',(1.,0.,0.));
#18787=DIRECTION('center_axis',(1.,0.,0.));
#18788=DIRECTION('ref_axis',(0.,-0.938439385487086,-0.345443945911084));
#18789=DIRECTION('',(1.,0.,0.));
#18790=DIRECTION('center_axis',(1.,0.,0.));
#18791=DIRECTION('ref_axis',(0.,-0.938439385487086,-0.345443945911084));
#18792=DIRECTION('',(1.,0.,0.));
#18793=DIRECTION('center_axis',(1.,0.,0.));
#18794=DIRECTION('ref_axis',(0.,-0.938439385487086,-0.345443945911084));
#18795=DIRECTION('',(1.,0.,0.));
#18796=DIRECTION('center_axis',(1.,0.,0.));
#18797=DIRECTION('ref_axis',(0.,-0.859572185905443,-0.511014341499081));
#18798=DIRECTION('',(1.,0.,0.));
#18799=DIRECTION('center_axis',(1.,0.,0.));
#18800=DIRECTION('ref_axis',(0.,-1.,0.));
#18801=DIRECTION('center_axis',(1.,0.,0.));
#18802=DIRECTION('ref_axis',(0.,-0.938439382918495,-0.345443952888967));
#18803=DIRECTION('',(1.,0.,0.));
#18804=DIRECTION('center_axis',(-1.,0.,0.));
#18805=DIRECTION('ref_axis',(0.,-1.,0.));
#18806=DIRECTION('center_axis',(1.,0.,0.));
#18807=DIRECTION('ref_axis',(0.,-0.938439382918495,-0.345443952888967));
#18808=DIRECTION('',(1.,0.,0.));
#18809=DIRECTION('center_axis',(1.,0.,0.));
#18810=DIRECTION('ref_axis',(0.,-0.938439382918495,-0.345443952888967));
#18811=DIRECTION('',(1.,0.,0.));
#18812=DIRECTION('center_axis',(1.,0.,0.));
#18813=DIRECTION('ref_axis',(0.,-0.938439382918495,-0.345443952888967));
#18814=DIRECTION('',(1.,0.,0.));
#18815=DIRECTION('center_axis',(1.,0.,0.));
#18816=DIRECTION('ref_axis',(0.,-0.938439382918495,-0.345443952888967));
#18817=DIRECTION('',(1.,0.,0.));
#18818=DIRECTION('center_axis',(1.,0.,0.));
#18819=DIRECTION('ref_axis',(0.,-0.938439382918495,-0.345443952888967));
#18820=DIRECTION('',(1.,0.,0.));
#18821=DIRECTION('center_axis',(1.,0.,0.));
#18822=DIRECTION('ref_axis',(0.,-0.938439382918495,-0.345443952888967));
#18823=DIRECTION('',(1.,0.,0.));
#18824=DIRECTION('center_axis',(1.,0.,0.));
#18825=DIRECTION('ref_axis',(0.,-0.938439382918495,-0.345443952888967));
#18826=DIRECTION('',(1.,0.,0.));
#18827=DIRECTION('center_axis',(1.,0.,0.));
#18828=DIRECTION('ref_axis',(0.,-0.938439382918495,-0.345443952888967));
#18829=DIRECTION('',(1.,0.,0.));
#18830=DIRECTION('center_axis',(1.,0.,0.));
#18831=DIRECTION('ref_axis',(0.,-0.938439382918495,-0.345443952888967));
#18832=DIRECTION('',(1.,0.,0.));
#18833=DIRECTION('center_axis',(1.,0.,0.));
#18834=DIRECTION('ref_axis',(0.,-0.938439382918495,-0.345443952888967));
#18835=DIRECTION('',(1.,0.,0.));
#18836=DIRECTION('center_axis',(1.,0.,0.));
#18837=DIRECTION('ref_axis',(0.,-0.938439382918495,-0.345443952888967));
#18838=DIRECTION('',(1.,0.,0.));
#18839=DIRECTION('center_axis',(1.,0.,0.));
#18840=DIRECTION('ref_axis',(0.,-0.938439382918495,-0.345443952888967));
#18841=DIRECTION('',(1.,0.,0.));
#18842=DIRECTION('center_axis',(1.,0.,0.));
#18843=DIRECTION('ref_axis',(0.,-0.859572206969555,-0.511014306067344));
#18844=DIRECTION('',(1.,0.,0.));
#18845=DIRECTION('center_axis',(1.,0.,0.));
#18846=DIRECTION('ref_axis',(0.,-1.,0.));
#18847=DIRECTION('center_axis',(1.,0.,0.));
#18848=DIRECTION('ref_axis',(0.,-0.938439382918495,-0.345443952888967));
#18849=DIRECTION('center_axis',(1.,0.,0.));
#18850=DIRECTION('ref_axis',(0.,-0.938439385487086,-0.345443945911084));
#18851=DIRECTION('center_axis',(1.,0.,0.));
#18852=DIRECTION('ref_axis',(0.,-0.938437989074542,-0.345447739407467));
#18853=DIRECTION('center_axis',(1.,0.,0.));
#18854=DIRECTION('ref_axis',(0.,-0.938437982150219,-0.345447758217975));
#18855=DIRECTION('center_axis',(1.,0.,0.));
#18856=DIRECTION('ref_axis',(0.,0.609339779193897,-0.792909221469856));
#18857=DIRECTION('center_axis',(1.,0.,0.));
#18858=DIRECTION('ref_axis',(0.,0.609339783037272,-0.792909218516275));
#18859=DIRECTION('center_axis',(1.,0.,0.));
#18860=DIRECTION('ref_axis',(0.,0.609343031978545,-0.792906721739193));
#18861=DIRECTION('center_axis',(1.,0.,0.));
#18862=DIRECTION('ref_axis',(0.,0.609343021033316,-0.792906730150521));
#18863=DIRECTION('center_axis',(0.,0.,-1.));
#18864=DIRECTION('ref_axis',(0.938439750900799,-0.345442953219843,0.));
#18865=DIRECTION('center_axis',(0.,0.,-1.));
#18866=DIRECTION('ref_axis',(-0.609338902889834,-0.792909894896648,0.));
#18867=DIRECTION('center_axis',(0.,0.,-1.));
#18868=DIRECTION('ref_axis',(0.938439751642368,-0.345442951205277,0.));
#18869=DIRECTION('center_axis',(0.,0.,-1.));
#18870=DIRECTION('ref_axis',(-0.609338902105852,-0.792909895499126,0.));
#18871=DIRECTION('center_axis',(0.,0.,1.));
#18872=DIRECTION('ref_axis',(1.,0.,0.));
#18873=DIRECTION('center_axis',(0.,0.,1.));
#18874=DIRECTION('ref_axis',(1.,0.,0.));
#18875=DIRECTION('center_axis',(0.,0.,-1.));
#18876=DIRECTION('ref_axis',(1.,0.,0.));
#18877=DIRECTION('center_axis',(0.,0.,-1.));
#18878=DIRECTION('ref_axis',(1.,0.,0.));
#18879=DIRECTION('center_axis',(0.,1.,0.));
#18880=DIRECTION('ref_axis',(1.,0.,0.));
#18881=DIRECTION('',(-1.,0.,0.));
#18882=DIRECTION('',(0.,0.,-1.));
#18883=DIRECTION('',(1.,0.,0.));
#18884=DIRECTION('',(0.,0.,-1.));
#18885=DIRECTION('center_axis',(-1.,0.,0.));
#18886=DIRECTION('ref_axis',(0.,1.,0.));
#18887=DIRECTION('center_axis',(1.,0.,0.));
#18888=DIRECTION('ref_axis',(0.,1.,0.));
#18889=DIRECTION('',(0.,1.,0.));
#18890=DIRECTION('',(0.,0.,-1.));
#18891=DIRECTION('center_axis',(0.,-1.,0.));
#18892=DIRECTION('ref_axis',(-1.,0.,0.));
#18893=DIRECTION('',(1.,0.,0.));
#18894=DIRECTION('',(-1.,0.,0.));
#18895=DIRECTION('',(0.,0.,-1.));
#18896=DIRECTION('center_axis',(1.,0.,0.));
#18897=DIRECTION('ref_axis',(0.,-1.,0.));
#18898=DIRECTION('center_axis',(-1.,0.,0.));
#18899=DIRECTION('ref_axis',(0.,1.,0.));
#18900=DIRECTION('',(0.,-1.,0.));
#18901=DIRECTION('center_axis',(0.,0.,-1.));
#18902=DIRECTION('ref_axis',(1.,0.,0.));
#18903=DIRECTION('center_axis',(0.,0.,-1.));
#18904=DIRECTION('ref_axis',(1.,0.,0.));
#18905=DIRECTION('',(0.,0.,-1.));
#18906=DIRECTION('center_axis',(0.,0.,1.));
#18907=DIRECTION('ref_axis',(1.,0.,0.));
#18908=DIRECTION('center_axis',(0.,0.,-1.));
#18909=DIRECTION('ref_axis',(1.,0.,0.));
#18910=DIRECTION('center_axis',(0.,0.,-1.));
#18911=DIRECTION('ref_axis',(1.,0.,0.));
#18912=DIRECTION('',(0.,0.,-1.));
#18913=DIRECTION('center_axis',(0.,0.,1.));
#18914=DIRECTION('ref_axis',(1.,0.,0.));
#18915=DIRECTION('center_axis',(0.,0.,-1.));
#18916=DIRECTION('ref_axis',(1.,0.,0.));
#18917=DIRECTION('center_axis',(0.,0.,-1.));
#18918=DIRECTION('ref_axis',(1.,0.,0.));
#18919=DIRECTION('',(0.,0.,-1.));
#18920=DIRECTION('center_axis',(0.,0.,1.));
#18921=DIRECTION('ref_axis',(1.,0.,0.));
#18922=DIRECTION('center_axis',(0.,0.,-1.));
#18923=DIRECTION('ref_axis',(1.,0.,0.));
#18924=DIRECTION('center_axis',(0.,0.,-1.));
#18925=DIRECTION('ref_axis',(1.,0.,0.));
#18926=DIRECTION('',(0.,0.,-1.));
#18927=DIRECTION('center_axis',(0.,0.,1.));
#18928=DIRECTION('ref_axis',(1.,0.,0.));
#18929=DIRECTION('center_axis',(1.,0.,0.));
#18930=DIRECTION('ref_axis',(0.,-1.,0.));
#18931=DIRECTION('center_axis',(1.,0.,0.));
#18932=DIRECTION('ref_axis',(0.,-1.,0.));
#18933=DIRECTION('center_axis',(1.,0.,0.));
#18934=DIRECTION('ref_axis',(0.,-1.,0.));
#18935=DIRECTION('center_axis',(1.,0.,0.));
#18936=DIRECTION('ref_axis',(0.,-1.,0.));
#18937=DIRECTION('center_axis',(-1.,0.,0.));
#18938=DIRECTION('ref_axis',(0.,1.,0.));
#18939=DIRECTION('center_axis',(-1.,0.,0.));
#18940=DIRECTION('ref_axis',(0.,1.,0.));
#18941=DIRECTION('',(-1.,0.,0.));
#18942=DIRECTION('center_axis',(1.,0.,0.));
#18943=DIRECTION('ref_axis',(0.,1.,0.));
#18944=DIRECTION('center_axis',(0.,0.,1.));
#18945=DIRECTION('ref_axis',(1.,0.,0.));
#18946=DIRECTION('',(0.,-1.,0.));
#18947=DIRECTION('',(1.,0.,0.));
#18948=DIRECTION('',(0.,1.,0.));
#18949=DIRECTION('',(-1.,0.,0.));
#18950=DIRECTION('',(-1.,0.,0.));
#18951=DIRECTION('',(0.,1.,0.));
#18952=DIRECTION('',(1.,0.,0.));
#18953=DIRECTION('',(0.,-1.,0.));
#18954=DIRECTION('center_axis',(0.,1.,0.));
#18955=DIRECTION('ref_axis',(-1.,0.,0.));
#18956=DIRECTION('',(-1.,0.,0.));
#18957=DIRECTION('',(0.,0.,1.));
#18958=DIRECTION('',(0.,0.,1.));
#18959=DIRECTION('center_axis',(1.,0.,0.));
#18960=DIRECTION('ref_axis',(0.,1.,0.));
#18961=DIRECTION('',(0.,1.,0.));
#18962=DIRECTION('',(0.,0.,1.));
#18963=DIRECTION('center_axis',(0.,-1.,0.));
#18964=DIRECTION('ref_axis',(1.,0.,0.));
#18965=DIRECTION('',(1.,0.,0.));
#18966=DIRECTION('',(0.,0.,1.));
#18967=DIRECTION('center_axis',(-1.,0.,0.));
#18968=DIRECTION('ref_axis',(0.,-1.,0.));
#18969=DIRECTION('',(0.,-1.,0.));
#18970=DIRECTION('center_axis',(0.,0.,1.));
#18971=DIRECTION('ref_axis',(1.,0.,0.));
#18972=DIRECTION('center_axis',(0.,1.,0.));
#18973=DIRECTION('ref_axis',(-1.,0.,0.));
#18974=DIRECTION('',(0.,0.,1.));
#18975=DIRECTION('',(-1.,0.,0.));
#18976=DIRECTION('',(0.,0.,1.));
#18977=DIRECTION('center_axis',(1.,0.,0.));
#18978=DIRECTION('ref_axis',(0.,1.,0.));
#18979=DIRECTION('',(0.,1.,0.));
#18980=DIRECTION('',(0.,0.,1.));
#18981=DIRECTION('center_axis',(0.,-1.,0.));
#18982=DIRECTION('ref_axis',(1.,0.,0.));
#18983=DIRECTION('',(1.,0.,0.));
#18984=DIRECTION('',(0.,0.,1.));
#18985=DIRECTION('center_axis',(-1.,0.,0.));
#18986=DIRECTION('ref_axis',(0.,-1.,0.));
#18987=DIRECTION('',(0.,-1.,0.));
#18988=DIRECTION('center_axis',(0.,0.,1.));
#18989=DIRECTION('ref_axis',(1.,0.,0.));
#18990=DIRECTION('axis',(0.,0.,1.));
#18991=DIRECTION('refdir',(1.,0.,0.));
#18992=DIRECTION('center_axis',(-1.,0.,0.));
#18993=DIRECTION('ref_axis',(0.,1.,0.));
#18994=DIRECTION('',(0.,0.,1.));
#18995=DIRECTION('',(0.,-1.,0.));
#18996=DIRECTION('',(0.,0.,-1.));
#18997=DIRECTION('',(0.,1.,0.));
#18998=DIRECTION('center_axis',(1.,0.,0.));
#18999=DIRECTION('ref_axis',(0.,-1.,0.));
#19000=DIRECTION('',(0.,0.,-1.));
#19001=DIRECTION('',(0.,-1.,0.));
#19002=DIRECTION('',(0.,0.,1.));
#19003=DIRECTION('',(0.,1.,0.));
#19004=DIRECTION('center_axis',(0.,0.,1.));
#19005=DIRECTION('ref_axis',(1.,0.,0.));
#19006=DIRECTION('center_axis',(0.,0.,1.));
#19007=DIRECTION('ref_axis',(1.,0.,0.));
#19008=DIRECTION('center_axis',(0.,0.,-1.));
#19009=DIRECTION('ref_axis',(1.,0.,0.));
#19010=DIRECTION('center_axis',(0.,0.,1.));
#19011=DIRECTION('ref_axis',(6.12323399573677E-17,-1.,0.));
#19012=DIRECTION('center_axis',(0.,0.,-1.));
#19013=DIRECTION('ref_axis',(1.,0.,0.));
#19014=DIRECTION('center_axis',(0.,0.,1.));
#19015=DIRECTION('ref_axis',(6.12323399573677E-17,-1.,0.));
#19016=DIRECTION('center_axis',(0.,0.,1.));
#19017=DIRECTION('ref_axis',(1.,0.,0.));
#19018=DIRECTION('center_axis',(0.,0.,1.));
#19019=DIRECTION('ref_axis',(1.,0.,0.));
#19020=DIRECTION('axis',(0.,0.,1.));
#19021=DIRECTION('refdir',(1.,0.,0.));
#19022=DIRECTION('center_axis',(0.,0.,1.));
#19023=DIRECTION('ref_axis',(-0.937223598005796,-0.348729017062059,0.));
#19024=DIRECTION('',(0.,0.,1.));
#19025=DIRECTION('center_axis',(0.,0.,-1.));
#19026=DIRECTION('ref_axis',(-1.,0.,0.));
#19027=DIRECTION('',(0.,0.,1.));
#19028=DIRECTION('center_axis',(0.,0.,-1.));
#19029=DIRECTION('ref_axis',(-1.,0.,0.));
#19030=DIRECTION('center_axis',(0.,0.,-1.));
#19031=DIRECTION('ref_axis',(-1.,0.,0.));
#19032=DIRECTION('center_axis',(0.,0.,1.));
#19033=DIRECTION('ref_axis',(-0.937223598005796,-0.348729017062059,0.));
#19034=DIRECTION('',(0.,0.,1.));
#19035=DIRECTION('center_axis',(0.,0.,1.));
#19036=DIRECTION('ref_axis',(-0.937223598005796,-0.348729017062059,0.));
#19037=DIRECTION('',(0.,0.,1.));
#19038=DIRECTION('center_axis',(0.,0.,1.));
#19039=DIRECTION('ref_axis',(-0.937223598005796,-0.348729017062059,0.));
#19040=DIRECTION('',(0.,0.,1.));
#19041=DIRECTION('center_axis',(0.,0.,1.));
#19042=DIRECTION('ref_axis',(-0.937223598005796,-0.348729017062059,0.));
#19043=DIRECTION('',(0.,0.,1.));
#19044=DIRECTION('center_axis',(0.,0.,1.));
#19045=DIRECTION('ref_axis',(-0.937223598005796,-0.348729017062059,0.));
#19046=DIRECTION('',(0.,0.,1.));
#19047=DIRECTION('center_axis',(0.,0.,1.));
#19048=DIRECTION('ref_axis',(-0.937223598005796,-0.348729017062059,0.));
#19049=DIRECTION('',(0.,0.,1.));
#19050=DIRECTION('center_axis',(0.,0.,1.));
#19051=DIRECTION('ref_axis',(-0.937223598005796,-0.348729017062059,0.));
#19052=DIRECTION('',(0.,0.,1.));
#19053=DIRECTION('center_axis',(0.,0.,1.));
#19054=DIRECTION('ref_axis',(-0.937223598005796,-0.348729017062059,0.));
#19055=DIRECTION('',(0.,0.,1.));
#19056=DIRECTION('center_axis',(0.,0.,1.));
#19057=DIRECTION('ref_axis',(-0.937223598005796,-0.348729017062059,0.));
#19058=DIRECTION('',(0.,0.,1.));
#19059=DIRECTION('center_axis',(0.,0.,1.));
#19060=DIRECTION('ref_axis',(-0.937223598005796,-0.348729017062059,0.));
#19061=DIRECTION('',(0.,0.,1.));
#19062=DIRECTION('center_axis',(0.,0.,1.));
#19063=DIRECTION('ref_axis',(-0.937223598005796,-0.348729017062059,0.));
#19064=DIRECTION('',(0.,0.,1.));
#19065=DIRECTION('center_axis',(0.,0.,1.));
#19066=DIRECTION('ref_axis',(-0.937223598005796,-0.348729017062059,0.));
#19067=DIRECTION('',(0.,0.,1.));
#19068=DIRECTION('center_axis',(0.,0.,1.));
#19069=DIRECTION('ref_axis',(-0.937223598005796,-0.348729017062059,0.));
#19070=DIRECTION('',(0.,0.,1.));
#19071=DIRECTION('center_axis',(0.,0.,1.));
#19072=DIRECTION('ref_axis',(-0.937223598005796,-0.348729017062059,0.));
#19073=DIRECTION('',(0.,0.,1.));
#19074=DIRECTION('center_axis',(0.,0.,1.));
#19075=DIRECTION('ref_axis',(-0.937223598005796,-0.348729017062059,0.));
#19076=DIRECTION('',(0.,0.,1.));
#19077=DIRECTION('center_axis',(0.,0.,1.));
#19078=DIRECTION('ref_axis',(-0.937223598005796,-0.348729017062059,0.));
#19079=DIRECTION('',(0.,0.,1.));
#19080=DIRECTION('center_axis',(0.,0.,1.));
#19081=DIRECTION('ref_axis',(-0.937223598005796,-0.348729017062059,0.));
#19082=DIRECTION('',(0.,0.,1.));
#19083=DIRECTION('center_axis',(0.,0.,1.));
#19084=DIRECTION('ref_axis',(-0.937223598005796,-0.348729017062059,0.));
#19085=DIRECTION('',(0.,0.,1.));
#19086=DIRECTION('center_axis',(0.,0.,1.));
#19087=DIRECTION('ref_axis',(-0.937223598005796,-0.348729017062059,0.));
#19088=DIRECTION('',(0.,0.,1.));
#19089=DIRECTION('center_axis',(0.,0.,1.));
#19090=DIRECTION('ref_axis',(-0.937223598005796,-0.348729017062059,0.));
#19091=DIRECTION('',(0.,0.,1.));
#19092=DIRECTION('center_axis',(0.,0.,1.));
#19093=DIRECTION('ref_axis',(-0.937223598005796,-0.348729017062059,0.));
#19094=DIRECTION('',(0.,0.,1.));
#19095=DIRECTION('center_axis',(0.,0.,1.));
#19096=DIRECTION('ref_axis',(-0.937223598005796,-0.348729017062059,0.));
#19097=DIRECTION('',(0.,0.,1.));
#19098=DIRECTION('center_axis',(0.,0.,1.));
#19099=DIRECTION('ref_axis',(-0.937223598005796,-0.348729017062059,0.));
#19100=DIRECTION('',(0.,0.,1.));
#19101=DIRECTION('center_axis',(0.,0.,1.));
#19102=DIRECTION('ref_axis',(-0.937223598005796,-0.348729017062059,0.));
#19103=DIRECTION('',(0.,0.,1.));
#19104=DIRECTION('center_axis',(0.,0.,1.));
#19105=DIRECTION('ref_axis',(-0.937223598005796,-0.348729017062059,0.));
#19106=DIRECTION('',(0.,0.,1.));
#19107=DIRECTION('center_axis',(0.,0.,1.));
#19108=DIRECTION('ref_axis',(-0.937223598005796,-0.348729017062059,0.));
#19109=DIRECTION('',(0.,0.,1.));
#19110=DIRECTION('center_axis',(0.,0.,1.));
#19111=DIRECTION('ref_axis',(-0.937223598005796,-0.348729017062059,0.));
#19112=DIRECTION('',(0.,0.,1.));
#19113=DIRECTION('center_axis',(0.,0.,1.));
#19114=DIRECTION('ref_axis',(-0.937223598005796,-0.348729017062059,0.));
#19115=DIRECTION('',(0.,0.,1.));
#19116=DIRECTION('center_axis',(0.,0.,1.));
#19117=DIRECTION('ref_axis',(-0.937223598005796,-0.348729017062059,0.));
#19118=DIRECTION('',(0.,0.,1.));
#19119=DIRECTION('center_axis',(0.,0.,1.));
#19120=DIRECTION('ref_axis',(-0.937223598005796,-0.348729017062059,0.));
#19121=DIRECTION('',(0.,0.,1.));
#19122=DIRECTION('center_axis',(0.,0.,1.));
#19123=DIRECTION('ref_axis',(-0.937223598005796,-0.348729017062059,0.));
#19124=DIRECTION('',(0.,0.,1.));
#19125=DIRECTION('center_axis',(0.,0.,1.));
#19126=DIRECTION('ref_axis',(-0.937223598005796,-0.348729017062059,0.));
#19127=DIRECTION('',(0.,0.,1.));
#19128=DIRECTION('center_axis',(0.,0.,1.));
#19129=DIRECTION('ref_axis',(-0.937223598005796,-0.348729017062059,0.));
#19130=DIRECTION('',(0.,0.,1.));
#19131=DIRECTION('center_axis',(0.,0.,1.));
#19132=DIRECTION('ref_axis',(-0.937223598005796,-0.348729017062059,0.));
#19133=DIRECTION('',(0.,0.,1.));
#19134=DIRECTION('center_axis',(0.,0.,1.));
#19135=DIRECTION('ref_axis',(-0.937223598005796,-0.348729017062059,0.));
#19136=DIRECTION('',(0.,0.,1.));
#19137=DIRECTION('center_axis',(0.,0.,1.));
#19138=DIRECTION('ref_axis',(-0.937223598005796,-0.348729017062059,0.));
#19139=DIRECTION('',(0.,0.,1.));
#19140=DIRECTION('center_axis',(0.,0.,1.));
#19141=DIRECTION('ref_axis',(-0.937223598005796,-0.348729017062059,0.));
#19142=DIRECTION('',(0.,0.,1.));
#19143=DIRECTION('center_axis',(0.,0.,1.));
#19144=DIRECTION('ref_axis',(-0.937223598005796,-0.348729017062059,0.));
#19145=DIRECTION('',(0.,0.,1.));
#19146=DIRECTION('center_axis',(0.,0.,1.));
#19147=DIRECTION('ref_axis',(-0.937223598005796,-0.348729017062059,0.));
#19148=DIRECTION('',(0.,0.,1.));
#19149=DIRECTION('center_axis',(0.,0.,1.));
#19150=DIRECTION('ref_axis',(-0.937223598005796,-0.348729017062059,0.));
#19151=DIRECTION('',(0.,0.,1.));
#19152=DIRECTION('center_axis',(0.,0.,1.));
#19153=DIRECTION('ref_axis',(-0.937223598005796,-0.348729017062059,0.));
#19154=DIRECTION('',(0.,0.,1.));
#19155=DIRECTION('center_axis',(0.,0.,1.));
#19156=DIRECTION('ref_axis',(-0.937223598005796,-0.348729017062059,0.));
#19157=DIRECTION('',(0.,0.,1.));
#19158=DIRECTION('center_axis',(0.,0.,1.));
#19159=DIRECTION('ref_axis',(-0.937223598005796,-0.348729017062059,0.));
#19160=DIRECTION('',(0.,0.,1.));
#19161=DIRECTION('center_axis',(0.,0.,1.));
#19162=DIRECTION('ref_axis',(-0.937223598005796,-0.348729017062059,0.));
#19163=DIRECTION('',(0.,0.,1.));
#19164=DIRECTION('center_axis',(0.,0.,1.));
#19165=DIRECTION('ref_axis',(-0.937223598005796,-0.348729017062059,0.));
#19166=DIRECTION('',(0.,0.,1.));
#19167=DIRECTION('center_axis',(0.,0.,1.));
#19168=DIRECTION('ref_axis',(-0.937223598005796,-0.348729017062059,0.));
#19169=DIRECTION('',(0.,0.,1.));
#19170=DIRECTION('center_axis',(0.,0.,1.));
#19171=DIRECTION('ref_axis',(-0.937223598005796,-0.348729017062059,0.));
#19172=DIRECTION('',(0.,0.,1.));
#19173=DIRECTION('center_axis',(0.,0.,1.));
#19174=DIRECTION('ref_axis',(-0.937223598005796,-0.348729017062059,0.));
#19175=DIRECTION('',(0.,0.,1.));
#19176=DIRECTION('center_axis',(0.,0.,-1.));
#19177=DIRECTION('ref_axis',(-1.,0.,0.));
#19178=DIRECTION('center_axis',(0.,0.,1.));
#19179=DIRECTION('ref_axis',(-0.937223598005796,-0.348729017062059,0.));
#19180=DIRECTION('center_axis',(0.,0.,1.));
#19181=DIRECTION('ref_axis',(-1.,5.36091303969838E-13,0.));
#19182=DIRECTION('center_axis',(0.,0.,1.));
#19183=DIRECTION('ref_axis',(-1.,5.36091303969838E-13,0.));
#19184=DIRECTION('center_axis',(0.,0.,-1.));
#19185=DIRECTION('ref_axis',(-1.,5.36091303969838E-13,0.));
#19186=DIRECTION('center_axis',(0.,0.,-1.));
#19187=DIRECTION('ref_axis',(-1.,0.,0.));
#19188=DIRECTION('center_axis',(0.,0.,1.));
#19189=DIRECTION('ref_axis',(1.,0.,0.));
#19190=DIRECTION('center_axis',(0.,0.,1.));
#19191=DIRECTION('ref_axis',(1.,0.,0.));
#19192=DIRECTION('center_axis',(0.,0.,1.));
#19193=DIRECTION('ref_axis',(1.,0.,0.));
#19194=DIRECTION('',(-0.0747899482416343,-9.15912707225136E-18,0.997199309888457));
#19195=DIRECTION('center_axis',(0.,0.,-1.));
#19196=DIRECTION('ref_axis',(1.,0.,0.));
#19197=DIRECTION('center_axis',(0.,-1.,0.));
#19198=DIRECTION('ref_axis',(-1.,0.,0.));
#19199=DIRECTION('',(-1.,0.,0.));
#19200=DIRECTION('',(0.,0.,-1.));
#19201=DIRECTION('',(1.,0.,0.));
#19202=DIRECTION('',(0.,0.,-1.));
#19203=DIRECTION('center_axis',(1.,0.,0.));
#19204=DIRECTION('ref_axis',(0.,-1.,0.));
#19205=DIRECTION('',(0.,0.,1.));
#19206=DIRECTION('',(0.,1.,0.));
#19207=DIRECTION('',(0.,-1.,0.));
#19208=DIRECTION('center_axis',(-1.,0.,0.));
#19209=DIRECTION('ref_axis',(0.,1.,0.));
#19210=DIRECTION('',(0.,0.,-1.));
#19211=DIRECTION('',(0.,1.,0.));
#19212=DIRECTION('',(0.,-1.,0.));
#19213=DIRECTION('center_axis',(0.,0.,1.));
#19214=DIRECTION('ref_axis',(1.,0.,0.));
#19215=DIRECTION('center_axis',(0.,0.,1.));
#19216=DIRECTION('ref_axis',(1.,0.,0.));
#19217=DIRECTION('center_axis',(0.,0.,1.));
#19218=DIRECTION('ref_axis',(1.,0.,0.));
#19219=DIRECTION('center_axis',(0.,0.,1.));
#19220=DIRECTION('ref_axis',(-1.,0.,0.));
#19221=DIRECTION('center_axis',(0.,0.,-1.));
#19222=DIRECTION('ref_axis',(1.,0.,0.));
#19223=DIRECTION('center_axis',(0.,0.,1.));
#19224=DIRECTION('ref_axis',(1.,0.,0.));
#19225=DIRECTION('',(0.,0.,1.));
#19226=DIRECTION('center_axis',(0.,0.,1.));
#19227=DIRECTION('ref_axis',(6.12323399573677E-17,-1.,0.));
#19228=DIRECTION('center_axis',(0.,0.,1.));
#19229=DIRECTION('ref_axis',(1.,0.,0.));
#19230=DIRECTION('center_axis',(0.,0.,1.));
#19231=DIRECTION('ref_axis',(1.,0.,0.));
#19232=DIRECTION('axis',(0.,0.,1.));
#19233=DIRECTION('refdir',(1.,0.,0.));
#19234=DIRECTION('center_axis',(0.,0.,-1.));
#19235=DIRECTION('ref_axis',(-1.,0.,0.));
#19236=DIRECTION('center_axis',(0.,0.,1.));
#19237=DIRECTION('ref_axis',(1.,0.,0.));
#19238=DIRECTION('center_axis',(0.,0.,1.));
#19239=DIRECTION('ref_axis',(1.,0.,0.));
#19240=DIRECTION('center_axis',(0.,0.,1.));
#19241=DIRECTION('ref_axis',(1.,0.,0.));
#19242=DIRECTION('',(0.0747899482416343,9.15912707225136E-18,-0.997199309888457));
#19243=DIRECTION('center_axis',(0.,0.,-1.));
#19244=DIRECTION('ref_axis',(-1.,0.,0.));
#19245=DIRECTION('center_axis',(0.,0.,1.));
#19246=DIRECTION('ref_axis',(1.,0.,0.));
#19247=DIRECTION('center_axis',(0.,0.,1.));
#19248=DIRECTION('ref_axis',(1.,0.,0.));
#19249=DIRECTION('center_axis',(0.,0.,1.));
#19250=DIRECTION('ref_axis',(1.,0.,0.));
#19251=DIRECTION('',(0.,0.,-1.));
#19252=DIRECTION('center_axis',(0.,0.,-1.));
#19253=DIRECTION('ref_axis',(1.,0.,0.));
#19254=DIRECTION('',(0.3976074376343,-4.86928675816027E-17,0.917555625309924));
#19255=DIRECTION('axis',(0.,0.,1.));
#19256=DIRECTION('refdir',(1.,0.,0.));
#19257=DIRECTION('center_axis',(0.,0.,-1.));
#19258=DIRECTION('ref_axis',(1.,0.,0.));
#19259=DIRECTION('center_axis',(0.,0.,-1.));
#19260=DIRECTION('ref_axis',(1.,0.,0.));
#19261=DIRECTION('',(0.,0.,-1.));
#19262=DIRECTION('center_axis',(0.,0.,1.));
#19263=DIRECTION('ref_axis',(1.,0.,0.));
#19264=DIRECTION('center_axis',(0.,0.,-1.));
#19265=DIRECTION('ref_axis',(1.,0.,0.));
#19266=DIRECTION('center_axis',(0.,0.,-1.));
#19267=DIRECTION('ref_axis',(1.,0.,0.));
#19268=DIRECTION('',(0.,0.,-1.));
#19269=DIRECTION('center_axis',(0.,0.,1.));
#19270=DIRECTION('ref_axis',(1.,0.,0.));
#19271=DIRECTION('center_axis',(0.,0.,1.));
#19272=DIRECTION('ref_axis',(1.,0.,0.));
#19273=DIRECTION('',(0.,-1.,0.));
#19274=DIRECTION('',(-1.,0.,0.));
#19275=DIRECTION('',(0.,1.,0.));
#19276=DIRECTION('',(1.,0.,0.));
#19277=DIRECTION('',(-1.,0.,0.));
#19278=DIRECTION('',(0.,-1.,0.));
#19279=DIRECTION('',(1.,0.,0.));
#19280=DIRECTION('',(0.,1.,0.));
#19281=DIRECTION('center_axis',(0.,1.,0.));
#19282=DIRECTION('ref_axis',(-1.,0.,0.));
#19283=DIRECTION('',(0.,0.,1.));
#19284=DIRECTION('',(-1.,0.,0.));
#19285=DIRECTION('',(0.,0.,1.));
#19286=DIRECTION('center_axis',(1.,0.,0.));
#19287=DIRECTION('ref_axis',(0.,1.,0.));
#19288=DIRECTION('',(0.,1.,0.));
#19289=DIRECTION('',(0.,0.,1.));
#19290=DIRECTION('center_axis',(0.,-1.,0.));
#19291=DIRECTION('ref_axis',(1.,0.,0.));
#19292=DIRECTION('',(1.,0.,0.));
#19293=DIRECTION('',(0.,0.,1.));
#19294=DIRECTION('center_axis',(-1.,0.,0.));
#19295=DIRECTION('ref_axis',(0.,-1.,0.));
#19296=DIRECTION('',(0.,-1.,0.));
#19297=DIRECTION('center_axis',(0.,0.,1.));
#19298=DIRECTION('ref_axis',(1.,0.,0.));
#19299=DIRECTION('center_axis',(0.,1.,0.));
#19300=DIRECTION('ref_axis',(-1.,0.,0.));
#19301=DIRECTION('',(-1.,0.,0.));
#19302=DIRECTION('',(0.,0.,1.));
#19303=DIRECTION('',(0.,0.,1.));
#19304=DIRECTION('center_axis',(1.,0.,0.));
#19305=DIRECTION('ref_axis',(0.,1.,0.));
#19306=DIRECTION('',(0.,1.,0.));
#19307=DIRECTION('',(0.,0.,1.));
#19308=DIRECTION('center_axis',(0.,-1.,0.));
#19309=DIRECTION('ref_axis',(1.,0.,0.));
#19310=DIRECTION('',(1.,0.,0.));
#19311=DIRECTION('',(0.,0.,1.));
#19312=DIRECTION('center_axis',(-1.,0.,0.));
#19313=DIRECTION('ref_axis',(0.,-1.,0.));
#19314=DIRECTION('',(0.,-1.,0.));
#19315=DIRECTION('center_axis',(0.,0.,1.));
#19316=DIRECTION('ref_axis',(1.,0.,0.));
#19317=DIRECTION('axis',(0.,0.,1.));
#19318=DIRECTION('refdir',(1.,0.,0.));
#19319=DIRECTION('center_axis',(0.,1.,0.));
#19320=DIRECTION('ref_axis',(1.,0.,0.));
#19321=DIRECTION('',(1.,0.,0.));
#19322=DIRECTION('',(0.,0.,1.));
#19323=DIRECTION('',(-1.,0.,0.));
#19324=DIRECTION('',(0.,0.,-1.));
#19325=DIRECTION('center_axis',(1.,0.,0.));
#19326=DIRECTION('ref_axis',(0.,1.,0.));
#19327=DIRECTION('',(0.,1.,0.));
#19328=DIRECTION('',(0.,0.,1.));
#19329=DIRECTION('',(0.,1.,0.));
#19330=DIRECTION('center_axis',(0.,0.,1.));
#19331=DIRECTION('ref_axis',(1.,0.,0.));
#19332=DIRECTION('',(0.,-1.,0.));
#19333=DIRECTION('',(-1.,0.,0.));
#19334=DIRECTION('center_axis',(0.,0.,1.));
#19335=DIRECTION('ref_axis',(1.,0.,0.));
#19336=DIRECTION('center_axis',(0.,0.,1.));
#19337=DIRECTION('ref_axis',(1.,0.,0.));
#19338=DIRECTION('center_axis',(0.,0.,1.));
#19339=DIRECTION('ref_axis',(1.,0.,0.));
#19340=DIRECTION('center_axis',(0.,0.,1.));
#19341=DIRECTION('ref_axis',(1.,0.,0.));
#19342=DIRECTION('center_axis',(0.,0.,1.));
#19343=DIRECTION('ref_axis',(1.,0.,0.));
#19344=DIRECTION('center_axis',(0.,0.,-1.));
#19345=DIRECTION('ref_axis',(1.,0.,0.));
#19346=DIRECTION('center_axis',(0.,0.,-1.));
#19347=DIRECTION('ref_axis',(1.,0.,0.));
#19348=DIRECTION('',(0.,0.,-1.));
#19349=DIRECTION('center_axis',(0.,0.,-1.));
#19350=DIRECTION('ref_axis',(1.,0.,0.));
#19351=DIRECTION('center_axis',(0.,0.,-1.));
#19352=DIRECTION('ref_axis',(1.,0.,0.));
#19353=DIRECTION('',(0.,0.,-1.));
#19354=DIRECTION('center_axis',(0.,0.,-1.));
#19355=DIRECTION('ref_axis',(1.,0.,0.));
#19356=DIRECTION('center_axis',(0.,0.,-1.));
#19357=DIRECTION('ref_axis',(1.,0.,0.));
#19358=DIRECTION('',(0.,0.,-1.));
#19359=DIRECTION('center_axis',(0.,0.,-1.));
#19360=DIRECTION('ref_axis',(1.,0.,0.));
#19361=DIRECTION('center_axis',(0.,0.,-1.));
#19362=DIRECTION('ref_axis',(1.,0.,0.));
#19363=DIRECTION('',(0.,0.,-1.));
#19364=DIRECTION('center_axis',(0.,0.,-1.));
#19365=DIRECTION('ref_axis',(1.,0.,0.));
#19366=DIRECTION('center_axis',(0.,0.,-1.));
#19367=DIRECTION('ref_axis',(1.,0.,0.));
#19368=DIRECTION('',(0.,0.,-1.));
#19369=DIRECTION('center_axis',(0.,1.,0.));
#19370=DIRECTION('ref_axis',(-1.,0.,0.));
#19371=DIRECTION('',(0.,0.,1.));
#19372=DIRECTION('',(-1.,0.,0.));
#19373=DIRECTION('center_axis',(-1.,0.,0.));
#19374=DIRECTION('ref_axis',(0.,-1.,0.));
#19375=DIRECTION('',(0.,-1.,0.));
#19376=DIRECTION('center_axis',(0.,0.,1.));
#19377=DIRECTION('ref_axis',(1.,0.,0.));
#19378=DIRECTION('axis',(0.,0.,1.));
#19379=DIRECTION('refdir',(1.,0.,0.));
#19380=DIRECTION('center_axis',(0.,0.,1.));
#19381=DIRECTION('ref_axis',(1.,0.,0.));
#19382=DIRECTION('center_axis',(0.,0.,-1.));
#19383=DIRECTION('ref_axis',(1.,0.,0.));
#19384=DIRECTION('',(0.,0.,1.));
#19385=DIRECTION('center_axis',(0.,0.,-1.));
#19386=DIRECTION('ref_axis',(1.,0.,0.));
#19387=DIRECTION('center_axis',(0.,0.,1.));
#19388=DIRECTION('ref_axis',(1.,0.,0.));
#19389=DIRECTION('center_axis',(0.,0.,1.));
#19390=DIRECTION('ref_axis',(1.,0.,0.));
#19391=DIRECTION('',(0.,0.,-1.));
#19392=DIRECTION('center_axis',(0.,0.,1.));
#19393=DIRECTION('ref_axis',(1.,0.,0.));
#19394=DIRECTION('center_axis',(0.,0.,1.));
#19395=DIRECTION('ref_axis',(1.,0.,0.));
#19396=DIRECTION('center_axis',(0.,0.,1.));
#19397=DIRECTION('ref_axis',(1.,0.,0.));
#19398=DIRECTION('axis',(0.,0.,1.));
#19399=DIRECTION('refdir',(1.,0.,0.));
#19400=DIRECTION('center_axis',(0.,0.,1.));
#19401=DIRECTION('ref_axis',(-0.457973429632235,-0.888965881094932,0.));
#19402=DIRECTION('',(0.,0.,-1.));
#19403=DIRECTION('center_axis',(0.,0.,-1.));
#19404=DIRECTION('ref_axis',(1.,-1.02558375769811E-12,0.));
#19405=DIRECTION('center_axis',(0.,0.,1.));
#19406=DIRECTION('ref_axis',(-0.457973429632235,-0.888965881094932,0.));
#19407=DIRECTION('',(0.,0.,-1.));
#19408=DIRECTION('center_axis',(0.,0.,1.));
#19409=DIRECTION('ref_axis',(-0.457973429632235,-0.888965881094932,0.));
#19410=DIRECTION('',(0.,0.,-1.));
#19411=DIRECTION('center_axis',(0.,0.,1.));
#19412=DIRECTION('ref_axis',(-0.457973429632235,-0.888965881094932,0.));
#19413=DIRECTION('',(0.,0.,-1.));
#19414=DIRECTION('center_axis',(0.,0.,1.));
#19415=DIRECTION('ref_axis',(-0.457973429632235,-0.888965881094932,0.));
#19416=DIRECTION('',(0.,0.,-1.));
#19417=DIRECTION('center_axis',(0.,0.,1.));
#19418=DIRECTION('ref_axis',(-0.457973429632235,-0.888965881094932,0.));
#19419=DIRECTION('',(0.,0.,-1.));
#19420=DIRECTION('center_axis',(0.,0.,1.));
#19421=DIRECTION('ref_axis',(-0.457973429632235,-0.888965881094932,0.));
#19422=DIRECTION('',(0.,0.,-1.));
#19423=DIRECTION('center_axis',(0.,0.,1.));
#19424=DIRECTION('ref_axis',(-0.457973429632235,-0.888965881094932,0.));
#19425=DIRECTION('',(0.,0.,-1.));
#19426=DIRECTION('center_axis',(0.,0.,1.));
#19427=DIRECTION('ref_axis',(-0.457973429632235,-0.888965881094932,0.));
#19428=DIRECTION('',(0.,0.,-1.));
#19429=DIRECTION('center_axis',(0.,0.,1.));
#19430=DIRECTION('ref_axis',(-0.457973429632235,-0.888965881094932,0.));
#19431=DIRECTION('',(0.,0.,-1.));
#19432=DIRECTION('center_axis',(0.,0.,1.));
#19433=DIRECTION('ref_axis',(-0.457973429632235,-0.888965881094932,0.));
#19434=DIRECTION('',(0.,0.,-1.));
#19435=DIRECTION('center_axis',(0.,0.,1.));
#19436=DIRECTION('ref_axis',(-0.457973429632235,-0.888965881094932,0.));
#19437=DIRECTION('',(0.,0.,-1.));
#19438=DIRECTION('center_axis',(0.,0.,1.));
#19439=DIRECTION('ref_axis',(-0.457973429632235,-0.888965881094932,0.));
#19440=DIRECTION('',(0.,0.,-1.));
#19441=DIRECTION('center_axis',(0.,0.,1.));
#19442=DIRECTION('ref_axis',(-0.457973429632235,-0.888965881094932,0.));
#19443=DIRECTION('',(0.,0.,-1.));
#19444=DIRECTION('center_axis',(0.,0.,1.));
#19445=DIRECTION('ref_axis',(-0.457973429632235,-0.888965881094932,0.));
#19446=DIRECTION('',(0.,0.,-1.));
#19447=DIRECTION('center_axis',(0.,0.,1.));
#19448=DIRECTION('ref_axis',(-0.457973429632235,-0.888965881094932,0.));
#19449=DIRECTION('',(0.,0.,-1.));
#19450=DIRECTION('center_axis',(0.,0.,1.));
#19451=DIRECTION('ref_axis',(-0.457973429632235,-0.888965881094932,0.));
#19452=DIRECTION('',(0.,0.,-1.));
#19453=DIRECTION('center_axis',(0.,0.,1.));
#19454=DIRECTION('ref_axis',(-0.457973429632235,-0.888965881094932,0.));
#19455=DIRECTION('',(0.,0.,-1.));
#19456=DIRECTION('center_axis',(0.,0.,1.));
#19457=DIRECTION('ref_axis',(-0.457973429632235,-0.888965881094932,0.));
#19458=DIRECTION('',(0.,0.,-1.));
#19459=DIRECTION('center_axis',(0.,0.,1.));
#19460=DIRECTION('ref_axis',(-0.457973429632235,-0.888965881094932,0.));
#19461=DIRECTION('',(0.,0.,-1.));
#19462=DIRECTION('center_axis',(0.,0.,1.));
#19463=DIRECTION('ref_axis',(-0.457973429632235,-0.888965881094932,0.));
#19464=DIRECTION('',(0.,0.,-1.));
#19465=DIRECTION('center_axis',(0.,0.,1.));
#19466=DIRECTION('ref_axis',(-0.457973429632235,-0.888965881094932,0.));
#19467=DIRECTION('',(0.,0.,-1.));
#19468=DIRECTION('center_axis',(0.,0.,1.));
#19469=DIRECTION('ref_axis',(-0.457973429632235,-0.888965881094932,0.));
#19470=DIRECTION('',(0.,0.,-1.));
#19471=DIRECTION('center_axis',(0.,0.,1.));
#19472=DIRECTION('ref_axis',(-0.457973429632235,-0.888965881094932,0.));
#19473=DIRECTION('',(0.,0.,-1.));
#19474=DIRECTION('center_axis',(0.,0.,1.));
#19475=DIRECTION('ref_axis',(-0.457973429632235,-0.888965881094932,0.));
#19476=DIRECTION('',(0.,0.,-1.));
#19477=DIRECTION('center_axis',(0.,0.,1.));
#19478=DIRECTION('ref_axis',(-0.457973429632235,-0.888965881094932,0.));
#19479=DIRECTION('',(0.,0.,-1.));
#19480=DIRECTION('center_axis',(0.,0.,1.));
#19481=DIRECTION('ref_axis',(-0.457973429632235,-0.888965881094932,0.));
#19482=DIRECTION('',(0.,0.,-1.));
#19483=DIRECTION('center_axis',(0.,0.,1.));
#19484=DIRECTION('ref_axis',(-0.457973429632235,-0.888965881094932,0.));
#19485=DIRECTION('',(0.,0.,-1.));
#19486=DIRECTION('center_axis',(0.,0.,1.));
#19487=DIRECTION('ref_axis',(-0.457973429632235,-0.888965881094932,0.));
#19488=DIRECTION('',(0.,0.,-1.));
#19489=DIRECTION('center_axis',(0.,0.,1.));
#19490=DIRECTION('ref_axis',(-0.457973429632235,-0.888965881094932,0.));
#19491=DIRECTION('',(0.,0.,-1.));
#19492=DIRECTION('center_axis',(0.,0.,1.));
#19493=DIRECTION('ref_axis',(-0.457973429632235,-0.888965881094932,0.));
#19494=DIRECTION('',(0.,0.,-1.));
#19495=DIRECTION('center_axis',(0.,0.,1.));
#19496=DIRECTION('ref_axis',(-0.457973429632235,-0.888965881094932,0.));
#19497=DIRECTION('',(0.,0.,-1.));
#19498=DIRECTION('center_axis',(0.,0.,1.));
#19499=DIRECTION('ref_axis',(-0.457973429632235,-0.888965881094932,0.));
#19500=DIRECTION('',(0.,0.,-1.));
#19501=DIRECTION('center_axis',(0.,0.,1.));
#19502=DIRECTION('ref_axis',(-0.457973429632235,-0.888965881094932,0.));
#19503=DIRECTION('',(0.,0.,-1.));
#19504=DIRECTION('center_axis',(0.,0.,1.));
#19505=DIRECTION('ref_axis',(-0.457973429632235,-0.888965881094932,0.));
#19506=DIRECTION('',(0.,0.,-1.));
#19507=DIRECTION('center_axis',(0.,0.,1.));
#19508=DIRECTION('ref_axis',(-0.457973429632235,-0.888965881094932,0.));
#19509=DIRECTION('',(0.,0.,-1.));
#19510=DIRECTION('center_axis',(0.,0.,1.));
#19511=DIRECTION('ref_axis',(-0.457973429632235,-0.888965881094932,0.));
#19512=DIRECTION('',(0.,0.,-1.));
#19513=DIRECTION('center_axis',(0.,0.,1.));
#19514=DIRECTION('ref_axis',(-0.457973429632235,-0.888965881094932,0.));
#19515=DIRECTION('',(0.,0.,-1.));
#19516=DIRECTION('center_axis',(0.,0.,1.));
#19517=DIRECTION('ref_axis',(-0.457973429632235,-0.888965881094932,0.));
#19518=DIRECTION('',(0.,0.,-1.));
#19519=DIRECTION('center_axis',(0.,0.,1.));
#19520=DIRECTION('ref_axis',(-0.457973429632235,-0.888965881094932,0.));
#19521=DIRECTION('',(0.,0.,-1.));
#19522=DIRECTION('center_axis',(0.,0.,1.));
#19523=DIRECTION('ref_axis',(-0.457973429632235,-0.888965881094932,0.));
#19524=DIRECTION('',(0.,0.,-1.));
#19525=DIRECTION('center_axis',(0.,0.,1.));
#19526=DIRECTION('ref_axis',(-0.457973429632235,-0.888965881094932,0.));
#19527=DIRECTION('',(0.,0.,-1.));
#19528=DIRECTION('center_axis',(0.,0.,1.));
#19529=DIRECTION('ref_axis',(-0.457973429632235,-0.888965881094932,0.));
#19530=DIRECTION('',(0.,0.,-1.));
#19531=DIRECTION('center_axis',(0.,0.,1.));
#19532=DIRECTION('ref_axis',(-0.457973429632235,-0.888965881094932,0.));
#19533=DIRECTION('',(0.,0.,-1.));
#19534=DIRECTION('center_axis',(0.,0.,1.));
#19535=DIRECTION('ref_axis',(-0.457973429632235,-0.888965881094932,0.));
#19536=DIRECTION('',(0.,0.,-1.));
#19537=DIRECTION('center_axis',(0.,0.,1.));
#19538=DIRECTION('ref_axis',(-0.457973429632235,-0.888965881094932,0.));
#19539=DIRECTION('',(0.,0.,-1.));
#19540=DIRECTION('center_axis',(0.,0.,1.));
#19541=DIRECTION('ref_axis',(-0.457973429632235,-0.888965881094932,0.));
#19542=DIRECTION('',(0.,0.,-1.));
#19543=DIRECTION('center_axis',(0.,0.,1.));
#19544=DIRECTION('ref_axis',(-0.457973429632235,-0.888965881094932,0.));
#19545=DIRECTION('',(0.,0.,-1.));
#19546=DIRECTION('center_axis',(0.,0.,1.));
#19547=DIRECTION('ref_axis',(-0.457973429632235,-0.888965881094932,0.));
#19548=DIRECTION('',(0.,0.,-1.));
#19549=DIRECTION('center_axis',(0.,0.,1.));
#19550=DIRECTION('ref_axis',(-0.457973429632235,-0.888965881094932,0.));
#19551=DIRECTION('',(0.,0.,-1.));
#19552=DIRECTION('center_axis',(0.,0.,1.));
#19553=DIRECTION('ref_axis',(-0.457973429632235,-0.888965881094932,0.));
#19554=DIRECTION('',(0.,0.,-1.));
#19555=DIRECTION('center_axis',(0.,0.,1.));
#19556=DIRECTION('ref_axis',(-0.457973429632235,-0.888965881094932,0.));
#19557=DIRECTION('',(0.,0.,-1.));
#19558=DIRECTION('center_axis',(0.,0.,1.));
#19559=DIRECTION('ref_axis',(-0.457973429632235,-0.888965881094932,0.));
#19560=DIRECTION('',(0.,0.,-1.));
#19561=DIRECTION('center_axis',(0.,0.,1.));
#19562=DIRECTION('ref_axis',(-0.457973429632235,-0.888965881094932,0.));
#19563=DIRECTION('',(0.,0.,-1.));
#19564=DIRECTION('center_axis',(0.,0.,1.));
#19565=DIRECTION('ref_axis',(-0.457973429632235,-0.888965881094932,0.));
#19566=DIRECTION('',(0.,0.,-1.));
#19567=DIRECTION('center_axis',(0.,0.,1.));
#19568=DIRECTION('ref_axis',(-0.457973429632235,-0.888965881094932,0.));
#19569=DIRECTION('',(0.,0.,-1.));
#19570=DIRECTION('center_axis',(0.,0.,1.));
#19571=DIRECTION('ref_axis',(-0.457973429632235,-0.888965881094932,0.));
#19572=DIRECTION('',(0.,0.,-1.));
#19573=DIRECTION('center_axis',(0.,0.,1.));
#19574=DIRECTION('ref_axis',(-0.457973429632235,-0.888965881094932,0.));
#19575=DIRECTION('',(0.,0.,-1.));
#19576=DIRECTION('center_axis',(0.,0.,1.));
#19577=DIRECTION('ref_axis',(-0.457973429632235,-0.888965881094932,0.));
#19578=DIRECTION('',(0.,0.,-1.));
#19579=DIRECTION('center_axis',(0.,0.,1.));
#19580=DIRECTION('ref_axis',(-0.457973429632235,-0.888965881094932,0.));
#19581=DIRECTION('',(0.,0.,-1.));
#19582=DIRECTION('center_axis',(0.,0.,1.));
#19583=DIRECTION('ref_axis',(-0.457973429632235,-0.888965881094932,0.));
#19584=DIRECTION('',(0.,0.,-1.));
#19585=DIRECTION('center_axis',(0.,0.,1.));
#19586=DIRECTION('ref_axis',(-0.457973429632235,-0.888965881094932,0.));
#19587=DIRECTION('',(0.,0.,-1.));
#19588=DIRECTION('center_axis',(0.,0.,1.));
#19589=DIRECTION('ref_axis',(-0.457973429632235,-0.888965881094932,0.));
#19590=DIRECTION('',(0.,0.,-1.));
#19591=DIRECTION('center_axis',(0.,0.,1.));
#19592=DIRECTION('ref_axis',(-0.457973429632235,-0.888965881094932,0.));
#19593=DIRECTION('',(0.,0.,-1.));
#19594=DIRECTION('center_axis',(0.,0.,1.));
#19595=DIRECTION('ref_axis',(-0.457973429632235,-0.888965881094932,0.));
#19596=DIRECTION('',(0.,0.,-1.));
#19597=DIRECTION('center_axis',(0.,0.,1.));
#19598=DIRECTION('ref_axis',(1.,0.,0.));
#19599=DIRECTION('center_axis',(0.,0.,-1.));
#19600=DIRECTION('ref_axis',(1.,0.,0.));
#19601=DIRECTION('center_axis',(0.,0.,-1.));
#19602=DIRECTION('ref_axis',(1.,0.,0.));
#19603=DIRECTION('center_axis',(0.,0.,1.));
#19604=DIRECTION('ref_axis',(-0.457973429632235,-0.888965881094932,0.));
#19605=DIRECTION('center_axis',(0.,0.,1.));
#19606=DIRECTION('ref_axis',(1.,-1.02558375769811E-12,0.));
#19607=DIRECTION('center_axis',(-1.,0.,0.));
#19608=DIRECTION('ref_axis',(0.,1.,0.));
#19609=DIRECTION('',(-1.,0.,0.));
#19610=DIRECTION('center_axis',(0.,0.,1.));
#19611=DIRECTION('ref_axis',(1.,0.,0.));
#19612=DIRECTION('center_axis',(0.,0.,1.));
#19613=DIRECTION('ref_axis',(1.,0.,0.));
#19614=DIRECTION('center_axis',(0.,0.,1.));
#19615=DIRECTION('ref_axis',(1.,0.,0.));
#19616=DIRECTION('center_axis',(0.,0.,-1.));
#19617=DIRECTION('ref_axis',(1.,0.,0.));
#19618=DIRECTION('center_axis',(0.,0.,1.));
#19619=DIRECTION('ref_axis',(1.,0.,0.));
#19620=DIRECTION('center_axis',(0.,0.,1.));
#19621=DIRECTION('ref_axis',(1.,0.,0.));
#19622=DIRECTION('',(0.,0.,-1.));
#19623=DIRECTION('center_axis',(0.,0.,1.));
#19624=DIRECTION('ref_axis',(1.,0.,0.));
#19625=DIRECTION('',(0.,0.,-1.));
#19626=DIRECTION('',(0.,0.,-1.));
#19627=DIRECTION('center_axis',(0.,0.,1.));
#19628=DIRECTION('ref_axis',(1.,0.,0.));
#19629=DIRECTION('center_axis',(0.,0.,1.));
#19630=DIRECTION('ref_axis',(1.,0.,0.));
#19631=DIRECTION('center_axis',(0.,0.,1.));
#19632=DIRECTION('ref_axis',(1.,0.,0.));
#19633=DIRECTION('axis',(0.,0.,1.));
#19634=DIRECTION('refdir',(1.,0.,0.));
#19635=DIRECTION('center_axis',(-1.,0.,0.));
#19636=DIRECTION('ref_axis',(0.,1.,0.));
#19637=DIRECTION('',(-1.,0.,0.));
#19638=DIRECTION('center_axis',(-1.,0.,0.));
#19639=DIRECTION('ref_axis',(0.,1.,0.));
#19640=DIRECTION('',(-1.,0.,0.));
#19641=DIRECTION('center_axis',(0.,0.,-1.));
#19642=DIRECTION('ref_axis',(1.,0.,0.));
#19643=DIRECTION('center_axis',(0.,0.,-1.));
#19644=DIRECTION('ref_axis',(1.,0.,0.));
#19645=DIRECTION('',(0.,0.,-1.));
#19646=DIRECTION('center_axis',(0.,0.,1.));
#19647=DIRECTION('ref_axis',(1.,0.,0.));
#19648=DIRECTION('center_axis',(0.,0.,-1.));
#19649=DIRECTION('ref_axis',(1.,0.,0.));
#19650=DIRECTION('center_axis',(0.,0.,-1.));
#19651=DIRECTION('ref_axis',(1.,0.,0.));
#19652=DIRECTION('',(0.,0.,-1.));
#19653=DIRECTION('center_axis',(0.,0.,1.));
#19654=DIRECTION('ref_axis',(1.,0.,0.));
#19655=DIRECTION('center_axis',(0.,0.,-1.));
#19656=DIRECTION('ref_axis',(1.,0.,0.));
#19657=DIRECTION('center_axis',(0.,0.,-1.));
#19658=DIRECTION('ref_axis',(1.,0.,0.));
#19659=DIRECTION('',(0.,0.,-1.));
#19660=DIRECTION('center_axis',(0.,0.,1.));
#19661=DIRECTION('ref_axis',(1.,0.,0.));
#19662=DIRECTION('center_axis',(0.,0.,-1.));
#19663=DIRECTION('ref_axis',(1.,0.,0.));
#19664=DIRECTION('center_axis',(0.,0.,-1.));
#19665=DIRECTION('ref_axis',(1.,0.,0.));
#19666=DIRECTION('',(0.,0.,-1.));
#19667=DIRECTION('center_axis',(0.,0.,1.));
#19668=DIRECTION('ref_axis',(1.,0.,0.));
#19669=DIRECTION('center_axis',(0.,0.,-1.));
#19670=DIRECTION('ref_axis',(1.,0.,0.));
#19671=DIRECTION('center_axis',(0.,0.,-1.));
#19672=DIRECTION('ref_axis',(1.,0.,0.));
#19673=DIRECTION('',(0.,0.,-1.));
#19674=DIRECTION('center_axis',(0.,0.,1.));
#19675=DIRECTION('ref_axis',(1.,0.,0.));
#19676=DIRECTION('center_axis',(0.,0.,-1.));
#19677=DIRECTION('ref_axis',(1.,0.,0.));
#19678=DIRECTION('center_axis',(0.,0.,-1.));
#19679=DIRECTION('ref_axis',(1.,0.,0.));
#19680=DIRECTION('',(0.,0.,-1.));
#19681=DIRECTION('center_axis',(0.,0.,1.));
#19682=DIRECTION('ref_axis',(1.,0.,0.));
#19683=DIRECTION('center_axis',(0.,0.,1.));
#19684=DIRECTION('ref_axis',(1.,0.,0.));
#19685=DIRECTION('center_axis',(0.,0.,1.));
#19686=DIRECTION('ref_axis',(1.,0.,0.));
#19687=DIRECTION('',(0.,0.,-1.));
#19688=DIRECTION('',(0.,0.,-1.));
#19689=DIRECTION('center_axis',(0.,0.,-1.));
#19690=DIRECTION('ref_axis',(1.,0.,0.));
#19691=DIRECTION('center_axis',(0.,0.,1.));
#19692=DIRECTION('ref_axis',(1.,0.,0.));
#19693=DIRECTION('center_axis',(0.,0.,-1.));
#19694=DIRECTION('ref_axis',(1.,0.,0.));
#19695=DIRECTION('center_axis',(0.,0.,1.));
#19696=DIRECTION('ref_axis',(1.,0.,0.));
#19697=DIRECTION('center_axis',(0.,0.,-1.));
#19698=DIRECTION('ref_axis',(1.,0.,0.));
#19699=DIRECTION('',(0.,0.,1.));
#19700=DIRECTION('',(0.,0.,1.));
#19701=DIRECTION('center_axis',(0.,0.,1.));
#19702=DIRECTION('ref_axis',(1.,0.,0.));
#19703=DIRECTION('center_axis',(0.,0.,-1.));
#19704=DIRECTION('ref_axis',(1.,0.,0.));
#19705=DIRECTION('',(0.,0.,-1.));
#19706=DIRECTION('center_axis',(0.,0.,-1.));
#19707=DIRECTION('ref_axis',(1.,0.,0.));
#19708=DIRECTION('center_axis',(0.,0.,1.));
#19709=DIRECTION('ref_axis',(1.,0.,0.));
#19710=DIRECTION('center_axis',(0.,0.,1.));
#19711=DIRECTION('ref_axis',(1.,0.,0.));
#19712=DIRECTION('axis',(0.,0.,1.));
#19713=DIRECTION('refdir',(1.,0.,0.));
#19714=DIRECTION('center_axis',(0.,0.,1.));
#19715=DIRECTION('ref_axis',(1.,0.,0.));
#19716=DIRECTION('center_axis',(0.,0.,1.));
#19717=DIRECTION('ref_axis',(1.,0.,0.));
#19718=DIRECTION('',(0.,0.,-1.));
#19719=DIRECTION('center_axis',(0.,0.,1.));
#19720=DIRECTION('ref_axis',(1.,0.,0.));
#19721=DIRECTION('center_axis',(0.,0.,-1.));
#19722=DIRECTION('ref_axis',(-1.,0.,0.));
#19723=DIRECTION('center_axis',(0.,0.,-1.));
#19724=DIRECTION('ref_axis',(1.,0.,0.));
#19725=DIRECTION('center_axis',(0.,0.,1.));
#19726=DIRECTION('ref_axis',(1.,0.,0.));
#19727=DIRECTION('center_axis',(0.,0.,1.));
#19728=DIRECTION('ref_axis',(1.,0.,0.));
#19729=DIRECTION('center_axis',(0.,0.,1.));
#19730=DIRECTION('ref_axis',(1.,0.,0.));
#19731=DIRECTION('center_axis',(0.,0.,1.));
#19732=DIRECTION('ref_axis',(1.,0.,0.));
#19733=DIRECTION('',(0.,0.,-1.));
#19734=DIRECTION('center_axis',(0.,0.,1.));
#19735=DIRECTION('ref_axis',(1.,0.,0.));
#19736=DIRECTION('center_axis',(0.,0.,1.));
#19737=DIRECTION('ref_axis',(1.,0.,0.));
#19738=DIRECTION('center_axis',(0.,0.,1.));
#19739=DIRECTION('ref_axis',(1.,0.,0.));
#19740=DIRECTION('center_axis',(0.,0.,1.));
#19741=DIRECTION('ref_axis',(1.,0.,0.));
#19742=DIRECTION('',(0.,0.,-1.));
#19743=DIRECTION('center_axis',(0.,0.,1.));
#19744=DIRECTION('ref_axis',(1.,0.,0.));
#19745=DIRECTION('center_axis',(0.,0.,1.));
#19746=DIRECTION('ref_axis',(1.,0.,0.));
#19747=DIRECTION('center_axis',(0.,0.,1.));
#19748=DIRECTION('ref_axis',(1.,0.,0.));
#19749=DIRECTION('',(0.,0.,-1.));
#19750=DIRECTION('center_axis',(0.,0.,1.));
#19751=DIRECTION('ref_axis',(1.,0.,0.));
#19752=DIRECTION('axis',(0.,0.,1.));
#19753=DIRECTION('refdir',(1.,0.,0.));
#19754=DIRECTION('center_axis',(0.,0.,1.));
#19755=DIRECTION('ref_axis',(1.,0.,0.));
#19756=DIRECTION('center_axis',(0.,0.,-1.));
#19757=DIRECTION('ref_axis',(1.,0.,0.));
#19758=DIRECTION('',(0.,0.,1.));
#19759=DIRECTION('center_axis',(0.,0.,-1.));
#19760=DIRECTION('ref_axis',(1.,0.,0.));
#19761=DIRECTION('center_axis',(0.,0.,1.));
#19762=DIRECTION('ref_axis',(1.,0.,0.));
#19763=DIRECTION('center_axis',(0.,0.,1.));
#19764=DIRECTION('ref_axis',(1.,0.,0.));
#19765=DIRECTION('',(0.,0.,-1.));
#19766=DIRECTION('center_axis',(0.,0.,1.));
#19767=DIRECTION('ref_axis',(1.,0.,0.));
#19768=DIRECTION('center_axis',(0.,0.,1.));
#19769=DIRECTION('ref_axis',(1.,0.,0.));
#19770=DIRECTION('center_axis',(0.,0.,1.));
#19771=DIRECTION('ref_axis',(1.,0.,0.));
#19772=DIRECTION('axis',(0.,0.,1.));
#19773=DIRECTION('refdir',(1.,0.,0.));
#19774=DIRECTION('center_axis',(-1.,0.,0.));
#19775=DIRECTION('ref_axis',(0.,1.,0.));
#19776=DIRECTION('',(0.,0.,1.));
#19777=DIRECTION('',(0.,-1.,0.));
#19778=DIRECTION('',(0.,0.,-1.));
#19779=DIRECTION('',(0.,1.,0.));
#19780=DIRECTION('center_axis',(1.,0.,0.));
#19781=DIRECTION('ref_axis',(0.,-1.,0.));
#19782=DIRECTION('',(0.,0.,-1.));
#19783=DIRECTION('',(0.,-1.,0.));
#19784=DIRECTION('',(0.,0.,1.));
#19785=DIRECTION('',(0.,1.,0.));
#19786=DIRECTION('center_axis',(0.,0.,1.));
#19787=DIRECTION('ref_axis',(1.,0.,0.));
#19788=DIRECTION('center_axis',(0.,0.,1.));
#19789=DIRECTION('ref_axis',(1.,0.,0.));
#19790=DIRECTION('center_axis',(0.,0.,-1.));
#19791=DIRECTION('ref_axis',(1.,0.,0.));
#19792=DIRECTION('center_axis',(0.,0.,1.));
#19793=DIRECTION('ref_axis',(6.12323399573677E-17,-1.,0.));
#19794=DIRECTION('center_axis',(0.,0.,-1.));
#19795=DIRECTION('ref_axis',(1.,0.,0.));
#19796=DIRECTION('center_axis',(0.,0.,1.));
#19797=DIRECTION('ref_axis',(6.12323399573677E-17,-1.,0.));
#19798=DIRECTION('center_axis',(0.,0.,1.));
#19799=DIRECTION('ref_axis',(1.,0.,0.));
#19800=DIRECTION('center_axis',(0.,0.,1.));
#19801=DIRECTION('ref_axis',(1.,0.,0.));
#19802=DIRECTION('axis',(0.,0.,1.));
#19803=DIRECTION('refdir',(1.,0.,0.));
#19804=DIRECTION('center_axis',(0.,0.,1.));
#19805=DIRECTION('ref_axis',(1.,0.,0.));
#19806=DIRECTION('center_axis',(0.,0.,-1.));
#19807=DIRECTION('ref_axis',(1.,0.,0.));
#19808=DIRECTION('',(0.,0.,1.));
#19809=DIRECTION('center_axis',(0.,0.,-1.));
#19810=DIRECTION('ref_axis',(1.,0.,0.));
#19811=DIRECTION('center_axis',(0.,0.,1.));
#19812=DIRECTION('ref_axis',(1.,0.,0.));
#19813=DIRECTION('center_axis',(0.,0.,1.));
#19814=DIRECTION('ref_axis',(1.,0.,0.));
#19815=DIRECTION('',(0.,0.,-1.));
#19816=DIRECTION('center_axis',(0.,0.,1.));
#19817=DIRECTION('ref_axis',(1.,0.,0.));
#19818=DIRECTION('center_axis',(0.,0.,1.));
#19819=DIRECTION('ref_axis',(1.,0.,0.));
#19820=DIRECTION('center_axis',(0.,0.,1.));
#19821=DIRECTION('ref_axis',(1.,0.,0.));
#19822=DIRECTION('axis',(0.,0.,1.));
#19823=DIRECTION('refdir',(1.,0.,0.));
#19824=DIRECTION('center_axis',(0.,0.,-1.));
#19825=DIRECTION('ref_axis',(1.,0.,0.));
#19826=DIRECTION('',(0.707106781186547,-8.65956056235493E-17,0.707106781186548));
#19827=DIRECTION('center_axis',(0.,0.,-1.));
#19828=DIRECTION('ref_axis',(1.,0.,0.));
#19829=DIRECTION('center_axis',(0.,0.,-1.));
#19830=DIRECTION('ref_axis',(1.,1.08690987399044E-13,0.));
#19831=DIRECTION('',(0.707106781186547,-8.65956056235493E-17,0.707106781186548));
#19832=DIRECTION('center_axis',(0.,0.,1.));
#19833=DIRECTION('ref_axis',(1.,0.,0.));
#19834=DIRECTION('center_axis',(0.,0.,-1.));
#19835=DIRECTION('ref_axis',(1.,1.08690987399044E-13,0.));
#19836=DIRECTION('center_axis',(0.,0.,1.));
#19837=DIRECTION('ref_axis',(1.,1.08690987399044E-13,0.));
#19838=DIRECTION('',(0.,0.,-1.));
#19839=DIRECTION('center_axis',(0.,0.,-1.));
#19840=DIRECTION('ref_axis',(1.,1.08690987399044E-13,0.));
#19841=DIRECTION('center_axis',(0.,0.,1.));
#19842=DIRECTION('ref_axis',(1.,1.08690987399044E-13,0.));
#19843=DIRECTION('',(0.,0.,-1.));
#19844=DIRECTION('center_axis',(0.,0.,1.));
#19845=DIRECTION('ref_axis',(1.,1.08690987399044E-13,0.));
#19846=DIRECTION('',(0.,0.,-1.));
#19847=DIRECTION('center_axis',(0.,0.,1.));
#19848=DIRECTION('ref_axis',(1.,1.08690987399044E-13,0.));
#19849=DIRECTION('',(0.,0.,-1.));
#19850=DIRECTION('center_axis',(0.,0.,1.));
#19851=DIRECTION('ref_axis',(1.,1.08690987399044E-13,0.));
#19852=DIRECTION('',(0.,0.,-1.));
#19853=DIRECTION('center_axis',(0.,0.,1.));
#19854=DIRECTION('ref_axis',(1.,1.08690987399044E-13,0.));
#19855=DIRECTION('',(0.,0.,-1.));
#19856=DIRECTION('center_axis',(0.,0.,1.));
#19857=DIRECTION('ref_axis',(1.,1.08690987399044E-13,0.));
#19858=DIRECTION('',(0.,0.,-1.));
#19859=DIRECTION('center_axis',(0.,0.,1.));
#19860=DIRECTION('ref_axis',(1.,1.08690987399044E-13,0.));
#19861=DIRECTION('',(0.,0.,-1.));
#19862=DIRECTION('center_axis',(0.,0.,1.));
#19863=DIRECTION('ref_axis',(1.,1.08690987399044E-13,0.));
#19864=DIRECTION('',(0.,0.,-1.));
#19865=DIRECTION('center_axis',(0.,0.,1.));
#19866=DIRECTION('ref_axis',(1.,1.08690987399044E-13,0.));
#19867=DIRECTION('',(0.,0.,-1.));
#19868=DIRECTION('center_axis',(0.,0.,1.));
#19869=DIRECTION('ref_axis',(1.,1.08690987399044E-13,0.));
#19870=DIRECTION('',(0.,0.,-1.));
#19871=DIRECTION('center_axis',(0.,0.,1.));
#19872=DIRECTION('ref_axis',(1.,1.08690987399044E-13,0.));
#19873=DIRECTION('',(0.,0.,-1.));
#19874=DIRECTION('center_axis',(0.,0.,1.));
#19875=DIRECTION('ref_axis',(1.,1.08690987399044E-13,0.));
#19876=DIRECTION('',(0.,0.,-1.));
#19877=DIRECTION('center_axis',(0.,0.,1.));
#19878=DIRECTION('ref_axis',(1.,1.08690987399044E-13,0.));
#19879=DIRECTION('',(0.,0.,-1.));
#19880=DIRECTION('center_axis',(0.,0.,1.));
#19881=DIRECTION('ref_axis',(1.,1.08690987399044E-13,0.));
#19882=DIRECTION('',(0.,0.,-1.));
#19883=DIRECTION('center_axis',(0.,0.,1.));
#19884=DIRECTION('ref_axis',(1.,1.08690987399044E-13,0.));
#19885=DIRECTION('',(0.,0.,-1.));
#19886=DIRECTION('center_axis',(0.,0.,1.));
#19887=DIRECTION('ref_axis',(1.,0.,0.));
#19888=DIRECTION('center_axis',(0.,0.,-1.));
#19889=DIRECTION('ref_axis',(1.,0.,0.));
#19890=DIRECTION('center_axis',(0.,0.,-1.));
#19891=DIRECTION('ref_axis',(1.,0.,0.));
#19892=DIRECTION('center_axis',(0.,0.,1.));
#19893=DIRECTION('ref_axis',(1.,1.08690987399044E-13,0.));
#19894=DIRECTION('center_axis',(0.,0.,-1.));
#19895=DIRECTION('ref_axis',(1.,0.,0.));
#19896=DIRECTION('center_axis',(-1.60246890531964E-16,-1.,0.));
#19897=DIRECTION('ref_axis',(1.,-1.60246890531964E-16,0.));
#19898=DIRECTION('',(1.,-1.60246890531964E-16,0.));
#19899=DIRECTION('',(0.,0.,1.));
#19900=DIRECTION('',(1.,-1.60246890531964E-16,0.));
#19901=DIRECTION('',(0.,0.,1.));
#19902=DIRECTION('center_axis',(-0.866025403784439,-0.5,0.));
#19903=DIRECTION('ref_axis',(0.5,-0.866025403784439,0.));
#19904=DIRECTION('',(0.5,-0.866025403784439,0.));
#19905=DIRECTION('',(0.,0.,1.));
#19906=DIRECTION('',(0.5,-0.866025403784439,0.));
#19907=DIRECTION('center_axis',(-0.866025403784439,0.5,0.));
#19908=DIRECTION('ref_axis',(-0.5,-0.866025403784439,0.));
#19909=DIRECTION('',(-0.5,-0.866025403784439,0.));
#19910=DIRECTION('',(0.,0.,1.));
#19911=DIRECTION('',(-0.5,-0.866025403784439,0.));
#19912=DIRECTION('center_axis',(1.60246890531964E-16,1.,0.));
#19913=DIRECTION('ref_axis',(-1.,1.60246890531964E-16,0.));
#19914=DIRECTION('',(-1.,1.60246890531964E-16,0.));
#19915=DIRECTION('',(0.,0.,1.));
#19916=DIRECTION('',(-1.,1.60246890531964E-16,0.));
#19917=DIRECTION('center_axis',(0.866025403784439,0.5,0.));
#19918=DIRECTION('ref_axis',(-0.5,0.866025403784439,0.));
#19919=DIRECTION('',(-0.5,0.866025403784439,0.));
#19920=DIRECTION('',(0.,0.,1.));
#19921=DIRECTION('',(-0.5,0.866025403784439,0.));
#19922=DIRECTION('center_axis',(0.866025403784439,-0.5,0.));
#19923=DIRECTION('ref_axis',(0.5,0.866025403784439,0.));
#19924=DIRECTION('',(0.5,0.866025403784439,0.));
#19925=DIRECTION('',(0.5,0.866025403784439,0.));
#19926=DIRECTION('center_axis',(0.,0.,1.));
#19927=DIRECTION('ref_axis',(1.,0.,0.));
#19928=DIRECTION('center_axis',(0.,0.,1.));
#19929=DIRECTION('ref_axis',(1.,0.,0.));
#19930=DIRECTION('center_axis',(0.,0.,1.));
#19931=DIRECTION('ref_axis',(1.,0.,0.));
#19932=DIRECTION('center_axis',(0.,0.,1.));
#19933=DIRECTION('ref_axis',(1.,0.,0.));
#19934=DIRECTION('',(0.,0.,-1.));
#19935=DIRECTION('center_axis',(0.,0.,1.));
#19936=DIRECTION('ref_axis',(1.,0.,0.));
#19937=DIRECTION('center_axis',(0.,0.,1.));
#19938=DIRECTION('ref_axis',(1.,0.,0.));
#19939=DIRECTION('center_axis',(0.,0.,1.));
#19940=DIRECTION('ref_axis',(1.,0.,0.));
#19941=DIRECTION('axis',(0.,0.,1.));
#19942=DIRECTION('refdir',(1.,0.,0.));
#19943=DIRECTION('center_axis',(0.,0.,-1.));
#19944=DIRECTION('ref_axis',(1.,0.,0.));
#19945=DIRECTION('',(0.707106781186547,-8.65956056235493E-17,0.707106781186548));
#19946=DIRECTION('center_axis',(0.,0.,-1.));
#19947=DIRECTION('ref_axis',(1.,0.,0.));
#19948=DIRECTION('center_axis',(0.,0.,-1.));
#19949=DIRECTION('ref_axis',(1.,-1.0233845463423E-13,0.));
#19950=DIRECTION('',(0.707106781186547,-8.65956056235493E-17,0.707106781186548));
#19951=DIRECTION('center_axis',(0.,0.,1.));
#19952=DIRECTION('ref_axis',(1.,0.,0.));
#19953=DIRECTION('center_axis',(0.,0.,-1.));
#19954=DIRECTION('ref_axis',(1.,-1.0233845463423E-13,0.));
#19955=DIRECTION('center_axis',(0.,0.,1.));
#19956=DIRECTION('ref_axis',(-0.922260805897494,-0.386568242235837,0.));
#19957=DIRECTION('',(0.,0.,-1.));
#19958=DIRECTION('center_axis',(0.,0.,-1.));
#19959=DIRECTION('ref_axis',(1.,-1.0233845463423E-13,0.));
#19960=DIRECTION('center_axis',(0.,0.,1.));
#19961=DIRECTION('ref_axis',(-0.922260805897494,-0.386568242235837,0.));
#19962=DIRECTION('',(0.,0.,-1.));
#19963=DIRECTION('center_axis',(0.,0.,1.));
#19964=DIRECTION('ref_axis',(-0.922260805897494,-0.386568242235837,0.));
#19965=DIRECTION('',(0.,0.,-1.));
#19966=DIRECTION('center_axis',(0.,0.,1.));
#19967=DIRECTION('ref_axis',(-0.922260805897494,-0.386568242235837,0.));
#19968=DIRECTION('',(0.,0.,-1.));
#19969=DIRECTION('center_axis',(0.,0.,1.));
#19970=DIRECTION('ref_axis',(-0.922260805897494,-0.386568242235837,0.));
#19971=DIRECTION('',(0.,0.,-1.));
#19972=DIRECTION('center_axis',(0.,0.,1.));
#19973=DIRECTION('ref_axis',(-0.922260805897494,-0.386568242235837,0.));
#19974=DIRECTION('',(0.,0.,-1.));
#19975=DIRECTION('center_axis',(0.,0.,1.));
#19976=DIRECTION('ref_axis',(-0.922260805897494,-0.386568242235837,0.));
#19977=DIRECTION('',(0.,0.,-1.));
#19978=DIRECTION('center_axis',(0.,0.,1.));
#19979=DIRECTION('ref_axis',(-0.922260805897494,-0.386568242235837,0.));
#19980=DIRECTION('',(0.,0.,-1.));
#19981=DIRECTION('center_axis',(0.,0.,1.));
#19982=DIRECTION('ref_axis',(-0.922260805897494,-0.386568242235837,0.));
#19983=DIRECTION('',(0.,0.,-1.));
#19984=DIRECTION('center_axis',(0.,0.,1.));
#19985=DIRECTION('ref_axis',(-0.922260805897494,-0.386568242235837,0.));
#19986=DIRECTION('',(0.,0.,-1.));
#19987=DIRECTION('center_axis',(0.,0.,1.));
#19988=DIRECTION('ref_axis',(-0.922260805897494,-0.386568242235837,0.));
#19989=DIRECTION('',(0.,0.,-1.));
#19990=DIRECTION('center_axis',(0.,0.,1.));
#19991=DIRECTION('ref_axis',(-0.922260805897494,-0.386568242235837,0.));
#19992=DIRECTION('',(0.,0.,-1.));
#19993=DIRECTION('center_axis',(0.,0.,1.));
#19994=DIRECTION('ref_axis',(-0.922260805897494,-0.386568242235837,0.));
#19995=DIRECTION('',(0.,0.,-1.));
#19996=DIRECTION('center_axis',(0.,0.,1.));
#19997=DIRECTION('ref_axis',(-0.922260805897494,-0.386568242235837,0.));
#19998=DIRECTION('',(0.,0.,-1.));
#19999=DIRECTION('center_axis',(0.,0.,1.));
#20000=DIRECTION('ref_axis',(-0.922260805897494,-0.386568242235837,0.));
#20001=DIRECTION('',(0.,0.,-1.));
#20002=DIRECTION('center_axis',(0.,0.,1.));
#20003=DIRECTION('ref_axis',(-0.922260805897494,-0.386568242235837,0.));
#20004=DIRECTION('',(0.,0.,-1.));
#20005=DIRECTION('center_axis',(0.,0.,1.));
#20006=DIRECTION('ref_axis',(-0.922260805897494,-0.386568242235837,0.));
#20007=DIRECTION('',(0.,0.,-1.));
#20008=DIRECTION('center_axis',(0.,0.,1.));
#20009=DIRECTION('ref_axis',(-0.922260805897494,-0.386568242235837,0.));
#20010=DIRECTION('',(0.,0.,-1.));
#20011=DIRECTION('center_axis',(0.,0.,1.));
#20012=DIRECTION('ref_axis',(-0.922260805897494,-0.386568242235837,0.));
#20013=DIRECTION('',(0.,0.,-1.));
#20014=DIRECTION('center_axis',(0.,0.,1.));
#20015=DIRECTION('ref_axis',(-0.922260805897494,-0.386568242235837,0.));
#20016=DIRECTION('',(0.,0.,-1.));
#20017=DIRECTION('center_axis',(0.,0.,1.));
#20018=DIRECTION('ref_axis',(-0.922260805897494,-0.386568242235837,0.));
#20019=DIRECTION('',(0.,0.,-1.));
#20020=DIRECTION('center_axis',(0.,0.,1.));
#20021=DIRECTION('ref_axis',(-0.922260805897494,-0.386568242235837,0.));
#20022=DIRECTION('',(0.,0.,-1.));
#20023=DIRECTION('center_axis',(0.,0.,1.));
#20024=DIRECTION('ref_axis',(-0.922260805897494,-0.386568242235837,0.));
#20025=DIRECTION('',(0.,0.,-1.));
#20026=DIRECTION('center_axis',(0.,0.,1.));
#20027=DIRECTION('ref_axis',(-0.922260805897494,-0.386568242235837,0.));
#20028=DIRECTION('',(0.,0.,-1.));
#20029=DIRECTION('center_axis',(0.,0.,1.));
#20030=DIRECTION('ref_axis',(-0.922260805897494,-0.386568242235837,0.));
#20031=DIRECTION('',(0.,0.,-1.));
#20032=DIRECTION('center_axis',(0.,0.,1.));
#20033=DIRECTION('ref_axis',(-0.922260805897494,-0.386568242235837,0.));
#20034=DIRECTION('',(0.,0.,-1.));
#20035=DIRECTION('center_axis',(0.,0.,1.));
#20036=DIRECTION('ref_axis',(-0.922260805897494,-0.386568242235837,0.));
#20037=DIRECTION('',(0.,0.,-1.));
#20038=DIRECTION('center_axis',(0.,0.,1.));
#20039=DIRECTION('ref_axis',(-0.922260805897494,-0.386568242235837,0.));
#20040=DIRECTION('',(0.,0.,-1.));
#20041=DIRECTION('center_axis',(0.,0.,1.));
#20042=DIRECTION('ref_axis',(1.,0.,0.));
#20043=DIRECTION('center_axis',(0.,0.,-1.));
#20044=DIRECTION('ref_axis',(1.,0.,0.));
#20045=DIRECTION('center_axis',(-0.00364373213059557,0.0569212501344872,
0.998372022093612));
#20046=DIRECTION('ref_axis',(-0.980992657570465,-0.193900834380623,0.00747477219278287));
#20047=DIRECTION('center_axis',(0.,0.,-1.));
#20048=DIRECTION('ref_axis',(1.,0.,0.));
#20049=DIRECTION('center_axis',(0.,0.,1.));
#20050=DIRECTION('ref_axis',(-0.922260805897494,-0.386568242235837,0.));
#20051=DIRECTION('center_axis',(0.,0.,-1.));
#20052=DIRECTION('ref_axis',(1.,0.,0.));
#20053=DIRECTION('center_axis',(-1.60246890531964E-16,-1.,0.));
#20054=DIRECTION('ref_axis',(1.,-1.60246890531964E-16,0.));
#20055=DIRECTION('',(1.,-1.60246890531964E-16,0.));
#20056=DIRECTION('',(0.,0.,1.));
#20057=DIRECTION('',(1.,-1.60246890531964E-16,0.));
#20058=DIRECTION('',(0.,0.,1.));
#20059=DIRECTION('center_axis',(-0.866025403784439,-0.5,0.));
#20060=DIRECTION('ref_axis',(0.5,-0.866025403784439,0.));
#20061=DIRECTION('',(0.5,-0.866025403784439,0.));
#20062=DIRECTION('',(0.,0.,1.));
#20063=DIRECTION('',(0.5,-0.866025403784439,0.));
#20064=DIRECTION('center_axis',(-0.866025403784439,0.5,0.));
#20065=DIRECTION('ref_axis',(-0.5,-0.866025403784439,0.));
#20066=DIRECTION('',(-0.5,-0.866025403784439,0.));
#20067=DIRECTION('',(0.,0.,1.));
#20068=DIRECTION('',(-0.5,-0.866025403784439,0.));
#20069=DIRECTION('center_axis',(1.60246890531964E-16,1.,0.));
#20070=DIRECTION('ref_axis',(-1.,1.60246890531964E-16,0.));
#20071=DIRECTION('',(-1.,1.60246890531964E-16,0.));
#20072=DIRECTION('',(0.,0.,1.));
#20073=DIRECTION('',(-1.,1.60246890531964E-16,0.));
#20074=DIRECTION('center_axis',(0.866025403784439,0.5,0.));
#20075=DIRECTION('ref_axis',(-0.5,0.866025403784439,0.));
#20076=DIRECTION('',(-0.5,0.866025403784439,0.));
#20077=DIRECTION('',(0.,0.,1.));
#20078=DIRECTION('',(-0.5,0.866025403784439,0.));
#20079=DIRECTION('center_axis',(0.866025403784439,-0.5,0.));
#20080=DIRECTION('ref_axis',(0.5,0.866025403784439,0.));
#20081=DIRECTION('',(0.5,0.866025403784439,0.));
#20082=DIRECTION('',(0.5,0.866025403784439,0.));
#20083=DIRECTION('center_axis',(0.,0.,1.));
#20084=DIRECTION('ref_axis',(1.,0.,0.));
#20085=DIRECTION('center_axis',(0.,0.,1.));
#20086=DIRECTION('ref_axis',(1.,0.,0.));
#20087=DIRECTION('center_axis',(0.,0.,1.));
#20088=DIRECTION('ref_axis',(1.,0.,0.));
#20089=DIRECTION('center_axis',(0.,0.,1.));
#20090=DIRECTION('ref_axis',(1.,0.,0.));
#20091=DIRECTION('',(0.,0.,-1.));
#20092=DIRECTION('center_axis',(0.,0.,1.));
#20093=DIRECTION('ref_axis',(1.,0.,0.));
#20094=DIRECTION('center_axis',(0.,0.,1.));
#20095=DIRECTION('ref_axis',(1.,0.,0.));
#20096=DIRECTION('center_axis',(0.,0.,1.));
#20097=DIRECTION('ref_axis',(1.,0.,0.));
#20098=DIRECTION('axis',(0.,0.,1.));
#20099=DIRECTION('refdir',(1.,0.,0.));
#20100=DIRECTION('center_axis',(0.,0.,1.));
#20101=DIRECTION('ref_axis',(1.,0.,0.));
#20102=DIRECTION('center_axis',(0.,0.,-1.));
#20103=DIRECTION('ref_axis',(1.,0.,0.));
#20104=DIRECTION('center_axis',(0.,0.,-1.));
#20105=DIRECTION('ref_axis',(1.,0.,0.));
#20106=DIRECTION('center_axis',(0.,0.,1.));
#20107=DIRECTION('ref_axis',(1.,1.29731060939901E-13,0.));
#20108=DIRECTION('center_axis',(0.,0.,-1.));
#20109=DIRECTION('ref_axis',(1.,1.29731060939901E-13,0.));
#20110=DIRECTION('center_axis',(0.,0.,-1.));
#20111=DIRECTION('ref_axis',(1.,1.29731060939901E-13,0.));
#20112=DIRECTION('center_axis',(0.,0.,-1.));
#20113=DIRECTION('ref_axis',(1.,0.,0.));
#20114=DIRECTION('',(0.707106781186548,-8.65956056235494E-17,0.707106781186547));
#20115=DIRECTION('center_axis',(0.,0.,1.));
#20116=DIRECTION('ref_axis',(1.,0.,0.));
#20117=DIRECTION('center_axis',(-1.60246890531964E-16,-1.,0.));
#20118=DIRECTION('ref_axis',(1.,-1.60246890531964E-16,0.));
#20119=DIRECTION('',(1.,-1.60246890531964E-16,0.));
#20120=DIRECTION('',(0.,0.,1.));
#20121=DIRECTION('',(1.,-1.60246890531964E-16,0.));
#20122=DIRECTION('',(0.,0.,1.));
#20123=DIRECTION('center_axis',(-0.866025403784439,-0.5,0.));
#20124=DIRECTION('ref_axis',(0.5,-0.866025403784439,0.));
#20125=DIRECTION('',(0.5,-0.866025403784439,0.));
#20126=DIRECTION('',(0.,0.,1.));
#20127=DIRECTION('',(0.5,-0.866025403784439,0.));
#20128=DIRECTION('center_axis',(-0.866025403784439,0.5,0.));
#20129=DIRECTION('ref_axis',(-0.5,-0.866025403784439,0.));
#20130=DIRECTION('',(-0.5,-0.866025403784439,0.));
#20131=DIRECTION('',(0.,0.,1.));
#20132=DIRECTION('',(-0.5,-0.866025403784439,0.));
#20133=DIRECTION('center_axis',(1.60246890531964E-16,1.,0.));
#20134=DIRECTION('ref_axis',(-1.,1.60246890531964E-16,0.));
#20135=DIRECTION('',(-1.,1.60246890531964E-16,0.));
#20136=DIRECTION('',(0.,0.,1.));
#20137=DIRECTION('',(-1.,1.60246890531964E-16,0.));
#20138=DIRECTION('center_axis',(0.866025403784439,0.5,0.));
#20139=DIRECTION('ref_axis',(-0.5,0.866025403784439,0.));
#20140=DIRECTION('',(-0.5,0.866025403784439,0.));
#20141=DIRECTION('',(0.,0.,1.));
#20142=DIRECTION('',(-0.5,0.866025403784439,0.));
#20143=DIRECTION('center_axis',(0.866025403784439,-0.5,0.));
#20144=DIRECTION('ref_axis',(0.5,0.866025403784439,0.));
#20145=DIRECTION('',(0.5,0.866025403784439,0.));
#20146=DIRECTION('',(0.5,0.866025403784439,0.));
#20147=DIRECTION('center_axis',(0.,0.,1.));
#20148=DIRECTION('ref_axis',(1.,0.,0.));
#20149=DIRECTION('center_axis',(0.,0.,1.));
#20150=DIRECTION('ref_axis',(1.,0.,0.));
#20151=DIRECTION('center_axis',(0.,0.,1.));
#20152=DIRECTION('ref_axis',(1.,0.,0.));
#20153=DIRECTION('center_axis',(0.,0.,1.));
#20154=DIRECTION('ref_axis',(1.,0.,0.));
#20155=DIRECTION('',(0.,0.,-1.));
#20156=DIRECTION('center_axis',(0.,0.,1.));
#20157=DIRECTION('ref_axis',(1.,0.,0.));
#20158=DIRECTION('center_axis',(0.,0.,1.));
#20159=DIRECTION('ref_axis',(1.,0.,0.));
#20160=DIRECTION('center_axis',(0.,0.,1.));
#20161=DIRECTION('ref_axis',(1.,0.,0.));
#20162=DIRECTION('',(0.,0.,1.));
#20163=DIRECTION('',(1.,0.,0.));
#20164=DIRECTION('',(0.,0.,1.));
#20165=DIRECTION('',(1.,0.,0.));
#20166=DIRECTION('',(1.,0.,0.));
#20167=DIRECTION('',(0.,1.,0.));
#20168=DIRECTION('',(1.,0.,0.));
#20169=DIRECTION('',(0.,1.,0.));
#20170=DIRECTION('',(1.,0.,0.));
#20171=DIRECTION('',(0.,1.,0.));
#20172=DIRECTION('',(0.,0.,1.));
#20173=DIRECTION('',(1.,0.,0.));
#20174=DIRECTION('',(1.,0.,0.));
#20175=DIRECTION('',(0.,1.,0.));
#20176=DIRECTION('',(1.,0.,0.));
#20177=DIRECTION('',(0.,1.,0.));
#20178=DIRECTION('',(1.,0.,0.));
#20179=DIRECTION('',(0.,1.,0.));
#20180=DIRECTION('',(1.,0.,0.));
#20181=DIRECTION('',(0.,-0.984807753012208,0.17364817766693));
#20182=DIRECTION('',(1.,0.,0.));
#20183=DIRECTION('',(0.,-0.984807753012208,0.17364817766693));
#20184=DIRECTION('',(0.,-0.984807753012208,0.17364817766693));
#20185=DIRECTION('',(0.,-0.17364817766693,-0.984807753012208));
#20186=DIRECTION('',(0.,-0.984807753012208,0.17364817766693));
#20187=DIRECTION('',(0.,-0.17364817766693,-0.984807753012208));
#20188=DIRECTION('',(0.,-0.984807753012208,0.17364817766693));
#20189=DIRECTION('',(0.,-0.17364817766693,-0.984807753012208));
#20190=DIRECTION('',(0.,-1.22464679914735E-16,-1.));
#20191=DIRECTION('',(1.,0.,0.));
#20192=DIRECTION('',(1.,0.,0.));
#20193=DIRECTION('',(0.,-0.342020143325669,0.939692620785908));
#20194=DIRECTION('',(8.36182424550692E-34,-1.22464679914735E-16,-1.));
#20195=DIRECTION('',(-0.766044443118978,-0.64278760968654,7.87187788734197E-17));
#20196=DIRECTION('',(1.,0.,0.));
#20197=DIRECTION('',(0.,1.,0.));
#20198=DIRECTION('',(0.,-1.22464679914735E-16,-1.));
#20199=DIRECTION('',(1.,0.,0.));
#20200=DIRECTION('',(0.,-1.22464679914735E-16,-1.));
#20201=DIRECTION('',(1.,0.,0.));
#20202=DIRECTION('',(0.,-1.22464679914735E-16,-1.));
#20203=DIRECTION('',(1.,0.,0.));
#20204=DIRECTION('',(1.,0.,0.));
#20205=DIRECTION('',(0.,-0.342020143325669,0.939692620785908));
#20206=DIRECTION('',(1.,0.,0.));
#20207=DIRECTION('',(0.,-0.342020143325669,0.939692620785908));
#20208=DIRECTION('',(1.,0.,0.));
#20209=DIRECTION('',(0.,-0.342020143325669,0.939692620785908));
#20210=DIRECTION('',(8.36182424550692E-34,-1.22464679914735E-16,-1.));
#20211=DIRECTION('',(-0.766044443118978,-0.64278760968654,7.87187788734197E-17));
#20212=CARTESIAN_POINT('',(0.,0.,0.));
#20213=CARTESIAN_POINT('',(0.,0.,0.));
#20214=CARTESIAN_POINT('Origin',(130.,-35.,32.7603849714045));
#20215=CARTESIAN_POINT('',(132.487160670875,-31.7594357285724,18.0469660640533));
#20216=CARTESIAN_POINT('',(132.487160670875,-31.7594357285724,17.9425407188119));
#20217=CARTESIAN_POINT('',(132.487160670875,-31.7594357285724,32.7603849714045));
#20218=CARTESIAN_POINT('',(125.917570547331,-35.0058571788241,17.1353849828742));
#20219=CARTESIAN_POINT('Ctrl Pts',(132.487160670875,-31.7594357285724,17.9425407188119));
#20220=CARTESIAN_POINT('Ctrl Pts',(132.581704114026,-31.8319986262038,17.9367376621138));
#20221=CARTESIAN_POINT('Ctrl Pts',(132.673155474161,-31.9087684968269,17.9309346054157));
#20222=CARTESIAN_POINT('Ctrl Pts',(132.761122894562,-31.9894476651075,17.9251315487176));
#20223=CARTESIAN_POINT('Ctrl Pts',(132.849041174532,-32.0700817643262,17.9193317337277));
#20224=CARTESIAN_POINT('Ctrl Pts',(132.933479084742,-32.1546205419903,17.9135319187378));
#20225=CARTESIAN_POINT('Ctrl Pts',(133.014078024373,-32.2427262263259,17.907732103748));
#20226=CARTESIAN_POINT('Ctrl Pts',(133.094654120592,-32.3308069396815,17.901933932546));
#20227=CARTESIAN_POINT('Ctrl Pts',(133.171393133673,-32.4224522480155,17.8961357613441));
#20228=CARTESIAN_POINT('Ctrl Pts',(133.243973935598,-32.5172881550293,17.8903375901422));
#20229=CARTESIAN_POINT('Ctrl Pts',(133.316551380068,-32.6121196751058,17.8845396871532));
#20230=CARTESIAN_POINT('Ctrl Pts',(133.384970747326,-32.7101411753726,17.8787417841642));
#20231=CARTESIAN_POINT('Ctrl Pts',(133.448952172999,-32.8109468009291,17.8729438811751));
#20232=CARTESIAN_POINT('Ctrl Pts',(133.512945812966,-32.9117716706553,17.8671448713448));
#20233=CARTESIAN_POINT('Ctrl Pts',(133.572499607407,-33.0153813771399,17.8613458615145));
#20234=CARTESIAN_POINT('Ctrl Pts',(133.627378224929,-33.1213429761359,17.8555468516842));
#20235=CARTESIAN_POINT('Ctrl Pts',(133.682314579367,-33.2274160556359,17.8497417408083));
#20236=CARTESIAN_POINT('Ctrl Pts',(133.732565744311,-33.3358456058072,17.8439366299325));
#20237=CARTESIAN_POINT('Ctrl Pts',(133.777943289161,-33.4461758452515,17.8381315190567));
#20238=CARTESIAN_POINT('Ctrl Pts',(133.823345287127,-33.5565655396092,17.8323232799146));
#20239=CARTESIAN_POINT('Ctrl Pts',(133.863868294095,-33.6688575789527,17.8265150407725));
#20240=CARTESIAN_POINT('Ctrl Pts',(133.899373395709,-33.7825797271113,17.8207068016304));
#20241=CARTESIAN_POINT('Ctrl Pts',(133.934935743661,-33.896485234177,17.8148891976249));
#20242=CARTESIAN_POINT('Ctrl Pts',(133.965463916952,-34.0118250612506,17.8090715936195));
#20243=CARTESIAN_POINT('Ctrl Pts',(133.990869754237,-34.1281149131264,17.803253989614));
#20244=CARTESIAN_POINT('Ctrl Pts',(134.012612161228,-34.2276361869148,17.7982752631673));
#20245=CARTESIAN_POINT('Ctrl Pts',(134.030603812871,-34.3278529548629,17.7932965367205));
#20246=CARTESIAN_POINT('Ctrl Pts',(134.044819691244,-34.4284593931121,17.7883178102738));
#20247=CARTESIAN_POINT('Ctrl Pts',(134.06147525078,-34.546331569412,17.7824846515646));
#20248=CARTESIAN_POINT('Ctrl Pts',(134.073000536758,-34.6651195996746,17.7766514928553));
#20249=CARTESIAN_POINT('Ctrl Pts',(134.079303348713,-34.7843401076304,17.7708183341461));
#20250=CARTESIAN_POINT('Ctrl Pts',(134.085598203868,-34.903410109157,17.7649925393368));
#20251=CARTESIAN_POINT('Ctrl Pts',(134.086683677878,-35.0229110995942,17.7591667445275));
#20252=CARTESIAN_POINT('Ctrl Pts',(134.082518952074,-35.1423516981127,17.7533409497181));
#20253=CARTESIAN_POINT('Ctrl Pts',(134.078358408253,-35.2616723611382,17.7475210048424));
#20254=CARTESIAN_POINT('Ctrl Pts',(134.068958167338,-35.3809323485755,17.7417010599667));
#20255=CARTESIAN_POINT('Ctrl Pts',(134.05432940372,-35.4996379550549,17.735881115091));
#20256=CARTESIAN_POINT('Ctrl Pts',(134.039180744297,-35.6225622739632,17.7298543335333));
#20257=CARTESIAN_POINT('Ctrl Pts',(134.018424994074,-35.7448916310486,17.7238275519756));
#20258=CARTESIAN_POINT('Ctrl Pts',(133.992133470621,-35.8660804539682,17.7178007704178));
#20259=CARTESIAN_POINT('Ctrl Pts',(133.966773358858,-35.9829760039448,17.7119874954985));
#20260=CARTESIAN_POINT('Ctrl Pts',(133.936263133592,-36.0988100265722,17.7061742205792));
#20261=CARTESIAN_POINT('Ctrl Pts',(133.900719114567,-36.2131015576818,17.7003609456598));
#20262=CARTESIAN_POINT('Ctrl Pts',(133.86518073122,-36.3273749673099,17.6945485924637));
#20263=CARTESIAN_POINT('Ctrl Pts',(133.824610262327,-36.4401059834592,17.6887362392676));
#20264=CARTESIAN_POINT('Ctrl Pts',(133.779174025344,-36.5508283870779,17.6829238860714));
#20265=CARTESIAN_POINT('Ctrl Pts',(133.733734366207,-36.6615591300547,17.6771110951021));
#20266=CARTESIAN_POINT('Ctrl Pts',(133.683428364855,-36.7702805833146,17.6712983041329));
#20267=CARTESIAN_POINT('Ctrl Pts',(133.628470409577,-36.8765466918841,17.6654855131636));
#20268=CARTESIAN_POINT('Ctrl Pts',(133.573495461997,-36.9828456565877,17.659670924953));
#20269=CARTESIAN_POINT('Ctrl Pts',(133.513865886678,-37.0866874055096,17.6538563367424));
#20270=CARTESIAN_POINT('Ctrl Pts',(133.449841614988,-37.1876512134011,17.6480417485318));
#20271=CARTESIAN_POINT('Ctrl Pts',(133.385748439847,-37.2887236793802,17.6422209026132));
#20272=CARTESIAN_POINT('Ctrl Pts',(133.317251345423,-37.3869116779491,17.6364000566945));
#20273=CARTESIAN_POINT('Ctrl Pts',(133.244653204869,-37.4818240429435,17.6305792107758));
#20274=CARTESIAN_POINT('Ctrl Pts',(133.172008572249,-37.5767971900996,17.6247546371701));
#20275=CARTESIAN_POINT('Ctrl Pts',(133.095257923063,-37.6684902141337,17.6189300635644));
#20276=CARTESIAN_POINT('Ctrl Pts',(133.014742893228,-37.7565468049227,17.6131054899586));
#20277=CARTESIAN_POINT('Ctrl Pts',(132.934115448857,-37.8447263397244,17.6072727841229));
#20278=CARTESIAN_POINT('Ctrl Pts',(132.849713419676,-37.9292590201806,17.6014400782871));
#20279=CARTESIAN_POINT('Ctrl Pts',(132.761913655608,-38.0098268985053,17.5956073724513));
#20280=CARTESIAN_POINT('Ctrl Pts',(132.739991385184,-38.0299434766635,17.5941510342027));
#20281=CARTESIAN_POINT('Ctrl Pts',(132.717857442463,-38.049813083404,17.592694695954));
#20282=CARTESIAN_POINT('Ctrl Pts',(132.695517984647,-38.0694311841847,17.5912383577053));
#20283=CARTESIAN_POINT('Ctrl Pts',(132.606178986837,-38.1478870481142,17.585414232488));
#20284=CARTESIAN_POINT('Ctrl Pts',(132.513269708122,-38.2225640338864,17.5795901072706));
#20285=CARTESIAN_POINT('Ctrl Pts',(132.417143086002,-38.2931207542073,17.5737659820533));
#20286=CARTESIAN_POINT('Ctrl Pts',(132.321136103841,-38.363589659073,17.5679491055885));
#20287=CARTESIAN_POINT('Ctrl Pts',(132.221920069128,-38.4299482589507,17.5621322291238));
#20288=CARTESIAN_POINT('Ctrl Pts',(132.119882780823,-38.4918937549089,17.556315352659));
#20289=CARTESIAN_POINT('Ctrl Pts',(132.017945927415,-38.5537782781614,17.5505042017226));
#20290=CARTESIAN_POINT('Ctrl Pts',(131.91319369184,-38.6112581284909,17.5446930507863));
#20291=CARTESIAN_POINT('Ctrl Pts',(131.806044305422,-38.6640727294711,17.5388818998499));
#20292=CARTESIAN_POINT('Ctrl Pts',(131.694857351711,-38.7188774725572,17.5328517750702));
#20293=CARTESIAN_POINT('Ctrl Pts',(131.581089398034,-38.7686581968064,17.5268216502905));
#20294=CARTESIAN_POINT('Ctrl Pts',(131.465237969362,-38.8131748836292,17.5207915255108));
#20295=CARTESIAN_POINT('Ctrl Pts',(131.353714643256,-38.8560284680744,17.5149866806334));
#20296=CARTESIAN_POINT('Ctrl Pts',(131.240261138487,-38.8940041214257,17.509181835756));
#20297=CARTESIAN_POINT('Ctrl Pts',(131.125342649476,-38.9269363276312,17.5033769908786));
#20298=CARTESIAN_POINT('Ctrl Pts',(131.010439464464,-38.9598641481678,17.4975729190477));
#20299=CARTESIAN_POINT('Ctrl Pts',(130.894072075446,-38.987749744817,17.4917688472168));
#20300=CARTESIAN_POINT('Ctrl Pts',(130.776720674511,-39.0104775269021,17.485964775386));
#20301=CARTESIAN_POINT('Ctrl Pts',(130.65935724065,-39.0332076394386,17.4801601084197));
#20302=CARTESIAN_POINT('Ctrl Pts',(130.541009994955,-39.0507788081581,17.4743554414534));
#20303=CARTESIAN_POINT('Ctrl Pts',(130.422168519274,-39.0631267198223,17.4685507744871));
#20304=CARTESIAN_POINT('Ctrl Pts',(130.303286845885,-39.0754788081238,17.4627441441129));
#20305=CARTESIAN_POINT('Ctrl Pts',(130.18391101576,-39.0826040834041,17.4569375137386));
#20306=CARTESIAN_POINT('Ctrl Pts',(130.06453427578,-39.0844902163244,17.4511308833643));
#20307=CARTESIAN_POINT('Ctrl Pts',(129.945023028346,-39.0863784744404,17.4453177103833));
#20308=CARTESIAN_POINT('Ctrl Pts',(129.825511277327,-39.083015800483,17.4395045374023));
#20309=CARTESIAN_POINT('Ctrl Pts',(129.70649098094,-39.0744419809013,17.4336913644213));
#20310=CARTESIAN_POINT('Ctrl Pts',(129.587391143467,-39.0658624314486,17.4278743065054));
#20311=CARTESIAN_POINT('Ctrl Pts',(129.468783819143,-39.0520648478111,17.4220572485895));
#20312=CARTESIAN_POINT('Ctrl Pts',(129.351152907099,-39.0331405195001,17.4162401906737));
#20313=CARTESIAN_POINT('Ctrl Pts',(129.233351764959,-39.0141888047636,17.4104147145767));
#20314=CARTESIAN_POINT('Ctrl Pts',(129.11653025366,-38.9900956192539,17.4045892384796));
#20315=CARTESIAN_POINT('Ctrl Pts',(129.001159350494,-38.9610026958958,17.3987637623826));
#20316=CARTESIAN_POINT('Ctrl Pts',(128.970760316404,-38.9533370129145,17.3972288099674));
#20317=CARTESIAN_POINT('Ctrl Pts',(128.940461894974,-38.9453244773613,17.3956938575521));
#20318=CARTESIAN_POINT('Ctrl Pts',(128.910272476765,-38.9369682402966,17.3941589051369));
#20319=CARTESIAN_POINT('Ctrl Pts',(128.7966252111,-38.9055114070744,17.3883806174033));
#20320=CARTESIAN_POINT('Ctrl Pts',(128.684141526411,-38.8690742365292,17.3826023296697));
#20321=CARTESIAN_POINT('Ctrl Pts',(128.573294774159,-38.8277587696401,17.3768240419362));
#20322=CARTESIAN_POINT('Ctrl Pts',(128.462589215034,-38.7864959291011,17.3710531144048));
#20323=CARTESIAN_POINT('Ctrl Pts',(128.353516828246,-38.7403672904179,17.3652821868735));
#20324=CARTESIAN_POINT('Ctrl Pts',(128.246538336773,-38.6895253347269,17.3595112593422));
#20325=CARTESIAN_POINT('Ctrl Pts',(128.139667079847,-38.6387343426837,17.3537461165513));
#20326=CARTESIAN_POINT('Ctrl Pts',(128.03488591716,-38.583239606427,17.3479809737605));
#20327=CARTESIAN_POINT('Ctrl Pts',(127.932637365784,-38.5232423616104,17.3422158309696));
#20328=CARTESIAN_POINT('Ctrl Pts',(127.825383702245,-38.4603082249189,17.3361684818696));
#20329=CARTESIAN_POINT('Ctrl Pts',(127.72091732099,-38.3924197627085,17.3301211327695));
#20330=CARTESIAN_POINT('Ctrl Pts',(127.619722083475,-38.3198647623211,17.3240737836695));
#20331=CARTESIAN_POINT('Ctrl Pts',(127.523352525227,-38.2507696793152,17.3183148134289));
#20332=CARTESIAN_POINT('Ctrl Pts',(127.429949706546,-38.1774431219199,17.3125558431884));
#20333=CARTESIAN_POINT('Ctrl Pts',(127.339902590464,-38.1001785064379,17.3067968729478));
#20334=CARTESIAN_POINT('Ctrl Pts',(127.249865669562,-38.0229226388944,17.3010385547408));
#20335=CARTESIAN_POINT('Ctrl Pts',(127.163184011491,-37.941729869919,17.2952802365337));
#20336=CARTESIAN_POINT('Ctrl Pts',(127.080213109896,-37.8569335862734,17.2895219183267));
#20337=CARTESIAN_POINT('Ctrl Pts',(126.997231227526,-37.7721260802728,17.2837628380356));
#20338=CARTESIAN_POINT('Ctrl Pts',(126.917961368612,-37.6837144084915,17.2780037577445));
#20339=CARTESIAN_POINT('Ctrl Pts',(126.842721276515,-37.5920679123491,17.2722446774535));
#20340=CARTESIAN_POINT('Ctrl Pts',(126.767452749201,-37.5003867805764,17.2664834206539));
#20341=CARTESIAN_POINT('Ctrl Pts',(126.696217280093,-37.4054687147629,17.2607221638544));
#20342=CARTESIAN_POINT('Ctrl Pts',(126.629291074734,-37.3077145276516,17.2549609070549));
#20343=CARTESIAN_POINT('Ctrl Pts',(126.562282534711,-37.2098400803499,17.249192562581));
#20344=CARTESIAN_POINT('Ctrl Pts',(126.499594073982,-37.1091228910951,17.2434242181072));
#20345=CARTESIAN_POINT('Ctrl Pts',(126.441457524535,-37.0059911391414,17.2376558736334));
#20346=CARTESIAN_POINT('Ctrl Pts',(126.383279228692,-36.9027853308665,17.2318833870562));
#20347=CARTESIAN_POINT('Ctrl Pts',(126.329659537295,-36.7971618781968,17.2261109004791));
#20348=CARTESIAN_POINT('Ctrl Pts',(126.280782651279,-36.6895701562747,17.220338413902));
#20349=CARTESIAN_POINT('Ctrl Pts',(126.231828296463,-36.5818079038151,17.2145567780592));
#20350=CARTESIAN_POINT('Ctrl Pts',(126.18763190295,-36.4720715400648,17.2087751422165));
#20351=CARTESIAN_POINT('Ctrl Pts',(126.148328293113,-36.3608269773817,17.2029935063738));
#20352=CARTESIAN_POINT('Ctrl Pts',(126.134927030354,-36.3228961709946,17.2010221551053));
#20353=CARTESIAN_POINT('Ctrl Pts',(126.122094161038,-36.2847901185301,17.1990508038369));
#20354=CARTESIAN_POINT('Ctrl Pts',(126.10983366812,-36.2465275409332,17.1970794525685));
#20355=CARTESIAN_POINT('Ctrl Pts',(126.063947737475,-36.103326611438,17.1897015038852));
#20356=CARTESIAN_POINT('Ctrl Pts',(126.02595987326,-35.9575499236023,17.1823235552019));
#20357=CARTESIAN_POINT('Ctrl Pts',(125.996104768623,-35.8099678858821,17.1749456065186));
#20358=CARTESIAN_POINT('Ctrl Pts',(125.966727677199,-35.6647487996489,17.1676857869456));
#20359=CARTESIAN_POINT('Ctrl Pts',(125.945224957893,-35.5177815783573,17.1604259673726));
#20360=CARTESIAN_POINT('Ctrl Pts',(125.931774609395,-35.369820458114,17.1531661477996));
#20361=CARTESIAN_POINT('Ctrl Pts',(125.920793500128,-35.2490223071195,17.1472390989943));
#20362=CARTESIAN_POINT('Ctrl Pts',(125.915178823828,-35.1275620126132,17.141312050189));
#20363=CARTESIAN_POINT('Ctrl Pts',(125.915004204916,-35.0058612407387,17.1353850013836));
#20364=CARTESIAN_POINT('',(126.824949217806,-32.429732011932,17.));
#20365=CARTESIAN_POINT('Ctrl Pts',(125.919160822134,-35.0058546617942,17.1353849714045));
#20366=CARTESIAN_POINT('Ctrl Pts',(125.92665513971,-34.0801598293983,17.090256647603));
#20367=CARTESIAN_POINT('Ctrl Pts',(126.2419104066,-33.1499595688096,17.0451283238015));
#20368=CARTESIAN_POINT('Ctrl Pts',(126.824949217806,-32.429732011932,17.));
#20369=CARTESIAN_POINT('',(128.537425967084,-31.1858025486036,17.0000001263181));
#20370=CARTESIAN_POINT('Origin',(130.,-35.,17.));
#20371=CARTESIAN_POINT('',(125.915001286748,-34.9967576658375,17.239615028553));
#20372=CARTESIAN_POINT('Ctrl Pts',(125.915001286748,-34.9967576658375,17.239615028553));
#20373=CARTESIAN_POINT('Ctrl Pts',(125.915121830798,-34.84488488998,17.2322214958407));
#20374=CARTESIAN_POINT('Ctrl Pts',(125.923715533729,-34.6933711864996,17.2248279631283));
#20375=CARTESIAN_POINT('Ctrl Pts',(125.940640899099,-34.5430222216247,17.217434430416));
#20376=CARTESIAN_POINT('Ctrl Pts',(125.957898968693,-34.3897178265603,17.2098955620188));
#20377=CARTESIAN_POINT('Ctrl Pts',(125.983819475205,-34.2376241677412,17.2023566936216));
#20378=CARTESIAN_POINT('Ctrl Pts',(126.018203886763,-34.0875720781268,17.1948178252245));
#20379=CARTESIAN_POINT('Ctrl Pts',(126.025778474723,-34.0545169028373,17.1931570778334));
#20380=CARTESIAN_POINT('Ctrl Pts',(126.033763617093,-34.0215607216557,17.1914963304423));
#20381=CARTESIAN_POINT('Ctrl Pts',(126.042156880036,-33.9887122873517,17.1898355830512));
#20382=CARTESIAN_POINT('Ctrl Pts',(126.071413140095,-33.8742130344265,17.1840467428947));
#20383=CARTESIAN_POINT('Ctrl Pts',(126.105691644772,-33.7607909591982,17.1782579027383));
#20384=CARTESIAN_POINT('Ctrl Pts',(126.144897526267,-33.6489226828134,17.1724690625818));
#20385=CARTESIAN_POINT('Ctrl Pts',(126.184054424549,-33.5371941728955,17.1666874549112));
#20386=CARTESIAN_POINT('Ctrl Pts',(126.228126322497,-33.4270159884914,17.1609058472407));
#20387=CARTESIAN_POINT('Ctrl Pts',(126.27696771855,-33.3188528823207,17.1551242395702));
#20388=CARTESIAN_POINT('Ctrl Pts',(126.325761225946,-33.2107958293414,17.1493483007267));
#20389=CARTESIAN_POINT('Ctrl Pts',(126.379314761018,-33.1047502998445,17.1435723618833));
#20390=CARTESIAN_POINT('Ctrl Pts',(126.437433784762,-33.0011635979796,17.1377964230398));
#20391=CARTESIAN_POINT('Ctrl Pts',(126.495513134357,-32.8976476081448,17.1320244270612));
#20392=CARTESIAN_POINT('Ctrl Pts',(126.558151571977,-32.7965874670979,17.1262524310825));
#20393=CARTESIAN_POINT('Ctrl Pts',(126.625107719851,-32.6984077039163,17.1204804351039));
#20394=CARTESIAN_POINT('Ctrl Pts',(126.692039837253,-32.600263177322,17.1147105106869));
#20395=CARTESIAN_POINT('Ctrl Pts',(126.763286351737,-32.5049973150308,17.10894058627));
#20396=CARTESIAN_POINT('Ctrl Pts',(126.838561805029,-32.4130068536275,17.1031706618531));
#20397=CARTESIAN_POINT('Ctrl Pts',(126.913828561771,-32.3210270198548,17.0974014040338));
#20398=CARTESIAN_POINT('Ctrl Pts',(126.993123069758,-32.2323221546499,17.0916321462146));
#20399=CARTESIAN_POINT('Ctrl Pts',(127.076119165966,-32.1472564313688,17.0858628883953));
#20400=CARTESIAN_POINT('Ctrl Pts',(127.159125872678,-32.062179832995,17.0800928930144));
#20401=CARTESIAN_POINT('Ctrl Pts',(127.245834819185,-31.980743597332,17.0743228976335));
#20402=CARTESIAN_POINT('Ctrl Pts',(127.335883040552,-31.9032749837315,17.0685529022526));
#20403=CARTESIAN_POINT('Ctrl Pts',(127.426020987657,-31.8257291789507,17.0627771575401));
#20404=CARTESIAN_POINT('Ctrl Pts',(127.519504541578,-31.7521591633589,17.0570014128275));
#20405=CARTESIAN_POINT('Ctrl Pts',(127.615937561779,-31.6828519341666,17.0512256681149));
#20406=CARTESIAN_POINT('Ctrl Pts',(127.712418239099,-31.6135104533982,17.045447069034));
#20407=CARTESIAN_POINT('Ctrl Pts',(127.811850939971,-31.5484361819415,17.0396684699532));
#20408=CARTESIAN_POINT('Ctrl Pts',(127.913811980347,-31.4878717923949,17.0338898708723));
#20409=CARTESIAN_POINT('Ctrl Pts',(128.01593821576,-31.4272092777552,17.0281019094322));
#20410=CARTESIAN_POINT('Ctrl Pts',(128.120600610571,-31.3710714403544,17.022313947992));
#20411=CARTESIAN_POINT('Ctrl Pts',(128.227351924597,-31.3196543911246,17.0165259865519));
#20412=CARTESIAN_POINT('Ctrl Pts',(128.328951155668,-31.2707188561064,17.011017366474));
#20413=CARTESIAN_POINT('Ctrl Pts',(128.432442089675,-31.2260591674412,17.005508746396));
#20414=CARTESIAN_POINT('Ctrl Pts',(128.537425967084,-31.1858025486036,17.0000001263181));
#20415=CARTESIAN_POINT('Ctrl Pts',(132.487160670875,-31.7594357285724,18.0469660640533));
#20416=CARTESIAN_POINT('Ctrl Pts',(132.581995825681,-31.8322225173823,18.0411567048122));
#20417=CARTESIAN_POINT('Ctrl Pts',(132.673587188726,-31.9091404736677,18.035347345571));
#20418=CARTESIAN_POINT('Ctrl Pts',(132.761569405332,-31.9898572426657,18.0295379863299));
#20419=CARTESIAN_POINT('Ctrl Pts',(132.849596841011,-32.0706154966078,18.0237256413283));
#20420=CARTESIAN_POINT('Ctrl Pts',(132.934011145747,-32.1551761643168,18.0179132963266));
#20421=CARTESIAN_POINT('Ctrl Pts',(133.014484707895,-32.2431708529785,18.012100951325));
#20422=CARTESIAN_POINT('Ctrl Pts',(133.095089062964,-32.3313085585774,18.0062791595738));
#20423=CARTESIAN_POINT('Ctrl Pts',(133.171739614314,-32.4228911245167,18.0004573678227));
#20424=CARTESIAN_POINT('Ctrl Pts',(133.244149453117,-32.5175175074448,17.9946355760715));
#20425=CARTESIAN_POINT('Ctrl Pts',(133.31248306625,-32.6068170108013,17.989141515156));
#20426=CARTESIAN_POINT('Ctrl Pts',(133.377040197403,-32.6988267736018,17.9836474542405));
#20427=CARTESIAN_POINT('Ctrl Pts',(133.437616796849,-32.7931887806115,17.978153393325));
#20428=CARTESIAN_POINT('Ctrl Pts',(133.501837123684,-32.8932267323347,17.9723288605703));
#20429=CARTESIAN_POINT('Ctrl Pts',(133.561790445962,-32.9962314200498,17.9665043278156));
#20430=CARTESIAN_POINT('Ctrl Pts',(133.617191501953,-33.1018033194102,17.9606797950608));
#20431=CARTESIAN_POINT('Ctrl Pts',(133.672522646919,-33.2072419967683,17.9548626123294));
#20432=CARTESIAN_POINT('Ctrl Pts',(133.723312763425,-33.3152410840024,17.9490454295979));
#20433=CARTESIAN_POINT('Ctrl Pts',(133.769319907765,-33.4253722875156,17.9432282468664));
#20434=CARTESIAN_POINT('Ctrl Pts',(133.815280976368,-33.535393195628,17.9374168899907));
#20435=CARTESIAN_POINT('Ctrl Pts',(133.856468445744,-33.6475415975982,17.9316055331149));
#20436=CARTESIAN_POINT('Ctrl Pts',(133.892686630217,-33.7613653488906,17.9257941762391));
#20437=CARTESIAN_POINT('Ctrl Pts',(133.93026752783,-33.8794717312346,17.9197641664274));
#20438=CARTESIAN_POINT('Ctrl Pts',(133.962497647065,-33.9993816132568,17.9137341566156));
#20439=CARTESIAN_POINT('Ctrl Pts',(133.989213398485,-34.1205675345144,17.9077041468038));
#20440=CARTESIAN_POINT('Ctrl Pts',(134.014931373,-34.2372274174997,17.901899345126));
#20441=CARTESIAN_POINT('Ctrl Pts',(134.035539398504,-34.3550692997241,17.8960945434482));
#20442=CARTESIAN_POINT('Ctrl Pts',(134.050942750205,-34.4736086678504,17.8902897417704));
#20443=CARTESIAN_POINT('Ctrl Pts',(134.066343808017,-34.5921303829263,17.8844858045519));
#20444=CARTESIAN_POINT('Ctrl Pts',(134.076541680862,-34.7113489726554,17.8786818673334));
#20445=CARTESIAN_POINT('Ctrl Pts',(134.081493237234,-34.8307724773791,17.8728779301149));
#20446=CARTESIAN_POINT('Ctrl Pts',(134.086445223776,-34.9502063570867,17.867073488676));
#20447=CARTESIAN_POINT('Ctrl Pts',(134.086149970745,-35.0698447793198,17.8612690472372));
#20448=CARTESIAN_POINT('Ctrl Pts',(134.080616448311,-35.1891940849229,17.8554646057984));
#20449=CARTESIAN_POINT('Ctrl Pts',(134.075081140371,-35.3085819010752,17.8496582914351));
#20450=CARTESIAN_POINT('Ctrl Pts',(134.06430422041,-35.4276800075163,17.8438519770719));
#20451=CARTESIAN_POINT('Ctrl Pts',(134.048346612716,-35.545998812552,17.8380456627087));
#20452=CARTESIAN_POINT('Ctrl Pts',(134.032371385358,-35.664448259837,17.8322329372769));
#20453=CARTESIAN_POINT('Ctrl Pts',(134.011204106662,-35.7821162833686,17.8264202118451));
#20454=CARTESIAN_POINT('Ctrl Pts',(133.984957050805,-35.898522288671,17.8206074864133));
#20455=CARTESIAN_POINT('Ctrl Pts',(133.958692800776,-36.0150045503334,17.8147909531257));
#20456=CARTESIAN_POINT('Ctrl Pts',(133.927342253215,-36.1302227543044,17.8089744198381));
#20457=CARTESIAN_POINT('Ctrl Pts',(133.891067426887,-36.2437118956641,17.8031578865505));
#20458=CARTESIAN_POINT('Ctrl Pts',(133.854740775171,-36.3573631775373,17.7973330432548));
#20459=CARTESIAN_POINT('Ctrl Pts',(133.813475943363,-36.4692800845744,17.791508199959));
#20460=CARTESIAN_POINT('Ctrl Pts',(133.767482925139,-36.5790178620857,17.7856833566632));
#20461=CARTESIAN_POINT('Ctrl Pts',(133.755350927817,-36.6079643951529,17.7841468846943));
#20462=CARTESIAN_POINT('Ctrl Pts',(133.742890192233,-36.636759442064,17.7826104127255));
#20463=CARTESIAN_POINT('Ctrl Pts',(133.730105093327,-36.6653951461247,17.7810739407566));
#20464=CARTESIAN_POINT('Ctrl Pts',(133.681642147958,-36.7739410847745,17.775249820221));
#20465=CARTESIAN_POINT('Ctrl Pts',(133.628359278819,-36.8805444906622,17.7694256996854));
#20466=CARTESIAN_POINT('Ctrl Pts',(133.570434298946,-36.9847478219934,17.7636015791498));
#20467=CARTESIAN_POINT('Ctrl Pts',(133.512582285387,-37.0888198915968,17.7577847950796));
#20468=CARTESIAN_POINT('Ctrl Pts',(133.450099988354,-37.1904975462668,17.7519680110093));
#20469=CARTESIAN_POINT('Ctrl Pts',(133.383213025757,-37.2893437099631,17.746151226939));
#20470=CARTESIAN_POINT('Ctrl Pts',(133.316392895301,-37.3880911085112,17.7403402548853));
#20471=CARTESIAN_POINT('Ctrl Pts',(133.245177082164,-37.4840123082296,17.7345292828316));
#20472=CARTESIAN_POINT('Ctrl Pts',(133.169836506206,-37.5766958539816,17.7287183107778));
#20473=CARTESIAN_POINT('Ctrl Pts',(133.091654118015,-37.672875380892,17.7226881515033));
#20474=CARTESIAN_POINT('Ctrl Pts',(133.009029889101,-37.7655678070874,17.7166579922287));
#20475=CARTESIAN_POINT('Ctrl Pts',(132.92231541916,-37.8543471391786,17.7106278329541));
#20476=CARTESIAN_POINT('Ctrl Pts',(132.838846628786,-37.9398035049379,17.7048233795479));
#20477=CARTESIAN_POINT('Ctrl Pts',(132.751588597142,-38.0216341246567,17.6990189261418));
#20478=CARTESIAN_POINT('Ctrl Pts',(132.660894654302,-38.099494255311,17.6932144727356));
#20479=CARTESIAN_POINT('Ctrl Pts',(132.570213999643,-38.1773429781525,17.687410869779));
#20480=CARTESIAN_POINT('Ctrl Pts',(132.476098744603,-38.2512221029872,17.6816072668224));
#20481=CARTESIAN_POINT('Ctrl Pts',(132.378936721682,-38.3208259626536,17.6758036638659));
#20482=CARTESIAN_POINT('Ctrl Pts',(132.281766017736,-38.3904360411364,17.6699995423814));
#20483=CARTESIAN_POINT('Ctrl Pts',(132.181548336559,-38.455769857223,17.664195420897));
#20484=CARTESIAN_POINT('Ctrl Pts',(132.078701484019,-38.5165643944533,17.6583912994125));
#20485=CARTESIAN_POINT('Ctrl Pts',(131.975821184969,-38.5773787024889,17.6525852903875));
#20486=CARTESIAN_POINT('Ctrl Pts',(131.870310365345,-38.633650588177,17.6467792813625));
#20487=CARTESIAN_POINT('Ctrl Pts',(131.76261189896,-38.6851627228176,17.6409732723375));
#20488=CARTESIAN_POINT('Ctrl Pts',(131.654794083567,-38.7367319420424,17.6351608292244));
#20489=CARTESIAN_POINT('Ctrl Pts',(131.544784150796,-38.7835307053043,17.6293483861113));
#20490=CARTESIAN_POINT('Ctrl Pts',(131.433045588882,-38.8253895671142,17.6235359429982));
#20491=CARTESIAN_POINT('Ctrl Pts',(131.321233573453,-38.8672759456601,17.6177196789627));
#20492=CARTESIAN_POINT('Ctrl Pts',(131.207691053125,-38.9042158295528,17.6119034149272));
#20493=CARTESIAN_POINT('Ctrl Pts',(131.092895733437,-38.9360899273054,17.6060871508917));
#20494=CARTESIAN_POINT('Ctrl Pts',(130.977935983922,-38.9680096806858,17.600262555791));
#20495=CARTESIAN_POINT('Ctrl Pts',(130.861720249722,-38.9948490735882,17.5944379606904));
#20496=CARTESIAN_POINT('Ctrl Pts',(130.744735586478,-39.0165400416568,17.5886133655897));
#20497=CARTESIAN_POINT('Ctrl Pts',(130.713812817997,-39.0222736546375,17.5870737397892));
#20498=CARTESIAN_POINT('Ctrl Pts',(130.682836344301,-39.0276478222182,17.5855341139886));
#20499=CARTESIAN_POINT('Ctrl Pts',(130.651815190333,-39.0326618947851,17.5839944881881));
#20500=CARTESIAN_POINT('Ctrl Pts',(130.534583268297,-39.0516105568768,17.578176094327));
#20501=CARTESIAN_POINT('Ctrl Pts',(130.416333240764,-39.0654738601746,17.5723577004659));
#20502=CARTESIAN_POINT('Ctrl Pts',(130.297544301261,-39.0741492840576,17.5665393066048));
#20503=CARTESIAN_POINT('Ctrl Pts',(130.178905628137,-39.0828137336484,17.5607282729322));
#20504=CARTESIAN_POINT('Ctrl Pts',(130.059729803323,-39.0863033265891,17.5549172392596));
#20505=CARTESIAN_POINT('Ctrl Pts',(129.940505181167,-39.0845667293523,17.549106205587));
#20506=CARTESIAN_POINT('Ctrl Pts',(129.821400146662,-39.0828318740006,17.5433010006422));
#20507=CARTESIAN_POINT('Ctrl Pts',(129.702246818913,-39.0758812624831,17.5374957956974));
#20508=CARTESIAN_POINT('Ctrl Pts',(129.583537018591,-39.0637154901784,17.5316905907525));
#20509=CARTESIAN_POINT('Ctrl Pts',(129.460183081588,-39.0510737714122,17.5256582759553));
#20510=CARTESIAN_POINT('Ctrl Pts',(129.337308532162,-39.0328004820631,17.5196259611581));
#20511=CARTESIAN_POINT('Ctrl Pts',(129.215463760267,-39.0089559599159,17.5135936463609));
#20512=CARTESIAN_POINT('Ctrl Pts',(129.098338076859,-38.9860349440316,17.5077949651195));
#20513=CARTESIAN_POINT('Ctrl Pts',(128.98216432776,-38.9579662978657,17.501996283878));
#20514=CARTESIAN_POINT('Ctrl Pts',(128.867423787524,-38.9248561913697,17.4961976026366));
#20515=CARTESIAN_POINT('Ctrl Pts',(128.752699916642,-38.8917508950661,17.4903997638199));
#20516=CARTESIAN_POINT('Ctrl Pts',(128.639409233592,-38.853605708297,17.4846019250032));
#20517=CARTESIAN_POINT('Ctrl Pts',(128.528019260807,-38.8105770827324,17.4788040861865));
#20518=CARTESIAN_POINT('Ctrl Pts',(128.416619052904,-38.7675445034627,17.4730057146327));
#20519=CARTESIAN_POINT('Ctrl Pts',(128.307120284198,-38.7196277406865,17.4672073430789));
#20520=CARTESIAN_POINT('Ctrl Pts',(128.199971240297,-38.6670316966507,17.4614089715251));
#20521=CARTESIAN_POINT('Ctrl Pts',(128.09278693909,-38.61441834593,17.4556086920219));
#20522=CARTESIAN_POINT('Ctrl Pts',(127.987954267406,-38.5571228321082,17.4498084125187));
#20523=CARTESIAN_POINT('Ctrl Pts',(127.885897033814,-38.4953960645915,17.4440081330155));
#20524=CARTESIAN_POINT('Ctrl Pts',(127.783725552764,-38.4336001973551,17.4382013604186));
#20525=CARTESIAN_POINT('Ctrl Pts',(127.684336061771,-38.3673633867531,17.4323945878217));
#20526=CARTESIAN_POINT('Ctrl Pts',(127.588123611192,-38.2969800249788,17.4265878152247));
#20527=CARTESIAN_POINT('Ctrl Pts',(127.491847393984,-38.2265500152951,17.420777194079));
#20528=CARTESIAN_POINT('Ctrl Pts',(127.398752728922,-38.1519682368748,17.4149665729333));
#20529=CARTESIAN_POINT('Ctrl Pts',(127.309200486926,-38.0735684440798,17.4091559517876));
#20530=CARTESIAN_POINT('Ctrl Pts',(127.219518559403,-37.9950551162322,17.4033369159617));
#20531=CARTESIAN_POINT('Ctrl Pts',(127.133389588573,-37.9127130201863,17.3975178801359));
#20532=CARTESIAN_POINT('Ctrl Pts',(127.051136702445,-37.8269117871514,17.3916988443101));
#20533=CARTESIAN_POINT('Ctrl Pts',(127.028596767237,-37.803399490812,17.3901042414133));
#20534=CARTESIAN_POINT('Ctrl Pts',(127.006347661452,-37.7796276189105,17.3885096385165));
#20535=CARTESIAN_POINT('Ctrl Pts',(126.98439548147,-37.7556041783652,17.3869150356197));
#20536=CARTESIAN_POINT('Ctrl Pts',(126.904949694774,-37.6686624197412,17.3811441061854));
#20537=CARTESIAN_POINT('Ctrl Pts',(126.829126420265,-37.5781282483199,17.3753731767511));
#20538=CARTESIAN_POINT('Ctrl Pts',(126.757271904743,-37.4843388456957,17.3696022473168));
#20539=CARTESIAN_POINT('Ctrl Pts',(126.68553138207,-37.3906982342941,17.3638404731136));
#20540=CARTESIAN_POINT('Ctrl Pts',(126.617747338226,-37.2938129978376,17.3580786989103));
#20541=CARTESIAN_POINT('Ctrl Pts',(126.554228208451,-37.1940560067062,17.352316924707));
#20542=CARTESIAN_POINT('Ctrl Pts',(126.490766915311,-37.0943898481901,17.346560396823));
#20543=CARTESIAN_POINT('Ctrl Pts',(126.431563040174,-36.9918574813407,17.3408038689389));
#20544=CARTESIAN_POINT('Ctrl Pts',(126.376883772214,-36.8868634820651,17.3350473410549));
#20545=CARTESIAN_POINT('Ctrl Pts',(126.322240771507,-36.7819391224183,17.3292946313173));
#20546=CARTESIAN_POINT('Ctrl Pts',(126.272116603255,-36.6745567447501,17.3235419215796));
#20547=CARTESIAN_POINT('Ctrl Pts',(126.226733859034,-36.5651477979528,17.317789211842));
#20548=CARTESIAN_POINT('Ctrl Pts',(126.181369996407,-36.4557843710003,17.3120388955326));
#20549=CARTESIAN_POINT('Ctrl Pts',(126.140743793312,-36.3443964363891,17.3062885792231));
#20550=CARTESIAN_POINT('Ctrl Pts',(126.105030474364,-36.2314371256241,17.3005382629137));
#20551=CARTESIAN_POINT('Ctrl Pts',(126.069314010461,-36.1184678675355,17.2947874402249));
#20552=CARTESIAN_POINT('Ctrl Pts',(126.038511430088,-36.0039273512483,17.2890366175361));
#20553=CARTESIAN_POINT('Ctrl Pts',(126.012748532405,-35.8882852774671,17.2832857948474));
#20554=CARTESIAN_POINT('Ctrl Pts',(125.986984650957,-35.7726387878505,17.2775347525613));
#20555=CARTESIAN_POINT('Ctrl Pts',(125.966260918392,-35.6558910655558,17.2717837102753));
#20556=CARTESIAN_POINT('Ctrl Pts',(125.950652058164,-35.5385222799012,17.2660326679892));
#20557=CARTESIAN_POINT('Ctrl Pts',(125.935032572806,-35.4210735999719,17.2602777109029));
#20558=CARTESIAN_POINT('Ctrl Pts',(125.924534958788,-35.3030034268805,17.2545227538166));
#20559=CARTESIAN_POINT('Ctrl Pts',(125.919182065361,-35.1847971437223,17.2487677967303));
#20560=CARTESIAN_POINT('Ctrl Pts',(125.916344291963,-35.1221314750591,17.2457168740187));
#20561=CARTESIAN_POINT('Ctrl Pts',(125.914951544561,-35.0594275863794,17.2426659513071));
#20562=CARTESIAN_POINT('Ctrl Pts',(125.915001286747,-34.9967576667114,17.2396150285955));
#20563=CARTESIAN_POINT('Origin',(130.,-35.,32.7603849714045));
#20564=CARTESIAN_POINT('',(132.487160670875,-31.7594357285724,19.2967873947729));
#20565=CARTESIAN_POINT('',(132.487160670875,-31.7594357285724,19.1927515499128));
#20566=CARTESIAN_POINT('',(132.487160670875,-31.7594357285724,32.7603849714045));
#20567=CARTESIAN_POINT('',(125.915000065373,-34.9992691782955,18.3853849714449));
#20568=CARTESIAN_POINT('Ctrl Pts',(132.487160670875,-31.7594357285724,19.1927515499128));
#20569=CARTESIAN_POINT('Ctrl Pts',(132.581827177387,-31.8320930783806,19.1869279757759));
#20570=CARTESIAN_POINT('Ctrl Pts',(132.673193329814,-31.908814616929,19.1811044016391));
#20571=CARTESIAN_POINT('Ctrl Pts',(132.760910607467,-31.9892529801437,19.1752808275022));
#20572=CARTESIAN_POINT('Ctrl Pts',(132.798099032587,-32.0233554526232,19.1728118777524));
#20573=CARTESIAN_POINT('Ctrl Pts',(132.834632084745,-32.0581255579088,19.1703429280026));
#20574=CARTESIAN_POINT('Ctrl Pts',(132.870485381043,-32.0935350204725,19.1678739782528));
#20575=CARTESIAN_POINT('Ctrl Pts',(132.955052701829,-32.1770554687629,19.1620504560929));
#20576=CARTESIAN_POINT('Ctrl Pts',(133.03610818553,-32.2644045741462,19.156226933933));
#20577=CARTESIAN_POINT('Ctrl Pts',(133.113286012663,-32.355255172354,19.1504034117731));
#20578=CARTESIAN_POINT('Ctrl Pts',(133.190366466249,-32.4459911463853,19.1445872370215));
#20579=CARTESIAN_POINT('Ctrl Pts',(133.263578731991,-32.5402195179648,19.1387710622698));
#20580=CARTESIAN_POINT('Ctrl Pts',(133.332592945845,-32.6375755552185,19.1329548875181));
#20581=CARTESIAN_POINT('Ctrl Pts',(133.401538075306,-32.7348341374344,19.1271445348556));
#20582=CARTESIAN_POINT('Ctrl Pts',(133.466293278075,-32.8352138256769,19.1213341821931));
#20583=CARTESIAN_POINT('Ctrl Pts',(133.526568593771,-32.9383164759288,19.1155238295306));
#20584=CARTESIAN_POINT('Ctrl Pts',(133.589126503954,-33.0453235692901,19.1094934418703));
#20585=CARTESIAN_POINT('Ctrl Pts',(133.646858227866,-33.155263593993,19.1034630542101));
#20586=CARTESIAN_POINT('Ctrl Pts',(133.699488433033,-33.2676575587207,19.0974326665498));
#20587=CARTESIAN_POINT('Ctrl Pts',(133.750141208964,-33.3758286421019,19.0916288534359));
#20588=CARTESIAN_POINT('Ctrl Pts',(133.79606871103,-33.4862721897746,19.0858250403219));
#20589=CARTESIAN_POINT('Ctrl Pts',(133.837072401333,-33.5985363412033,19.0800212272079));
#20590=CARTESIAN_POINT('Ctrl Pts',(133.878070036958,-33.7107839155086,19.0742182710952));
#20591=CARTESIAN_POINT('Ctrl Pts',(133.914145166652,-33.8248511754843,19.0684153149826));
#20592=CARTESIAN_POINT('Ctrl Pts',(133.945147960975,-33.9402676913422,19.0626123588699));
#20593=CARTESIAN_POINT('Ctrl Pts',(133.976153494533,-34.0556944047638,19.0568088900402));
#20594=CARTESIAN_POINT('Ctrl Pts',(134.002085695723,-34.1724702167038,19.0510054212106));
#20595=CARTESIAN_POINT('Ctrl Pts',(134.022845199161,-34.2901116259668,19.0452019523809));
#20596=CARTESIAN_POINT('Ctrl Pts',(134.043611436343,-34.4077911944864,19.0393966010843));
#20597=CARTESIAN_POINT('Ctrl Pts',(134.059201567955,-34.5263365167954,19.0335912497877));
#20598=CARTESIAN_POINT('Ctrl Pts',(134.069567812193,-34.6452566815796,19.0277858984912));
#20599=CARTESIAN_POINT('Ctrl Pts',(134.079945538032,-34.7643085617543,19.021974117216));
#20600=CARTESIAN_POINT('Ctrl Pts',(134.08508779176,-34.8837357060798,19.0161623359409));
#20601=CARTESIAN_POINT('Ctrl Pts',(134.08499886531,-35.0030447355878,19.0103505546657));
#20602=CARTESIAN_POINT('Ctrl Pts',(134.084909880444,-35.1224321392741,19.0045349556277));
#20603=CARTESIAN_POINT('Ctrl Pts',(134.079582889975,-35.241700866618,18.9987193565897));
#20604=CARTESIAN_POINT('Ctrl Pts',(134.069074136742,-35.3603618593873,18.9929037575517));
#20605=CARTESIAN_POINT('Ctrl Pts',(134.058550328391,-35.4791928490312,18.9870798269328));
#20606=CARTESIAN_POINT('Ctrl Pts',(134.042829993951,-35.59741396297,18.9812558963139));
#20607=CARTESIAN_POINT('Ctrl Pts',(134.022020620761,-35.7145453982577,18.975431965695));
#20608=CARTESIAN_POINT('Ctrl Pts',(134.016497305201,-35.7456349401286,18.9738861523581));
#20609=CARTESIAN_POINT('Ctrl Pts',(134.01061573948,-35.7766477941407,18.9723403390213));
#20610=CARTESIAN_POINT('Ctrl Pts',(134.004378520275,-35.8075751769097,18.9707945256845));
#20611=CARTESIAN_POINT('Ctrl Pts',(133.980880487633,-35.9240906665762,18.9649708451222));
#20612=CARTESIAN_POINT('Ctrl Pts',(133.952254965274,-36.0397675904643,18.9591471645599));
#20613=CARTESIAN_POINT('Ctrl Pts',(133.91857506942,-36.1541206285814,18.9533234839977));
#20614=CARTESIAN_POINT('Ctrl Pts',(133.88493766735,-36.2683293879503,18.9475071511487));
#20615=CARTESIAN_POINT('Ctrl Pts',(133.846258690005,-36.3812171955832,18.9416908182998));
#20616=CARTESIAN_POINT('Ctrl Pts',(133.802662383301,-36.4923082116737,18.9358744854508));
#20617=CARTESIAN_POINT('Ctrl Pts',(133.759109719698,-36.6032880175059,18.9300639751778));
#20618=CARTESIAN_POINT('Ctrl Pts',(133.71064966797,-36.7124742322112,18.9242534649048));
#20619=CARTESIAN_POINT('Ctrl Pts',(133.65745629243,-36.8194060758835,18.9184429546318));
#20620=CARTESIAN_POINT('Ctrl Pts',(133.602250551807,-36.9303832711881,18.9124126262353));
#20621=CARTESIAN_POINT('Ctrl Pts',(133.541946407721,-37.0389317263569,18.9063822978388));
#20622=CARTESIAN_POINT('Ctrl Pts',(133.476793534076,-37.1445586309089,18.9003519694423));
#20623=CARTESIAN_POINT('Ctrl Pts',(133.414086297717,-37.2462206282868,18.8945480009153));
#20624=CARTESIAN_POINT('Ctrl Pts',(133.346888017009,-37.3451760749478,18.8887440323882));
#20625=CARTESIAN_POINT('Ctrl Pts',(133.275467795461,-37.4410112086788,18.8829400638611));
#20626=CARTESIAN_POINT('Ctrl Pts',(133.204058132901,-37.5368321738467,18.8771369534107));
#20627=CARTESIAN_POINT('Ctrl Pts',(133.12842801474,-37.6295334161818,18.8713338429603));
#20628=CARTESIAN_POINT('Ctrl Pts',(133.04888877558,-37.7187317326541,18.8655307325099));
#20629=CARTESIAN_POINT('Ctrl Pts',(132.969342525942,-37.8079379109431,18.8597271105814));
#20630=CARTESIAN_POINT('Ctrl Pts',(132.885886742036,-37.8936402447414,18.8539234886528));
#20631=CARTESIAN_POINT('Ctrl Pts',(132.798871353915,-37.975490572029,18.8481198667243));
#20632=CARTESIAN_POINT('Ctrl Pts',(132.711827762464,-38.0573674285532,18.8423143637323));
#20633=CARTESIAN_POINT('Ctrl Pts',(132.621222569546,-38.1353895159424,18.8365088607403));
#20634=CARTESIAN_POINT('Ctrl Pts',(132.527440179702,-38.2092477526714,18.8307033577483));
#20635=CARTESIAN_POINT('Ctrl Pts',(132.433553965407,-38.283187756254,18.8248914276097));
#20636=CARTESIAN_POINT('Ctrl Pts',(132.336483854118,-38.3529544550157,18.8190794974711));
#20637=CARTESIAN_POINT('Ctrl Pts',(132.236644859884,-38.4182809672049,18.8132675673325));
#20638=CARTESIAN_POINT('Ctrl Pts',(132.136740308358,-38.4836503747498,18.8074518209055));
#20639=CARTESIAN_POINT('Ctrl Pts',(132.034063603382,-38.5445735814209,18.8016360744785));
#20640=CARTESIAN_POINT('Ctrl Pts',(131.929054624238,-38.6008295234163,18.7958203280516));
#20641=CARTESIAN_POINT('Ctrl Pts',(131.82389526941,-38.6571660254343,18.7899962533192));
#20642=CARTESIAN_POINT('Ctrl Pts',(131.716397340927,-38.7088217463478,18.7841721785869));
#20643=CARTESIAN_POINT('Ctrl Pts',(131.607021068971,-38.7556235546025,18.7783481038545));
#20644=CARTESIAN_POINT('Ctrl Pts',(131.578018257175,-38.7680337786138,18.776803760275));
#20645=CARTESIAN_POINT('Ctrl Pts',(131.548883456525,-38.7801029826979,18.7752594166955));
#20646=CARTESIAN_POINT('Ctrl Pts',(131.519625411257,-38.791828531126,18.773715073116));
#20647=CARTESIAN_POINT('Ctrl Pts',(131.409293643512,-38.8360454456193,18.7678913704191));
#20648=CARTESIAN_POINT('Ctrl Pts',(131.296852532956,-38.8755141152904,18.7620676677222));
#20649=CARTESIAN_POINT('Ctrl Pts',(131.182748077146,-38.9100296656174,18.7562439650253));
#20650=CARTESIAN_POINT('Ctrl Pts',(131.068787554557,-38.9445016774661,18.750427608442));
#20651=CARTESIAN_POINT('Ctrl Pts',(130.953168247317,-38.9740328798198,18.7446112518587));
#20652=CARTESIAN_POINT('Ctrl Pts',(130.836356250139,-38.9984663588497,18.7387948952753));
#20653=CARTESIAN_POINT('Ctrl Pts',(130.719661158745,-39.0228753847833,18.7329843597185));
#20654=CARTESIAN_POINT('Ctrl Pts',(130.601776149403,-39.0421967537167,18.7271738241616));
#20655=CARTESIAN_POINT('Ctrl Pts',(130.483182028482,-39.0563234742008,18.7213632886047));
#20656=CARTESIAN_POINT('Ctrl Pts',(130.360102075995,-39.0709845389522,18.7153329691024));
#20657=CARTESIAN_POINT('Ctrl Pts',(130.236258737322,-39.0800500903439,18.7093026496));
#20658=CARTESIAN_POINT('Ctrl Pts',(130.112201044107,-39.083458818906,18.7032723300976));
#20659=CARTESIAN_POINT('Ctrl Pts',(129.992799321315,-39.0867396155442,18.6974683326275));
#20660=CARTESIAN_POINT('Ctrl Pts',(129.873199488605,-39.0847805341232,18.6916643351573));
#20661=CARTESIAN_POINT('Ctrl Pts',(129.753895122748,-39.0775798446374,18.6858603376872));
#20662=CARTESIAN_POINT('Ctrl Pts',(129.634608368584,-39.0703802181162,18.6800571970023));
#20663=CARTESIAN_POINT('Ctrl Pts',(129.515617401998,-39.0579405468999,18.6742540563174));
#20664=CARTESIAN_POINT('Ctrl Pts',(129.397413389351,-39.0403111732473,18.6684509156325));
#20665=CARTESIAN_POINT('Ctrl Pts',(129.279198932917,-39.0226802419705,18.6626472622174));
#20666=CARTESIAN_POINT('Ctrl Pts',(129.161771972536,-38.9998587568216,18.6568436088023));
#20667=CARTESIAN_POINT('Ctrl Pts',(129.045615522846,-38.9719485482276,18.6510399553872));
#20668=CARTESIAN_POINT('Ctrl Pts',(128.929421400574,-38.9440292876214,18.6452344196951));
#20669=CARTESIAN_POINT('Ctrl Pts',(128.814499005302,-38.9110181166276,18.6394288840031));
#20670=CARTESIAN_POINT('Ctrl Pts',(128.701317562576,-38.8730671213814,18.6336233483111));
#20671=CARTESIAN_POINT('Ctrl Pts',(128.588010788321,-38.8350741010814,18.6278113838561));
#20672=CARTESIAN_POINT('Ctrl Pts',(128.47644920212,-38.7921304675922,18.6219994194012));
#20673=CARTESIAN_POINT('Ctrl Pts',(128.367083513114,-38.7444370400442,18.6161874549463));
#20674=CARTESIAN_POINT('Ctrl Pts',(128.257645993281,-38.6967122876964,18.6103716732228));
#20675=CARTESIAN_POINT('Ctrl Pts',(128.150407608846,-38.6442317075111,18.6045558914993));
#20676=CARTESIAN_POINT('Ctrl Pts',(128.045794377579,-38.5872420304878,18.5987401097757));
#20677=CARTESIAN_POINT('Ctrl Pts',(127.941031317505,-38.5301707319026,18.592915998593));
#20678=CARTESIAN_POINT('Ctrl Pts',(127.838901263346,-38.4685776567739,18.5870918874104));
#20679=CARTESIAN_POINT('Ctrl Pts',(127.739801298729,-38.4027528312785,18.5812677762277));
#20680=CARTESIAN_POINT('Ctrl Pts',(127.713528536551,-38.3853017656568,18.5797237243343));
#20681=CARTESIAN_POINT('Ctrl Pts',(127.687468563015,-38.3675534882863,18.5781796724409));
#20682=CARTESIAN_POINT('Ctrl Pts',(127.661628371752,-38.3495138644596,18.5766356205475));
#20683=CARTESIAN_POINT('Ctrl Pts',(127.564645404129,-38.2818078542471,18.5708405111669));
#20684=CARTESIAN_POINT('Ctrl Pts',(127.470441320797,-38.2097715994423,18.5650454017863));
#20685=CARTESIAN_POINT('Ctrl Pts',(127.379429648083,-38.1336617607289,18.5592502924056));
#20686=CARTESIAN_POINT('Ctrl Pts',(127.288533132876,-38.0576482241601,18.5534625156047));
#20687=CARTESIAN_POINT('Ctrl Pts',(127.20082130956,-37.977571615792,18.5476747388038));
#20688=CARTESIAN_POINT('Ctrl Pts',(127.11667881418,-37.8937318361248,18.5418869620029));
#20689=CARTESIAN_POINT('Ctrl Pts',(127.032620266486,-37.8099757021282,18.5361049595787));
#20690=CARTESIAN_POINT('Ctrl Pts',(126.952124254574,-37.722464154091,18.5303229571545));
#20691=CARTESIAN_POINT('Ctrl Pts',(126.875541868502,-37.6315368864056,18.5245409547303));
#20692=CARTESIAN_POINT('Ctrl Pts',(126.798745396922,-37.5403554321999,18.5187427887601));
#20693=CARTESIAN_POINT('Ctrl Pts',(126.725884781323,-37.4457394066967,18.5129446227899));
#20694=CARTESIAN_POINT('Ctrl Pts',(126.65727658786,-37.3480683954962,18.5071464568196));
#20695=CARTESIAN_POINT('Ctrl Pts',(126.58893403817,-37.2507755562707,18.5013707407437));
#20696=CARTESIAN_POINT('Ctrl Pts',(126.524811277393,-37.1504516870973,18.4955950246677));
#20697=CARTESIAN_POINT('Ctrl Pts',(126.465180005024,-37.0475039934317,18.4898193085918));
#20698=CARTESIAN_POINT('Ctrl Pts',(126.405556722735,-36.9445700938754,18.4840443664124));
#20699=CARTESIAN_POINT('Ctrl Pts',(126.350423939006,-36.8390134261195,18.4782694242329));
#20700=CARTESIAN_POINT('Ctrl Pts',(126.300008586202,-36.7312678989178,18.4724944820535));
#20701=CARTESIAN_POINT('Ctrl Pts',(126.249587776293,-36.6235107090232,18.4667189147773));
#20702=CARTESIAN_POINT('Ctrl Pts',(126.203885587117,-36.5135645627699,18.4609433475011));
#20703=CARTESIAN_POINT('Ctrl Pts',(126.163081481472,-36.4018849033276,18.4551677802249));
#20704=CARTESIAN_POINT('Ctrl Pts',(126.121997131868,-36.2894382242567,18.4493525461599));
#20705=CARTESIAN_POINT('Ctrl Pts',(126.08587855545,-36.1752345254005,18.4435373120949));
#20706=CARTESIAN_POINT('Ctrl Pts',(126.054858042081,-36.0597546564499,18.4377220780299));
#20707=CARTESIAN_POINT('Ctrl Pts',(126.024004228695,-35.9448953604704,18.4319380942349));
#20708=CARTESIAN_POINT('Ctrl Pts',(125.998193853041,-35.8287739946131,18.4261541104399));
#20709=CARTESIAN_POINT('Ctrl Pts',(125.977505578191,-35.7118733219564,18.4203701266449));
#20710=CARTESIAN_POINT('Ctrl Pts',(125.956649638406,-35.5940252458205,18.4145392674449));
#20711=CARTESIAN_POINT('Ctrl Pts',(125.940999242795,-35.4753855999452,18.4087084082449));
#20712=CARTESIAN_POINT('Ctrl Pts',(125.930581536691,-35.3564524799731,18.4028775490449));
#20713=CARTESIAN_POINT('Ctrl Pts',(125.920163830587,-35.2375193600011,18.3970466898449));
#20714=CARTESIAN_POINT('Ctrl Pts',(125.914978771534,-35.1182931914366,18.3912158306449));
#20715=CARTESIAN_POINT('Ctrl Pts',(125.915000065373,-34.9992691782955,18.3853849714449));
#20716=CARTESIAN_POINT('Ctrl Pts',(125.915000065374,-34.9992691774698,18.3853849714045));
#20717=CARTESIAN_POINT('Ctrl Pts',(125.915007160825,-34.9596084944438,18.3834420369294));
#20718=CARTESIAN_POINT('Ctrl Pts',(125.915591831957,-34.9199536068433,18.3814991024543));
#20719=CARTESIAN_POINT('Ctrl Pts',(125.916753658639,-34.8803157664518,18.3795561679791));
#20720=CARTESIAN_POINT('Ctrl Pts',(125.920236584366,-34.7614893904925,18.3737316361649));
#20721=CARTESIAN_POINT('Ctrl Pts',(125.928916364881,-34.6426238185521,18.3679071043506));
#20722=CARTESIAN_POINT('Ctrl Pts',(125.942802846095,-34.5242098631234,18.3620825725364));
#20723=CARTESIAN_POINT('Ctrl Pts',(125.956671803865,-34.4059453350683,18.3562653907384));
#20724=CARTESIAN_POINT('Ctrl Pts',(125.975734346806,-34.2881316918524,18.3504482089403));
#20725=CARTESIAN_POINT('Ctrl Pts',(125.999948324585,-34.1712590308118,18.3446310271423));
#20726=CARTESIAN_POINT('Ctrl Pts',(126.024138052315,-34.0545034165374,18.3388196711919));
#20727=CARTESIAN_POINT('Ctrl Pts',(126.053468869069,-33.9386873070813,18.3330083152416));
#20728=CARTESIAN_POINT('Ctrl Pts',(126.087846978892,-33.8242943653134,18.3271969592912));
#20729=CARTESIAN_POINT('Ctrl Pts',(126.123518576595,-33.7055973508514,18.3211669491295));
#20730=CARTESIAN_POINT('Ctrl Pts',(126.164624688392,-33.588433146939,18.3151369389678));
#20731=CARTESIAN_POINT('Ctrl Pts',(126.211002501278,-33.4733294544416,18.3091069288061));
#20732=CARTESIAN_POINT('Ctrl Pts',(126.255648191268,-33.3625246654219,18.3033021280282));
#20733=CARTESIAN_POINT('Ctrl Pts',(126.305178700704,-33.2536296476363,18.2974973272503));
#20734=CARTESIAN_POINT('Ctrl Pts',(126.359398630354,-33.1470977717822,18.2916925264723));
#20735=CARTESIAN_POINT('Ctrl Pts',(126.413610485596,-33.0405817606087,18.2858885901428));
#20736=CARTESIAN_POINT('Ctrl Pts',(126.472510187143,-32.9364285551924,18.2800846538133));
#20737=CARTESIAN_POINT('Ctrl Pts',(126.535855549591,-32.8350685399535,18.2742807174837));
#20738=CARTESIAN_POINT('Ctrl Pts',(126.599206415331,-32.7336997187998,18.2684762769222));
#20739=CARTESIAN_POINT('Ctrl Pts',(126.66700349354,-32.6351249164702,18.2626718363606));
#20740=CARTESIAN_POINT('Ctrl Pts',(126.738960637975,-32.5397465010037,18.256867395799));
#20741=CARTESIAN_POINT('Ctrl Pts',(126.810941001048,-32.4443373094839,18.2510610823003));
#20742=CARTESIAN_POINT('Ctrl Pts',(126.887083854255,-32.3521268817277,18.2452547688016));
#20743=CARTESIAN_POINT('Ctrl Pts',(126.967062468593,-32.2634848930473,18.2394484553029));
#20744=CARTESIAN_POINT('Ctrl Pts',(127.047129392011,-32.1747450295463,18.2336357307128));
#20745=CARTESIAN_POINT('Ctrl Pts',(127.131040256969,-32.0895817732114,18.2278230061228));
#20746=CARTESIAN_POINT('Ctrl Pts',(127.218431033966,-32.0083283791175,18.2220102815327));
#20747=CARTESIAN_POINT('Ctrl Pts',(127.305879059942,-31.9270217565923,18.2161937490744));
#20748=CARTESIAN_POINT('Ctrl Pts',(127.396811227873,-31.8496303612636,18.2103772166162));
#20749=CARTESIAN_POINT('Ctrl Pts',(127.490831255007,-31.7764464935186,18.204560684158));
#20750=CARTESIAN_POINT('Ctrl Pts',(127.584985607785,-31.7031580685799,18.1987358416673));
#20751=CARTESIAN_POINT('Ctrl Pts',(127.682236293481,-31.6340894049455,18.1929109991767));
#20752=CARTESIAN_POINT('Ctrl Pts',(127.782158868308,-31.5694890009543,18.1870861566861));
#20753=CARTESIAN_POINT('Ctrl Pts',(127.808516504672,-31.5524486678726,18.185549676261));
#20754=CARTESIAN_POINT('Ctrl Pts',(127.835059925452,-31.5357189856054,18.1840131958358));
#20755=CARTESIAN_POINT('Ctrl Pts',(127.861781083475,-31.5193039683111,18.1824767154107));
#20756=CARTESIAN_POINT('Ctrl Pts',(127.963069165046,-31.4570819040853,18.1766525982635));
#20757=CARTESIAN_POINT('Ctrl Pts',(128.067238441947,-31.399184622791,18.1708284811163));
#20758=CARTESIAN_POINT('Ctrl Pts',(128.173883810515,-31.3458893472556,18.1650043639691));
#20759=CARTESIAN_POINT('Ctrl Pts',(128.280394840776,-31.2926612063475,18.1591875833059));
#20760=CARTESIAN_POINT('Ctrl Pts',(128.389375396946,-31.2440237218838,18.1533708026427));
#20761=CARTESIAN_POINT('Ctrl Pts',(128.500392476305,-31.2002102328055,18.1475540219795));
#20762=CARTESIAN_POINT('Ctrl Pts',(128.611298629235,-31.1564405214402,18.1417430533472));
#20763=CARTESIAN_POINT('Ctrl Pts',(128.724236879665,-31.1174853655095,18.1359320847149));
#20764=CARTESIAN_POINT('Ctrl Pts',(128.838751302399,-31.0835313786116,18.1301211160827));
#20765=CARTESIAN_POINT('Ctrl Pts',(128.95758525217,-31.0482966345749,18.124090955531));
#20766=CARTESIAN_POINT('Ctrl Pts',(129.078116222543,-31.0184479812632,18.1180607949793));
#20767=CARTESIAN_POINT('Ctrl Pts',(129.199813490375,-30.9941384759563,18.1120306344276));
#20768=CARTESIAN_POINT('Ctrl Pts',(129.316955595742,-30.9707388821707,18.1062261844567));
#20769=CARTESIAN_POINT('Ctrl Pts',(129.435177821768,-30.9524713116863,18.1004217344858));
#20770=CARTESIAN_POINT('Ctrl Pts',(129.553993896093,-30.9394207857404,18.0946172845148));
#20771=CARTESIAN_POINT('Ctrl Pts',(129.672792561881,-30.9263721719142,18.0888136849927));
#20772=CARTESIAN_POINT('Ctrl Pts',(129.79218449724,-30.9185391270626,18.0830100854705));
#20773=CARTESIAN_POINT('Ctrl Pts',(129.911677017859,-30.9159549401573,18.0772064859483));
#20774=CARTESIAN_POINT('Ctrl Pts',(130.031180214741,-30.9133705223633,18.0714023678936));
#20775=CARTESIAN_POINT('Ctrl Pts',(130.150783606583,-30.9160359037771,18.0655982498389));
#20776=CARTESIAN_POINT('Ctrl Pts',(130.269993853628,-30.9239322479866,18.0597941317842));
#20777=CARTESIAN_POINT('Ctrl Pts',(130.389242868866,-30.931831160155,18.0539881261806));
#20778=CARTESIAN_POINT('Ctrl Pts',(130.508098077894,-30.9449643913867,18.048182120577));
#20779=CARTESIAN_POINT('Ctrl Pts',(130.626071248985,-30.9632612431328,18.0423761149734));
#20780=CARTESIAN_POINT('Ctrl Pts',(130.744175155961,-30.9815783711422,18.036563675252));
#20781=CARTESIAN_POINT('Ctrl Pts',(130.861394670249,-31.0050704791497,18.0307512355306));
#20782=CARTESIAN_POINT('Ctrl Pts',(130.977251583454,-31.0336157091582,18.0249387958092));
#20783=CARTESIAN_POINT('Ctrl Pts',(131.093184657763,-31.0621797040047,18.0191225351521));
#20784=CARTESIAN_POINT('Ctrl Pts',(131.20775295628,-31.0958033215968,18.0133062744949));
#20785=CARTESIAN_POINT('Ctrl Pts',(131.320494855899,-31.1343152824441,18.0074900138378));
#20786=CARTESIAN_POINT('Ctrl Pts',(131.433398245051,-31.1728824071535,18.0016654220702));
#20787=CARTESIAN_POINT('Ctrl Pts',(131.544469634885,-31.2163517024487,17.9958408303027));
#20788=CARTESIAN_POINT('Ctrl Pts',(131.653268610582,-31.2645043299095,17.9900162385351));
#20789=CARTESIAN_POINT('Ctrl Pts',(131.682028269868,-31.2772328795179,17.9884765799708));
#20790=CARTESIAN_POINT('Ctrl Pts',(131.710629287558,-31.2902884296224,17.9869369214065));
#20791=CARTESIAN_POINT('Ctrl Pts',(131.739063847766,-31.3036664201683,17.9853972628422));
#20792=CARTESIAN_POINT('Ctrl Pts',(131.846528250602,-31.3542266452825,17.9795783408343));
#20793=CARTESIAN_POINT('Ctrl Pts',(131.951961127314,-31.4095597189194,17.9737594188264));
#20794=CARTESIAN_POINT('Ctrl Pts',(132.054908974376,-31.4694796265946,17.9679404968185));
#20795=CARTESIAN_POINT('Ctrl Pts',(132.157711772312,-31.5293151096759,17.9621297734234));
#20796=CARTESIAN_POINT('Ctrl Pts',(132.258036157374,-31.5937243625645,17.9563190500284));
#20797=CARTESIAN_POINT('Ctrl Pts',(132.355450161183,-31.6624740393248,17.9505083266334));
#20798=CARTESIAN_POINT('Ctrl Pts',(132.399974541707,-31.6938970036755,17.9478524573595));
#20799=CARTESIAN_POINT('Ctrl Pts',(132.443891228791,-31.7262260633449,17.9451965880857));
#20800=CARTESIAN_POINT('Ctrl Pts',(132.487160670875,-31.7594357285724,17.9425407188119));
#20801=CARTESIAN_POINT('',(125.915000466472,-35.0019521977367,18.4896150286331));
#20802=CARTESIAN_POINT('Ctrl Pts',(125.915000466472,-35.0019521969606,18.4896150285955));
#20803=CARTESIAN_POINT('Ctrl Pts',(125.914942432893,-34.8805161196803,18.4837275172242));
#20804=CARTESIAN_POINT('Ctrl Pts',(125.920303700108,-34.7590882866263,18.4778400058528));
#20805=CARTESIAN_POINT('Ctrl Pts',(125.931055605275,-34.6381761303638,18.4719524944815));
#20806=CARTESIAN_POINT('Ctrl Pts',(125.941810869229,-34.5172262023751,18.4660631439115));
#20807=CARTESIAN_POINT('Ctrl Pts',(125.957960089699,-34.3967926619571,18.4601737933416));
#20808=CARTESIAN_POINT('Ctrl Pts',(125.979422788629,-34.2773770779969,18.4542844427717));
#20809=CARTESIAN_POINT('Ctrl Pts',(126.000896647879,-34.1578993995112,18.4483920298173));
#20810=CARTESIAN_POINT('Ctrl Pts',(126.027689417893,-34.0394411165113,18.4424996168629));
#20811=CARTESIAN_POINT('Ctrl Pts',(126.0596697468,-33.9224924614117,18.4366072039085));
#20812=CARTESIAN_POINT('Ctrl Pts',(126.091695452381,-33.8053778686486,18.4307064302488));
#20813=CARTESIAN_POINT('Ctrl Pts',(126.128923314983,-33.689777560173,18.4248056565891));
#20814=CARTESIAN_POINT('Ctrl Pts',(126.171172249785,-33.5761660703631,18.4189048829295));
#20815=CARTESIAN_POINT('Ctrl Pts',(126.213453797143,-33.4624668822243,18.4129995543785));
#20816=CARTESIAN_POINT('Ctrl Pts',(126.260763988836,-33.3507599323557,18.4070942258275));
#20817=CARTESIAN_POINT('Ctrl Pts',(126.312874489663,-33.241497662491,18.4011888972765));
#20818=CARTESIAN_POINT('Ctrl Pts',(126.365076832098,-33.1320428244831,18.395273160941));
#20819=CARTESIAN_POINT('Ctrl Pts',(126.422096202377,-33.0250416198214,18.3893574246055));
#20820=CARTESIAN_POINT('Ctrl Pts',(126.483659068718,-32.9209205270143,18.3834416882701));
#20821=CARTESIAN_POINT('Ctrl Pts',(126.52226554126,-32.8556255147855,18.3797318916674));
#20822=CARTESIAN_POINT('Ctrl Pts',(126.562657934769,-32.7914625588259,18.3760220950646));
#20823=CARTESIAN_POINT('Ctrl Pts',(126.604760614246,-32.7285303186201,18.3723122984619));
#20824=CARTESIAN_POINT('Ctrl Pts',(126.670854132907,-32.6297381931789,18.3664885952195));
#20825=CARTESIAN_POINT('Ctrl Pts',(126.741369641896,-32.5336739181619,18.3606648919772));
#20826=CARTESIAN_POINT('Ctrl Pts',(126.816054726341,-32.4407584142282,18.3548411887348));
#20827=CARTESIAN_POINT('Ctrl Pts',(126.890645601849,-32.3479601153677,18.3490248316029));
#20828=CARTESIAN_POINT('Ctrl Pts',(126.969395338088,-32.2583030029975,18.3432084744711));
#20829=CARTESIAN_POINT('Ctrl Pts',(127.052007852507,-32.1721797620218,18.3373921173392));
#20830=CARTESIAN_POINT('Ctrl Pts',(127.134537688124,-32.0861427133913,18.3315815812315));
#20831=CARTESIAN_POINT('Ctrl Pts',(127.220922330196,-32.0036327932832,18.3257710451238));
#20832=CARTESIAN_POINT('Ctrl Pts',(127.310825365669,-31.9250097908984,18.3199605090161));
#20833=CARTESIAN_POINT('Ctrl Pts',(127.40412897821,-31.8434128780386,18.3139301897193));
#20834=CARTESIAN_POINT('Ctrl Pts',(127.501222124778,-31.7660030829177,18.3078998704225));
#20835=CARTESIAN_POINT('Ctrl Pts',(127.601686289747,-31.6931410149187,18.3018695511257));
#20836=CARTESIAN_POINT('Ctrl Pts',(127.698379978124,-31.6230135012949,18.2960655531024));
#20837=CARTESIAN_POINT('Ctrl Pts',(127.79819585213,-31.5570987701424,18.2902615550791));
#20838=CARTESIAN_POINT('Ctrl Pts',(127.900727523391,-31.4956769456922,18.2844575570558));
#20839=CARTESIAN_POINT('Ctrl Pts',(128.003244058942,-31.4342641883224,18.2786544158178));
#20840=CARTESIAN_POINT('Ctrl Pts',(128.10847524429,-31.3773432284515,18.2728512745798));
#20841=CARTESIAN_POINT('Ctrl Pts',(128.215987278031,-31.3251498523268,18.2670481333418));
#20842=CARTESIAN_POINT('Ctrl Pts',(128.323508810868,-31.2729518647198,18.2612444793744));
#20843=CARTESIAN_POINT('Ctrl Pts',(128.433311225432,-31.2254824696792,18.2554408254069));
#20844=CARTESIAN_POINT('Ctrl Pts',(128.544938375596,-31.1829303557327,18.2496371714394));
#20845=CARTESIAN_POINT('Ctrl Pts',(128.656601729342,-31.1403644410311,18.2438316351963));
#20846=CARTESIAN_POINT('Ctrl Pts',(128.770090614322,-31.1027191244947,18.2380260989532));
#20847=CARTESIAN_POINT('Ctrl Pts',(128.884931888289,-31.0701338310006,18.2322205627101));
#20848=CARTESIAN_POINT('Ctrl Pts',(128.999900331694,-31.0375124541951,18.2264085977088));
#20849=CARTESIAN_POINT('Ctrl Pts',(129.116223760316,-31.0099623964539,18.2205966327076));
#20850=CARTESIAN_POINT('Ctrl Pts',(129.233416797189,-30.987572406489,18.2147846677063));
#20851=CARTESIAN_POINT('Ctrl Pts',(129.350686805802,-30.9651677109024,18.2089688854385));
#20852=CARTESIAN_POINT('Ctrl Pts',(129.468827157024,-30.947929891404,18.2031531031708));
#20853=CARTESIAN_POINT('Ctrl Pts',(129.587346928516,-30.9358958622355,18.197337320903));
#20854=CARTESIAN_POINT('Ctrl Pts',(129.706036445829,-30.9238445977472,18.1915132091833));
#20855=CARTESIAN_POINT('Ctrl Pts',(129.82510606183,-30.9170120225813,18.1856890974636));
#20856=CARTESIAN_POINT('Ctrl Pts',(129.944064288009,-30.9153829804835,18.1798649857439));
#20857=CARTESIAN_POINT('Ctrl Pts',(129.975601637482,-30.9149511005572,18.1783209391271));
#20858=CARTESIAN_POINT('Ctrl Pts',(130.007131185099,-30.914884667119,18.1767768925103));
#20859=CARTESIAN_POINT('Ctrl Pts',(130.038643847061,-30.9151827882897,18.1752328458935));
#20860=CARTESIAN_POINT('Ctrl Pts',(130.157465221301,-30.9163068814317,18.1694108768983));
#20861=CARTESIAN_POINT('Ctrl Pts',(130.276429325207,-30.9226216024877,18.1635889079031));
#20862=CARTESIAN_POINT('Ctrl Pts',(130.395046111187,-30.9341466369241,18.1577669389079));
#20863=CARTESIAN_POINT('Ctrl Pts',(130.513522711005,-30.9456580506041,18.1519518505534));
#20864=CARTESIAN_POINT('Ctrl Pts',(130.631652406412,-30.9623674952217,18.1461367621989));
#20865=CARTESIAN_POINT('Ctrl Pts',(130.748944700955,-30.9842426822688,18.1403216738444));
#20866=CARTESIAN_POINT('Ctrl Pts',(130.866126084286,-31.0060971842101,18.1345120842186));
#20867=CARTESIAN_POINT('Ctrl Pts',(130.982471242487,-31.0331076396458,18.1287024945928));
#20868=CARTESIAN_POINT('Ctrl Pts',(131.097494992829,-31.0651899994134,18.122892904967));
#20869=CARTESIAN_POINT('Ctrl Pts',(131.212437145711,-31.0972496000637,18.1170874366443));
#20870=CARTESIAN_POINT('Ctrl Pts',(131.326059363574,-31.1343738378891,18.1112819683217));
#20871=CARTESIAN_POINT('Ctrl Pts',(131.437887480208,-31.1764277704924,18.1054764999991));
#20872=CARTESIAN_POINT('Ctrl Pts',(131.549670783362,-31.2184648505982,18.0996733581329));
#20873=CARTESIAN_POINT('Ctrl Pts',(131.659661033301,-31.2654275536267,18.0938702162667));
#20874=CARTESIAN_POINT('Ctrl Pts',(131.767400549396,-31.3171315122592,18.0880670744004));
#20875=CARTESIAN_POINT('Ctrl Pts',(131.875115307195,-31.3688235894393,18.0822652660831));
#20876=CARTESIAN_POINT('Ctrl Pts',(131.980579993813,-31.4252545745619,18.0764634577657));
#20877=CARTESIAN_POINT('Ctrl Pts',(132.083358870215,-31.4861928314297,18.0706616494483));
#20878=CARTESIAN_POINT('Ctrl Pts',(132.186158067372,-31.5471431366042,18.064858694036));
#20879=CARTESIAN_POINT('Ctrl Pts',(132.286270042872,-31.6126022843173,18.0590557386236));
#20880=CARTESIAN_POINT('Ctrl Pts',(132.383285852153,-31.6822939330125,18.0532527832113));
#20881=CARTESIAN_POINT('Ctrl Pts',(132.418320364943,-31.7074610988143,18.0511572101586));
#20882=CARTESIAN_POINT('Ctrl Pts',(132.452951391226,-31.7331798151592,18.049061637106));
#20883=CARTESIAN_POINT('Ctrl Pts',(132.487160670875,-31.7594357285724,18.0469660640533));
#20884=CARTESIAN_POINT('Ctrl Pts',(132.487160670875,-31.7594357285724,19.2967873947729));
#20885=CARTESIAN_POINT('Ctrl Pts',(132.581876164488,-31.8321306763978,19.2909824707339));
#20886=CARTESIAN_POINT('Ctrl Pts',(132.673459485987,-31.9090257878229,19.2851775466948));
#20887=CARTESIAN_POINT('Ctrl Pts',(132.761523547418,-31.9898151722764,19.2793726226558));
#20888=CARTESIAN_POINT('Ctrl Pts',(132.849563241322,-32.0705822021225,19.2735693048525));
#20889=CARTESIAN_POINT('Ctrl Pts',(132.93408531082,-32.15524108653,19.2677659870493));
#20890=CARTESIAN_POINT('Ctrl Pts',(133.01473686711,-32.2434466045282,19.261962669246));
#20891=CARTESIAN_POINT('Ctrl Pts',(133.095385140938,-32.3316485326231,19.2561595876337));
#20892=CARTESIAN_POINT('Ctrl Pts',(133.172162939408,-32.4233965057908,19.2503565060214));
#20893=CARTESIAN_POINT('Ctrl Pts',(133.244755719231,-32.5183099866179,19.2445534244092));
#20894=CARTESIAN_POINT('Ctrl Pts',(133.317362676565,-32.6132420042339,19.2387492094437));
#20895=CARTESIAN_POINT('Ctrl Pts',(133.385782741859,-32.7113404345906,19.2329449944782));
#20896=CARTESIAN_POINT('Ctrl Pts',(133.449743380949,-32.8121938829971,19.2271407795127));
#20897=CARTESIAN_POINT('Ctrl Pts',(133.513770830608,-32.9131526786342,19.2213305017107));
#20898=CARTESIAN_POINT('Ctrl Pts',(133.57332933159,-33.0168718945394,19.2155202239086));
#20899=CARTESIAN_POINT('Ctrl Pts',(133.628191087686,-33.1229133128067,19.2097099461066));
#20900=CARTESIAN_POINT('Ctrl Pts',(133.683082530687,-33.2290121124242,19.2038965242351));
#20901=CARTESIAN_POINT('Ctrl Pts',(133.73327199399,-33.3374352474132,19.1980831023636));
#20902=CARTESIAN_POINT('Ctrl Pts',(133.778579567858,-33.4477237844481,19.1922696804921));
#20903=CARTESIAN_POINT('Ctrl Pts',(133.823958924307,-33.5581870559732,19.1864470481864));
#20904=CARTESIAN_POINT('Ctrl Pts',(133.864440800237,-33.6705212498169,19.1806244158808));
#20905=CARTESIAN_POINT('Ctrl Pts',(133.899894794839,-33.784251017195,19.1748017835751));
#20906=CARTESIAN_POINT('Ctrl Pts',(133.928658559913,-33.8765197826057,19.170077891962));
#20907=CARTESIAN_POINT('Ctrl Pts',(133.954113889628,-33.9697067625727,19.1653540003488));
#20908=CARTESIAN_POINT('Ctrl Pts',(133.976216025045,-34.0635539939876,19.1606301087357));
#20909=CARTESIAN_POINT('Ctrl Pts',(134.00346347904,-34.1792486122797,19.1548065076683));
#20910=CARTESIAN_POINT('Ctrl Pts',(134.025701189129,-34.2963199975551,19.148982906601));
#20911=CARTESIAN_POINT('Ctrl Pts',(134.042793156588,-34.4142965826944,19.1431593055336));
#20912=CARTESIAN_POINT('Ctrl Pts',(134.059863559868,-34.5321243219905,19.1373430518463));
#20913=CARTESIAN_POINT('Ctrl Pts',(134.071801075234,-34.6508545890837,19.1315267981591));
#20914=CARTESIAN_POINT('Ctrl Pts',(134.078520127177,-34.7700031038992,19.1257105444718));
#20915=CARTESIAN_POINT('Ctrl Pts',(134.085232453251,-34.8890323493252,19.1199001129387));
#20916=CARTESIAN_POINT('Ctrl Pts',(134.086736685062,-35.0084786042326,19.1140896814056));
#20917=CARTESIAN_POINT('Ctrl Pts',(134.082998806176,-35.1278504938013,19.1082792498726));
#20918=CARTESIAN_POINT('Ctrl Pts',(134.079119447478,-35.2517406444073,19.1022488918015));
#20919=CARTESIAN_POINT('Ctrl Pts',(134.069593242568,-35.375550245363,19.0962185337304));
#20920=CARTESIAN_POINT('Ctrl Pts',(134.054441532247,-35.4987272416763,19.0901881756594));
#20921=CARTESIAN_POINT('Ctrl Pts',(134.039858835987,-35.6172783943498,19.0843842843343));
#20922=CARTESIAN_POINT('Ctrl Pts',(134.020065594749,-35.7352431580727,19.0785803930091));
#20923=CARTESIAN_POINT('Ctrl Pts',(133.995133781718,-35.8521332443793,19.072776501684));
#20924=CARTESIAN_POINT('Ctrl Pts',(133.970205651734,-35.9690060631193,19.0669734677377));
#20925=CARTESIAN_POINT('Ctrl Pts',(133.940140544713,-36.0848041209145,19.0611704337913));
#20926=CARTESIAN_POINT('Ctrl Pts',(133.905061562704,-36.1990492865157,19.055367399845));
#20927=CARTESIAN_POINT('Ctrl Pts',(133.869979484137,-36.3133045369806,19.0495638536424));
#20928=CARTESIAN_POINT('Ctrl Pts',(133.829882770461,-36.4260062323352,19.0437603074397));
#20929=CARTESIAN_POINT('Ctrl Pts',(133.784944217865,-36.5366919885432,19.0379567612371));
#20930=CARTESIAN_POINT('Ctrl Pts',(133.739991092992,-36.6474136369469,19.0321513331119));
#20931=CARTESIAN_POINT('Ctrl Pts',(133.690193160215,-36.7561176679729,19.0263459049867));
#20932=CARTESIAN_POINT('Ctrl Pts',(133.635770849495,-36.8623628352079,19.0205404768616));
#20933=CARTESIAN_POINT('Ctrl Pts',(133.581288272842,-36.9687256557357,19.0147286199477));
#20934=CARTESIAN_POINT('Ctrl Pts',(133.522171282718,-37.0726238137133,19.0089167630338));
#20935=CARTESIAN_POINT('Ctrl Pts',(133.458685731352,-37.1736416474993,19.0031049061199));
#20936=CARTESIAN_POINT('Ctrl Pts',(133.395158483429,-37.2747258285993,18.9972892320474));
#20937=CARTESIAN_POINT('Ctrl Pts',(133.327257191844,-37.3729255829226,18.9914735579748));
#20938=CARTESIAN_POINT('Ctrl Pts',(133.255289419488,-37.4678565183916,18.9856578839023));
#20939=CARTESIAN_POINT('Ctrl Pts',(133.183218563532,-37.5629234289266,18.9798338797037));
#20940=CARTESIAN_POINT('Ctrl Pts',(133.107069860903,-37.6547118622023,18.974009875505));
#20941=CARTESIAN_POINT('Ctrl Pts',(133.027189364268,-37.7428725002925,18.9681858713064));
#20942=CARTESIAN_POINT('Ctrl Pts',(133.005997570519,-37.7662609635338,18.9666407995933));
#20943=CARTESIAN_POINT('Ctrl Pts',(132.984543318965,-37.78939431269,18.9650957278803));
#20944=CARTESIAN_POINT('Ctrl Pts',(132.962833467165,-37.8122664962353,18.9635506561672));
#20945=CARTESIAN_POINT('Ctrl Pts',(132.881005718716,-37.8984752506235,18.9577270448116));
#20946=CARTESIAN_POINT('Ctrl Pts',(132.795280311605,-37.9812486725524,18.951903433456));
#20947=CARTESIAN_POINT('Ctrl Pts',(132.705977104063,-38.0602145206319,18.9460798221004));
#20948=CARTESIAN_POINT('Ctrl Pts',(132.616786563406,-38.1390807436659,18.9402635579406));
#20949=CARTESIAN_POINT('Ctrl Pts',(132.524027503426,-38.2141486792318,18.9344472937808));
#20950=CARTESIAN_POINT('Ctrl Pts',(132.428058055112,-38.285081289863,18.928631029621));
#20951=CARTESIAN_POINT('Ctrl Pts',(132.332184670638,-38.3559428981164,18.922820587446));
#20952=CARTESIAN_POINT('Ctrl Pts',(132.233107617269,-38.4226771749324,18.9170101452711));
#20953=CARTESIAN_POINT('Ctrl Pts',(132.13121922248,-38.4849863164338,18.9111997030961));
#20954=CARTESIAN_POINT('Ctrl Pts',(132.025474584566,-38.5496537166859,18.9051693489504));
#20955=CARTESIAN_POINT('Ctrl Pts',(131.91670193106,-38.6095541045878,18.8991389948047));
#20956=CARTESIAN_POINT('Ctrl Pts',(131.805374681896,-38.6644027150367,18.8931086406589));
#20957=CARTESIAN_POINT('Ctrl Pts',(131.698227993033,-38.7171916507418,18.8873047383418));
#20958=CARTESIAN_POINT('Ctrl Pts',(131.588715508498,-38.765301179574,18.8815008360246));
#20959=CARTESIAN_POINT('Ctrl Pts',(131.477285073716,-38.8085238362096,18.8756969337074));
#20960=CARTESIAN_POINT('Ctrl Pts',(131.365871097844,-38.8517401086123,18.8698938886598));
#20961=CARTESIAN_POINT('Ctrl Pts',(131.252540115701,-38.89007079666,18.8640908436121));
#20962=CARTESIAN_POINT('Ctrl Pts',(131.137759504369,-38.9233567656049,18.8582877985644));
#20963=CARTESIAN_POINT('Ctrl Pts',(131.022968759016,-38.9566456733799,18.8524842411637));
#20964=CARTESIAN_POINT('Ctrl Pts',(130.9067285222,-38.9848888627538,18.8466806837631));
#20965=CARTESIAN_POINT('Ctrl Pts',(130.789520240903,-39.0079773937991,18.8408771263625));
#20966=CARTESIAN_POINT('Ctrl Pts',(130.67227395072,-39.0310734121083,18.8350716869553));
#20967=CARTESIAN_POINT('Ctrl Pts',(130.554059392165,-39.049011368817,18.8292662475481));
#20968=CARTESIAN_POINT('Ctrl Pts',(130.435366444342,-39.0617337504003,18.823460808141));
#20969=CARTESIAN_POINT('Ctrl Pts',(130.316542057763,-39.0744702205544,18.817648939879));
#20970=CARTESIAN_POINT('Ctrl Pts',(130.197238630717,-39.0819795433496,18.8118370716169));
#20971=CARTESIAN_POINT('Ctrl Pts',(130.077949542718,-39.0842562197774,18.8060252033549));
#20972=CARTESIAN_POINT('Ctrl Pts',(129.958582106154,-39.0865343915166,18.8002095178826));
#20973=CARTESIAN_POINT('Ctrl Pts',(129.839229434664,-39.0835730825584,18.7943938324103));
#20974=CARTESIAN_POINT('Ctrl Pts',(129.720381619031,-39.0754188203207,18.7885781469381));
#20975=CARTESIAN_POINT('Ctrl Pts',(129.601363571389,-39.0672528783022,18.7827541313521));
#20976=CARTESIAN_POINT('Ctrl Pts',(129.482852227254,-39.0538791825038,18.7769301157661));
#20977=CARTESIAN_POINT('Ctrl Pts',(129.365329441072,-39.0353956784472,18.7711061001802));
#20978=CARTESIAN_POINT('Ctrl Pts',(129.334153588154,-39.0304924675669,18.7695611346531));
#20979=CARTESIAN_POINT('Ctrl Pts',(129.303047226244,-39.0252299498191,18.7680161691259));
#20980=CARTESIAN_POINT('Ctrl Pts',(129.27201917389,-39.0196105429278,18.7664712035988));
#20981=CARTESIAN_POINT('Ctrl Pts',(129.155063461701,-38.9984290092772,18.7606476816623));
#20982=CARTESIAN_POINT('Ctrl Pts',(129.038844346339,-38.9721046129996,18.7548241597257));
#20983=CARTESIAN_POINT('Ctrl Pts',(128.923848482773,-38.9407008148259,18.7490006377892));
#20984=CARTESIAN_POINT('Ctrl Pts',(128.808997706935,-38.9093366381272,18.743184463261));
#20985=CARTESIAN_POINT('Ctrl Pts',(128.695367503658,-38.8729059126443,18.7373682887328));
#20986=CARTESIAN_POINT('Ctrl Pts',(128.583436065122,-38.8315234070018,18.7315521142046));
#20987=CARTESIAN_POINT('Ctrl Pts',(128.471616671848,-38.7901823259472,18.7257417617654));
#20988=CARTESIAN_POINT('Ctrl Pts',(128.361493041206,-38.7438994664882,18.7199314093263));
#20989=CARTESIAN_POINT('Ctrl Pts',(128.253529297619,-38.6928397048511,18.7141210568872));
#20990=CARTESIAN_POINT('Ctrl Pts',(128.141477018012,-38.6398463341364,18.7080906691431));
#20991=CARTESIAN_POINT('Ctrl Pts',(128.031751879363,-38.5817072295166,18.7020602813991));
#20992=CARTESIAN_POINT('Ctrl Pts',(127.924851583423,-38.5186622527854,18.6960298936551));
#20993=CARTESIAN_POINT('Ctrl Pts',(127.821967765316,-38.4579860136645,18.6902260807628));
#20994=CARTESIAN_POINT('Ctrl Pts',(127.721700731998,-38.3927661261518,18.6844222678704));
#20995=CARTESIAN_POINT('Ctrl Pts',(127.624469484752,-38.3232634218679,18.6786184549781));
#20996=CARTESIAN_POINT('Ctrl Pts',(127.527252594828,-38.2537709804647,18.6728154990861));
#20997=CARTESIAN_POINT('Ctrl Pts',(127.433070931625,-38.1799972173488,18.6670125431941));
#20998=CARTESIAN_POINT('Ctrl Pts',(127.3423137808,-38.1022457930139,18.6612095873021));
#20999=CARTESIAN_POINT('Ctrl Pts',(127.251548611156,-38.0244874989774,18.6554061186918));
#21000=CARTESIAN_POINT('Ctrl Pts',(127.164208865598,-37.9427511106475,18.6496026500815));
#21001=CARTESIAN_POINT('Ctrl Pts',(127.080649560863,-37.85737957113,18.6437991814713));
#21002=CARTESIAN_POINT('Ctrl Pts',(126.997063152035,-37.7719803396865,18.6379938303926));
#21003=CARTESIAN_POINT('Ctrl Pts',(126.917259908267,-37.6829439037049,18.632188479314));
#21004=CARTESIAN_POINT('Ctrl Pts',(126.841556456764,-37.5906484485915,18.6263831282353));
#21005=CARTESIAN_POINT('Ctrl Pts',(126.765769156444,-37.4982507674301,18.6205713471749));
#21006=CARTESIAN_POINT('Ctrl Pts',(126.694090971559,-37.4025871778309,18.6147595661144));
#21007=CARTESIAN_POINT('Ctrl Pts',(126.6267969445,-37.3040673050859,18.6089477850539));
#21008=CARTESIAN_POINT('Ctrl Pts',(126.55945871193,-37.2054827145426,18.603132186229));
#21009=CARTESIAN_POINT('Ctrl Pts',(126.496510587499,-37.1040384503452,18.597316587404));
#21010=CARTESIAN_POINT('Ctrl Pts',(126.438182297114,-37.0001699056351,18.591500988579));
#21011=CARTESIAN_POINT('Ctrl Pts',(126.379770444036,-36.8961525560254,18.5856770581691));
#21012=CARTESIAN_POINT('Ctrl Pts',(126.325991818649,-36.7897043569867,18.5798531277592));
#21013=CARTESIAN_POINT('Ctrl Pts',(126.277028627127,-36.6812819979907,18.5740291973493));
#21014=CARTESIAN_POINT('Ctrl Pts',(126.264032582858,-36.6525040173584,18.5724833819097));
#21015=CARTESIAN_POINT('Ctrl Pts',(126.251375516676,-36.6235870446739,18.57093756647));
#21016=CARTESIAN_POINT('Ctrl Pts',(126.239060244978,-36.5945397953937,18.5693917510304));
#21017=CARTESIAN_POINT('Ctrl Pts',(126.18609618114,-36.4696168214741,18.5627436908306));
#21018=CARTESIAN_POINT('Ctrl Pts',(126.139308118626,-36.3419289321288,18.5560956306308));
#21019=CARTESIAN_POINT('Ctrl Pts',(126.098961571492,-36.2120743291181,18.549447570431));
#21020=CARTESIAN_POINT('Ctrl Pts',(126.059996554439,-36.0866661546856,18.5430271504086));
#21021=CARTESIAN_POINT('Ctrl Pts',(126.027039355238,-35.9592374719865,18.5366067303862));
#21022=CARTESIAN_POINT('Ctrl Pts',(126.000282119951,-35.8303504561443,18.5301863103638));
#21023=CARTESIAN_POINT('Ctrl Pts',(125.973599394212,-35.7018223455884,18.5237837689669));
#21024=CARTESIAN_POINT('Ctrl Pts',(125.953082273561,-35.5718442467167,18.51738122757));
#21025=CARTESIAN_POINT('Ctrl Pts',(125.938873294589,-35.4409930641106,18.5109786861731));
#21026=CARTESIAN_POINT('Ctrl Pts',(125.92472284485,-35.3106808800761,18.5046025179476));
#21027=CARTESIAN_POINT('Ctrl Pts',(125.916828774108,-35.1795030367883,18.4982263497221));
#21028=CARTESIAN_POINT('Ctrl Pts',(125.915282546399,-35.0480450231657,18.4918501814966));
#21029=CARTESIAN_POINT('Ctrl Pts',(125.915101870735,-35.0326842429822,18.4911051305421));
#21030=CARTESIAN_POINT('Ctrl Pts',(125.91500781049,-35.0173196526052,18.4903600795876));
#21031=CARTESIAN_POINT('Ctrl Pts',(125.915000466472,-35.0019521977368,18.4896150286331));
#21032=CARTESIAN_POINT('Origin',(130.,-35.,32.7603849714045));
#21033=CARTESIAN_POINT('',(132.487160670875,-31.7594357285724,20.546920387862));
#21034=CARTESIAN_POINT('',(132.487160670875,-31.7594357285724,20.4426725214427));
#21035=CARTESIAN_POINT('',(132.487160670875,-31.7594357285724,32.7603849714045));
#21036=CARTESIAN_POINT('',(125.915000768169,-34.9974948168759,19.6353849713624));
#21037=CARTESIAN_POINT('Ctrl Pts',(132.487160670875,-31.7594357285724,20.4426725214427));
#21038=CARTESIAN_POINT('Ctrl Pts',(132.581973816846,-31.8322056254144,20.4368690159672));
#21039=CARTESIAN_POINT('Ctrl Pts',(132.673580943561,-31.9091326155342,20.4310655104917));
#21040=CARTESIAN_POINT('Ctrl Pts',(132.761608938129,-31.9898935113773,20.4252620050163));
#21041=CARTESIAN_POINT('Ctrl Pts',(132.849664876522,-32.0706800441597,20.4194566572616));
#21042=CARTESIAN_POINT('Ctrl Pts',(132.934139122451,-32.1553026271649,20.4136513095069));
#21043=CARTESIAN_POINT('Ctrl Pts',(133.014694978785,-32.24340079357,20.4078459617522));
#21044=CARTESIAN_POINT('Ctrl Pts',(133.095339789209,-32.3315962426887,20.4020342034217));
#21045=CARTESIAN_POINT('Ctrl Pts',(133.172057297195,-32.4232746347158,20.3962224450911));
#21046=CARTESIAN_POINT('Ctrl Pts',(133.244550616061,-32.518041841647,20.3904106867605));
#21047=CARTESIAN_POINT('Ctrl Pts',(133.317091103821,-32.6128707103202,20.3845951469199));
#21048=CARTESIAN_POINT('Ctrl Pts',(133.385401695484,-32.7107920623311,20.3787796070793));
#21049=CARTESIAN_POINT('Ctrl Pts',(133.449229353136,-32.8113835718737,20.3729640672387));
#21050=CARTESIAN_POINT('Ctrl Pts',(133.513148928066,-32.9121199417804,20.3671401525241));
#21051=CARTESIAN_POINT('Ctrl Pts',(133.572572480076,-33.0155337916903,20.3613162378095));
#21052=CARTESIAN_POINT('Ctrl Pts',(133.627293255973,-33.1211789241196,20.3554923230949));
#21053=CARTESIAN_POINT('Ctrl Pts',(133.643396625479,-33.1522684431573,20.3537784466178));
#21054=CARTESIAN_POINT('Ctrl Pts',(133.65909304477,-33.1835510716237,20.3520645701407));
#21055=CARTESIAN_POINT('Ctrl Pts',(133.67437805383,-33.2150151492148,20.3503506936635));
#21056=CARTESIAN_POINT('Ctrl Pts',(133.726315092385,-33.3219271572154,20.3445271008662));
#21057=CARTESIAN_POINT('Ctrl Pts',(133.773665842176,-33.4312802395044,20.3387035080688));
#21058=CARTESIAN_POINT('Ctrl Pts',(133.816194276671,-33.5426440919575,20.3328799152715));
#21059=CARTESIAN_POINT('Ctrl Pts',(133.858669055222,-33.6538674423517,20.3270636698024));
#21060=CARTESIAN_POINT('Ctrl Pts',(133.896333475151,-33.7670961389996,20.3212474243333));
#21061=CARTESIAN_POINT('Ctrl Pts',(133.928997921894,-33.8818764246515,20.3154311788642));
#21062=CARTESIAN_POINT('Ctrl Pts',(133.961629671348,-33.9965418146112,20.3096207554886));
#21063=CARTESIAN_POINT('Ctrl Pts',(133.989271293318,-34.1127553132915,20.3038103321129));
#21064=CARTESIAN_POINT('Ctrl Pts',(134.011781924575,-34.2300449430975,20.2979999087373));
#21065=CARTESIAN_POINT('Ctrl Pts',(134.035144634565,-34.3517742528843,20.2919695475855));
#21066=CARTESIAN_POINT('Ctrl Pts',(134.052980079544,-34.4746623527927,20.2859391864338));
#21067=CARTESIAN_POINT('Ctrl Pts',(134.065188110948,-34.5981659265273,20.279908825282));
#21068=CARTESIAN_POINT('Ctrl Pts',(134.076937654409,-34.7170311685227,20.2741049419129));
#21069=CARTESIAN_POINT('Ctrl Pts',(134.083474806984,-34.8364660453647,20.2683010585438));
#21070=CARTESIAN_POINT('Ctrl Pts',(134.084762795524,-34.9559783655528,20.2624971751747));
#21071=CARTESIAN_POINT('Ctrl Pts',(134.086050593816,-35.0754730325862,20.2566941490967));
#21072=CARTESIAN_POINT('Ctrl Pts',(134.082090765608,-35.1950447120137,20.2508911230188));
#21073=CARTESIAN_POINT('Ctrl Pts',(134.072898649722,-35.3141999189945,20.2450880969408));
#21074=CARTESIAN_POINT('Ctrl Pts',(134.063705722259,-35.4333656462495,20.2392845585107));
#21075=CARTESIAN_POINT('Ctrl Pts',(134.049279620036,-35.5521144208015,20.2334810200806));
#21076=CARTESIAN_POINT('Ctrl Pts',(134.029687618902,-35.6699572330127,20.2276774816504));
#21077=CARTESIAN_POINT('Ctrl Pts',(134.010089264288,-35.7878382604115,20.2218720611937));
#21078=CARTESIAN_POINT('Ctrl Pts',(133.985321746008,-35.9048123385787,20.216066640737));
#21079=CARTESIAN_POINT('Ctrl Pts',(133.955503447826,-36.0204006439795,20.2102612202802));
#21080=CARTESIAN_POINT('Ctrl Pts',(133.925652128563,-36.1361169530231,20.204449370843));
#21081=CARTESIAN_POINT('Ctrl Pts',(133.890738966784,-36.2504440304432,20.1986375214057));
#21082=CARTESIAN_POINT('Ctrl Pts',(133.850932270891,-36.3629180624723,20.1928256719684));
#21083=CARTESIAN_POINT('Ctrl Pts',(133.811099429694,-36.4754659681972,20.1870100052696));
#21084=CARTESIAN_POINT('Ctrl Pts',(133.766366806055,-36.5861580269391,20.1811943385708));
#21085=CARTESIAN_POINT('Ctrl Pts',(133.716950257289,-36.6945517946766,20.175378671872));
#21086=CARTESIAN_POINT('Ctrl Pts',(133.667462924501,-36.8031008251138,20.1695546748408));
#21087=CARTESIAN_POINT('Ctrl Pts',(133.613278460185,-36.9093446313024,20.1637306778096));
#21088=CARTESIAN_POINT('Ctrl Pts',(133.554657961643,-37.0128665568614,20.1579066807784));
#21089=CARTESIAN_POINT('Ctrl Pts',(133.539105539269,-37.0403316373585,20.1563615342173));
#21090=CARTESIAN_POINT('Ctrl Pts',(133.523241105197,-37.0676052971867,20.1548163876562));
#21091=CARTESIAN_POINT('Ctrl Pts',(133.507070025072,-37.0946801281448,20.1532712410951));
#21092=CARTESIAN_POINT('Ctrl Pts',(133.446121885322,-37.1967240589228,20.1474476468881));
#21093=CARTESIAN_POINT('Ctrl Pts',(133.380618063255,-37.2962702566973,20.1416240526811));
#21094=CARTESIAN_POINT('Ctrl Pts',(133.31078907183,-37.3928854385135,20.1358004584741));
#21095=CARTESIAN_POINT('Ctrl Pts',(133.24104818012,-37.4893787258295,20.129984211602));
#21096=CARTESIAN_POINT('Ctrl Pts',(133.166993209679,-37.5829480242237,20.12416796473));
#21097=CARTESIAN_POINT('Ctrl Pts',(133.088899730329,-37.6731860122284,20.118351717858));
#21098=CARTESIAN_POINT('Ctrl Pts',(133.01088442307,-37.7633336714078,20.1125412930877));
#21099=CARTESIAN_POINT('Ctrl Pts',(132.928838914779,-37.8501563471065,20.1067308683174));
#21100=CARTESIAN_POINT('Ctrl Pts',(132.843080737952,-37.9332775043436,20.1009204435472));
#21101=CARTESIAN_POINT('Ctrl Pts',(132.754076447675,-38.0195449587201,20.0948900829213));
#21102=CARTESIAN_POINT('Ctrl Pts',(132.661073134648,-38.1018247753736,20.0888597222954));
#21103=CARTESIAN_POINT('Ctrl Pts',(132.564470314909,-38.1797353669689,20.0828293616696));
#21104=CARTESIAN_POINT('Ctrl Pts',(132.471495505345,-38.2547199526789,20.0770254769351));
#21105=CARTESIAN_POINT('Ctrl Pts',(132.375187025567,-38.3256572963924,20.0712215922007));
#21106=CARTESIAN_POINT('Ctrl Pts',(132.275936372773,-38.3922468405305,20.0654177074662));
#21107=CARTESIAN_POINT('Ctrl Pts',(132.176700380505,-38.4588265485846,20.059614680036));
#21108=CARTESIAN_POINT('Ctrl Pts',(132.074523418492,-38.5210595068002,20.0538116526058));
#21109=CARTESIAN_POINT('Ctrl Pts',(131.969826631532,-38.5786880335823,20.0480086251756));
#21110=CARTESIAN_POINT('Ctrl Pts',(131.865120601104,-38.6363216482714,20.0422050854077));
#21111=CARTESIAN_POINT('Ctrl Pts',(131.757894661149,-38.6893498263612,20.0364015456399));
#21112=CARTESIAN_POINT('Ctrl Pts',(131.648594683529,-38.7375607780262,20.030598005872));
#21113=CARTESIAN_POINT('Ctrl Pts',(131.539259261383,-38.7857873638604,20.0247925840935));
#21114=CARTESIAN_POINT('Ctrl Pts',(131.42784883737,-38.8291934517726,20.018987162315));
#21115=CARTESIAN_POINT('Ctrl Pts',(131.314828779498,-38.8676155807685,20.0131817405366));
#21116=CARTESIAN_POINT('Ctrl Pts',(131.201683562701,-38.9060802586044,20.0073698898076));
#21117=CARTESIAN_POINT('Ctrl Pts',(131.086925540826,-38.9395498291027,20.0015580390787));
#21118=CARTESIAN_POINT('Ctrl Pts',(130.971034895023,-38.9679108146036,19.9957461883498));
#21119=CARTESIAN_POINT('Ctrl Pts',(130.855068131805,-38.9962904277069,19.9899305203754));
#21120=CARTESIAN_POINT('Ctrl Pts',(130.73796766273,-39.0195546941866,19.984114852401));
#21121=CARTESIAN_POINT('Ctrl Pts',(130.620221860504,-39.0376416190337,19.9782991844266));
#21122=CARTESIAN_POINT('Ctrl Pts',(130.502307400478,-39.0557544513943,19.9724751861529));
#21123=CARTESIAN_POINT('Ctrl Pts',(130.383746166805,-39.0686750961732,19.9666511878792));
#21124=CARTESIAN_POINT('Ctrl Pts',(130.265029763085,-39.0763935316256,19.9608271896056));
#21125=CARTESIAN_POINT('Ctrl Pts',(130.233533751809,-39.0784412682687,19.9592820559126));
#21126=CARTESIAN_POINT('Ctrl Pts',(130.20202680599,-39.0801231235685,19.9577369222196));
#21127=CARTESIAN_POINT('Ctrl Pts',(130.170518062655,-39.0814395242743,19.9561917885266));
#21128=CARTESIAN_POINT('Ctrl Pts',(130.051761867813,-39.0864010277223,19.9503681923283));
#21129=CARTESIAN_POINT('Ctrl Pts',(129.932597446586,-39.0861831196748,19.94454459613));
#21130=CARTESIAN_POINT('Ctrl Pts',(129.813513543482,-39.0807410848442,19.9387209999317));
#21131=CARTESIAN_POINT('Ctrl Pts',(129.694579882059,-39.0753059159329,19.9329047510479));
#21132=CARTESIAN_POINT('Ctrl Pts',(129.575726941025,-39.0646597480532,19.9270885021641));
#21133=CARTESIAN_POINT('Ctrl Pts',(129.457446449946,-39.0488097813214,19.9212722532804));
#21134=CARTESIAN_POINT('Ctrl Pts',(129.339284358021,-39.0329756804576,19.9154618264805));
#21135=CARTESIAN_POINT('Ctrl Pts',(129.221693978482,-39.0119481973629,19.9096513996806));
#21136=CARTESIAN_POINT('Ctrl Pts',(129.105164294347,-38.9857865045544,19.9038409728807));
#21137=CARTESIAN_POINT('Ctrl Pts',(128.984223792851,-38.9586345537728,19.897810613009));
#21138=CARTESIAN_POINT('Ctrl Pts',(128.864426318758,-38.9259520597147,19.8917802531372));
#21139=CARTESIAN_POINT('Ctrl Pts',(128.746310020357,-38.8878639938842,19.8857498932654));
#21140=CARTESIAN_POINT('Ctrl Pts',(128.632629636571,-38.8512063437561,19.8799460064703));
#21141=CARTESIAN_POINT('Ctrl Pts',(128.520506854486,-38.8095419542711,19.8741421196751));
#21142=CARTESIAN_POINT('Ctrl Pts',(128.410407656527,-38.7630335078993,19.86833823288));
#21143=CARTESIAN_POINT('Ctrl Pts',(128.300324721403,-38.7165319313245,19.8625352033812));
#21144=CARTESIAN_POINT('Ctrl Pts',(128.192265152028,-38.6651878796574,19.8567321738825));
#21145=CARTESIAN_POINT('Ctrl Pts',(128.086675322317,-38.6092123348132,19.8509291443837));
#21146=CARTESIAN_POINT('Ctrl Pts',(127.981076170194,-38.5532318479493,19.8451256025418));
#21147=CARTESIAN_POINT('Ctrl Pts',(127.877947552067,-38.4926192461628,19.8393220607));
#21148=CARTESIAN_POINT('Ctrl Pts',(127.77771101376,-38.427631348561,19.8335185188581));
#21149=CARTESIAN_POINT('Ctrl Pts',(127.677441970036,-38.3626223762214,19.8277130950023));
#21150=CARTESIAN_POINT('Ctrl Pts',(127.580067213783,-38.2932355083157,19.8219076711466));
#21151=CARTESIAN_POINT('Ctrl Pts',(127.485978557059,-38.2197703620652,19.8161022472909));
#21152=CARTESIAN_POINT('Ctrl Pts',(127.39178570626,-38.1462238602805,19.8102903944905));
#21153=CARTESIAN_POINT('Ctrl Pts',(127.300886540859,-38.0685903166835,19.8044785416901));
#21154=CARTESIAN_POINT('Ctrl Pts',(127.213639188317,-37.9872091368231,19.7986666888897));
#21155=CARTESIAN_POINT('Ctrl Pts',(127.12633453142,-37.9057745055292,19.7928510188448));
#21156=CARTESIAN_POINT('Ctrl Pts',(127.042686749539,-37.8205876265996,19.7870353487999));
#21157=CARTESIAN_POINT('Ctrl Pts',(126.963015401848,-37.732022977683,19.7812196787549));
#21158=CARTESIAN_POINT('Ctrl Pts',(126.883229934067,-37.6433314700399,19.7753956784281));
#21159=CARTESIAN_POINT('Ctrl Pts',(126.807432527555,-37.55125284963,19.7695716781012));
#21160=CARTESIAN_POINT('Ctrl Pts',(126.735901043608,-37.4561927861793,19.7637476777744));
#21161=CARTESIAN_POINT('Ctrl Pts',(126.716923659215,-37.4309732427707,19.7622025638356));
#21162=CARTESIAN_POINT('Ctrl Pts',(126.698246285856,-37.4055439965965,19.7606574498969));
#21163=CARTESIAN_POINT('Ctrl Pts',(126.679873575016,-37.3799129232232,19.7591123359582));
#21164=CARTESIAN_POINT('Ctrl Pts',(126.61011205585,-37.2825912687329,19.7532455100666));
#21165=CARTESIAN_POINT('Ctrl Pts',(126.544521954487,-37.1820446244611,19.7473786841751));
#21166=CARTESIAN_POINT('Ctrl Pts',(126.483412467191,-37.078662340086,19.7415118582836));
#21167=CARTESIAN_POINT('Ctrl Pts',(126.422382088058,-36.9754138873468,19.7356526271837));
#21168=CARTESIAN_POINT('Ctrl Pts',(126.36582098778,-36.8693374369891,19.7297933960838));
#21169=CARTESIAN_POINT('Ctrl Pts',(126.313996697074,-36.7608533870868,19.7239341649839));
#21170=CARTESIAN_POINT('Ctrl Pts',(126.262227895367,-36.6524854925888,19.7180812074455));
#21171=CARTESIAN_POINT('Ctrl Pts',(126.215185984591,-36.5417154858371,19.7122282499071));
#21172=CARTESIAN_POINT('Ctrl Pts',(126.173093650344,-36.4289901297627,19.7063752923687));
#21173=CARTESIAN_POINT('Ctrl Pts',(126.130548943974,-36.3150532987387,19.7004594322883));
#21174=CARTESIAN_POINT('Ctrl Pts',(126.093061051907,-36.1991191920976,19.694543572208));
#21175=CARTESIAN_POINT('Ctrl Pts',(126.060811055506,-36.0816725288085,19.6886277121276));
#21176=CARTESIAN_POINT('Ctrl Pts',(126.028952031247,-35.9656496912095,19.6827835710159));
#21177=CARTESIAN_POINT('Ctrl Pts',(126.002204712301,-35.8481511652892,19.6769394299042));
#21178=CARTESIAN_POINT('Ctrl Pts',(125.980694158762,-35.7296612601705,19.6710952887925));
#21179=CARTESIAN_POINT('Ctrl Pts',(125.958787640782,-35.6089902029473,19.6651435692279));
#21180=CARTESIAN_POINT('Ctrl Pts',(125.942312718397,-35.4872913124443,19.6591918496632));
#21181=CARTESIAN_POINT('Ctrl Pts',(125.93134717999,-35.3650879760073,19.6532401300985));
#21182=CARTESIAN_POINT('Ctrl Pts',(125.920381641583,-35.2428846395704,19.6472884105338));
#21183=CARTESIAN_POINT('Ctrl Pts',(125.914925531444,-35.1201772941067,19.6413366909692));
#21184=CARTESIAN_POINT('Ctrl Pts',(125.915000768169,-34.9974948177444,19.6353849714045));
#21185=CARTESIAN_POINT('Ctrl Pts',(125.915000768169,-34.9974948168759,19.6353849713624));
#21186=CARTESIAN_POINT('Ctrl Pts',(125.915083357695,-34.8628227653834,19.6288515991363));
#21187=CARTESIAN_POINT('Ctrl Pts',(125.921829701158,-34.7283970455392,19.6223182269103));
#21188=CARTESIAN_POINT('Ctrl Pts',(125.935142558186,-34.5948346291612,19.6157848546842));
#21189=CARTESIAN_POINT('Ctrl Pts',(125.948507987138,-34.4607447803019,19.6092256824403));
#21190=CARTESIAN_POINT('Ctrl Pts',(125.968491780673,-34.3275252624722,19.6026665101964));
#21191=CARTESIAN_POINT('Ctrl Pts',(125.994945663311,-34.1957831385947,19.5961073379525));
#21192=CARTESIAN_POINT('Ctrl Pts',(126.021539621642,-34.0633434282967,19.5895134343004));
#21193=CARTESIAN_POINT('Ctrl Pts',(126.05467226789,-33.9323969920297,19.5829195306483));
#21194=CARTESIAN_POINT('Ctrl Pts',(126.09414425753,-33.8035402560003,19.5763256269961));
#21195=CARTESIAN_POINT('Ctrl Pts',(126.122663682811,-33.7104382844833,19.5715613791273));
#21196=CARTESIAN_POINT('Ctrl Pts',(126.154491475401,-33.6184268020555,19.5667971312585));
#21197=CARTESIAN_POINT('Ctrl Pts',(126.189537223219,-33.5277233864641,19.5620328833897));
#21198=CARTESIAN_POINT('Ctrl Pts',(126.23237555984,-33.4168516347736,19.5562092823351));
#21199=CARTESIAN_POINT('Ctrl Pts',(126.280125989455,-33.3076723261669,19.5503856812804));
#21200=CARTESIAN_POINT('Ctrl Pts',(126.332634487578,-33.2006514516925,19.5445620802257));
#21201=CARTESIAN_POINT('Ctrl Pts',(126.385076738051,-33.0937656007214,19.5387458265509));
#21202=CARTESIAN_POINT('Ctrl Pts',(126.44226493884,-32.9890331308576,19.5329295728761));
#21203=CARTESIAN_POINT('Ctrl Pts',(126.503996271198,-32.8869020542812,19.5271133192013));
#21204=CARTESIAN_POINT('Ctrl Pts',(126.5656658096,-32.7848732123888,19.5213028876804));
#21205=CARTESIAN_POINT('Ctrl Pts',(126.631869222394,-32.685440930835,19.5154924561596));
#21206=CARTESIAN_POINT('Ctrl Pts',(126.702357131409,-32.5890299646765,19.5096820246388));
#21207=CARTESIAN_POINT('Ctrl Pts',(126.775513028668,-32.4889698148787,19.5036516665631));
#21208=CARTESIAN_POINT('Ctrl Pts',(126.853283971756,-32.3921646170861,19.4976213084873));
#21209=CARTESIAN_POINT('Ctrl Pts',(126.935340631508,-32.2990579504334,19.4915909504116));
#21210=CARTESIAN_POINT('Ctrl Pts',(127.014315698788,-32.2094478531512,19.4857870590981));
#21211=CARTESIAN_POINT('Ctrl Pts',(127.097260097743,-32.1232638377191,19.4799831677846));
#21212=CARTESIAN_POINT('Ctrl Pts',(127.183838716184,-32.0408682652616,19.4741792764712));
#21213=CARTESIAN_POINT('Ctrl Pts',(127.270404544818,-31.9584848646717,19.4683762425362));
#21214=CARTESIAN_POINT('Ctrl Pts',(127.360603229571,-31.8798890755223,19.4625732086013));
#21215=CARTESIAN_POINT('Ctrl Pts',(127.454063195155,-31.8054060061196,19.4567701746663));
#21216=CARTESIAN_POINT('Ctrl Pts',(127.547531410817,-31.7309163618041,19.4509666284748));
#21217=CARTESIAN_POINT('Ctrl Pts',(127.64426116035,-31.6605404135621,19.4451630822833));
#21218=CARTESIAN_POINT('Ctrl Pts',(127.743848745869,-31.5945622133882,19.4393595360918));
#21219=CARTESIAN_POINT('Ctrl Pts',(127.843468624772,-31.5285626183855,19.4335541079775));
#21220=CARTESIAN_POINT('Ctrl Pts',(127.945947842454,-31.4669638329767,19.4277486798632));
#21221=CARTESIAN_POINT('Ctrl Pts',(128.050855322594,-31.4100055673388,19.4219432517489));
#21222=CARTESIAN_POINT('Ctrl Pts',(128.155878974712,-31.3529842275098,19.4161313948455));
#21223=CARTESIAN_POINT('Ctrl Pts',(128.263335897692,-31.3006138598848,19.410319537942));
#21224=CARTESIAN_POINT('Ctrl Pts',(128.372771973071,-31.2530874111643,19.4045076810385));
#21225=CARTESIAN_POINT('Ctrl Pts',(128.482279924769,-31.2055297476345,19.3986920069762));
#21226=CARTESIAN_POINT('Ctrl Pts',(128.593769237178,-31.1628224846373,19.3928763329138));
#21227=CARTESIAN_POINT('Ctrl Pts',(128.706769022905,-31.1251092092962,19.3870606588515));
#21228=CARTESIAN_POINT('Ctrl Pts',(128.819930664764,-31.0873419150481,19.3812366546626));
#21229=CARTESIAN_POINT('Ctrl Pts',(128.93460670701,-31.0545829975725,19.3754126504737));
#21230=CARTESIAN_POINT('Ctrl Pts',(129.050314299865,-31.026925363027,19.3695886462848));
#21231=CARTESIAN_POINT('Ctrl Pts',(129.081010799286,-31.0195879658703,19.3680435744636));
#21232=CARTESIAN_POINT('Ctrl Pts',(129.11177986451,-31.0126093186781,19.3664985026424));
#21233=CARTESIAN_POINT('Ctrl Pts',(129.142612418793,-31.005990543878,19.3649534308213));
#21234=CARTESIAN_POINT('Ctrl Pts',(129.258835029655,-30.9810412230756,19.3591293177954));
#21235=CARTESIAN_POINT('Ctrl Pts',(129.376334978398,-30.9611288626928,19.3533052047695));
#21236=CARTESIAN_POINT('Ctrl Pts',(129.494637967476,-30.9463801095708,19.3474810917436));
#21237=CARTESIAN_POINT('Ctrl Pts',(129.61278929623,-30.9316502638382,19.3416644450284));
#21238=CARTESIAN_POINT('Ctrl Pts',(129.731741215775,-30.9220709082435,19.3358477983132));
#21239=CARTESIAN_POINT('Ctrl Pts',(129.851007744688,-30.9177180024088,19.330031151598));
#21240=CARTESIAN_POINT('Ctrl Pts',(129.970134825831,-30.9133701860407,19.3242213057718));
#21241=CARTESIAN_POINT('Ctrl Pts',(130.089575378288,-30.9142366686104,19.3184114599455));
#21242=CARTESIAN_POINT('Ctrl Pts',(130.208837598351,-30.9203416984366,19.3126016141192));
#21243=CARTESIAN_POINT('Ctrl Pts',(130.32802135689,-30.9264427118196,19.3067955905373));
#21244=CARTESIAN_POINT('Ctrl Pts',(130.447026610071,-30.937775398331,19.3009895669555));
#21245=CARTESIAN_POINT('Ctrl Pts',(130.565361081706,-30.9543119438973,19.2951835433736));
#21246=CARTESIAN_POINT('Ctrl Pts',(130.683645629729,-30.9708415129327,19.2893799692696));
#21247=CARTESIAN_POINT('Ctrl Pts',(130.801259555445,-30.9925705175673,19.2835763951656));
#21248=CARTESIAN_POINT('Ctrl Pts',(130.917715872798,-31.0194193166304,19.2777728210616));
#21249=CARTESIAN_POINT('Ctrl Pts',(131.034150542079,-31.0462631247686,19.2719703257844));
#21250=CARTESIAN_POINT('Ctrl Pts',(131.149427633751,-31.0782247411371,19.2661678305072));
#21251=CARTESIAN_POINT('Ctrl Pts',(131.263071151461,-31.1151735860729,19.2603653352299));
#21252=CARTESIAN_POINT('Ctrl Pts',(131.37676782237,-31.1521397126744,19.2545601260171));
#21253=CARTESIAN_POINT('Ctrl Pts',(131.48882900263,-31.1940976062958,19.2487549168043));
#21254=CARTESIAN_POINT('Ctrl Pts',(131.598794675586,-31.2408670434104,19.2429497075916));
#21255=CARTESIAN_POINT('Ctrl Pts',(131.708783852424,-31.2876464769478,19.2371432575829));
#21256=CARTESIAN_POINT('Ctrl Pts',(131.816676258096,-31.3392393327794,19.2313368075742));
#21257=CARTESIAN_POINT('Ctrl Pts',(131.92203391114,-31.3954181040753,19.2255303575655));
#21258=CARTESIAN_POINT('Ctrl Pts',(132.027506882934,-31.4516583655951,19.2197175521328));
#21259=CARTESIAN_POINT('Ctrl Pts',(132.13043920323,-31.5124943695596,19.2139047467001));
#21260=CARTESIAN_POINT('Ctrl Pts',(132.23041920653,-31.5776535588658,19.2080919412675));
#21261=CARTESIAN_POINT('Ctrl Pts',(132.318370563582,-31.6349734121843,19.2029784774826));
#21262=CARTESIAN_POINT('Ctrl Pts',(132.404037533551,-31.6956380129049,19.1978650136977));
#21263=CARTESIAN_POINT('Ctrl Pts',(132.487160670875,-31.7594357285724,19.1927515499128));
#21264=CARTESIAN_POINT('',(125.915000261184,-35.0014607794641,19.7396150285596));
#21265=CARTESIAN_POINT('Ctrl Pts',(125.915000261184,-35.0014607794641,19.7396150285596));
#21266=CARTESIAN_POINT('Ctrl Pts',(125.914958122368,-34.8836216006865,19.7338448931807));
#21267=CARTESIAN_POINT('Ctrl Pts',(125.920019141927,-34.7655803622538,19.7280747578018));
#21268=CARTESIAN_POINT('Ctrl Pts',(125.930209565061,-34.647819910157,19.722304622423));
#21269=CARTESIAN_POINT('Ctrl Pts',(125.940387587582,-34.5302027594559,19.7165415086582));
#21270=CARTESIAN_POINT('Ctrl Pts',(125.95568256745,-34.4128661270332,19.7107783948935));
#21271=CARTESIAN_POINT('Ctrl Pts',(125.976068747181,-34.296293901839,19.7050152811287));
#21272=CARTESIAN_POINT('Ctrl Pts',(125.99643568078,-34.1798317298528,19.6992576081897));
#21273=CARTESIAN_POINT('Ctrl Pts',(126.021884184083,-34.0641329379567,19.6934999352506));
#21274=CARTESIAN_POINT('Ctrl Pts',(126.052336666458,-33.9496766188433,19.6877422623115));
#21275=CARTESIAN_POINT('Ctrl Pts',(126.082770032877,-33.8352921474657,19.6819882036401));
#21276=CARTESIAN_POINT('Ctrl Pts',(126.118201025278,-33.722148999268,19.6762341449686));
#21277=CARTESIAN_POINT('Ctrl Pts',(126.158501038491,-33.6107157494872,19.6704800862971));
#21278=CARTESIAN_POINT('Ctrl Pts',(126.198788206539,-33.4993180177683,19.6647278616654));
#21279=CARTESIAN_POINT('Ctrl Pts',(126.243941169215,-33.3896294924763,19.6589756370337));
#21280=CARTESIAN_POINT('Ctrl Pts',(126.293781763902,-33.2821026263431,19.653223412402));
#21281=CARTESIAN_POINT('Ctrl Pts',(126.343618775953,-33.1745834894454,19.6474716012511));
#21282=CARTESIAN_POINT('Ctrl Pts',(126.398142574666,-33.0692260805372,19.6417197901003));
#21283=CARTESIAN_POINT('Ctrl Pts',(126.457127560634,-32.9664612424684,19.6359679789494));
#21284=CARTESIAN_POINT('Ctrl Pts',(126.516122867989,-32.8636784222707,19.6302151613278));
#21285=CARTESIAN_POINT('Ctrl Pts',(126.579580706547,-32.763489435633,19.6244623437061));
#21286=CARTESIAN_POINT('Ctrl Pts',(126.647230782565,-32.6662983107046,19.6187095260844));
#21287=CARTESIAN_POINT('Ctrl Pts',(126.714949685685,-32.5690083036481,19.6129508555534));
#21288=CARTESIAN_POINT('Ctrl Pts',(126.78686910445,-32.4747225907782,19.6071921850223));
#21289=CARTESIAN_POINT('Ctrl Pts',(126.862676808916,-32.3838141895719,19.6014335144912));
#21290=CARTESIAN_POINT('Ctrl Pts',(126.938525657659,-32.2928564482559,19.5956717184686));
#21291=CARTESIAN_POINT('Ctrl Pts',(127.018266713885,-32.2052799760541,19.589909922446));
#21292=CARTESIAN_POINT('Ctrl Pts',(127.10155029257,-32.1214214804004,19.5841481264234));
#21293=CARTESIAN_POINT('Ctrl Pts',(127.184962488869,-32.0374334792696,19.5783774322667));
#21294=CARTESIAN_POINT('Ctrl Pts',(127.271927827314,-31.9571752034551,19.57260673811));
#21295=CARTESIAN_POINT('Ctrl Pts',(127.362062681455,-31.8809437800148,19.5668360439533));
#21296=CARTESIAN_POINT('Ctrl Pts',(127.424785193379,-31.8278963056356,19.5628203672597));
#21297=CARTESIAN_POINT('Ctrl Pts',(127.489041833148,-31.7767979365938,19.5588046905661));
#21298=CARTESIAN_POINT('Ctrl Pts',(127.554695457865,-31.7277361511926,19.5547890138725));
#21299=CARTESIAN_POINT('Ctrl Pts',(127.649907355974,-31.6565859940937,19.5489654176607));
#21300=CARTESIAN_POINT('Ctrl Pts',(127.748380713119,-31.5894800720813,19.5431418214489));
#21301=CARTESIAN_POINT('Ctrl Pts',(127.849737400708,-31.5267312580099,19.5373182252371));
#21302=CARTESIAN_POINT('Ctrl Pts',(127.95096621208,-31.4640616107024,19.5315019763397));
#21303=CARTESIAN_POINT('Ctrl Pts',(128.055070774387,-31.4057383507268,19.5256857274423));
#21304=CARTESIAN_POINT('Ctrl Pts',(128.161641181523,-31.352033188949,19.5198694785449));
#21305=CARTESIAN_POINT('Ctrl Pts',(128.268104911339,-31.2983817862112,19.5140590517314));
#21306=CARTESIAN_POINT('Ctrl Pts',(128.377029213014,-31.249339468026,19.5082486249179));
#21307=CARTESIAN_POINT('Ctrl Pts',(128.487977101229,-31.2051334998985,19.5024381981043));
#21308=CARTESIAN_POINT('Ctrl Pts',(128.603124527375,-31.159254271983,19.4964078382377));
#21309=CARTESIAN_POINT('Ctrl Pts',(128.720451377084,-31.118584989689,19.490377478371));
#21310=CARTESIAN_POINT('Ctrl Pts',(128.83944293416,-31.083326373448,19.4843471185043));
#21311=CARTESIAN_POINT('Ctrl Pts',(128.953965706223,-31.0493919114555,19.4785432316955));
#21312=CARTESIAN_POINT('Ctrl Pts',(129.070029976031,-31.0204691704228,19.4727393448867));
#21313=CARTESIAN_POINT('Ctrl Pts',(129.18715929488,-30.996686998485,19.4669354580779));
#21314=CARTESIAN_POINT('Ctrl Pts',(129.30427131247,-30.9729083394294,19.4611324285656));
#21315=CARTESIAN_POINT('Ctrl Pts',(129.422447666179,-30.9542688206558,19.4553293990532));
#21316=CARTESIAN_POINT('Ctrl Pts',(129.541200818743,-30.9408463553004,19.4495263695409));
#21317=CARTESIAN_POINT('Ctrl Pts',(129.659964455893,-30.9274227048903,19.4437228276854));
#21318=CARTESIAN_POINT('Ctrl Pts',(129.779304587376,-30.9192170695619,19.4379192858299));
#21319=CARTESIAN_POINT('Ctrl Pts',(129.898728285557,-30.9162555124183,19.4321157439744));
#21320=CARTESIAN_POINT('Ctrl Pts',(130.018190711304,-30.9132929948799,19.4263103201051));
#21321=CARTESIAN_POINT('Ctrl Pts',(130.137736349643,-30.9155779477278,19.4205048962358));
#21322=CARTESIAN_POINT('Ctrl Pts',(130.25687264739,-30.9230843223066,19.4146994723666));
#21323=CARTESIAN_POINT('Ctrl Pts',(130.376140877046,-30.9305990094679,19.4088876195528));
#21324=CARTESIAN_POINT('Ctrl Pts',(130.494998453504,-30.9433466344716,19.403075766739));
#21325=CARTESIAN_POINT('Ctrl Pts',(130.61295815825,-30.9612492901599,19.3972639139252));
#21326=CARTESIAN_POINT('Ctrl Pts',(130.730995339327,-30.9791637043725,19.391448243867));
#21327=CARTESIAN_POINT('Ctrl Pts',(130.848133074523,-31.0022398135148,19.3856325738087));
#21328=CARTESIAN_POINT('Ctrl Pts',(130.96389617366,-31.0303489868247,19.3798169037505));
#21329=CARTESIAN_POINT('Ctrl Pts',(131.079825090187,-31.0584984233081,19.3739929034105));
#21330=CARTESIAN_POINT('Ctrl Pts',(131.194375049813,-31.0916952000503,19.3681689030705));
#21331=CARTESIAN_POINT('Ctrl Pts',(131.307087664496,-31.1297613978822,19.3623449027305));
#21332=CARTESIAN_POINT('Ctrl Pts',(131.336990447327,-31.1398604027732,19.3607997889217));
#21333=CARTESIAN_POINT('Ctrl Pts',(131.36676402913,-31.1503018823635,19.3592546751129));
#21334=CARTESIAN_POINT('Ctrl Pts',(131.396400123974,-31.1610819631353,19.3577095613041));
#21335=CARTESIAN_POINT('Ctrl Pts',(131.508084011257,-31.2017067935042,19.3518867861588));
#21336=CARTESIAN_POINT('Ctrl Pts',(131.618173684181,-31.2472749228511,19.3460640110134));
#21337=CARTESIAN_POINT('Ctrl Pts',(131.726200384617,-31.297641666161,19.340241235868));
#21338=CARTESIAN_POINT('Ctrl Pts',(131.834107403958,-31.3479526089421,19.3344249116844));
#21339=CARTESIAN_POINT('Ctrl Pts',(131.939955626777,-31.4030514283356,19.3286085875007));
#21340=CARTESIAN_POINT('Ctrl Pts',(132.043293084972,-31.4627442319075,19.3227922633171));
#21341=CARTESIAN_POINT('Ctrl Pts',(132.146519156579,-31.5223726931019,19.316982208501));
#21342=CARTESIAN_POINT('Ctrl Pts',(132.247239497912,-31.5865850807773,19.3111721536849));
#21343=CARTESIAN_POINT('Ctrl Pts',(132.345024568614,-31.6551405451656,19.3053620988688));
#21344=CARTESIAN_POINT('Ctrl Pts',(132.393129567781,-31.6888661490192,19.3025038641702));
#21345=CARTESIAN_POINT('Ctrl Pts',(132.440524554963,-31.723642112516,19.2996456294715));
#21346=CARTESIAN_POINT('Ctrl Pts',(132.487160670875,-31.7594357285724,19.2967873947729));
#21347=CARTESIAN_POINT('Ctrl Pts',(132.487160670875,-31.7594357285724,20.546920387862));
#21348=CARTESIAN_POINT('Ctrl Pts',(132.523548068931,-31.7873633664098,20.5446756841462));
#21349=CARTESIAN_POINT('Ctrl Pts',(132.55944402042,-31.8158878360481,20.5424309804305));
#21350=CARTESIAN_POINT('Ctrl Pts',(132.594828390306,-31.8449895998809,20.5401862767148));
#21351=CARTESIAN_POINT('Ctrl Pts',(132.686628563226,-31.9204903636558,20.5343626831361));
#21352=CARTESIAN_POINT('Ctrl Pts',(132.775278808919,-32.0001228172305,20.5285390895573));
#21353=CARTESIAN_POINT('Ctrl Pts',(132.860385118183,-32.0835943396574,20.5227154959786));
#21354=CARTESIAN_POINT('Ctrl Pts',(132.945384053196,-32.1669605503598,20.5168992497283));
#21355=CARTESIAN_POINT('Ctrl Pts',(133.026847655943,-32.2541559127918,20.5110830034779));
#21356=CARTESIAN_POINT('Ctrl Pts',(133.104414314979,-32.3448471303985,20.5052667572275));
#21357=CARTESIAN_POINT('Ctrl Pts',(133.181903329363,-32.4354475655976,20.4994563330716));
#21358=CARTESIAN_POINT('Ctrl Pts',(133.255502896433,-32.5295365858737,20.4936459089157));
#21359=CARTESIAN_POINT('Ctrl Pts',(133.324888111438,-32.6267439989716,20.4878354847598));
#21360=CARTESIAN_POINT('Ctrl Pts',(133.396899701905,-32.7276309159011,20.481805123901));
#21361=CARTESIAN_POINT('Ctrl Pts',(133.464371272422,-32.8318766516566,20.4757747630421));
#21362=CARTESIAN_POINT('Ctrl Pts',(133.526985163046,-32.9390291948563,20.4697444021832));
#21363=CARTESIAN_POINT('Ctrl Pts',(133.587247521362,-33.0421575085327,20.4639405180413));
#21364=CARTESIAN_POINT('Ctrl Pts',(133.643010266103,-33.1479778462274,20.4581366338994));
#21365=CARTESIAN_POINT('Ctrl Pts',(133.694034661689,-33.2560582239541,20.4523327497575));
#21366=CARTESIAN_POINT('Ctrl Pts',(133.745051520432,-33.3641226370634,20.4465297229109));
#21367=CARTESIAN_POINT('Ctrl Pts',(133.791331247631,-33.4744460571622,20.4407266960642));
#21368=CARTESIAN_POINT('Ctrl Pts',(133.83268192967,-33.586573586641,20.4349236692176));
#21369=CARTESIAN_POINT('Ctrl Pts',(133.874036262546,-33.6987110158207,20.4291201300237));
#21370=CARTESIAN_POINT('Ctrl Pts',(133.910460543719,-33.8126524879418,20.4233165908298));
#21371=CARTESIAN_POINT('Ctrl Pts',(133.941811928845,-33.9279255074333,20.4175130516359));
#21372=CARTESIAN_POINT('Ctrl Pts',(133.973173480865,-34.0432359086363,20.4117076304211));
#21373=CARTESIAN_POINT('Ctrl Pts',(133.999458758033,-34.1598783221522,20.4059022092063));
#21374=CARTESIAN_POINT('Ctrl Pts',(134.020575614019,-34.2773681906033,20.4000967879916));
#21375=CARTESIAN_POINT('Ctrl Pts',(134.041715854976,-34.3949881682423,20.3942849378085));
#21376=CARTESIAN_POINT('Ctrl Pts',(134.057676177778,-34.5134570719638,20.3884730876255));
#21377=CARTESIAN_POINT('Ctrl Pts',(134.068416070864,-34.6322831601186,20.3826612374424));
#21378=CARTESIAN_POINT('Ctrl Pts',(134.079163017972,-34.7511872939037,20.3768455700041));
#21379=CARTESIAN_POINT('Ctrl Pts',(134.084682687972,-34.8704486723726,20.3710299025658));
#21380=CARTESIAN_POINT('Ctrl Pts',(134.084986697936,-34.9895751408295,20.3652142351274));
#21381=CARTESIAN_POINT('Ctrl Pts',(134.085291143361,-35.1088722451291,20.3593902373715));
#21382=CARTESIAN_POINT('Ctrl Pts',(134.080365034102,-35.2280336471716,20.3535662396156));
#21383=CARTESIAN_POINT('Ctrl Pts',(134.070271860316,-35.346571757529,20.3477422418597));
#21384=CARTESIAN_POINT('Ctrl Pts',(134.067594084757,-35.3780205824025,20.3461971026219));
#21385=CARTESIAN_POINT('Ctrl Pts',(134.064552893826,-35.4094255905554,20.3446519633841));
#21386=CARTESIAN_POINT('Ctrl Pts',(134.061150073727,-35.4407778109978,20.3431068241463));
#21387=CARTESIAN_POINT('Ctrl Pts',(134.048324924255,-35.5589435975309,20.3372832304498));
#21388=CARTESIAN_POINT('Ctrl Pts',(134.030317473101,-35.6767397176403,20.3314596367534));
#21389=CARTESIAN_POINT('Ctrl Pts',(134.007156478494,-35.7936762292395,20.3256360430569));
#21390=CARTESIAN_POINT('Ctrl Pts',(133.984024704926,-35.9104652080444,20.3198197966897));
#21391=CARTESIAN_POINT('Ctrl Pts',(133.955752398789,-36.0263963384068,20.3140035503225));
#21392=CARTESIAN_POINT('Ctrl Pts',(133.922420097489,-36.1409844779025,20.3081873039553));
#21393=CARTESIAN_POINT('Ctrl Pts',(133.889121162011,-36.2554579140226,20.3023768796835));
#21394=CARTESIAN_POINT('Ctrl Pts',(133.850772421123,-36.368590643845,20.2965664554118));
#21395=CARTESIAN_POINT('Ctrl Pts',(133.807505391999,-36.479908000485,20.2907560311401));
#21396=CARTESIAN_POINT('Ctrl Pts',(133.762600616579,-36.595438948679,20.284725670325));
#21397=CARTESIAN_POINT('Ctrl Pts',(133.712397948556,-36.7090139373482,20.2786953095099));
#21398=CARTESIAN_POINT('Ctrl Pts',(133.657101307584,-36.820119508732,20.2726649486948));
#21399=CARTESIAN_POINT('Ctrl Pts',(133.603881390285,-36.9270523931991,20.2668610644404));
#21400=CARTESIAN_POINT('Ctrl Pts',(133.545943417351,-37.0316976001409,20.2610571801859));
#21401=CARTESIAN_POINT('Ctrl Pts',(133.483517821578,-37.1336186601058,20.2552532959315));
#21402=CARTESIAN_POINT('Ctrl Pts',(133.421101446741,-37.2355246652257,20.2494502689736));
#21403=CARTESIAN_POINT('Ctrl Pts',(133.354198980525,-37.3347069754688,20.2436472420158));
#21404=CARTESIAN_POINT('Ctrl Pts',(133.283085686113,-37.4307557215072,20.237844215058));
#21405=CARTESIAN_POINT('Ctrl Pts',(133.211966113151,-37.5268129476313,20.2320406757544));
#21406=CARTESIAN_POINT('Ctrl Pts',(133.136635215813,-37.6197357312892,20.2262371364508));
#21407=CARTESIAN_POINT('Ctrl Pts',(133.057409873698,-37.7091455967172,20.2204335971472));
#21408=CARTESIAN_POINT('Ctrl Pts',(132.978158839741,-37.7985844567084,20.2146281758244));
#21409=CARTESIAN_POINT('Ctrl Pts',(132.895011120008,-37.8845078274006,20.2088227545015));
#21410=CARTESIAN_POINT('Ctrl Pts',(132.808321473052,-37.9665730235404,20.2030173331787));
#21411=CARTESIAN_POINT('Ctrl Pts',(132.721535825356,-38.0487290992693,20.1972054828905));
#21412=CARTESIAN_POINT('Ctrl Pts',(132.631200717793,-38.1270181911431,20.1913936326023));
#21413=CARTESIAN_POINT('Ctrl Pts',(132.537705221933,-38.2011368615813,20.1855817823141));
#21414=CARTESIAN_POINT('Ctrl Pts',(132.444148317742,-38.2753042135501,20.1797661147722));
#21415=CARTESIAN_POINT('Ctrl Pts',(132.347427221373,-38.3452954501526,20.1739504472303));
#21416=CARTESIAN_POINT('Ctrl Pts',(132.247959924876,-38.4108505062744,20.1681347796885));
#21417=CARTESIAN_POINT('Ctrl Pts',(132.148350152239,-38.4764994629209,20.1623107818321));
#21418=CARTESIAN_POINT('Ctrl Pts',(132.045986677384,-38.5376993473583,20.1564867839757));
#21419=CARTESIAN_POINT('Ctrl Pts',(131.941312109039,-38.5942359821383,20.1506627861194));
#21420=CARTESIAN_POINT('Ctrl Pts',(131.913541379025,-38.6092354576102,20.1491176479389));
#21421=CARTESIAN_POINT('Ctrl Pts',(131.885608085202,-38.6239069646692,20.1475725097584));
#21422=CARTESIAN_POINT('Ctrl Pts',(131.857520709763,-38.6382470796802,20.1460273715779));
#21423=CARTESIAN_POINT('Ctrl Pts',(131.751659969621,-38.6922946781139,20.1402037775663));
#21424=CARTESIAN_POINT('Ctrl Pts',(131.643267658643,-38.7418053106816,20.1343801835548));
#21425=CARTESIAN_POINT('Ctrl Pts',(131.53276931453,-38.7865344615405,20.1285565895432));
#21426=CARTESIAN_POINT('Ctrl Pts',(131.422410380457,-38.8312071799459,20.1227403428587));
#21427=CARTESIAN_POINT('Ctrl Pts',(131.309951073269,-38.8711102633735,20.1169240961742));
#21428=CARTESIAN_POINT('Ctrl Pts',(131.19584129982,-38.9060451335903,20.1111078494896));
#21429=CARTESIAN_POINT('Ctrl Pts',(131.081845750858,-38.9409450338173,20.1052974248988));
#21430=CARTESIAN_POINT('Ctrl Pts',(130.966203410539,-38.9708864955649,20.0994870003079));
#21431=CARTESIAN_POINT('Ctrl Pts',(130.849383369527,-38.9957193209197,20.093676575717));
#21432=CARTESIAN_POINT('Ctrl Pts',(130.728141458058,-39.0214921180109,20.0876462150209));
#21433=CARTESIAN_POINT('Ctrl Pts',(130.60563134316,-39.0417617250352,20.0816158543247));
#21434=CARTESIAN_POINT('Ctrl Pts',(130.482394247349,-39.056417235705,20.0755854936286));
#21435=CARTESIAN_POINT('Ctrl Pts',(130.363785441738,-39.0705223442743,20.0697816090525));
#21436=CARTESIAN_POINT('Ctrl Pts',(130.244503717389,-39.0794273851999,20.0639777244764));
#21437=CARTESIAN_POINT('Ctrl Pts',(130.12504043967,-39.0830858291796,20.0581738399004));
#21438=CARTESIAN_POINT('Ctrl Pts',(130.005594807964,-39.0867437327677,20.0523708126206));
#21439=CARTESIAN_POINT('Ctrl Pts',(129.885968084255,-39.0851565681025,20.0465677853408));
#21440=CARTESIAN_POINT('Ctrl Pts',(129.766653960719,-39.0783298819433,20.040764758061));
#21441=CARTESIAN_POINT('Ctrl Pts',(129.647329303011,-39.0715025930602,20.0349612184354));
#21442=CARTESIAN_POINT('Ctrl Pts',(129.528317708041,-39.0594348862607,20.0291576788098));
#21443=CARTESIAN_POINT('Ctrl Pts',(129.410109423915,-39.0421843238831,20.0233541391843));
#21444=CARTESIAN_POINT('Ctrl Pts',(129.291862806249,-39.0249281673533,20.0175487175398));
#21445=CARTESIAN_POINT('Ctrl Pts',(129.174420421361,-39.0024858715713,20.0117432958954));
#21446=CARTESIAN_POINT('Ctrl Pts',(129.05826334707,-38.9749662987915,20.005937874251));
#21447=CARTESIAN_POINT('Ctrl Pts',(128.941977639649,-38.9474162506505,20.0001260236433));
#21448=CARTESIAN_POINT('Ctrl Pts',(128.82698048155,-38.9147777964909,19.9943141730357));
#21449=CARTESIAN_POINT('Ctrl Pts',(128.713738934119,-38.8772100111288,19.988502322428));
#21450=CARTESIAN_POINT('Ctrl Pts',(128.600423009067,-38.8396175510559,19.9826866545676));
#21451=CARTESIAN_POINT('Ctrl Pts',(128.488865371773,-38.7970894571204,19.9768709867071));
#21452=CARTESIAN_POINT('Ctrl Pts',(128.379512661255,-38.7498327676002,19.9710553188467));
#21453=CARTESIAN_POINT('Ctrl Pts',(128.270003314891,-38.7025083880196,19.9652313206755));
#21454=CARTESIAN_POINT('Ctrl Pts',(128.162705565199,-38.6504420715526,19.9594073225043));
#21455=CARTESIAN_POINT('Ctrl Pts',(128.058041166046,-38.5938865991053,19.9535833243331));
#21456=CARTESIAN_POINT('Ctrl Pts',(128.030273190693,-38.5788821565466,19.9520381892252));
#21457=CARTESIAN_POINT('Ctrl Pts',(128.002690406367,-38.5635619712292,19.9504930541173));
#21458=CARTESIAN_POINT('Ctrl Pts',(127.97530032608,-38.5479312606687,19.9489479190094));
#21459=CARTESIAN_POINT('Ctrl Pts',(127.872067493333,-38.489019329336,19.943124326216));
#21460=CARTESIAN_POINT('Ctrl Pts',(127.771241531577,-38.4255030674034,19.9373007334226));
#21461=CARTESIAN_POINT('Ctrl Pts',(127.673260210972,-38.3576043474708,19.9314771406292));
#21462=CARTESIAN_POINT('Ctrl Pts',(127.575402508372,-38.2897912918693,19.9256608951641));
#21463=CARTESIAN_POINT('Ctrl Pts',(127.480382641277,-38.2176070060932,19.9198446496989));
#21464=CARTESIAN_POINT('Ctrl Pts',(127.388613317249,-38.1413189257303,19.9140284042337));
#21465=CARTESIAN_POINT('Ctrl Pts',(127.296935854815,-38.0651072101519,19.908217980862));
#21466=CARTESIAN_POINT('Ctrl Pts',(127.208502774595,-37.9848001317203,19.9024075574903));
#21467=CARTESIAN_POINT('Ctrl Pts',(127.123696836121,-37.9007076911436,19.8965971341186));
#21468=CARTESIAN_POINT('Ctrl Pts',(127.035680799385,-37.8134321598283,19.8905667729653));
#21469=CARTESIAN_POINT('Ctrl Pts',(126.951572289504,-37.7220792902935,19.8845364118121));
#21470=CARTESIAN_POINT('Ctrl Pts',(126.871760744005,-37.6270409508138,19.8785060506589));
#21471=CARTESIAN_POINT('Ctrl Pts',(126.794946621351,-37.5355718955536,19.8727021672936));
#21472=CARTESIAN_POINT('Ctrl Pts',(126.722112814015,-37.4406895438645,19.8668982839284));
#21473=CARTESIAN_POINT('Ctrl Pts',(126.653567586273,-37.3427793537506,19.8610944005632));
#21474=CARTESIAN_POINT('Ctrl Pts',(126.585032483341,-37.2448836259423,19.8552913744891));
#21475=CARTESIAN_POINT('Ctrl Pts',(126.520784934362,-37.1439612835512,19.849488348415));
#21476=CARTESIAN_POINT('Ctrl Pts',(126.461090924169,-37.0404282768574,19.8436853223409));
#21477=CARTESIAN_POINT('Ctrl Pts',(126.40139164356,-36.9368861291808,19.8378817839146));
#21478=CARTESIAN_POINT('Ctrl Pts',(126.346246905051,-36.8307332126852,19.8320782454883));
#21479=CARTESIAN_POINT('Ctrl Pts',(126.29587730123,-36.7224111101761,19.826274707062));
#21480=CARTESIAN_POINT('Ctrl Pts',(126.245491363076,-36.6140538799459,19.8204692866091));
#21481=CARTESIAN_POINT('Ctrl Pts',(126.199883811363,-36.5035264347844,19.8146638661562));
#21482=CARTESIAN_POINT('Ctrl Pts',(126.159227306094,-36.3912908084738,19.8088584457033));
#21483=CARTESIAN_POINT('Ctrl Pts',(126.118525777404,-36.2789308913088,19.8030465962698));
#21484=CARTESIAN_POINT('Ctrl Pts',(126.082786378527,-36.1648594012373,19.7972347468362));
#21485=CARTESIAN_POINT('Ctrl Pts',(126.052132089805,-36.0495541737595,19.7914228974027));
#21486=CARTESIAN_POINT('Ctrl Pts',(126.021457667142,-35.9341732130374,19.7856072307076));
#21487=CARTESIAN_POINT('Ctrl Pts',(125.995875093492,-35.8175572990579,19.7797915640125));
#21488=CARTESIAN_POINT('Ctrl Pts',(125.975456039167,-35.7001934784911,19.7739758973174));
#21489=CARTESIAN_POINT('Ctrl Pts',(125.955007736688,-35.5826615465633,19.7681519002899));
#21490=CARTESIAN_POINT('Ctrl Pts',(125.939737768042,-35.464379973335,19.7623279032623));
#21491=CARTESIAN_POINT('Ctrl Pts',(125.929665904588,-35.345840066687,19.7565039062348));
#21492=CARTESIAN_POINT('Ctrl Pts',(125.926993769716,-35.3143906115087,19.7549587596368));
#21493=CARTESIAN_POINT('Ctrl Pts',(125.92468723338,-35.2829229658023,19.7534136130389));
#21494=CARTESIAN_POINT('Ctrl Pts',(125.922746050153,-35.2514462734928,19.751868466441));
#21495=CARTESIAN_POINT('Ctrl Pts',(125.917614677707,-35.1682399953501,19.7477839871591));
#21496=CARTESIAN_POINT('Ctrl Pts',(125.91503008981,-35.0848750595345,19.7436995078773));
#21497=CARTESIAN_POINT('Ctrl Pts',(125.915000261185,-35.0014607801979,19.7396150285955));
#21498=CARTESIAN_POINT('Origin',(130.,-35.,32.7603849714045));
#21499=CARTESIAN_POINT('',(132.487160670875,-31.7594357285724,21.7969524316048));
#21500=CARTESIAN_POINT('',(132.487160670875,-31.7594357285724,21.6925409193069));
#21501=CARTESIAN_POINT('',(132.487160670875,-31.7594357285724,32.7603849714045));
#21502=CARTESIAN_POINT('',(125.915001474033,-35.0034702810671,20.8853849714288));
#21503=CARTESIAN_POINT('Ctrl Pts',(132.487160670875,-31.7594357285724,21.6925409193069));
#21504=CARTESIAN_POINT('Ctrl Pts',(132.581750072248,-31.8320338995304,21.686731190181));
#21505=CARTESIAN_POINT('Ctrl Pts',(132.673252096067,-31.9088490454524,21.6809214610551));
#21506=CARTESIAN_POINT('Ctrl Pts',(132.7612728889,-31.9895852390367,21.6751117319293));
#21507=CARTESIAN_POINT('Ctrl Pts',(132.851093333724,-32.0719721454453,21.669183218477));
#21508=CARTESIAN_POINT('Ctrl Pts',(132.937288272235,-32.1584419595542,21.6632547050247));
#21509=CARTESIAN_POINT('Ctrl Pts',(133.019473900383,-32.2486362717907,21.6573261915724));
#21510=CARTESIAN_POINT('Ctrl Pts',(133.099929339428,-32.3369317944248,21.6515224864303));
#21511=CARTESIAN_POINT('Ctrl Pts',(133.176542332567,-32.4287962210242,21.6457187812882));
#21512=CARTESIAN_POINT('Ctrl Pts',(133.248990082593,-32.5238561343873,21.6399150761461));
#21513=CARTESIAN_POINT('Ctrl Pts',(133.321429231274,-32.6189047617812,21.6341120600478));
#21514=CARTESIAN_POINT('Ctrl Pts',(133.389703872855,-32.7171477967207,21.6283090439495));
#21515=CARTESIAN_POINT('Ctrl Pts',(133.453532313997,-32.8181797608012,21.6225060278511));
#21516=CARTESIAN_POINT('Ctrl Pts',(133.517368240634,-32.9192235734274,21.6167023312028));
#21517=CARTESIAN_POINT('Ctrl Pts',(133.576756711935,-33.0230566203116,21.6108986345545));
#21518=CARTESIAN_POINT('Ctrl Pts',(133.631460429976,-33.1292461023645,21.6050949379061));
#21519=CARTESIAN_POINT('Ctrl Pts',(133.688224574743,-33.2394352329726,21.5990726438368));
#21520=CARTESIAN_POINT('Ctrl Pts',(133.739943902747,-33.3521613770866,21.5930503497675));
#21521=CARTESIAN_POINT('Ctrl Pts',(133.786407175595,-33.4669162773674,21.5870280556982));
#21522=CARTESIAN_POINT('Ctrl Pts',(133.831250903433,-33.5776712285531,21.5812156774551));
#21523=CARTESIAN_POINT('Ctrl Pts',(133.871198788336,-33.6903154573991,21.5754032992121));
#21524=CARTESIAN_POINT('Ctrl Pts',(133.906111585419,-33.8043757771527,21.569590920969));
#21525=CARTESIAN_POINT('Ctrl Pts',(133.941048496566,-33.9185148777014,21.5637745281504));
#21526=CARTESIAN_POINT('Ctrl Pts',(133.970943292541,-34.0340716227221,21.5579581353317));
#21527=CARTESIAN_POINT('Ctrl Pts',(133.995707688656,-34.1505619111331,21.552141742513));
#21528=CARTESIAN_POINT('Ctrl Pts',(134.020506523705,-34.2672141983023,21.5463172610509));
#21529=CARTESIAN_POINT('Ctrl Pts',(134.040160655904,-34.3848022184481,21.5404927795887));
#21530=CARTESIAN_POINT('Ctrl Pts',(134.054633516296,-34.502835994338,21.5346682981265));
#21531=CARTESIAN_POINT('Ctrl Pts',(134.056158283232,-34.5152712693208,21.5340546684424));
#21532=CARTESIAN_POINT('Ctrl Pts',(134.05762558901,-34.5277114917279,21.5334410387583));
#21533=CARTESIAN_POINT('Ctrl Pts',(134.059035424522,-34.540156089013,21.5328274090742));
#21534=CARTESIAN_POINT('Ctrl Pts',(134.072415333228,-34.6582603459497,21.5270038154121));
#21535=CARTESIAN_POINT('Ctrl Pts',(134.080657885567,-34.7771395049127,21.52118022175));
#21536=CARTESIAN_POINT('Ctrl Pts',(134.083683781112,-34.896309229528,21.515356628088));
#21537=CARTESIAN_POINT('Ctrl Pts',(134.086705859041,-35.0153286038346,21.5095403817543));
#21538=CARTESIAN_POINT('Ctrl Pts',(134.084524360526,-35.134637410044,21.5037241354207));
#21539=CARTESIAN_POINT('Ctrl Pts',(134.077111557626,-35.2537446485602,21.497907889087));
#21540=CARTESIAN_POINT('Ctrl Pts',(134.069706174982,-35.3727326600739,21.492097464848));
#21541=CARTESIAN_POINT('Ctrl Pts',(134.057079930669,-35.4915191000857,21.486287040609));
#21542=CARTESIAN_POINT('Ctrl Pts',(134.039257132993,-35.6096120188813,21.48047661637));
#21543=CARTESIAN_POINT('Ctrl Pts',(134.020759705521,-35.7321749991799,21.4744462555423));
#21544=CARTESIAN_POINT('Ctrl Pts',(133.996664539723,-35.8539904703923,21.4684158947146));
#21545=CARTESIAN_POINT('Ctrl Pts',(133.967058086598,-35.9745127693146,21.462385533887));
#21546=CARTESIAN_POINT('Ctrl Pts',(133.938563535254,-36.0905087253357,21.4565816496629));
#21547=CARTESIAN_POINT('Ctrl Pts',(133.904964301935,-36.2053064581143,21.4507777654389));
#21548=CARTESIAN_POINT('Ctrl Pts',(133.866389576652,-36.3184296119088,21.4449738812149));
#21549=CARTESIAN_POINT('Ctrl Pts',(133.827820549268,-36.431536056205,21.4391708542865));
#21550=CARTESIAN_POINT('Ctrl Pts',(133.784277623227,-36.5429680270441,21.4333678273582));
#21551=CARTESIAN_POINT('Ctrl Pts',(133.735939558198,-36.652265298761,21.4275648004299));
#21552=CARTESIAN_POINT('Ctrl Pts',(133.687597225423,-36.7615722202854,21.4217612611549));
#21553=CARTESIAN_POINT('Ctrl Pts',(133.634459077087,-36.8687436944971,21.4159577218799));
#21554=CARTESIAN_POINT('Ctrl Pts',(133.576751357031,-36.9733410070182,21.4101541826049));
#21555=CARTESIAN_POINT('Ctrl Pts',(133.519024923033,-37.0779722392296,21.4043487613097));
#21556=CARTESIAN_POINT('Ctrl Pts',(133.456726167387,-37.1800272922317,21.3985433400145));
#21557=CARTESIAN_POINT('Ctrl Pts',(133.390126134966,-37.2790940719986,21.3927379187193));
#21558=CARTESIAN_POINT('Ctrl Pts',(133.323452349172,-37.3782705590576,21.3869260684572));
#21559=CARTESIAN_POINT('Ctrl Pts',(133.25246800667,-37.4744518282846,21.3811142181951));
#21560=CARTESIAN_POINT('Ctrl Pts',(133.177486231656,-37.5672565605406,21.375302367933));
#21561=CARTESIAN_POINT('Ctrl Pts',(133.102455208208,-37.6601222474446,21.3694867004164));
#21562=CARTESIAN_POINT('Ctrl Pts',(133.023421793118,-37.749606675364,21.3636710328997));
#21563=CARTESIAN_POINT('Ctrl Pts',(132.94073683228,-37.8353645062447,21.3578553653831));
#21564=CARTESIAN_POINT('Ctrl Pts',(132.857933434161,-37.9212451759609,21.3520313675505));
#21565=CARTESIAN_POINT('Ctrl Pts',(132.771468345601,-38.0033883141385,21.3462073697179));
#21566=CARTESIAN_POINT('Ctrl Pts',(132.681726486139,-38.0814879609596,21.3403833718853));
#21567=CARTESIAN_POINT('Ctrl Pts',(132.657917480281,-38.102208224166,21.3388382334254));
#21568=CARTESIAN_POINT('Ctrl Pts',(132.633877994583,-38.1226441118969,21.3372930949656));
#21569=CARTESIAN_POINT('Ctrl Pts',(132.609615554879,-38.1427904250415,21.3357479565057));
#21570=CARTESIAN_POINT('Ctrl Pts',(132.51817094072,-38.2187214466004,21.3299243628355));
#21571=CARTESIAN_POINT('Ctrl Pts',(132.423262109218,-38.2907805045869,21.3241007691653));
#21572=CARTESIAN_POINT('Ctrl Pts',(132.325250675735,-38.3586357788534,21.3182771754951));
#21573=CARTESIAN_POINT('Ctrl Pts',(132.227362898235,-38.4264054436113,21.3124609291534));
#21574=CARTESIAN_POINT('Ctrl Pts',(132.126380637163,-38.4899816431958,21.3066446828117));
#21575=CARTESIAN_POINT('Ctrl Pts',(132.022699350964,-38.5490720386617,21.30082843647));
#21576=CARTESIAN_POINT('Ctrl Pts',(131.919121850306,-38.6081032843147,21.2950180122231));
#21577=CARTESIAN_POINT('Ctrl Pts',(131.812851052025,-38.662657457747,21.2892075879762));
#21578=CARTESIAN_POINT('Ctrl Pts',(131.704311733594,-38.7124852208099,21.2833971637292));
#21579=CARTESIAN_POINT('Ctrl Pts',(131.591663977427,-38.7641990677833,21.2773668029046));
#21580=CARTESIAN_POINT('Ctrl Pts',(131.476572940032,-38.810821370695,21.2713364420799));
#21581=CARTESIAN_POINT('Ctrl Pts',(131.359542387655,-38.852125321971,21.2653060812552));
#21582=CARTESIAN_POINT('Ctrl Pts',(131.246907041727,-38.8918780595738,21.2595021970237));
#21583=CARTESIAN_POINT('Ctrl Pts',(131.13247565441,-38.9267045661159,21.2536983127921));
#21584=CARTESIAN_POINT('Ctrl Pts',(131.016717453162,-38.9564517715292,21.2478944285605));
#21585=CARTESIAN_POINT('Ctrl Pts',(130.90097635064,-38.9861945829617,21.2420914016247));
#21586=CARTESIAN_POINT('Ctrl Pts',(130.783909219319,-39.010859483706,21.236288374689));
#21587=CARTESIAN_POINT('Ctrl Pts',(130.665998968207,-39.030343704245,21.2304853477532));
#21588=CARTESIAN_POINT('Ctrl Pts',(130.548078306854,-39.0498296450367,21.2246818084709));
#21589=CARTESIAN_POINT('Ctrl Pts',(130.429314780602,-39.0641339296251,21.2188782691887));
#21590=CARTESIAN_POINT('Ctrl Pts',(130.310199336132,-39.0732052945884,21.2130747299064));
#21591=CARTESIAN_POINT('Ctrl Pts',(130.191045263914,-39.0822796012895,21.2072693086041));
#21592=CARTESIAN_POINT('Ctrl Pts',(130.071539453462,-39.0861175824741,21.2014638873018));
#21593=CARTESIAN_POINT('Ctrl Pts',(129.952175145256,-39.0847200373182,21.1956584659995));
#21594=CARTESIAN_POINT('Ctrl Pts',(129.832678652129,-39.0833209445104,21.1898466157305));
#21595=CARTESIAN_POINT('Ctrl Pts',(129.713324382588,-39.0766747571188,21.1840347654616));
#21596=CARTESIAN_POINT('Ctrl Pts',(129.594602904237,-39.0648343379217,21.1782229151926));
#21597=CARTESIAN_POINT('Ctrl Pts',(129.475803448983,-39.0529861418737,21.1724072476693));
#21598=CARTESIAN_POINT('Ctrl Pts',(129.357638015862,-39.035936977912,21.1665915801459));
#21599=CARTESIAN_POINT('Ctrl Pts',(129.240587756598,-39.0137909816745,21.1607759126225));
#21600=CARTESIAN_POINT('Ctrl Pts',(129.123369835479,-38.9916132636891,21.1549519147835));
#21601=CARTESIAN_POINT('Ctrl Pts',(129.007270672566,-38.9643242348053,21.1491279169445));
#21602=CARTESIAN_POINT('Ctrl Pts',(128.892757162696,-38.9320781145903,21.1433039191054));
#21603=CARTESIAN_POINT('Ctrl Pts',(128.862376103999,-38.9235230430346,21.141758780716));
#21604=CARTESIAN_POINT('Ctrl Pts',(128.83210654808,-38.9146193205452,21.1402136423267));
#21605=CARTESIAN_POINT('Ctrl Pts',(128.801956968712,-38.9053703915485,21.1386685039373));
#21606=CARTESIAN_POINT('Ctrl Pts',(128.688323845553,-38.8705113749443,21.1328449102228));
#21607=CARTESIAN_POINT('Ctrl Pts',(128.576030163275,-38.830632517438,21.1270213165083));
#21608=CARTESIAN_POINT('Ctrl Pts',(128.465551671052,-38.7858543719732,21.1211977227938));
#21609=CARTESIAN_POINT('Ctrl Pts',(128.355212563853,-38.7411327207887,21.1153814764076));
#21610=CARTESIAN_POINT('Ctrl Pts',(128.246684466789,-38.6915242278978,21.1095652300214));
#21611=CARTESIAN_POINT('Ctrl Pts',(128.14042865964,-38.6371993937798,21.1037489836352));
#21612=CARTESIAN_POINT('Ctrl Pts',(128.034279215138,-38.5829289391193,21.0979385593436));
#21613=CARTESIAN_POINT('Ctrl Pts',(127.930397897051,-38.5239517200571,21.092128135052));
#21614=CARTESIAN_POINT('Ctrl Pts',(127.829226092157,-38.4604863301319,21.0863177107604));
#21615=CARTESIAN_POINT('Ctrl Pts',(127.724224726253,-38.3946186445961,21.0802873499524));
#21616=CARTESIAN_POINT('Ctrl Pts',(127.622142463111,-38.3239164701803,21.0742569891444));
#21617=CARTESIAN_POINT('Ctrl Pts',(127.523445144338,-38.2486768147812,21.0682266283365));
#21618=CARTESIAN_POINT('Ctrl Pts',(127.428454506996,-38.1762628636363,21.06242274406));
#21619=CARTESIAN_POINT('Ctrl Pts',(127.336599502754,-38.0996463748078,21.0566188597836));
#21620=CARTESIAN_POINT('Ctrl Pts',(127.248265368406,-38.0191358891715,21.0508149755071));
#21621=CARTESIAN_POINT('Ctrl Pts',(127.159944281955,-37.9386372957963,21.0450119485266));
#21622=CARTESIAN_POINT('Ctrl Pts',(127.075143332853,-37.854246124464,21.039208921546));
#21623=CARTESIAN_POINT('Ctrl Pts',(126.994213187693,-37.7663099318341,21.0334058945654));
#21624=CARTESIAN_POINT('Ctrl Pts',(126.91327589725,-37.6783659753601,21.0276023552384));
#21625=CARTESIAN_POINT('Ctrl Pts',(126.836210366766,-37.5868766757659,21.0217988159114));
#21626=CARTESIAN_POINT('Ctrl Pts',(126.763328590582,-37.4922245459543,21.0159952765844));
#21627=CARTESIAN_POINT('Ctrl Pts',(126.69042317969,-37.3975417215643,21.0101898552374));
#21628=CARTESIAN_POINT('Ctrl Pts',(126.621704470347,-37.2996943505045,21.0043844338905));
#21629=CARTESIAN_POINT('Ctrl Pts',(126.557442170616,-37.1990954029655,20.9985790125435));
#21630=CARTESIAN_POINT('Ctrl Pts',(126.493108706341,-37.0983850514128,20.9927671622303));
#21631=CARTESIAN_POINT('Ctrl Pts',(126.433241722433,-36.9949173853986,20.9869553119172));
#21632=CARTESIAN_POINT('Ctrl Pts',(126.378065917287,-36.8891316789677,20.981143461604));
#21633=CARTESIAN_POINT('Ctrl Pts',(126.322853872378,-36.7832764919218,20.9753277940366));
#21634=CARTESIAN_POINT('Ctrl Pts',(126.272339314874,-36.6751006014944,20.9695121264692));
#21635=CARTESIAN_POINT('Ctrl Pts',(126.226698898587,-36.5650635124743,20.9636964589018));
#21636=CARTESIAN_POINT('Ctrl Pts',(126.180993107338,-36.4548688072199,20.9578724610193));
#21637=CARTESIAN_POINT('Ctrl Pts',(126.140175531616,-36.3428079645657,20.9520484631368));
#21638=CARTESIAN_POINT('Ctrl Pts',(126.104373121373,-36.2293560194356,20.9462244652543));
#21639=CARTESIAN_POINT('Ctrl Pts',(126.094874549378,-36.1992566082064,20.9446793272925));
#21640=CARTESIAN_POINT('Ctrl Pts',(126.08572870053,-36.1690593369959,20.9431341893307));
#21641=CARTESIAN_POINT('Ctrl Pts',(126.076937339023,-36.1387731811246,20.9415890513689));
#21642=CARTESIAN_POINT('Ctrl Pts',(126.035980316619,-35.997676632698,20.9343905929649));
#21643=CARTESIAN_POINT('Ctrl Pts',(126.002614949914,-35.8542850934519,20.927192134561));
#21644=CARTESIAN_POINT('Ctrl Pts',(125.977056286364,-35.7093298787686,20.919993676157));
#21645=CARTESIAN_POINT('Ctrl Pts',(125.951848625687,-35.5663653666423,20.9128940758009));
#21646=CARTESIAN_POINT('Ctrl Pts',(125.934234725755,-35.4218797790436,20.9057944754448));
#21647=CARTESIAN_POINT('Ctrl Pts',(125.924374885708,-35.2765952417385,20.8986948750887));
#21648=CARTESIAN_POINT('Ctrl Pts',(125.918213340713,-35.185805004833,20.8942582405354));
#21649=CARTESIAN_POINT('Ctrl Pts',(125.915078978048,-35.0947031752966,20.8898216059821));
#21650=CARTESIAN_POINT('Ctrl Pts',(125.915001474033,-35.0034702810671,20.8853849714288));
#21651=CARTESIAN_POINT('Ctrl Pts',(125.915001474033,-35.003470280567,20.8853849714045));
#21652=CARTESIAN_POINT('Ctrl Pts',(125.914898933796,-34.8827662892301,20.8795151642127));
#21653=CARTESIAN_POINT('Ctrl Pts',(125.920150846961,-34.7619569650232,20.8736453570208));
#21654=CARTESIAN_POINT('Ctrl Pts',(125.930756371625,-34.6415571273887,20.867775549829));
#21655=CARTESIAN_POINT('Ctrl Pts',(125.941161880961,-34.5234279754281,20.8620164445065));
#21656=CARTESIAN_POINT('Ctrl Pts',(125.956720796162,-34.4056934311284,20.8562573391841));
#21657=CARTESIAN_POINT('Ctrl Pts',(125.977379782769,-34.2888378610145,20.8504982338616));
#21658=CARTESIAN_POINT('Ctrl Pts',(125.998035648516,-34.1719999437465,20.8447399985413));
#21659=CARTESIAN_POINT('Ctrl Pts',(126.023789981672,-34.0560411455548,20.838981763221));
#21660=CARTESIAN_POINT('Ctrl Pts',(126.054537987098,-33.9414375291237,20.8332235279008));
#21661=CARTESIAN_POINT('Ctrl Pts',(126.085288892143,-33.8268231052669,20.8274647495636));
#21662=CARTESIAN_POINT('Ctrl Pts',(126.121034297585,-33.7135645182732,20.8217059712264));
#21663=CARTESIAN_POINT('Ctrl Pts',(126.161619205863,-33.6021237968987,20.8159471928892));
#21664=CARTESIAN_POINT('Ctrl Pts',(126.203573824735,-33.4869220337182,20.8099940600485));
#21665=CARTESIAN_POINT('Ctrl Pts',(126.250700225609,-33.3736634602182,20.8040409272077));
#21666=CARTESIAN_POINT('Ctrl Pts',(126.302773206644,-33.2628359206759,20.798087794367));
#21667=CARTESIAN_POINT('Ctrl Pts',(126.353220680837,-33.1554679665127,20.7923204941399));
#21668=CARTESIAN_POINT('Ctrl Pts',(126.408310257633,-33.0503818750327,20.7865531939128));
#21669=CARTESIAN_POINT('Ctrl Pts',(126.467791010027,-32.9479949680485,20.7807858936857));
#21670=CARTESIAN_POINT('Ctrl Pts',(126.530146624985,-32.8406594302205,20.7747398445382));
#21671=CARTESIAN_POINT('Ctrl Pts',(126.597328220364,-32.7362909643389,20.7686937953906));
#21672=CARTESIAN_POINT('Ctrl Pts',(126.668997397386,-32.6353337103565,20.7626477462431));
#21673=CARTESIAN_POINT('Ctrl Pts',(126.740666574408,-32.534376456374,20.7566016970955));
#21674=CARTESIAN_POINT('Ctrl Pts',(126.816822954776,-32.43683077537,20.750555647948));
#21675=CARTESIAN_POINT('Ctrl Pts',(126.897082912047,-32.3430975657186,20.7445095988004));
#21676=CARTESIAN_POINT('Ctrl Pts',(126.9743898227,-32.2528131311135,20.7386860051039));
#21677=CARTESIAN_POINT('Ctrl Pts',(127.055765126528,-32.1657599626625,20.7328624114074));
#21678=CARTESIAN_POINT('Ctrl Pts',(127.140908444355,-32.0823261874503,20.7270388177108));
#21679=CARTESIAN_POINT('Ctrl Pts',(127.225944341228,-31.9989976763494,20.7212225713435));
#21680=CARTESIAN_POINT('Ctrl Pts',(127.314738507605,-31.9192797592956,20.7154063249762));
#21681=CARTESIAN_POINT('Ctrl Pts',(127.406950539366,-31.8435273651268,20.7095900786089));
#21682=CARTESIAN_POINT('Ctrl Pts',(127.49907026636,-31.767850799533,20.7037796543371));
#21683=CARTESIAN_POINT('Ctrl Pts',(127.594600738773,-31.6961321176856,20.6979692300653));
#21684=CARTESIAN_POINT('Ctrl Pts',(127.693165392179,-31.6286888170687,20.6921588057936));
#21685=CARTESIAN_POINT('Ctrl Pts',(127.795460921015,-31.5586926484149,20.6861284449785));
#21686=CARTESIAN_POINT('Ctrl Pts',(127.901024549233,-31.4933022337859,20.6800980841634));
#21687=CARTESIAN_POINT('Ctrl Pts',(128.009398053128,-31.4328262042469,20.6740677233484));
#21688=CARTESIAN_POINT('Ctrl Pts',(128.113701475784,-31.3746214157803,20.6682638390938));
#21689=CARTESIAN_POINT('Ctrl Pts',(128.220607135908,-31.3209687562226,20.6624599548393));
#21690=CARTESIAN_POINT('Ctrl Pts',(128.329678398803,-31.2720983451041,20.6566560705848));
#21691=CARTESIAN_POINT('Ctrl Pts',(128.438733550691,-31.2232351526749,20.6508530436268));
#21692=CARTESIAN_POINT('Ctrl Pts',(128.549953296664,-31.1791529708189,20.6450500166689));
#21693=CARTESIAN_POINT('Ctrl Pts',(128.662879021698,-31.1400346517897,20.639246989711));
#21694=CARTESIAN_POINT('Ctrl Pts',(128.775814716876,-31.1009128790277,20.6334434504073));
#21695=CARTESIAN_POINT('Ctrl Pts',(128.890456304722,-31.0667559741176,20.6276399111036));
#21696=CARTESIAN_POINT('Ctrl Pts',(129.006328549081,-31.0376973806095,20.6218363717999));
#21697=CARTESIAN_POINT('Ctrl Pts',(129.12223836944,-31.0086293637427,20.616030950477));
#21698=CARTESIAN_POINT('Ctrl Pts',(129.239379244138,-30.9846630456388,20.6102255291541));
#21699=CARTESIAN_POINT('Ctrl Pts',(129.357264883258,-30.9658809425469,20.6044201078312));
#21700=CARTESIAN_POINT('Ctrl Pts',(129.475281069784,-30.9470780400187,20.5986082575429));
#21701=CARTESIAN_POINT('Ctrl Pts',(129.594043263529,-30.9334708763901,20.5927964072546));
#21702=CARTESIAN_POINT('Ctrl Pts',(129.713059015976,-30.9250902007913,20.5869845569663));
#21703=CARTESIAN_POINT('Ctrl Pts',(129.832152938592,-30.9167040207209,20.5811688894243));
#21704=CARTESIAN_POINT('Ctrl Pts',(129.95150034432,-30.9135511759163,20.5753532218823));
#21705=CARTESIAN_POINT('Ctrl Pts',(130.070609405729,-30.9156102889388,20.5695375543403));
#21706=CARTESIAN_POINT('Ctrl Pts',(130.18988907798,-30.9176723514179,20.5637135564838));
#21707=CARTESIAN_POINT('Ctrl Pts',(130.308929318364,-30.9249612477197,20.5578895586274));
#21708=CARTESIAN_POINT('Ctrl Pts',(130.427243892803,-30.9374038280844,20.5520655607709));
#21709=CARTESIAN_POINT('Ctrl Pts',(130.458633390305,-30.9407049120561,20.5505204225913));
#21710=CARTESIAN_POINT('Ctrl Pts',(130.489971870862,-30.9443684702231,20.5489752844116));
#21711=CARTESIAN_POINT('Ctrl Pts',(130.521250400698,-30.9483925387851,20.547430146232));
#21712=CARTESIAN_POINT('Ctrl Pts',(130.639133823985,-30.9635585641743,20.5416067849992));
#21713=CARTESIAN_POINT('Ctrl Pts',(130.756544892001,-30.9838981252513,20.5357834237664));
#21714=CARTESIAN_POINT('Ctrl Pts',(130.872994388123,-31.0093727562818,20.5299600625335));
#21715=CARTESIAN_POINT('Ctrl Pts',(130.989303093239,-31.0348165877036,20.5241437419227));
#21716=CARTESIAN_POINT('Ctrl Pts',(131.104652142935,-31.0653830568798,20.5183274213119));
#21717=CARTESIAN_POINT('Ctrl Pts',(131.218558069123,-31.1009820169465,20.5125111007011));
#21718=CARTESIAN_POINT('Ctrl Pts',(131.332533733271,-31.1366027721814,20.5066912190963));
#21719=CARTESIAN_POINT('Ctrl Pts',(131.445064099874,-31.1772621231237,20.5008713374914));
#21720=CARTESIAN_POINT('Ctrl Pts',(131.555674906802,-31.2228184337596,20.4950514558865));
#21721=CARTESIAN_POINT('Ctrl Pts',(131.666021155679,-31.2682657831728,20.4892454942283));
#21722=CARTESIAN_POINT('Ctrl Pts',(131.774456630174,-31.318586560334,20.4834395325702));
#21723=CARTESIAN_POINT('Ctrl Pts',(131.880526439234,-31.3735905758807,20.477633570912));
#21724=CARTESIAN_POINT('Ctrl Pts',(131.986977706055,-31.4287924018014,20.4718067293338));
#21725=CARTESIAN_POINT('Ctrl Pts',(132.091045869467,-31.4887110738161,20.4659798877556));
#21726=CARTESIAN_POINT('Ctrl Pts',(132.192293101711,-31.5531063323345,20.4601530461774));
#21727=CARTESIAN_POINT('Ctrl Pts',(132.293540333954,-31.617501590853,20.4543262045991));
#21728=CARTESIAN_POINT('Ctrl Pts',(132.391966277858,-31.6863732213768,20.4484993630209));
#21729=CARTESIAN_POINT('Ctrl Pts',(132.487160670875,-31.7594357285724,20.4426725214427));
#21730=CARTESIAN_POINT('',(125.915001496759,-34.9965030704355,20.9896150285509));
#21731=CARTESIAN_POINT('Ctrl Pts',(125.915001496759,-34.9965030704355,20.9896150285509));
#21732=CARTESIAN_POINT('Ctrl Pts',(125.91512689229,-34.8500201210564,20.9824905061118));
#21733=CARTESIAN_POINT('Ctrl Pts',(125.923135046557,-34.7038771894251,20.9753659836726));
#21734=CARTESIAN_POINT('Ctrl Pts',(125.938894207772,-34.5588143878878,20.9682414612335));
#21735=CARTESIAN_POINT('Ctrl Pts',(125.954891578428,-34.41155887264,20.9610092472438));
#21736=CARTESIAN_POINT('Ctrl Pts',(125.978876003809,-34.2654163169503,20.953777033254));
#21737=CARTESIAN_POINT('Ctrl Pts',(126.010660788167,-34.1211384335784,20.9465448192643));
#21738=CARTESIAN_POINT('Ctrl Pts',(126.028532809329,-34.0400135357117,20.9424782734601));
#21739=CARTESIAN_POINT('Ctrl Pts',(126.048870132568,-33.9594777781739,20.9384117276559));
#21740=CARTESIAN_POINT('Ctrl Pts',(126.071632971449,-33.8796618863085,20.9343451818516));
#21741=CARTESIAN_POINT('Ctrl Pts',(126.104231036441,-33.7653596393831,20.9285215881815));
#21742=CARTESIAN_POINT('Ctrl Pts',(126.14187452446,-33.6522969932765,20.9226979945113));
#21743=CARTESIAN_POINT('Ctrl Pts',(126.184452343526,-33.540951994904,20.9168744008411));
#21744=CARTESIAN_POINT('Ctrl Pts',(126.226976444347,-33.4297474747878,20.9110581544995));
#21745=CARTESIAN_POINT('Ctrl Pts',(126.274422349496,-33.3202566701994,20.9052419081578));
#21746=CARTESIAN_POINT('Ctrl Pts',(126.32662874226,-33.2129441522971,20.8994256618162));
#21747=CARTESIAN_POINT('Ctrl Pts',(126.378782876136,-33.1057390548189,20.8936152375693));
#21748=CARTESIAN_POINT('Ctrl Pts',(126.435687840096,-33.0007082713178,20.8878048133224));
#21749=CARTESIAN_POINT('Ctrl Pts',(126.497133839223,-32.8982974378659,20.8819943890755));
#21750=CARTESIAN_POINT('Ctrl Pts',(126.56090569653,-32.7920101425102,20.8759640282508));
#21751=CARTESIAN_POINT('Ctrl Pts',(126.629568996516,-32.6885454758239,20.8699336674261));
#21752=CARTESIAN_POINT('Ctrl Pts',(126.702836030425,-32.5883750793839,20.8639033066015));
#21753=CARTESIAN_POINT('Ctrl Pts',(126.773351443211,-32.4919666883655,20.8580994223699));
#21754=CARTESIAN_POINT('Ctrl Pts',(126.84813076695,-32.3986099494432,20.8522955381384));
#21755=CARTESIAN_POINT('Ctrl Pts',(126.926873163261,-32.3086961440013,20.8464916539068));
#21756=CARTESIAN_POINT('Ctrl Pts',(127.005603928477,-32.2187956197913,20.8406886269711));
#21757=CARTESIAN_POINT('Ctrl Pts',(127.088296333163,-32.1323373248072,20.8348856000354));
#21758=CARTESIAN_POINT('Ctrl Pts',(127.174609845076,-32.0496787509732,20.8290825730997));
#21759=CARTESIAN_POINT('Ctrl Pts',(127.260930977569,-31.9670128792525,20.8232790338174));
#21760=CARTESIAN_POINT('Ctrl Pts',(127.350873558013,-31.8881476781286,20.8174754945352));
#21761=CARTESIAN_POINT('Ctrl Pts',(127.444061337675,-31.8134026682948,20.811671955253));
#21762=CARTESIAN_POINT('Ctrl Pts',(127.537279337046,-31.738633419527,20.8058665339507));
#21763=CARTESIAN_POINT('Ctrl Pts',(127.633744310213,-31.6679872746706,20.8000611126484));
#21764=CARTESIAN_POINT('Ctrl Pts',(127.733048718335,-31.6017420806308,20.7942556913462));
#21765=CARTESIAN_POINT('Ctrl Pts',(127.832463096895,-31.5354235261713,20.7884438410772));
#21766=CARTESIAN_POINT('Ctrl Pts',(127.934722847032,-31.4735158774813,20.7826319908083));
#21767=CARTESIAN_POINT('Ctrl Pts',(128.039393238387,-31.416252502433,20.7768201405394));
#21768=CARTESIAN_POINT('Ctrl Pts',(128.144132377816,-31.3589515164932,20.7710044730161));
#21769=CARTESIAN_POINT('Ctrl Pts',(128.251284946046,-31.3063010587736,20.7651888054928));
#21770=CARTESIAN_POINT('Ctrl Pts',(128.360395032915,-31.2584868633254,20.7593731379695));
#21771=CARTESIAN_POINT('Ctrl Pts',(128.4696614082,-31.2106041792058,20.7535491401305));
#21772=CARTESIAN_POINT('Ctrl Pts',(128.580890519145,-31.1675717309309,20.7477251422915));
#21773=CARTESIAN_POINT('Ctrl Pts',(128.693609942556,-31.1295258665364,20.7419011444524));
#21774=CARTESIAN_POINT('Ctrl Pts',(128.723515020338,-31.1194320912171,20.7403560060627));
#21775=CARTESIAN_POINT('Ctrl Pts',(128.753524935726,-31.1096890286293,20.738810867673));
#21776=CARTESIAN_POINT('Ctrl Pts',(128.783630750152,-31.1002986206603,20.7372657292832));
#21777=CARTESIAN_POINT('Ctrl Pts',(128.897101478,-31.0649055762484,20.7314420044961));
#21778=CARTESIAN_POINT('Ctrl Pts',(129.012301234534,-31.0344121028999,20.725618279709));
#21779=CARTESIAN_POINT('Ctrl Pts',(129.128769267185,-31.0089873452721,20.7197945549218));
#21780=CARTESIAN_POINT('Ctrl Pts',(129.245089716674,-30.9835948047774,20.7139782097023));
#21781=CARTESIAN_POINT('Ctrl Pts',(129.362674850251,-30.9632582911488,20.7081618644827));
#21782=CARTESIAN_POINT('Ctrl Pts',(129.481047661269,-30.9480975492831,20.7023455192632));
#21783=CARTESIAN_POINT('Ctrl Pts',(129.599301329125,-30.9329520668231,20.6965350282407));
#21784=CARTESIAN_POINT('Ctrl Pts',(129.718340694462,-30.9229720438498,20.6907245372182));
#21785=CARTESIAN_POINT('Ctrl Pts',(129.837678020972,-30.9182262954538,20.6849140461958));
#21786=CARTESIAN_POINT('Ctrl Pts',(129.956926128198,-30.9134840950867,20.6791078992278));
#21787=CARTESIAN_POINT('Ctrl Pts',(130.076471346678,-30.9139683982542,20.6733017522598));
#21788=CARTESIAN_POINT('Ctrl Pts',(130.195820874261,-30.9196961895953,20.6674956052919));
#21789=CARTESIAN_POINT('Ctrl Pts',(130.315122580259,-30.9254216858953,20.6616917847609));
#21790=CARTESIAN_POINT('Ctrl Pts',(130.434228344077,-30.9363864729506,20.6558879642299));
#21791=CARTESIAN_POINT('Ctrl Pts',(130.552645896452,-30.9525554342111,20.6500841436989));
#21792=CARTESIAN_POINT('Ctrl Pts',(130.671043947322,-30.9687217326982,20.6442812789658));
#21793=CARTESIAN_POINT('Ctrl Pts',(130.788753607799,-30.9900904452799,20.6384784142326));
#21794=CARTESIAN_POINT('Ctrl Pts',(130.905288900095,-31.0165747142233,20.6326755494995));
#21795=CARTESIAN_POINT('Ctrl Pts',(131.021832502884,-31.0430608718421,20.6268722709461));
#21796=CARTESIAN_POINT('Ctrl Pts',(131.137201172975,-31.0746632200958,20.6210689923927));
#21797=CARTESIAN_POINT('Ctrl Pts',(131.250920904946,-31.1112441720303,20.6152657138392));
#21798=CARTESIAN_POINT('Ctrl Pts',(131.364740372975,-31.1478572066988,20.609457345614));
#21799=CARTESIAN_POINT('Ctrl Pts',(131.476907624376,-31.1894574428983,20.6036489773887));
#21800=CARTESIAN_POINT('Ctrl Pts',(131.586965380306,-31.2358578823707,20.5978406091634));
#21801=CARTESIAN_POINT('Ctrl Pts',(131.697070883064,-31.2822784519451,20.5920297210688));
#21802=CARTESIAN_POINT('Ctrl Pts',(131.8050646971,-31.3335032005729,20.5862188329742));
#21803=CARTESIAN_POINT('Ctrl Pts',(131.910512544768,-31.3892982930898,20.5804079448795));
#21804=CARTESIAN_POINT('Ctrl Pts',(132.016116110585,-31.4451757799725,20.5745884756639));
#21805=CARTESIAN_POINT('Ctrl Pts',(132.119165843915,-31.5056368914197,20.5687690064483));
#21806=CARTESIAN_POINT('Ctrl Pts',(132.21925449863,-31.5704031621328,20.5629495372327));
#21807=CARTESIAN_POINT('Ctrl Pts',(132.311149248095,-31.6298672466273,20.5576064874425));
#21808=CARTESIAN_POINT('Ctrl Pts',(132.400548046593,-31.6929598019526,20.5522634376522));
#21809=CARTESIAN_POINT('Ctrl Pts',(132.487160670875,-31.7594357285724,20.546920387862));
#21810=CARTESIAN_POINT('Ctrl Pts',(132.487160670875,-31.7594357285724,21.7969524316048));
#21811=CARTESIAN_POINT('Ctrl Pts',(132.581957158607,-31.8321928400738,21.7911469930517));
#21812=CARTESIAN_POINT('Ctrl Pts',(132.673521068581,-31.9090843242138,21.7853415544986));
#21813=CARTESIAN_POINT('Ctrl Pts',(132.761485630824,-31.9897803882855,21.7795361159454));
#21814=CARTESIAN_POINT('Ctrl Pts',(132.849547669554,-32.0705658743763,21.7737242441909));
#21815=CARTESIAN_POINT('Ctrl Pts',(132.934002098028,-32.1551640796059,21.7679123724363));
#21816=CARTESIAN_POINT('Ctrl Pts',(133.014518887018,-32.2432082269764,21.7621005006818));
#21817=CARTESIAN_POINT('Ctrl Pts',(133.095088674169,-32.3313103272023,21.7562848034082));
#21818=CARTESIAN_POINT('Ctrl Pts',(133.171715398641,-32.4228625743367,21.7504691061346));
#21819=CARTESIAN_POINT('Ctrl Pts',(133.244110264468,-32.5174662959045,21.744653408861));
#21820=CARTESIAN_POINT('Ctrl Pts',(133.316608699753,-32.6122053593371,21.7388293915414));
#21821=CARTESIAN_POINT('Ctrl Pts',(133.384862959886,-32.7100042767398,21.7330053742217));
#21822=CARTESIAN_POINT('Ctrl Pts',(133.448628295567,-32.8104366008229,21.7271813569022));
#21823=CARTESIAN_POINT('Ctrl Pts',(133.465118347645,-32.8364089294683,21.7256752353099));
#21824=CARTESIAN_POINT('Ctrl Pts',(133.481308438933,-32.8625572522097,21.7241691137177));
#21825=CARTESIAN_POINT('Ctrl Pts',(133.497194851732,-32.8888739570981,21.7226629921254));
#21826=CARTESIAN_POINT('Ctrl Pts',(133.558621507787,-32.9906305462117,21.7168393984549));
#21827=CARTESIAN_POINT('Ctrl Pts',(133.615702371735,-33.0952344137982,21.7110158047843));
#21828=CARTESIAN_POINT('Ctrl Pts',(133.668163334243,-33.2022784550113,21.7051922111138));
#21829=CARTESIAN_POINT('Ctrl Pts',(133.720558109454,-33.3091874442664,21.6993759647716));
#21830=CARTESIAN_POINT('Ctrl Pts',(133.768344398241,-33.4185301203645,21.6935597184295));
#21831=CARTESIAN_POINT('Ctrl Pts',(133.811292182914,-33.5298718095139,21.6877434720874));
#21832=CARTESIAN_POINT('Ctrl Pts',(133.854196976617,-33.6411020450188,21.6819330478399));
#21833=CARTESIAN_POINT('Ctrl Pts',(133.892272755379,-33.754326934,21.6761226235925));
#21834=CARTESIAN_POINT('Ctrl Pts',(133.925336397826,-33.8690892325637,21.670312199345));
#21835=CARTESIAN_POINT('Ctrl Pts',(133.959651567534,-33.9881955215219,21.6642818385205));
#21836=CARTESIAN_POINT('Ctrl Pts',(133.988567467094,-34.1089575054924,21.658251477696));
#21837=CARTESIAN_POINT('Ctrl Pts',(134.011935046681,-34.2308432011541,21.6522211168715));
#21838=CARTESIAN_POINT('Ctrl Pts',(134.03442503205,-34.3481513503324,21.6464172326392));
#21839=CARTESIAN_POINT('Ctrl Pts',(134.051775844246,-34.4664998918664,21.6406133484068));
#21840=CARTESIAN_POINT('Ctrl Pts',(134.063906187566,-34.5854020035479,21.6348094641745));
#21841=CARTESIAN_POINT('Ctrl Pts',(134.076034739105,-34.7042865521161,21.6290064372379));
#21842=CARTESIAN_POINT('Ctrl Pts',(134.082944313849,-34.823724102102,21.6232034103013));
#21843=CARTESIAN_POINT('Ctrl Pts',(134.084605395569,-34.943221813292,21.6174003833647));
#21844=CARTESIAN_POINT('Ctrl Pts',(134.086266623946,-35.0627300748804,21.6115968440815));
#21845=CARTESIAN_POINT('Ctrl Pts',(134.082678432297,-35.182298099916,21.6057933047983));
#21846=CARTESIAN_POINT('Ctrl Pts',(134.073863433233,-35.3014327907893,21.5999897655151));
#21847=CARTESIAN_POINT('Ctrl Pts',(134.065045575568,-35.4206061156535,21.5941843442118));
#21848=CARTESIAN_POINT('Ctrl Pts',(134.050997569646,-35.5393454198682,21.5883789229085));
#21849=CARTESIAN_POINT('Ctrl Pts',(134.031793849582,-35.6571631110081,21.5825735016052));
#21850=CARTESIAN_POINT('Ctrl Pts',(134.012568863176,-35.7751112743365,21.5767616513352));
#21851=CARTESIAN_POINT('Ctrl Pts',(133.988176831755,-35.8921353841254,21.5709498010651));
#21852=CARTESIAN_POINT('Ctrl Pts',(133.958743270378,-36.0077582642874,21.565137950795));
#21853=CARTESIAN_POINT('Ctrl Pts',(133.92929037688,-36.1234570861776,21.5593222832705));
#21854=CARTESIAN_POINT('Ctrl Pts',(133.894789476611,-36.2377524555536,21.553506615746));
#21855=CARTESIAN_POINT('Ctrl Pts',(133.855415376923,-36.350184162025,21.5476909482214));
#21856=CARTESIAN_POINT('Ctrl Pts',(133.81598487809,-36.4627769147761,21.5418669503811));
#21857=CARTESIAN_POINT('Ctrl Pts',(133.771667398671,-36.5735002987015,21.5360429525408));
#21858=CARTESIAN_POINT('Ctrl Pts',(133.722685139917,-36.6819156783392,21.5302189547005));
#21859=CARTESIAN_POINT('Ctrl Pts',(133.709689879603,-36.7106788696696,21.5286738163193));
#21860=CARTESIAN_POINT('Ctrl Pts',(133.696366524453,-36.7392797522863,21.5271286779382));
#21861=CARTESIAN_POINT('Ctrl Pts',(133.682719745472,-36.7677104616737,21.525583539557));
#21862=CARTESIAN_POINT('Ctrl Pts',(133.631285325959,-36.8748652002156,21.5197599458861));
#21863=CARTESIAN_POINT('Ctrl Pts',(133.575087319942,-36.9799460179862,21.5139363522152));
#21864=CARTESIAN_POINT('Ctrl Pts',(133.514315961416,-37.0825004978007,21.5081127585444));
#21865=CARTESIAN_POINT('Ctrl Pts',(133.453621274985,-37.1849255899053,21.502296512202));
#21866=CARTESIAN_POINT('Ctrl Pts',(133.3883649187,-37.2848303354245,21.4964802658595));
#21867=CARTESIAN_POINT('Ctrl Pts',(133.318784353857,-37.3817840818588,21.4906640195171));
#21868=CARTESIAN_POINT('Ctrl Pts',(133.249273439543,-37.4786407770581,21.4848535952694));
#21869=CARTESIAN_POINT('Ctrl Pts',(133.175447164514,-37.5725520198836,21.4790431710217));
#21870=CARTESIAN_POINT('Ctrl Pts',(133.0975875739,-37.663114008453,21.4732327467739));
#21871=CARTESIAN_POINT('Ctrl Pts',(133.01678083673,-37.7571039556174,21.4672023859495));
#21872=CARTESIAN_POINT('Ctrl Pts',(132.931629640789,-37.8474857007242,21.4611720251251));
#21873=CARTESIAN_POINT('Ctrl Pts',(132.842497217892,-37.933842968919,21.4551416643007));
#21874=CARTESIAN_POINT('Ctrl Pts',(132.756712257601,-38.0169569983845,21.4493377800681));
#21875=CARTESIAN_POINT('Ctrl Pts',(132.667240035614,-38.0963430768909,21.4435338958355));
#21876=CARTESIAN_POINT('Ctrl Pts',(132.574443152638,-38.1716663528558,21.4377300116029));
#21877=CARTESIAN_POINT('Ctrl Pts',(132.481659976753,-38.2469785027672,21.4319269846661));
#21878=CARTESIAN_POINT('Ctrl Pts',(132.385553433452,-38.3182287863131,21.4261239577293));
#21879=CARTESIAN_POINT('Ctrl Pts',(132.286519540347,-38.385122359917,21.4203209307924));
#21880=CARTESIAN_POINT('Ctrl Pts',(132.187476903585,-38.452021839524,21.414517391509));
#21881=CARTESIAN_POINT('Ctrl Pts',(132.085506741543,-38.5145636158361,21.4087138522256));
#21882=CARTESIAN_POINT('Ctrl Pts',(131.981033862242,-38.5724963032383,21.4029103129422));
#21883=CARTESIAN_POINT('Ctrl Pts',(131.876527103605,-38.6304477775353,21.3971048916386));
#21884=CARTESIAN_POINT('Ctrl Pts',(131.769516370539,-38.6837869924312,21.3912994703351));
#21885=CARTESIAN_POINT('Ctrl Pts',(131.660450273352,-38.732308922065,21.3854940490315));
#21886=CARTESIAN_POINT('Ctrl Pts',(131.551263395557,-38.7808845852445,21.3796821987613));
#21887=CARTESIAN_POINT('Ctrl Pts',(131.440016983603,-38.8246321485716,21.373870348491));
#21888=CARTESIAN_POINT('Ctrl Pts',(131.327178936584,-38.8633950186705,21.3680584982208));
#21889=CARTESIAN_POINT('Ctrl Pts',(131.21426677693,-38.9021833484305,21.362242830696));
#21890=CARTESIAN_POINT('Ctrl Pts',(131.099761291015,-38.9359803494343,21.3564271631713));
#21891=CARTESIAN_POINT('Ctrl Pts',(130.984143208555,-38.9646799549341,21.3506114956466));
#21892=CARTESIAN_POINT('Ctrl Pts',(130.868359515676,-38.9934206695197,21.3447874978061));
#21893=CARTESIAN_POINT('Ctrl Pts',(130.751460444186,-39.0170493346535,21.3389634999656));
#21894=CARTESIAN_POINT('Ctrl Pts',(130.63393465876,-39.0355113490638,21.3331395021252));
#21895=CARTESIAN_POINT('Ctrl Pts',(130.602754427149,-39.0404094221398,21.3315943637463));
#21896=CARTESIAN_POINT('Ctrl Pts',(130.571530096223,-39.0449441144374,21.3300492253674));
#21897=CARTESIAN_POINT('Ctrl Pts',(130.540270804112,-39.0491150216096,21.3285040869885));
#21898=CARTESIAN_POINT('Ctrl Pts',(130.422455197195,-39.0648350820046,21.3226804933117));
#21899=CARTESIAN_POINT('Ctrl Pts',(130.303762933154,-39.0754341682595,21.316856899635));
#21900=CARTESIAN_POINT('Ctrl Pts',(130.184676680017,-39.0808233879767,21.3110333059582));
#21901=CARTESIAN_POINT('Ctrl Pts',(130.065740671876,-39.0862058083928,21.3052170596099));
#21902=CARTESIAN_POINT('Ctrl Pts',(129.946412067634,-39.0863914175571,21.2994008132615));
#21903=CARTESIAN_POINT('Ctrl Pts',(129.827181220251,-39.0813427532328,21.2935845669132));
#21904=CARTESIAN_POINT('Ctrl Pts',(129.708069723603,-39.0762991426494,21.2877741426595));
#21905=CARTESIAN_POINT('Ctrl Pts',(129.589056194769,-39.0660316991624,21.2819637184058));
#21906=CARTESIAN_POINT('Ctrl Pts',(129.470632968861,-39.050554967698,21.2761532941521));
#21907=CARTESIAN_POINT('Ctrl Pts',(129.347727179064,-39.0344924099563,21.2701229333299));
#21908=CARTESIAN_POINT('Ctrl Pts',(129.2254577113,-39.0128183873161,21.2640925725078));
#21909=CARTESIAN_POINT('Ctrl Pts',(129.104371836293,-38.9856085096726,21.2580622116856));
#21910=CARTESIAN_POINT('Ctrl Pts',(128.987833469488,-38.9594205277848,21.2522583274471));
#21911=CARTESIAN_POINT('Ctrl Pts',(128.872391830741,-38.9281050996682,21.2464544432085));
#21912=CARTESIAN_POINT('Ctrl Pts',(128.758525744755,-38.8917819406493,21.24065055897));
#21913=CARTESIAN_POINT('Ctrl Pts',(128.644676478008,-38.8554641469495,21.2348475320272));
#21914=CARTESIAN_POINT('Ctrl Pts',(128.53240269012,-38.8141402174323,21.2290445050844));
#21915=CARTESIAN_POINT('Ctrl Pts',(128.422168062184,-38.7679797472927,21.2232414781417));
#21916=CARTESIAN_POINT('Ctrl Pts',(128.311923701683,-38.7218152016666,21.2174379388524));
#21917=CARTESIAN_POINT('Ctrl Pts',(128.203719235756,-38.6708134241352,21.211634399563));
#21918=CARTESIAN_POINT('Ctrl Pts',(128.097997780361,-38.6151919114329,21.2058308602737));
#21919=CARTESIAN_POINT('Ctrl Pts',(127.992242040732,-38.5595523613225,21.2000254389642));
#21920=CARTESIAN_POINT('Ctrl Pts',(127.888971274208,-38.4992902866326,21.1942200176547));
#21921=CARTESIAN_POINT('Ctrl Pts',(127.788602870336,-38.4346685043705,21.1884145963453));
#21922=CARTESIAN_POINT('Ctrl Pts',(127.688123317749,-38.3699751594673,21.1826027460692));
#21923=CARTESIAN_POINT('Ctrl Pts',(127.590552886961,-38.3009126911278,21.1767908957931));
#21924=CARTESIAN_POINT('Ctrl Pts',(127.496279033396,-38.2277865978695,21.170979045517));
#21925=CARTESIAN_POINT('Ctrl Pts',(127.401943260257,-38.1546124750005,21.1651633779864));
#21926=CARTESIAN_POINT('Ctrl Pts',(127.310908687054,-38.077369675391,21.1593477104559));
#21927=CARTESIAN_POINT('Ctrl Pts',(127.223527543474,-37.9964021255757,21.1535320429253));
#21928=CARTESIAN_POINT('Ctrl Pts',(127.136021235844,-37.91531859849,21.1477080450792));
#21929=CARTESIAN_POINT('Ctrl Pts',(127.052179088948,-37.830499961599,21.141884047233));
#21930=CARTESIAN_POINT('Ctrl Pts',(126.972314637893,-37.7423249895085,21.1360600493868));
#21931=CARTESIAN_POINT('Ctrl Pts',(126.951126164413,-37.7189316895732,21.1345149110645));
#21932=CARTESIAN_POINT('Ctrl Pts',(126.930217438473,-37.695302314154,21.1329697727423));
#21933=CARTESIAN_POINT('Ctrl Pts',(126.909593807446,-37.6714442844691,21.1314246344201));
#21934=CARTESIAN_POINT('Ctrl Pts',(126.830727378882,-37.5802092545508,21.1255159008441));
#21935=CARTESIAN_POINT('Ctrl Pts',(126.755762331177,-37.4853140262217,21.119607167268));
#21936=CARTESIAN_POINT('Ctrl Pts',(126.685059339014,-37.3871307911681,21.113698433692));
#21937=CARTESIAN_POINT('Ctrl Pts',(126.616054083285,-37.2913051544312,21.1079315819793));
#21938=CARTESIAN_POINT('Ctrl Pts',(126.551108816856,-37.1923479642437,21.1021647302665));
#21939=CARTESIAN_POINT('Ctrl Pts',(126.490521185757,-37.0906418756876,21.0963978785538));
#21940=CARTESIAN_POINT('Ctrl Pts',(126.429989538292,-36.9890297646709,21.0906363554752));
#21941=CARTESIAN_POINT('Ctrl Pts',(126.373807733833,-36.8846741590728,21.0848748323965));
#21942=CARTESIAN_POINT('Ctrl Pts',(126.322231234452,-36.7779881628293,21.0791133093179));
#21943=CARTESIAN_POINT('Ctrl Pts',(126.270689699326,-36.6713744901527,21.0733556920368));
#21944=CARTESIAN_POINT('Ctrl Pts',(126.223747441912,-36.5624339410496,21.0675980747557));
#21945=CARTESIAN_POINT('Ctrl Pts',(126.181614543349,-36.451605147564,21.0618404574746));
#21946=CARTESIAN_POINT('Ctrl Pts',(126.137570475,-36.3357491034337,21.0558216717347));
#21947=CARTESIAN_POINT('Ctrl Pts',(126.09878257563,-36.2178298937377,21.0498028859948));
#21948=CARTESIAN_POINT('Ctrl Pts',(126.065434963677,-36.0983728760976,21.0437841002549));
#21949=CARTESIAN_POINT('Ctrl Pts',(126.033547892699,-35.9841477733897,21.038028922092));
#21950=CARTESIAN_POINT('Ctrl Pts',(126.006634741561,-35.8685171588103,21.0322737439292));
#21951=CARTESIAN_POINT('Ctrl Pts',(125.984805368353,-35.7519554973474,21.0265185657663));
#21952=CARTESIAN_POINT('Ctrl Pts',(125.962975205303,-35.6353896183894,21.0207631793666));
#21953=CARTESIAN_POINT('Ctrl Pts',(125.946229255171,-35.5178930355523,21.0150077929669));
#21954=CARTESIAN_POINT('Ctrl Pts',(125.934625988469,-35.3999489296956,21.0092524065672));
#21955=CARTESIAN_POINT('Ctrl Pts',(125.923016652512,-35.2819431314981,21.0034940097308));
#21956=CARTESIAN_POINT('Ctrl Pts',(125.916555398921,-35.1634897576063,20.9977356128944));
#21957=CARTESIAN_POINT('Ctrl Pts',(125.915248694863,-35.0450752169156,20.9919772160581));
#21958=CARTESIAN_POINT('Ctrl Pts',(125.915070017821,-35.0288833640235,20.9911898202372));
#21959=CARTESIAN_POINT('Ctrl Pts',(125.91498763816,-35.0126922353489,20.9904024244164));
#21960=CARTESIAN_POINT('Ctrl Pts',(125.915001496758,-34.9965030713517,20.9896150285955));
#21961=CARTESIAN_POINT('Origin',(130.,-35.,32.7603849714045));
#21962=CARTESIAN_POINT('',(132.487160670875,-31.7594357285724,23.0467792200739));
#21963=CARTESIAN_POINT('',(132.487160670875,-31.7594357285724,22.9427607399423));
#21964=CARTESIAN_POINT('',(132.487160670875,-31.7594357285724,32.7603849714045));
#21965=CARTESIAN_POINT('',(125.915000225098,-34.9986438840781,22.1353849714387));
#21966=CARTESIAN_POINT('Ctrl Pts',(132.487160670875,-31.7594357285724,22.9427607399423));
#21967=CARTESIAN_POINT('Ctrl Pts',(132.581883176809,-31.8321360584143,22.9369379462702));
#21968=CARTESIAN_POINT('Ctrl Pts',(132.673310070028,-31.9089120318643,22.931115152598));
#21969=CARTESIAN_POINT('Ctrl Pts',(132.761090344536,-31.9894178122312,22.9252923589258));
#21970=CARTESIAN_POINT('Ctrl Pts',(132.825958200078,-32.0489099630639,22.920989431635));
#21971=CARTESIAN_POINT('Ctrl Pts',(132.888835410539,-32.1104381248282,22.9166865043441));
#21972=CARTESIAN_POINT('Ctrl Pts',(132.949594421577,-32.1738510746601,22.9123835770533));
#21973=CARTESIAN_POINT('Ctrl Pts',(133.031825834812,-32.2596743359825,22.9065599833817));
#21974=CARTESIAN_POINT('Ctrl Pts',(133.110440991607,-32.3492279582961,22.9007363897102));
#21975=CARTESIAN_POINT('Ctrl Pts',(133.185083236696,-32.4421747957844,22.8949127960386));
#21976=CARTESIAN_POINT('Ctrl Pts',(133.259631309504,-32.535004367031,22.8890965496955));
#21977=CARTESIAN_POINT('Ctrl Pts',(133.330216186761,-32.6312183229795,22.8832803033524));
#21978=CARTESIAN_POINT('Ctrl Pts',(133.396518192138,-32.7304429572103,22.8774640570093));
#21979=CARTESIAN_POINT('Ctrl Pts',(133.462753828841,-32.8295682670347,22.8716536327609));
#21980=CARTESIAN_POINT('Ctrl Pts',(133.524714896913,-32.9316979221826,22.8658432085125));
#21981=CARTESIAN_POINT('Ctrl Pts',(133.582122530858,-33.0364259184035,22.8600327842641));
#21982=CARTESIAN_POINT('Ctrl Pts',(133.641703162486,-33.145118085894,22.8540024234399));
#21983=CARTESIAN_POINT('Ctrl Pts',(133.696378554533,-33.2566088367296,22.8479720626158));
#21984=CARTESIAN_POINT('Ctrl Pts',(133.74588670753,-33.3704117776715,22.8419417017917));
#21985=CARTESIAN_POINT('Ctrl Pts',(133.79353552938,-33.4799407285751,22.8361378175583));
#21986=CARTESIAN_POINT('Ctrl Pts',(133.836398057633,-33.5916109199558,22.830333933325));
#21987=CARTESIAN_POINT('Ctrl Pts',(133.874288296302,-33.70496517532,22.8245300490917));
#21988=CARTESIAN_POINT('Ctrl Pts',(133.912172938179,-33.8183026870484,22.8187270221542));
#21989=CARTESIAN_POINT('Ctrl Pts',(133.945086621664,-33.9333233808971,22.8129239952166));
#21990=CARTESIAN_POINT('Ctrl Pts',(133.972892553101,-34.0495528623264,22.8071209682791));
#21991=CARTESIAN_POINT('Ctrl Pts',(134.000700939511,-34.1657926056034,22.8013174289949));
#21992=CARTESIAN_POINT('Ctrl Pts',(134.023400582241,-34.2832409515025,22.7955138897108));
#21993=CARTESIAN_POINT('Ctrl Pts',(134.040905493144,-34.4014118314883,22.7897103504266));
#21994=CARTESIAN_POINT('Ctrl Pts',(134.058416080684,-34.5196210329124,22.7839049291224));
#21995=CARTESIAN_POINT('Ctrl Pts',(134.070728526322,-34.6385528306901,22.7780995078181));
#21996=CARTESIAN_POINT('Ctrl Pts',(134.077808610295,-34.7577151721628,22.7722940865139));
#21997=CARTESIAN_POINT('Ctrl Pts',(134.084896534807,-34.877009474899,22.7664822362429));
#21998=CARTESIAN_POINT('Ctrl Pts',(134.086740507389,-34.9965344230827,22.7606703859719));
#21999=CARTESIAN_POINT('Ctrl Pts',(134.083358430272,-35.1157969340037,22.7548585357009));
#22000=CARTESIAN_POINT('Ctrl Pts',(134.079974131789,-35.2351377771821,22.7490428681754));
#22001=CARTESIAN_POINT('Ctrl Pts',(134.071356977106,-35.3542154334826,22.74322720065));
#22002=CARTESIAN_POINT('Ctrl Pts',(134.057576680408,-35.4725425722714,22.7374115331245));
#22003=CARTESIAN_POINT('Ctrl Pts',(134.043776644923,-35.5910392019093,22.7315875352833));
#22004=CARTESIAN_POINT('Ctrl Pts',(134.024798770866,-35.7087827666205,22.7257635374421));
#22005=CARTESIAN_POINT('Ctrl Pts',(134.000763742125,-35.825296601048,22.7199395396009));
#22006=CARTESIAN_POINT('Ctrl Pts',(133.994387117992,-35.856208356401,22.7183944012289));
#22007=CARTESIAN_POINT('Ctrl Pts',(133.987654806676,-35.8870336423118,22.7168492628569));
#22008=CARTESIAN_POINT('Ctrl Pts',(133.980569642328,-35.9177637618566,22.7153041244849));
#22009=CARTESIAN_POINT('Ctrl Pts',(133.953865808544,-36.0335849290374,22.7094805308135));
#22010=CARTESIAN_POINT('Ctrl Pts',(133.9220597084,-36.1484264117011,22.7036569371421));
#22011=CARTESIAN_POINT('Ctrl Pts',(133.885237815503,-36.261805102616,22.6978333434707));
#22012=CARTESIAN_POINT('Ctrl Pts',(133.848462378892,-36.3750407494713,22.6920170971278));
#22013=CARTESIAN_POINT('Ctrl Pts',(133.806683861123,-36.4868168903464,22.6862008507848));
#22014=CARTESIAN_POINT('Ctrl Pts',(133.760039584541,-36.5966613049366,22.6803846044419));
#22015=CARTESIAN_POINT('Ctrl Pts',(133.713441999138,-36.7063957646617,22.6745741801936));
#22016=CARTESIAN_POINT('Ctrl Pts',(133.661988503165,-36.8142019712026,22.6687637559454));
#22017=CARTESIAN_POINT('Ctrl Pts',(133.605865802954,-36.9196241327626,22.6629533316971));
#22018=CARTESIAN_POINT('Ctrl Pts',(133.547618742458,-37.0290367411901,22.6569229708729));
#22019=CARTESIAN_POINT('Ctrl Pts',(133.48434215393,-37.1358808302264,22.6508926100487));
#22020=CARTESIAN_POINT('Ctrl Pts',(133.416299224074,-37.2396706480178,22.6448622492245));
#22021=CARTESIAN_POINT('Ctrl Pts',(133.350811718553,-37.3395625292177,22.6390583649913));
#22022=CARTESIAN_POINT('Ctrl Pts',(133.280909669463,-37.436625042598,22.6332544807582));
#22023=CARTESIAN_POINT('Ctrl Pts',(133.206873489809,-37.5304520189804,22.627450596525));
#22024=CARTESIAN_POINT('Ctrl Pts',(133.132848246089,-37.624265136115,22.6216475695876));
#22025=CARTESIAN_POINT('Ctrl Pts',(133.054690339081,-37.7148433462175,22.6158445426502));
#22026=CARTESIAN_POINT('Ctrl Pts',(132.972721553387,-37.8018121932118,22.6100415157128));
#22027=CARTESIAN_POINT('Ctrl Pts',(132.890745530706,-37.8887887186459,22.6042379764288));
#22028=CARTESIAN_POINT('Ctrl Pts',(132.804958240457,-37.9721549502126,22.5984344371448));
#22029=CARTESIAN_POINT('Ctrl Pts',(132.715719080768,-38.0515725248392,22.5926308978609));
#22030=CARTESIAN_POINT('Ctrl Pts',(132.62645098186,-38.131015853659,22.5868254765568));
#22031=CARTESIAN_POINT('Ctrl Pts',(132.533729092154,-38.2065077075828,22.5810200552527));
#22032=CARTESIAN_POINT('Ctrl Pts',(132.437946192269,-38.277749740844,22.5752146339485));
#22033=CARTESIAN_POINT('Ctrl Pts',(132.342057221687,-38.3490706680631,22.5694027836777));
#22034=CARTESIAN_POINT('Ctrl Pts',(132.243100802464,-38.4161321366339,22.5635909334068));
#22035=CARTESIAN_POINT('Ctrl Pts',(132.141499148098,-38.478678829483,22.557779083136));
#22036=CARTESIAN_POINT('Ctrl Pts',(132.039830761221,-38.5412666033358,22.5519634156107));
#22037=CARTESIAN_POINT('Ctrl Pts',(131.935514035084,-38.5993334977942,22.5461477480854));
#22038=CARTESIAN_POINT('Ctrl Pts',(131.828994773743,-38.652670682887,22.5403320805601));
#22039=CARTESIAN_POINT('Ctrl Pts',(131.722322935062,-38.706084267738,22.534508082719));
#22040=CARTESIAN_POINT('Ctrl Pts',(131.613442635645,-38.7547544550479,22.5286840848779));
#22041=CARTESIAN_POINT('Ctrl Pts',(131.502818699154,-38.798520890751,22.5228600870369));
#22042=CARTESIAN_POINT('Ctrl Pts',(131.473469565799,-38.8101323647112,22.5213149486634));
#22043=CARTESIAN_POINT('Ctrl Pts',(131.443997778231,-38.8213989527745,22.5197698102899));
#22044=CARTESIAN_POINT('Ctrl Pts',(131.414412163886,-38.8323182580068,22.5182246719164));
#22045=CARTESIAN_POINT('Ctrl Pts',(131.302904612573,-38.8734728872218,22.5124010782451));
#22046=CARTESIAN_POINT('Ctrl Pts',(131.189419564544,-38.9098231007079,22.5065774845737));
#22047=CARTESIAN_POINT('Ctrl Pts',(131.07440847843,-38.9411764007054,22.5007538909024));
#22048=CARTESIAN_POINT('Ctrl Pts',(130.959542495885,-38.9724901438579,22.4949376445594));
#22049=CARTESIAN_POINT('Ctrl Pts',(130.843154695165,-38.9988194062718,22.4891213982165));
#22050=CARTESIAN_POINT('Ctrl Pts',(130.725715302816,-39.0200201864243,22.4833051518736));
#22051=CARTESIAN_POINT('Ctrl Pts',(130.608393467947,-39.0411997444788,22.4774947276254));
#22052=CARTESIAN_POINT('Ctrl Pts',(130.490022535097,-39.0572609608853,22.4716843033772));
#22053=CARTESIAN_POINT('Ctrl Pts',(130.371086060982,-39.0681101429711,22.4658738791289));
#22054=CARTESIAN_POINT('Ctrl Pts',(130.247647595317,-39.0793699890391,22.4598435183047));
#22055=CARTESIAN_POINT('Ctrl Pts',(130.123600361081,-39.0850153142089,22.4538131574805));
#22056=CARTESIAN_POINT('Ctrl Pts',(129.999494896475,-39.0849999687724,22.4477827966563));
#22057=CARTESIAN_POINT('Ctrl Pts',(129.880050344106,-39.08498519965,22.4419789124232));
#22058=CARTESIAN_POINT('Ctrl Pts',(129.760552301349,-39.0797272772828,22.4361750281901));
#22059=CARTESIAN_POINT('Ctrl Pts',(129.641494188579,-39.069238083865,22.4303711439569));
#22060=CARTESIAN_POINT('Ctrl Pts',(129.522453661967,-39.0587504398133,22.4245681170196));
#22061=CARTESIAN_POINT('Ctrl Pts',(129.403853342764,-39.0430330972231,22.4187650900822));
#22062=CARTESIAN_POINT('Ctrl Pts',(129.286182805827,-39.0221499242697,22.4129620631449));
#22063=CARTESIAN_POINT('Ctrl Pts',(129.168501879813,-39.0012649075506,22.4071585238609));
#22064=CARTESIAN_POINT('Ctrl Pts',(129.051751301354,-38.9752132250104,22.401354984577));
#22065=CARTESIAN_POINT('Ctrl Pts',(128.936411076525,-38.9441099885602,22.395551445293));
#22066=CARTESIAN_POINT('Ctrl Pts',(128.821033448205,-38.9129966656931,22.389746023989));
#22067=CARTESIAN_POINT('Ctrl Pts',(128.707067477154,-38.8768286372472,22.3839406026849));
#22068=CARTESIAN_POINT('Ctrl Pts',(128.59497799919,-38.8357708713164,22.3781351813808));
#22069=CARTESIAN_POINT('Ctrl Pts',(128.482764392504,-38.7946676377102,22.37232333111));
#22070=CARTESIAN_POINT('Ctrl Pts',(128.372431810508,-38.7486639984812,22.3665114808392));
#22071=CARTESIAN_POINT('Ctrl Pts',(128.264425235097,-38.6979731252989,22.3606996305684));
#22072=CARTESIAN_POINT('Ctrl Pts',(128.156347720388,-38.647248958079,22.3548839630431));
#22073=CARTESIAN_POINT('Ctrl Pts',(128.050599615636,-38.5918316148993,22.3490682955179));
#22074=CARTESIAN_POINT('Ctrl Pts',(127.947599953748,-38.5319794804252,22.3432526279926));
#22075=CARTESIAN_POINT('Ctrl Pts',(127.844452755967,-38.4720416142313,22.3374286301516));
#22076=CARTESIAN_POINT('Ctrl Pts',(127.744062201284,-38.4076564974399,22.3316046323106));
#22077=CARTESIAN_POINT('Ctrl Pts',(127.646817204616,-38.3391249948913,22.3257806344696));
#22078=CARTESIAN_POINT('Ctrl Pts',(127.621017576917,-38.3209432136995,22.3242354960957));
#22079=CARTESIAN_POINT('Ctrl Pts',(127.595439167258,-38.3024697941764,22.3226903577218));
#22080=CARTESIAN_POINT('Ctrl Pts',(127.570088819245,-38.2837108054217,22.321145219348));
#22081=CARTESIAN_POINT('Ctrl Pts',(127.475346633759,-38.2136025926574,22.315370553598));
#22082=CARTESIAN_POINT('Ctrl Pts',(127.383475506378,-38.1392680574956,22.309595887848));
#22083=CARTESIAN_POINT('Ctrl Pts',(127.29488013663,-38.0609723168952,22.303821222098));
#22084=CARTESIAN_POINT('Ctrl Pts',(127.206396987134,-37.9827757504145,22.2980538708889));
#22085=CARTESIAN_POINT('Ctrl Pts',(127.121181654222,-37.9006282275451,22.2922865196798));
#22086=CARTESIAN_POINT('Ctrl Pts',(127.039608898642,-37.814837389087,22.2865191684706));
#22087=CARTESIAN_POINT('Ctrl Pts',(126.95811726467,-37.7291318669908,22.2807575527157));
#22088=CARTESIAN_POINT('Ctrl Pts',(126.88026128903,-37.6397905344547,22.2749959369607));
#22089=CARTESIAN_POINT('Ctrl Pts',(126.806381191527,-37.5471599687034,22.2692343212057));
#22090=CARTESIAN_POINT('Ctrl Pts',(126.732553088088,-37.4545945928993,22.2634767602617));
#22091=CARTESIAN_POINT('Ctrl Pts',(126.662695556031,-37.35874491222,22.2577191993176));
#22092=CARTESIAN_POINT('Ctrl Pts',(126.597110128043,-37.2599923715208,22.2519616383735));
#22093=CARTESIAN_POINT('Ctrl Pts',(126.53154875107,-37.1612760446406,22.2462061888007));
#22094=CARTESIAN_POINT('Ctrl Pts',(126.470256594023,-37.0596593197758,22.2404507392278));
#22095=CARTESIAN_POINT('Ctrl Pts',(126.413492877872,-36.955554055229,22.2346952896549));
#22096=CARTESIAN_POINT('Ctrl Pts',(126.356735998231,-36.8514613289169,22.2289405332572));
#22097=CARTESIAN_POINT('Ctrl Pts',(126.304506673962,-36.7448810241795,22.2231857768594));
#22098=CARTESIAN_POINT('Ctrl Pts',(126.257018645826,-36.6362504644172,22.2174310204617));
#22099=CARTESIAN_POINT('Ctrl Pts',(126.209524641704,-36.5276062343738,22.2116755398742));
#22100=CARTESIAN_POINT('Ctrl Pts',(126.166773285701,-36.4169116179162,22.2059200592867));
#22101=CARTESIAN_POINT('Ctrl Pts',(126.128930263853,-36.3046241213032,22.2001645786991));
#22102=CARTESIAN_POINT('Ctrl Pts',(126.091051218587,-36.1922297363084,22.1944036193716));
#22103=CARTESIAN_POINT('Ctrl Pts',(126.058089971144,-36.0782398380018,22.188642660044));
#22104=CARTESIAN_POINT('Ctrl Pts',(126.030162393893,-35.9631273961087,22.1828817007164));
#22105=CARTESIAN_POINT('Ctrl Pts',(126.002220875286,-35.8479574904619,22.1771178655368));
#22106=CARTESIAN_POINT('Ctrl Pts',(125.979318111483,-35.7316643332545,22.1713540303573));
#22107=CARTESIAN_POINT('Ctrl Pts',(125.961518545287,-35.6147296478435,22.1655901951777));
#22108=CARTESIAN_POINT('Ctrl Pts',(125.943692203764,-35.4976190612692,22.1598176896424));
#22109=CARTESIAN_POINT('Ctrl Pts',(125.930984437041,-35.3798654324984,22.1540451841071));
#22110=CARTESIAN_POINT('Ctrl Pts',(125.923407691792,-35.2619544858525,22.1482726785719));
#22111=CARTESIAN_POINT('Ctrl Pts',(125.917769073044,-35.1742050825885,22.1439767761941));
#22112=CARTESIAN_POINT('Ctrl Pts',(125.914971102718,-35.0863686220552,22.1396808738164));
#22113=CARTESIAN_POINT('Ctrl Pts',(125.915000225098,-34.9986438840781,22.1353849714387));
#22114=CARTESIAN_POINT('Ctrl Pts',(125.915000225098,-34.9986438833803,22.1353849714045));
#22115=CARTESIAN_POINT('Ctrl Pts',(125.915025803142,-34.921595712626,22.1316119031962));
#22116=CARTESIAN_POINT('Ctrl Pts',(125.917231078305,-34.8445868960673,22.1278388349879));
#22117=CARTESIAN_POINT('Ctrl Pts',(125.921610227948,-34.7677030623887,22.1240657667795));
#22118=CARTESIAN_POINT('Ctrl Pts',(125.928369286289,-34.6490356589768,22.118242173109));
#22119=CARTESIAN_POINT('Ctrl Pts',(125.940322775489,-34.5304721391276,22.1124185794384));
#22120=CARTESIAN_POINT('Ctrl Pts',(125.957467056685,-34.4125032747234,22.1065949857679));
#22121=CARTESIAN_POINT('Ctrl Pts',(125.974589707823,-34.2946832455644,22.1007787394257));
#22122=CARTESIAN_POINT('Ctrl Pts',(125.99689006703,-34.1774567801585,22.0949624930836));
#22123=CARTESIAN_POINT('Ctrl Pts',(126.024312538453,-34.0613125077557,22.0891462467415));
#22124=CARTESIAN_POINT('Ctrl Pts',(126.05170755983,-33.9452844964101,22.083335822494));
#22125=CARTESIAN_POINT('Ctrl Pts',(126.084214400078,-33.8303369181398,22.0775253982466));
#22126=CARTESIAN_POINT('Ctrl Pts',(126.121726014143,-33.716950550204,22.0717149739991));
#22127=CARTESIAN_POINT('Ctrl Pts',(126.160657520395,-33.5992722736939,22.0656846131746));
#22128=CARTESIAN_POINT('Ctrl Pts',(126.204980104197,-33.4832761764104,22.0596542523501));
#22129=CARTESIAN_POINT('Ctrl Pts',(126.254516398774,-33.3694854821411,22.0536238915256));
#22130=CARTESIAN_POINT('Ctrl Pts',(126.302192305306,-33.2599683179982,22.0478200072933));
#22131=CARTESIAN_POINT('Ctrl Pts',(126.354697194335,-33.1524942997649,22.0420161230609));
#22132=CARTESIAN_POINT('Ctrl Pts',(126.41182327944,-33.0475111211504,22.0362122388286));
#22133=CARTESIAN_POINT('Ctrl Pts',(126.468940926411,-32.9425434496741,22.030409211892));
#22134=CARTESIAN_POINT('Ctrl Pts',(126.530678216865,-32.8400662447102,22.0246061849554));
#22135=CARTESIAN_POINT('Ctrl Pts',(126.596781231034,-32.7405029297297,22.0188031580188));
#22136=CARTESIAN_POINT('Ctrl Pts',(126.662890081408,-32.6409308243493,22.0129996187356));
#22137=CARTESIAN_POINT('Ctrl Pts',(126.73336519599,-32.544273460662,22.0071960794524));
#22138=CARTESIAN_POINT('Ctrl Pts',(126.807909486029,-32.4509250402118,22.0013925401692));
#22139=CARTESIAN_POINT('Ctrl Pts',(126.882477949913,-32.3575463479574,21.9955871188659));
#22140=CARTESIAN_POINT('Ctrl Pts',(126.961117958938,-32.2674790519153,21.9897816975626));
#22141=CARTESIAN_POINT('Ctrl Pts',(127.043492762845,-32.1810835491896,21.9839762762592));
#22142=CARTESIAN_POINT('Ctrl Pts',(127.125958789223,-32.094592371441,21.9781644259892));
#22143=CARTESIAN_POINT('Ctrl Pts',(127.212167584225,-32.0117813991429,21.9723525757191));
#22144=CARTESIAN_POINT('Ctrl Pts',(127.301746120357,-31.932973589779,21.966540725449));
#22145=CARTESIAN_POINT('Ctrl Pts',(127.391383492153,-31.8541140190227,21.9607250579245));
#22146=CARTESIAN_POINT('Ctrl Pts',(127.484394695461,-31.7792631029338,21.9549093903999));
#22147=CARTESIAN_POINT('Ctrl Pts',(127.580375599858,-31.70870196393,21.9490937228754));
#22148=CARTESIAN_POINT('Ctrl Pts',(127.676493986537,-31.6380397537135,21.9432697250351));
#22149=CARTESIAN_POINT('Ctrl Pts',(127.775590226525,-31.5716798113531,21.9374457271948));
#22150=CARTESIAN_POINT('Ctrl Pts',(127.877233255865,-31.5098586919733,21.9316217293544));
#22151=CARTESIAN_POINT('Ctrl Pts',(127.904199705735,-31.4934572119356,21.9300765909733));
#22152=CARTESIAN_POINT('Ctrl Pts',(127.931345296024,-31.4773749482052,21.9285314525922));
#22153=CARTESIAN_POINT('Ctrl Pts',(127.958661730927,-31.4616157541588,21.9269863142111));
#22154=CARTESIAN_POINT('Ctrl Pts',(128.061616792655,-31.4022196872256,21.9211627205402));
#22155=CARTESIAN_POINT('Ctrl Pts',(128.167332366969,-31.3472250375658,21.9153391268693));
#22156=CARTESIAN_POINT('Ctrl Pts',(128.275395991733,-31.2968977850092,21.9095155331985));
#22157=CARTESIAN_POINT('Ctrl Pts',(128.383323278183,-31.2466340277573,21.903699286856));
#22158=CARTESIAN_POINT('Ctrl Pts',(128.493592356012,-31.2010261261643,21.8978830405136));
#22159=CARTESIAN_POINT('Ctrl Pts',(128.605764074192,-31.1602954302203,21.8920667941712));
#22160=CARTESIAN_POINT('Ctrl Pts',(128.717823507863,-31.1196055059278,21.8862563699235));
#22161=CARTESIAN_POINT('Ctrl Pts',(128.831781411402,-31.0837832134984,21.8804459456757));
#22162=CARTESIAN_POINT('Ctrl Pts',(128.94717699838,-31.0530025681208,21.874635521428));
#22163=CARTESIAN_POINT('Ctrl Pts',(129.066940547023,-31.0210568116458,21.8686051606036));
#22164=CARTESIAN_POINT('Ctrl Pts',(129.188252361851,-30.9945421062579,21.8625747997792));
#22165=CARTESIAN_POINT('Ctrl Pts',(129.31057760758,-30.9735969197273,21.8565444389548));
#22166=CARTESIAN_POINT('Ctrl Pts',(129.428308799065,-30.9534383518746,21.8507405547222));
#22167=CARTESIAN_POINT('Ctrl Pts',(129.546978234582,-30.9384385838142,21.8449366704896));
#22168=CARTESIAN_POINT('Ctrl Pts',(129.666097575084,-30.928669238365,21.839132786257));
#22169=CARTESIAN_POINT('Ctrl Pts',(129.785199320386,-30.9189013359527,21.8333297593202));
#22170=CARTESIAN_POINT('Ctrl Pts',(129.904750431653,-30.9143623530833,21.8275267323834));
#22171=CARTESIAN_POINT('Ctrl Pts',(130.024257580144,-30.9150720239145,21.8217237054465));
#22172=CARTESIAN_POINT('Ctrl Pts',(130.143775279866,-30.9157817574023,21.8159201661631));
#22173=CARTESIAN_POINT('Ctrl Pts',(130.263248600744,-30.9217410635192,21.8101166268797));
#22174=CARTESIAN_POINT('Ctrl Pts',(130.382184990751,-30.9329175527358,21.8043130875963));
#22175=CARTESIAN_POINT('Ctrl Pts',(130.501159950442,-30.9440976663574,21.7985076662927));
#22176=CARTESIAN_POINT('Ctrl Pts',(130.619597226637,-30.9604982896458,21.7927022449892));
#22177=CARTESIAN_POINT('Ctrl Pts',(130.737010799371,-30.9820353309654,21.7868968236857));
#22178=CARTESIAN_POINT('Ctrl Pts',(130.854554396769,-31.0035962225649,21.7810849734154));
#22179=CARTESIAN_POINT('Ctrl Pts',(130.971071625956,-31.0303048124299,21.7752731231451));
#22180=CARTESIAN_POINT('Ctrl Pts',(131.086087894523,-31.0620261446564,21.7694612728749));
#22181=CARTESIAN_POINT('Ctrl Pts',(131.201179706394,-31.0937683116242,21.7636456053501));
#22182=CARTESIAN_POINT('Ctrl Pts',(131.314768206717,-31.1305296524004,21.7578299378254));
#22183=CARTESIAN_POINT('Ctrl Pts',(131.426396743237,-31.1721262650287,21.7520142703007));
#22184=CARTESIAN_POINT('Ctrl Pts',(131.538185175581,-31.213782460313,21.7461902724602));
#22185=CARTESIAN_POINT('Ctrl Pts',(131.648007665952,-31.2602875927179,21.7403662746197));
#22186=CARTESIAN_POINT('Ctrl Pts',(131.755430072907,-31.3114108036901,21.7345422767793));
#22187=CARTESIAN_POINT('Ctrl Pts',(131.783929823127,-31.3249740702793,21.7329971384004));
#22188=CARTESIAN_POINT('Ctrl Pts',(131.812260788292,-31.3388621474973,21.7314520000215));
#22189=CARTESIAN_POINT('Ctrl Pts',(131.84041519809,-31.353070209253,21.7299068616426));
#22190=CARTESIAN_POINT('Ctrl Pts',(131.946546836178,-31.4066293099055,21.7240822654817));
#22191=CARTESIAN_POINT('Ctrl Pts',(132.050509721292,-31.4649115473487,21.7182576693207));
#22192=CARTESIAN_POINT('Ctrl Pts',(132.15185506879,-31.5277176435486,21.7124330731598));
#22193=CARTESIAN_POINT('Ctrl Pts',(132.253060538421,-31.5904370541431,21.706616516165));
#22194=CARTESIAN_POINT('Ctrl Pts',(132.351655314945,-31.6576676858431,21.7007999591702));
#22195=CARTESIAN_POINT('Ctrl Pts',(132.447213477537,-31.7291635327704,21.6949834021754));
#22196=CARTESIAN_POINT('Ctrl Pts',(132.460589040624,-31.7391710212468,21.6941692412192));
#22197=CARTESIAN_POINT('Ctrl Pts',(132.473905147975,-31.7492620018798,21.6933550802631));
#22198=CARTESIAN_POINT('Ctrl Pts',(132.487160670875,-31.7594357285724,21.6925409193069));
#22199=CARTESIAN_POINT('',(125.915000722565,-35.0024296824293,22.2396150286373));
#22200=CARTESIAN_POINT('Ctrl Pts',(125.915000722565,-35.0024296815665,22.2396150285955));
#22201=CARTESIAN_POINT('Ctrl Pts',(125.914929010373,-34.8818606921115,22.233766442302));
#22202=CARTESIAN_POINT('Ctrl Pts',(125.920199535175,-34.7612723331104,22.2279178560086));
#22203=CARTESIAN_POINT('Ctrl Pts',(125.930790852349,-34.6411658981193,22.2220692697151));
#22204=CARTESIAN_POINT('Ctrl Pts',(125.941383317302,-34.5210464472191,22.2162200496115));
#22205=CARTESIAN_POINT('Ctrl Pts',(125.957297687507,-34.4014094220477,22.210370829508));
#22206=CARTESIAN_POINT('Ctrl Pts',(125.978460616568,-34.282751097943,22.2045216094045));
#22207=CARTESIAN_POINT('Ctrl Pts',(125.999630529126,-34.164053618095,22.1986704591324));
#22208=CARTESIAN_POINT('Ctrl Pts',(126.026052377497,-34.0463358750143,22.1928193088603));
#22209=CARTESIAN_POINT('Ctrl Pts',(126.057601774298,-33.930083540654,22.1869681585883));
#22210=CARTESIAN_POINT('Ctrl Pts',(126.089190817938,-33.8136851167277,22.1811096554144));
#22211=CARTESIAN_POINT('Ctrl Pts',(126.125920177321,-33.6987561662663,22.1752511522405));
#22212=CARTESIAN_POINT('Ctrl Pts',(126.167615514837,-33.5857672900539,22.1693926490666));
#22213=CARTESIAN_POINT('Ctrl Pts',(126.209337132696,-33.4727071975717,22.1635304533102));
#22214=CARTESIAN_POINT('Ctrl Pts',(126.25603081164,-33.3615899841467,22.1576682575538));
#22215=CARTESIAN_POINT('Ctrl Pts',(126.307474687368,-33.2528646830963,22.1518060617975));
#22216=CARTESIAN_POINT('Ctrl Pts',(126.359011363295,-33.1439432512265,22.1459332911588));
#22217=CARTESIAN_POINT('Ctrl Pts',(126.415315175187,-33.0374227087894,22.1400605205202));
#22218=CARTESIAN_POINT('Ctrl Pts',(126.476118646657,-32.9337267345384,22.1341877498816));
#22219=CARTESIAN_POINT('Ctrl Pts',(126.536050842734,-32.8315166581898,22.1283991323418));
#22220=CARTESIAN_POINT('Ctrl Pts',(126.600354320998,-32.7320509915407,22.1226105148021));
#22221=CARTESIAN_POINT('Ctrl Pts',(126.668734188096,-32.635704525564,22.1168218972623));
#22222=CARTESIAN_POINT('Ctrl Pts',(126.73752722176,-32.5387759125289,22.110998303591));
#22223=CARTESIAN_POINT('Ctrl Pts',(126.81066514483,-32.4446959552825,22.1051747099196));
#22224=CARTESIAN_POINT('Ctrl Pts',(126.887884046831,-32.3538784430739,22.0993511162483));
#22225=CARTESIAN_POINT('Ctrl Pts',(126.965005525716,-32.2631755106467,22.0935348699054));
#22226=CARTESIAN_POINT('Ctrl Pts',(127.046197480592,-32.1757271448576,22.0877186235624));
#22227=CARTESIAN_POINT('Ctrl Pts',(127.131153127975,-32.091917706654,22.0819023772195));
#22228=CARTESIAN_POINT('Ctrl Pts',(127.216023734286,-32.0081921621603,22.0760919529713));
#22229=CARTESIAN_POINT('Ctrl Pts',(127.304650249154,-31.928098583899,22.0702815287231));
#22230=CARTESIAN_POINT('Ctrl Pts',(127.396686480553,-31.8519873381029,22.0644711044748));
#22231=CARTESIAN_POINT('Ctrl Pts',(127.492206473676,-31.7729951242263,22.0584407436506));
#22232=CARTESIAN_POINT('Ctrl Pts',(127.591399122868,-31.6982930200788,22.0524103828264));
#22233=CARTESIAN_POINT('Ctrl Pts',(127.693836109116,-31.6282299739775,22.0463800220022));
#22234=CARTESIAN_POINT('Ctrl Pts',(127.792425965794,-31.5607982198177,22.0405761377691));
#22235=CARTESIAN_POINT('Ctrl Pts',(127.894020497765,-31.4976636093088,22.0347722535359));
#22236=CARTESIAN_POINT('Ctrl Pts',(127.998205759725,-31.4390949437533,22.0289683693028));
#22237=CARTESIAN_POINT('Ctrl Pts',(128.102375632409,-31.380534929416,22.0231653423654));
#22238=CARTESIAN_POINT('Ctrl Pts',(128.209135118203,-31.3265397188316,22.0173623154281));
#22239=CARTESIAN_POINT('Ctrl Pts',(128.318044091939,-31.2773330362037,22.0115592884907));
#22240=CARTESIAN_POINT('Ctrl Pts',(128.426962681199,-31.2281220091405,22.0057557492068));
#22241=CARTESIAN_POINT('Ctrl Pts',(128.538030763587,-31.1837005187533,21.9999522099228));
#22242=CARTESIAN_POINT('Ctrl Pts',(128.650787176772,-31.1442445931261,21.9941486706389));
#22243=CARTESIAN_POINT('Ctrl Pts',(128.763580155547,-31.1047758724024,21.9883432493348));
#22244=CARTESIAN_POINT('Ctrl Pts',(128.87806216876,-31.0702760537098,21.9825378280308));
#22245=CARTESIAN_POINT('Ctrl Pts',(128.993756423474,-31.0408714513545,21.9767324067267));
#22246=CARTESIAN_POINT('Ctrl Pts',(129.109578798866,-31.0114342861237,21.9709205564559));
#22247=CARTESIAN_POINT('Ctrl Pts',(129.226615699404,-30.9871037007483,21.9651087061851));
#22248=CARTESIAN_POINT('Ctrl Pts',(129.344379500266,-30.9679550150911,21.9592968559143));
#22249=CARTESIAN_POINT('Ctrl Pts',(129.462220649026,-30.9487937524743,21.953481188389));
#22250=CARTESIAN_POINT('Ctrl Pts',(129.580789244328,-30.9348212154102,21.9476655208637));
#22251=CARTESIAN_POINT('Ctrl Pts',(129.699593548547,-30.926060755985,21.9418498533384));
#22252=CARTESIAN_POINT('Ctrl Pts',(129.818568027102,-30.9172877481478,21.9360258554974));
#22253=CARTESIAN_POINT('Ctrl Pts',(129.937778481752,-30.9137417312552,21.9302018576564));
#22254=CARTESIAN_POINT('Ctrl Pts',(130.05673404596,-30.9153939910893,21.9243778598154));
#22255=CARTESIAN_POINT('Ctrl Pts',(130.088293605571,-30.9158323446298,21.9228327214416));
#22256=CARTESIAN_POINT('Ctrl Pts',(130.119835259209,-30.91663630686,21.9212875830677));
#22257=CARTESIAN_POINT('Ctrl Pts',(130.151349931726,-30.9178047329695,21.9197424446939));
#22258=CARTESIAN_POINT('Ctrl Pts',(130.27011093384,-30.9222078710817,21.9139196908137));
#22259=CARTESIAN_POINT('Ctrl Pts',(130.388871112727,-30.9318049791032,21.9080969369335));
#22260=CARTESIAN_POINT('Ctrl Pts',(130.507139933393,-30.9466021552334,21.9022741830532));
#22261=CARTESIAN_POINT('Ctrl Pts',(130.625268256982,-30.9613817531045,21.8964583462953));
#22262=CARTESIAN_POINT('Ctrl Pts',(130.742905981611,-30.9813490860618,21.8906425095373));
#22263=CARTESIAN_POINT('Ctrl Pts',(130.859563574337,-31.006458280965,21.8848266727793));
#22264=CARTESIAN_POINT('Ctrl Pts',(130.97611012843,-31.0315435760891,21.8790163717311));
#22265=CARTESIAN_POINT('Ctrl Pts',(131.091678009264,-31.0617609139633,21.8732060706829));
#22266=CARTESIAN_POINT('Ctrl Pts',(131.205784439581,-31.0970128253781,21.8673957696346));
#22267=CARTESIAN_POINT('Ctrl Pts',(131.321068739188,-31.1326286263979,21.8615254914655));
#22268=CARTESIAN_POINT('Ctrl Pts',(131.434860824508,-31.1733834844684,21.8556552132963));
#22269=CARTESIAN_POINT('Ctrl Pts',(131.546674675407,-31.2191241162327,21.8497849351272));
#22270=CARTESIAN_POINT('Ctrl Pts',(131.65721808492,-31.2643450378611,21.8439813557102));
#22271=CARTESIAN_POINT('Ctrl Pts',(131.765827598369,-31.3144388528637,21.8381777762933));
#22272=CARTESIAN_POINT('Ctrl Pts',(131.872050994275,-31.3692080650586,21.8323741968764));
#22273=CARTESIAN_POINT('Ctrl Pts',(131.980105579379,-31.4249214458048,21.8264705693311));
#22274=CARTESIAN_POINT('Ctrl Pts',(132.085690609827,-31.4854727630239,21.8205669417858));
#22275=CARTESIAN_POINT('Ctrl Pts',(132.188354523964,-31.5506044765137,21.8146633142406));
#22276=CARTESIAN_POINT('Ctrl Pts',(132.2910184381,-31.6157361900034,21.8087596866953));
#22277=CARTESIAN_POINT('Ctrl Pts',(132.390760863858,-31.6854480558678,21.80285605915));
#22278=CARTESIAN_POINT('Ctrl Pts',(132.487160670875,-31.7594357285724,21.7969524316048));
#22279=CARTESIAN_POINT('Ctrl Pts',(132.487160670875,-31.7594357285724,23.0467792200739));
#22280=CARTESIAN_POINT('Ctrl Pts',(132.583414813671,-31.8333116027474,23.0408775737182));
#22281=CARTESIAN_POINT('Ctrl Pts',(132.676442847798,-31.9115320435499,23.0349759273624));
#22282=CARTESIAN_POINT('Ctrl Pts',(132.765836767039,-31.9937777896347,23.0290742810067));
#22283=CARTESIAN_POINT('Ctrl Pts',(132.853746479267,-32.0746580098064,23.0232706196704));
#22284=CARTESIAN_POINT('Ctrl Pts',(132.938141520463,-32.1594306027935,23.0174669583341));
#22285=CARTESIAN_POINT('Ctrl Pts',(133.018667701034,-32.2477517715999,23.0116632969978));
#22286=CARTESIAN_POINT('Ctrl Pts',(133.099184936904,-32.3360631298518,23.0058602803216));
#22287=CARTESIAN_POINT('Ctrl Pts',(133.175833891759,-32.4279219783005,23.0000572636454));
#22288=CARTESIAN_POINT('Ctrl Pts',(133.248298528059,-32.522948996769,22.9942542469692));
#22289=CARTESIAN_POINT('Ctrl Pts',(133.320772216772,-32.6179878861828,22.9884505053698));
#22290=CARTESIAN_POINT('Ctrl Pts',(133.389060299958,-32.7161954078661,22.9826467637704));
#22291=CARTESIAN_POINT('Ctrl Pts',(133.452888584027,-32.8171611543005,22.976843022171));
#22292=CARTESIAN_POINT('Ctrl Pts',(133.51860336843,-32.9211110310011,22.9708677459514));
#22293=CARTESIAN_POINT('Ctrl Pts',(133.579590374359,-33.0279843254672,22.9648924697318));
#22294=CARTESIAN_POINT('Ctrl Pts',(133.635600506457,-33.1373046525406,22.9589171935123));
#22295=CARTESIAN_POINT('Ctrl Pts',(133.690084466923,-33.2436462046002,22.9531047324249));
#22296=CARTESIAN_POINT('Ctrl Pts',(133.739859151942,-33.3523027579522,22.9472922713375));
#22297=CARTESIAN_POINT('Ctrl Pts',(133.784744129264,-33.4628152759022,22.9414798102501));
#22298=CARTESIAN_POINT('Ctrl Pts',(133.831515042701,-33.5779712082205,22.9354231264644));
#22299=CARTESIAN_POINT('Ctrl Pts',(133.872976211536,-33.6951419989656,22.9293664426788));
#22300=CARTESIAN_POINT('Ctrl Pts',(133.908981331102,-33.8137917749825,22.9233097588931));
#22301=CARTESIAN_POINT('Ctrl Pts',(133.944986450668,-33.9324415509994,22.9172530751074));
#22302=CARTESIAN_POINT('Ctrl Pts',(133.975535465614,-34.0525698163222,22.9111963913218));
#22303=CARTESIAN_POINT('Ctrl Pts',(134.00054240192,-34.1736311414126,22.9051397075361));
#22304=CARTESIAN_POINT('Ctrl Pts',(134.024586951902,-34.2900334486165,22.8993161138646));
#22305=CARTESIAN_POINT('Ctrl Pts',(134.043585686199,-34.4076737573641,22.8934925201931));
#22306=CARTESIAN_POINT('Ctrl Pts',(134.057415670364,-34.5260769283036,22.8876689265217));
#22307=CARTESIAN_POINT('Ctrl Pts',(134.071228205949,-34.6443307160558,22.8818526801786));
#22308=CARTESIAN_POINT('Ctrl Pts',(134.079884914853,-34.7633450496769,22.8760364338356));
#22309=CARTESIAN_POINT('Ctrl Pts',(134.083313617438,-34.882633473061,22.8702201874926));
#22310=CARTESIAN_POINT('Ctrl Pts',(134.086738887873,-35.0018024880749,22.8644097632442));
#22311=CARTESIAN_POINT('Ctrl Pts',(134.084946551254,-35.1212446412136,22.8585993389959));
#22312=CARTESIAN_POINT('Ctrl Pts',(134.077916163162,-35.2404678070435,22.8527889147475));
#22313=CARTESIAN_POINT('Ctrl Pts',(134.070619660339,-35.3642038162958,22.8467585539234));
#22314=CARTESIAN_POINT('Ctrl Pts',(134.057680676829,-35.4877034872399,22.8407281930992));
#22315=CARTESIAN_POINT('Ctrl Pts',(134.039135779025,-35.6104155622194,22.834697832275));
#22316=CARTESIAN_POINT('Ctrl Pts',(134.021287354509,-35.7285190551891,22.8288939480418));
#22317=CARTESIAN_POINT('Ctrl Pts',(133.998246560815,-35.845892603303,22.8230900638086));
#22318=CARTESIAN_POINT('Ctrl Pts',(133.970098817708,-35.962050091022,22.8172861795753));
#22319=CARTESIAN_POINT('Ctrl Pts',(133.941955232323,-36.0781904210379,22.8114831526379));
#22320=CARTESIAN_POINT('Ctrl Pts',(133.90870629383,-36.1931146511323,22.8056801257004));
#22321=CARTESIAN_POINT('Ctrl Pts',(133.870488251105,-36.3063482300135,22.7998770987629));
#22322=CARTESIAN_POINT('Ctrl Pts',(133.832266834126,-36.4195918062359,22.7940735594788));
#22323=CARTESIAN_POINT('Ctrl Pts',(133.789075571221,-36.5311440475533,22.7882700201948));
#22324=CARTESIAN_POINT('Ctrl Pts',(133.74109995193,-36.6405475152117,22.7824664809107));
#22325=CARTESIAN_POINT('Ctrl Pts',(133.693108774706,-36.749986461139,22.7766610596065));
#22326=CARTESIAN_POINT('Ctrl Pts',(133.640330319394,-36.857274873817,22.7708556383023));
#22327=CARTESIAN_POINT('Ctrl Pts',(133.582997107867,-36.9619777585432,22.7650502169981));
#22328=CARTESIAN_POINT('Ctrl Pts',(133.525600405114,-37.0667965920228,22.7592383667271));
#22329=CARTESIAN_POINT('Ctrl Pts',(133.463639074183,-37.1690238239237,22.7534265164562));
#22330=CARTESIAN_POINT('Ctrl Pts',(133.397390335889,-37.2682512880201,22.7476146661853));
#22331=CARTESIAN_POINT('Ctrl Pts',(133.331098085069,-37.3675439252471,22.7417989986599));
#22332=CARTESIAN_POINT('Ctrl Pts',(133.260513059629,-37.4638325422687,22.7359833311345));
#22333=CARTESIAN_POINT('Ctrl Pts',(133.18595331224,-37.5567413815683,22.7301676636092));
#22334=CARTESIAN_POINT('Ctrl Pts',(133.111286766065,-37.649783302748,22.724343665768));
#22335=CARTESIAN_POINT('Ctrl Pts',(133.032634402642,-37.7394354776361,22.7185196679269));
#22336=CARTESIAN_POINT('Ctrl Pts',(132.950351781853,-37.8253582716739,22.7126956700858));
#22337=CARTESIAN_POINT('Ctrl Pts',(132.928521754051,-37.8481540572805,22.7111505317131));
#22338=CARTESIAN_POINT('Ctrl Pts',(132.906436386135,-37.8706875610478,22.7096053933404));
#22339=CARTESIAN_POINT('Ctrl Pts',(132.884102700967,-37.8929529222359,22.7080602549676));
#22340=CARTESIAN_POINT('Ctrl Pts',(132.799927516468,-37.9768705951102,22.7022366612962));
#22341=CARTESIAN_POINT('Ctrl Pts',(132.711950970825,-38.0572467206934,22.6964130676247));
#22342=CARTESIAN_POINT('Ctrl Pts',(132.620503068697,-38.1337180260751,22.6905894739533));
#22343=CARTESIAN_POINT('Ctrl Pts',(132.529170541681,-38.2100928515462,22.6847732276103));
#22344=CARTESIAN_POINT('Ctrl Pts',(132.434375679651,-38.2825723958932,22.6789569812673));
#22345=CARTESIAN_POINT('Ctrl Pts',(132.336485774208,-38.3508296326316,22.6731407349243));
#22346=CARTESIAN_POINT('Ctrl Pts',(132.238693857101,-38.4190185434996,22.667330310676));
#22347=CARTESIAN_POINT('Ctrl Pts',(132.137813393003,-38.4829933227504,22.6615198864277));
#22348=CARTESIAN_POINT('Ctrl Pts',(132.03424477454,-38.5424671060233,22.6557094621793));
#22349=CARTESIAN_POINT('Ctrl Pts',(131.926755869651,-38.6041920950062,22.6496791013552));
#22350=CARTESIAN_POINT('Ctrl Pts',(131.816371628909,-38.6610683239017,22.643648740531));
#22351=CARTESIAN_POINT('Ctrl Pts',(131.703573152674,-38.7128241964153,22.6376183797068));
#22352=CARTESIAN_POINT('Ctrl Pts',(131.595010942745,-38.7626363222924,22.6318144954736));
#22353=CARTESIAN_POINT('Ctrl Pts',(131.484212969969,-38.8077055712292,22.6260106112404));
#22354=CARTESIAN_POINT('Ctrl Pts',(131.371632631363,-38.8478369150188,22.6202067270071));
#22355=CARTESIAN_POINT('Ctrl Pts',(131.259068922076,-38.8879623309797,22.6144037000697));
#22356=CARTESIAN_POINT('Ctrl Pts',(131.144723755054,-38.9231511552312,22.6086006731322));
#22357=CARTESIAN_POINT('Ctrl Pts',(131.029068717973,-38.9532572106668,22.6027976461948));
#22358=CARTESIAN_POINT('Ctrl Pts',(130.913403469762,-38.9833659241523,22.5969941069107));
#22359=CARTESIAN_POINT('Ctrl Pts',(130.796428516745,-39.0083908737169,22.5911905676267));
#22360=CARTESIAN_POINT('Ctrl Pts',(130.678628126105,-39.0282364461956,22.5853870283426));
#22361=CARTESIAN_POINT('Ctrl Pts',(130.560789534173,-39.0480884543621,22.5795816070385));
#22362=CARTESIAN_POINT('Ctrl Pts',(130.442125374718,-39.0627576772734,22.5737761857343));
#22363=CARTESIAN_POINT('Ctrl Pts',(130.32312692478,-39.0722001412605,22.5679707644302));
#22364=CARTESIAN_POINT('Ctrl Pts',(130.203996695073,-39.0816530619025,22.5621589141593));
#22365=CARTESIAN_POINT('Ctrl Pts',(130.084531843238,-39.0858676376548,22.5563470638883));
#22366=CARTESIAN_POINT('Ctrl Pts',(129.965225710083,-39.0848519861509,22.5505352136174));
#22367=CARTESIAN_POINT('Ctrl Pts',(129.845841216019,-39.0838356675615,22.5447195460921));
#22368=CARTESIAN_POINT('Ctrl Pts',(129.726616055086,-39.0775823016849,22.5389038785667));
#22369=CARTESIAN_POINT('Ctrl Pts',(129.608038844918,-39.0661519220151,22.5330882110413));
#22370=CARTESIAN_POINT('Ctrl Pts',(129.489291785701,-39.0547051695606,22.5272642132002));
#22371=CARTESIAN_POINT('Ctrl Pts',(129.371194932633,-39.0380666591171,22.5214402153591));
#22372=CARTESIAN_POINT('Ctrl Pts',(129.254227251238,-39.016347595416,22.515616217518));
#22373=CARTESIAN_POINT('Ctrl Pts',(129.223195087791,-39.0105854094289,22.5140710791451));
#22374=CARTESIAN_POINT('Ctrl Pts',(129.192242321156,-39.0044658909861,22.5125259407721));
#22375=CARTESIAN_POINT('Ctrl Pts',(129.161377702765,-38.9979917011646,22.5109808023992));
#22376=CARTESIAN_POINT('Ctrl Pts',(129.045049612359,-38.9735906173953,22.5051572087276));
#22377=CARTESIAN_POINT('Ctrl Pts',(128.929599802197,-38.9440688376213,22.4993336150561));
#22378=CARTESIAN_POINT('Ctrl Pts',(128.815512999793,-38.9095032352386,22.4935100213846));
#22379=CARTESIAN_POINT('Ctrl Pts',(128.701570134837,-38.8749812424978,22.4876937750415));
#22380=CARTESIAN_POINT('Ctrl Pts',(128.588987244671,-38.8354282014207,22.4818775286984));
#22381=CARTESIAN_POINT('Ctrl Pts',(128.478239180689,-38.7909720400987,22.4760612823553));
#22382=CARTESIAN_POINT('Ctrl Pts',(128.36760197613,-38.7465603796394,22.4702508581068));
#22383=CARTESIAN_POINT('Ctrl Pts',(128.258796320694,-38.6972555141347,22.4644404338584));
#22384=CARTESIAN_POINT('Ctrl Pts',(128.152281620109,-38.6432350718299,22.45863000961));
#22385=CARTESIAN_POINT('Ctrl Pts',(128.041735117798,-38.5871698440516,22.4525996487858));
#22386=CARTESIAN_POINT('Ctrl Pts',(127.933656860859,-38.5260251272367,22.4465692879617));
#22387=CARTESIAN_POINT('Ctrl Pts',(127.82853772629,-38.4600544206492,22.4405389271376));
#22388=CARTESIAN_POINT('Ctrl Pts',(127.727366452209,-38.3965613138534,22.4347350429043));
#22389=CARTESIAN_POINT('Ctrl Pts',(127.62893641979,-38.3285984071376,22.4289311586709));
#22390=CARTESIAN_POINT('Ctrl Pts',(127.533659280727,-38.2564380013221,22.4231272744376));
#22391=CARTESIAN_POINT('Ctrl Pts',(127.438396215116,-38.1842882543705,22.4173242475001));
#22392=CARTESIAN_POINT('Ctrl Pts',(127.346285442124,-38.1079424878032,22.4115212205626));
#22393=CARTESIAN_POINT('Ctrl Pts',(127.257707727253,-38.027714994981,22.405718193625));
#22394=CARTESIAN_POINT('Ctrl Pts',(127.169122191896,-37.9474804189099,22.3999146543409));
#22395=CARTESIAN_POINT('Ctrl Pts',(127.084070637522,-37.8633637093151,22.3941111150568));
#22396=CARTESIAN_POINT('Ctrl Pts',(127.002898489856,-37.7757174816415,22.3883075757726));
#22397=CARTESIAN_POINT('Ctrl Pts',(126.921700019007,-37.6880428313175,22.3825021544683));
#22398=CARTESIAN_POINT('Ctrl Pts',(126.844383734154,-37.5968366860366,22.3766967331641));
#22399=CARTESIAN_POINT('Ctrl Pts',(126.771255713783,-37.5024858309735,22.3708913118598));
#22400=CARTESIAN_POINT('Ctrl Pts',(126.698046710899,-37.4080304910724,22.3650794615888));
#22401=CARTESIAN_POINT('Ctrl Pts',(126.629035480868,-37.3104238130077,22.3592676113178));
#22402=CARTESIAN_POINT('Ctrl Pts',(126.564485665799,-37.210082862587,22.3534557610468));
#22403=CARTESIAN_POINT('Ctrl Pts',(126.499893454065,-37.1096760076916,22.3476400935213));
#22404=CARTESIAN_POINT('Ctrl Pts',(126.439768698188,-37.0065316558561,22.3418244259959));
#22405=CARTESIAN_POINT('Ctrl Pts',(126.384329030278,-36.9010913809467,22.3360087584704));
#22406=CARTESIAN_POINT('Ctrl Pts',(126.32880995103,-36.795500074229,22.3301847606292));
#22407=CARTESIAN_POINT('Ctrl Pts',(126.277989527687,-36.6876066485449,22.324360762788));
#22408=CARTESIAN_POINT('Ctrl Pts',(126.232037303275,-36.5778726552195,22.3185367649468));
#22409=CARTESIAN_POINT('Ctrl Pts',(126.219845927668,-36.5487596286653,22.3169916265748));
#22410=CARTESIAN_POINT('Ctrl Pts',(126.207996937055,-36.5195171306766,22.3154464882028));
#22411=CARTESIAN_POINT('Ctrl Pts',(126.196492903007,-36.4901539394042,22.3139013498308));
#22412=CARTESIAN_POINT('Ctrl Pts',(126.147593400051,-36.3653415951119,22.307333523443));
#22413=CARTESIAN_POINT('Ctrl Pts',(126.104798671117,-36.2380114730377,22.3007656970552));
#22414=CARTESIAN_POINT('Ctrl Pts',(126.068343047717,-36.1087373943196,22.2941978706675));
#22415=CARTESIAN_POINT('Ctrl Pts',(126.03200196934,-35.9798694999168,22.2876506806524));
#22416=CARTESIAN_POINT('Ctrl Pts',(126.001960341602,-35.8490700312458,22.2811034906373));
#22417=CARTESIAN_POINT('Ctrl Pts',(125.978403669589,-35.7169295329545,22.2745563006222));
#22418=CARTESIAN_POINT('Ctrl Pts',(125.954985042458,-35.5855633935992,22.2680474779143));
#22419=CARTESIAN_POINT('Ctrl Pts',(125.937975683309,-35.4528720958563,22.2615386552065));
#22420=CARTESIAN_POINT('Ctrl Pts',(125.927510148756,-35.319454866162,22.2550298324986));
#22421=CARTESIAN_POINT('Ctrl Pts',(125.919248328881,-35.2141311376499,22.2498915645449));
#22422=CARTESIAN_POINT('Ctrl Pts',(125.915063725241,-35.1083554127925,22.2447532965911));
#22423=CARTESIAN_POINT('Ctrl Pts',(125.915000722565,-35.0024296824293,22.2396150286373));
#22424=CARTESIAN_POINT('Origin',(130.,-35.,32.7603849714045));
#22425=CARTESIAN_POINT('',(132.487160670875,-31.7594357285724,24.2969444293292));
#22426=CARTESIAN_POINT('',(132.487160670875,-31.7594357285724,24.1926561452238));
#22427=CARTESIAN_POINT('',(132.487160670875,-31.7594357285724,32.7603849714045));
#22428=CARTESIAN_POINT('',(125.915000507333,-34.997964094252,23.3853849713659));
#22429=CARTESIAN_POINT('Ctrl Pts',(132.487160670875,-31.7594357285724,24.1926561452238));
#22430=CARTESIAN_POINT('Ctrl Pts',(132.581972317179,-31.8322044744069,24.186852936304));
#22431=CARTESIAN_POINT('Ctrl Pts',(132.673586441412,-31.9091366288103,24.1810497273843));
#22432=CARTESIAN_POINT('Ctrl Pts',(132.761628074101,-31.989911067703,24.1752465184646));
#22433=CARTESIAN_POINT('Ctrl Pts',(132.84969112169,-32.0707051538523,24.1694418979952));
#22434=CARTESIAN_POINT('Ctrl Pts',(132.93417964885,-32.1553431070645,24.1636372775258));
#22435=CARTESIAN_POINT('Ctrl Pts',(133.014754835976,-32.2434662565174,24.1578326570563));
#22436=CARTESIAN_POINT('Ctrl Pts',(133.095416138222,-32.3316835880113,24.1520218328708));
#22437=CARTESIAN_POINT('Ctrl Pts',(133.172155473104,-32.4233932517347,24.1462110086852));
#22438=CARTESIAN_POINT('Ctrl Pts',(133.244673563067,-32.5182025729052,24.1404001844997));
#22439=CARTESIAN_POINT('Ctrl Pts',(133.317234011662,-32.613067273267,24.1345859661463));
#22440=CARTESIAN_POINT('Ctrl Pts',(133.385568070478,-32.711034903007,24.128771747793));
#22441=CARTESIAN_POINT('Ctrl Pts',(133.449420121027,-32.81168424841,24.1229575294397));
#22442=CARTESIAN_POINT('Ctrl Pts',(133.513369618591,-32.9124871985645,24.117134437789));
#22443=CARTESIAN_POINT('Ctrl Pts',(133.572823243656,-33.0159796845002,24.1113113461384));
#22444=CARTESIAN_POINT('Ctrl Pts',(133.627571421346,-33.1217160536719,24.1054882544877));
#22445=CARTESIAN_POINT('Ctrl Pts',(133.660879131881,-33.1860439733586,24.1019456004798));
#22446=CARTESIAN_POINT('Ctrl Pts',(133.692446162948,-33.2512019997072,24.0984029464718));
#22447=CARTESIAN_POINT('Ctrl Pts',(133.722234217902,-33.3170866252006,24.0948602924639));
#22448=CARTESIAN_POINT('Ctrl Pts',(133.771201327851,-33.425391101791,24.0890366987924));
#22449=CARTESIAN_POINT('Ctrl Pts',(133.81551653434,-33.5360091682225,24.083213105121));
#22450=CARTESIAN_POINT('Ctrl Pts',(133.854955774648,-33.6485041711093,24.0773895114495));
#22451=CARTESIAN_POINT('Ctrl Pts',(133.894345256496,-33.7608572448401,24.0715732651064));
#22452=CARTESIAN_POINT('Ctrl Pts',(133.928870873956,-33.875082163117,24.0657570187634));
#22453=CARTESIAN_POINT('Ctrl Pts',(133.958355605774,-33.9907201090709,24.0599407724204));
#22454=CARTESIAN_POINT('Ctrl Pts',(133.987810823214,-34.1062423008031,24.054130348172));
#22455=CARTESIAN_POINT('Ctrl Pts',(134.012235093006,-34.223174312939,24.0483199239236));
#22456=CARTESIAN_POINT('Ctrl Pts',(134.03150062945,-34.341040460466,24.0425094996753));
#22457=CARTESIAN_POINT('Ctrl Pts',(134.051495406297,-34.4633680854653,24.0364791388511));
#22458=CARTESIAN_POINT('Ctrl Pts',(134.065933047646,-34.5867015380635,24.030448778027));
#22459=CARTESIAN_POINT('Ctrl Pts',(134.074728435545,-34.7104949455294,24.0244184172028));
#22460=CARTESIAN_POINT('Ctrl Pts',(134.08319350333,-34.8296391603986,24.0186145329696));
#22461=CARTESIAN_POINT('Ctrl Pts',(134.086432445026,-34.9492089610494,24.0128106487363));
#22462=CARTESIAN_POINT('Ctrl Pts',(134.084422083151,-35.0687113285592,24.007006764503));
#22463=CARTESIAN_POINT('Ctrl Pts',(134.082412018227,-35.1881960442914,24.0012037375656));
#22464=CARTESIAN_POINT('Ctrl Pts',(134.075154198583,-35.3076129385223,23.9954007106281));
#22465=CARTESIAN_POINT('Ctrl Pts',(134.062677574554,-35.4264691374727,23.9895976836906));
#22466=CARTESIAN_POINT('Ctrl Pts',(134.050199848969,-35.5453358301824,23.9837941444065));
#22467=CARTESIAN_POINT('Ctrl Pts',(134.032502445518,-35.6636413230609,23.9779906051225));
#22468=CARTESIAN_POINT('Ctrl Pts',(134.009666108294,-35.7808986489905,23.9721870658384));
#22469=CARTESIAN_POINT('Ctrl Pts',(133.986822365513,-35.898194000104,23.9663816445342));
#22470=CARTESIAN_POINT('Ctrl Pts',(133.958836452693,-36.0144401076672,23.96057622323));
#22471=CARTESIAN_POINT('Ctrl Pts',(133.925839921304,-36.1291615970682,23.9547708019258));
#22472=CARTESIAN_POINT('Ctrl Pts',(133.892806849311,-36.2440101298999,23.9489589516549));
#22473=CARTESIAN_POINT('Ctrl Pts',(133.854752195815,-36.3573302817714,23.9431471013839));
#22474=CARTESIAN_POINT('Ctrl Pts',(133.811857003735,-36.4686630597519,23.937335251113));
#22475=CARTESIAN_POINT('Ctrl Pts',(133.768933637861,-36.5800689616986,23.9315195835876));
#22476=CARTESIAN_POINT('Ctrl Pts',(133.721163564773,-36.6894845168158,23.9257039160622));
#22477=CARTESIAN_POINT('Ctrl Pts',(133.668774768512,-36.7964734058513,23.9198882485368));
#22478=CARTESIAN_POINT('Ctrl Pts',(133.616310930957,-36.9036155449176,23.9140642506957));
#22479=CARTESIAN_POINT('Ctrl Pts',(133.559215360202,-37.0083237228902,23.9082402528545));
#22480=CARTESIAN_POINT('Ctrl Pts',(133.497760551461,-37.1101886466956,23.9024162550134));
#22481=CARTESIAN_POINT('Ctrl Pts',(133.481456255725,-37.1372139662253,23.9008711166408));
#22482=CARTESIAN_POINT('Ctrl Pts',(133.464845352462,-37.1640393303555,23.8993259782681));
#22483=CARTESIAN_POINT('Ctrl Pts',(133.447933409605,-37.1906574818822,23.8977808398955));
#22484=CARTESIAN_POINT('Ctrl Pts',(133.384192656586,-37.2909807289924,23.891957246224));
#22485=CARTESIAN_POINT('Ctrl Pts',(133.315966879741,-37.3886814839588,23.8861336525526));
#22486=CARTESIAN_POINT('Ctrl Pts',(133.243498460342,-37.4833329897058,23.8803100588811));
#22487=CARTESIAN_POINT('Ctrl Pts',(133.171121470617,-37.577865078519,23.8744938125381));
#22488=CARTESIAN_POINT('Ctrl Pts',(133.094512730825,-37.6693552485036,23.8686775661951));
#22489=CARTESIAN_POINT('Ctrl Pts',(133.013958945554,-37.7574039374957,23.8628613198521));
#22490=CARTESIAN_POINT('Ctrl Pts',(132.933485795066,-37.8453644892642,23.8570508956037));
#22491=CARTESIAN_POINT('Ctrl Pts',(132.849075729214,-37.9298901137807,23.8512404713554));
#22492=CARTESIAN_POINT('Ctrl Pts',(132.761056549752,-38.0106131815746,23.845430047107));
#22493=CARTESIAN_POINT('Ctrl Pts',(132.669705662293,-38.0943917844485,23.8393996862829));
#22494=CARTESIAN_POINT('Ctrl Pts',(132.574467310381,-38.1740739175952,23.8333693254587));
#22495=CARTESIAN_POINT('Ctrl Pts',(132.475751387658,-38.249289163265,23.8273389646345));
#22496=CARTESIAN_POINT('Ctrl Pts',(132.380742846018,-38.3216796206806,23.8215350804013));
#22497=CARTESIAN_POINT('Ctrl Pts',(132.28251358474,-38.3899323876553,23.815731196168));
#22498=CARTESIAN_POINT('Ctrl Pts',(132.181463245574,-38.4537578241979,23.8099273119348));
#22499=CARTESIAN_POINT('Ctrl Pts',(132.080427832625,-38.517573833041,23.8041242849973));
#22500=CARTESIAN_POINT('Ctrl Pts',(131.976572515624,-38.5769635939797,23.7983212580599));
#22501=CARTESIAN_POINT('Ctrl Pts',(131.870325389499,-38.6316811447861,23.7925182311224));
#22502=CARTESIAN_POINT('Ctrl Pts',(131.764068882864,-38.68640352658,23.7867146918383));
#22503=CARTESIAN_POINT('Ctrl Pts',(131.655420510286,-38.7364526911104,23.7809111525543));
#22504=CARTESIAN_POINT('Ctrl Pts',(131.544831817982,-38.7816292327712,23.7751076132702));
#22505=CARTESIAN_POINT('Ctrl Pts',(131.434207263055,-38.8268204246576,23.7693021919661));
#22506=CARTESIAN_POINT('Ctrl Pts',(131.321641514837,-38.8671356968009,23.7634967706619));
#22507=CARTESIAN_POINT('Ctrl Pts',(131.207604274662,-38.9024244920072,23.7576913493577));
#22508=CARTESIAN_POINT('Ctrl Pts',(131.093440748798,-38.9377523662879,23.7518794990868));
#22509=CARTESIAN_POINT('Ctrl Pts',(130.977802868591,-38.9680425319206,23.7460676488159));
#22510=CARTESIAN_POINT('Ctrl Pts',(130.861173763618,-38.9931948047717,23.7402557985449));
#22511=CARTESIAN_POINT('Ctrl Pts',(130.744468056023,-39.0183635977706,23.7344401310196));
#22512=CARTESIAN_POINT('Ctrl Pts',(130.626770228723,-39.0383877090663,23.7286244634942));
#22513=CARTESIAN_POINT('Ctrl Pts',(130.508570179099,-39.0532186436129,23.7228087959689));
#22514=CARTESIAN_POINT('Ctrl Pts',(130.390200820667,-39.0680708218719,23.7169847981277));
#22515=CARTESIAN_POINT('Ctrl Pts',(130.271328209625,-39.0777149433084,23.7111608002866));
#22516=CARTESIAN_POINT('Ctrl Pts',(130.152444038842,-39.0821545555039,23.7053368024455));
#22517=CARTESIAN_POINT('Ctrl Pts',(130.120903420318,-39.0833324088189,23.7037916640727));
#22518=CARTESIAN_POINT('Ctrl Pts',(130.089361967641,-39.0841442161781,23.7022465256999));
#22519=CARTESIAN_POINT('Ctrl Pts',(130.057828802667,-39.084590656306,23.7007013873271));
#22520=CARTESIAN_POINT('Ctrl Pts',(129.938980974395,-39.0862732796548,23.6948777936556));
#22521=CARTESIAN_POINT('Ctrl Pts',(129.81986799618,-39.0827672038154,23.6890541999842));
#22522=CARTESIAN_POINT('Ctrl Pts',(129.70097965991,-39.0740412168033,23.6832306063127));
#22523=CARTESIAN_POINT('Ctrl Pts',(129.582241318934,-39.06532623892,23.6774143599697));
#22524=CARTESIAN_POINT('Ctrl Pts',(129.463727459842,-39.05140447828,23.6715981136266));
#22525=CARTESIAN_POINT('Ctrl Pts',(129.345929425908,-39.0322967009022,23.6657818672836));
#22526=CARTESIAN_POINT('Ctrl Pts',(129.228249308457,-39.0132080505151,23.6599714430352));
#22527=CARTESIAN_POINT('Ctrl Pts',(129.111283991439,-38.9889437757074,23.6541610187869));
#22528=CARTESIAN_POINT('Ctrl Pts',(128.995520638518,-38.9595765193207,23.6483505945385));
#22529=CARTESIAN_POINT('Ctrl Pts',(128.875375403249,-38.929097651538,23.6423202337143));
#22530=CARTESIAN_POINT('Ctrl Pts',(128.75652537064,-38.8931218851609,23.6362898728902));
#22531=CARTESIAN_POINT('Ctrl Pts',(128.639505036172,-38.8517889938831,23.630259512066));
#22532=CARTESIAN_POINT('Ctrl Pts',(128.526879524368,-38.8120084031364,23.6244556278328));
#22533=CARTESIAN_POINT('Ctrl Pts',(128.415949176261,-38.7672659642247,23.6186517435995));
#22534=CARTESIAN_POINT('Ctrl Pts',(128.307175307434,-38.7177371558837,23.6128478593663));
#22535=CARTESIAN_POINT('Ctrl Pts',(128.19841750567,-38.6682156634772,23.6070448324288));
#22536=CARTESIAN_POINT('Ctrl Pts',(128.091815921246,-38.6139093768061,23.6012418054913));
#22537=CARTESIAN_POINT('Ctrl Pts',(127.987810935918,-38.5550415145804,23.5954387785538));
#22538=CARTESIAN_POINT('Ctrl Pts',(127.883796768038,-38.4961684549381,23.5896352392697));
#22539=CARTESIAN_POINT('Ctrl Pts',(127.782380010442,-38.4327332201464,23.5838316999857));
#22540=CARTESIAN_POINT('Ctrl Pts',(127.683974961418,-38.3650041635426,23.5780281607016));
#22541=CARTESIAN_POINT('Ctrl Pts',(127.585538000782,-38.2972531431953,23.5722227393974));
#22542=CARTESIAN_POINT('Ctrl Pts',(127.490115027271,-38.2252057631852,23.5664173180931));
#22543=CARTESIAN_POINT('Ctrl Pts',(127.398089435739,-38.1491723381845,23.5606118967889));
#22544=CARTESIAN_POINT('Ctrl Pts',(127.305961934383,-38.0730547132036,23.554800046518));
#22545=CARTESIAN_POINT('Ctrl Pts',(127.217239639829,-37.9929424924006,23.548988196247));
#22546=CARTESIAN_POINT('Ctrl Pts',(127.132271177233,-37.90918483412,23.5431763459761));
#22547=CARTESIAN_POINT('Ctrl Pts',(127.047246906896,-37.8253721633599,23.5373606784507));
#22548=CARTESIAN_POINT('Ctrl Pts',(126.965981656001,-37.7379095851817,23.5315450109253));
#22549=CARTESIAN_POINT('Ctrl Pts',(126.888784528308,-37.6471802524019,23.5257293433999));
#22550=CARTESIAN_POINT('Ctrl Pts',(126.811476824066,-37.5563209596498,23.5199053455588));
#22551=CARTESIAN_POINT('Ctrl Pts',(126.738249123523,-37.4621858938798,23.5140813477176));
#22552=CARTESIAN_POINT('Ctrl Pts',(126.669367987707,-37.3651882374751,23.5082573498765));
#22553=CARTESIAN_POINT('Ctrl Pts',(126.651093446919,-37.3394542305172,23.5067122115038));
#22554=CARTESIAN_POINT('Ctrl Pts',(126.633124599154,-37.3135188728382,23.5051670731312));
#22555=CARTESIAN_POINT('Ctrl Pts',(126.615465877015,-37.287390165746,23.5036219347586));
#22556=CARTESIAN_POINT('Ctrl Pts',(126.547946051236,-37.1874845362868,23.4977139492936));
#22557=CARTESIAN_POINT('Ctrl Pts',(126.484750138235,-37.0844341712422,23.4918059638286));
#22558=CARTESIAN_POINT('Ctrl Pts',(126.426178854133,-36.9786428220761,23.4858979783636));
#22559=CARTESIAN_POINT('Ctrl Pts',(126.367686936567,-36.8729948246073,23.4799979984658));
#22560=CARTESIAN_POINT('Ctrl Pts',(126.313807367995,-36.7646135732641,23.4740980185679));
#22561=CARTESIAN_POINT('Ctrl Pts',(126.264798248164,-36.6539325479227,23.46819803867));
#22562=CARTESIAN_POINT('Ctrl Pts',(126.215845205528,-36.5433781659803,23.4623048096448));
#22563=CARTESIAN_POINT('Ctrl Pts',(126.171751679283,-36.4305296035708,23.4564115806196));
#22564=CARTESIAN_POINT('Ctrl Pts',(126.132730166999,-36.3158453703833,23.4505183515944));
#22565=CARTESIAN_POINT('Ctrl Pts',(126.093751609521,-36.2012873813831,23.4446316098245));
#22566=CARTESIAN_POINT('Ctrl Pts',(126.059834070597,-36.0848981168303,23.4387448680547));
#22567=CARTESIAN_POINT('Ctrl Pts',(126.031141913439,-35.9671558761317,23.4328581262849));
#22568=CARTESIAN_POINT('Ctrl Pts',(126.002468405445,-35.849490164864,23.4269752107459));
#22569=CARTESIAN_POINT('Ctrl Pts',(125.979013612725,-35.7304736079775,23.4210922952069));
#22570=CARTESIAN_POINT('Ctrl Pts',(125.960892007609,-35.6105993987934,23.415209379668));
#22571=CARTESIAN_POINT('Ctrl Pts',(125.942777952188,-35.4907751307492,23.4093289150274));
#22572=CARTESIAN_POINT('Ctrl Pts',(125.929992721259,-35.3700943092338,23.4034484503869));
#22573=CARTESIAN_POINT('Ctrl Pts',(125.922599567219,-35.2490596530117,23.3975679857463));
#22574=CARTESIAN_POINT('Ctrl Pts',(125.917493910484,-35.1654740271159,23.3935069809657));
#22575=CARTESIAN_POINT('Ctrl Pts',(125.914958764663,-35.0817198648688,23.3894459761851));
#22576=CARTESIAN_POINT('Ctrl Pts',(125.915000507333,-34.9979640950484,23.3853849714045));
#22577=CARTESIAN_POINT('Ctrl Pts',(125.915000507333,-34.997964094252,23.3853849713659));
#22578=CARTESIAN_POINT('Ctrl Pts',(125.915068041878,-34.8624575358967,23.3788147639346));
#22579=CARTESIAN_POINT('Ctrl Pts',(125.921882638121,-34.7271788853975,23.3722445565033));
#22580=CARTESIAN_POINT('Ctrl Pts',(125.935349060719,-34.5927681964749,23.365674349072));
#22581=CARTESIAN_POINT('Ctrl Pts',(125.948524496332,-34.461261898893,23.359246112891));
#22582=CARTESIAN_POINT('Ctrl Pts',(125.968067066152,-34.3305866411253,23.3528178767101));
#22583=CARTESIAN_POINT('Ctrl Pts',(125.993836675524,-34.2013258376368,23.3463896405291));
#22584=CARTESIAN_POINT('Ctrl Pts',(126.020459989605,-34.0677828366577,23.3397484474726));
#22585=CARTESIAN_POINT('Ctrl Pts',(126.053729887508,-33.9357499211089,23.3331072544161));
#22586=CARTESIAN_POINT('Ctrl Pts',(126.093437848864,-33.8058487703357,23.3264660613596));
#22587=CARTESIAN_POINT('Ctrl Pts',(126.133145810219,-33.6759476195625,23.3198248683031));
#22588=CARTESIAN_POINT('Ctrl Pts',(126.179291657194,-33.5481784751308,23.3131836752467));
#22589=CARTESIAN_POINT('Ctrl Pts',(126.231614536202,-33.4231372931558,23.3065424821902));
#22590=CARTESIAN_POINT('Ctrl Pts',(126.277495928968,-33.3134899707806,23.3007188885187));
#22591=CARTESIAN_POINT('Ctrl Pts',(126.328240832554,-33.2056699869784,23.2948952948472));
#22592=CARTESIAN_POINT('Ctrl Pts',(126.38368242305,-33.1001389043826,23.2890717011758));
#22593=CARTESIAN_POINT('Ctrl Pts',(126.439054065743,-32.9947409649228,23.2832554548327));
#22594=CARTESIAN_POINT('Ctrl Pts',(126.499110421294,-32.8916265412262,23.2774392084897));
#22595=CARTESIAN_POINT('Ctrl Pts',(126.563636386211,-32.791237877492,23.2716229621467));
#22596=CARTESIAN_POINT('Ctrl Pts',(126.628097760281,-32.6909497033638,23.2658125378984));
#22597=CARTESIAN_POINT('Ctrl Pts',(126.697019623524,-32.5933822027085,23.26000211365));
#22598=CARTESIAN_POINT('Ctrl Pts',(126.770140972508,-32.4989530867004,23.2541916894017));
#22599=CARTESIAN_POINT('Ctrl Pts',(126.846030115791,-32.4009496333386,23.2481613285775));
#22600=CARTESIAN_POINT('Ctrl Pts',(126.926442736365,-32.3063272444975,23.2421309677533));
#22601=CARTESIAN_POINT('Ctrl Pts',(127.0110373891,-32.2155202441672,23.2361006069292));
#22602=CARTESIAN_POINT('Ctrl Pts',(127.09245500001,-32.1281235969596,23.2302967226959));
#22603=CARTESIAN_POINT('Ctrl Pts',(127.177745883189,-32.0442612501205,23.2244928384627));
#22604=CARTESIAN_POINT('Ctrl Pts',(127.26656505548,-31.9642861788243,23.2186889542295));
#22605=CARTESIAN_POINT('Ctrl Pts',(127.355371108229,-31.8843229207015,23.212885927292));
#22606=CARTESIAN_POINT('Ctrl Pts',(127.447704110287,-31.8082460693953,23.2070829003545));
#22607=CARTESIAN_POINT('Ctrl Pts',(127.54318365727,-31.7363703552494,23.2012798734171));
#22608=CARTESIAN_POINT('Ctrl Pts',(127.638671634099,-31.6644882952296,23.195476334133));
#22609=CARTESIAN_POINT('Ctrl Pts',(127.737306381951,-31.5968083554373,23.1896727948489));
#22610=CARTESIAN_POINT('Ctrl Pts',(127.838676519037,-31.5336033391087,23.1838692555648));
#22611=CARTESIAN_POINT('Ctrl Pts',(127.940079529277,-31.4703778261305,23.1780638342607));
#22612=CARTESIAN_POINT('Ctrl Pts',(128.044219346579,-31.4116303385915,23.1722584129565));
#22613=CARTESIAN_POINT('Ctrl Pts',(128.150658444779,-31.3575885992749,23.1664529916523));
#22614=CARTESIAN_POINT('Ctrl Pts',(128.257215414428,-31.3034870137343,23.1606411413814));
#22615=CARTESIAN_POINT('Ctrl Pts',(128.366076383178,-31.2541017633487,23.1548292911105));
#22616=CARTESIAN_POINT('Ctrl Pts',(128.476782081958,-31.2096131893757,23.1490174408395));
#22617=CARTESIAN_POINT('Ctrl Pts',(128.587560492835,-31.1650953950685,23.1432017733142));
#22618=CARTESIAN_POINT('Ctrl Pts',(128.700185662413,-31.1254808174235,23.1373861057888));
#22619=CARTESIAN_POINT('Ctrl Pts',(128.814182921209,-31.0908999941613,23.1315704382634));
#22620=CARTESIAN_POINT('Ctrl Pts',(128.92834346877,-31.0562696376038,23.1257464404223));
#22621=CARTESIAN_POINT('Ctrl Pts',(129.043879634147,-31.0266875277395,23.1199224425811));
#22622=CARTESIAN_POINT('Ctrl Pts',(129.160306188627,-31.0022332105109,23.11409844474));
#22623=CARTESIAN_POINT('Ctrl Pts',(129.19119478815,-30.9957453468543,23.1125533063673));
#22624=CARTESIAN_POINT('Ctrl Pts',(129.222146031755,-30.9896181299174,23.1110081679945));
#22625=CARTESIAN_POINT('Ctrl Pts',(129.253150813995,-30.9838524313263,23.1094630296218));
#22626=CARTESIAN_POINT('Ctrl Pts',(129.370019603658,-30.962119325424,23.1036388167605));
#22627=CARTESIAN_POINT('Ctrl Pts',(129.488026301746,-30.9454566790275,23.0978146038993));
#22628=CARTESIAN_POINT('Ctrl Pts',(129.606693270705,-30.9339780107959,23.0919903910381));
#22629=CARTESIAN_POINT('Ctrl Pts',(129.725207575952,-30.922514109741,23.0861736709608));
#22630=CARTESIAN_POINT('Ctrl Pts',(129.844380059347,-30.9162209598086,23.0803569508835));
#22631=CARTESIAN_POINT('Ctrl Pts',(129.963722808182,-30.9151610845281,23.0745402308062));
#22632=CARTESIAN_POINT('Ctrl Pts',(130.082924450892,-30.9141024624019,23.0687303881876));
#22633=CARTESIAN_POINT('Ctrl Pts',(130.202295552223,-30.9182647994427,23.062920545569));
#22634=CARTESIAN_POINT('Ctrl Pts',(130.321343825436,-30.9276587635791,23.0571107029504));
#22635=CARTESIAN_POINT('Ctrl Pts',(130.440313011485,-30.9370464870371,23.0513047199759));
#22636=CARTESIAN_POINT('Ctrl Pts',(130.558959390375,-30.9516588939429,23.0454987370015));
#22637=CARTESIAN_POINT('Ctrl Pts',(130.676791649195,-30.9714545970562,23.0396927540271));
#22638=CARTESIAN_POINT('Ctrl Pts',(130.794573438416,-30.9912418213266,23.0338892578558));
#22639=CARTESIAN_POINT('Ctrl Pts',(130.911541399294,-31.0162078577871,23.0280857616846));
#22640=CARTESIAN_POINT('Ctrl Pts',(131.027210946426,-31.0462596605818,23.0222822655134));
#22641=CARTESIAN_POINT('Ctrl Pts',(131.142858248281,-31.0763056838893,23.016479885456));
#22642=CARTESIAN_POINT('Ctrl Pts',(131.257207238655,-31.1114354235755,23.0106775053986));
#22643=CARTESIAN_POINT('Ctrl Pts',(131.369785731835,-31.1515052229657,23.0048751253412));
#22644=CARTESIAN_POINT('Ctrl Pts',(131.482409236857,-31.1915910433152,22.9990704253397));
#22645=CARTESIAN_POINT('Ctrl Pts',(131.593260444397,-31.2366207354387,22.9932657253382));
#22646=CARTESIAN_POINT('Ctrl Pts',(131.701884602897,-31.2864015027977,22.9874610253367));
#22647=CARTESIAN_POINT('Ctrl Pts',(131.810531700828,-31.3361927829424,22.9816550994889));
#22648=CARTESIAN_POINT('Ctrl Pts',(131.916950446232,-31.3907369569506,22.9758491736412));
#22649=CARTESIAN_POINT('Ctrl Pts',(132.020709414005,-31.4497945884568,22.9700432477934));
#22650=CARTESIAN_POINT('Ctrl Pts',(132.124565043882,-31.5089072381948,22.9642319131312));
#22651=CARTESIAN_POINT('Ctrl Pts',(132.225755598332,-31.5725415309082,22.958420578469));
#22652=CARTESIAN_POINT('Ctrl Pts',(132.323877385357,-31.6404138799805,22.9526092438067));
#22653=CARTESIAN_POINT('Ctrl Pts',(132.379306579903,-31.678755106278,22.9493264091853));
#22654=CARTESIAN_POINT('Ctrl Pts',(132.433757040346,-31.7184479874236,22.9460435745638));
#22655=CARTESIAN_POINT('Ctrl Pts',(132.487160670875,-31.7594357285724,22.9427607399423));
#22656=CARTESIAN_POINT('',(125.915000083441,-35.0008256610612,23.4896150285496));
#22657=CARTESIAN_POINT('Ctrl Pts',(125.915000083441,-35.0008256610612,23.4896150285496));
#22658=CARTESIAN_POINT('Ctrl Pts',(125.914976188112,-34.8826023086113,23.4838237303786));
#22659=CARTESIAN_POINT('Ctrl Pts',(125.920088782344,-34.7641789032467,23.4780324322077));
#22660=CARTESIAN_POINT('Ctrl Pts',(125.930363891994,-34.6460410356922,23.4722411340368));
#22661=CARTESIAN_POINT('Ctrl Pts',(125.940626165892,-34.5280507469398,23.4664570704035));
#22662=CARTESIAN_POINT('Ctrl Pts',(125.956038095578,-34.4103456948175,23.4606730067702));
#22663=CARTESIAN_POINT('Ctrl Pts',(125.976573711133,-34.2934124979475,23.454888943137));
#22664=CARTESIAN_POINT('Ctrl Pts',(125.997089184842,-34.1765939920917,23.4491105526584));
#22665=CARTESIAN_POINT('Ctrl Pts',(126.022718277938,-34.0605462405633,23.4433321621799));
#22666=CARTESIAN_POINT('Ctrl Pts',(126.053383190379,-33.9457510929488,23.4375537717014));
#22667=CARTESIAN_POINT('Ctrl Pts',(126.0840271413,-33.8310344155049,23.4317793311397));
#22668=CARTESIAN_POINT('Ctrl Pts',(126.119699958342,-33.7175690369885,23.4260048905781));
#22669=CARTESIAN_POINT('Ctrl Pts',(126.160272822346,-33.6058263375076,23.4202304500164));
#22670=CARTESIAN_POINT('Ctrl Pts',(126.200831076437,-33.4941238755415,23.4144580887775));
#22671=CARTESIAN_POINT('Ctrl Pts',(126.246285729108,-33.3841432475703,23.4086857275386));
#22672=CARTESIAN_POINT('Ctrl Pts',(126.296458370552,-33.276339824981,23.4029133662996));
#22673=CARTESIAN_POINT('Ctrl Pts',(126.346625133143,-33.1685490339875,23.3971416814227));
#22674=CARTESIAN_POINT('Ctrl Pts',(126.401508610812,-33.0629353158185,23.3913699965457));
#22675=CARTESIAN_POINT('Ctrl Pts',(126.46088288993,-32.9599325792491,23.3855983116687));
#22676=CARTESIAN_POINT('Ctrl Pts',(126.520264635338,-32.8569168901294,23.3798259010049));
#22677=CARTESIAN_POINT('Ctrl Pts',(126.584138098127,-32.7565131933276,23.374053490341));
#22678=CARTESIAN_POINT('Ctrl Pts',(126.652232561365,-32.6591287568908,23.3682810796771));
#22679=CARTESIAN_POINT('Ctrl Pts',(126.720394941295,-32.5616471902553,23.3625029116723));
#22680=CARTESIAN_POINT('Ctrl Pts',(126.792786493865,-32.4671912387105,23.3567247436676));
#22681=CARTESIAN_POINT('Ctrl Pts',(126.869094375303,-32.3761373951285,23.3509465756629));
#22682=CARTESIAN_POINT('Ctrl Pts',(126.945439758011,-32.2850388034211,23.3451655679956));
#22683=CARTESIAN_POINT('Ctrl Pts',(127.025705024388,-32.1973459552064,23.3393845603283));
#22684=CARTESIAN_POINT('Ctrl Pts',(127.109539652373,-32.1133992346024,23.3336035526611));
#22685=CARTESIAN_POINT('Ctrl Pts',(127.193510877075,-32.0293157346422,23.3278131256562));
#22686=CARTESIAN_POINT('Ctrl Pts',(127.281062779314,-31.9489908384644,23.3220226986513));
#22687=CARTESIAN_POINT('Ctrl Pts',(127.37181044764,-31.872725679307,23.3162322716463));
#22688=CARTESIAN_POINT('Ctrl Pts',(127.460271975996,-31.7983818128054,23.3105877186552));
#22689=CARTESIAN_POINT('Ctrl Pts',(127.551769842018,-31.7278957223704,23.3049431656641));
#22690=CARTESIAN_POINT('Ctrl Pts',(127.645922334693,-31.6615058266181,23.299298612673));
#22691=CARTESIAN_POINT('Ctrl Pts',(127.743061268699,-31.5930100967773,23.2934750190015));
#22692=CARTESIAN_POINT('Ctrl Pts',(127.8433488203,-31.5286470550448,23.28765142533));
#22693=CARTESIAN_POINT('Ctrl Pts',(127.946398371878,-31.4687190209535,23.2818278316586));
#22694=CARTESIAN_POINT('Ctrl Pts',(128.04931791114,-31.4088665949787,23.2760115853155));
#22695=CARTESIAN_POINT('Ctrl Pts',(128.154992169571,-31.3534382509531,23.2701953389725));
#22696=CARTESIAN_POINT('Ctrl Pts',(128.263003899946,-31.3026942852399,23.2643790926294));
#22697=CARTESIAN_POINT('Ctrl Pts',(128.370907509983,-31.2520011145162,23.2585686683811));
#22698=CARTESIAN_POINT('Ctrl Pts',(128.481143569719,-31.2059831663763,23.2527582441327));
#22699=CARTESIAN_POINT('Ctrl Pts',(128.593268989437,-31.1648555615309,23.2469478198844));
#22700=CARTESIAN_POINT('Ctrl Pts',(128.709638588206,-31.1221711917759,23.2409174590602));
#22701=CARTESIAN_POINT('Ctrl Pts',(128.828043017953,-31.0847549248083,23.234887098236));
#22702=CARTESIAN_POINT('Ctrl Pts',(128.947962219258,-31.0527932017828,23.2288567374119));
#22703=CARTESIAN_POINT('Ctrl Pts',(129.063377727884,-31.0220318351343,23.2230528531786));
#22704=CARTESIAN_POINT('Ctrl Pts',(129.180195852158,-30.9963228131408,23.2172489689454));
#22705=CARTESIAN_POINT('Ctrl Pts',(129.297936769714,-30.9757817876413,23.2114450847121));
#22706=CARTESIAN_POINT('Ctrl Pts',(129.415660295676,-30.9552437962709,23.2056420577747));
#22707=CARTESIAN_POINT('Ctrl Pts',(129.534305941696,-30.9398723534553,23.1998390308372));
#22708=CARTESIAN_POINT('Ctrl Pts',(129.653384206572,-30.9297318894517,23.1940360038997));
#22709=CARTESIAN_POINT('Ctrl Pts',(129.772472984814,-30.9195905301512,23.1882324646156));
#22710=CARTESIAN_POINT('Ctrl Pts',(129.891994050969,-30.914681102563,23.1824289253315));
#22711=CARTESIAN_POINT('Ctrl Pts',(130.011453946277,-30.9150160579123,23.1766253860475));
#22712=CARTESIAN_POINT('Ctrl Pts',(130.130952581035,-30.9153511218836,23.1708199647433));
#22713=CARTESIAN_POINT('Ctrl Pts',(130.250389597369,-30.9209339499411,23.1650145434391));
#22714=CARTESIAN_POINT('Ctrl Pts',(130.369273348815,-30.9317249117279,23.1592091221349));
#22715=CARTESIAN_POINT('Ctrl Pts',(130.488288753011,-30.9425278235061,23.153397271864));
#22716=CARTESIAN_POINT('Ctrl Pts',(130.606749262431,-30.9585503445551,23.147585421593));
#22717=CARTESIAN_POINT('Ctrl Pts',(130.724169994246,-30.9797011529696,23.1417735713221));
#22718=CARTESIAN_POINT('Ctrl Pts',(130.841667848627,-31.0008658533486,23.1359579037967));
#22719=CARTESIAN_POINT('Ctrl Pts',(130.958124167937,-31.0271654593772,23.1301422362714));
#22720=CARTESIAN_POINT('Ctrl Pts',(131.073067492797,-31.0584582767776,23.124326568746));
#22721=CARTESIAN_POINT('Ctrl Pts',(131.188175461558,-31.08979591776,23.1185025709048));
#22722=CARTESIAN_POINT('Ctrl Pts',(131.30176572272,-31.1261409215911,23.1126785730637));
#22723=CARTESIAN_POINT('Ctrl Pts',(131.41338497273,-31.1673027880015,23.1068545752225));
#22724=CARTESIAN_POINT('Ctrl Pts',(131.442998168172,-31.1782232555251,23.1053094368499));
#22725=CARTESIAN_POINT('Ctrl Pts',(131.472472757079,-31.1894825129043,23.1037642984772));
#22726=CARTESIAN_POINT('Ctrl Pts',(131.501800563169,-31.2010764592501,23.1022191601045));
#22727=CARTESIAN_POINT('Ctrl Pts',(131.612327895284,-31.2447704182979,23.0963960166496));
#22728=CARTESIAN_POINT('Ctrl Pts',(131.721124991535,-31.2933624212854,23.0905728731948));
#22729=CARTESIAN_POINT('Ctrl Pts',(131.827727178127,-31.3466948714436,23.0847497297399));
#22730=CARTESIAN_POINT('Ctrl Pts',(131.934210987089,-31.3999680979665,23.078933052662));
#22731=CARTESIAN_POINT('Ctrl Pts',(132.038504368934,-31.4579711278646,23.0731163755841));
#22732=CARTESIAN_POINT('Ctrl Pts',(132.140160799607,-31.5204976287083,23.0672996985061));
#22733=CARTESIAN_POINT('Ctrl Pts',(132.241707615468,-31.5829567080364,23.0614892934757));
#22734=CARTESIAN_POINT('Ctrl Pts',(132.340622792912,-31.6499293386126,23.0556788884453));
#22735=CARTESIAN_POINT('Ctrl Pts',(132.43648352961,-31.7211628570575,23.0498684834149));
#22736=CARTESIAN_POINT('Ctrl Pts',(132.453472538016,-31.7337872837555,23.0488387289679));
#22737=CARTESIAN_POINT('Ctrl Pts',(132.470365674088,-31.7465454255331,23.0478089745209));
#22738=CARTESIAN_POINT('Ctrl Pts',(132.487160670875,-31.7594357285724,23.0467792200739));
#22739=CARTESIAN_POINT('Ctrl Pts',(132.487160670875,-31.7594357285724,24.2969444293292));
#22740=CARTESIAN_POINT('Ctrl Pts',(132.553405700193,-31.8102793526328,24.2928615780578));
#22741=CARTESIAN_POINT('Ctrl Pts',(132.618025634951,-31.8631049026459,24.2887787267865));
#22742=CARTESIAN_POINT('Ctrl Pts',(132.680900483629,-31.9177933883531,24.2846958755152));
#22743=CARTESIAN_POINT('Ctrl Pts',(132.770582312949,-31.9957985612347,24.2788722818436));
#22744=CARTESIAN_POINT('Ctrl Pts',(132.857001403455,-32.077846930771,24.2730486881721));
#22745=CARTESIAN_POINT('Ctrl Pts',(132.939771970637,-32.1636351150355,24.2672250945006));
#22746=CARTESIAN_POINT('Ctrl Pts',(133.022438110453,-32.2493150647627,24.2614088481575));
#22747=CARTESIAN_POINT('Ctrl Pts',(133.101464601485,-32.3387251532974,24.2555926018144));
#22748=CARTESIAN_POINT('Ctrl Pts',(133.176499167056,-32.4315222325874,24.2497763554713));
#22749=CARTESIAN_POINT('Ctrl Pts',(133.251458622613,-32.5242264214889,24.2439659312229));
#22750=CARTESIAN_POINT('Ctrl Pts',(133.322433846866,-32.6203105406738,24.2381555069745));
#22751=CARTESIAN_POINT('Ctrl Pts',(133.389110273962,-32.7193955733341,24.232345082726));
#22752=CARTESIAN_POINT('Ctrl Pts',(133.458310541732,-32.8222311794219,24.2263147219019));
#22753=CARTESIAN_POINT('Ctrl Pts',(133.522879834287,-32.9282990467355,24.2202843610778));
#22754=CARTESIAN_POINT('Ctrl Pts',(133.58251308558,-33.0371385704409,24.2142540002536));
#22755=CARTESIAN_POINT('Ctrl Pts',(133.63990674693,-33.1418905105017,24.2084501160203));
#22756=CARTESIAN_POINT('Ctrl Pts',(133.692728223576,-33.2492092860081,24.202646231787));
#22757=CARTESIAN_POINT('Ctrl Pts',(133.740750791123,-33.3586564897268,24.1968423475537));
#22758=CARTESIAN_POINT('Ctrl Pts',(133.788766265222,-33.4680875269231,24.1910393206161));
#22759=CARTESIAN_POINT('Ctrl Pts',(133.831984075877,-33.5796459932815,24.1852362936786));
#22760=CARTESIAN_POINT('Ctrl Pts',(133.870224935108,-33.6928718686883,24.179433266741));
#22761=CARTESIAN_POINT('Ctrl Pts',(133.908469170607,-33.8061077407558,24.1736297274569));
#22762=CARTESIAN_POINT('Ctrl Pts',(133.941735450357,-33.9210109276833,24.1678261881727));
#22763=CARTESIAN_POINT('Ctrl Pts',(133.969894022572,-34.0371051721276,24.1620226488886));
#22764=CARTESIAN_POINT('Ctrl Pts',(133.998061726284,-34.1532370645816,24.1562172275843));
#22765=CARTESIAN_POINT('Ctrl Pts',(134.021118332114,-34.2705603860818,24.1504118062801));
#22766=CARTESIAN_POINT('Ctrl Pts',(134.038985099818,-34.3885882210449,24.1446063849758));
#22767=CARTESIAN_POINT('Ctrl Pts',(134.056871653315,-34.5067467609107,24.1387945347048));
#22768=CARTESIAN_POINT('Ctrl Pts',(134.069556835499,-34.6256109675757,24.1329826844338));
#22769=CARTESIAN_POINT('Ctrl Pts',(134.077013719479,-34.7446881687441,24.1271708341628));
#22770=CARTESIAN_POINT('Ctrl Pts',(134.084475501181,-34.8638435804575,24.1213551666374));
#22771=CARTESIAN_POINT('Ctrl Pts',(134.086702138233,-34.983211857953,24.1155394991119));
#22772=CARTESIAN_POINT('Ctrl Pts',(134.083718823924,-35.1023013544955,24.1097238315864));
#22773=CARTESIAN_POINT('Ctrl Pts',(134.080731236339,-35.2215614338824,24.1038998337452));
#22774=CARTESIAN_POINT('Ctrl Pts',(134.072518830281,-35.3405415293661,24.098075835904));
#22775=CARTESIAN_POINT('Ctrl Pts',(134.059158526398,-35.4587559891402,24.0922518380628));
#22776=CARTESIAN_POINT('Ctrl Pts',(134.055613964955,-35.4901189296677,24.0907066996908));
#22777=CARTESIAN_POINT('Ctrl Pts',(134.051707336022,-35.5214280420399,24.0891615613188));
#22778=CARTESIAN_POINT('Ctrl Pts',(134.047440672667,-35.5526744079872,24.0876164229467));
#22779=CARTESIAN_POINT('Ctrl Pts',(134.031359709197,-35.6704412968824,24.0817928292753));
#22780=CARTESIAN_POINT('Ctrl Pts',(134.010108618132,-35.7876956583175,24.0759692356038));
#22781=CARTESIAN_POINT('Ctrl Pts',(133.983729666343,-35.9039485303376,24.0701456419324));
#22782=CARTESIAN_POINT('Ctrl Pts',(133.95738399552,-36.0200547320917,24.0643293955894));
#22783=CARTESIAN_POINT('Ctrl Pts',(133.925923421333,-36.1351615628538,24.0585131492464));
#22784=CARTESIAN_POINT('Ctrl Pts',(133.88944183767,-36.2487862873119,24.0526969029033));
#22785=CARTESIAN_POINT('Ctrl Pts',(133.852996772274,-36.362297272794,24.046886478655));
#22786=CARTESIAN_POINT('Ctrl Pts',(133.811540820233,-36.4743287168497,24.0410760544067));
#22787=CARTESIAN_POINT('Ctrl Pts',(133.765218546725,-36.584409762467,24.0352656301584));
#22788=CARTESIAN_POINT('Ctrl Pts',(133.717142879353,-36.6986576033481,24.0292352693342));
#22789=CARTESIAN_POINT('Ctrl Pts',(133.663825310019,-36.8108040380569,24.02320490851));
#22790=CARTESIAN_POINT('Ctrl Pts',(133.605483849221,-36.9203414313629,24.0171745476859));
#22791=CARTESIAN_POINT('Ctrl Pts',(133.549333463805,-37.0257650317899,24.0113706634526));
#22792=CARTESIAN_POINT('Ctrl Pts',(133.488529946167,-37.128771634557,24.0055667792194));
#22793=CARTESIAN_POINT('Ctrl Pts',(133.423315685409,-37.2289312950451,23.9997628949862));
#22794=CARTESIAN_POINT('Ctrl Pts',(133.358111057496,-37.3290761608802,23.9939598680487));
#22795=CARTESIAN_POINT('Ctrl Pts',(133.288497204863,-37.4263745786227,23.9881568411113));
#22796=CARTESIAN_POINT('Ctrl Pts',(133.21476059592,-37.5204244307099,23.9823538141738));
#22797=CARTESIAN_POINT('Ctrl Pts',(133.141017476806,-37.6144825864156,23.9765502748897));
#22798=CARTESIAN_POINT('Ctrl Pts',(133.063151129624,-37.7052912848461,23.9707467356057));
#22799=CARTESIAN_POINT('Ctrl Pts',(132.981488757071,-37.7924809384234,23.9649431963216));
#22800=CARTESIAN_POINT('Ctrl Pts',(132.899799902363,-37.8796988665885,23.9591377750175));
#22801=CARTESIAN_POINT('Ctrl Pts',(132.814312853083,-37.9632951179704,23.9533323537133));
#22802=CARTESIAN_POINT('Ctrl Pts',(132.725391688841,-38.0429369271146,23.9475269324092));
#22803=CARTESIAN_POINT('Ctrl Pts',(132.63637205264,-38.1226669321908,23.9417150821382));
#22804=CARTESIAN_POINT('Ctrl Pts',(132.543911014788,-38.1984334812215,23.9359032318673));
#22805=CARTESIAN_POINT('Ctrl Pts',(132.448405871834,-38.2699439883226,23.9300913815964));
#22806=CARTESIAN_POINT('Ctrl Pts',(132.352838000591,-38.3415014639086,23.9242757140711));
#22807=CARTESIAN_POINT('Ctrl Pts',(132.254222378933,-38.4087971008361,23.9184600465457));
#22808=CARTESIAN_POINT('Ctrl Pts',(132.152984016047,-38.4715824672108,23.9126443790203));
#22809=CARTESIAN_POINT('Ctrl Pts',(132.051600640138,-38.5344577668432,23.9068203811792));
#22810=CARTESIAN_POINT('Ctrl Pts',(131.947587379506,-38.5928097020869,23.9009963833381));
#22811=CARTESIAN_POINT('Ctrl Pts',(131.841392584403,-38.6464363905196,23.895172385497));
#22812=CARTESIAN_POINT('Ctrl Pts',(131.813218526412,-38.660663843271,23.8936272471241));
#22813=CARTESIAN_POINT('Ctrl Pts',(131.784891016527,-38.674558966587,23.8920821087512));
#22814=CARTESIAN_POINT('Ctrl Pts',(131.756418628183,-38.6881185721951,23.8905369703783));
#22815=CARTESIAN_POINT('Ctrl Pts',(131.649106801957,-38.7392244373993,23.8847133767068));
#22816=CARTESIAN_POINT('Ctrl Pts',(131.539389563275,-38.7857252081775,23.8788897830354));
#22817=CARTESIAN_POINT('Ctrl Pts',(131.427699034966,-38.827388204188,23.8730661893639));
#22818=CARTESIAN_POINT('Ctrl Pts',(131.316149420849,-38.8689986361404,23.8672499430209));
#22819=CARTESIAN_POINT('Ctrl Pts',(131.202631848071,-38.9057832917305,23.8614336966779));
#22820=CARTESIAN_POINT('Ctrl Pts',(131.087601531726,-38.9375560831799,23.8556174503348));
#22821=CARTESIAN_POINT('Ctrl Pts',(130.972686361363,-38.9692970698898,23.8498070260865));
#22822=CARTESIAN_POINT('Ctrl Pts',(130.856261851211,-38.9960360648757,23.8439966018381));
#22823=CARTESIAN_POINT('Ctrl Pts',(130.738801057855,-39.0176358716181,23.8381861775898));
#22824=CARTESIAN_POINT('Ctrl Pts',(130.616894130519,-39.0400532757217,23.8321558167656));
#22825=CARTESIAN_POINT('Ctrl Pts',(130.493871338942,-39.0569345899523,23.8261254559415));
#22826=CARTESIAN_POINT('Ctrl Pts',(130.370276759998,-39.0681838848565,23.8200950951173));
#22827=CARTESIAN_POINT('Ctrl Pts',(130.251323906434,-39.0790107005699,23.8142912108841));
#22828=CARTESIAN_POINT('Ctrl Pts',(130.13184188237,-39.0846208606734,23.8084873266508));
#22829=CARTESIAN_POINT('Ctrl Pts',(130.012323149957,-39.0849814124394,23.8026834424176));
#22830=CARTESIAN_POINT('Ctrl Pts',(129.892822071738,-39.085341910948,23.7968804154801));
#22831=CARTESIAN_POINT('Ctrl Pts',(129.773284704179,-39.0804543419596,23.7910773885427));
#22832=CARTESIAN_POINT('Ctrl Pts',(129.654204398353,-39.0703378731847,23.7852743616052));
#22833=CARTESIAN_POINT('Ctrl Pts',(129.535113578981,-39.0602205112314,23.7794708223211));
#22834=CARTESIAN_POINT('Ctrl Pts',(129.416480308468,-39.044873366173,23.773667283037));
#22835=CARTESIAN_POINT('Ctrl Pts',(129.298793059799,-39.0243675064554,23.767863743753));
#22836=CARTESIAN_POINT('Ctrl Pts',(129.181067646528,-39.0038549969266,23.7620583224488));
#22837=CARTESIAN_POINT('Ctrl Pts',(129.064289267295,-38.9781805157527,23.7562529011446));
#22838=CARTESIAN_POINT('Ctrl Pts',(128.948935812706,-38.9474661587135,23.7504474798405));
#22839=CARTESIAN_POINT('Ctrl Pts',(128.833454614843,-38.9167177883667,23.7446356295695));
#22840=CARTESIAN_POINT('Ctrl Pts',(128.719401886215,-38.880918506736,23.7388237792986));
#22841=CARTESIAN_POINT('Ctrl Pts',(128.607240120711,-38.8402402162679,23.7330119290277));
#22842=CARTESIAN_POINT('Ctrl Pts',(128.495004686756,-38.7995352080802,23.7271962615023));
#22843=CARTESIAN_POINT('Ctrl Pts',(128.384663065915,-38.7539449646649,23.7213805939769));
#22844=CARTESIAN_POINT('Ctrl Pts',(128.276656014011,-38.7036887701256,23.7155649264515));
#22845=CARTESIAN_POINT('Ctrl Pts',(128.168494253667,-38.6533605890145,23.7097409286104));
#22846=CARTESIAN_POINT('Ctrl Pts',(128.062674097762,-38.5983533046016,23.7039169307692));
#22847=CARTESIAN_POINT('Ctrl Pts',(127.959610164208,-38.5389312395121,23.6980929329281));
#22848=CARTESIAN_POINT('Ctrl Pts',(127.932266740854,-38.5231662417456,23.6965477945554));
#22849=CARTESIAN_POINT('Ctrl Pts',(127.905117151511,-38.5070907303505,23.6950026561826));
#22850=CARTESIAN_POINT('Ctrl Pts',(127.878168762405,-38.4907101282068,23.6934575178099));
#22851=CARTESIAN_POINT('Ctrl Pts',(127.776600856886,-38.42897198704,23.6876339241384));
#22852=CARTESIAN_POINT('Ctrl Pts',(127.677565959971,-38.3626976832694,23.6818103304669));
#22853=CARTESIAN_POINT('Ctrl Pts',(127.581495552781,-38.2921210850732,23.6759867367955));
#22854=CARTESIAN_POINT('Ctrl Pts',(127.48554635268,-38.221633529739,23.6701704904524));
#22855=CARTESIAN_POINT('Ctrl Pts',(127.392554529426,-38.1468547157337,23.6643542441094));
#22856=CARTESIAN_POINT('Ctrl Pts',(127.302925253799,-38.0680633652851,23.6585379977664));
#22857=CARTESIAN_POINT('Ctrl Pts',(127.213385697572,-37.9893508854131,23.652727573518));
#22858=CARTESIAN_POINT('Ctrl Pts',(127.127202297796,-37.9066341276188,23.6469171492697));
#22859=CARTESIAN_POINT('Ctrl Pts',(127.04474911407,-37.8202335366442,23.6411067250213));
#22860=CARTESIAN_POINT('Ctrl Pts',(126.959174906799,-37.7305625045942,23.6350763641972));
#22861=CARTESIAN_POINT('Ctrl Pts',(126.877619249222,-37.6369235130641,23.629046003373));
#22862=CARTESIAN_POINT('Ctrl Pts',(126.800460617092,-37.5397190272199,23.6230156425488));
#22863=CARTESIAN_POINT('Ctrl Pts',(126.726199759155,-37.4461651588457,23.6172117583156));
#22864=CARTESIAN_POINT('Ctrl Pts',(126.656011889451,-37.3493091269353,23.6114078740823));
#22865=CARTESIAN_POINT('Ctrl Pts',(126.590194518506,-37.2495447491381,23.6056039898491));
#22866=CARTESIAN_POINT('Ctrl Pts',(126.524386869491,-37.1497951076065,23.5998009629116));
#22867=CARTESIAN_POINT('Ctrl Pts',(126.462948660205,-37.0471383152667,23.5939979359741));
#22868=CARTESIAN_POINT('Ctrl Pts',(126.406134296419,-36.9419975037632,23.5881949090366));
#22869=CARTESIAN_POINT('Ctrl Pts',(126.349314916518,-36.8368474094255,23.5823913697525));
#22870=CARTESIAN_POINT('Ctrl Pts',(126.297120387922,-36.7292132191378,23.5765878304684));
#22871=CARTESIAN_POINT('Ctrl Pts',(126.249759034134,-36.6195424347449,23.5707842911843));
#22872=CARTESIAN_POINT('Ctrl Pts',(126.202382321611,-36.5098360853956,23.5649788698802));
#22873=CARTESIAN_POINT('Ctrl Pts',(126.159842062791,-36.3980922031492,23.559173448576));
#22874=CARTESIAN_POINT('Ctrl Pts',(126.122298102512,-36.2847774103789,23.5533680272718));
#22875=CARTESIAN_POINT('Ctrl Pts',(126.084712565772,-36.171337131964,23.5475561770008));
#22876=CARTESIAN_POINT('Ctrl Pts',(126.052134500294,-36.0563228584039,23.5417443267299));
#22877=CARTESIAN_POINT('Ctrl Pts',(126.024673654136,-35.9402156369025,23.535932476459));
#22878=CARTESIAN_POINT('Ctrl Pts',(125.997194771546,-35.8240321555548,23.5301168089336));
#22879=CARTESIAN_POINT('Ctrl Pts',(125.97483987811,-35.7067546968341,23.5243011414082));
#22880=CARTESIAN_POINT('Ctrl Pts',(125.957667177219,-35.588872099752,23.5184854738828));
#22881=CARTESIAN_POINT('Ctrl Pts',(125.940469878288,-35.4708206485788,23.5126614760416));
#22882=CARTESIAN_POINT('Ctrl Pts',(125.92846962861,-35.3521627337903,23.5068374782005));
#22883=CARTESIAN_POINT('Ctrl Pts',(125.921672634806,-35.2333900218802,23.5010134803594));
#22884=CARTESIAN_POINT('Ctrl Pts',(125.919869355301,-35.2018789740052,23.4994683419867));
#22885=CARTESIAN_POINT('Ctrl Pts',(125.91843203318,-35.1703598310429,23.497923203614));
#22886=CARTESIAN_POINT('Ctrl Pts',(125.917360170799,-35.1388417265164,23.4963780652414));
#22887=CARTESIAN_POINT('Ctrl Pts',(125.915796331449,-35.0928570432683,23.4941237196927));
#22888=CARTESIAN_POINT('Ctrl Pts',(125.91500938505,-35.0468457909017,23.4918693741441));
#22889=CARTESIAN_POINT('Ctrl Pts',(125.915000083442,-35.0008256619992,23.4896150285955));
#22890=CARTESIAN_POINT('Origin',(130.,-35.,32.7603849714045));
#22891=CARTESIAN_POINT('',(132.487160670875,-31.7594357285724,25.5469383396565));
#22892=CARTESIAN_POINT('',(132.487160670875,-31.7594357285724,25.4425452647471));
#22893=CARTESIAN_POINT('',(132.487160670875,-31.7594357285724,32.7603849714045));
#22894=CARTESIAN_POINT('',(125.915001572211,-35.0035839873014,24.6353849714487));
#22895=CARTESIAN_POINT('Ctrl Pts',(132.487160670875,-31.7594357285724,25.4425452647471));
#22896=CARTESIAN_POINT('Ctrl Pts',(132.581714430403,-31.8320065441103,25.4367339326408));
#22897=CARTESIAN_POINT('Ctrl Pts',(132.673191712905,-31.9087977384192,25.4309226005346));
#22898=CARTESIAN_POINT('Ctrl Pts',(132.761197144929,-31.9895157653901,25.4251112684283));
#22899=CARTESIAN_POINT('Ctrl Pts',(132.849133405474,-32.070170348716,25.419304503977));
#22900=CARTESIAN_POINT('Ctrl Pts',(132.933602945501,-32.154745348426,25.4134977395256));
#22901=CARTESIAN_POINT('Ctrl Pts',(133.014243150667,-32.2429067428431,25.4076909750742));
#22902=CARTESIAN_POINT('Ctrl Pts',(133.094848361656,-32.3310298792302,25.4018867304942));
#22903=CARTESIAN_POINT('Ctrl Pts',(133.171627266642,-32.4227360152345,25.3960824859141));
#22904=CARTESIAN_POINT('Ctrl Pts',(133.244254186697,-32.5176543810142,25.3902782413341));
#22905=CARTESIAN_POINT('Ctrl Pts',(133.316866721276,-32.6125539459704,25.3844751464217));
#22906=CARTESIAN_POINT('Ctrl Pts',(133.385328658296,-32.7106641513093,25.3786720515093));
#22907=CARTESIAN_POINT('Ctrl Pts',(133.449355108616,-32.8115817733659,25.372868956597));
#22908=CARTESIAN_POINT('Ctrl Pts',(133.513383987267,-32.9125032229253,25.3670656415906));
#22909=CARTESIAN_POINT('Ctrl Pts',(133.572976826082,-33.0162319560225,25.3612623265843));
#22910=CARTESIAN_POINT('Ctrl Pts',(133.62789286766,-33.12233700021,25.3554590115779));
#22911=CARTESIAN_POINT('Ctrl Pts',(133.682823952171,-33.2284711093287,25.3496541068927));
#22912=CARTESIAN_POINT('Ctrl Pts',(133.73307550409,-33.336982461524,25.3438492022074));
#22913=CARTESIAN_POINT('Ctrl Pts',(133.778453683459,-33.4474173896512,25.3380442975221));
#22914=CARTESIAN_POINT('Ctrl Pts',(133.82388104049,-33.5579719993444,25.3322331018916));
#22915=CARTESIAN_POINT('Ctrl Pts',(133.864424325119,-33.6704539689137,25.3264219062611));
#22916=CARTESIAN_POINT('Ctrl Pts',(133.899938573092,-33.7843914585251,25.3206107106306));
#22917=CARTESIAN_POINT('Ctrl Pts',(133.935474542879,-33.8983986364736,25.3147959606603));
#22918=CARTESIAN_POINT('Ctrl Pts',(133.9659752453,-34.0138627134301,25.30898121069));
#22919=CARTESIAN_POINT('Ctrl Pts',(133.991346549699,-34.1303002125992,25.3031664607196));
#22920=CARTESIAN_POINT('Ctrl Pts',(134.016755656369,-34.2469111991799,25.2973430469947));
#22921=CARTESIAN_POINT('Ctrl Pts',(134.037020035604,-34.3644981023516,25.2915196332697));
#22922=CARTESIAN_POINT('Ctrl Pts',(134.05209720878,-34.4825705742856,25.2856962195447));
#22923=CARTESIAN_POINT('Ctrl Pts',(134.059311378333,-34.539066233128,25.2829098156547));
#22924=CARTESIAN_POINT('Ctrl Pts',(134.065338727097,-34.5956730301281,25.2801234117646));
#22925=CARTESIAN_POINT('Ctrl Pts',(134.07017882144,-34.6523372877341,25.2773370078746));
#22926=CARTESIAN_POINT('Ctrl Pts',(134.080294635191,-34.7707657801741,25.2715134142026));
#22927=CARTESIAN_POINT('Ctrl Pts',(134.085253665983,-34.8898271179956,25.2656898205305));
#22928=CARTESIAN_POINT('Ctrl Pts',(134.084990008492,-35.009034961019,25.2598662268584));
#22929=CARTESIAN_POINT('Ctrl Pts',(134.084726683644,-35.1280924056418,25.2540499805148));
#22930=CARTESIAN_POINT('Ctrl Pts',(134.079253777168,-35.2472955830911,25.2482337341712));
#22931=CARTESIAN_POINT('Ctrl Pts',(134.068557120453,-35.3661529156075,25.2424174878276));
#22932=CARTESIAN_POINT('Ctrl Pts',(134.057871171151,-35.4848912712785,25.2366070635786));
#22933=CARTESIAN_POINT('Ctrl Pts',(134.041971910454,-35.6032840663682,25.2307966393297));
#22934=CARTESIAN_POINT('Ctrl Pts',(134.020897212403,-35.7208402092625,25.2249862150807));
#22935=CARTESIAN_POINT('Ctrl Pts',(133.999024793444,-35.8428460952959,25.2189558542568));
#22936=CARTESIAN_POINT('Ctrl Pts',(133.971577394719,-35.9639502914226,25.2129254934329));
#22937=CARTESIAN_POINT('Ctrl Pts',(133.938656491478,-36.0836097277777,25.2068951326089));
#22938=CARTESIAN_POINT('Ctrl Pts',(133.90697196764,-36.1987752272179,25.2010912483751));
#22939=CARTESIAN_POINT('Ctrl Pts',(133.87021776973,-36.3126020997472,25.1952873641412));
#22940=CARTESIAN_POINT('Ctrl Pts',(133.828536183256,-36.4246177359195,25.1894834799073));
#22941=CARTESIAN_POINT('Ctrl Pts',(133.786860753598,-36.5366168261844,25.1836804529692));
#22942=CARTESIAN_POINT('Ctrl Pts',(133.740259525162,-36.6468048295454,25.1778774260311));
#22943=CARTESIAN_POINT('Ctrl Pts',(133.688923889136,-36.7547266283285,25.172074399093));
#22944=CARTESIAN_POINT('Ctrl Pts',(133.637583720709,-36.8626579554779,25.1662708598084));
#22945=CARTESIAN_POINT('Ctrl Pts',(133.581508489022,-36.9683223114745,25.1604673205237));
#22946=CARTESIAN_POINT('Ctrl Pts',(133.520936457764,-37.0712873920311,25.154663781239));
#22947=CARTESIAN_POINT('Ctrl Pts',(133.460344783703,-37.1742858629626,25.1488583599342));
#22948=CARTESIAN_POINT('Ctrl Pts',(133.395253616862,-37.2745829658215,25.1430529386293));
#22949=CARTESIAN_POINT('Ctrl Pts',(133.325945270333,-37.3717742427873,25.1372475173245));
#22950=CARTESIAN_POINT('Ctrl Pts',(133.256560171226,-37.4690731500963,25.131435667053));
#22951=CARTESIAN_POINT('Ctrl Pts',(133.182948807663,-37.5632590334871,25.1256238167814));
#22952=CARTESIAN_POINT('Ctrl Pts',(133.105434706826,-37.6539593594549,25.1198119665099));
#22953=CARTESIAN_POINT('Ctrl Pts',(133.027869694312,-37.7447192578837,25.1139962989839));
#22954=CARTESIAN_POINT('Ctrl Pts',(132.946397117582,-37.8319887418307,25.1081806314578));
#22955=CARTESIAN_POINT('Ctrl Pts',(132.861377218281,-37.9154322860769,25.1023649639318));
#22956=CARTESIAN_POINT('Ctrl Pts',(132.776235537155,-37.99899535419,25.0965409660901));
#22957=CARTESIAN_POINT('Ctrl Pts',(132.687536694358,-38.0787212723311,25.0907169682483));
#22958=CARTESIAN_POINT('Ctrl Pts',(132.595673905588,-38.1543148187598,25.0848929704065));
#22959=CARTESIAN_POINT('Ctrl Pts',(132.571302207098,-38.1743701985937,25.0833478320398));
#22960=CARTESIAN_POINT('Ctrl Pts',(132.546707963692,-38.194134951354,25.081802693673));
#22961=CARTESIAN_POINT('Ctrl Pts',(132.521898841803,-38.2136040875807,25.0802575553062));
#22962=CARTESIAN_POINT('Ctrl Pts',(132.428393788576,-38.286982848314,25.0744339616348));
#22963=CARTESIAN_POINT('Ctrl Pts',(132.331532681142,-38.3563955273654,25.0686103679635));
#22964=CARTESIAN_POINT('Ctrl Pts',(132.231686153495,-38.4215204094524,25.0627867742921));
#22965=CARTESIAN_POINT('Ctrl Pts',(132.131965597074,-38.486563126827,25.0569705279492));
#22966=CARTESIAN_POINT('Ctrl Pts',(132.029267451023,-38.547328585876,25.0511542816063));
#22967=CARTESIAN_POINT('Ctrl Pts',(131.92399509008,-38.6035354713597,25.0453380352634));
#22968=CARTESIAN_POINT('Ctrl Pts',(131.818828107351,-38.6596860934409,25.0395276110152));
#22969=CARTESIAN_POINT('Ctrl Pts',(131.711092394101,-38.711287028576,25.033717186767));
#22970=CARTESIAN_POINT('Ctrl Pts',(131.601219446355,-38.7581007549844,25.0279067625187));
#22971=CARTESIAN_POINT('Ctrl Pts',(131.487187580277,-38.8066864777663,25.0218764016945));
#22972=CARTESIAN_POINT('Ctrl Pts',(131.37085386077,-38.8501151747698,25.0158460408703));
#22973=CARTESIAN_POINT('Ctrl Pts',(131.252728120834,-38.8881740258469,25.0098156800461));
#22974=CARTESIAN_POINT('Ctrl Pts',(131.139038718239,-38.9248035364411,25.004011795813));
#22975=CARTESIAN_POINT('Ctrl Pts',(131.023689893896,-38.9564591314116,24.9982079115799));
#22976=CARTESIAN_POINT('Ctrl Pts',(130.907154920439,-38.983000746965,24.9924040273467));
#22977=CARTESIAN_POINT('Ctrl Pts',(130.790637160444,-39.0095384420378,24.9866010004094));
#22978=CARTESIAN_POINT('Ctrl Pts',(130.672933997801,-39.0309635692697,24.980797973472));
#22979=CARTESIAN_POINT('Ctrl Pts',(130.554530993478,-39.0471867237963,24.9749949465347));
#22980=CARTESIAN_POINT('Ctrl Pts',(130.436117535408,-39.0634113106577,24.9691914072507));
#22981=CARTESIAN_POINT('Ctrl Pts',(130.317004517384,-39.074432956221,24.9633878679668));
#22982=CARTESIAN_POINT('Ctrl Pts',(130.197684113715,-39.0802139638975,24.9575843286828));
#22983=CARTESIAN_POINT('Ctrl Pts',(130.078325015831,-39.0859968462875,24.9517789073787));
#22984=CARTESIAN_POINT('Ctrl Pts',(129.9587588062,-39.0865356911628,24.9459734860747));
#22985=CARTESIAN_POINT('Ctrl Pts',(129.839478515428,-39.0818449080031,24.9401680647706));
#22986=CARTESIAN_POINT('Ctrl Pts',(129.720066132774,-39.0771489302352,24.9343562144998));
#22987=CARTESIAN_POINT('Ctrl Pts',(129.60094070926,-39.067211780499,24.928544364229));
#22988=CARTESIAN_POINT('Ctrl Pts',(129.482591166976,-39.0520998382949,24.9227325139582));
#22989=CARTESIAN_POINT('Ctrl Pts',(129.364163892078,-39.0369779704859,24.9169168464329));
#22990=CARTESIAN_POINT('Ctrl Pts',(129.246513914762,-39.0166746106328,24.9111011789076));
#22991=CARTESIAN_POINT('Ctrl Pts',(129.130119329986,-38.9913071317472,24.9052855113824));
#22992=CARTESIAN_POINT('Ctrl Pts',(129.013558022536,-38.9659033166873,24.8994615135414));
#22993=CARTESIAN_POINT('Ctrl Pts',(128.898256090138,-38.935421008393,24.8936375157003));
#22994=CARTESIAN_POINT('Ctrl Pts',(128.784675994262,-38.900027251325,24.8878135178593));
#22995=CARTESIAN_POINT('Ctrl Pts',(128.7545425757,-38.8906370946432,24.8862683794854));
#22996=CARTESIAN_POINT('Ctrl Pts',(128.724530238221,-38.880901496636,24.8847232411116));
#22997=CARTESIAN_POINT('Ctrl Pts',(128.694647357324,-38.8708241342457,24.8831781027377));
#22998=CARTESIAN_POINT('Ctrl Pts',(128.582019414727,-38.832842769707,24.8773545090663));
#22999=CARTESIAN_POINT('Ctrl Pts',(128.470868921731,-38.7898804367451,24.8715309153949));
#23000=CARTESIAN_POINT('Ctrl Pts',(128.361668119773,-38.7420707703399,24.8657073217235));
#23001=CARTESIAN_POINT('Ctrl Pts',(128.252605090847,-38.6943214229304,24.8598910753806));
#23002=CARTESIAN_POINT('Ctrl Pts',(128.145487231185,-38.6417370682485,24.8540748290376));
#23003=CARTESIAN_POINT('Ctrl Pts',(128.040770940075,-38.584500870518,24.8482585826947));
#23004=CARTESIAN_POINT('Ctrl Pts',(127.93615947055,-38.5273219665372,24.8424481584464));
#23005=CARTESIAN_POINT('Ctrl Pts',(127.833945143398,-38.4655006777978,24.8366377341981));
#23006=CARTESIAN_POINT('Ctrl Pts',(127.734563145387,-38.3992676943364,24.8308273099498));
#23007=CARTESIAN_POINT('Ctrl Pts',(127.631419333192,-38.3305276554567,24.8247969491256));
#23008=CARTESIAN_POINT('Ctrl Pts',(127.531326916346,-38.257035519091,24.8187665883015));
#23009=CARTESIAN_POINT('Ctrl Pts',(127.434743363361,-38.1791010345973,24.8127362274773));
#23010=CARTESIAN_POINT('Ctrl Pts',(127.341787108056,-38.1040934622545,24.8069323432441));
#23011=CARTESIAN_POINT('Ctrl Pts',(127.252081257698,-38.0249714780642,24.8011284590109));
#23012=CARTESIAN_POINT('Ctrl Pts',(127.166002388424,-37.9420541357325,24.7953245747778));
#23013=CARTESIAN_POINT('Ctrl Pts',(127.079936233919,-37.8591490411788,24.7895215478404));
#23014=CARTESIAN_POINT('Ctrl Pts',(126.99749628908,-37.7724499865799,24.783718520903));
#23015=CARTESIAN_POINT('Ctrl Pts',(126.919023496393,-37.6823140726292,24.7779154939656));
#23016=CARTESIAN_POINT('Ctrl Pts',(126.84054377538,-37.59217020062,24.7721119546816));
#23017=CARTESIAN_POINT('Ctrl Pts',(126.766032171054,-37.4985891739393,24.7663084153976));
#23018=CARTESIAN_POINT('Ctrl Pts',(126.695790003784,-37.4019619690804,24.7605048761136));
#23019=CARTESIAN_POINT('Ctrl Pts',(126.625525057799,-37.3053034291459,24.7546994548095));
#23020=CARTESIAN_POINT('Ctrl Pts',(126.55953254236,-37.2055970765615,24.7488940335054));
#23021=CARTESIAN_POINT('Ctrl Pts',(126.498070667217,-37.1032631666515,24.7430886122013));
#23022=CARTESIAN_POINT('Ctrl Pts',(126.436540728735,-37.0008159314082,24.7372767619305));
#23023=CARTESIAN_POINT('Ctrl Pts',(126.379551655806,-36.8957356809368,24.7314649116596));
#23024=CARTESIAN_POINT('Ctrl Pts',(126.327315939811,-36.7884677223906,24.7256530613888));
#23025=CARTESIAN_POINT('Ctrl Pts',(126.275045915117,-36.6811293096734,24.7198373938634));
#23026=CARTESIAN_POINT('Ctrl Pts',(126.227535627083,-36.5716007010129,24.7140217263381));
#23027=CARTESIAN_POINT('Ctrl Pts',(126.184948982551,-36.4603461008479,24.7082060588128));
#23028=CARTESIAN_POINT('Ctrl Pts',(126.142301337249,-36.3489321404818,24.7023820609718));
#23029=CARTESIAN_POINT('Ctrl Pts',(126.104591540684,-36.2357876400545,24.6965580631307));
#23030=CARTESIAN_POINT('Ctrl Pts',(126.071933386223,-36.1213909566845,24.6907340652897));
#23031=CARTESIAN_POINT('Ctrl Pts',(126.063268999827,-36.0910408930177,24.6891889269162));
#23032=CARTESIAN_POINT('Ctrl Pts',(126.054959902828,-36.0606027397222,24.6876437885428));
#23033=CARTESIAN_POINT('Ctrl Pts',(126.047007611079,-36.0300855173897,24.6860986501693));
#23034=CARTESIAN_POINT('Ctrl Pts',(126.008453455647,-35.882132478141,24.6786075385628));
#23035=CARTESIAN_POINT('Ctrl Pts',(125.978189862158,-35.7319372299234,24.6711164269563));
#23036=CARTESIAN_POINT('Ctrl Pts',(125.956429349327,-35.5803114620726,24.6636253153498));
#23037=CARTESIAN_POINT('Ctrl Pts',(125.935075376487,-35.4315184371298,24.6562741561642));
#23038=CARTESIAN_POINT('Ctrl Pts',(125.921909712316,-35.2813476384019,24.6489229969786));
#23039=CARTESIAN_POINT('Ctrl Pts',(125.917087813763,-35.1305874399659,24.6415718377929));
#23040=CARTESIAN_POINT('Ctrl Pts',(125.915735081896,-35.0882932849811,24.6395095490115));
#23041=CARTESIAN_POINT('Ctrl Pts',(125.915038744708,-35.0459528841619,24.6374472602301));
#23042=CARTESIAN_POINT('Ctrl Pts',(125.915001572211,-35.0035839873014,24.6353849714487));
#23043=CARTESIAN_POINT('Ctrl Pts',(125.915001572211,-35.0035839863923,24.6353849714045));
#23044=CARTESIAN_POINT('Ctrl Pts',(125.914897993777,-34.8855261338114,24.629638553561));
#23045=CARTESIAN_POINT('Ctrl Pts',(125.919916516331,-34.7673454041149,24.6238921357174));
#23046=CARTESIAN_POINT('Ctrl Pts',(125.930062305213,-34.6495258061531,24.6181457178739));
#23047=CARTESIAN_POINT('Ctrl Pts',(125.940202397681,-34.5317723587141,24.6124025263913));
#23048=CARTESIAN_POINT('Ctrl Pts',(125.955463997557,-34.414380055344,24.6066593349087));
#23049=CARTESIAN_POINT('Ctrl Pts',(125.975800204933,-34.2978312101882,24.600916143426));
#23050=CARTESIAN_POINT('Ctrl Pts',(125.996130870098,-34.1813141280032,24.5951745171312));
#23051=CARTESIAN_POINT('Ctrl Pts',(126.021533322221,-34.0656404586676,24.5894328908363));
#23052=CARTESIAN_POINT('Ctrl Pts',(126.051909088729,-33.9512849975634,24.5836912645414));
#23053=CARTESIAN_POINT('Ctrl Pts',(126.082284131011,-33.8369322629426,24.5779497751394));
#23054=CARTESIAN_POINT('Ctrl Pts',(126.11763214416,-33.7238980780043,24.5722082857373));
#23055=CARTESIAN_POINT('Ctrl Pts',(126.157804255104,-33.6126439325464,24.5664667963353));
#23056=CARTESIAN_POINT('Ctrl Pts',(126.197985399101,-33.5013647706106,24.5607240159087));
#23057=CARTESIAN_POINT('Ctrl Pts',(126.242992654503,-33.3918668366453,24.554981235482));
#23058=CARTESIAN_POINT('Ctrl Pts',(126.292628585109,-33.2845927037431,24.5492384550554));
#23059=CARTESIAN_POINT('Ctrl Pts',(126.34231651387,-33.1772061914231,24.5434896585436));
#23060=CARTESIAN_POINT('Ctrl Pts',(126.396642621412,-33.0720485102871,24.5377408620317));
#23061=CARTESIAN_POINT('Ctrl Pts',(126.455362953409,-32.9695386711551,24.5319920655199));
#23062=CARTESIAN_POINT('Ctrl Pts',(126.514117959328,-32.8669683007208,24.5262398743862));
#23063=CARTESIAN_POINT('Ctrl Pts',(126.577272131778,-32.7670492373216,24.5204876832525));
#23064=CARTESIAN_POINT('Ctrl Pts',(126.644538532043,-32.6701709639857,24.5147354921189));
#23065=CARTESIAN_POINT('Ctrl Pts',(126.711905430002,-32.5731479520721,24.5089747070669));
#23066=CARTESIAN_POINT('Ctrl Pts',(126.783396567165,-32.4791751304812,24.503213922015));
#23067=CARTESIAN_POINT('Ctrl Pts',(126.858685058136,-32.388608524939,24.4974531369631));
#23068=CARTESIAN_POINT('Ctrl Pts',(126.895426495388,-32.3444112351312,24.4946418238423));
#23069=CARTESIAN_POINT('Ctrl Pts',(126.933071724442,-32.3010245830182,24.4918305107216));
#23070=CARTESIAN_POINT('Ctrl Pts',(126.971579748943,-32.2584865889459,24.4890191976008));
#23071=CARTESIAN_POINT('Ctrl Pts',(127.051348553824,-32.1703697615288,24.4831956039294));
#23072=CARTESIAN_POINT('Ctrl Pts',(127.135095038229,-32.0855952341228,24.4773720102579));
#23073=CARTESIAN_POINT('Ctrl Pts',(127.222508227281,-32.0045426972705,24.4715484165865));
#23074=CARTESIAN_POINT('Ctrl Pts',(127.30981113161,-31.9235924202328,24.4657321702435));
#23075=CARTESIAN_POINT('Ctrl Pts',(127.400771242611,-31.8463550690165,24.4599159239005));
#23076=CARTESIAN_POINT('Ctrl Pts',(127.495038491786,-31.7731760441003,24.4540996775575));
#23077=CARTESIAN_POINT('Ctrl Pts',(127.589211378925,-31.7000702717917,24.4482892533091));
#23078=CARTESIAN_POINT('Ctrl Pts',(127.686684497781,-31.6310149930845,24.4424788290608));
#23079=CARTESIAN_POINT('Ctrl Pts',(127.787072666214,-31.5663171935396,24.4366684048125));
#23080=CARTESIAN_POINT('Ctrl Pts',(127.89126073446,-31.4991704484638,24.4306380439883));
#23081=CARTESIAN_POINT('Ctrl Pts',(127.998588565236,-31.436717884397,24.4246076831641));
#23082=CARTESIAN_POINT('Ctrl Pts',(128.108589592872,-31.379255370534,24.4185773223399));
#23083=CARTESIAN_POINT('Ctrl Pts',(128.21445941535,-31.3239509222704,24.4127734381067));
#23084=CARTESIAN_POINT('Ctrl Pts',(128.322804871712,-31.2732686763006,24.4069695538735));
#23085=CARTESIAN_POINT('Ctrl Pts',(128.433183143552,-31.2274266159093,24.4011656696403));
#23086=CARTESIAN_POINT('Ctrl Pts',(128.54354511134,-31.1815913268806,24.3953626427028));
#23087=CARTESIAN_POINT('Ctrl Pts',(128.655938920462,-31.1405949582032,24.3895596157653));
#23088=CARTESIAN_POINT('Ctrl Pts',(128.769901084859,-31.104607637353,24.3837565888279));
#23089=CARTESIAN_POINT('Ctrl Pts',(128.883873310923,-31.0686171391988,24.3779530495438));
#23090=CARTESIAN_POINT('Ctrl Pts',(128.99941377817,-31.0376366911317,24.3721495102598));
#23091=CARTESIAN_POINT('Ctrl Pts',(129.116043749136,-31.0117865720905,24.3663459709757));
#23092=CARTESIAN_POINT('Ctrl Pts',(129.232711541842,-30.9859280701569,24.3605405496715));
#23093=CARTESIAN_POINT('Ctrl Pts',(129.35046914247,-30.9652032942997,24.3547351283673));
#23094=CARTESIAN_POINT('Ctrl Pts',(129.468828169307,-30.949681310529,24.3489297070631));
#23095=CARTESIAN_POINT('Ctrl Pts',(129.587318267811,-30.934142137598,24.3431178567922));
#23096=CARTESIAN_POINT('Ctrl Pts',(129.706410716854,-30.9238173105492,24.3373060065213));
#23097=CARTESIAN_POINT('Ctrl Pts',(129.825612406945,-30.9187239780446,24.3314941562504));
#23098=CARTESIAN_POINT('Ctrl Pts',(129.944892389345,-30.9136273002118,24.325678488725));
#23099=CARTESIAN_POINT('Ctrl Pts',(130.064281348287,-30.9137689594673,24.3198628211996));
#23100=CARTESIAN_POINT('Ctrl Pts',(130.183288233521,-30.9191140148918,24.3140471536742));
#23101=CARTESIAN_POINT('Ctrl Pts',(130.302465583268,-30.924466726531,24.3082231558331));
#23102=CARTESIAN_POINT('Ctrl Pts',(130.421259361681,-30.9350376746623,24.302399157992));
#23103=CARTESIAN_POINT('Ctrl Pts',(130.539185538356,-30.9507403201045,24.2965751601509));
#23104=CARTESIAN_POINT('Ctrl Pts',(130.570471995823,-30.9549063175326,24.2950300217781));
#23105=CARTESIAN_POINT('Ctrl Pts',(130.601697453545,-30.9594332434423,24.2934848834052));
#23106=CARTESIAN_POINT('Ctrl Pts',(130.632853035338,-30.964318888259,24.2919397450324));
#23107=CARTESIAN_POINT('Ctrl Pts',(130.750277186332,-30.9827326896275,24.2861161798426));
#23108=CARTESIAN_POINT('Ctrl Pts',(130.86708635909,-31.0063053840004,24.2802926146528));
#23109=CARTESIAN_POINT('Ctrl Pts',(130.98279253345,-31.0349850143794,24.274469049463));
#23110=CARTESIAN_POINT('Ctrl Pts',(131.098358075083,-31.0636297866824,24.2686525624076));
#23111=CARTESIAN_POINT('Ctrl Pts',(131.212822891391,-31.0973690542092,24.2628360753522));
#23112=CARTESIAN_POINT('Ctrl Pts',(131.325706145032,-31.1360993520763,24.2570195882968));
#23113=CARTESIAN_POINT('Ctrl Pts',(131.438460699241,-31.1747854931074,24.2512097326819));
#23114=CARTESIAN_POINT('Ctrl Pts',(131.549636896169,-31.2184512054732,24.245399877067));
#23115=CARTESIAN_POINT('Ctrl Pts',(131.658766976281,-31.2669426580348,24.2395900214521));
#23116=CARTESIAN_POINT('Ctrl Pts',(131.76782430422,-31.3154017835011,24.2337840390096));
#23117=CARTESIAN_POINT('Ctrl Pts',(131.874837856293,-31.3686800860968,24.2279780565671));
#23118=CARTESIAN_POINT('Ctrl Pts',(131.979358124371,-31.4265749741338,24.2221720741247));
#23119=CARTESIAN_POINT('Ctrl Pts',(132.083838706939,-31.4844478799449,24.2163682961673));
#23120=CARTESIAN_POINT('Ctrl Pts',(132.185827530777,-31.5469336892226,24.2105645182099));
#23121=CARTESIAN_POINT('Ctrl Pts',(132.284898567803,-31.6137833006653,24.2047607402525));
#23122=CARTESIAN_POINT('Ctrl Pts',(132.353774094002,-31.6602580555742,24.200725875243));
#23123=CARTESIAN_POINT('Ctrl Pts',(132.421239867495,-31.7088409506797,24.1966910102334));
#23124=CARTESIAN_POINT('Ctrl Pts',(132.487160670875,-31.7594357285724,24.1926561452238));
#23125=CARTESIAN_POINT('',(125.915001332191,-34.9967009094887,24.7396150285626));
#23126=CARTESIAN_POINT('Ctrl Pts',(125.915001332191,-34.9967009094887,24.7396150285626));
#23127=CARTESIAN_POINT('Ctrl Pts',(125.915116126591,-34.8545602292439,24.7327077308601));
#23128=CARTESIAN_POINT('Ctrl Pts',(125.922653598402,-34.712731699299,24.7258004331577));
#23129=CARTESIAN_POINT('Ctrl Pts',(125.93749319404,-34.5719071928536,24.7188931354552));
#23130=CARTESIAN_POINT('Ctrl Pts',(125.952505705087,-34.4294417571279,24.7119053518535));
#23131=CARTESIAN_POINT('Ctrl Pts',(125.974991434025,-34.2880039252054,24.7049175682517));
#23132=CARTESIAN_POINT('Ctrl Pts',(126.00477616189,-34.148289084606,24.69792978465));
#23133=CARTESIAN_POINT('Ctrl Pts',(126.031877926699,-34.0211595446883,24.691571449984));
#23134=CARTESIAN_POINT('Ctrl Pts',(126.065022300518,-33.8954563164075,24.685213115318));
#23135=CARTESIAN_POINT('Ctrl Pts',(126.104043775727,-33.7716881102292,24.6788547806521));
#23136=CARTESIAN_POINT('Ctrl Pts',(126.139783513885,-33.6583289084763,24.6730311869807));
#23137=CARTESIAN_POINT('Ctrl Pts',(126.180532547933,-33.546348060245,24.6672075933094));
#23138=CARTESIAN_POINT('Ctrl Pts',(126.226166636842,-33.4362203649119,24.661383999638));
#23139=CARTESIAN_POINT('Ctrl Pts',(126.271743151569,-33.3262316120246,24.6555677532951));
#23140=CARTESIAN_POINT('Ctrl Pts',(126.322192307714,-33.218091735661,24.6497515069522));
#23141=CARTESIAN_POINT('Ctrl Pts',(126.377340030494,-33.1122606786577,24.6439352606093));
#23142=CARTESIAN_POINT('Ctrl Pts',(126.4324325501,-33.0065355591265,24.6381248363611));
#23143=CARTESIAN_POINT('Ctrl Pts',(126.49221409211,-32.9031150212668,24.6323144121129));
#23144=CARTESIAN_POINT('Ctrl Pts',(126.556462644498,-32.8024387423191,24.6265039878647));
#23145=CARTESIAN_POINT('Ctrl Pts',(126.623143137484,-32.6979516579758,24.6204736270405));
#23146=CARTESIAN_POINT('Ctrl Pts',(126.694635322155,-32.5964211032217,24.6144432662162));
#23147=CARTESIAN_POINT('Ctrl Pts',(126.770638584713,-32.4983106009231,24.608412905392));
#23148=CARTESIAN_POINT('Ctrl Pts',(126.843787464204,-32.4038847425054,24.6026090211589));
#23149=CARTESIAN_POINT('Ctrl Pts',(126.921114422887,-32.3126270336183,24.5968051369258));
#23150=CARTESIAN_POINT('Ctrl Pts',(127.002307939814,-32.2249203052349,24.5910012526927));
#23151=CARTESIAN_POINT('Ctrl Pts',(127.08348946359,-32.1372265320732,24.5851982257553));
#23152=CARTESIAN_POINT('Ctrl Pts',(127.168536132488,-32.0530829958835,24.579395198818));
#23153=CARTESIAN_POINT('Ctrl Pts',(127.257097679211,-31.9728376557226,24.5735921718806));
#23154=CARTESIAN_POINT('Ctrl Pts',(127.345667044993,-31.8925852307372,24.5677886325967));
#23155=CARTESIAN_POINT('Ctrl Pts',(127.437751602994,-31.8162319602679,24.5619850933127));
#23156=CARTESIAN_POINT('Ctrl Pts',(127.532966430816,-31.7440868610295,24.5561815540288));
#23157=CARTESIAN_POINT('Ctrl Pts',(127.628212135697,-31.6719183659768,24.5503761327247));
#23158=CARTESIAN_POINT('Ctrl Pts',(127.72658980393,-31.6039610026355,24.5445707114206));
#23159=CARTESIAN_POINT('Ctrl Pts',(127.827684384881,-31.5404812663739,24.5387652901166));
#23160=CARTESIAN_POINT('Ctrl Pts',(127.928890918723,-31.47693123218,24.5329534398458));
#23161=CARTESIAN_POINT('Ctrl Pts',(128.032820024944,-31.4178689400449,24.527141589575));
#23162=CARTESIAN_POINT('Ctrl Pts',(128.139030699115,-31.3635156729112,24.5213297393041));
#23163=CARTESIAN_POINT('Ctrl Pts',(128.245311133026,-31.3091267062598,24.5155140717789));
#23164=CARTESIAN_POINT('Ctrl Pts',(128.353875748818,-31.2594530937282,24.5096984042536));
#23165=CARTESIAN_POINT('Ctrl Pts',(128.46426368474,-31.2146679181355,24.5038827367283));
#23166=CARTESIAN_POINT('Ctrl Pts',(128.574809739461,-31.1698185926148,24.4980587388873));
#23167=CARTESIAN_POINT('Ctrl Pts',(128.687183943758,-31.1298718162454,24.4922347410463));
#23168=CARTESIAN_POINT('Ctrl Pts',(128.800910291907,-31.0949508489719,24.4864107432053));
#23169=CARTESIAN_POINT('Ctrl Pts',(128.831082511994,-31.0856861259998,24.4848656048314));
#23170=CARTESIAN_POINT('Ctrl Pts',(128.861349852103,-31.0767748751189,24.4833204664575));
#23171=CARTESIAN_POINT('Ctrl Pts',(128.891703323487,-31.068218790824,24.4817753280836));
#23172=CARTESIAN_POINT('Ctrl Pts',(129.006109646572,-31.0359697563784,24.4759514933801));
#23173=CARTESIAN_POINT('Ctrl Pts',(129.122109200103,-31.0086663253676,24.4701276586767));
#23174=CARTESIAN_POINT('Ctrl Pts',(129.239236713014,-30.9864648723135,24.4643038239732));
#23175=CARTESIAN_POINT('Ctrl Pts',(129.356215278894,-30.9642916520838,24.4584873952401));
#23176=CARTESIAN_POINT('Ctrl Pts',(129.474318553343,-30.947207580189,24.4526709665069));
#23177=CARTESIAN_POINT('Ctrl Pts',(129.593066386045,-30.9353191965625,24.4468545377738));
#23178=CARTESIAN_POINT('Ctrl Pts',(129.711694163114,-30.9234428322493,24.4410439895272));
#23179=CARTESIAN_POINT('Ctrl Pts',(129.830964797952,-30.9167517461088,24.4352334412805));
#23180=CARTESIAN_POINT('Ctrl Pts',(129.950388826314,-30.9153012679702,24.4294228930339));
#23181=CARTESIAN_POINT('Ctrl Pts',(130.069721285963,-30.9138519019899,24.4236168000416));
#23182=CARTESIAN_POINT('Ctrl Pts',(130.189206498132,-30.9176351517947,24.4178107070493));
#23183=CARTESIAN_POINT('Ctrl Pts',(130.308351393327,-30.9266543949435,24.412004614057));
#23184=CARTESIAN_POINT('Ctrl Pts',(130.427447782068,-30.9356699661641,24.4062008848502));
#23185=CARTESIAN_POINT('Ctrl Pts',(130.546203722889,-30.9499172606221,24.4003971556435));
#23186=CARTESIAN_POINT('Ctrl Pts',(130.664128126284,-30.9693475922776,24.3945934264368));
#23187=CARTESIAN_POINT('Ctrl Pts',(130.782032350306,-30.9887745989902,24.3887906903715));
#23188=CARTESIAN_POINT('Ctrl Pts',(130.899104917337,-31.0133828118102,24.3829879543062));
#23189=CARTESIAN_POINT('Ctrl Pts',(131.014862463637,-31.0430720021839,24.377185218241));
#23190=CARTESIAN_POINT('Ctrl Pts',(131.130627519586,-31.0727631186128,24.3713821057292));
#23191=CARTESIAN_POINT('Ctrl Pts',(131.245076990013,-31.1075357655392,24.3655789932175));
#23192=CARTESIAN_POINT('Ctrl Pts',(131.357740886636,-31.147239342399,24.3597758807058));
#23193=CARTESIAN_POINT('Ctrl Pts',(131.470494548954,-31.1869745533434,24.3539681445262));
#23194=CARTESIAN_POINT('Ctrl Pts',(131.581459410504,-31.2316484049158,24.3481604083467));
#23195=CARTESIAN_POINT('Ctrl Pts',(131.69018367221,-31.2810614210241,24.3423526721671));
#23196=CARTESIAN_POINT('Ctrl Pts',(131.798954822992,-31.3304957472854,24.3365424313085));
#23197=CARTESIAN_POINT('Ctrl Pts',(131.905483084001,-31.3846731267033,24.3307321904498));
#23198=CARTESIAN_POINT('Ctrl Pts',(132.009340932909,-31.4433479203983,24.3249219495912));
#23199=CARTESIAN_POINT('Ctrl Pts',(132.113332546551,-31.5020982848682,24.319104225376));
#23200=CARTESIAN_POINT('Ctrl Pts',(132.214646531498,-31.5653574180558,24.3132865011608));
#23201=CARTESIAN_POINT('Ctrl Pts',(132.312883826761,-31.6328359998496,24.3074687769456));
#23202=CARTESIAN_POINT('Ctrl Pts',(132.372121391485,-31.6735259114135,24.3039606610735));
#23203=CARTESIAN_POINT('Ctrl Pts',(132.43024083144,-31.7157492671488,24.3004525452013));
#23204=CARTESIAN_POINT('Ctrl Pts',(132.487160670875,-31.7594357285724,24.2969444293292));
#23205=CARTESIAN_POINT('Ctrl Pts',(132.487160670875,-31.7594357285724,25.5469383396565));
#23206=CARTESIAN_POINT('Ctrl Pts',(132.581965719039,-31.8321994102783,25.5411336436149));
#23207=CARTESIAN_POINT('Ctrl Pts',(132.67354602429,-31.909104676569,25.5353289475733));
#23208=CARTESIAN_POINT('Ctrl Pts',(132.761532853475,-31.9898237096175,25.5295242515317));
#23209=CARTESIAN_POINT('Ctrl Pts',(132.849614083683,-32.0706293460753,25.5237133276347));
#23210=CARTESIAN_POINT('Ctrl Pts',(132.934093838299,-32.1552566430948,25.5179024037377));
#23211=CARTESIAN_POINT('Ctrl Pts',(133.014639827328,-32.2433404795867,25.5120914798407));
#23212=CARTESIAN_POINT('Ctrl Pts',(133.095233471736,-32.3314764312567,25.5062771178857));
#23213=CARTESIAN_POINT('Ctrl Pts',(133.171888452797,-32.4230726831881,25.5004627559307));
#23214=CARTESIAN_POINT('Ctrl Pts',(133.244313495104,-32.5177318949217,25.4946483939758));
#23215=CARTESIAN_POINT('Ctrl Pts',(133.316848344028,-32.6125346234227,25.4888252166249));
#23216=CARTESIAN_POINT('Ctrl Pts',(133.385140213338,-32.7104092514028,25.483002039274));
#23217=CARTESIAN_POINT('Ctrl Pts',(133.448941585321,-32.8109301196535,25.477178861923));
#23218=CARTESIAN_POINT('Ctrl Pts',(133.485485999684,-32.8685068793262,25.4738434382573));
#23219=CARTESIAN_POINT('Ctrl Pts',(133.520558010519,-32.9269513631098,25.4705080145915));
#23220=CARTESIAN_POINT('Ctrl Pts',(133.554118108444,-32.9861803776824,25.4671725909258));
#23221=CARTESIAN_POINT('Ctrl Pts',(133.612713475523,-33.089593241923,25.4613489972493));
#23222=CARTESIAN_POINT('Ctrl Pts',(133.666886136784,-33.1957323814797,25.4555254035728));
#23223=CARTESIAN_POINT('Ctrl Pts',(133.716373321031,-33.3041832826833,25.4497018098963));
#23224=CARTESIAN_POINT('Ctrl Pts',(133.765798069845,-33.4124973569673,25.4438855635481));
#23225=CARTESIAN_POINT('Ctrl Pts',(133.810548931312,-33.5231170235738,25.4380693172));
#23226=CARTESIAN_POINT('Ctrl Pts',(133.850407969835,-33.6356014270622,25.4322530708519));
#23227=CARTESIAN_POINT('Ctrl Pts',(133.89022710924,-33.7479732330426,25.4264426465984));
#23228=CARTESIAN_POINT('Ctrl Pts',(133.925164031561,-33.862205679837,25.4206322223449));
#23229=CARTESIAN_POINT('Ctrl Pts',(133.955048302462,-33.9778366445668,25.4148217980914));
#23230=CARTESIAN_POINT('Ctrl Pts',(133.986063754792,-34.0978444803334,25.4087914372692));
#23231=CARTESIAN_POINT('Ctrl Pts',(134.011636305304,-34.2193583917457,25.4027610764469));
#23232=CARTESIAN_POINT('Ctrl Pts',(134.031631640618,-34.3418424851396,25.3967307156247));
#23233=CARTESIAN_POINT('Ctrl Pts',(134.05087602995,-34.4597265587583,25.3909268313862));
#23234=CARTESIAN_POINT('Ctrl Pts',(134.064954494204,-34.578508816858,25.3851229471477));
#23235=CARTESIAN_POINT('Ctrl Pts',(134.073799202137,-34.6977003793139,25.3793190629091));
#23236=CARTESIAN_POINT('Ctrl Pts',(134.082642603612,-34.816874335902,25.3735160359664));
#23237=CARTESIAN_POINT('Ctrl Pts',(134.086253755971,-34.9364570695058,25.3677130090236));
#23238=CARTESIAN_POINT('Ctrl Pts',(134.084616753787,-35.0559551131028,25.3619099820808));
#23239=CARTESIAN_POINT('Ctrl Pts',(134.082979607073,-35.1754637071277,25.3561064427914));
#23240=CARTESIAN_POINT('Ctrl Pts',(134.076093390145,-35.2948871879604,25.350302903502));
#23241=CARTESIAN_POINT('Ctrl Pts',(134.063994313666,-35.4137332697378,25.3444993642127));
#23242=CARTESIAN_POINT('Ctrl Pts',(134.051891313598,-35.5326178919144,25.3386939429031));
#23243=CARTESIAN_POINT('Ctrl Pts',(134.034572133353,-35.6509243366218,25.3328885215936));
#23244=CARTESIAN_POINT('Ctrl Pts',(134.012124633458,-35.7681672510609,25.327083100284));
#23245=CARTESIAN_POINT('Ctrl Pts',(133.989652275034,-35.8855400011756,25.3212712500078));
#23246=CARTESIAN_POINT('Ctrl Pts',(133.962040337742,-36.0018464688193,25.3154593997315));
#23247=CARTESIAN_POINT('Ctrl Pts',(133.929427456171,-36.1166131231056,25.3096475494552));
#23248=CARTESIAN_POINT('Ctrl Pts',(133.896793154284,-36.2314551567464,25.3038318819244));
#23249=CARTESIAN_POINT('Ctrl Pts',(133.859151495107,-36.3447549762657,25.2980162143937));
#23250=CARTESIAN_POINT('Ctrl Pts',(133.816689918593,-36.4560573701981,25.292200546863));
#23251=CARTESIAN_POINT('Ctrl Pts',(133.774167520457,-36.5675191927906,25.2863765490165));
#23252=CARTESIAN_POINT('Ctrl Pts',(133.726811586517,-36.6769775057666,25.28055255117));
#23253=CARTESIAN_POINT('Ctrl Pts',(133.674856337231,-36.7839999721731,25.2747285533236));
#23254=CARTESIAN_POINT('Ctrl Pts',(133.661072326862,-36.8123936149122,25.2731834150015));
#23255=CARTESIAN_POINT('Ctrl Pts',(133.646964825407,-36.8406159572215,25.2716382766794));
#23256=CARTESIAN_POINT('Ctrl Pts',(133.632538719108,-36.8686592664739,25.2700931383574));
#23257=CARTESIAN_POINT('Ctrl Pts',(133.578167029443,-36.9743539061957,25.2642695446866));
#23258=CARTESIAN_POINT('Ctrl Pts',(133.519090795536,-37.0778439672222,25.2584459510158));
#23259=CARTESIAN_POINT('Ctrl Pts',(133.455512663061,-37.1786824540134,25.252622357345));
#23260=CARTESIAN_POINT('Ctrl Pts',(133.392014743844,-37.2793937180753,25.2468061110026));
#23261=CARTESIAN_POINT('Ctrl Pts',(133.324026438936,-37.3774597193653,25.2409898646602));
#23262=CARTESIAN_POINT('Ctrl Pts',(133.251797002751,-37.4724565219435,25.2351736183179));
#23263=CARTESIAN_POINT('Ctrl Pts',(133.17963986863,-37.567358232198,25.2293631940702));
#23264=CARTESIAN_POINT('Ctrl Pts',(133.103250294646,-37.6591965324894,25.2235527698225));
#23265=CARTESIAN_POINT('Ctrl Pts',(133.022921361146,-37.7475755575285,25.2177423455749));
#23266=CARTESIAN_POINT('Ctrl Pts',(132.939551811351,-37.8392999114788,25.2117119847504));
#23267=CARTESIAN_POINT('Ctrl Pts',(132.851939022809,-37.927297555214,25.205681623926));
#23268=CARTESIAN_POINT('Ctrl Pts',(132.760457575815,-38.0111623955089,25.1996512631016));
#23269=CARTESIAN_POINT('Ctrl Pts',(132.672411811516,-38.0918776028455,25.193847378869));
#23270=CARTESIAN_POINT('Ctrl Pts',(132.58078305967,-38.1687645315343,25.1880434946364));
#23271=CARTESIAN_POINT('Ctrl Pts',(132.485943022891,-38.2414984632021,25.1822396104038));
#23272=CARTESIAN_POINT('Ctrl Pts',(132.391116994998,-38.3142216512904,25.176436583467));
#23273=CARTESIAN_POINT('Ctrl Pts',(132.293080949419,-38.3827928138722,25.1706335565301));
#23274=CARTESIAN_POINT('Ctrl Pts',(132.192238888955,-38.4469281474602,25.1648305295933));
#23275=CARTESIAN_POINT('Ctrl Pts',(132.091387925192,-38.5110691435275,25.1590269903099));
#23276=CARTESIAN_POINT('Ctrl Pts',(131.987730798546,-38.5707733127841,25.1532234510265));
#23277=CARTESIAN_POINT('Ctrl Pts',(131.881699092075,-38.6258010876057,25.147419911743));
#23278=CARTESIAN_POINT('Ctrl Pts',(131.775633000759,-38.6808467072931,25.1416144904395));
#23279=CARTESIAN_POINT('Ctrl Pts',(131.667191160414,-38.7312127285709,25.1358090691359));
#23280=CARTESIAN_POINT('Ctrl Pts',(131.556827668056,-38.7767065827219,25.1300036478324));
#23281=CARTESIAN_POINT('Ctrl Pts',(131.446341958346,-38.8222508171055,25.1241917975621));
#23282=CARTESIAN_POINT('Ctrl Pts',(131.333930726594,-38.8629119588209,25.1183799472918));
#23283=CARTESIAN_POINT('Ctrl Pts',(131.2200660148,-38.898546385453,25.1125680970215));
#23284=CARTESIAN_POINT('Ctrl Pts',(131.106126516053,-38.9342042169678,25.1067524294967));
#23285=CARTESIAN_POINT('Ctrl Pts',(130.990732029815,-38.9648286537308,25.1009367619719));
#23286=CARTESIAN_POINT('Ctrl Pts',(130.874366029577,-38.9903269347664,25.0951210944472));
#23287=CARTESIAN_POINT('Ctrl Pts',(130.757833347608,-39.0158617393362,25.0892970966067));
#23288=CARTESIAN_POINT('Ctrl Pts',(130.640326774998,-39.0362556630418,25.0834730987662));
#23289=CARTESIAN_POINT('Ctrl Pts',(130.522336297021,-39.0514676097452,25.0776491009256));
#23290=CARTESIAN_POINT('Ctrl Pts',(130.491032779942,-39.0555034221396,25.0761039625467));
#23291=CARTESIAN_POINT('Ctrl Pts',(130.459695207567,-39.0591747752407,25.0745588241678));
#23292=CARTESIAN_POINT('Ctrl Pts',(130.428332725701,-39.0624815170156,25.0730136857889));
#23293=CARTESIAN_POINT('Ctrl Pts',(130.310128198923,-39.0749445564,25.0671900921183));
#23294=CARTESIAN_POINT('Ctrl Pts',(130.191188658355,-39.0822643809855,25.0613664984476));
#23295=CARTESIAN_POINT('Ctrl Pts',(130.071999041145,-39.084365451092,25.055542904777));
#23296=CARTESIAN_POINT('Ctrl Pts',(129.952959799342,-39.0864638703865,25.0497266584348));
#23297=CARTESIAN_POINT('Ctrl Pts',(129.833671513113,-39.0833566239554,25.0439104120926));
#23298=CARTESIAN_POINT('Ctrl Pts',(129.714625382435,-39.0750197947556,25.0380941657504));
#23299=CARTESIAN_POINT('Ctrl Pts',(129.59569841759,-39.0666913107677,25.0322837415029));
#23300=CARTESIAN_POINT('Ctrl Pts',(129.477013531071,-39.0531436864415,25.0264733172554));
#23301=CARTESIAN_POINT('Ctrl Pts',(129.359062469155,-39.0344050467887,25.0206628930078));
#23302=CARTESIAN_POINT('Ctrl Pts',(129.236646715557,-39.0149571108631,25.0146325321834));
#23303=CARTESIAN_POINT('Ctrl Pts',(129.115021885921,-38.9899174056844,25.0086021713589));
#23304=CARTESIAN_POINT('Ctrl Pts',(128.994732956178,-38.9593766138883,25.0025718105344));
#23305=CARTESIAN_POINT('Ctrl Pts',(128.878961604681,-38.9299828138971,24.9967679263021));
#23306=CARTESIAN_POINT('Ctrl Pts',(128.764428051713,-38.8954937835913,24.9909640420697));
#23307=CARTESIAN_POINT('Ctrl Pts',(128.651607636185,-38.8560424055248,24.9851601578373));
#23308=CARTESIAN_POINT('Ctrl Pts',(128.538803885439,-38.8165968548488,24.9793571309008));
#23309=CARTESIAN_POINT('Ctrl Pts',(128.427713154244,-38.7721905488504,24.9735541039642));
#23310=CARTESIAN_POINT('Ctrl Pts',(128.318794267271,-38.7230058130816,24.9677510770276));
#23311=CARTESIAN_POINT('Ctrl Pts',(128.209865763899,-38.673816734815,24.9619475377444));
#23312=CARTESIAN_POINT('Ctrl Pts',(128.103109858166,-38.6198485560297,24.9561439984613));
#23313=CARTESIAN_POINT('Ctrl Pts',(127.998963495633,-38.5613309180965,24.9503404591781));
#23314=CARTESIAN_POINT('Ctrl Pts',(127.894783359649,-38.5027943035756,24.9445350378748));
#23315=CARTESIAN_POINT('Ctrl Pts',(127.793214805662,-38.4397054957163,24.9387296165715));
#23316=CARTESIAN_POINT('Ctrl Pts',(127.694667812035,-38.3723387290031,24.9329241952682));
#23317=CARTESIAN_POINT('Ctrl Pts',(127.596011686735,-38.3048973598316,24.9271123449982));
#23318=CARTESIAN_POINT('Ctrl Pts',(127.500384138194,-38.2331688060413,24.9213004947282));
#23319=CARTESIAN_POINT('Ctrl Pts',(127.408164044286,-38.1574691413643,24.9154886444582));
#23320=CARTESIAN_POINT('Ctrl Pts',(127.315883379725,-38.0817197567409,24.9096729769337));
#23321=CARTESIAN_POINT('Ctrl Pts',(127.227014930152,-38.001994338893,24.9038573094093));
#23322=CARTESIAN_POINT('Ctrl Pts',(127.141901300726,-37.9186464029085,24.8980416418848));
#23323=CARTESIAN_POINT('Ctrl Pts',(127.056665755218,-37.8351790800058,24.8922176440446));
#23324=CARTESIAN_POINT('Ctrl Pts',(126.975196042748,-37.7480791794289,24.8863936462043));
#23325=CARTESIAN_POINT('Ctrl Pts',(126.897795127024,-37.6577339833181,24.8805696483641));
#23326=CARTESIAN_POINT('Ctrl Pts',(126.877260242069,-37.6337649102004,24.8790245099829));
#23327=CARTESIAN_POINT('Ctrl Pts',(126.857011512478,-37.6095675709048,24.8774793716017));
#23328=CARTESIAN_POINT('Ctrl Pts',(126.837054078806,-37.5851495313814,24.8759342332205));
#23329=CARTESIAN_POINT('Ctrl Pts',(126.762195742137,-37.4935599085143,24.8701385737665));
#23330=CARTESIAN_POINT('Ctrl Pts',(126.691190191979,-37.3985584741059,24.8643429143124));
#23331=CARTESIAN_POINT('Ctrl Pts',(126.624365980108,-37.3005042846615,24.8585472548584));
#23332=CARTESIAN_POINT('Ctrl Pts',(126.557622092833,-37.2025679591328,24.8527585619513));
#23333=CARTESIAN_POINT('Ctrl Pts',(126.495049783104,-37.1015865096678,24.8469698690443));
#23334=CARTESIAN_POINT('Ctrl Pts',(126.436938220602,-36.9979528913849,24.8411811761372));
#23335=CARTESIAN_POINT('Ctrl Pts',(126.378882465277,-36.8944187971804,24.8353980423753));
#23336=CARTESIAN_POINT('Ctrl Pts',(126.325279140324,-36.7882379553403,24.8296149086134));
#23337=CARTESIAN_POINT('Ctrl Pts',(126.27637444219,-36.6798326420283,24.8238317748515));
#23338=CARTESIAN_POINT('Ctrl Pts',(126.22750489271,-36.5715052414952,24.8180527975282));
#23339=CARTESIAN_POINT('Ctrl Pts',(126.183327422775,-36.4609569235521,24.8122738202048));
#23340=CARTESIAN_POINT('Ctrl Pts',(126.144042212232,-36.3486343236595,24.8064948428815));
#23341=CARTESIAN_POINT('Ctrl Pts',(126.104770622542,-36.2363506679293,24.8007178692282));
#23342=CARTESIAN_POINT('Ctrl Pts',(126.070388060113,-36.1222943403461,24.7949408955749));
#23343=CARTESIAN_POINT('Ctrl Pts',(126.041046289914,-36.006931239657,24.7891639219216));
#23344=CARTESIAN_POINT('Ctrl Pts',(126.011711368871,-35.8915950678071,24.7833882967688));
#23345=CARTESIAN_POINT('Ctrl Pts',(125.98741499763,-35.7749531300053,24.777612671616));
#23346=CARTESIAN_POINT('Ctrl Pts',(125.968258611742,-35.6574848881995,24.7718370464631));
#23347=CARTESIAN_POINT('Ctrl Pts',(125.949095050159,-35.5399726445438,24.7660592578473));
#23348=CARTESIAN_POINT('Ctrl Pts',(125.93507538937,-35.4216338854961,24.7602814692315));
#23349=CARTESIAN_POINT('Ctrl Pts',(125.926249593192,-35.302956470529,24.7545036806157));
#23350=CARTESIAN_POINT('Ctrl Pts',(125.918668595408,-35.2010174270874,24.749540796609));
#23351=CARTESIAN_POINT('Ctrl Pts',(125.914918852587,-35.0988287956417,24.7445779126023));
#23352=CARTESIAN_POINT('Ctrl Pts',(125.91500133219,-34.9967009101661,24.7396150285955));
#23353=CARTESIAN_POINT('Origin',(130.,-35.,32.7603849714045));
#23354=CARTESIAN_POINT('',(132.487160670875,-31.7594357285724,26.7967734504842));
#23355=CARTESIAN_POINT('',(132.487160670875,-31.7594357285724,26.6927660718219));
#23356=CARTESIAN_POINT('',(132.487160670875,-31.7594357285724,32.7603849714045));
#23357=CARTESIAN_POINT('',(125.91500046357,-34.998053885216,25.8853849714464));
#23358=CARTESIAN_POINT('Ctrl Pts',(132.487160670875,-31.7594357285724,26.6927660718219));
#23359=CARTESIAN_POINT('Ctrl Pts',(132.584486290898,-31.8341339706419,26.6867872558272));
#23360=CARTESIAN_POINT('Ctrl Pts',(132.678341578341,-31.9131420984798,26.6808084398325));
#23361=CARTESIAN_POINT('Ctrl Pts',(132.768344329939,-31.9960867737405,26.6748296238378));
#23362=CARTESIAN_POINT('Ctrl Pts',(132.858347081536,-32.0790314490012,26.6688508078431));
#23363=CARTESIAN_POINT('Ctrl Pts',(132.944497017134,-32.1659122971067,26.6628719918484));
#23364=CARTESIAN_POINT('Ctrl Pts',(133.026456729518,-32.2563191394852,26.6568931758537));
#23365=CARTESIAN_POINT('Ctrl Pts',(133.106288598545,-32.3443788335715,26.6510695822667));
#23366=CARTESIAN_POINT('Ctrl Pts',(133.182402651789,-32.4360676801457,26.6452459886798));
#23367=CARTESIAN_POINT('Ctrl Pts',(133.254451673081,-32.5310388201556,26.6394223950928));
#23368=CARTESIAN_POINT('Ctrl Pts',(133.326409793813,-32.6258901399413,26.6336061488357));
#23369=CARTESIAN_POINT('Ctrl Pts',(133.394312838722,-32.7240151941611,26.6277899025786));
#23370=CARTESIAN_POINT('Ctrl Pts',(133.457851565361,-32.8250315974873,26.6219736563214));
#23371=CARTESIAN_POINT('Ctrl Pts',(133.521326689369,-32.9259468828127,26.6161632321602));
#23372=CARTESIAN_POINT('Ctrl Pts',(133.58044596995,-33.0297474158179,26.6103528079991));
#23373=CARTESIAN_POINT('Ctrl Pts',(133.634941851182,-33.1360196517866,26.6045423838379));
#23374=CARTESIAN_POINT('Ctrl Pts',(133.691500515386,-33.2463145139389,26.5985120229815));
#23375=CARTESIAN_POINT('Ctrl Pts',(133.743078583024,-33.3592715373707,26.5924816621252));
#23376=CARTESIAN_POINT('Ctrl Pts',(133.789427576039,-33.4743972843641,26.5864513012688));
#23377=CARTESIAN_POINT('Ctrl Pts',(133.834035882578,-33.5851993596284,26.5806474171254));
#23378=CARTESIAN_POINT('Ctrl Pts',(133.873800632321,-33.6980097857414,26.5748435329819));
#23379=CARTESIAN_POINT('Ctrl Pts',(133.908548515549,-33.8123664278925,26.5690396488385));
#23380=CARTESIAN_POINT('Ctrl Pts',(133.943291266139,-33.9267061783283,26.5632366219916));
#23381=CARTESIAN_POINT('Ctrl Pts',(133.973018505237,-34.0425913000075,26.5574335951448));
#23382=CARTESIAN_POINT('Ctrl Pts',(133.997606581839,-34.159543804331,26.5516305682979));
#23383=CARTESIAN_POINT('Ctrl Pts',(134.022196829308,-34.2765066343234,26.5458270291052));
#23384=CARTESIAN_POINT('Ctrl Pts',(134.041646928132,-34.3945366347084,26.5400234899125));
#23385=CARTESIAN_POINT('Ctrl Pts',(134.055884335606,-34.5131455492763,26.5342199507197));
#23386=CARTESIAN_POINT('Ctrl Pts',(134.070126360103,-34.6317929273198,26.5284145295075));
#23387=CARTESIAN_POINT('Ctrl Pts',(134.079152282757,-34.7510191876909,26.5226091082953));
#23388=CARTESIAN_POINT('Ctrl Pts',(134.082941474662,-34.8703315208451,26.5168036870831));
#23389=CARTESIAN_POINT('Ctrl Pts',(134.086734862746,-34.9897759813572,26.5109918369046));
#23390=CARTESIAN_POINT('Ctrl Pts',(134.085279931424,-35.1093062965414,26.5051799867261));
#23391=CARTESIAN_POINT('Ctrl Pts',(134.078608182357,-35.2284300654614,26.4993681365476));
#23392=CARTESIAN_POINT('Ctrl Pts',(134.071932051251,-35.3476320755059,26.493552469115));
#23393=CARTESIAN_POINT('Ctrl Pts',(134.060032319177,-35.4664266021361,26.4877368016825));
#23394=CARTESIAN_POINT('Ctrl Pts',(134.042992121299,-35.5843284240144,26.4819211342499));
#23395=CARTESIAN_POINT('Ctrl Pts',(134.025927515177,-35.7023991275269,26.4760971365014));
#23396=CARTESIAN_POINT('Ctrl Pts',(134.003707822585,-35.8195741743018,26.470273138753));
#23397=CARTESIAN_POINT('Ctrl Pts',(133.976466834679,-35.9353804106881,26.4644491410045));
#23398=CARTESIAN_POINT('Ctrl Pts',(133.969239647932,-35.9661044541676,26.4629040017647));
#23399=CARTESIAN_POINT('Ctrl Pts',(133.961659295106,-35.9967322461004,26.461358862525));
#23400=CARTESIAN_POINT('Ctrl Pts',(133.953728849266,-36.0272551710664,26.4598137232852));
#23401=CARTESIAN_POINT('Ctrl Pts',(133.923839184084,-36.1422953624942,26.4539901295726));
#23402=CARTESIAN_POINT('Ctrl Pts',(133.888876229056,-36.2562154491357,26.4481665358599));
#23403=CARTESIAN_POINT('Ctrl Pts',(133.848939755854,-36.3685348938938,26.4423429421472));
#23404=CARTESIAN_POINT('Ctrl Pts',(133.809053668442,-36.4807126309992,26.4365266957625));
#23405=CARTESIAN_POINT('Ctrl Pts',(133.764206678942,-36.5912933615056,26.4307104493778));
#23406=CARTESIAN_POINT('Ctrl Pts',(133.714549087987,-36.6998088342318,26.4248942029931));
#23407=CARTESIAN_POINT('Ctrl Pts',(133.664941204552,-36.8082156823799,26.4190837787026));
#23408=CARTESIAN_POINT('Ctrl Pts',(133.610532468316,-36.9145610162808,26.4132733544121));
#23409=CARTESIAN_POINT('Ctrl Pts',(133.551522091763,-37.0183943697208,26.4074629301217));
#23410=CARTESIAN_POINT('Ctrl Pts',(133.490278051005,-37.1261580292921,26.4014325693131));
#23411=CARTESIAN_POINT('Ctrl Pts',(133.424077273874,-37.2312153614181,26.3954022085046));
#23412=CARTESIAN_POINT('Ctrl Pts',(133.353196250816,-37.3330880616707,26.389371847696));
#23413=CARTESIAN_POINT('Ctrl Pts',(133.284977239009,-37.4311348256938,26.3835679634199));
#23414=CARTESIAN_POINT('Ctrl Pts',(133.212423438938,-37.5262314831677,26.3777640791437));
#23415=CARTESIAN_POINT('Ctrl Pts',(133.135826364774,-37.6179797573683,26.3719601948675));
#23416=CARTESIAN_POINT('Ctrl Pts',(133.059240604813,-37.7097144793713,26.3661571678869));
#23417=CARTESIAN_POINT('Ctrl Pts',(132.978613020091,-37.7981014883151,26.3603541409062));
#23418=CARTESIAN_POINT('Ctrl Pts',(132.894275605525,-37.8827753501207,26.3545511139256));
#23419=CARTESIAN_POINT('Ctrl Pts',(132.809930744844,-37.9674566877454,26.3487475745982));
#23420=CARTESIAN_POINT('Ctrl Pts',(132.721875691268,-38.0484239370961,26.3429440352708));
#23421=CARTESIAN_POINT('Ctrl Pts',(132.630479042952,-38.1253487812709,26.3371404959433));
#23422=CARTESIAN_POINT('Ctrl Pts',(132.539052755767,-38.2022985712772,26.3313350745957));
#23423=CARTESIAN_POINT('Ctrl Pts',(132.444283030975,-38.275203086206,26.325529653248));
#23424=CARTESIAN_POINT('Ctrl Pts',(132.346570732266,-38.3437749323889,26.3197242319004));
#23425=CARTESIAN_POINT('Ctrl Pts',(132.248750226231,-38.4124227155436,26.313912381586));
#23426=CARTESIAN_POINT('Ctrl Pts',(132.14798097622,-38.476728017972,26.3081005312716));
#23427=CARTESIAN_POINT('Ctrl Pts',(132.044692080248,-38.5364472704922,26.3022886809572));
#23428=CARTESIAN_POINT('Ctrl Pts',(131.941335343575,-38.5962057469382,26.2964730133883));
#23429=CARTESIAN_POINT('Ctrl Pts',(131.835456026431,-38.6513719864717,26.2906573458195));
#23430=CARTESIAN_POINT('Ctrl Pts',(131.727505525628,-38.7017495402748,26.2848416782506));
#23431=CARTESIAN_POINT('Ctrl Pts',(131.619400397396,-38.7521992544809,26.2790176803662));
#23432=CARTESIAN_POINT('Ctrl Pts',(131.509218539945,-38.7978464364833,26.2731936824819));
#23433=CARTESIAN_POINT('Ctrl Pts',(131.397429024793,-38.8385436197425,26.2673696845975));
#23434=CARTESIAN_POINT('Ctrl Pts',(131.367770665218,-38.8493408013311,26.2658245466373));
#23435=CARTESIAN_POINT('Ctrl Pts',(131.33799921507,-38.8597898439868,26.264279408677));
#23436=CARTESIAN_POINT('Ctrl Pts',(131.308123564557,-38.8698885952765,26.2627342707168));
#23437=CARTESIAN_POINT('Ctrl Pts',(131.195522843021,-38.9079505842978,26.2569106770474));
#23438=CARTESIAN_POINT('Ctrl Pts',(131.081077952104,-38.9411554195207,26.251087083378));
#23439=CARTESIAN_POINT('Ctrl Pts',(130.965245490355,-38.9693231341563,26.2452634897087));
#23440=CARTESIAN_POINT('Ctrl Pts',(130.849559168462,-38.9974553110362,26.2394472433676));
#23441=CARTESIAN_POINT('Ctrl Pts',(130.732489150969,-39.0205629117897,26.2336309970266));
#23442=CARTESIAN_POINT('Ctrl Pts',(130.61450945898,-39.0385149652842,26.2278147506856));
#23443=CARTESIAN_POINT('Ctrl Pts',(130.496647865311,-39.0564490486743,26.2220043264392));
#23444=CARTESIAN_POINT('Ctrl Pts',(130.37787881002,-39.0692377903677,26.2161939021928));
#23445=CARTESIAN_POINT('Ctrl Pts',(130.258688251069,-39.0768008767609,26.2103834779464));
#23446=CARTESIAN_POINT('Ctrl Pts',(130.134986082877,-39.0846502416209,26.2043531171215));
#23447=CARTESIAN_POINT('Ctrl Pts',(130.010830306499,-39.0868704250375,26.1983227562966));
#23448=CARTESIAN_POINT('Ctrl Pts',(129.886772523961,-39.0834304865725,26.1922923954717));
#23449=CARTESIAN_POINT('Ctrl Pts',(129.767373862958,-39.0801197386432,26.1864885112402));
#23450=CARTESIAN_POINT('Ctrl Pts',(129.648066412888,-39.0715663580064,26.1806846270087));
#23451=CARTESIAN_POINT('Ctrl Pts',(129.529343078356,-39.0577958379037,26.1748807427773));
#23452=CARTESIAN_POINT('Ctrl Pts',(129.410637280528,-39.0440273518539,26.1690777158415));
#23453=CARTESIAN_POINT('Ctrl Pts',(129.292515832161,-39.0250433059067,26.1632746889057));
#23454=CARTESIAN_POINT('Ctrl Pts',(129.175466359289,-39.0009210533746,26.1574716619699));
#23455=CARTESIAN_POINT('Ctrl Pts',(129.058406552172,-38.9767966710997,26.1516681226875));
#23456=CARTESIAN_POINT('Ctrl Pts',(128.942419308677,-38.9475332626986,26.145864583405));
#23457=CARTESIAN_POINT('Ctrl Pts',(128.827981275665,-38.913259141663,26.1400610441226));
#23458=CARTESIAN_POINT('Ctrl Pts',(128.713506131733,-38.8789739059292,26.13425562282));
#23459=CARTESIAN_POINT('Ctrl Pts',(128.600581588395,-38.839674843065,26.1284502015173));
#23460=CARTESIAN_POINT('Ctrl Pts',(128.489667752291,-38.7955396851478,26.1226447802147));
#23461=CARTESIAN_POINT('Ctrl Pts',(128.378631089378,-38.7513556516274,26.1168329299452));
#23462=CARTESIAN_POINT('Ctrl Pts',(128.269609957953,-38.7023249840245,26.1110210796757));
#23463=CARTESIAN_POINT('Ctrl Pts',(128.163043288153,-38.6486730517819,26.1052092294062));
#23464=CARTESIAN_POINT('Ctrl Pts',(128.05640662479,-38.5949858806616,26.0993935618822));
#23465=CARTESIAN_POINT('Ctrl Pts',(127.952227989091,-38.5366715990711,26.0935778943582));
#23466=CARTESIAN_POINT('Ctrl Pts',(127.850919124464,-38.4740000561894,26.0877622268341));
#23467=CARTESIAN_POINT('Ctrl Pts',(127.749465145825,-38.4112387430886,26.0819382289943));
#23468=CARTESIAN_POINT('Ctrl Pts',(127.650889479176,-38.3441079404169,26.0761142311544));
#23469=CARTESIAN_POINT('Ctrl Pts',(127.555572589189,-38.2729191302681,26.0702902333145));
#23470=CARTESIAN_POINT('Ctrl Pts',(127.530284498455,-38.2540323506999,26.0687450949258));
#23471=CARTESIAN_POINT('Ctrl Pts',(127.505225589072,-38.2348601481981,26.0671999565371));
#23472=CARTESIAN_POINT('Ctrl Pts',(127.480402534567,-38.2154087783959,26.0656548181484));
#23473=CARTESIAN_POINT('Ctrl Pts',(127.387890871815,-38.1429165489286,26.0598963277298));
#23474=CARTESIAN_POINT('Ctrl Pts',(127.298344601786,-38.0662984777782,26.0541378373113));
#23475=CARTESIAN_POINT('Ctrl Pts',(127.212159759073,-37.9858284932445,26.0483793468928));
#23476=CARTESIAN_POINT('Ctrl Pts',(127.126084184856,-37.9054605316861,26.0426281573123));
#23477=CARTESIAN_POINT('Ctrl Pts',(127.043361868387,-37.8212506484488,26.0368769677319));
#23478=CARTESIAN_POINT('Ctrl Pts',(126.964357841702,-37.7335145301908,26.0311257781514));
#23479=CARTESIAN_POINT('Ctrl Pts',(126.88543220804,-37.6458654695144,26.0253802952818));
#23480=CARTESIAN_POINT('Ctrl Pts',(126.810217805869,-37.5546974406822,26.0196348124122));
#23481=CARTESIAN_POINT('Ctrl Pts',(126.73904413004,-37.460364162919,26.0138893295426));
#23482=CARTESIAN_POINT('Ctrl Pts',(126.667920512358,-37.3660972320024,26.0081478876082));
#23483=CARTESIAN_POINT('Ctrl Pts',(126.60083221996,-37.2686698127851,26.0024064456739));
#23484=CARTESIAN_POINT('Ctrl Pts',(126.538069144986,-37.1684694498891,25.9966650037395));
#23485=CARTESIAN_POINT('Ctrl Pts',(126.475328663353,-37.0683051569421,25.9909256285992));
#23486=CARTESIAN_POINT('Ctrl Pts',(126.416910526328,-36.9653702585504,25.985186253459));
#23487=CARTESIAN_POINT('Ctrl Pts',(126.363061503257,-36.8600815495317,25.9794468783187));
#23488=CARTESIAN_POINT('Ctrl Pts',(126.309218443453,-36.7548045002363,25.9737081387597));
#23489=CARTESIAN_POINT('Ctrl Pts',(126.259943681615,-36.6471745313558,25.9679693992006));
#23490=CARTESIAN_POINT('Ctrl Pts',(126.215437817401,-36.537632623887,25.9622306596416));
#23491=CARTESIAN_POINT('Ctrl Pts',(126.170925788961,-36.4280755444595,25.9564911252459));
#23492=CARTESIAN_POINT('Ctrl Pts',(126.13118412738,-36.3166063882113,25.9507515908502));
#23493=CARTESIAN_POINT('Ctrl Pts',(126.096364826132,-36.2036849377379,25.9450120564546));
#23494=CARTESIAN_POINT('Ctrl Pts',(126.061513761251,-36.0906604755645,25.939267286214));
#23495=CARTESIAN_POINT('Ctrl Pts',(126.031594144116,-35.9761814747901,25.9335225159735));
#23496=CARTESIAN_POINT('Ctrl Pts',(126.006707715966,-35.860721635765,25.927777745733));
#23497=CARTESIAN_POINT('Ctrl Pts',(125.981808406243,-35.7452020330715,25.922030001917));
#23498=CARTESIAN_POINT('Ctrl Pts',(125.961947542635,-35.6287009933682,25.916282258101));
#23499=CARTESIAN_POINT('Ctrl Pts',(125.947175220414,-35.5116994293291,25.910534514285));
#23500=CARTESIAN_POINT('Ctrl Pts',(125.932382690922,-35.3945378171746,25.904778908048));
#23501=CARTESIAN_POINT('Ctrl Pts',(125.922692631631,-35.2768747301239,25.8990233018109));
#23502=CARTESIAN_POINT('Ctrl Pts',(125.918103075061,-35.159193260448,25.8932676955738));
#23503=CARTESIAN_POINT('Ctrl Pts',(125.916007830481,-35.1054687975995,25.8906401208647));
#23504=CARTESIAN_POINT('Ctrl Pts',(125.914974887006,-35.0517404675829,25.8880125461556));
#23505=CARTESIAN_POINT('Ctrl Pts',(125.91500046357,-34.998053885216,25.8853849714464));
#23506=CARTESIAN_POINT('Ctrl Pts',(125.91500046357,-34.9980538843595,25.8853849714045));
#23507=CARTESIAN_POINT('Ctrl Pts',(125.915055004632,-34.8835693136621,25.879781769463));
#23508=CARTESIAN_POINT('Ctrl Pts',(125.919921914211,-34.7692049072162,25.8741785675215));
#23509=CARTESIAN_POINT('Ctrl Pts',(125.92957331797,-34.6552513579166,25.8685753655799));
#23510=CARTESIAN_POINT('Ctrl Pts',(125.939604342104,-34.536815653468,25.8627517719035));
#23511=CARTESIAN_POINT('Ctrl Pts',(125.954824952508,-34.4186271295216,25.856928178227));
#23512=CARTESIAN_POINT('Ctrl Pts',(125.975217969216,-34.3011762706659,25.8511045845505));
#23513=CARTESIAN_POINT('Ctrl Pts',(125.995585257105,-34.183873593513,25.8452883382024));
#23514=CARTESIAN_POINT('Ctrl Pts',(126.021111902477,-34.0673071291332,25.8394720918543));
#23515=CARTESIAN_POINT('Ctrl Pts',(126.051728847284,-33.9519637865835,25.8336558455062));
#23516=CARTESIAN_POINT('Ctrl Pts',(126.082315144362,-33.8367359033547,25.8278454212527));
#23517=CARTESIAN_POINT('Ctrl Pts',(126.117981500013,-33.7227290986611,25.8220349969993));
#23518=CARTESIAN_POINT('Ctrl Pts',(126.158607643251,-33.6104210128559,25.8162245727458));
#23519=CARTESIAN_POINT('Ctrl Pts',(126.20077156999,-33.4938618338497,25.8101942119235));
#23520=CARTESIAN_POINT('Ctrl Pts',(126.248278102886,-33.3791329563222,25.8041638511013));
#23521=CARTESIAN_POINT('Ctrl Pts',(126.300935504727,-33.2667525105132,25.798133490279));
#23522=CARTESIAN_POINT('Ctrl Pts',(126.351615302105,-33.1585926313008,25.7923296060405));
#23523=CARTESIAN_POINT('Ctrl Pts',(126.407065864033,-33.0526083722017,25.786525721802));
#23524=CARTESIAN_POINT('Ctrl Pts',(126.467067129435,-32.9492415227334,25.7807218375636));
#23525=CARTESIAN_POINT('Ctrl Pts',(126.527059532009,-32.8458899416535,25.7749188106208));
#23526=CARTESIAN_POINT('Ctrl Pts',(126.591601096351,-32.7451553543973,25.7691157836781));
#23527=CARTESIAN_POINT('Ctrl Pts',(126.660426315324,-32.6474540164702,25.7633127567353));
#23528=CARTESIAN_POINT('Ctrl Pts',(126.729257610845,-32.5497440525362,25.757509217446));
#23529=CARTESIAN_POINT('Ctrl Pts',(126.802373077782,-32.4550682042312,25.7517056781566));
#23530=CARTESIAN_POINT('Ctrl Pts',(126.879464862814,-32.3638123250448,25.7459021388673));
#23531=CARTESIAN_POINT('Ctrl Pts',(126.956581647812,-32.2725268526405,25.7400967175577));
#23532=CARTESIAN_POINT('Ctrl Pts',(127.037677051999,-32.1846638667855,25.7342912962482));
#23533=CARTESIAN_POINT('Ctrl Pts',(127.122404508452,-32.1005743349722,25.7284858749387));
#23534=CARTESIAN_POINT('Ctrl Pts',(127.20722579272,-32.0163916817859,25.7226740246625));
#23535=CARTESIAN_POINT('Ctrl Pts',(127.295686867836,-31.9359911116015,25.7168621743862));
#23536=CARTESIAN_POINT('Ctrl Pts',(127.387405936575,-31.8596851655038,25.71105032411));
#23537=CARTESIAN_POINT('Ctrl Pts',(127.479185246891,-31.783329101251,25.7052346565793));
#23538=CARTESIAN_POINT('Ctrl Pts',(127.574226488116,-31.7110732635981,25.6994189890486));
#23539=CARTESIAN_POINT('Ctrl Pts',(127.67211792635,-31.6431875162321,25.6936033215179));
#23540=CARTESIAN_POINT('Ctrl Pts',(127.770149583498,-31.5752045298638,25.6877793236714));
#23541=CARTESIAN_POINT('Ctrl Pts',(127.871039242098,-31.5116043447514,25.681955325825));
#23542=CARTESIAN_POINT('Ctrl Pts',(127.974349474773,-31.4526115310488,25.6761313279786));
#23543=CARTESIAN_POINT('Ctrl Pts',(128.001758241707,-31.4369604165395,25.6745861896562));
#23544=CARTESIAN_POINT('Ctrl Pts',(128.029337272293,-31.4216333400051,25.6730410513338));
#23545=CARTESIAN_POINT('Ctrl Pts',(128.057078167553,-31.406633924438,25.6714959130115));
#23546=CARTESIAN_POINT('Ctrl Pts',(128.161633015309,-31.3501014442725,25.6656723193407));
#23547=CARTESIAN_POINT('Ctrl Pts',(128.268825870595,-31.2980448796578,25.6598487256699));
#23548=CARTESIAN_POINT('Ctrl Pts',(128.378237088824,-31.2507187275515,25.6540251319991));
#23549=CARTESIAN_POINT('Ctrl Pts',(128.487510268548,-31.2034522844158,25.6482088856567));
#23550=CARTESIAN_POINT('Ctrl Pts',(128.598995873004,-31.1609045440246,25.6423926393143));
#23551=CARTESIAN_POINT('Ctrl Pts',(128.712248810399,-31.1232846540299,25.636576392972));
#23552=CARTESIAN_POINT('Ctrl Pts',(128.825388380978,-31.0857024217527,25.6307659687243));
#23553=CARTESIAN_POINT('Ctrl Pts',(128.940291379782,-31.0530383546505,25.6249555444766));
#23554=CARTESIAN_POINT('Ctrl Pts',(129.056492394029,-31.0254536865858,25.6191451202289));
#23555=CARTESIAN_POINT('Ctrl Pts',(129.177091857028,-30.9968248817756,25.6131147594045));
#23556=CARTESIAN_POINT('Ctrl Pts',(129.299089130788,-30.9736677832049,25.6070843985801));
#23557=CARTESIAN_POINT('Ctrl Pts',(129.42194576277,-30.9561060475304,25.6010540377557));
#23558=CARTESIAN_POINT('Ctrl Pts',(129.540188383732,-30.9392038614513,25.5952501535231));
#23559=CARTESIAN_POINT('Ctrl Pts',(129.659226538169,-30.9274844008765,25.5894462692905));
#23560=CARTESIAN_POINT('Ctrl Pts',(129.778570096611,-30.9210057859952,25.5836423850579));
#23561=CARTESIAN_POINT('Ctrl Pts',(129.897896026732,-30.9145281280745,25.5778393581211));
#23562=CARTESIAN_POINT('Ctrl Pts',(130.01752686352,-30.9132897984775,25.5720363311842));
#23563=CARTESIAN_POINT('Ctrl Pts',(130.136968921539,-30.9172969108038,25.5662333042474));
#23564=CARTESIAN_POINT('Ctrl Pts',(130.256421525043,-30.9213043769162,25.560429764964));
#23565=CARTESIAN_POINT('Ctrl Pts',(130.375684908512,-30.9305581920495,25.5546262256806));
#23566=CARTESIAN_POINT('Ctrl Pts',(130.494267601245,-30.9450123873975,25.5488226863971));
#23567=CARTESIAN_POINT('Ctrl Pts',(130.612888748962,-30.9594712700724,25.5430172650936));
#23568=CARTESIAN_POINT('Ctrl Pts',(130.730828361811,-30.9791338374944,25.53721184379));
#23569=CARTESIAN_POINT('Ctrl Pts',(130.847602925348,-31.0039026186863,25.5314064224865));
#23570=CARTESIAN_POINT('Ctrl Pts',(130.964506805905,-31.0286988290109,25.5255945722162));
#23571=CARTESIAN_POINT('Ctrl Pts',(131.080242662143,-31.0586124555127,25.5197827219459));
#23572=CARTESIAN_POINT('Ctrl Pts',(131.194339806386,-31.0934954976499,25.5139708716756));
#23573=CARTESIAN_POINT('Ctrl Pts',(131.308511890247,-31.1284014511566,25.5081552041508));
#23574=CARTESIAN_POINT('Ctrl Pts',(131.421042734608,-31.1682831844245,25.502339536626));
#23575=CARTESIAN_POINT('Ctrl Pts',(131.531480935743,-31.2129442645434,25.4965238691012));
#23576=CARTESIAN_POINT('Ctrl Pts',(131.642077327677,-31.2576693168372,25.4906998712607));
#23577=CARTESIAN_POINT('Ctrl Pts',(131.750574723407,-31.3071872110837,25.4848758734202));
#23578=CARTESIAN_POINT('Ctrl Pts',(131.856545517183,-31.3612551968259,25.4790518755796));
#23579=CARTESIAN_POINT('Ctrl Pts',(131.884660146513,-31.3755997282159,25.4775067372008));
#23580=CARTESIAN_POINT('Ctrl Pts',(131.91259709215,-31.3902642890495,25.4759615988219));
#23581=CARTESIAN_POINT('Ctrl Pts',(131.940348719913,-31.4052438406572,25.474416460443));
#23582=CARTESIAN_POINT('Ctrl Pts',(132.044926391124,-31.4616919393519,25.4685938479916));
#23583=CARTESIAN_POINT('Ctrl Pts',(132.147207370064,-31.5227983537948,25.4627712355401));
#23584=CARTESIAN_POINT('Ctrl Pts',(132.246748991077,-31.588351722247,25.4569486230886));
#23585=CARTESIAN_POINT('Ctrl Pts',(132.328827476711,-31.6424047018551,25.4521475036415));
#23586=CARTESIAN_POINT('Ctrl Pts',(132.409043659943,-31.6994802575364,25.4473463841943));
#23587=CARTESIAN_POINT('Ctrl Pts',(132.487160670875,-31.7594357285724,25.4425452647471));
#23588=CARTESIAN_POINT('',(125.915000988625,-35.0028420178004,25.9896150286367));
#23589=CARTESIAN_POINT('Ctrl Pts',(125.915000988624,-35.0028420169516,25.9896150285955));
#23590=CARTESIAN_POINT('Ctrl Pts',(125.914917631215,-34.8830274839136,25.98379925565));
#23591=CARTESIAN_POINT('Ctrl Pts',(125.920109897602,-34.7631670310304,25.9779834827044));
#23592=CARTESIAN_POINT('Ctrl Pts',(125.930563220774,-34.6437566844379,25.9721677097589));
#23593=CARTESIAN_POINT('Ctrl Pts',(125.941015823111,-34.5243545720863,25.9663523378546));
#23594=CARTESIAN_POINT('Ctrl Pts',(125.956728725648,-34.4054029082059,25.9605369659503));
#23595=CARTESIAN_POINT('Ctrl Pts',(125.977635392704,-34.2873935406028,25.954721594046));
#23596=CARTESIAN_POINT('Ctrl Pts',(125.998545461785,-34.16936497,25.948905275839));
#23597=CARTESIAN_POINT('Ctrl Pts',(126.024650905997,-34.0522793999723,25.943088957632));
#23598=CARTESIAN_POINT('Ctrl Pts',(126.05583399618,-33.9366188198428,25.937272639425));
#23599=CARTESIAN_POINT('Ctrl Pts',(126.087029385142,-33.820912622558,25.9314540272308));
#23600=CARTESIAN_POINT('Ctrl Pts',(126.123306298709,-33.7066329244786,25.9256354150366));
#23601=CARTESIAN_POINT('Ctrl Pts',(126.164497225102,-33.5942463004665,25.9198168028424));
#23602=CARTESIAN_POINT('Ctrl Pts',(126.205738353575,-33.4817227035156,25.9139910991244));
#23603=CARTESIAN_POINT('Ctrl Pts',(126.251905311348,-33.3710971675099,25.9081653954065));
#23604=CARTESIAN_POINT('Ctrl Pts',(126.302782435853,-33.2628162781789,25.9023396916885));
#23605=CARTESIAN_POINT('Ctrl Pts',(126.353695625483,-33.1544586320743,25.8965098583201));
#23606=CARTESIAN_POINT('Ctrl Pts',(126.409325443941,-33.0484493010495,25.8906800249518));
#23607=CARTESIAN_POINT('Ctrl Pts',(126.469411107928,-32.9452087514349,25.8848501915834));
#23608=CARTESIAN_POINT('Ctrl Pts',(126.529589512802,-32.8418088523261,25.8790113599967));
#23609=CARTESIAN_POINT('Ctrl Pts',(126.594237274589,-32.7411866060431,25.8731725284101));
#23610=CARTESIAN_POINT('Ctrl Pts',(126.663051158471,-32.6437323095588,25.8673336968235));
#23611=CARTESIAN_POINT('Ctrl Pts',(126.686630918682,-32.6103386277456,25.8653329632365));
#23612=CARTESIAN_POINT('Ctrl Pts',(126.710699509638,-32.5773166148935,25.8633322296496));
#23613=CARTESIAN_POINT('Ctrl Pts',(126.735243706803,-32.5446810093122,25.8613314960627));
#23614=CARTESIAN_POINT('Ctrl Pts',(126.80668521814,-32.4496875992438,25.8555079023934));
#23615=CARTESIAN_POINT('Ctrl Pts',(126.882391357813,-32.3576616542344,25.849684308724));
#23616=CARTESIAN_POINT('Ctrl Pts',(126.962086897633,-32.2690095235488,25.8438607150547));
#23617=CARTESIAN_POINT('Ctrl Pts',(127.041681889693,-32.1804692406932,25.8380444687137));
#23618=CARTESIAN_POINT('Ctrl Pts',(127.125256000357,-32.0952946069411,25.8322282223727));
#23619=CARTESIAN_POINT('Ctrl Pts',(127.212491956808,-32.0138613714127,25.8264119760317));
#23620=CARTESIAN_POINT('Ctrl Pts',(127.299640589586,-31.9325096510016,25.8206015517854));
#23621=CARTESIAN_POINT('Ctrl Pts',(127.390443479258,-31.8548921553197,25.814791127539));
#23622=CARTESIAN_POINT('Ctrl Pts',(127.484544897526,-31.7813495642682,25.8089807032927));
#23623=CARTESIAN_POINT('Ctrl Pts',(127.582208249156,-31.7050232339974,25.8029503424677));
#23624=CARTESIAN_POINT('Ctrl Pts',(127.683424475912,-31.6330867240478,25.7969199816428));
#23625=CARTESIAN_POINT('Ctrl Pts',(127.78775579291,-31.5658770307111,25.7908896208179));
#23626=CARTESIAN_POINT('Ctrl Pts',(127.888168836698,-31.5011914686559,25.7850857365864));
#23627=CARTESIAN_POINT('Ctrl Pts',(127.991466835099,-31.4408843257239,25.779281852355));
#23628=CARTESIAN_POINT('Ctrl Pts',(128.097228583065,-31.3852128783433,25.7734779681235));
#23629=CARTESIAN_POINT('Ctrl Pts',(128.202974708891,-31.3295496542302,25.7676749411878));
#23630=CARTESIAN_POINT('Ctrl Pts',(128.31118349932,-31.2785209540833,25.761871914252));
#23631=CARTESIAN_POINT('Ctrl Pts',(128.421408823274,-31.2323382719833,25.7560688873162));
#23632=CARTESIAN_POINT('Ctrl Pts',(128.531643878972,-31.1861515124349,25.7502653480338));
#23633=CARTESIAN_POINT('Ctrl Pts',(128.643895445546,-31.144811779412,25.7444618087514));
#23634=CARTESIAN_POINT('Ctrl Pts',(128.757697678905,-31.1084823085327,25.738658269469));
#23635=CARTESIAN_POINT('Ctrl Pts',(128.871536817004,-31.0721410564291,25.7328528481664));
#23636=CARTESIAN_POINT('Ctrl Pts',(128.986927233173,-31.040813421886,25.7270474268638));
#23637=CARTESIAN_POINT('Ctrl Pts',(129.103388830485,-31.0146125143595,25.7212420055612));
#23638=CARTESIAN_POINT('Ctrl Pts',(129.219979398238,-30.9883825917524,25.7154301552918));
#23639=CARTESIAN_POINT('Ctrl Pts',(129.337643116341,-30.9672908183684,25.7096183050223));
#23640=CARTESIAN_POINT('Ctrl Pts',(129.455890467262,-30.9513990297408,25.7038064547528));
#23641=CARTESIAN_POINT('Ctrl Pts',(129.57421548368,-30.9354968033008,25.6979907872288));
#23642=CARTESIAN_POINT('Ctrl Pts',(129.693124490572,-30.9248013999251,25.6921751197048));
#23643=CARTESIAN_POINT('Ctrl Pts',(129.812125293178,-30.9193225936694,25.6863594521808));
#23644=CARTESIAN_POINT('Ctrl Pts',(129.931296551588,-30.9138359396153,25.680535454341));
#23645=CARTESIAN_POINT('Ctrl Pts',(130.050559461267,-30.9135807976808,25.6747114565011));
#23646=CARTESIAN_POINT('Ctrl Pts',(130.169424134947,-30.9185149194812,25.6688874586613));
#23647=CARTESIAN_POINT('Ctrl Pts',(130.200959581122,-30.9198239689039,25.6673423202723));
#23648=CARTESIAN_POINT('Ctrl Pts',(130.232467039439,-30.9214979936995,25.6657971818832));
#23649=CARTESIAN_POINT('Ctrl Pts',(130.263937469796,-30.9235355990714,25.6642520434942));
#23650=CARTESIAN_POINT('Ctrl Pts',(130.382535283496,-30.9312144118348,25.6584291159803));
#23651=CARTESIAN_POINT('Ctrl Pts',(130.500988941927,-30.9440855038667,25.6526061884664));
#23652=CARTESIAN_POINT('Ctrl Pts',(130.618807884703,-30.9621414336521,25.6467832609524));
#23653=CARTESIAN_POINT('Ctrl Pts',(130.736486110336,-30.9801757983241,25.6409672880564));
#23654=CARTESIAN_POINT('Ctrl Pts',(130.853530727798,-31.0033826262588,25.6351513151604));
#23655=CARTESIAN_POINT('Ctrl Pts',(130.969453622283,-31.0317025471566,25.6293353422643));
#23656=CARTESIAN_POINT('Ctrl Pts',(131.085265436093,-31.0599953310862,25.623524942402));
#23657=CARTESIAN_POINT('Ctrl Pts',(131.199957270419,-31.0933913669269,25.6177145425396));
#23658=CARTESIAN_POINT('Ctrl Pts',(131.313049197558,-31.1317798918892,25.6119041426772));
#23659=CARTESIAN_POINT('Ctrl Pts',(131.426056890353,-31.170139823898,25.6060980705793));
#23660=CARTESIAN_POINT('Ctrl Pts',(131.537466661935,-31.2134847146107,25.6002919984813));
#23661=CARTESIAN_POINT('Ctrl Pts',(131.646812448055,-31.2616536060806,25.5944859263834));
#23662=CARTESIAN_POINT('Ctrl Pts',(131.75610939188,-31.3098009815934,25.5886824477269));
#23663=CARTESIAN_POINT('Ctrl Pts',(131.863343811697,-31.3627679059948,25.5828789690703));
#23664=CARTESIAN_POINT('Ctrl Pts',(131.968068894647,-31.4203450130042,25.5770754904138));
#23665=CARTESIAN_POINT('Ctrl Pts',(132.072791333078,-31.477920666076,25.5712721583068));
#23666=CARTESIAN_POINT('Ctrl Pts',(132.175004198702,-31.5401060813459,25.5654688261997));
#23667=CARTESIAN_POINT('Ctrl Pts',(132.274284934959,-31.6066457546229,25.5596654940927));
#23668=CARTESIAN_POINT('Ctrl Pts',(132.346861702901,-31.6552879646674,25.5554231092806));
#23669=CARTESIAN_POINT('Ctrl Pts',(132.417872030513,-31.7062561071201,25.5511807244686));
#23670=CARTESIAN_POINT('Ctrl Pts',(132.487160670875,-31.7594357285724,25.5469383396565));
#23671=CARTESIAN_POINT('Ctrl Pts',(132.487160670875,-31.7594357285724,26.7967734504842));
#23672=CARTESIAN_POINT('Ctrl Pts',(132.581820842687,-31.8320882164445,26.7909668279223));
#23673=CARTESIAN_POINT('Ctrl Pts',(132.673369442088,-31.9089489675386,26.7851602053605));
#23674=CARTESIAN_POINT('Ctrl Pts',(132.76141620503,-31.9897167006079,26.7793535827986));
#23675=CARTESIAN_POINT('Ctrl Pts',(132.849425873815,-32.0704504061804,26.7735494065705));
#23676=CARTESIAN_POINT('Ctrl Pts',(132.933936338899,-32.1550875457114,26.7677452303424));
#23677=CARTESIAN_POINT('Ctrl Pts',(133.014590944703,-32.2432870232625,26.7619410541143));
#23678=CARTESIAN_POINT('Ctrl Pts',(133.095230284945,-32.3314698072271,26.7561379764474));
#23679=CARTESIAN_POINT('Ctrl Pts',(133.172014941736,-32.4232132872004,26.7503348987804));
#23680=CARTESIAN_POINT('Ctrl Pts',(133.244626084105,-32.5181405006837,26.7445318211134));
#23681=CARTESIAN_POINT('Ctrl Pts',(133.317240619587,-32.6130721501085,26.7387284722691));
#23682=CARTESIAN_POINT('Ctrl Pts',(133.385681004865,-32.7111875044315,26.7329251234247));
#23683=CARTESIAN_POINT('Ctrl Pts',(133.449669970158,-32.8120781327959,26.7271217745804));
#23684=CARTESIAN_POINT('Ctrl Pts',(133.513677026994,-32.9129972858761,26.7213167849605));
#23685=CARTESIAN_POINT('Ctrl Pts',(133.573229942324,-33.0166929287383,26.7155117953405));
#23686=CARTESIAN_POINT('Ctrl Pts',(133.628096220153,-33.1227299562102,26.7097068057206));
#23687=CARTESIAN_POINT('Ctrl Pts',(133.683022189654,-33.2288823464814,26.7038955005724));
#23688=CARTESIAN_POINT('Ctrl Pts',(133.733251154285,-33.3373808439128,26.6980841954241));
#23689=CARTESIAN_POINT('Ctrl Pts',(133.778597736247,-33.4477680110159,26.6922728902759));
#23690=CARTESIAN_POINT('Ctrl Pts',(133.82397241188,-33.5582235665286,26.6864579848367));
#23691=CARTESIAN_POINT('Ctrl Pts',(133.864458542072,-33.6705697386857,26.6806430793975));
#23692=CARTESIAN_POINT('Ctrl Pts',(133.899920380554,-33.7843330944115,26.6748281739584));
#23693=CARTESIAN_POINT('Ctrl Pts',(133.935434693245,-33.8982647900363,26.6690046639858));
#23694=CARTESIAN_POINT('Ctrl Pts',(133.965909766219,-34.0136174623106,26.6631811540132));
#23695=CARTESIAN_POINT('Ctrl Pts',(133.991260715997,-34.1299063861051,26.6573576440406));
#23696=CARTESIAN_POINT('Ctrl Pts',(134.002446048264,-34.1812153217859,26.6547881981392));
#23697=CARTESIAN_POINT('Ctrl Pts',(134.012634521584,-34.2327064385346,26.6522187522379));
#23698=CARTESIAN_POINT('Ctrl Pts',(134.021822060174,-34.2843378476543,26.6496493063365));
#23699=CARTESIAN_POINT('Ctrl Pts',(134.042645419241,-34.4013593285178,26.6438257123361));
#23700=CARTESIAN_POINT('Ctrl Pts',(134.058390721628,-34.5194791038513,26.6380021183358));
#23701=CARTESIAN_POINT('Ctrl Pts',(134.068948190858,-34.6382188228866,26.6321785243355));
#23702=CARTESIAN_POINT('Ctrl Pts',(134.079492340279,-34.7568087342102,26.62636227766));
#23703=CARTESIAN_POINT('Ctrl Pts',(134.084861638985,-34.8760166304091,26.6205460309846));
#23704=CARTESIAN_POINT('Ctrl Pts',(134.084997358261,-34.9953542488175,26.6147297843091));
#23705=CARTESIAN_POINT('Ctrl Pts',(134.08513294168,-35.1145724096823,26.6089193597252));
#23706=CARTESIAN_POINT('Ctrl Pts',(134.080045367229,-35.2339196284414,26.6031089351413));
#23707=CARTESIAN_POINT('Ctrl Pts',(134.06972777815,-35.3529034028614,26.5972985105574));
#23708=CARTESIAN_POINT('Ctrl Pts',(134.059019647824,-35.4763909495606,26.5912681498578));
#23709=CARTESIAN_POINT('Ctrl Pts',(134.042677707291,-35.5994865476445,26.5852377891583));
#23710=CARTESIAN_POINT('Ctrl Pts',(134.020753720595,-35.7216401584744,26.5792074284587));
#23711=CARTESIAN_POINT('Ctrl Pts',(133.999653110775,-35.839206170349,26.5734035438842));
#23712=CARTESIAN_POINT('Ctrl Pts',(133.973382250749,-35.9558992354687,26.5675996593098));
#23713=CARTESIAN_POINT('Ctrl Pts',(133.94203994179,-36.0712357804576,26.5617957747353));
#23714=CARTESIAN_POINT('Ctrl Pts',(133.910702262416,-36.1865552890363,26.5559927474551));
#23715=CARTESIAN_POINT('Ctrl Pts',(133.874294730895,-36.3005182820209,26.5501897201749));
#23716=CARTESIAN_POINT('Ctrl Pts',(133.832966639145,-36.412654148474,26.5443866928947));
#23717=CARTESIAN_POINT('Ctrl Pts',(133.791634898549,-36.5247999153723,26.5385831532667));
#23718=CARTESIAN_POINT('Ctrl Pts',(133.745381875178,-36.6351178518403,26.5327796136388));
#23719=CARTESIAN_POINT('Ctrl Pts',(133.694405610657,-36.7431558117236,26.5269760740109));
#23720=CARTESIAN_POINT('Ctrl Pts',(133.643412815122,-36.8512288070687,26.5211706523622));
#23721=CARTESIAN_POINT('Ctrl Pts',(133.587693906403,-36.957019986286,26.5153652307134));
#23722=CARTESIAN_POINT('Ctrl Pts',(133.527493321216,-37.0601009365497,26.5095598090647));
#23723=CARTESIAN_POINT('Ctrl Pts',(133.467226069464,-37.1632960394077,26.5037479584497));
#23724=CARTESIAN_POINT('Ctrl Pts',(133.402467440639,-37.2637745695883,26.4979361078348));
#23725=CARTESIAN_POINT('Ctrl Pts',(133.333505813073,-37.3611361659615,26.4921242572199));
#23726=CARTESIAN_POINT('Ctrl Pts',(133.264498891141,-37.4585617099506,26.4863085893505));
#23727=CARTESIAN_POINT('Ctrl Pts',(133.191283722595,-37.5528659212446,26.4804929214811));
#23728=CARTESIAN_POINT('Ctrl Pts',(133.114188607779,-37.6436819618065,26.4746772536117));
#23729=CARTESIAN_POINT('Ctrl Pts',(133.036983062576,-37.7346280864924,26.4688532554291));
#23730=CARTESIAN_POINT('Ctrl Pts',(132.955886755106,-37.8220757695081,26.4630292572465));
#23731=CARTESIAN_POINT('Ctrl Pts',(132.871264481853,-37.9056953170025,26.4572052590639));
#23732=CARTESIAN_POINT('Ctrl Pts',(132.848813780388,-37.9278799904371,26.4556601239653));
#23733=CARTESIAN_POINT('Ctrl Pts',(132.826115074573,-37.9497954371215,26.4541149888666));
#23734=CARTESIAN_POINT('Ctrl Pts',(132.803175546273,-37.9714359923744,26.452569853768));
#23735=CARTESIAN_POINT('Ctrl Pts',(132.71671676846,-38.0529989580071,26.4467462600813));
#23736=CARTESIAN_POINT('Ctrl Pts',(132.62655580342,-38.1309168291375,26.4409226663946));
#23737=CARTESIAN_POINT('Ctrl Pts',(132.533032554403,-38.2048355774258,26.4350990727079));
#23738=CARTESIAN_POINT('Ctrl Pts',(132.43962729884,-38.2786610662467,26.4292828263486));
#23739=CARTESIAN_POINT('Ctrl Pts',(132.34286851411,-38.3484972166099,26.4234665799893));
#23740=CARTESIAN_POINT('Ctrl Pts',(132.243132376016,-38.4140272617056,26.4176503336301));
#23741=CARTESIAN_POINT('Ctrl Pts',(132.143496074328,-38.4794917108768,26.4118399093644));
#23742=CARTESIAN_POINT('Ctrl Pts',(132.040888687611,-38.5406584069209,26.4060294850987));
#23743=CARTESIAN_POINT('Ctrl Pts',(131.935718371841,-38.5972516432571,26.400219060833));
#23744=CARTESIAN_POINT('Ctrl Pts',(131.826567142526,-38.6559870504088,26.394188700015));
#23745=CARTESIAN_POINT('Ctrl Pts',(131.714655477881,-38.7097956491854,26.3881583391969));
#23746=CARTESIAN_POINT('Ctrl Pts',(131.600471789566,-38.758419222333,26.3821279783788));
#23747=CARTESIAN_POINT('Ctrl Pts',(131.490576390177,-38.8052166858733,26.3763240941258));
#23748=CARTESIAN_POINT('Ctrl Pts',(131.378576955514,-38.8472113842628,26.3705202098727));
#23749=CARTESIAN_POINT('Ctrl Pts',(131.264932091607,-38.8842208747216,26.3647163256197));
#23750=CARTESIAN_POINT('Ctrl Pts',(131.151304014243,-38.9212248984886,26.3589132986615));
#23751=CARTESIAN_POINT('Ctrl Pts',(131.036031379141,-38.9532450523193,26.3531102717033));
#23752=CARTESIAN_POINT('Ctrl Pts',(130.919589628053,-38.9801482278901,26.3473072447451));
#23753=CARTESIAN_POINT('Ctrl Pts',(130.803137596359,-39.0070537787339,26.3415037054395));
#23754=CARTESIAN_POINT('Ctrl Pts',(130.685516641328,-39.0288413611504,26.3357001661339));
#23755=CARTESIAN_POINT('Ctrl Pts',(130.567213484114,-39.0454287613848,26.3298966268282));
#23756=CARTESIAN_POINT('Ctrl Pts',(130.448871962547,-39.0620215407223,26.3240912055016));
#23757=CARTESIAN_POINT('Ctrl Pts',(130.329848202995,-39.0734107274202,26.318285784175));
#23758=CARTESIAN_POINT('Ctrl Pts',(130.210634508843,-39.0795659209877,26.3124803628483));
#23759=CARTESIAN_POINT('Ctrl Pts',(130.091288796536,-39.0857279308636,26.3066685125538));
#23760=CARTESIAN_POINT('Ctrl Pts',(129.971753137817,-39.0866443569019,26.3008566622593));
#23761=CARTESIAN_POINT('Ctrl Pts',(129.852520461635,-39.0823369270264,26.2950448119648));
#23762=CARTESIAN_POINT('Ctrl Pts',(129.733209472777,-39.0780266680074,26.2892291444151));
#23763=CARTESIAN_POINT('Ctrl Pts',(129.614202268867,-39.0684857525945,26.2834134768654));
#23764=CARTESIAN_POINT('Ctrl Pts',(129.495985624897,-39.0537876744705,26.2775978093158));
#23765=CARTESIAN_POINT('Ctrl Pts',(129.377599648333,-39.0390685429347,26.2717738114495));
#23766=CARTESIAN_POINT('Ctrl Pts',(129.260006893091,-39.0191775723406,26.2659498135832));
#23767=CARTESIAN_POINT('Ctrl Pts',(129.143683073694,-38.9942391417792,26.2601258157169));
#23768=CARTESIAN_POINT('Ctrl Pts',(129.112821734483,-38.987622841103,26.2585806775445));
#23769=CARTESIAN_POINT('Ctrl Pts',(129.082049622154,-38.9806515350318,26.2570355393721));
#23770=CARTESIAN_POINT('Ctrl Pts',(129.051375411372,-38.9733281251176,26.2554904011996));
#23771=CARTESIAN_POINT('Ctrl Pts',(128.935764949884,-38.9457263456983,26.2496668076131));
#23772=CARTESIAN_POINT('Ctrl Pts',(128.82117373593,-38.9130300558571,26.2438432140266));
#23773=CARTESIAN_POINT('Ctrl Pts',(128.708084191167,-38.8753294753978,26.23801962044));
#23774=CARTESIAN_POINT('Ctrl Pts',(128.595137325691,-38.8376764598303,26.2322033741833));
#23775=CARTESIAN_POINT('Ctrl Pts',(128.483688745096,-38.7950318393624,26.2263871279266));
#23776=CARTESIAN_POINT('Ctrl Pts',(128.374209589866,-38.7475365965281,26.2205708816699));
#23777=CARTESIAN_POINT('Ctrl Pts',(128.264840023901,-38.7000888967052,26.2147604575092));
#23778=CARTESIAN_POINT('Ctrl Pts',(128.157436333883,-38.6478003955138,26.2089500333485));
#23779=CARTESIAN_POINT('Ctrl Pts',(128.052452849073,-38.5908613305049,26.2031396091877));
#23780=CARTESIAN_POINT('Ctrl Pts',(127.943495519992,-38.531767002907,26.1971092483312));
#23781=CARTESIAN_POINT('Ctrl Pts',(127.837145661117,-38.4676632298352,26.1910788874747));
#23782=CARTESIAN_POINT('Ctrl Pts',(127.733886967421,-38.3988169594102,26.1850485266182));
#23783=CARTESIAN_POINT('Ctrl Pts',(127.634506265465,-38.3325562850112,26.1792446424752));
#23784=CARTESIAN_POINT('Ctrl Pts',(127.537989102031,-38.2619031554098,26.1734407583322));
#23785=CARTESIAN_POINT('Ctrl Pts',(127.444739458112,-38.1871411269462,26.1676368741892));
#23786=CARTESIAN_POINT('Ctrl Pts',(127.351503588177,-38.1123901416446,26.1618338473428));
#23787=CARTESIAN_POINT('Ctrl Pts',(127.261534596423,-38.0335317198258,26.1560308204964));
#23788=CARTESIAN_POINT('Ctrl Pts',(127.175204430662,-37.9508905420987,26.15022779365));
#23789=CARTESIAN_POINT('Ctrl Pts',(127.08886664286,-37.86824206803,26.1444242544578));
#23790=CARTESIAN_POINT('Ctrl Pts',(127.006168614799,-37.7818104564063,26.1386207152655));
#23791=CARTESIAN_POINT('Ctrl Pts',(126.927445910499,-37.6919577201531,26.1328171760733));
#23792=CARTESIAN_POINT('Ctrl Pts',(126.848697677352,-37.6020758457143,26.1270117548615));
#23793=CARTESIAN_POINT('Ctrl Pts',(126.773927600746,-37.508770947214,26.1212063336498));
#23794=CARTESIAN_POINT('Ctrl Pts',(126.703430969558,-37.4124381085387,26.115400912438));
#23795=CARTESIAN_POINT('Ctrl Pts',(126.632856269881,-37.3159985901676,26.10958906226));
#23796=CARTESIAN_POINT('Ctrl Pts',(126.566564703279,-37.2165247681411,26.103777212082));
#23797=CARTESIAN_POINT('Ctrl Pts',(126.504808302838,-37.114440824448,26.0979653619039));
#23798=CARTESIAN_POINT('Ctrl Pts',(126.443011340466,-37.0122898314788,26.0921496944719));
#23799=CARTESIAN_POINT('Ctrl Pts',(126.385755671832,-36.9075256601811,26.0863340270398));
#23800=CARTESIAN_POINT('Ctrl Pts',(126.333246661262,-36.8005957216576,26.0805183596078));
#23801=CARTESIAN_POINT('Ctrl Pts',(126.280662437201,-36.6935126175377,26.0746943618598));
#23802=CARTESIAN_POINT('Ctrl Pts',(126.232838604949,-36.584257927056,26.0688703641118));
#23803=CARTESIAN_POINT('Ctrl Pts',(126.189931906797,-36.4732977041844,26.0630463663638));
#23804=CARTESIAN_POINT('Ctrl Pts',(126.178548519299,-36.4438593351597,26.0615012271196));
#23805=CARTESIAN_POINT('Ctrl Pts',(126.167510959477,-36.4143009917256,26.0599560878754));
#23806=CARTESIAN_POINT('Ctrl Pts',(126.156821555698,-36.3846315196659,26.0584109486312));
#23807=CARTESIAN_POINT('Ctrl Pts',(126.110323273239,-36.2555710481221,26.0516896831143));
#23808=CARTESIAN_POINT('Ctrl Pts',(126.070293444533,-36.1240650790749,26.0449684175974));
#23809=CARTESIAN_POINT('Ctrl Pts',(126.03695945865,-35.9907243146395,26.0382471520806));
#23810=CARTESIAN_POINT('Ctrl Pts',(126.003758284155,-35.8579148149631,26.0315526658575));
#23811=CARTESIAN_POINT('Ctrl Pts',(125.977199802155,-35.7232852451568,26.0248581796344));
#23812=CARTESIAN_POINT('Ctrl Pts',(125.957461778018,-35.5874604019115,26.0181636934114));
#23813=CARTESIAN_POINT('Ctrl Pts',(125.937867450406,-35.4526243890526,26.0115179443062));
#23814=CARTESIAN_POINT('Ctrl Pts',(125.924994719631,-35.316610591759,26.004872195201));
#23815=CARTESIAN_POINT('Ctrl Pts',(125.91896982726,-35.1800492410075,25.9982264460959));
#23816=CARTESIAN_POINT('Ctrl Pts',(125.916367519001,-35.1210648294937,25.9953559736095));
#23817=CARTESIAN_POINT('Ctrl Pts',(125.915042131088,-35.0619784943742,25.9924855011231));
#23818=CARTESIAN_POINT('Ctrl Pts',(125.915000988625,-35.0028420178004,25.9896150286367));
#23819=CARTESIAN_POINT('Origin',(130.,-35.,32.7603849714045));
#23820=CARTESIAN_POINT('',(132.487160670875,-31.7594357285724,28.0469635236591));
#23821=CARTESIAN_POINT('',(132.487160670875,-31.7594357285724,27.9426397368634));
#23822=CARTESIAN_POINT('',(132.487160670875,-31.7594357285724,32.7603849714045));
#23823=CARTESIAN_POINT('',(125.915000279441,-34.9984890288179,27.1353849713731));
#23824=CARTESIAN_POINT('Ctrl Pts',(132.487160670875,-31.7594357285724,27.9426397368634));
#23825=CARTESIAN_POINT('Ctrl Pts',(132.581967877144,-31.8322010666427,27.9368366816923));
#23826=CARTESIAN_POINT('Ctrl Pts',(132.673586253723,-31.9091358676846,27.9310336265213));
#23827=CARTESIAN_POINT('Ctrl Pts',(132.761639006081,-31.989921097364,27.9252305713502));
#23828=CARTESIAN_POINT('Ctrl Pts',(132.849706643262,-32.0707199833336,27.9194265352053));
#23829=CARTESIAN_POINT('Ctrl Pts',(132.934207156769,-32.1553703162151,27.9136224990603));
#23830=CARTESIAN_POINT('Ctrl Pts',(133.014799632995,-32.2435152507423,27.9078184629153));
#23831=CARTESIAN_POINT('Ctrl Pts',(133.095475188514,-32.3317510500642,27.9020084436409));
#23832=CARTESIAN_POINT('Ctrl Pts',(133.172234383558,-32.4234883449647,27.8961984243665));
#23833=CARTESIAN_POINT('Ctrl Pts',(133.244775576362,-32.5183359496006,27.890388405092));
#23834=CARTESIAN_POINT('Ctrl Pts',(133.317354314023,-32.6132326441337,27.884575378749));
#23835=CARTESIAN_POINT('Ctrl Pts',(133.385710466145,-32.7112425208822,27.8787623524061));
#23836=CARTESIAN_POINT('Ctrl Pts',(133.449585855986,-32.8119455166326,27.8729493260631));
#23837=CARTESIAN_POINT('Ctrl Pts',(133.513564534955,-32.9128113532636,27.8671268998177));
#23838=CARTESIAN_POINT('Ctrl Pts',(133.573047769814,-33.0163786564525,27.8613044735724));
#23839=CARTESIAN_POINT('Ctrl Pts',(133.627823176215,-33.1222023532567,27.855482047327));
#23840=CARTESIAN_POINT('Ctrl Pts',(133.6783490715,-33.2198161798754,27.8501113286395));
#23841=CARTESIAN_POINT('Ctrl Pts',(133.724869706477,-33.3193493960304,27.8447406099519));
#23842=CARTESIAN_POINT('Ctrl Pts',(133.767255489786,-33.4204395944825,27.8393698912643));
#23843=CARTESIAN_POINT('Ctrl Pts',(133.813215309588,-33.5300538788457,27.8335463050565));
#23844=CARTESIAN_POINT('Ctrl Pts',(133.854461171478,-33.6418525051197,27.8277227188486));
#23845=CARTESIAN_POINT('Ctrl Pts',(133.890781146522,-33.7553928049892,27.8218991326408));
#23846=CARTESIAN_POINT('Ctrl Pts',(133.927055297774,-33.8687898545676,27.8160828938718));
#23847=CARTESIAN_POINT('Ctrl Pts',(133.958415800033,-33.9839238216377,27.8102666551029));
#23848=CARTESIAN_POINT('Ctrl Pts',(133.984698359438,-34.1003311807697,27.804450416334));
#23849=CARTESIAN_POINT('Ctrl Pts',(134.010954609366,-34.2166220133285,27.7986399997603));
#23850=CARTESIAN_POINT('Ctrl Pts',(134.032142939308,-34.3341833060769,27.7928295831866));
#23851=CARTESIAN_POINT('Ctrl Pts',(134.048148737625,-34.4525360303471,27.7870191666129));
#23852=CARTESIAN_POINT('Ctrl Pts',(134.064760418275,-34.575368870098,27.7809888029497));
#23853=CARTESIAN_POINT('Ctrl Pts',(134.075789319628,-34.6990538159745,27.7749584392865));
#23854=CARTESIAN_POINT('Ctrl Pts',(134.081165417872,-34.8230428527432,27.7689280756233));
#23855=CARTESIAN_POINT('Ctrl Pts',(134.086339601592,-34.9423751317172,27.7631241992668));
#23856=CARTESIAN_POINT('Ctrl Pts',(134.086277919101,-35.0619886269096,27.7573203229102));
#23857=CARTESIAN_POINT('Ctrl Pts',(134.080970805523,-35.181389868696,27.7515164465537));
#23858=CARTESIAN_POINT('Ctrl Pts',(134.075664475921,-35.3007734723626,27.7457134275539));
#23859=CARTESIAN_POINT('Ctrl Pts',(134.065114274316,-35.4199444771519,27.7399104085542));
#23860=CARTESIAN_POINT('Ctrl Pts',(134.049362739796,-35.5384109968717,27.7341073895544));
#23861=CARTESIAN_POINT('Ctrl Pts',(134.033609814721,-35.6568879748883,27.7283038582606));
#23862=CARTESIAN_POINT('Ctrl Pts',(134.0126546976,-35.7746599393862,27.7225003269668));
#23863=CARTESIAN_POINT('Ctrl Pts',(133.986591538575,-35.8912423377291,27.7166967956729));
#23864=CARTESIAN_POINT('Ctrl Pts',(133.960519927758,-36.0078625415514,27.7108913824031));
#23865=CARTESIAN_POINT('Ctrl Pts',(133.929337069791,-36.1232920137451,27.7050859691332));
#23866=CARTESIAN_POINT('Ctrl Pts',(133.893187582972,-36.2370591917086,27.6992805558633));
#23867=CARTESIAN_POINT('Ctrl Pts',(133.856998064044,-36.3509523559731,27.6934687136518));
#23868=CARTESIAN_POINT('Ctrl Pts',(133.815831061387,-36.4631791621531,27.6876568714403));
#23869=CARTESIAN_POINT('Ctrl Pts',(133.769880213874,-36.5732857887369,27.6818450292288));
#23870=CARTESIAN_POINT('Ctrl Pts',(133.723899185746,-36.6834647335877,27.676029369787));
#23871=CARTESIAN_POINT('Ctrl Pts',(133.673128228562,-36.7915203568409,27.6702137103452));
#23872=CARTESIAN_POINT('Ctrl Pts',(133.617807278788,-36.8970227973193,27.6643980509033));
#23873=CARTESIAN_POINT('Ctrl Pts',(133.562407087369,-37.0026763593348,27.6585740611197));
#23874=CARTESIAN_POINT('Ctrl Pts',(133.502444099556,-37.1057690873322,27.652750071336));
#23875=CARTESIAN_POINT('Ctrl Pts',(133.43820200028,-37.2058993642659,27.6469260815523));
#23876=CARTESIAN_POINT('Ctrl Pts',(133.421157360228,-37.2324658144272,27.6453808672669));
#23877=CARTESIAN_POINT('Ctrl Pts',(133.403811717253,-37.258823904402,27.6438356529814));
#23878=CARTESIAN_POINT('Ctrl Pts',(133.386170838292,-37.2849665323374,27.6422904386959));
#23879=CARTESIAN_POINT('Ctrl Pts',(133.31968597873,-37.3834927424374,27.636466842548));
#23880=CARTESIAN_POINT('Ctrl Pts',(133.248790165754,-37.4792736942146,27.6306432464));
#23881=CARTESIAN_POINT('Ctrl Pts',(133.173737464888,-37.571889481289,27.6248196502521));
#23882=CARTESIAN_POINT('Ctrl Pts',(133.098779453809,-37.6643884202153,27.6190034014091));
#23883=CARTESIAN_POINT('Ctrl Pts',(133.019675240873,-37.7537298225903,27.613187152566));
#23884=CARTESIAN_POINT('Ctrl Pts',(132.936722447597,-37.8395221896964,27.607370903723));
#23885=CARTESIAN_POINT('Ctrl Pts',(132.853852690199,-37.9252286785066,27.6015604769543));
#23886=CARTESIAN_POINT('Ctrl Pts',(132.767142298611,-38.0073929076184,27.5957500501856));
#23887=CARTESIAN_POINT('Ctrl Pts',(132.676929094683,-38.0856564329233,27.5899396234168));
#23888=CARTESIAN_POINT('Ctrl Pts',(132.583301189555,-38.1668823466824,27.5839092635298));
#23889=CARTESIAN_POINT('Ctrl Pts',(132.485900341863,-38.2439060792931,27.5778789036427));
#23890=CARTESIAN_POINT('Ctrl Pts',(132.385146510296,-38.3163686653362,27.5718485437557));
#23891=CARTESIAN_POINT('Ctrl Pts',(132.288176537885,-38.3861098837109,27.5660446569677));
#23892=CARTESIAN_POINT('Ctrl Pts',(132.188101247147,-38.4516261097104,27.5602407701796));
#23893=CARTESIAN_POINT('Ctrl Pts',(132.085328120449,-38.5126388413934,27.5544368833916));
#23894=CARTESIAN_POINT('Ctrl Pts',(131.982570174288,-38.5736425609341,27.5486338538911));
#23895=CARTESIAN_POINT('Ctrl Pts',(131.877115535678,-38.630143900653,27.5428308243906));
#23896=CARTESIAN_POINT('Ctrl Pts',(131.769398924054,-38.6819088048941,27.5370277948901));
#23897=CARTESIAN_POINT('Ctrl Pts',(131.661672802084,-38.7336782794812,27.5312242530376));
#23898=CARTESIAN_POINT('Ctrl Pts',(131.551684678089,-38.7807103102658,27.5254207111851));
#23899=CARTESIAN_POINT('Ctrl Pts',(131.439891429161,-38.8228180276112,27.5196171693326));
#23900=CARTESIAN_POINT('Ctrl Pts',(131.328061926951,-38.8649394000114,27.5138117454573));
#23901=CARTESIAN_POINT('Ctrl Pts',(131.214426517548,-38.9021331392433,27.5080063215821));
#23902=CARTESIAN_POINT('Ctrl Pts',(131.099458878302,-38.9342617064606,27.5022008977068));
#23903=CARTESIAN_POINT('Ctrl Pts',(130.984363923273,-38.9664258530264,27.4963890448739));
#23904=CARTESIAN_POINT('Ctrl Pts',(130.86793418704,-38.9935135211693,27.4905771920409));
#23905=CARTESIAN_POINT('Ctrl Pts',(130.750655380073,-39.015437896465,27.484765339208));
#23906=CARTESIAN_POINT('Ctrl Pts',(130.633299543836,-39.0373766717931,27.4789496691228));
#23907=CARTESIAN_POINT('Ctrl Pts',(130.515093929603,-39.0541453432434,27.4731339990377));
#23908=CARTESIAN_POINT('Ctrl Pts',(130.396529586751,-39.0657089525482,27.4673183289526));
#23909=CARTESIAN_POINT('Ctrl Pts',(130.277795413823,-39.0772891254219,27.4614943285746));
#23910=CARTESIAN_POINT('Ctrl Pts',(130.158701892992,-39.0836493333476,27.4556703281966));
#23911=CARTESIAN_POINT('Ctrl Pts',(130.039740432367,-39.0848066904121,27.4498463278186));
#23912=CARTESIAN_POINT('Ctrl Pts',(130.008179822116,-39.0851137385522,27.4483012139216));
#23913=CARTESIAN_POINT('Ctrl Pts',(129.976628478564,-39.0850548687037,27.4467561000245));
#23914=CARTESIAN_POINT('Ctrl Pts',(129.945095500927,-39.0846310109949,27.4452109861274));
#23915=CARTESIAN_POINT('Ctrl Pts',(129.826246487294,-39.0830334748794,27.4393873920245));
#23916=CARTESIAN_POINT('Ctrl Pts',(129.707275603482,-39.0762418978146,27.4335637979216));
#23917=CARTESIAN_POINT('Ctrl Pts',(129.588673316219,-39.0642385952611,27.4277402038187));
#23918=CARTESIAN_POINT('Ctrl Pts',(129.470220663076,-39.0522504366281,27.4219239570309));
#23919=CARTESIAN_POINT('Ctrl Pts',(129.352136084213,-39.0350636714838,27.4161077102431));
#23920=CARTESIAN_POINT('Ctrl Pts',(129.234910162847,-39.012712616309,27.4102914634554));
#23921=CARTESIAN_POINT('Ctrl Pts',(129.117801585011,-38.9903839346133,27.4044810387495));
#23922=CARTESIAN_POINT('Ctrl Pts',(129.001550353571,-38.9629013229485,27.3986706140437));
#23923=CARTESIAN_POINT('Ctrl Pts',(128.886641442207,-38.9303508395295,27.3928601893378));
#23924=CARTESIAN_POINT('Ctrl Pts',(128.767383003563,-38.8965682565809,27.3868298286804));
#23925=CARTESIAN_POINT('Ctrl Pts',(128.649570957648,-38.857326608824,27.3807994680229));
#23926=CARTESIAN_POINT('Ctrl Pts',(128.533735739328,-38.8127803658061,27.3747691073655));
#23927=CARTESIAN_POINT('Ctrl Pts',(128.422250822954,-38.7699070993704,27.3689652226458));
#23928=CARTESIAN_POINT('Ctrl Pts',(128.312597343979,-38.722120650378,27.3631613379261));
#23929=CARTESIAN_POINT('Ctrl Pts',(128.205231600146,-38.6696091605081,27.3573574532065));
#23930=CARTESIAN_POINT('Ctrl Pts',(128.097881715197,-38.6171054270566,27.3515544257726));
#23931=CARTESIAN_POINT('Ctrl Pts',(127.99281926009,-38.5598782200485,27.3457513983388));
#23932=CARTESIAN_POINT('Ctrl Pts',(127.890478289355,-38.4981628253007,27.339948370905));
#23933=CARTESIAN_POINT('Ctrl Pts',(127.788128282817,-38.4364419816295,27.3341448311152));
#23934=CARTESIAN_POINT('Ctrl Pts',(127.688500588084,-38.370232373222,27.3283412913254));
#23935=CARTESIAN_POINT('Ctrl Pts',(127.592001940681,-38.2998136835764,27.3225377515357));
#23936=CARTESIAN_POINT('Ctrl Pts',(127.495471999748,-38.2293721578649,27.3167323297169));
#23937=CARTESIAN_POINT('Ctrl Pts',(127.402073453869,-38.1547190768931,27.3109269078981));
#23938=CARTESIAN_POINT('Ctrl Pts',(127.312180989011,-38.0761752167533,27.3051214860793));
#23939=CARTESIAN_POINT('Ctrl Pts',(127.222188976412,-37.9975443764219,27.2993096352831));
#23940=CARTESIAN_POINT('Ctrl Pts',(127.135711102645,-37.9150144252529,27.2934977844868));
#23941=CARTESIAN_POINT('Ctrl Pts',(127.053086225347,-37.828944008771,27.2876859336906));
#23942=CARTESIAN_POINT('Ctrl Pts',(126.970407079494,-37.7428170606814,27.2818702656331));
#23943=CARTESIAN_POINT('Ctrl Pts',(126.891586238974,-37.653145322177,27.2760545975756));
#23944=CARTESIAN_POINT('Ctrl Pts',(126.81692211702,-37.5603203297405,27.2702389295181));
#23945=CARTESIAN_POINT('Ctrl Pts',(126.742151046706,-37.4673623754414,27.2644149311388));
#23946=CARTESIAN_POINT('Ctrl Pts',(126.671548819799,-37.3712424800554,27.2585909327595));
#23947=CARTESIAN_POINT('Ctrl Pts',(126.605370494355,-37.272381024257,27.2527669343802));
#23948=CARTESIAN_POINT('Ctrl Pts',(126.587813079664,-37.2461526244792,27.2512218007732));
#23949=CARTESIAN_POINT('Ctrl Pts',(126.570566795795,-37.2197313872462,27.2496766671661));
#23950=CARTESIAN_POINT('Ctrl Pts',(126.553635852833,-37.1931254330573,27.248131533559));
#23951=CARTESIAN_POINT('Ctrl Pts',(126.488371803247,-37.0905669212635,27.2421754756729));
#23952=CARTESIAN_POINT('Ctrl Pts',(126.427594206521,-36.9849433324307,27.2362194177869));
#23953=CARTESIAN_POINT('Ctrl Pts',(126.371595291619,-36.8766737255578,27.2302633599008));
#23954=CARTESIAN_POINT('Ctrl Pts',(126.315676623236,-36.7685592691748,27.2243158370535));
#23955=CARTESIAN_POINT('Ctrl Pts',(126.26452318171,-36.6578066792033,27.2183683142063));
#23956=CARTESIAN_POINT('Ctrl Pts',(126.21838365865,-36.5448633748115,27.212420791359));
#23957=CARTESIAN_POINT('Ctrl Pts',(126.172301362931,-36.4320601552009,27.2064806452876));
#23958=CARTESIAN_POINT('Ctrl Pts',(126.131220750067,-36.3170719829805,27.2005404992162));
#23959=CARTESIAN_POINT('Ctrl Pts',(126.095344190135,-36.2003699456776,27.1946003531448));
#23960=CARTESIAN_POINT('Ctrl Pts',(126.059514012327,-36.083818783723,27.1886678866446));
#23961=CARTESIAN_POINT('Ctrl Pts',(126.028874593329,-35.9655585367119,27.1827354201444));
#23962=CARTESIAN_POINT('Ctrl Pts',(126.003579608631,-35.8460786343174,27.1768029536441));
#23963=CARTESIAN_POINT('Ctrl Pts',(125.97830389398,-35.726689753263,27.1708750065739));
#23964=CARTESIAN_POINT('Ctrl Pts',(125.958364588432,-35.6060834401769,27.1649470595037));
#23965=CARTESIAN_POINT('Ctrl Pts',(125.943865134624,-35.4847627810422,27.1590191124334));
#23966=CARTESIAN_POINT('Ctrl Pts',(125.929375293527,-35.3635225539295,27.1530950954174));
#23967=CARTESIAN_POINT('Ctrl Pts',(125.920318164864,-35.2415693042346,27.1471710784014));
#23968=CARTESIAN_POINT('Ctrl Pts',(125.91674575583,-35.1194143101378,27.1412470613853));
#23969=CARTESIAN_POINT('Ctrl Pts',(125.915567400943,-35.0791216300713,27.1392930313917));
#23970=CARTESIAN_POINT('Ctrl Pts',(125.914985366504,-35.0388070499743,27.1373390013981));
#23971=CARTESIAN_POINT('Ctrl Pts',(125.915000279441,-34.9984890294654,27.1353849714045));
#23972=CARTESIAN_POINT('Ctrl Pts',(125.915000279441,-34.9984890288179,27.1353849713731));
#23973=CARTESIAN_POINT('Ctrl Pts',(125.915048271955,-34.8687384366259,27.1290965537963));
#23974=CARTESIAN_POINT('Ctrl Pts',(125.921282283113,-34.7391739314318,27.1228081362194));
#23975=CARTESIAN_POINT('Ctrl Pts',(125.933624288931,-34.6103673827449,27.1165197186425));
#23976=CARTESIAN_POINT('Ctrl Pts',(125.946018781103,-34.4810130636042,27.1102045585639));
#23977=CARTESIAN_POINT('Ctrl Pts',(125.96457324065,-34.3524234430616,27.1038893984853));
#23978=CARTESIAN_POINT('Ctrl Pts',(125.989158035434,-34.2251634138238,27.0975742384067));
#23979=CARTESIAN_POINT('Ctrl Pts',(126.013796778806,-34.0976241266608,27.0912452204144));
#23980=CARTESIAN_POINT('Ctrl Pts',(126.044492226841,-33.9714205392625,27.0849162024222));
#23981=CARTESIAN_POINT('Ctrl Pts',(126.081064803441,-33.8471028124032,27.0785871844299));
#23982=CARTESIAN_POINT('Ctrl Pts',(126.117752826942,-33.7223926577274,27.0722381879295));
#23983=CARTESIAN_POINT('Ctrl Pts',(126.160355004743,-33.5995805477314,27.0658891914291));
#23984=CARTESIAN_POINT('Ctrl Pts',(126.208642673094,-33.4791993491208,27.0595401949288));
#23985=CARTESIAN_POINT('Ctrl Pts',(126.230161623936,-33.4255525862153,27.056710823616));
#23986=CARTESIAN_POINT('Ctrl Pts',(126.252809073796,-33.3723882700398,27.0538814523033));
#23987=CARTESIAN_POINT('Ctrl Pts',(126.276561884102,-33.3197519239476,27.0510520809905));
#23988=CARTESIAN_POINT('Ctrl Pts',(126.325451445864,-33.211412411272,27.0452284869921));
#23989=CARTESIAN_POINT('Ctrl Pts',(126.379152242892,-33.1050337467732,27.0394048929937));
#23990=CARTESIAN_POINT('Ctrl Pts',(126.437484778255,-33.0010727139704,27.0335812989953));
#23991=CARTESIAN_POINT('Ctrl Pts',(126.495743718499,-32.897242843382,27.0277650523218));
#23992=CARTESIAN_POINT('Ctrl Pts',(126.558622576199,-32.7958248906842,27.0219488056483));
#23993=CARTESIAN_POINT('Ctrl Pts',(126.625894126307,-32.6972549960733,27.0161325589748));
#23994=CARTESIAN_POINT('Ctrl Pts',(126.693098337262,-32.5987837704124,27.0103221343928));
#23995=CARTESIAN_POINT('Ctrl Pts',(126.764686264268,-32.5031552666232,27.0045117098109));
#23996=CARTESIAN_POINT('Ctrl Pts',(126.840385476788,-32.4107798346396,26.9987012852289));
#23997=CARTESIAN_POINT('Ctrl Pts',(126.918950054951,-32.3149078089642,26.9926709245286));
#23998=CARTESIAN_POINT('Ctrl Pts',(127.001943089565,-32.2225403823583,26.9866405638283));
#23999=CARTESIAN_POINT('Ctrl Pts',(127.089011280693,-32.1341022914157,26.9806102031281));
#24000=CARTESIAN_POINT('Ctrl Pts',(127.17280954026,-32.0489855799698,26.9748063185556));
#24001=CARTESIAN_POINT('Ctrl Pts',(127.260382071063,-31.9675087036601,26.9690024339831));
#24002=CARTESIAN_POINT('Ctrl Pts',(127.35137428117,-31.8900149837096,26.9631985494106));
#24003=CARTESIAN_POINT('Ctrl Pts',(127.442353050778,-31.8125327103898,26.9573955221324));
#24004=CARTESIAN_POINT('Ctrl Pts',(127.536750184372,-31.7390326880646,26.9515924948542));
#24005=CARTESIAN_POINT('Ctrl Pts',(127.634176737621,-31.6698190302651,26.945789467576));
#24006=CARTESIAN_POINT('Ctrl Pts',(127.731611892633,-31.6005992616106,26.9399859279501));
#24007=CARTESIAN_POINT('Ctrl Pts',(127.832076666188,-31.5356668464153,26.9341823883242));
#24008=CARTESIAN_POINT('Ctrl Pts',(127.935152305295,-31.4752831322686,26.9283788486983));
#24009=CARTESIAN_POINT('Ctrl Pts',(128.03826137064,-31.4148798363808,26.9225734270515));
#24010=CARTESIAN_POINT('Ctrl Pts',(128.143982633231,-31.3590283814611,26.9167680054048));
#24011=CARTESIAN_POINT('Ctrl Pts',(128.251872449618,-31.3079443303769,26.910962583758));
#24012=CARTESIAN_POINT('Ctrl Pts',(128.359881743972,-31.2568037084433,26.9051507331451));
#24013=CARTESIAN_POINT('Ctrl Pts',(128.470064016391,-31.2104412034413,26.8993388825322));
#24014=CARTESIAN_POINT('Ctrl Pts',(128.58195519626,-31.1690244147754,26.8935270319193));
#24015=CARTESIAN_POINT('Ctrl Pts',(128.693919866853,-31.1275804233417,26.8877113640519));
#24016=CARTESIAN_POINT('Ctrl Pts',(128.807595292322,-31.0910887419833,26.8818956961845));
#24017=CARTESIAN_POINT('Ctrl Pts',(128.922503381796,-31.0596667605696,26.8760800283171));
#24018=CARTESIAN_POINT('Ctrl Pts',(129.037576064641,-31.028199770577,26.8702560301365));
#24019=CARTESIAN_POINT('Ctrl Pts',(129.153884538841,-31.0018170646865,26.8644320319559));
#24020=CARTESIAN_POINT('Ctrl Pts',(129.270941565394,-30.9805847690329,26.8586080337753));
#24021=CARTESIAN_POINT('Ctrl Pts',(129.301997365361,-30.9749517374578,26.8570628986576));
#24022=CARTESIAN_POINT('Ctrl Pts',(129.333105833546,-30.9696809423615,26.8555177635399));
#24023=CARTESIAN_POINT('Ctrl Pts',(129.364257843974,-30.9647730037764,26.8539726284221));
#24024=CARTESIAN_POINT('Ctrl Pts',(129.481684253281,-30.946272701638,26.8481482958581));
#24025=CARTESIAN_POINT('Ctrl Pts',(129.600108263132,-30.9328725377778,26.8423239632941));
#24026=CARTESIAN_POINT('Ctrl Pts',(129.719049255623,-30.9246728132291,26.8364996307302));
#24027=CARTESIAN_POINT('Ctrl Pts',(129.841350909668,-30.9162414065793,26.8305107324423));
#24028=CARTESIAN_POINT('Ctrl Pts',(129.964198789592,-30.9133088376121,26.8245218341545));
#24029=CARTESIAN_POINT('Ctrl Pts',(130.087058565302,-30.9159277912594,26.8185329358666));
#24030=CARTESIAN_POINT('Ctrl Pts',(130.206242809622,-30.9184683950457,26.8127232043038));
#24031=CARTESIAN_POINT('Ctrl Pts',(130.325437801707,-30.9262331086285,26.8069134727409));
#24032=CARTESIAN_POINT('Ctrl Pts',(130.444151130485,-30.9392174678655,26.801103741178));
#24033=CARTESIAN_POINT('Ctrl Pts',(130.562785662325,-30.9521932086283,26.7952978658718));
#24034=CARTESIAN_POINT('Ctrl Pts',(130.680938762273,-30.9703816604703,26.7894919905656));
#24035=CARTESIAN_POINT('Ctrl Pts',(130.79812060953,-30.9937263582421,26.7836861152593));
#24036=CARTESIAN_POINT('Ctrl Pts',(130.915252332796,-31.0170610704281,26.7778827233893));
#24037=CARTESIAN_POINT('Ctrl Pts',(131.031413230179,-31.0455475608967,26.7720793315192));
#24038=CARTESIAN_POINT('Ctrl Pts',(131.14612180951,-31.0790779403606,26.7662759396491));
#24039=CARTESIAN_POINT('Ctrl Pts',(131.26080839399,-31.1126018905265,26.7604736605531));
#24040=CARTESIAN_POINT('Ctrl Pts',(131.374042823382,-31.1511676892085,26.7546713814571));
#24041=CARTESIAN_POINT('Ctrl Pts',(131.485357570412,-31.1946172481577,26.7488691023611));
#24042=CARTESIAN_POINT('Ctrl Pts',(131.596710416444,-31.2380816783154,26.7430648373553));
#24043=CARTESIAN_POINT('Ctrl Pts',(131.706141886445,-31.286433060929,26.7372605723496));
#24044=CARTESIAN_POINT('Ctrl Pts',(131.813203480861,-31.3394647745183,26.7314563073438));
#24045=CARTESIAN_POINT('Ctrl Pts',(131.920288081564,-31.392507884004,26.7256507950693));
#24046=CARTESIAN_POINT('Ctrl Pts',(132.025001431504,-31.4502331367428,26.7198452827947));
#24047=CARTESIAN_POINT('Ctrl Pts',(132.126919781745,-31.5123880316151,26.7140397705201));
#24048=CARTESIAN_POINT('Ctrl Pts',(132.228918116506,-31.5745917050384,26.7082297021366));
#24049=CARTESIAN_POINT('Ctrl Pts',(132.328116731462,-31.6412317367213,26.702419633753));
#24050=CARTESIAN_POINT('Ctrl Pts',(132.42412112861,-31.712012507045,26.6966095653694));
#24051=CARTESIAN_POINT('Ctrl Pts',(132.445290832453,-31.7276202082552,26.6953284008536));
#24052=CARTESIAN_POINT('Ctrl Pts',(132.466305349192,-31.7434290916029,26.6940472363378));
#24053=CARTESIAN_POINT('Ctrl Pts',(132.487160670875,-31.7594357285724,26.6927660718219));
#24054=CARTESIAN_POINT('',(125.915000003014,-35.0001569306028,27.2396150285593));
#24055=CARTESIAN_POINT('Ctrl Pts',(125.915000003014,-35.0001569306028,27.2396150285593));
#24056=CARTESIAN_POINT('Ctrl Pts',(125.914995442009,-34.8814311542579,27.233798040467));
#24057=CARTESIAN_POINT('Ctrl Pts',(125.92017111884,-34.7625116039888,27.2279810523747));
#24058=CARTESIAN_POINT('Ctrl Pts',(125.930551771801,-34.6438874924847,27.2221640642824));
#24059=CARTESIAN_POINT('Ctrl Pts',(125.94091932464,-34.5254130816157,27.2163544170823));
#24060=CARTESIAN_POINT('Ctrl Pts',(125.956478754177,-34.4072337721956,27.2105447698822));
#24061=CARTESIAN_POINT('Ctrl Pts',(125.977202804404,-34.2898396497237,27.2047351226821));
#24062=CARTESIAN_POINT('Ctrl Pts',(125.997906137868,-34.1725628800947,27.1989312830863));
#24063=CARTESIAN_POINT('Ctrl Pts',(126.023763750967,-34.0560701368371,27.1931274434906));
#24064=CARTESIAN_POINT('Ctrl Pts',(126.054696570661,-33.9408466350681,27.1873236038948));
#24065=CARTESIAN_POINT('Ctrl Pts',(126.086567252157,-33.822129636033,27.1813437958773));
#24066=CARTESIAN_POINT('Ctrl Pts',(126.123825766704,-33.7047605122388,27.1753639878597));
#24067=CARTESIAN_POINT('Ctrl Pts',(126.166328678678,-33.5892593434404,27.1693841798421));
#24068=CARTESIAN_POINT('Ctrl Pts',(126.207534872779,-33.4772819903711,27.1635868092992));
#24069=CARTESIAN_POINT('Ctrl Pts',(126.253669957725,-33.3670606804676,27.1577894387562));
#24070=CARTESIAN_POINT('Ctrl Pts',(126.304552755601,-33.2590535149335,27.1519920682133));
#24071=CARTESIAN_POINT('Ctrl Pts',(126.355428250343,-33.1510618515125,27.1461955297586));
#24072=CARTESIAN_POINT('Ctrl Pts',(126.411049928465,-33.045284070752,27.1403989913039));
#24073=CARTESIAN_POINT('Ctrl Pts',(126.47118915546,-32.9421567058065,27.1346024528492));
#24074=CARTESIAN_POINT('Ctrl Pts',(126.531334034412,-32.8390196488263,27.1288053696288));
#24075=CARTESIAN_POINT('Ctrl Pts',(126.595997100056,-32.7385338565421,27.1230082864084));
#24076=CARTESIAN_POINT('Ctrl Pts',(126.664904942831,-32.641109167501,27.1172112031881));
#24077=CARTESIAN_POINT('Ctrl Pts',(126.73383562791,-32.5436521830885,27.1114121982889));
#24078=CARTESIAN_POINT('Ctrl Pts',(126.80701365207,-32.4492586539039,27.1056131933898));
#24079=CARTESIAN_POINT('Ctrl Pts',(126.88412407846,-32.358306936534,27.0998141884906));
#24080=CARTESIAN_POINT('Ctrl Pts',(126.961320033087,-32.2672543386412,27.0940087515343));
#24081=CARTESIAN_POINT('Ctrl Pts',(127.042456830683,-32.1796514845169,27.088203314578));
#24082=CARTESIAN_POINT('Ctrl Pts',(127.127181197167,-32.0958414082406,27.0823978776217));
#24083=CARTESIAN_POINT('Ctrl Pts',(127.211961991813,-32.011975512739,27.0765885741256));
#24084=CARTESIAN_POINT('Ctrl Pts',(127.300334810834,-31.9319076995307,27.0707792706295));
#24085=CARTESIAN_POINT('Ctrl Pts',(127.391912963374,-31.8559409977894,27.0649699671334));
#24086=CARTESIAN_POINT('Ctrl Pts',(127.483621027563,-31.779866530612,27.0591524226302));
#24087=CARTESIAN_POINT('Ctrl Pts',(127.57854317475,-31.7079050316072,27.0533348781271));
#24088=CARTESIAN_POINT('Ctrl Pts',(127.676263350047,-31.6403165354951,27.0475173336239));
#24089=CARTESIAN_POINT('Ctrl Pts',(127.6970313371,-31.6259522856575,27.0462809595738));
#24090=CARTESIAN_POINT('Ctrl Pts',(127.717925614027,-31.6117853855417,27.0450445855236));
#24091=CARTESIAN_POINT('Ctrl Pts',(127.738942050042,-31.5978180608714,27.0438082114734));
#24092=CARTESIAN_POINT('Ctrl Pts',(127.837934092804,-31.5320288851969,27.0379846173701));
#24093=CARTESIAN_POINT('Ctrl Pts',(127.939959515866,-31.4704577087745,27.0321610232669));
#24094=CARTESIAN_POINT('Ctrl Pts',(128.044623506418,-31.4133960675386,27.0263374291637));
#24095=CARTESIAN_POINT('Ctrl Pts',(128.149155448049,-31.3564064179026,27.0205211823755));
#24096=CARTESIAN_POINT('Ctrl Pts',(128.256318980633,-31.3039151810317,27.0147049355874));
#24097=CARTESIAN_POINT('Ctrl Pts',(128.365689833025,-31.2561710404826,27.0088886887992));
#24098=CARTESIAN_POINT('Ctrl Pts',(128.474951204838,-31.2084746919733,27.003078264093));
#24099=CARTESIAN_POINT('Ctrl Pts',(128.586415128783,-31.1655161489778,26.9972678393867));
#24100=CARTESIAN_POINT('Ctrl Pts',(128.699632747665,-31.1274982234923,26.9914574146805));
#24101=CARTESIAN_POINT('Ctrl Pts',(128.817135875086,-31.0880412450935,26.9854270540232));
#24102=CARTESIAN_POINT('Ctrl Pts',(128.936527688634,-31.0539065129513,26.9793966933659));
#24103=CARTESIAN_POINT('Ctrl Pts',(129.057283182286,-31.0252660464379,26.9733663327086));
#24104=CARTESIAN_POINT('Ctrl Pts',(129.17350358838,-30.9977011999184,26.9675624479884));
#24105=CARTESIAN_POINT('Ctrl Pts',(129.29098666009,-30.9752254791916,26.9617585632682));
#24106=CARTESIAN_POINT('Ctrl Pts',(129.40924956635,-30.9579412516463,26.955954678548));
#24107=CARTESIAN_POINT('Ctrl Pts',(129.527495004119,-30.9406595771364,26.9501516511137));
#24108=CARTESIAN_POINT('Ctrl Pts',(129.646519643429,-30.9285679298605,26.9443486236793));
#24109=CARTESIAN_POINT('Ctrl Pts',(129.7658323915,-30.9217172080483,26.938545596245));
#24110=CARTESIAN_POINT('Ctrl Pts',(129.885155673832,-30.9148658813779,26.9327420564546));
#24111=CARTESIAN_POINT('Ctrl Pts',(130.004766707816,-30.9132564235935,26.9269385166643));
#24112=CARTESIAN_POINT('Ctrl Pts',(130.124171878948,-30.9168876644796,26.9211349768739));
#24113=CARTESIAN_POINT('Ctrl Pts',(130.243615771964,-30.9205200829403,26.9153295550545));
#24114=CARTESIAN_POINT('Ctrl Pts',(130.362853261423,-30.9293965675983,26.9095241332352));
#24115=CARTESIAN_POINT('Ctrl Pts',(130.481393981588,-30.9434639364982,26.9037187114158));
#24116=CARTESIAN_POINT('Ctrl Pts',(130.600065974837,-30.9575468837317,26.8979068606189));
#24117=CARTESIAN_POINT('Ctrl Pts',(130.718039252864,-30.9768321414227,26.8920950098221));
#24118=CARTESIAN_POINT('Ctrl Pts',(130.834831637392,-31.0012150423897,26.8862831590252));
#24119=CARTESIAN_POINT('Ctrl Pts',(130.951700731915,-31.0256139582044,26.880467490967));
#24120=CARTESIAN_POINT('Ctrl Pts',(131.067386993512,-31.0551170845753,26.8746518229088));
#24121=CARTESIAN_POINT('Ctrl Pts',(131.181423052239,-31.0895697715419,26.8688361548507));
#24122=CARTESIAN_POINT('Ctrl Pts',(131.295622455409,-31.1240718082937,26.8630121564707));
#24123=CARTESIAN_POINT('Ctrl Pts',(131.408166553851,-31.1635374216842,26.8571881580907));
#24124=CARTESIAN_POINT('Ctrl Pts',(131.518607473302,-31.2077636753452,26.8513641597107));
#24125=CARTESIAN_POINT('Ctrl Pts',(131.547907958044,-31.219497104196,26.8498190261087));
#24126=CARTESIAN_POINT('Ctrl Pts',(131.577060541274,-31.2315653670552,26.8482738925068));
#24127=CARTESIAN_POINT('Ctrl Pts',(131.606057163059,-31.2439641390173,26.8467287589049));
#24128=CARTESIAN_POINT('Ctrl Pts',(131.71534415369,-31.2906945645586,26.8409052183997));
#24129=CARTESIAN_POINT('Ctrl Pts',(131.822766155584,-31.3422740861352,26.8350816778945));
#24130=CARTESIAN_POINT('Ctrl Pts',(131.927862926942,-31.3985323082215,26.8292581373893));
#24131=CARTESIAN_POINT('Ctrl Pts',(132.032811661674,-31.4547112864148,26.8234427997744));
#24132=CARTESIAN_POINT('Ctrl Pts',(132.135441326964,-31.5155556592987,26.8176274621594));
#24133=CARTESIAN_POINT('Ctrl Pts',(132.235311565566,-31.5808470047619,26.8118121245445));
#24134=CARTESIAN_POINT('Ctrl Pts',(132.321400919049,-31.6371289341695,26.806799233191));
#24135=CARTESIAN_POINT('Ctrl Pts',(132.405439988716,-31.6967144091857,26.8017863418376));
#24136=CARTESIAN_POINT('Ctrl Pts',(132.487160670875,-31.7594357285724,26.7967734504842));
#24137=CARTESIAN_POINT('Ctrl Pts',(132.487160670875,-31.7594357285724,28.0469635236591));
#24138=CARTESIAN_POINT('Ctrl Pts',(132.583285464304,-31.8332123260063,28.0410441738779));
#24139=CARTESIAN_POINT('Ctrl Pts',(132.675995739581,-31.9111704788722,28.0351248240968));
#24140=CARTESIAN_POINT('Ctrl Pts',(132.764929491174,-31.9929433146618,28.0292054743156));
#24141=CARTESIAN_POINT('Ctrl Pts',(132.852423570101,-32.0733923997447,28.0233819478403));
#24142=CARTESIAN_POINT('Ctrl Pts',(132.936544708698,-32.1577930401039,28.017558421365));
#24143=CARTESIAN_POINT('Ctrl Pts',(133.016915641834,-32.2458313395763,28.0117348948897));
#24144=CARTESIAN_POINT('Ctrl Pts',(133.097185160871,-32.3337585500728,28.0059187166889));
#24145=CARTESIAN_POINT('Ctrl Pts',(133.1737136136,-32.4253139911846,28.0001025384881));
#24146=CARTESIAN_POINT('Ctrl Pts',(133.246158326206,-32.5201449394763,27.9942863602873));
#24147=CARTESIAN_POINT('Ctrl Pts',(133.318530509731,-32.6148809463805,27.9884760050381));
#24148=CARTESIAN_POINT('Ctrl Pts',(133.386826840217,-32.7128856140347,27.982665649789));
#24149=CARTESIAN_POINT('Ctrl Pts',(133.450743329231,-32.8137714035883,27.9768552945399));
#24150=CARTESIAN_POINT('Ctrl Pts',(133.517080258284,-32.9184776158247,27.9708249081735));
#24151=CARTESIAN_POINT('Ctrl Pts',(133.57869876802,-33.0262871414312,27.9647945218072));
#24152=CARTESIAN_POINT('Ctrl Pts',(133.635306602846,-33.1367311242586,27.9587641354408));
#24153=CARTESIAN_POINT('Ctrl Pts',(133.689787576045,-33.2430255212621,27.9529603219047));
#24154=CARTESIAN_POINT('Ctrl Pts',(133.739627399038,-33.3517595880501,27.9471565083687));
#24155=CARTESIAN_POINT('Ctrl Pts',(133.784611529896,-33.4624888397864,27.9413526948326));
#24156=CARTESIAN_POINT('Ctrl Pts',(133.829589012122,-33.5732017257961,27.9355497390972));
#24157=CARTESIAN_POINT('Ctrl Pts',(133.869712075777,-33.6859088320985,27.9297467833618));
#24158=CARTESIAN_POINT('Ctrl Pts',(133.904814193391,-33.8001453775171,27.9239438276264));
#24159=CARTESIAN_POINT('Ctrl Pts',(133.939919407601,-33.9143920005167,27.9181403599728));
#24160=CARTESIAN_POINT('Ctrl Pts',(133.970002675169,-34.0301679405346,27.9123368923193));
#24161=CARTESIAN_POINT('Ctrl Pts',(133.994947433845,-34.1469935517149,27.9065334246658));
#24162=CARTESIAN_POINT('Ctrl Pts',(134.019900280401,-34.2638570414536,27.9007280753445));
#24163=CARTESIAN_POINT('Ctrl Pts',(134.039711219411,-34.3817704800661,27.8949227260232));
#24164=CARTESIAN_POINT('Ctrl Pts',(134.054314974779,-34.5002449747268,27.8891173767019));
#24165=CARTESIAN_POINT('Ctrl Pts',(134.068934902246,-34.6188506672473,27.8833055985757));
#24166=CARTESIAN_POINT('Ctrl Pts',(134.078336085858,-34.7380182504821,27.8774938204496));
#24167=CARTESIAN_POINT('Ctrl Pts',(134.082505201968,-34.8572545065437,27.8716820423234));
#24168=CARTESIAN_POINT('Ctrl Pts',(134.086677056282,-34.976569074918,27.8658664471218));
#24169=CARTESIAN_POINT('Ctrl Pts',(134.085610003201,-35.09595199855,27.8600508519202));
#24170=CARTESIAN_POINT('Ctrl Pts',(134.079342791129,-35.214912522814,27.8542352567186));
#24171=CARTESIAN_POINT('Ctrl Pts',(134.073066601531,-35.3340434531873,27.8484113309136));
#24172=CARTESIAN_POINT('Ctrl Pts',(134.061575424321,-35.4527503715008,27.8425874051085));
#24173=CARTESIAN_POINT('Ctrl Pts',(134.044959550162,-35.5705499430857,27.8367634793035));
#24174=CARTESIAN_POINT('Ctrl Pts',(134.040549271268,-35.6018169687812,27.835217660118));
#24175=CARTESIAN_POINT('Ctrl Pts',(134.035778229449,-35.6330201415283,27.8336718409326));
#24176=CARTESIAN_POINT('Ctrl Pts',(134.030648706208,-35.6641505907097,27.8321260217471));
#24177=CARTESIAN_POINT('Ctrl Pts',(134.011324098236,-35.7814292729995,27.8263024103989));
#24178=CARTESIAN_POINT('Ctrl Pts',(133.986845442312,-35.8980529423074,27.8204787990506));
#24179=CARTESIAN_POINT('Ctrl Pts',(133.957268484404,-36.013533986771,27.8146551877024));
#24180=CARTESIAN_POINT('Ctrl Pts',(133.927728841429,-36.1288693378441,27.8088389235485));
#24181=CARTESIAN_POINT('Ctrl Pts',(133.893103790243,-36.2430645392233,27.8030226593946));
#24182=CARTESIAN_POINT('Ctrl Pts',(133.853500512317,-36.3556396282095,27.7972063952408));
#24183=CARTESIAN_POINT('Ctrl Pts',(133.813936876611,-36.4681020314088,27.7913959530703));
#24184=CARTESIAN_POINT('Ctrl Pts',(133.7694050622,-36.5789471654182,27.7855855108999));
#24185=CARTESIAN_POINT('Ctrl Pts',(133.720062574716,-36.6877083397909,27.7797750687295));
#24186=CARTESIAN_POINT('Ctrl Pts',(133.668852586673,-36.8005858764355,27.7737447145815));
#24187=CARTESIAN_POINT('Ctrl Pts',(133.612460696619,-36.9112181565411,27.7677143604336));
#24188=CARTESIAN_POINT('Ctrl Pts',(133.551118839586,-37.0191037583881,27.7616840062856));
#24189=CARTESIAN_POINT('Ctrl Pts',(133.492080491692,-37.1229380406002,27.7558801039695));
#24190=CARTESIAN_POINT('Ctrl Pts',(133.428457455569,-37.2242278244811,27.7500762016534));
#24191=CARTESIAN_POINT('Ctrl Pts',(133.36050389423,-37.3225500160098,27.7442722993372));
#24192=CARTESIAN_POINT('Ctrl Pts',(133.292560370003,-37.4208576848121,27.7384692542893));
#24193=CARTESIAN_POINT('Ctrl Pts',(133.220287824704,-37.5161982971386,27.7326662092413));
#24194=CARTESIAN_POINT('Ctrl Pts',(133.143983715939,-37.6081777918516,27.7268631641934));
#24195=CARTESIAN_POINT('Ctrl Pts',(133.06767287024,-37.7001654074883,27.7210596067912));
#24196=CARTESIAN_POINT('Ctrl Pts',(132.987330014086,-37.7887910012047,27.715256049389));
#24197=CARTESIAN_POINT('Ctrl Pts',(132.903292426176,-37.8736941535434,27.7094524919868));
#24198=CARTESIAN_POINT('Ctrl Pts',(132.819227586119,-37.9586248387187,27.7036470525767));
#24199=CARTESIAN_POINT('Ctrl Pts',(132.731465918567,-38.0398303917396,27.6978416131667));
#24200=CARTESIAN_POINT('Ctrl Pts',(132.640380548991,-38.1169882188601,27.6920361737567));
#24201=CARTESIAN_POINT('Ctrl Pts',(132.549194312839,-38.1942314894038,27.6862243054899));
#24202=CARTESIAN_POINT('Ctrl Pts',(132.454677339591,-38.2674178227229,27.6804124372231));
#24203=CARTESIAN_POINT('Ctrl Pts',(132.357234850278,-38.3362657059409,27.6746005689564));
#24204=CARTESIAN_POINT('Ctrl Pts',(132.259728361135,-38.405158808168,27.6687848834782));
#24205=CARTESIAN_POINT('Ctrl Pts',(132.159292871994,-38.4697075652274,27.662969198));
#24206=CARTESIAN_POINT('Ctrl Pts',(132.056360087618,-38.5296753660996,27.6571535125219));
#24207=CARTESIAN_POINT('Ctrl Pts',(131.953279867147,-38.5897290620387,27.6513294969285));
#24208=CARTESIAN_POINT('Ctrl Pts',(131.847695572142,-38.6451885160911,27.645505481335));
#24209=CARTESIAN_POINT('Ctrl Pts',(131.740060955099,-38.695864293036,27.6396814657416));
#24210=CARTESIAN_POINT('Ctrl Pts',(131.711508186047,-38.7093073078893,27.6381365002207));
#24211=CARTESIAN_POINT('Ctrl Pts',(131.682811226506,-38.7224139605503,27.6365915346997));
#24212=CARTESIAN_POINT('Ctrl Pts',(131.653978731678,-38.7351813015111,27.6350465691787));
#24213=CARTESIAN_POINT('Ctrl Pts',(131.545297395498,-38.7833065741717,27.6292229691686));
#24214=CARTESIAN_POINT('Ctrl Pts',(131.434338636625,-38.8267621156396,27.6233993691585));
#24215=CARTESIAN_POINT('Ctrl Pts',(131.32154083558,-38.8653272590938,27.6175757691484));
#24216=CARTESIAN_POINT('Ctrl Pts',(131.208885342653,-38.9038437479384,27.6117595163166));
#24217=CARTESIAN_POINT('Ctrl Pts',(131.0943958053,-38.9374819794818,27.6059432634847));
#24218=CARTESIAN_POINT('Ctrl Pts',(130.978532401663,-38.966068499017,27.6001270106529));
#24219=CARTESIAN_POINT('Ctrl Pts',(130.862784974987,-38.9946264040154,27.5943165797744));
#24220=CARTESIAN_POINT('Ctrl Pts',(130.745666812013,-39.0181425593596,27.5885061488959));
#24221=CARTESIAN_POINT('Ctrl Pts',(130.627654576307,-39.0364928753611,27.5826957180173));
#24222=CARTESIAN_POINT('Ctrl Pts',(130.505175522547,-39.0555377593652,27.5766653596254));
#24223=CARTESIAN_POINT('Ctrl Pts',(130.381733800796,-39.0690178737889,27.5706350012334));
#24224=CARTESIAN_POINT('Ctrl Pts',(130.257875926543,-39.076852340533,27.5646046428414));
#24225=CARTESIAN_POINT('Ctrl Pts',(130.138669475346,-39.0843925876366,27.5588007516663));
#24226=CARTESIAN_POINT('Ctrl Pts',(130.019078008971,-39.086703551476,27.5529968604911));
#24227=CARTESIAN_POINT('Ctrl Pts',(129.899594712356,-39.0837658819052,27.5471929693159));
#24228=CARTESIAN_POINT('Ctrl Pts',(129.780129062552,-39.0808286462068,27.5413899353331));
#24229=CARTESIAN_POINT('Ctrl Pts',(129.660771958839,-39.07264432873,27.5355869013503));
#24230=CARTESIAN_POINT('Ctrl Pts',(129.542016036404,-39.0592457044491,27.5297838673675));
#24231=CARTESIAN_POINT('Ctrl Pts',(129.423249627108,-39.0458458969894,27.5239803209419));
#24232=CARTESIAN_POINT('Ctrl Pts',(129.305084910422,-39.0272309130128,27.5181767745164));
#24233=CARTESIAN_POINT('Ctrl Pts',(129.18800821304,-39.0034852738469,27.5123732280909));
#24234=CARTESIAN_POINT('Ctrl Pts',(129.070893547304,-38.979731933893,27.5065677995564));
#24235=CARTESIAN_POINT('Ctrl Pts',(128.954868002589,-38.9508447107762,27.5007623710218));
#24236=CARTESIAN_POINT('Ctrl Pts',(128.840405919094,-38.9169588416945,27.4949569424873));
#24237=CARTESIAN_POINT('Ctrl Pts',(128.725817077699,-38.8830354466347,27.4891450848899));
#24238=CARTESIAN_POINT('Ctrl Pts',(128.612795545343,-38.8441024720326,27.4833332272925));
#24239=CARTESIAN_POINT('Ctrl Pts',(128.50179889693,-38.8003445179036,27.4775213696951));
#24240=CARTESIAN_POINT('Ctrl Pts',(128.39072934418,-38.7565578228647,27.4717056947785));
#24241=CARTESIAN_POINT('Ctrl Pts',(128.281687696141,-38.7079400028129,27.465890019862));
#24242=CARTESIAN_POINT('Ctrl Pts',(128.175108490418,-38.6547224215056,27.4600743449455));
#24243=CARTESIAN_POINT('Ctrl Pts',(128.06837662097,-38.6014286114995,27.4542503396742));
#24244=CARTESIAN_POINT('Ctrl Pts',(127.964114589634,-38.5435220871408,27.4484263344029));
#24245=CARTESIAN_POINT('Ctrl Pts',(127.86272956321,-38.4812785122744,27.4426023291316));
#24246=CARTESIAN_POINT('Ctrl Pts',(127.835832772996,-38.4647656953982,27.4410572582911));
#24247=CARTESIAN_POINT('Ctrl Pts',(127.809138293843,-38.4479478588015,27.4395121874507));
#24248=CARTESIAN_POINT('Ctrl Pts',(127.782653338569,-38.4308306258164,27.4379671166102));
#24249=CARTESIAN_POINT('Ctrl Pts',(127.682827870727,-38.3663134018596,27.4321435304308));
#24250=CARTESIAN_POINT('Ctrl Pts',(127.585659606409,-38.2973316490775,27.4263199442514));
#24251=CARTESIAN_POINT('Ctrl Pts',(127.491573408628,-38.22413105126,27.4204963580719));
#24252=CARTESIAN_POINT('Ctrl Pts',(127.397605916506,-38.1510228083828,27.4146801193319));
#24253=CARTESIAN_POINT('Ctrl Pts',(127.306713076136,-38.0737065559006,27.4088638805918));
#24254=CARTESIAN_POINT('Ctrl Pts',(127.219292212636,-37.9924720886408,27.4030476418517));
#24255=CARTESIAN_POINT('Ctrl Pts',(127.131958859535,-37.9113189390471,27.3972372253073));
#24256=CARTESIAN_POINT('Ctrl Pts',(127.048090866573,-37.8262556538245,27.3914268087628));
#24257=CARTESIAN_POINT('Ctrl Pts',(126.968053308347,-37.737612876024,27.3856163922184));
#24258=CARTESIAN_POINT('Ctrl Pts',(126.884986013602,-37.6456146202838,27.3795860285444));
#24259=CARTESIAN_POINT('Ctrl Pts',(126.806045231511,-37.5497607967383,27.3735556648704));
#24260=CARTESIAN_POINT('Ctrl Pts',(126.731598189897,-37.4504641616877,27.3675253011963));
#24261=CARTESIAN_POINT('Ctrl Pts',(126.659947217293,-37.3548968923447,27.3617214248698));
#24262=CARTESIAN_POINT('Ctrl Pts',(126.592458789477,-37.256141112707,27.3559175485433));
#24263=CARTESIAN_POINT('Ctrl Pts',(126.529419436531,-37.154598698707,27.3501136722168));
#24264=CARTESIAN_POINT('Ctrl Pts',(126.46638939585,-37.0530712846997,27.3443106532473));
#24265=CARTESIAN_POINT('Ctrl Pts',(126.407807338344,-36.9487584017903,27.3385076342779));
#24266=CARTESIAN_POINT('Ctrl Pts',(126.353915896904,-36.8420900393705,27.3327046153084));
#24267=CARTESIAN_POINT('Ctrl Pts',(126.300019697896,-36.7354122602064,27.326901084045));
#24268=CARTESIAN_POINT('Ctrl Pts',(126.250815122409,-36.6263789525728,27.3210975527817));
#24269=CARTESIAN_POINT('Ctrl Pts',(126.206498066165,-36.5154431952367,27.3152940215184));
#24270=CARTESIAN_POINT('Ctrl Pts',(126.162166638734,-36.404471463524,27.3094886082791));
#24271=CARTESIAN_POINT('Ctrl Pts',(126.122726034021,-36.2915964341819,27.3036831950399));
#24272=CARTESIAN_POINT('Ctrl Pts',(126.088323159943,-36.1772889615392,27.2978777818007));
#24273=CARTESIAN_POINT('Ctrl Pts',(126.053882187963,-36.0628549042724,27.29206593962));
#24274=CARTESIAN_POINT('Ctrl Pts',(126.024490200144,-35.9469856285703,27.2862540974393));
#24275=CARTESIAN_POINT('Ctrl Pts',(126.000243628667,-35.8301650257512,27.2804422552586));
#24276=CARTESIAN_POINT('Ctrl Pts',(125.975981131991,-35.7132676949128,27.2746265958477));
#24277=CARTESIAN_POINT('Ctrl Pts',(125.956870847267,-35.595418194732,27.2688109364367));
#24278=CARTESIAN_POINT('Ctrl Pts',(125.942957466631,-35.4771067830487,27.2629952770258));
#24279=CARTESIAN_POINT('Ctrl Pts',(125.929024156488,-35.3586259022743,27.2571712872729));
#24280=CARTESIAN_POINT('Ctrl Pts',(125.920302638081,-35.2396821951967,27.25134729752));
#24281=CARTESIAN_POINT('Ctrl Pts',(125.91678554855,-35.12076731126,27.2455233077671));
#24282=CARTESIAN_POINT('Ctrl Pts',(125.915852398212,-35.0892169446464,27.243978093192));
#24283=CARTESIAN_POINT('Ctrl Pts',(125.915285325465,-35.0576685843124,27.2424328786169));
#24284=CARTESIAN_POINT('Ctrl Pts',(125.915083580701,-35.0261313479364,27.2408876640418));
#24285=CARTESIAN_POINT('Ctrl Pts',(125.915028195182,-35.0174733476091,27.2404634522263));
#24286=CARTESIAN_POINT('Ctrl Pts',(125.915000335634,-35.0088151710232,27.2400392404109));
#24287=CARTESIAN_POINT('Ctrl Pts',(125.915000003014,-35.0001569313426,27.2396150285955));
#24288=CARTESIAN_POINT('Origin',(130.,-35.,32.7603849714045));
#24289=CARTESIAN_POINT('',(132.487160670875,-31.7594357285724,29.296931249476));
#24290=CARTESIAN_POINT('',(132.487160670875,-31.7594357285724,29.1925548588025));
#24291=CARTESIAN_POINT('',(132.487160670875,-31.7594357285724,32.7603849714045));
#24292=CARTESIAN_POINT('',(125.917751433657,-35.0038808860531,29.7396160660207));
#24293=CARTESIAN_POINT('Ctrl Pts',(125.915001825726,-35.0038621470065,29.7396150285955));
#24294=CARTESIAN_POINT('Ctrl Pts',(125.914889706146,-34.88527311404,29.7338556330042));
#24295=CARTESIAN_POINT('Ctrl Pts',(125.919945886409,-34.7666043470561,29.7280962374129));
#24296=CARTESIAN_POINT('Ctrl Pts',(125.930164310688,-34.6483432611132,29.7223368418217));
#24297=CARTESIAN_POINT('Ctrl Pts',(125.940380151039,-34.5301120797944,29.716578902606));
#24298=CARTESIAN_POINT('Ctrl Pts',(125.955755605104,-34.4122887877864,29.7108209633903));
#24299=CARTESIAN_POINT('Ctrl Pts',(125.976232588964,-34.2953576638563,29.7050630241746));
#24300=CARTESIAN_POINT('Ctrl Pts',(125.99670941053,-34.1784274666885,29.6993051305947));
#24301=CARTESIAN_POINT('Ctrl Pts',(126.022287609829,-34.0623898323388,29.6935472370148));
#24302=CARTESIAN_POINT('Ctrl Pts',(126.052857746502,-33.9477200797059,29.6877893434349));
#24303=CARTESIAN_POINT('Ctrl Pts',(126.083435129142,-33.8330231471781,29.6820300850753));
#24304=CARTESIAN_POINT('Ctrl Pts',(126.11900669447,-33.7196951418414,29.6762708267158));
#24305=CARTESIAN_POINT('Ctrl Pts',(126.159412985297,-33.6081967155889,29.6705115683562));
#24306=CARTESIAN_POINT('Ctrl Pts',(126.199864385646,-33.4965738126658,29.6647458803696));
#24307=CARTESIAN_POINT('Ctrl Pts',(126.245161147391,-33.3867849580306,29.6589801923829));
#24308=CARTESIAN_POINT('Ctrl Pts',(126.295095376145,-33.2792714542557,29.6532145043962));
#24309=CARTESIAN_POINT('Ctrl Pts',(126.345059189201,-33.1716942524512,29.647445400439));
#24310=CARTESIAN_POINT('Ctrl Pts',(126.399665748915,-33.0663954535246,29.6416762964818));
#24311=CARTESIAN_POINT('Ctrl Pts',(126.458661736905,-32.9637907017352,29.6359071925245));
#24312=CARTESIAN_POINT('Ctrl Pts',(126.517754586706,-32.8610174896421,29.6301286166375));
#24313=CARTESIAN_POINT('Ctrl Pts',(126.581251035677,-32.7609475085123,29.6243500407505));
#24314=CARTESIAN_POINT('Ctrl Pts',(126.648854860074,-32.6639667701102,29.6185714648635));
#24315=CARTESIAN_POINT('Ctrl Pts',(126.698499254289,-32.5927496451699,29.6143280081967));
#24316=CARTESIAN_POINT('Ctrl Pts',(126.750357702169,-32.5231977812645,29.6100845515299));
#24317=CARTESIAN_POINT('Ctrl Pts',(126.804299925717,-32.4554517031058,29.6058410948631));
#24318=CARTESIAN_POINT('Ctrl Pts',(126.878347621069,-32.362455148147,29.6000160070964));
#24319=CARTESIAN_POINT('Ctrl Pts',(126.956578253727,-32.2725425605472,29.5941909193296));
#24320=CARTESIAN_POINT('Ctrl Pts',(127.038705676932,-32.1861128430297,29.5883658315628));
#24321=CARTESIAN_POINT('Ctrl Pts',(127.120728387972,-32.0997933230852,29.5825481707616));
#24322=CARTESIAN_POINT('Ctrl Pts',(127.206637728886,-32.0169481340628,29.5767305099604));
#24323=CARTESIAN_POINT('Ctrl Pts',(127.296106343381,-31.9379444659358,29.5709128491592));
#24324=CARTESIAN_POINT('Ctrl Pts',(127.385484176038,-31.8590209610953,29.5651010914106));
#24325=CARTESIAN_POINT('Ctrl Pts',(127.478413793455,-31.7839314912864,29.559289333662));
#24326=CARTESIAN_POINT('Ctrl Pts',(127.574530335048,-31.7130071639266,29.5534775759134));
#24327=CARTESIAN_POINT('Ctrl Pts',(127.674253428406,-31.6394215645971,29.5474477453459));
#24328=CARTESIAN_POINT('Ctrl Pts',(127.777406988163,-31.5703201313939,29.5414179147785));
#24329=CARTESIAN_POINT('Ctrl Pts',(127.883544615322,-31.5060278185615,29.535388084211));
#24330=CARTESIAN_POINT('Ctrl Pts',(127.985724855635,-31.4441326721242,29.5295830784565));
#24331=CARTESIAN_POINT('Ctrl Pts',(128.090670241815,-31.3866946760441,29.523778072702));
#24332=CARTESIAN_POINT('Ctrl Pts',(128.197952699211,-31.3339598303184,29.5179730669474));
#24333=CARTESIAN_POINT('Ctrl Pts',(128.305217823592,-31.281233504661,29.5121689990746));
#24334=CARTESIAN_POINT('Ctrl Pts',(128.414818902106,-31.2332089981539,29.5063649312017));
#24335=CARTESIAN_POINT('Ctrl Pts',(128.526304156129,-31.1900858855144,29.5005608633288));
#24336=CARTESIAN_POINT('Ctrl Pts',(128.637797675485,-31.1469595757983,29.4947563651519));
#24337=CARTESIAN_POINT('Ctrl Pts',(128.751175267391,-31.1087355295797,29.488951866975));
#24338=CARTESIAN_POINT('Ctrl Pts',(128.865966722983,-31.0755645595043,29.4831473687981));
#24339=CARTESIAN_POINT('Ctrl Pts',(128.98079374545,-31.0423833117676,29.4773410721611));
#24340=CARTESIAN_POINT('Ctrl Pts',(129.097035110911,-31.0142583670542,29.4715347755241));
#24341=CARTESIAN_POINT('Ctrl Pts',(129.214207684855,-30.9912900532143,29.4657284788871));
#24342=CARTESIAN_POINT('Ctrl Pts',(129.331507394359,-30.9682968181035,29.4599158822538));
#24343=CARTESIAN_POINT('Ctrl Pts',(129.44973992843,-30.9504714607943,29.4541032856206));
#24344=CARTESIAN_POINT('Ctrl Pts',(129.568414095604,-30.9378628030153,29.4482906889873));
#24345=CARTESIAN_POINT('Ctrl Pts',(129.687164680749,-30.9252460261311,29.442474349443));
#24346=CARTESIAN_POINT('Ctrl Pts',(129.806357058913,-30.917852664184,29.4366580098987));
#24347=CARTESIAN_POINT('Ctrl Pts',(129.925498726576,-30.9156794248911,29.4308416703545));
#24348=CARTESIAN_POINT('Ctrl Pts',(130.044808685338,-30.9135031158339,29.4250171150601));
#24349=CARTESIAN_POINT('Ctrl Pts',(130.164067384022,-30.9165616364723,29.4191925597657));
#24350=CARTESIAN_POINT('Ctrl Pts',(130.282785995545,-30.9247997496168,29.4133680044714));
#24351=CARTESIAN_POINT('Ctrl Pts',(130.314082285943,-30.9269714594944,29.4118325504125));
#24352=CARTESIAN_POINT('Ctrl Pts',(130.345341092885,-30.9295028438761,29.4102970963536));
#24353=CARTESIAN_POINT('Ctrl Pts',(130.376553582223,-30.9323923001702,29.4087616422947));
#24354=CARTESIAN_POINT('Ctrl Pts',(130.495101758289,-30.9433667460012,29.4029298332344));
#24355=CARTESIAN_POINT('Ctrl Pts',(130.613354428765,-30.9595451065276,29.3970980241742));
#24356=CARTESIAN_POINT('Ctrl Pts',(130.730820038436,-30.9809046949071,29.3912662151139));
#24357=CARTESIAN_POINT('Ctrl Pts',(130.848147694306,-31.0022391981878,29.3854412550389));
#24358=CARTESIAN_POINT('Ctrl Pts',(130.964689730705,-31.0287427564402,29.3796162949639));
#24359=CARTESIAN_POINT('Ctrl Pts',(131.079958684508,-31.0603408472616,29.3737913348889));
#24360=CARTESIAN_POINT('Ctrl Pts',(131.195119236869,-31.0919092225481,29.3679718527336));
#24361=CARTESIAN_POINT('Ctrl Pts',(131.309008697878,-31.1285624933226,29.3621523705783));
#24362=CARTESIAN_POINT('Ctrl Pts',(131.421149399369,-31.1701750190547,29.3563328884229));
#24363=CARTESIAN_POINT('Ctrl Pts',(131.533206474952,-31.2117565133665,29.3505177459897));
#24364=CARTESIAN_POINT('Ctrl Pts',(131.643517006468,-31.2582897605415,29.3447026035565));
#24365=CARTESIAN_POINT('Ctrl Pts',(131.751618760839,-31.3095993826311,29.3388874611232));
#24366=CARTESIAN_POINT('Ctrl Pts',(131.859673816909,-31.3608868397502,29.3330748307424));
#24367=CARTESIAN_POINT('Ctrl Pts',(131.965521627783,-31.4169463914047,29.3272622003616));
#24368=CARTESIAN_POINT('Ctrl Pts',(132.068720680817,-31.477554862775,29.3214495699808));
#24369=CARTESIAN_POINT('Ctrl Pts',(132.171910341834,-31.5381578182435,29.3156374686003));
#24370=CARTESIAN_POINT('Ctrl Pts',(132.272451372145,-31.603308666982,29.3098253672197));
#24371=CARTESIAN_POINT('Ctrl Pts',(132.369927990263,-31.6727389160201,29.3040132658392));
#24372=CARTESIAN_POINT('Ctrl Pts',(132.409519580254,-31.7009390526884,29.3016525937181));
#24373=CARTESIAN_POINT('Ctrl Pts',(132.448605957911,-31.7298446580891,29.2992919215971));
#24374=CARTESIAN_POINT('Ctrl Pts',(132.487160670875,-31.7594357285724,29.296931249476));
#24375=CARTESIAN_POINT('',(128.942095577027,-38.9456385074984,30.));
#24376=CARTESIAN_POINT('Ctrl Pts',(128.942095577027,-38.9456385074984,30.));
#24377=CARTESIAN_POINT('Ctrl Pts',(127.639207105396,-38.596308107828,29.9343068491439));
#24378=CARTESIAN_POINT('Ctrl Pts',(126.178813349621,-37.2185119668352,29.8475123998799));
#24379=CARTESIAN_POINT('Ctrl Pts',(125.916229787505,-35.4379239995562,29.7607179506158));
#24380=CARTESIAN_POINT('Ctrl Pts',(125.919305073524,-35.0038914743736,29.739616652208));
#24381=CARTESIAN_POINT('',(131.058681718482,-38.9454300169882,29.999999873734));
#24382=CARTESIAN_POINT('Origin',(130.,-35.,30.));
#24383=CARTESIAN_POINT('',(125.915000700056,-34.9976084607349,29.6353849714475));
#24384=CARTESIAN_POINT('Ctrl Pts',(131.058681718482,-38.9454300169882,29.999999873734));
#24385=CARTESIAN_POINT('Ctrl Pts',(130.944553579868,-38.9760541500725,29.9942106257328));
#24386=CARTESIAN_POINT('Ctrl Pts',(130.828900823923,-39.0017743570889,29.9884213777316));
#24387=CARTESIAN_POINT('Ctrl Pts',(130.712185167928,-39.0224392209931,29.9826321297304));
#24388=CARTESIAN_POINT('Ctrl Pts',(130.595617050571,-39.0430779627302,29.976850199837));
#24389=CARTESIAN_POINT('Ctrl Pts',(130.477989108527,-39.0586739970541,29.9710682699437));
#24390=CARTESIAN_POINT('Ctrl Pts',(130.359777597801,-39.0691258373416,29.9652863400504));
#24391=CARTESIAN_POINT('Ctrl Pts',(130.241683728729,-39.0795672761734,29.9595101642143));
#24392=CARTESIAN_POINT('Ctrl Pts',(130.123007855757,-39.0848746667639,29.9537339883782));
#24393=CARTESIAN_POINT('Ctrl Pts',(130.004235129155,-39.0849978046115,29.9479578125421));
#24394=CARTESIAN_POINT('Ctrl Pts',(129.88554614853,-39.0851208556354,29.9421857094549));
#24395=CARTESIAN_POINT('Ctrl Pts',(129.766760862474,-39.0800669244702,29.9364136063676));
#24396=CARTESIAN_POINT('Ctrl Pts',(129.648367584554,-39.0698377909209,29.9306415032804));
#24397=CARTESIAN_POINT('Ctrl Pts',(129.530018417893,-39.0596124685672,29.9248715507774));
#24398=CARTESIAN_POINT('Ctrl Pts',(129.412061380663,-39.0442158123201,29.9191015982745));
#24399=CARTESIAN_POINT('Ctrl Pts',(129.294982237339,-39.0237016482752,29.9133316457716));
#24400=CARTESIAN_POINT('Ctrl Pts',(129.177918221597,-39.0031901348279,29.9075624387937));
#24401=CARTESIAN_POINT('Ctrl Pts',(129.061732281649,-38.9775624998559,29.9017932318157));
#24402=CARTESIAN_POINT('Ctrl Pts',(128.946901819112,-38.9469240202227,29.8960240248378));
#24403=CARTESIAN_POINT('Ctrl Pts',(128.832058246409,-38.9162820426015,29.8902541591908));
#24404=CARTESIAN_POINT('Ctrl Pts',(128.718570858412,-38.8806281901078,29.8844842935439));
#24405=CARTESIAN_POINT('Ctrl Pts',(128.606902986808,-38.8401179294176,29.8787144278969));
#24406=CARTESIAN_POINT('Ctrl Pts',(128.495126237423,-38.799568170641,29.872938936548));
#24407=CARTESIAN_POINT('Ctrl Pts',(128.385172937777,-38.7541526867095,29.8671634451991));
#24408=CARTESIAN_POINT('Ctrl Pts',(128.27748764131,-38.7040756166905,29.8613879538502));
#24409=CARTESIAN_POINT('Ctrl Pts',(128.169750388419,-38.65397438529,29.8556096759195));
#24410=CARTESIAN_POINT('Ctrl Pts',(128.064283685775,-38.5992072781454,29.8498313979889));
#24411=CARTESIAN_POINT('Ctrl Pts',(127.961507016297,-38.5400242026565,29.8440531200582));
#24412=CARTESIAN_POINT('Ctrl Pts',(127.85856581443,-38.480746382583,29.8382655918388));
#24413=CARTESIAN_POINT('Ctrl Pts',(127.758323599919,-38.4170386909014,29.8324780636193));
#24414=CARTESIAN_POINT('Ctrl Pts',(127.661170868142,-38.3491944243311,29.8266905353998));
#24415=CARTESIAN_POINT('Ctrl Pts',(127.568698601784,-38.2846186478772,29.8211818292494));
#24416=CARTESIAN_POINT('Ctrl Pts',(127.479025300208,-38.2162957863241,29.8156731230991));
#24417=CARTESIAN_POINT('Ctrl Pts',(127.392457740908,-38.1445108311233,29.8101644169487));
#24418=CARTESIAN_POINT('Ctrl Pts',(127.302025730489,-38.0695213331038,29.8044097973659));
#24419=CARTESIAN_POINT('Ctrl Pts',(127.21467127379,-37.990494710053,29.7986551777831));
#24420=CARTESIAN_POINT('Ctrl Pts',(127.130781940669,-37.9077160672954,29.7929005582002));
#24421=CARTESIAN_POINT('Ctrl Pts',(127.046997022695,-37.8250404572341,29.7871531012616));
#24422=CARTESIAN_POINT('Ctrl Pts',(126.966668949469,-37.7386224034269,29.7814056443231));
#24423=CARTESIAN_POINT('Ctrl Pts',(126.890153059589,-37.6487878373355,29.7756581873845));
#24424=CARTESIAN_POINT('Ctrl Pts',(126.812342342182,-37.5574330606155,29.7698134700538));
#24425=CARTESIAN_POINT('Ctrl Pts',(126.738474361781,-37.4625453450967,29.7639687527231));
#24426=CARTESIAN_POINT('Ctrl Pts',(126.668884865751,-37.3645077632303,29.7581240353924));
#24427=CARTESIAN_POINT('Ctrl Pts',(126.600566624001,-37.2682611225644,29.7523860888007));
#24428=CARTESIAN_POINT('Ctrl Pts',(126.536372134257,-37.1689790755732,29.7466481422091));
#24429=CARTESIAN_POINT('Ctrl Pts',(126.47657871807,-37.0670576842563,29.7409101956174));
#24430=CARTESIAN_POINT('Ctrl Pts',(126.416805277182,-36.9651703420097,29.7351741659124));
#24431=CARTESIAN_POINT('Ctrl Pts',(126.361430199031,-36.8606457691834,29.7294381362073));
#24432=CARTESIAN_POINT('Ctrl Pts',(126.310686761419,-36.7539078731891,29.7237021065022));
#24433=CARTESIAN_POINT('Ctrl Pts',(126.259947595204,-36.6471789619982,29.7179665596351));
#24434=CARTESIAN_POINT('Ctrl Pts',(126.213839473349,-36.5382374769035,29.7122310127679));
#24435=CARTESIAN_POINT('Ctrl Pts',(126.172548747324,-36.4275300026224,29.7064954659007));
#24436=CARTESIAN_POINT('Ctrl Pts',(126.129887835005,-36.3131488253476,29.7005695913629));
#24437=CARTESIAN_POINT('Ctrl Pts',(126.092369787723,-36.1968828533769,29.6946437168251));
#24438=CARTESIAN_POINT('Ctrl Pts',(126.060144891387,-36.0792435884163,29.6887178422874));
#24439=CARTESIAN_POINT('Ctrl Pts',(126.028921932286,-35.9652619662481,29.6829762151801));
#24440=CARTESIAN_POINT('Ctrl Pts',(126.002667897363,-35.8499916120652,29.6772345880728));
#24441=CARTESIAN_POINT('Ctrl Pts',(125.981467567398,-35.7339087737072,29.6714929609655));
#24442=CARTESIAN_POINT('Ctrl Pts',(125.959246767212,-35.6122383298786,29.6654749627125));
#24443=CARTESIAN_POINT('Ctrl Pts',(125.942578393723,-35.4896757557052,29.6594569644595));
#24444=CARTESIAN_POINT('Ctrl Pts',(125.931498881111,-35.3667746523376,29.6534389662065));
#24445=CARTESIAN_POINT('Ctrl Pts',(125.920419368499,-35.2438735489701,29.6474209679535));
#24446=CARTESIAN_POINT('Ctrl Pts',(125.914928675205,-35.1206344422539,29.6414029697005));
#24447=CARTESIAN_POINT('Ctrl Pts',(125.915000700056,-34.9976084607349,29.6353849714475));
#24448=CARTESIAN_POINT('Ctrl Pts',(125.915000700057,-34.9976084598567,29.6353849714045));
#24449=CARTESIAN_POINT('Ctrl Pts',(125.915089664039,-34.845648725259,29.6279516357298));
#24450=CARTESIAN_POINT('Ctrl Pts',(125.923657510955,-34.693945020907,29.6205183000551));
#24451=CARTESIAN_POINT('Ctrl Pts',(125.940621229176,-34.543196984482,29.6130849643803));
#24452=CARTESIAN_POINT('Ctrl Pts',(125.953900069263,-34.4251946077035,29.6072663063214));
#24453=CARTESIAN_POINT('Ctrl Pts',(125.972350285853,-34.307578263497,29.6014476482625));
#24454=CARTESIAN_POINT('Ctrl Pts',(125.995942018589,-34.1908370488571,29.5956289902035));
#24455=CARTESIAN_POINT('Ctrl Pts',(126.019503712228,-34.0742444795399,29.5898177409788));
#24456=CARTESIAN_POINT('Ctrl Pts',(126.048193821194,-33.9585252210092,29.5840064917541));
#24457=CARTESIAN_POINT('Ctrl Pts',(126.081930718129,-33.8441634620494,29.5781952425294));
#24458=CARTESIAN_POINT('Ctrl Pts',(126.115633495392,-33.7299173623876,29.5723898704878));
#24459=CARTESIAN_POINT('Ctrl Pts',(126.154372792127,-33.6170264213218,29.5665844984463));
#24460=CARTESIAN_POINT('Ctrl Pts',(126.198016026887,-33.5059642346352,29.5607791264047));
#24461=CARTESIAN_POINT('Ctrl Pts',(126.24336474875,-33.390561968021,29.5547468924634));
#24462=CARTESIAN_POINT('Ctrl Pts',(126.29400840197,-33.2771347374572,29.548714658522));
#24463=CARTESIAN_POINT('Ctrl Pts',(126.349741154889,-33.1661964762586,29.5426824245806));
#24464=CARTESIAN_POINT('Ctrl Pts',(126.4033164962,-33.0595526286651,29.5368836980625));
#24465=CARTESIAN_POINT('Ctrl Pts',(126.461594070909,-32.9552090404644,29.5310849715443));
#24466=CARTESIAN_POINT('Ctrl Pts',(126.524342428739,-32.8536008182687,29.5252862450261));
#24467=CARTESIAN_POINT('Ctrl Pts',(126.587081183805,-32.7520081457994,29.5194884059225));
#24468=CARTESIAN_POINT('Ctrl Pts',(126.654289146494,-32.6531503549122,29.5136905668188));
#24469=CARTESIAN_POINT('Ctrl Pts',(126.725690118207,-32.5574358149699,29.5078927277152));
#24470=CARTESIAN_POINT('Ctrl Pts',(126.797097096589,-32.4617132229587,29.5020944008633));
#24471=CARTESIAN_POINT('Ctrl Pts',(126.872697540618,-32.3691347355745,29.4962960740114));
#24472=CARTESIAN_POINT('Ctrl Pts',(126.952173738435,-32.2800771923975,29.4904977471595));
#24473=CARTESIAN_POINT('Ctrl Pts',(127.03167547094,-32.1909910361686,29.4846975573792));
#24474=CARTESIAN_POINT('Ctrl Pts',(127.115055161299,-32.105428378916,29.4788973675989));
#24475=CARTESIAN_POINT('Ctrl Pts',(127.20195734371,-32.0237301376421,29.4730971778186));
#24476=CARTESIAN_POINT('Ctrl Pts',(127.288955816632,-31.9419413719968,29.4672905612349));
#24477=CARTESIAN_POINT('Ctrl Pts',(127.379484274045,-31.8640258497032,29.4614839446512));
#24478=CARTESIAN_POINT('Ctrl Pts',(127.473153080475,-31.790285114642,29.4556773280675));
#24479=CARTESIAN_POINT('Ctrl Pts',(127.566883344002,-31.7164959975027,29.4498669017011));
#24480=CARTESIAN_POINT('Ctrl Pts',(127.663757728217,-31.6468873605511,29.4440564753347));
#24481=CARTESIAN_POINT('Ctrl Pts',(127.763357846448,-31.5817172619934,29.4382460489683));
#24482=CARTESIAN_POINT('Ctrl Pts',(127.863101256293,-31.5164534052278,29.4324272633209));
#24483=CARTESIAN_POINT('Ctrl Pts',(127.965577876409,-31.4556410400234,29.4266084776736));
#24484=CARTESIAN_POINT('Ctrl Pts',(128.070344885655,-31.3994922386303,29.4207896920263));
#24485=CARTESIAN_POINT('Ctrl Pts',(128.099057878545,-31.3841038053175,29.4191949652881));
#24486=CARTESIAN_POINT('Ctrl Pts',(128.127942793974,-31.3690653801131,29.41760023855));
#24487=CARTESIAN_POINT('Ctrl Pts',(128.156990278416,-31.3543806882578,29.4160055118119));
#24488=CARTESIAN_POINT('Ctrl Pts',(128.263076116259,-31.3007499567556,29.4101813268474));
#24489=CARTESIAN_POINT('Ctrl Pts',(128.371675762737,-31.2516672333729,29.4043571418829));
#24490=CARTESIAN_POINT('Ctrl Pts',(128.482362616791,-31.2073753450827,29.3985329569184));
#24491=CARTESIAN_POINT('Ctrl Pts',(128.592909797229,-31.163139347876,29.3927161213811));
#24492=CARTESIAN_POINT('Ctrl Pts',(128.705538570954,-31.1236823117551,29.3868992858438));
#24493=CARTESIAN_POINT('Ctrl Pts',(128.819798154847,-31.0892010273222,29.3810824503064));
#24494=CARTESIAN_POINT('Ctrl Pts',(128.933943320326,-31.0547542721054,29.3752714396905));
#24495=CARTESIAN_POINT('Ctrl Pts',(129.049715658567,-31.025273473399,29.3694604290746));
#24496=CARTESIAN_POINT('Ctrl Pts',(129.166645398469,-31.0009069643096,29.3636494184587));
#24497=CARTESIAN_POINT('Ctrl Pts',(129.287984481213,-30.9756216103437,29.3576192784914));
#24498=CARTESIAN_POINT('Ctrl Pts',(129.410569557824,-30.9558440186323,29.3515891385241));
#24499=CARTESIAN_POINT('Ctrl Pts',(129.533859097536,-30.9416829030927,29.3455589985568));
#24500=CARTESIAN_POINT('Ctrl Pts',(129.652534477305,-30.9280517729211,29.3397545389704));
#24501=CARTESIAN_POINT('Ctrl Pts',(129.771862096122,-30.9196243260056,29.3339500793841));
#24502=CARTESIAN_POINT('Ctrl Pts',(129.891350325346,-30.9164451456852,29.3281456197977));
#24503=CARTESIAN_POINT('Ctrl Pts',(130.010820801379,-30.9132664377176,29.3223420226199));
#24504=CARTESIAN_POINT('Ctrl Pts',(130.130451432377,-30.9153344564683,29.3165384254422));
#24505=CARTESIAN_POINT('Ctrl Pts',(130.249748468838,-30.9226417005231,29.3107348282645));
#24506=CARTESIAN_POINT('Ctrl Pts',(130.369055918311,-30.9299495824011,29.3049307245115));
#24507=CARTESIAN_POINT('Ctrl Pts',(130.488029307856,-30.9424975738677,29.2991266207586));
#24508=CARTESIAN_POINT('Ctrl Pts',(130.606178536407,-30.960226171925,29.2933225170056));
#24509=CARTESIAN_POINT('Ctrl Pts',(130.724365944667,-30.9779604989467,29.287516537667));
#24510=CARTESIAN_POINT('Ctrl Pts',(130.841728258753,-31.0008787014336,29.2817105583284));
#24511=CARTESIAN_POINT('Ctrl Pts',(130.957784748129,-31.0288700126725,29.2759045789898));
#24512=CARTESIAN_POINT('Ctrl Pts',(131.073969498395,-31.0568922587649,29.2700921831201));
#24513=CARTESIAN_POINT('Ctrl Pts',(131.188845146208,-31.0899987090927,29.2642797872503));
#24514=CARTESIAN_POINT('Ctrl Pts',(131.301945173453,-31.1280284394999,29.2584673913806));
#24515=CARTESIAN_POINT('Ctrl Pts',(131.415119349703,-31.166083102409,29.2526511848719));
#24516=CARTESIAN_POINT('Ctrl Pts',(131.526515207018,-31.2090673269266,29.2468349783632));
#24517=CARTESIAN_POINT('Ctrl Pts',(131.635686834075,-31.2567723044366,29.2410187718545));
#24518=CARTESIAN_POINT('Ctrl Pts',(131.745014562896,-31.3045454940943,29.2351942488984));
#24519=CARTESIAN_POINT('Ctrl Pts',(131.852111348333,-31.3570527305047,29.2293697259423));
#24520=CARTESIAN_POINT('Ctrl Pts',(131.956556340386,-31.4140395586544,29.2235452029863));
#24521=CARTESIAN_POINT('Ctrl Pts',(131.984166408778,-31.4291040456322,29.2220054884053));
#24522=CARTESIAN_POINT('Ctrl Pts',(132.011591328512,-31.4444813395595,29.2204657738244));
#24523=CARTESIAN_POINT('Ctrl Pts',(132.038823685636,-31.4601662498232,29.2189260592434));
#24524=CARTESIAN_POINT('Ctrl Pts',(132.141833733249,-31.5194965290832,29.2131018820864));
#24525=CARTESIAN_POINT('Ctrl Pts',(132.242417377746,-31.5834223086336,29.2072777049293));
#24526=CARTESIAN_POINT('Ctrl Pts',(132.340137746395,-31.6517197954921,29.2014535277723));
#24527=CARTESIAN_POINT('Ctrl Pts',(132.389906219477,-31.6865033486382,29.1984873047823));
#24528=CARTESIAN_POINT('Ctrl Pts',(132.438932337297,-31.7224200719,29.1955210817924));
#24529=CARTESIAN_POINT('Ctrl Pts',(132.487160670875,-31.7594357285724,29.1925548588025));
#24530=CARTESIAN_POINT('Origin',(130.,-35.,23.));
#24531=CARTESIAN_POINT('',(126.821241975899,-33.8227564029848,17.9148966234937));
#24532=CARTESIAN_POINT('',(126.821241915871,-33.8227565650715,17.5703600952825));
#24533=CARTESIAN_POINT('',(126.821241915871,-33.8227565650715,23.));
#24534=CARTESIAN_POINT('',(133.378768828602,-35.2726284383002,17.));
#24535=CARTESIAN_POINT('Ctrl Pts',(126.821241915871,-33.8227565650715,17.5703600952825));
#24536=CARTESIAN_POINT('Ctrl Pts',(126.857212086853,-33.7256309677594,17.5642667500865));
#24537=CARTESIAN_POINT('Ctrl Pts',(126.897684653908,-33.6300288363987,17.5581734048904));
#24538=CARTESIAN_POINT('Ctrl Pts',(126.942506928975,-33.536394457808,17.5520800596944));
#24539=CARTESIAN_POINT('Ctrl Pts',(126.987285654953,-33.4428510538928,17.5459926347609));
#24540=CARTESIAN_POINT('Ctrl Pts',(127.036405501013,-33.3512719845787,17.5399052098273));
#24541=CARTESIAN_POINT('Ctrl Pts',(127.089665306779,-33.2620825577905,17.5338177848938));
#24542=CARTESIAN_POINT('Ctrl Pts',(127.142891448156,-33.1729495057405,17.527734207692));
#24543=CARTESIAN_POINT('Ctrl Pts',(127.200252127707,-33.086203459193,17.5216506304902));
#24544=CARTESIAN_POINT('Ctrl Pts',(127.261500154244,-33.0022453460714,17.5155670532884));
#24545=CARTESIAN_POINT('Ctrl Pts',(127.322728683129,-32.9183139601134,17.5094854127281));
#24546=CARTESIAN_POINT('Ctrl Pts',(127.387841847681,-32.8371690887653,17.5034037721677));
#24547=CARTESIAN_POINT('Ctrl Pts',(127.456549491797,-32.7591821638473,17.4973221316074));
#24548=CARTESIAN_POINT('Ctrl Pts',(127.525253041812,-32.6811998859558,17.4912408534353));
#24549=CARTESIAN_POINT('Ctrl Pts',(127.59755036266,-32.6063755009931,17.4851595752632));
#24550=CARTESIAN_POINT('Ctrl Pts',(127.673112026926,-32.5350461620416,17.4790782970911));
#24551=CARTESIAN_POINT('Ctrl Pts',(127.74868874015,-32.4637026170487,17.472995807764));
#24552=CARTESIAN_POINT('Ctrl Pts',(127.827530777778,-32.3958557947502,17.4669133184368));
#24553=CARTESIAN_POINT('Ctrl Pts',(127.909273677431,-32.3318042600632,17.4608308291097));
#24554=CARTESIAN_POINT('Ctrl Pts',(127.991104779775,-32.2676836121229,17.4547417766201));
#24555=CARTESIAN_POINT('Ctrl Pts',(128.075842656886,-32.2073666928101,17.4486527241306));
#24556=CARTESIAN_POINT('Ctrl Pts',(128.163091785404,-32.1511101682148,17.442563671641));
#24557=CARTESIAN_POINT('Ctrl Pts',(128.250391702938,-32.0948208958592,17.4364710746234));
#24558=CARTESIAN_POINT('Ctrl Pts',(128.34020541377,-32.0425969403403,17.4303784776057));
#24559=CARTESIAN_POINT('Ctrl Pts',(128.432112321585,-31.9946492234062,17.4242858805881));
#24560=CARTESIAN_POINT('Ctrl Pts',(128.524167018222,-31.946624405231,17.4181834865077));
#24561=CARTESIAN_POINT('Ctrl Pts',(128.618321246487,-31.9028897387552,17.4120810924273));
#24562=CARTESIAN_POINT('Ctrl Pts',(128.714133823855,-31.8636082452048,17.4059786983469));
#24563=CARTESIAN_POINT('Ctrl Pts',(128.775993963582,-31.8382466617216,17.4020387672769));
#24564=CARTESIAN_POINT('Ctrl Pts',(128.838545020091,-31.8147403681239,17.3980988362069));
#24565=CARTESIAN_POINT('Ctrl Pts',(128.901665374432,-31.7931220614469,17.3941589051368));
#24566=CARTESIAN_POINT('Ctrl Pts',(128.998656182998,-31.7599033467185,17.3881048025551));
#24567=CARTESIAN_POINT('Ctrl Pts',(129.097333999467,-31.7310277136576,17.3820506999734));
#24568=CARTESIAN_POINT('Ctrl Pts',(129.19727047136,-31.70666880403,17.3759965973917));
#24569=CARTESIAN_POINT('Ctrl Pts',(129.297074246778,-31.6823422383642,17.3699505334975));
#24570=CARTESIAN_POINT('Ctrl Pts',(129.398132937558,-31.6625205801586,17.3639044696033));
#24571=CARTESIAN_POINT('Ctrl Pts',(129.500000401422,-31.6473286078231,17.3578584057091));
#24572=CARTESIAN_POINT('Ctrl Pts',(129.601762953542,-31.6321522814676,17.3518185685636));
#24573=CARTESIAN_POINT('Ctrl Pts',(129.704332195085,-31.621596227296,17.3457787314182));
#24574=CARTESIAN_POINT('Ctrl Pts',(129.807250029976,-31.6157345683951,17.3397388942727));
#24575=CARTESIAN_POINT('Ctrl Pts',(129.910098444688,-31.6098768633027,17.3337031311206));
#24576=CARTESIAN_POINT('Ctrl Pts',(130.013294552223,-31.6087072854238,17.3276673679685));
#24577=CARTESIAN_POINT('Ctrl Pts',(130.116374231673,-31.6122482232751,17.3216316048163));
#24578=CARTESIAN_POINT('Ctrl Pts',(130.219418282801,-31.6157879372414,17.3155979278573));
#24579=CARTESIAN_POINT('Ctrl Pts',(130.322345551185,-31.624034917913,17.3095642508982));
#24580=CARTESIAN_POINT('Ctrl Pts',(130.424691943871,-31.6369594389435,17.3035305739392));
#24581=CARTESIAN_POINT('Ctrl Pts',(130.52703055245,-31.6498829769805,17.2974973558804));
#24582=CARTESIAN_POINT('Ctrl Pts',(130.628787941222,-31.6674832938503,17.2914641378216));
#24583=CARTESIAN_POINT('Ctrl Pts',(130.729506183834,-31.6896788992232,17.2854309197627));
#24584=CARTESIAN_POINT('Ctrl Pts',(130.830243919015,-31.7118788002366,17.2793965340612));
#24585=CARTESIAN_POINT('Ctrl Pts',(130.929941683416,-31.7386756626943,17.2733621483597));
#24586=CARTESIAN_POINT('Ctrl Pts',(131.028153768648,-31.7699373240577,17.2673277626582));
#24587=CARTESIAN_POINT('Ctrl Pts',(131.126480044199,-31.8012353330771,17.26128636083));
#24588=CARTESIAN_POINT('Ctrl Pts',(131.223316775647,-31.8370083746529,17.2552449590019));
#24589=CARTESIAN_POINT('Ctrl Pts',(131.318235456208,-31.8770750338031,17.2492035571737));
#24590=CARTESIAN_POINT('Ctrl Pts',(131.41321041572,-31.9171654491783,17.2431585732924));
#24591=CARTESIAN_POINT('Ctrl Pts',(131.506264667989,-31.9615543620595,17.2371135894111));
#24592=CARTESIAN_POINT('Ctrl Pts',(131.596993644016,-32.010013986074,17.2310686055298));
#24593=CARTESIAN_POINT('Ctrl Pts',(131.687886896195,-32.0585613522949,17.2250126764496));
#24594=CARTESIAN_POINT('Ctrl Pts',(131.776446088358,-32.1111939292309,17.2189567473694));
#24595=CARTESIAN_POINT('Ctrl Pts',(131.862294784052,-32.16763999467,17.2129008182892));
#24596=CARTESIAN_POINT('Ctrl Pts',(131.937055875936,-32.2167958898257,17.2076270297157));
#24597=CARTESIAN_POINT('Ctrl Pts',(132.009761740428,-32.2688430573262,17.2023532411421));
#24598=CARTESIAN_POINT('Ctrl Pts',(132.0801854484,-32.3235782165803,17.1970794525685));
#24599=CARTESIAN_POINT('Ctrl Pts',(132.163725198345,-32.3885075088443,17.1908234488535));
#24600=CARTESIAN_POINT('Ctrl Pts',(132.244340954018,-32.4574437278421,17.1845674451385));
#24601=CARTESIAN_POINT('Ctrl Pts',(132.321637206882,-32.5301000542288,17.1783114414236));
#24602=CARTESIAN_POINT('Ctrl Pts',(132.398820375414,-32.60265008449,17.1720645902352));
#24603=CARTESIAN_POINT('Ctrl Pts',(132.472693415881,-32.6789091177425,17.1658177390467));
#24604=CARTESIAN_POINT('Ctrl Pts',(132.542892921555,-32.7585494312818,17.1595708878583));
#24605=CARTESIAN_POINT('Ctrl Pts',(132.613005970988,-32.8380916614787,17.153331730161));
#24606=CARTESIAN_POINT('Ctrl Pts',(132.679454227142,-32.9210065833029,17.1470925724636));
#24607=CARTESIAN_POINT('Ctrl Pts',(132.741910682205,-33.0069292854214,17.1408534147663));
#24608=CARTESIAN_POINT('Ctrl Pts',(132.804294288443,-33.0927517678289,17.1346215343841));
#24609=CARTESIAN_POINT('Ctrl Pts',(132.862695133877,-33.1815747181818,17.1283896540019));
#24610=CARTESIAN_POINT('Ctrl Pts',(132.916826607734,-33.273000404484,17.1221577736197));
#24611=CARTESIAN_POINT('Ctrl Pts',(132.970921300909,-33.3643639698258,17.1159301276099));
#24612=CARTESIAN_POINT('Ctrl Pts',(133.020752191913,-33.4583264071137,17.1097024816));
#24613=CARTESIAN_POINT('Ctrl Pts',(133.066076207699,-33.5544614321713,17.1034748355901));
#24614=CARTESIAN_POINT('Ctrl Pts',(133.111378919699,-33.6505512705878,17.0972501167798));
#24615=CARTESIAN_POINT('Ctrl Pts',(133.15217880271,-33.7488113013554,17.0910253979695));
#24616=CARTESIAN_POINT('Ctrl Pts',(133.18827920759,-33.8487916101105,17.0848006791592));
#24617=CARTESIAN_POINT('Ctrl Pts',(133.224370200206,-33.9487458515422,17.078577583286));
#24618=CARTESIAN_POINT('Ctrl Pts',(133.255764019014,-34.050419100345,17.0723544874129));
#24619=CARTESIAN_POINT('Ctrl Pts',(133.282312756489,-34.1533430263166,17.0661313915397));
#24620=CARTESIAN_POINT('Ctrl Pts',(133.308867658179,-34.2562908496664,17.0599068507579));
#24621=CARTESIAN_POINT('Ctrl Pts',(133.330575125734,-34.3604895427839,17.0536823099761));
#24622=CARTESIAN_POINT('Ctrl Pts',(133.34733763752,-34.4654573890282,17.0474577691943));
#24623=CARTESIAN_POINT('Ctrl Pts',(133.364101852332,-34.5704358997268,17.0412325960156));
#24624=CARTESIAN_POINT('Ctrl Pts',(133.375920054006,-34.6761833216448,17.035007422837));
#24625=CARTESIAN_POINT('Ctrl Pts',(133.382746348089,-34.7822106361798,17.0287822496584));
#24626=CARTESIAN_POINT('Ctrl Pts',(133.38957746019,-34.8883127850986,17.0225526827346));
#24627=CARTESIAN_POINT('Ctrl Pts',(133.391409607669,-34.994694819922,17.0163231158108));
#24628=CARTESIAN_POINT('Ctrl Pts',(133.388248988362,-35.1008655311097,17.010093548887));
#24629=CARTESIAN_POINT('Ctrl Pts',(133.386541974809,-35.1582070914918,17.0067290325913));
#24630=CARTESIAN_POINT('Ctrl Pts',(133.383379494437,-35.2154870259768,17.0033645162957));
#24631=CARTESIAN_POINT('Ctrl Pts',(133.378768828602,-35.2726284383002,17.));
#24632=CARTESIAN_POINT('',(126.821241915871,-33.8227565650715,17.));
#24633=CARTESIAN_POINT('Origin',(130.,-35.,17.));
#24634=CARTESIAN_POINT('',(126.821241915871,-33.8227565650715,16.));
#24635=CARTESIAN_POINT('',(126.821241915871,-33.8227565650715,23.));
#24636=CARTESIAN_POINT('Origin',(130.,-35.,16.));
#24637=CARTESIAN_POINT('',(129.213983878817,-38.3003700508738,16.998298898493));
#24638=CARTESIAN_POINT('Origin',(130.,-35.,17.));
#24639=CARTESIAN_POINT('Ctrl Pts',(129.214786760262,-38.2975513992415,16.9966191224731));
#24640=CARTESIAN_POINT('Ctrl Pts',(129.246653588405,-38.3051395312634,16.9986057882608));
#24641=CARTESIAN_POINT('Ctrl Pts',(129.278627725152,-38.3122650918281,17.0006144214925));
#24642=CARTESIAN_POINT('Ctrl Pts',(129.562948150419,-38.371315022687,17.0185812798767));
#24643=CARTESIAN_POINT('Ctrl Pts',(129.820339259371,-38.3947753103289,17.0355059067697));
#24644=CARTESIAN_POINT('Ctrl Pts',(130.186419839379,-38.3863602280712,17.0588775137659));
#24645=CARTESIAN_POINT('Ctrl Pts',(130.294764342428,-38.3786543348929,17.0657189329248));
#24646=CARTESIAN_POINT('Ctrl Pts',(130.47777413777,-38.356765566798,17.077099281972));
#24647=CARTESIAN_POINT('Ctrl Pts',(130.552669845413,-38.3452504522162,17.0817067208494));
#24648=CARTESIAN_POINT('Ctrl Pts',(130.661059909158,-38.324845485086,17.0883038359326));
#24649=CARTESIAN_POINT('Ctrl Pts',(130.694899655733,-38.3179379594991,17.0903534317222));
#24650=CARTESIAN_POINT('Ctrl Pts',(130.754814885438,-38.3047508944395,17.0939658163127));
#24651=CARTESIAN_POINT('Ctrl Pts',(130.780932103144,-38.2986768705901,17.0955348410941));
#24652=CARTESIAN_POINT('Ctrl Pts',(130.83611855973,-38.285150101204,17.0988393862245));
#24653=CARTESIAN_POINT('Ctrl Pts',(130.86516655488,-38.2776199212549,17.1005723354365));
#24654=CARTESIAN_POINT('Ctrl Pts',(130.943853737324,-38.2561026555034,17.1052516552153));
#24655=CARTESIAN_POINT('Ctrl Pts',(130.993280849296,-38.2413666750523,17.10817448793));
#24656=CARTESIAN_POINT('Ctrl Pts',(131.268952899463,-38.15228056572,17.1244180377395));
#24657=CARTESIAN_POINT('Ctrl Pts',(131.487204870787,-38.0553798822507,17.136996498997));
#24658=CARTESIAN_POINT('Ctrl Pts',(131.842051924174,-37.8507285068452,17.1588181106744));
#24659=CARTESIAN_POINT('Ctrl Pts',(131.983862781221,-37.753921631808,17.1679974824299));
#24660=CARTESIAN_POINT('Ctrl Pts',(132.141492708805,-37.6278014531061,17.179470787434));
#24661=CARTESIAN_POINT('Ctrl Pts',(132.165001097274,-37.6084672921821,17.1812181425926));
#24662=CARTESIAN_POINT('Ctrl Pts',(132.201356071569,-37.5777376172861,17.1839833503402));
#24663=CARTESIAN_POINT('Ctrl Pts',(132.214382372257,-37.5665561477482,17.1849871056437));
#24664=CARTESIAN_POINT('Ctrl Pts',(132.23893598053,-37.5451538400591,17.1869050866599));
#24665=CARTESIAN_POINT('Ctrl Pts',(132.25047933074,-37.5349526902266,17.1878180019822));
#24666=CARTESIAN_POINT('Ctrl Pts',(132.275884266371,-37.5121914263325,17.1898516986653));
#24667=CARTESIAN_POINT('Ctrl Pts',(132.28971212245,-37.499594630796,17.1909750023959));
#24668=CARTESIAN_POINT('Ctrl Pts',(132.33741636256,-37.4554093833093,17.1949053798742));
#24669=CARTESIAN_POINT('Ctrl Pts',(132.370747660348,-37.4232427825009,17.19774951986));
#24670=CARTESIAN_POINT('Ctrl Pts',(132.550534164409,-37.2424783328038,17.2135896489576));
#24671=CARTESIAN_POINT('Ctrl Pts',(132.683682891899,-37.0812912981307,17.2271676473973));
#24672=CARTESIAN_POINT('Ctrl Pts',(132.892770772903,-36.7744701147091,17.2509959832686));
#24673=CARTESIAN_POINT('Ctrl Pts',(132.974590106743,-36.6336128830552,17.2612963397486));
#24674=CARTESIAN_POINT('Ctrl Pts',(133.073909781551,-36.4302216959482,17.2751714707825));
#24675=CARTESIAN_POINT('Ctrl Pts',(133.100221104257,-36.3722555726456,17.2790221057876));
#24676=CARTESIAN_POINT('Ctrl Pts',(133.137407413537,-36.283792757709,17.2847463889883));
#24677=CARTESIAN_POINT('Ctrl Pts',(133.149502540497,-36.2538273319791,17.2866597683682));
#24678=CARTESIAN_POINT('Ctrl Pts',(133.169818863107,-36.2013441392698,17.28996767964));
#24679=CARTESIAN_POINT('Ctrl Pts',(133.178232960908,-36.1789040060696,17.2913684474965));
#24680=CARTESIAN_POINT('Ctrl Pts',(133.196759108508,-36.1278549787408,17.2945251990383));
#24681=CARTESIAN_POINT('Ctrl Pts',(133.206726507739,-36.0991955427724,17.2962763900253));
#24682=CARTESIAN_POINT('Ctrl Pts',(133.232770263813,-36.0209403912586,17.301003672655));
#24683=CARTESIAN_POINT('Ctrl Pts',(133.248089773987,-35.9711004502343,17.3039555377369));
#24684=CARTESIAN_POINT('Ctrl Pts',(133.339695926222,-35.6465978698149,17.3228374367854));
#24685=CARTESIAN_POINT('Ctrl Pts',(133.382225693376,-35.3636102281896,17.3376348850357));
#24686=CARTESIAN_POINT('Ctrl Pts',(133.39203495278,-34.9408405567215,17.3602397627774));
#24687=CARTESIAN_POINT('Ctrl Pts',(133.386825023489,-34.8029984839704,17.367711907507));
#24688=CARTESIAN_POINT('Ctrl Pts',(133.370491590856,-34.6381019210267,17.3771552266791));
#24689=CARTESIAN_POINT('Ctrl Pts',(133.367398216467,-34.6103682135816,17.3787608947107));
#24690=CARTESIAN_POINT('Ctrl Pts',(133.36193445253,-34.5663258502553,17.3813428951952));
#24691=CARTESIAN_POINT('Ctrl Pts',(133.359786859501,-34.5499902608899,17.3823076295064));
#24692=CARTESIAN_POINT('Ctrl Pts',(133.355428641472,-34.5186115206496,17.3841754447154));
#24693=CARTESIAN_POINT('Ctrl Pts',(133.35323576391,-34.5035666072459,17.3850775920919));
#24694=CARTESIAN_POINT('Ctrl Pts',(133.34749503266,-34.4659551448432,17.3873487369644));
#24695=CARTESIAN_POINT('Ctrl Pts',(133.34382016177,-34.443408979409,17.388724418097));
#24696=CARTESIAN_POINT('Ctrl Pts',(133.329315865579,-34.3597561471504,17.3938773108535));
#24697=CARTESIAN_POINT('Ctrl Pts',(133.317037395229,-34.2989163673974,17.3977217156788));
#24698=CARTESIAN_POINT('Ctrl Pts',(133.259119330531,-34.0477057062228,17.4139080375364));
#24699=CARTESIAN_POINT('Ctrl Pts',(133.198703243129,-33.8611331160025,17.4266587307535));
#24700=CARTESIAN_POINT('Ctrl Pts',(133.061601489316,-33.5366100299174,17.4492664527907));
#24701=CARTESIAN_POINT('Ctrl Pts',(132.990753741091,-33.3967796417927,17.4591699197234));
#24702=CARTESIAN_POINT('Ctrl Pts',(132.878227077439,-33.2083041914475,17.472623776482));
#24703=CARTESIAN_POINT('Ctrl Pts',(132.844469017732,-33.1551797439451,17.4764303505179));
#24704=CARTESIAN_POINT('Ctrl Pts',(132.791354519797,-33.07652201559,17.4820907619841));
#24705=CARTESIAN_POINT('Ctrl Pts',(132.773084780329,-33.0502747582276,17.483983884035));
#24706=CARTESIAN_POINT('Ctrl Pts',(132.74062458761,-33.0050202367912,17.4872565678502));
#24707=CARTESIAN_POINT('Ctrl Pts',(132.726601223124,-32.9858964280754,17.4886423094046));
#24708=CARTESIAN_POINT('Ctrl Pts',(132.694380940432,-32.9429105986351,17.4917642271968));
#24709=CARTESIAN_POINT('Ctrl Pts',(132.676065395201,-32.9191397111135,17.4934956756242));
#24710=CARTESIAN_POINT('Ctrl Pts',(132.625480575953,-32.8552607617076,17.4981648705749));
#24711=CARTESIAN_POINT('Ctrl Pts',(132.59260884792,-32.8156386724102,17.5010787857782));
#24712=CARTESIAN_POINT('Ctrl Pts',(132.399350179993,-32.5932049948419,17.5175754641937));
#24713=CARTESIAN_POINT('Ctrl Pts',(132.220563895338,-32.4273261407114,17.5303624326294));
#24714=CARTESIAN_POINT('Ctrl Pts',(131.882756521121,-32.1755799866038,17.5527002228185));
#24715=CARTESIAN_POINT('Ctrl Pts',(131.731811098369,-32.0805931202618,17.5621884574029));
#24716=CARTESIAN_POINT('Ctrl Pts',(131.547882638817,-31.9841514626025,17.5739916659524));
#24717=CARTESIAN_POINT('Ctrl Pts',(131.521461893255,-31.9707366168401,17.5756929030975));
#24718=CARTESIAN_POINT('Ctrl Pts',(131.479840105132,-31.9502854642561,17.5783870928013));
#24719=CARTESIAN_POINT('Ctrl Pts',(131.46475638466,-31.9430122352426,17.5793663367062));
#24720=CARTESIAN_POINT('Ctrl Pts',(131.435881510991,-31.9293518061251,17.5812475193309));
#24721=CARTESIAN_POINT('Ctrl Pts',(131.422100313304,-31.9229451241244,17.582148290383));
#24722=CARTESIAN_POINT('Ctrl Pts',(131.391501006749,-31.9089694032447,17.5841541577313));
#24723=CARTESIAN_POINT('Ctrl Pts',(131.374663247239,-31.9014445099043,17.5852617574366));
#24724=CARTESIAN_POINT('Ctrl Pts',(131.324175077923,-31.8793735642484,17.5885925128912));
#24725=CARTESIAN_POINT('Ctrl Pts',(131.290350204207,-31.8652360356505,17.5908366212593));
#24726=CARTESIAN_POINT('Ctrl Pts',(131.056094103312,-31.7717594643386,17.606432860539));
#24727=CARTESIAN_POINT('Ctrl Pts',(130.848730782378,-31.7111522455224,17.620475932065));
#24728=CARTESIAN_POINT('Ctrl Pts',(130.440723554191,-31.6330853269384,17.6471676354725));
#24729=CARTESIAN_POINT('Ctrl Pts',(130.241457003235,-31.6129553756024,17.6597912237735));
#24730=CARTESIAN_POINT('Ctrl Pts',(129.996504147064,-31.6099524303263,17.6746053971701));
#24731=CARTESIAN_POINT('Ctrl Pts',(129.951447474415,-31.6102982888666,17.6773029781026));
#24732=CARTESIAN_POINT('Ctrl Pts',(129.877901061925,-31.612329671128,17.6816634435273));
#24733=CARTESIAN_POINT('Ctrl Pts',(129.84940317427,-31.613476845188,17.6833425559684));
#24734=CARTESIAN_POINT('Ctrl Pts',(129.793965853927,-31.6164096454853,17.6865895372866));
#24735=CARTESIAN_POINT('Ctrl Pts',(129.767026665636,-31.6181577145443,17.6881584330661));
#24736=CARTESIAN_POINT('Ctrl Pts',(129.703130681684,-31.6230710291277,17.6918597855181));
#24737=CARTESIAN_POINT('Ctrl Pts',(129.666198903818,-31.6265214321399,17.6939833455082));
#24738=CARTESIAN_POINT('Ctrl Pts',(129.541890723164,-31.6401965635318,17.7010842142481));
#24739=CARTESIAN_POINT('Ctrl Pts',(129.454854740657,-31.6532162297086,17.705976729016));
#24740=CARTESIAN_POINT('Ctrl Pts',(129.102215377666,-31.7200913790053,17.7256267014328));
#24741=CARTESIAN_POINT('Ctrl Pts',(128.843043375157,-31.8023039745643,17.7395819899753));
#24742=CARTESIAN_POINT('Ctrl Pts',(128.536169557994,-31.9418979547433,17.7578435251758));
#24743=CARTESIAN_POINT('Ctrl Pts',(128.4767287526,-31.9710675944567,17.7614733431461));
#24744=CARTESIAN_POINT('Ctrl Pts',(128.378398845571,-32.022948073835,17.767695627102));
#24745=CARTESIAN_POINT('Ctrl Pts',(128.339038193529,-32.0447277699912,17.7702471671157));
#24746=CARTESIAN_POINT('Ctrl Pts',(128.283021520079,-32.0771964229438,17.7739835673084));
#24747=CARTESIAN_POINT('Ctrl Pts',(128.266005979289,-32.0872589291292,17.7751328041374));
#24748=CARTESIAN_POINT('Ctrl Pts',(128.23626218091,-32.1052015532937,17.7771686632877));
#24749=CARTESIAN_POINT('Ctrl Pts',(128.223496593929,-32.1130180502889,17.7780513348182));
#24750=CARTESIAN_POINT('Ctrl Pts',(128.195387319012,-32.130486680041,17.7800151047999));
#24751=CARTESIAN_POINT('Ctrl Pts',(128.180069212159,-32.1401773627175,17.7810985249039));
#24752=CARTESIAN_POINT('Ctrl Pts',(128.134522445272,-32.1695057047648,17.7843580694332));
#24753=CARTESIAN_POINT('Ctrl Pts',(128.104529448348,-32.1895026015404,17.7865551929456));
#24754=CARTESIAN_POINT('Ctrl Pts',(127.950109119443,-32.2960536835067,17.7981105954731));
#24755=CARTESIAN_POINT('Ctrl Pts',(127.831279267454,-32.3903982079125,17.8078311676037));
#24756=CARTESIAN_POINT('Ctrl Pts',(127.620274920782,-32.5823182342661,17.8262058188554));
#24757=CARTESIAN_POINT('Ctrl Pts',(127.526783218911,-32.6780443680471,17.8348355513102));
#24758=CARTESIAN_POINT('Ctrl Pts',(127.345737839644,-32.8867938804341,17.8523767568404));
#24759=CARTESIAN_POINT('Ctrl Pts',(127.259173822995,-33.0003430635596,17.8612498184799));
#24760=CARTESIAN_POINT('Ctrl Pts',(127.15662883227,-33.1540797984807,17.8723963115759));
#24761=CARTESIAN_POINT('Ctrl Pts',(127.133899371468,-33.1895723115996,17.8749145222812));
#24762=CARTESIAN_POINT('Ctrl Pts',(127.097225588055,-33.2492616416814,17.8790606277824));
#24763=CARTESIAN_POINT('Ctrl Pts',(127.082908266727,-33.2732226619712,17.8807018318563));
#24764=CARTESIAN_POINT('Ctrl Pts',(127.055322196428,-33.3207123116181,17.8839103644606));
#24765=CARTESIAN_POINT('Ctrl Pts',(127.042035519745,-33.3442280644754,17.8854782469751));
#24766=CARTESIAN_POINT('Ctrl Pts',(127.013287952726,-33.3965582904307,17.8889227133214));
#24767=CARTESIAN_POINT('Ctrl Pts',(126.997959980009,-33.4254429217099,17.8907945805525));
#24768=CARTESIAN_POINT('Ctrl Pts',(126.94586323027,-33.5271432253532,17.8972881061284));
#24769=CARTESIAN_POINT('Ctrl Pts',(126.911305318637,-33.6010628842526,17.901835336003));
#24770=CARTESIAN_POINT('Ctrl Pts',(126.858897982631,-33.7245975362169,17.9092034732774));
#24771=CARTESIAN_POINT('Ctrl Pts',(126.839492810672,-33.7734760436544,17.9120614947518));
#24772=CARTESIAN_POINT('Ctrl Pts',(126.821241975899,-33.822756402985,17.9148966234937));
#24773=CARTESIAN_POINT('Origin',(130.,-35.,23.));
#24774=CARTESIAN_POINT('',(126.821241915874,-33.8227565650612,19.1602708352289));
#24775=CARTESIAN_POINT('',(126.821241893434,-33.8227566256554,18.8206072661261));
#24776=CARTESIAN_POINT('',(126.821241915871,-33.8227565650715,23.));
#24777=CARTESIAN_POINT('',(126.610251067749,-34.9973094977347,17.6410178032139));
#24778=CARTESIAN_POINT('Ctrl Pts',(126.821241893434,-33.8227566256554,18.8206072661261));
#24779=CARTESIAN_POINT('Ctrl Pts',(126.872479374406,-33.6844066790341,18.8127841894891));
#24780=CARTESIAN_POINT('Ctrl Pts',(126.932705550863,-33.5495191200307,18.8049941367639));
#24781=CARTESIAN_POINT('Ctrl Pts',(127.037869634602,-33.3500747900148,18.7926713874759));
#24782=CARTESIAN_POINT('Ctrl Pts',(127.076552171449,-33.2824667254386,18.7883412995881));
#24783=CARTESIAN_POINT('Ctrl Pts',(127.130542146319,-33.1952206221931,18.7824701353746));
#24784=CARTESIAN_POINT('Ctrl Pts',(127.143788586656,-33.17432936633,18.7810420946335));
#24785=CARTESIAN_POINT('Ctrl Pts',(127.164997311195,-33.1416764330164,18.778771873033));
#24786=CARTESIAN_POINT('Ctrl Pts',(127.172807166187,-33.1298162150347,18.7779392259102));
#24787=CARTESIAN_POINT('Ctrl Pts',(127.189336970124,-33.1050538545283,18.7761830540479));
#24788=CARTESIAN_POINT('Ctrl Pts',(127.198071642585,-33.0921622158202,18.7752584997376));
#24789=CARTESIAN_POINT('Ctrl Pts',(127.220391478412,-33.0597039032994,18.7729054933203));
#24790=CARTESIAN_POINT('Ctrl Pts',(127.234094501365,-33.0402196095835,18.7714696213604));
#24791=CARTESIAN_POINT('Ctrl Pts',(127.292175730443,-32.9594566312733,18.7654249352887));
#24792=CARTESIAN_POINT('Ctrl Pts',(127.338391257065,-32.8995317784167,18.7607139581683));
#24793=CARTESIAN_POINT('Ctrl Pts',(127.482307380556,-32.7253071129506,18.7464425807166));
#24794=CARTESIAN_POINT('Ctrl Pts',(127.585646593267,-32.6159070946926,18.7367079120512));
#24795=CARTESIAN_POINT('Ctrl Pts',(127.843950841067,-32.3765290529526,18.7140381619089));
#24796=CARTESIAN_POINT('Ctrl Pts',(128.003976365774,-32.2528090965189,18.7012126145115));
#24797=CARTESIAN_POINT('Ctrl Pts',(128.218745824074,-32.1154984803714,18.68569093999));
#24798=CARTESIAN_POINT('Ctrl Pts',(128.264076154793,-32.0879930745865,18.6824993711428));
#24799=CARTESIAN_POINT('Ctrl Pts',(128.336414855755,-32.0463893949651,18.6775352697771));
#24800=CARTESIAN_POINT('Ctrl Pts',(128.362998427676,-32.0315732986999,18.6757376260792));
#24801=CARTESIAN_POINT('Ctrl Pts',(128.41306159038,-32.0045481783305,18.6724005284951));
#24802=CARTESIAN_POINT('Ctrl Pts',(128.436491426823,-31.9922523157666,18.6708581275333));
#24803=CARTESIAN_POINT('Ctrl Pts',(128.489529453397,-31.965205471087,18.6674087726325));
#24804=CARTESIAN_POINT('Ctrl Pts',(128.519214639358,-31.9506108921657,18.6655073023659));
#24805=CARTESIAN_POINT('Ctrl Pts',(128.610903353846,-31.907187279465,18.6597189049237));
#24806=CARTESIAN_POINT('Ctrl Pts',(128.673571120008,-31.8797969116484,18.6558801290074));
#24807=CARTESIAN_POINT('Ctrl Pts',(128.82433161832,-31.8192674497629,18.646883010352));
#24808=CARTESIAN_POINT('Ctrl Pts',(128.913060561971,-31.7878636476055,18.6417756905233));
#24809=CARTESIAN_POINT('Ctrl Pts',(129.210783131956,-31.6962428785311,18.6250580347284));
#24810=CARTESIAN_POINT('Ctrl Pts',(129.424239369143,-31.6524387938148,18.6137671149021));
#24811=CARTESIAN_POINT('Ctrl Pts',(129.728490527445,-31.619980136382,18.5971368694424));
#24812=CARTESIAN_POINT('Ctrl Pts',(129.816899630509,-31.6140402425482,18.592236964465));
#24813=CARTESIAN_POINT('Ctrl Pts',(129.931168232004,-31.6108511249035,18.5857050149143));
#24814=CARTESIAN_POINT('Ctrl Pts',(129.956910556111,-31.610426114622,18.5842204741831));
#24815=CARTESIAN_POINT('Ctrl Pts',(129.998628748054,-31.6102126365942,18.5817899669335));
#24816=CARTESIAN_POINT('Ctrl Pts',(130.014603132038,-31.6102438177388,18.5808534404523));
#24817=CARTESIAN_POINT('Ctrl Pts',(130.046312340625,-31.6105298538767,18.5789817673671));
#24818=CARTESIAN_POINT('Ctrl Pts',(130.062046732567,-31.6107813761176,18.5780468085892));
#24819=CARTESIAN_POINT('Ctrl Pts',(130.102436165932,-31.6117083624268,18.5756318280374));
#24820=CARTESIAN_POINT('Ctrl Pts',(130.127086269569,-31.612543374149,18.5741436011085));
#24821=CARTESIAN_POINT('Ctrl Pts',(130.236231515571,-31.6174335860123,18.5674969431972));
#24822=CARTESIAN_POINT('Ctrl Pts',(130.320561165176,-31.6243816574958,18.5622103125906));
#24823=CARTESIAN_POINT('Ctrl Pts',(130.590819805894,-31.6568667108661,18.5449544077272));
#24824=CARTESIAN_POINT('Ctrl Pts',(130.774921413269,-31.6946852726754,18.5327380604987));
#24825=CARTESIAN_POINT('Ctrl Pts',(131.119304909335,-31.7957991067441,18.5097810698537));
#24826=CARTESIAN_POINT('Ctrl Pts',(131.279784417032,-31.856449069798,18.4990356839066));
#24827=CARTESIAN_POINT('Ctrl Pts',(131.475321083837,-31.9478183744436,18.48598938053));
#24828=CARTESIAN_POINT('Ctrl Pts',(131.515259950041,-31.9674478500741,18.4833259867266));
#24829=CARTESIAN_POINT('Ctrl Pts',(131.580010039091,-32.0008704467106,18.4790084581413));
#24830=CARTESIAN_POINT('Ctrl Pts',(131.605054064868,-32.0141983784849,18.4773386153349));
#24831=CARTESIAN_POINT('Ctrl Pts',(131.653591554047,-32.0408162650525,18.4741014986323));
#24832=CARTESIAN_POINT('Ctrl Pts',(131.677099357026,-32.0540754909154,18.4725333070905));
#24833=CARTESIAN_POINT('Ctrl Pts',(131.732712194422,-32.0863245478238,18.4688210940066));
#24834=CARTESIAN_POINT('Ctrl Pts',(131.764667424581,-32.1055665103633,18.4666862025069));
#24835=CARTESIAN_POINT('Ctrl Pts',(131.877453589975,-32.1760434378618,18.4591373253655));
#24836=CARTESIAN_POINT('Ctrl Pts',(131.956427944607,-32.2301706697105,18.4538273535168));
#24837=CARTESIAN_POINT('Ctrl Pts',(132.159303587464,-32.3822293628704,18.4399913404817));
#24838=CARTESIAN_POINT('Ctrl Pts',(132.278835326839,-32.4855959242417,18.4316394144455));
#24839=CARTESIAN_POINT('Ctrl Pts',(132.52336848855,-32.7288722685458,18.4133516375025));
#24840=CARTESIAN_POINT('Ctrl Pts',(132.64483913155,-32.8715684590044,18.403440393696));
#24841=CARTESIAN_POINT('Ctrl Pts',(132.774104580174,-33.0516804879517,18.3909148352169));
#24842=CARTESIAN_POINT('Ctrl Pts',(132.793869980971,-33.0801313903786,18.3889354357717));
#24843=CARTESIAN_POINT('Ctrl Pts',(132.823265630189,-33.123859791205,18.3858838012358));
#24844=CARTESIAN_POINT('Ctrl Pts',(132.833216113432,-33.138920387393,18.3848311294798));
#24845=CARTESIAN_POINT('Ctrl Pts',(132.851183733382,-33.166593413168,18.3828925184227));
#24846=CARTESIAN_POINT('Ctrl Pts',(132.859238425888,-33.1791804066967,18.3820090016143));
#24847=CARTESIAN_POINT('Ctrl Pts',(132.877759871358,-33.2085496471616,18.3799436211155));
#24848=CARTESIAN_POINT('Ctrl Pts',(132.888163230465,-33.2253706425049,18.378757909768));
#24849=CARTESIAN_POINT('Ctrl Pts',(132.921850351345,-33.2809195608662,18.3748356537938));
#24850=CARTESIAN_POINT('Ctrl Pts',(132.944506054018,-33.3200206216849,18.372064344113));
#24851=CARTESIAN_POINT('Ctrl Pts',(132.998623802116,-33.4178806216072,18.3651243598338));
#24852=CARTESIAN_POINT('Ctrl Pts',(133.029146924831,-33.4771361038905,18.3609187200448));
#24853=CARTESIAN_POINT('Ctrl Pts',(133.177026067828,-33.7862796863532,18.3390900475411));
#24854=CARTESIAN_POINT('Ctrl Pts',(133.265301156773,-34.0489725543816,18.3210233726508));
#24855=CARTESIAN_POINT('Ctrl Pts',(133.337659882871,-34.4020544940123,18.2986418583056));
#24856=CARTESIAN_POINT('Ctrl Pts',(133.351499164393,-34.4852500478249,18.2934898142347));
#24857=CARTESIAN_POINT('Ctrl Pts',(133.366429082766,-34.6016858558133,18.2864479223638));
#24858=CARTESIAN_POINT('Ctrl Pts',(133.370155257105,-34.6345515275437,18.2844786358201));
#24859=CARTESIAN_POINT('Ctrl Pts',(133.376058582061,-34.6944382097129,18.2809226455731));
#24860=CARTESIAN_POINT('Ctrl Pts',(133.378393736691,-34.7214405258275,18.279331207424));
#24861=CARTESIAN_POINT('Ctrl Pts',(133.382466923121,-34.7761812699939,18.2761281119568));
#24862=CARTESIAN_POINT('Ctrl Pts',(133.384188170422,-34.8039188838642,18.2745170891414));
#24863=CARTESIAN_POINT('Ctrl Pts',(133.387630316049,-34.873151788719,18.2705242603528));
#24864=CARTESIAN_POINT('Ctrl Pts',(133.388930157072,-34.9146640198602,18.268155480267));
#24865=CARTESIAN_POINT('Ctrl Pts',(133.391211033744,-35.0911335231722,18.258180995659));
#24866=CARTESIAN_POINT('Ctrl Pts',(133.384895344212,-35.2260670193766,18.2507971253351));
#24867=CARTESIAN_POINT('Ctrl Pts',(133.355835061997,-35.4979398308932,18.2360976861326));
#24868=CARTESIAN_POINT('Ctrl Pts',(133.332699803436,-35.6345753081353,18.2288024029005));
#24869=CARTESIAN_POINT('Ctrl Pts',(133.2630799492,-35.9332890870801,18.2125030741845));
#24870=CARTESIAN_POINT('Ctrl Pts',(133.212740722508,-36.094076702464,18.2034922062943));
#24871=CARTESIAN_POINT('Ctrl Pts',(133.140089794339,-36.2771317983322,18.1922827891402));
#24872=CARTESIAN_POINT('Ctrl Pts',(133.129159248019,-36.3036839463369,18.1906323372373));
#24873=CARTESIAN_POINT('Ctrl Pts',(133.111371119638,-36.3453813908292,18.1879967718016));
#24874=CARTESIAN_POINT('Ctrl Pts',(133.104736922516,-36.3606211623851,18.1870241875102));
#24875=CARTESIAN_POINT('Ctrl Pts',(133.091756207061,-36.3898505662743,18.1851396671487));
#24876=CARTESIAN_POINT('Ctrl Pts',(133.085426242942,-36.4038468240844,18.184228670821));
#24877=CARTESIAN_POINT('Ctrl Pts',(133.069542534958,-36.4383411049273,18.1819629060496));
#24878=CARTESIAN_POINT('Ctrl Pts',(133.059878442487,-36.4587872925124,18.1806018248118));
#24879=CARTESIAN_POINT('Ctrl Pts',(133.02177986218,-36.5373474708199,18.1753063967178));
#24880=CARTESIAN_POINT('Ctrl Pts',(132.991889921864,-36.5947364601631,18.1712981279529));
#24881=CARTESIAN_POINT('Ctrl Pts',(132.904597971617,-36.7512361804467,18.1600431191));
#24882=CARTESIAN_POINT('Ctrl Pts',(132.843788341487,-36.8483460157888,18.1526885743109));
#24883=CARTESIAN_POINT('Ctrl Pts',(132.631465179245,-37.1520617793127,18.1288196479806));
#24884=CARTESIAN_POINT('Ctrl Pts',(132.461411011713,-37.3446694078615,18.1123734838229));
#24885=CARTESIAN_POINT('Ctrl Pts',(132.233803173838,-37.5501127231479,18.0937499008354));
#24886=CARTESIAN_POINT('Ctrl Pts',(132.195591825298,-37.583085067533,18.090718049193));
#24887=CARTESIAN_POINT('Ctrl Pts',(132.133794364905,-37.6340472351923,18.0859601753148));
#24888=CARTESIAN_POINT('Ctrl Pts',(132.110685048688,-37.6526009759333,18.0842119226885));
#24889=CARTESIAN_POINT('Ctrl Pts',(132.066359731432,-37.6872423028046,18.0809157832972));
#24890=CARTESIAN_POINT('Ctrl Pts',(132.045191826167,-37.7033875392322,18.0793657187491));
#24891=CARTESIAN_POINT('Ctrl Pts',(131.996183847535,-37.7398619035306,18.0758304275401));
#24892=CARTESIAN_POINT('Ctrl Pts',(131.968219244793,-37.7600192630136,18.0738518384433));
#24893=CARTESIAN_POINT('Ctrl Pts',(131.877336565676,-37.8234451659866,18.0675397857226));
#24894=CARTESIAN_POINT('Ctrl Pts',(131.813260478001,-37.8650170688038,18.0632685564321));
#24895=CARTESIAN_POINT('Ctrl Pts',(131.653346132881,-37.9612517954993,18.0529807859348));
#24896=CARTESIAN_POINT('Ctrl Pts',(131.556138539751,-38.0134698723063,18.0470393456623));
#24897=CARTESIAN_POINT('Ctrl Pts',(131.26405781251,-38.152460730579,18.0297841027004));
#24898=CARTESIAN_POINT('Ctrl Pts',(131.063363848881,-38.2256931656923,18.0186901417195));
#24899=CARTESIAN_POINT('Ctrl Pts',(130.79039754933,-38.2970343272597,18.0031905499797));
#24900=CARTESIAN_POINT('Ctrl Pts',(130.723144287412,-38.3124348622644,17.9993373986244));
#24901=CARTESIAN_POINT('Ctrl Pts',(130.63214379847,-38.3303700489791,17.9940222027271));
#24902=CARTESIAN_POINT('Ctrl Pts',(130.608767773328,-38.3347222035616,17.9926479188277));
#24903=CARTESIAN_POINT('Ctrl Pts',(130.571542219136,-38.3412484237817,17.9904425171903));
#24904=CARTESIAN_POINT('Ctrl Pts',(130.557721218131,-38.3435831924806,17.9896200133399));
#24905=CARTESIAN_POINT('Ctrl Pts',(130.528418821226,-38.3483464844744,17.9878676412538));
#24906=CARTESIAN_POINT('Ctrl Pts',(130.512934484609,-38.3507534696772,17.9869365395897));
#24907=CARTESIAN_POINT('Ctrl Pts',(130.473101252477,-38.3566628375464,17.9845291745354));
#24908=CARTESIAN_POINT('Ctrl Pts',(130.44873021279,-38.3600076367347,17.9830446835731));
#24909=CARTESIAN_POINT('Ctrl Pts',(130.340283266068,-38.3736905512696,17.9763938969927));
#24910=CARTESIAN_POINT('Ctrl Pts',(130.255879136783,-38.3811394912298,17.9710980995961));
#24911=CARTESIAN_POINT('Ctrl Pts',(129.983389289538,-38.3949266414624,17.9537936223479));
#24912=CARTESIAN_POINT('Ctrl Pts',(129.795023440882,-38.388773793292,17.9415341060517));
#24913=CARTESIAN_POINT('Ctrl Pts',(129.437052341674,-38.3471125981063,17.9184678384327));
#24914=CARTESIAN_POINT('Ctrl Pts',(129.267712327729,-38.3141879324533,17.9076576356069));
#24915=CARTESIAN_POINT('Ctrl Pts',(129.058730850768,-38.2567457812821,17.8945556969853));
#24916=CARTESIAN_POINT('Ctrl Pts',(129.01610672144,-38.2441231472432,17.8918950544516));
#24917=CARTESIAN_POINT('Ctrl Pts',(128.946795296086,-38.2221055674022,17.8875859317341));
#24918=CARTESIAN_POINT('Ctrl Pts',(128.919956556696,-38.2132087808207,17.8859216547072));
#24919=CARTESIAN_POINT('Ctrl Pts',(128.867856397371,-38.1952115208429,17.882698338912));
#24920=CARTESIAN_POINT('Ctrl Pts',(128.842585664371,-38.1861446791763,17.8811383458599));
#24921=CARTESIAN_POINT('Ctrl Pts',(128.782739572441,-38.163866604405,17.8774508339721));
#24922=CARTESIAN_POINT('Ctrl Pts',(128.748267254708,-38.1503872978444,17.8753322919282));
#24923=CARTESIAN_POINT('Ctrl Pts',(128.626792755377,-38.1005797848743,17.867879709799));
#24924=CARTESIAN_POINT('Ctrl Pts',(128.541089620823,-38.0611886156602,17.8626467271575));
#24925=CARTESIAN_POINT('Ctrl Pts',(128.319971360017,-37.9481585207498,17.8490894622658));
#24926=CARTESIAN_POINT('Ctrl Pts',(128.187742043829,-37.8687731229112,17.8409305495564));
#24927=CARTESIAN_POINT('Ctrl Pts',(127.903132206333,-37.6703481708868,17.8225442555283));
#24928=CARTESIAN_POINT('Ctrl Pts',(127.754618625309,-37.5467352224207,17.8123493429224));
#24929=CARTESIAN_POINT('Ctrl Pts',(127.592876456827,-37.3869129949111,17.7995020696251));
#24930=CARTESIAN_POINT('Ctrl Pts',(127.568687843633,-37.3622697565442,17.7975289659534));
#24931=CARTESIAN_POINT('Ctrl Pts',(127.532474516033,-37.3242303670103,17.7944869797433));
#24932=CARTESIAN_POINT('Ctrl Pts',(127.520172400123,-37.3111001398097,17.7934376143206));
#24933=CARTESIAN_POINT('Ctrl Pts',(127.497835876034,-37.2868763629743,17.7915014614576));
#24934=CARTESIAN_POINT('Ctrl Pts',(127.487769518351,-37.2758134326629,17.7906170411775));
#24935=CARTESIAN_POINT('Ctrl Pts',(127.464521012875,-37.2499211180624,17.7885469536882));
#24936=CARTESIAN_POINT('Ctrl Pts',(127.451395444455,-37.2350421716924,17.7873573817174));
#24937=CARTESIAN_POINT('Ctrl Pts',(127.408718700198,-37.1857997149593,17.7834229196771));
#24938=CARTESIAN_POINT('Ctrl Pts',(127.379727158317,-37.1509600143214,17.7806431702724));
#24939=CARTESIAN_POINT('Ctrl Pts',(127.309722490491,-37.0633179667377,17.7736815097468));
#24940=CARTESIAN_POINT('Ctrl Pts',(127.269556988181,-37.0098642165119,17.7694625353038));
#24941=CARTESIAN_POINT('Ctrl Pts',(127.078705362645,-36.7395841170604,17.7483860149391));
#24942=CARTESIAN_POINT('Ctrl Pts',(126.952109567845,-36.5068195970155,17.731116821213));
#24943=CARTESIAN_POINT('Ctrl Pts',(126.81899010555,-36.1748767563502,17.7088108716309));
#24944=CARTESIAN_POINT('Ctrl Pts',(126.787772220534,-36.0866252862021,17.7030738942789));
#24945=CARTESIAN_POINT('Ctrl Pts',(126.74903620437,-35.960776209736,17.6951634063781));
#24946=CARTESIAN_POINT('Ctrl Pts',(126.738442944244,-35.9241765386893,17.692894075791));
#24947=CARTESIAN_POINT('Ctrl Pts',(126.721406087775,-35.8613679941586,17.6890512677439));
#24948=CARTESIAN_POINT('Ctrl Pts',(126.714654492358,-35.835247161283,17.6874681773312));
#24949=CARTESIAN_POINT('Ctrl Pts',(126.701459571084,-35.7815607998907,17.6842442175936));
#24950=CARTESIAN_POINT('Ctrl Pts',(126.695048248268,-35.7539895451384,17.6826044651235));
#24951=CARTESIAN_POINT('Ctrl Pts',(126.68281683795,-35.6982327706171,17.6793190421195));
#24952=CARTESIAN_POINT('Ctrl Pts',(126.677008842061,-35.6700469891726,17.6776738631822));
#24953=CARTESIAN_POINT('Ctrl Pts',(126.663698493986,-35.6010171084343,17.6736804751609));
#24954=CARTESIAN_POINT('Ctrl Pts',(126.656586298347,-35.5601020621826,17.6713440228477));
#24955=CARTESIAN_POINT('Ctrl Pts',(126.623479488232,-35.3464483074093,17.6592834070774));
#24956=CARTESIAN_POINT('Ctrl Pts',(126.610113414419,-35.1720170055958,17.6499289047321));
#24957=CARTESIAN_POINT('Ctrl Pts',(126.610251052174,-34.9973291930011,17.6406471279412));
#24958=CARTESIAN_POINT('Ctrl Pts',(126.610251067749,-34.9973094977347,17.6410178032139));
#24959=CARTESIAN_POINT('Ctrl Pts',(126.610355871654,-34.865267636549,17.6332712573477));
#24960=CARTESIAN_POINT('Ctrl Pts',(126.618179523068,-34.733553041647,17.6255247114816));
#24961=CARTESIAN_POINT('Ctrl Pts',(126.633585920167,-34.6029341293948,17.6177781656156));
#24962=CARTESIAN_POINT('Ctrl Pts',(126.649300610227,-34.4697014398218,17.6098766058579));
#24963=CARTESIAN_POINT('Ctrl Pts',(126.672904558712,-34.3376084643416,17.6019750461003));
#24964=CARTESIAN_POINT('Ctrl Pts',(126.704204838343,-34.2074475948576,17.5940734863427));
#24965=CARTESIAN_POINT('Ctrl Pts',(126.707948416483,-34.191880085832,17.5931284434636));
#24966=CARTESIAN_POINT('Ctrl Pts',(126.711802031722,-34.1763401910708,17.5921834005845));
#24967=CARTESIAN_POINT('Ctrl Pts',(126.715765308226,-34.1608292475032,17.5912383577054));
#24968=CARTESIAN_POINT('Ctrl Pts',(126.741359218008,-34.0606632131708,17.5851354925212));
#24969=CARTESIAN_POINT('Ctrl Pts',(126.77158242967,-33.9615021246093,17.579032627337));
#24970=CARTESIAN_POINT('Ctrl Pts',(126.806339696859,-33.863805064858,17.5729297621527));
#24971=CARTESIAN_POINT('Ctrl Pts',(126.811217984641,-33.8500929864498,17.5720732065293));
#24972=CARTESIAN_POINT('Ctrl Pts',(126.816185505764,-33.8364097348622,17.5712166509059));
#24973=CARTESIAN_POINT('Ctrl Pts',(126.821241915871,-33.8227565650715,17.5703600952825));
#24974=CARTESIAN_POINT('Ctrl Pts',(126.821241975899,-33.822756402985,17.9148966234937));
#24975=CARTESIAN_POINT('Ctrl Pts',(126.742546197666,-34.0352483945782,17.9271214157023));
#24976=CARTESIAN_POINT('Ctrl Pts',(126.685311296885,-34.2552138019534,17.9388788299414));
#24977=CARTESIAN_POINT('Ctrl Pts',(126.640195493197,-34.5454746126536,17.9547793874544));
#24978=CARTESIAN_POINT('Ctrl Pts',(126.631880958229,-34.611859722398,17.9584447972027));
#24979=CARTESIAN_POINT('Ctrl Pts',(126.621238169152,-34.7235468980125,17.9647214780077));
#24980=CARTESIAN_POINT('Ctrl Pts',(126.617845161582,-34.7687294485601,17.9672907212788));
#24981=CARTESIAN_POINT('Ctrl Pts',(126.614272276037,-34.8337326882671,17.9710471355269));
#24982=CARTESIAN_POINT('Ctrl Pts',(126.613358943449,-34.8535098883138,17.9721980028177));
#24983=CARTESIAN_POINT('Ctrl Pts',(126.612060270353,-34.8882286937041,17.9742340908642));
#24984=CARTESIAN_POINT('Ctrl Pts',(126.61160041897,-34.9031666160634,17.9751153082091));
#24985=CARTESIAN_POINT('Ctrl Pts',(126.610803622922,-34.9361385413936,17.9770722020195));
#24986=CARTESIAN_POINT('Ctrl Pts',(126.610511815254,-34.9541722615471,17.978150144148));
#24987=CARTESIAN_POINT('Ctrl Pts',(126.610071562035,-35.0078655716658,17.9813806106298));
#24988=CARTESIAN_POINT('Ctrl Pts',(126.610341899981,-35.0435250438162,17.983553654545));
#24989=CARTESIAN_POINT('Ctrl Pts',(126.615219413334,-35.2522987528171,17.9964123801132));
#24990=CARTESIAN_POINT('Ctrl Pts',(126.632524775447,-35.4248481566212,18.0075757552706));
#24991=CARTESIAN_POINT('Ctrl Pts',(126.692217547691,-35.7594643548647,18.0294869038277));
#24992=CARTESIAN_POINT('Ctrl Pts',(126.733577611508,-35.9212513033148,18.0402040886711));
#24993=CARTESIAN_POINT('Ctrl Pts',(126.818119506551,-36.1729406631513,18.05679038483));
#24994=CARTESIAN_POINT('Ctrl Pts',(126.853633743345,-36.2651227487906,18.062849467648));
#24995=CARTESIAN_POINT('Ctrl Pts',(126.908200264692,-36.3901799965359,18.0710431028602));
#24996=CARTESIAN_POINT('Ctrl Pts',(126.92385123098,-36.4244770791736,18.0732876594508));
#24997=CARTESIAN_POINT('Ctrl Pts',(126.951712606116,-36.4829298758816,18.0771100750361));
#24998=CARTESIAN_POINT('Ctrl Pts',(126.963645910807,-36.5072129779049,18.0786971296182));
#24999=CARTESIAN_POINT('Ctrl Pts',(126.988628986083,-36.5565498621974,18.0819207510702));
#25000=CARTESIAN_POINT('Ctrl Pts',(127.001703768039,-36.5815886420373,18.0835562987486));
#25001=CARTESIAN_POINT('Ctrl Pts',(127.035892859641,-36.6451141874476,18.0877064703405));
#25002=CARTESIAN_POINT('Ctrl Pts',(127.057444890778,-36.6833601834662,18.0902056770278));
#25003=CARTESIAN_POINT('Ctrl Pts',(127.158033880521,-36.8540261765712,18.1013763490971));
#25004=CARTESIAN_POINT('Ctrl Pts',(127.245311037512,-36.9813834030212,18.1097524451115));
#25005=CARTESIAN_POINT('Ctrl Pts',(127.361761917975,-37.1286684165079,18.1197877427296));
#25006=CARTESIAN_POINT('Ctrl Pts',(127.382947691325,-37.1546616099905,18.121573565333));
#25007=CARTESIAN_POINT('Ctrl Pts',(127.527383069498,-37.326598263652,18.1335087744686));
#25008=CARTESIAN_POINT('Ctrl Pts',(127.662385320098,-37.4622027197175,18.1435048935434));
#25009=CARTESIAN_POINT('Ctrl Pts',(127.860000073998,-37.6297221624873,18.1577444317777));
#25010=CARTESIAN_POINT('Ctrl Pts',(127.913233223272,-37.6721604618926,18.1615482296479));
#25011=CARTESIAN_POINT('Ctrl Pts',(127.986639249914,-37.7271492989601,18.1668050267503));
#25012=CARTESIAN_POINT('Ctrl Pts',(128.005721961065,-37.7411347731954,18.1681726127466));
#25013=CARTESIAN_POINT('Ctrl Pts',(128.036322262084,-37.7630726810373,18.1703699412898));
#25014=CARTESIAN_POINT('Ctrl Pts',(128.04774576274,-37.771155765516,18.1711911762168));
#25015=CARTESIAN_POINT('Ctrl Pts',(128.072168910665,-37.7882112267234,18.1729497030175));
#25016=CARTESIAN_POINT('Ctrl Pts',(128.085181804485,-37.797163886516,18.1738883093237));
#25017=CARTESIAN_POINT('Ctrl Pts',(128.118877158737,-37.8200004330194,18.176321943342));
#25018=CARTESIAN_POINT('Ctrl Pts',(128.139650614521,-37.833747637063,18.1778253925099));
#25019=CARTESIAN_POINT('Ctrl Pts',(128.233896834548,-37.894633817142,18.1846534521182));
#25020=CARTESIAN_POINT('Ctrl Pts',(128.309017618409,-37.9391497939088,18.1901145102757));
#25021=CARTESIAN_POINT('Ctrl Pts',(128.562564195531,-38.0764603716429,18.2084111320971));
#25022=CARTESIAN_POINT('Ctrl Pts',(128.747529951231,-38.1562876207681,18.2215191385987));
#25023=CARTESIAN_POINT('Ctrl Pts',(129.086265750315,-38.2679824174949,18.2442529740116));
#25024=CARTESIAN_POINT('Ctrl Pts',(129.237242419853,-38.3064831384604,18.2539759954902));
#25025=CARTESIAN_POINT('Ctrl Pts',(129.433612589681,-38.3423860922147,18.2660370087093));
#25026=CARTESIAN_POINT('Ctrl Pts',(129.477028794827,-38.3494538180393,18.2686686583663));
#25027=CARTESIAN_POINT('Ctrl Pts',(129.54856497468,-38.3596742537292,18.2729492882096));
#25028=CARTESIAN_POINT('Ctrl Pts',(129.576607664316,-38.3633233082362,18.2746134255675));
#25029=CARTESIAN_POINT('Ctrl Pts',(129.631578842907,-38.3697779908043,18.2778494120573));
#25030=CARTESIAN_POINT('Ctrl Pts',(129.65850170181,-38.3726127602939,18.2794220475535));
#25031=CARTESIAN_POINT('Ctrl Pts',(129.722985151813,-38.3786222768921,18.283160893169));
#25032=CARTESIAN_POINT('Ctrl Pts',(129.760570812204,-38.381493684856,18.2853176406677));
#25033=CARTESIAN_POINT('Ctrl Pts',(129.896601036891,-38.3896063762216,18.2930495096983));
#25034=CARTESIAN_POINT('Ctrl Pts',(129.995218555166,-38.3911800628745,18.2985135970312));
#25035=CARTESIAN_POINT('Ctrl Pts',(130.259982339619,-38.3838530728876,18.3129496554169));
#25036=CARTESIAN_POINT('Ctrl Pts',(130.425635436939,-38.3670298453148,18.3217256475646));
#25037=CARTESIAN_POINT('Ctrl Pts',(130.760502564446,-38.3079048222386,18.3397663067097));
#25038=CARTESIAN_POINT('Ctrl Pts',(130.929025161924,-38.264582429495,18.3490119741938));
#25039=CARTESIAN_POINT('Ctrl Pts',(131.127198495656,-38.1970453090688,18.3608337963474));
#25040=CARTESIAN_POINT('Ctrl Pts',(131.160746944978,-38.1850182850464,18.3628694341934));
#25041=CARTESIAN_POINT('Ctrl Pts',(131.210981919776,-38.1661101213727,18.3659782799465));
#25042=CARTESIAN_POINT('Ctrl Pts',(131.227814304606,-38.1596206279186,18.3670303620466));
#25043=CARTESIAN_POINT('Ctrl Pts',(131.258500617846,-38.1475077117334,18.3689688014109));
#25044=CARTESIAN_POINT('Ctrl Pts',(131.272370277748,-38.1419265507441,18.3698527520082));
#25045=CARTESIAN_POINT('Ctrl Pts',(131.304534209077,-38.1287358676301,18.3719206923424));
#25046=CARTESIAN_POINT('Ctrl Pts',(131.322799120678,-38.1210575253567,18.3731085551237));
#25047=CARTESIAN_POINT('Ctrl Pts',(131.382693801934,-38.0952583572703,18.3770460636406));
#25048=CARTESIAN_POINT('Ctrl Pts',(131.424025266718,-38.0764619393618,18.3798308321482));
#25049=CARTESIAN_POINT('Ctrl Pts',(131.525470725824,-38.0278451003667,18.3868131419406));
#25050=CARTESIAN_POINT('Ctrl Pts',(131.58509968408,-37.9970593870271,18.3910481812307));
#25051=CARTESIAN_POINT('Ctrl Pts',(131.890786374131,-37.8275620167856,18.4133166027036));
#25052=CARTESIAN_POINT('Ctrl Pts',(132.119756924759,-37.6602346346548,18.4318015867138));
#25053=CARTESIAN_POINT('Ctrl Pts',(132.382870797524,-37.4121750693482,18.4541959423932));
#25054=CARTESIAN_POINT('Ctrl Pts',(132.438511173619,-37.3559131115129,18.4590199506016));
#25055=CARTESIAN_POINT('Ctrl Pts',(132.514032687282,-37.2740026894461,18.4656968409419));
#25056=CARTESIAN_POINT('Ctrl Pts',(132.535589703829,-37.2499407873399,18.4676187016614));
#25057=CARTESIAN_POINT('Ctrl Pts',(132.57446485489,-37.2052799500275,18.4711152887041));
#25058=CARTESIAN_POINT('Ctrl Pts',(132.591887789899,-37.1847761198377,18.472694218555));
#25059=CARTESIAN_POINT('Ctrl Pts',(132.626961324399,-37.1424903891693,18.4758981838077));
#25060=CARTESIAN_POINT('Ctrl Pts',(132.644589549149,-37.1206925880053,18.4775222555223));
#25061=CARTESIAN_POINT('Ctrl Pts',(132.688436208715,-37.0650778526825,18.4815987891301));
#25062=CARTESIAN_POINT('Ctrl Pts',(132.714288903343,-37.0309780319581,18.4840369732826));
#25063=CARTESIAN_POINT('Ctrl Pts',(132.828873267993,-36.8737434000694,18.4950192977643));
#25064=CARTESIAN_POINT('Ctrl Pts',(132.909923400294,-36.7452194459429,18.5032763502417));
#25065=CARTESIAN_POINT('Ctrl Pts',(133.003058114906,-36.5728926723312,18.5137573189503));
#25066=CARTESIAN_POINT('Ctrl Pts',(133.023264564435,-36.5336951625509,18.5161050236613));
#25067=CARTESIAN_POINT('Ctrl Pts',(133.131185549468,-36.3139186180434,18.5291112895381));
#25068=CARTESIAN_POINT('Ctrl Pts',(133.203480922128,-36.1262336873626,18.5396166872158));
#25069=CARTESIAN_POINT('Ctrl Pts',(133.274168459502,-35.8794117713362,18.5538461856615));
#25070=CARTESIAN_POINT('Ctrl Pts',(133.288255491707,-35.8251783221317,18.5569988105232));
#25071=CARTESIAN_POINT('Ctrl Pts',(133.305997809209,-35.7491785622284,18.5614837708066));
#25072=CARTESIAN_POINT('Ctrl Pts',(133.310795041277,-35.7276854898212,18.5627595369943));
#25073=CARTESIAN_POINT('Ctrl Pts',(133.318524602358,-35.691394999471,18.5649283821967));
#25074=CARTESIAN_POINT('Ctrl Pts',(133.321568274232,-35.6766215898298,18.5658154125245));
#25075=CARTESIAN_POINT('Ctrl Pts',(133.327784335631,-35.6453969083609,18.5676996797267));
#25076=CARTESIAN_POINT('Ctrl Pts',(133.330933483938,-35.6289418519974,18.568698072102));
#25077=CARTESIAN_POINT('Ctrl Pts',(133.339268824645,-35.5835682907358,18.5714646538095));
#25078=CARTESIAN_POINT('Ctrl Pts',(133.344201108174,-35.5546053144903,18.5732457794629));
#25079=CARTESIAN_POINT('Ctrl Pts',(133.377084226314,-35.3450902651531,18.5862218493349));
#25080=CARTESIAN_POINT('Ctrl Pts',(133.390771218413,-35.1626177062943,18.5979964196479));
#25081=CARTESIAN_POINT('Ctrl Pts',(133.388291363512,-34.7433832583471,18.6250213381813));
#25082=CARTESIAN_POINT('Ctrl Pts',(133.362130793579,-34.5075786205291,18.6401649137118));
#25083=CARTESIAN_POINT('Ctrl Pts',(133.300529997481,-34.2256590417183,18.6577220000289));
#25084=CARTESIAN_POINT('Ctrl Pts',(133.288278822042,-34.175181826916,18.6608466664282));
#25085=CARTESIAN_POINT('Ctrl Pts',(133.267077481984,-34.0958309879908,18.6657306688188));
#25086=CARTESIAN_POINT('Ctrl Pts',(133.258893281555,-34.066762868622,18.6675138100103));
#25087=CARTESIAN_POINT('Ctrl Pts',(133.243557427608,-34.0149578041453,18.6706819713804));
#25088=CARTESIAN_POINT('Ctrl Pts',(133.23655242203,-33.9921798890356,18.6720715644554));
#25089=CARTESIAN_POINT('Ctrl Pts',(133.219549827643,-33.93889954081,18.6753148693733));
#25090=CARTESIAN_POINT('Ctrl Pts',(133.209357947523,-33.9084612040258,18.6771621894245));
#25091=CARTESIAN_POINT('Ctrl Pts',(133.177867064261,-33.8186694164423,18.6825986761169));
#25092=CARTESIAN_POINT('Ctrl Pts',(133.155342094371,-33.7597588996141,18.6861481439059));
#25093=CARTESIAN_POINT('Ctrl Pts',(133.071184427493,-33.5568209103673,18.6983564846071));
#25094=CARTESIAN_POINT('Ctrl Pts',(133.001223381791,-33.4164585476328,18.7067563143908));
#25095=CARTESIAN_POINT('Ctrl Pts',(132.822420502467,-33.112469274648,18.7254963833426));
#25096=CARTESIAN_POINT('Ctrl Pts',(132.708578115965,-32.9524592028829,18.7357545263718));
#25097=CARTESIAN_POINT('Ctrl Pts',(132.541560314946,-32.7561894822093,18.7499797088768));
#25098=CARTESIAN_POINT('Ctrl Pts',(132.500287046359,-32.7102886160496,18.7534410390833));
#25099=CARTESIAN_POINT('Ctrl Pts',(132.442054517504,-32.6489796613059,18.7582937228304));
#25100=CARTESIAN_POINT('Ctrl Pts',(132.426155886665,-32.6325764105409,18.759615607848));
#25101=CARTESIAN_POINT('Ctrl Pts',(132.399385536062,-32.6055092452614,18.761839030863));
#25102=CARTESIAN_POINT('Ctrl Pts',(132.388605223777,-32.5947553133353,18.7627337762472));
#25103=CARTESIAN_POINT('Ctrl Pts',(132.366029953173,-32.5725367422475,18.764607071456));
#25104=CARTESIAN_POINT('Ctrl Pts',(132.354223493009,-32.5610848052609,18.7655864510681));
#25105=CARTESIAN_POINT('Ctrl Pts',(132.32213319358,-32.5304082302105,18.7682463979172));
#25106=CARTESIAN_POINT('Ctrl Pts',(132.301694610797,-32.5113481788546,18.7699383749244));
#25107=CARTESIAN_POINT('Ctrl Pts',(132.176650579833,-32.3975961004797,18.7802643474275));
#25108=CARTESIAN_POINT('Ctrl Pts',(132.06646031676,-32.3092662225133,18.789251639162));
#25109=CARTESIAN_POINT('Ctrl Pts',(131.755785293099,-32.0905892657241,18.8136751399559));
#25110=CARTESIAN_POINT('Ctrl Pts',(131.546460729699,-31.9741220393048,18.8291495214459));
#25111=CARTESIAN_POINT('Ctrl Pts',(131.255407028713,-31.8503419047845,18.8487181809404));
#25112=CARTESIAN_POINT('Ctrl Pts',(131.183177960155,-31.8225034579676,18.853434021677));
#25113=CARTESIAN_POINT('Ctrl Pts',(131.07680873452,-31.7856375320606,18.8601782595072));
#25114=CARTESIAN_POINT('Ctrl Pts',(131.043384477365,-31.774633028868,18.8622694667274));
#25115=CARTESIAN_POINT('Ctrl Pts',(130.984242693153,-31.756176973093,18.8659218907131));
#25116=CARTESIAN_POINT('Ctrl Pts',(130.958597353015,-31.7485060841511,18.8674900448567));
#25117=CARTESIAN_POINT('Ctrl Pts',(130.905045337785,-31.7331765816433,18.8707332236701));
#25118=CARTESIAN_POINT('Ctrl Pts',(130.87712597474,-31.7255699106833,18.8724064802458));
#25119=CARTESIAN_POINT('Ctrl Pts',(130.803418281729,-31.7064985465092,18.8767799067361));
#25120=CARTESIAN_POINT('Ctrl Pts',(130.757481168686,-31.6956308704177,18.8794611586634));
#25121=CARTESIAN_POINT('Ctrl Pts',(130.500602450114,-31.640497941406,18.8942336851626));
#25122=CARTESIAN_POINT('Ctrl Pts',(130.286036047075,-31.6154686476948,18.9057081681737));
#25123=CARTESIAN_POINT('Ctrl Pts',(129.864530546271,-31.6066968560081,18.9280616241933));
#25124=CARTESIAN_POINT('Ctrl Pts',(129.658594487553,-31.6212011923239,18.9389118029072));
#25125=CARTESIAN_POINT('Ctrl Pts',(129.422296688807,-31.6596736027537,18.9524564735133));
#25126=CARTESIAN_POINT('Ctrl Pts',(129.389399459689,-31.6655302729447,18.9543677409905));
#25127=CARTESIAN_POINT('Ctrl Pts',(129.339121196669,-31.675250229995,18.9573354323215));
#25128=CARTESIAN_POINT('Ctrl Pts',(129.321674194063,-31.6787659076372,18.958373903616));
#25129=CARTESIAN_POINT('Ctrl Pts',(129.289596782035,-31.6854929963254,18.9603004959578));
#25130=CARTESIAN_POINT('Ctrl Pts',(129.274958829442,-31.6886642148989,18.9611864381891));
#25131=CARTESIAN_POINT('Ctrl Pts',(129.240679099206,-31.696328888878,18.9632768311574));
#25132=CARTESIAN_POINT('Ctrl Pts',(129.221055836689,-31.7009005793288,18.9644854538693));
#25133=CARTESIAN_POINT('Ctrl Pts',(129.155367778879,-31.7168228411771,18.9685688919492));
#25134=CARTESIAN_POINT('Ctrl Pts',(129.109502613729,-31.7289650303944,18.9714823328456));
#25135=CARTESIAN_POINT('Ctrl Pts',(128.99525996173,-31.7617899380875,18.978871068747));
#25136=CARTESIAN_POINT('Ctrl Pts',(128.927253994525,-31.7836788233089,18.9833891606425));
#25137=CARTESIAN_POINT('Ctrl Pts',(128.707117692007,-31.8622919144508,18.998309184041));
#25138=CARTESIAN_POINT('Ctrl Pts',(128.558360746719,-31.9277965724441,19.0088507860279));
#25139=CARTESIAN_POINT('Ctrl Pts',(128.263205566821,-32.0839428285042,19.0302111957088));
#25140=CARTESIAN_POINT('Ctrl Pts',(128.117837333673,-32.1755846957157,19.0409776975598));
#25141=CARTESIAN_POINT('Ctrl Pts',(127.943986652209,-32.3045914302407,19.054067765254));
#25142=CARTESIAN_POINT('Ctrl Pts',(127.908488116279,-32.33204262144,19.0567541039752));
#25143=CARTESIAN_POINT('Ctrl Pts',(127.851384171362,-32.3780418077401,19.0610995874499));
#25144=CARTESIAN_POINT('Ctrl Pts',(127.829449772376,-32.3961707958878,19.0627748092974));
#25145=CARTESIAN_POINT('Ctrl Pts',(127.787177295572,-32.432014802443,19.0660162626987));
#25146=CARTESIAN_POINT('Ctrl Pts',(127.76681729208,-32.4497005370415,19.0675834933851));
#25147=CARTESIAN_POINT('Ctrl Pts',(127.718951662944,-32.4922918481688,19.0712838446877));
#25148=CARTESIAN_POINT('Ctrl Pts',(127.691639343045,-32.5174100375277,19.0734080204768));
#25149=CARTESIAN_POINT('Ctrl Pts',(127.596497904265,-32.6078362071488,19.0808601780285));
#25150=CARTESIAN_POINT('Ctrl Pts',(127.530980377487,-32.6755185264377,19.0860879141772));
#25151=CARTESIAN_POINT('Ctrl Pts',(127.366309369364,-32.860460328479,19.0996118788348));
#25152=CARTESIAN_POINT('Ctrl Pts',(127.272154537069,-32.9818774315783,19.1077449333051));
#25153=CARTESIAN_POINT('Ctrl Pts',(127.078619855762,-33.2698600250653,19.1261397481423));
#25154=CARTESIAN_POINT('Ctrl Pts',(126.984651439986,-33.4393901057894,19.136367731128));
#25155=CARTESIAN_POINT('Ctrl Pts',(126.891515948642,-33.647619573974,19.1492555193022));
#25156=CARTESIAN_POINT('Ctrl Pts',(126.877853698947,-33.679466700531,19.1512355482606));
#25157=CARTESIAN_POINT('Ctrl Pts',(126.857818504125,-33.7282191195397,19.1542882232668));
#25158=CARTESIAN_POINT('Ctrl Pts',(126.851088120362,-33.7449760546561,19.1553413055566));
#25159=CARTESIAN_POINT('Ctrl Pts',(126.83903263467,-33.7756986652119,19.1572804176327));
#25160=CARTESIAN_POINT('Ctrl Pts',(126.833665552645,-33.7896469175918,19.1581640207011));
#25161=CARTESIAN_POINT('Ctrl Pts',(126.825988669521,-33.8099985449431,19.1594578654587));
#25162=CARTESIAN_POINT('Ctrl Pts',(126.823605668016,-33.8163740310795,19.1598638224713));
#25163=CARTESIAN_POINT('Ctrl Pts',(126.821241915874,-33.8227565650612,19.1602708352289));
#25164=CARTESIAN_POINT('Origin',(130.,-35.,23.));
#25165=CARTESIAN_POINT('',(126.821241916136,-33.8227565643555,20.4155868599104));
#25166=CARTESIAN_POINT('',(126.82124191022,-33.822756580328,20.0676573852273));
#25167=CARTESIAN_POINT('',(126.821241915871,-33.8227565650715,23.));
#25168=CARTESIAN_POINT('Ctrl Pts',(126.82124191022,-33.822756580328,20.0676573852273));
#25169=CARTESIAN_POINT('Ctrl Pts',(126.830737944534,-33.7971156675063,20.0659955135839));
#25170=CARTESIAN_POINT('Ctrl Pts',(126.840545002458,-33.7715875409957,20.0643431471796));
#25171=CARTESIAN_POINT('Ctrl Pts',(126.864662288883,-33.7110099642004,20.0604270690341));
#25172=CARTESIAN_POINT('Ctrl Pts',(126.879251901058,-33.6760780414383,20.0581728848126));
#25173=CARTESIAN_POINT('Ctrl Pts',(126.905283146217,-33.6165742766722,20.0543385598621));
#25174=CARTESIAN_POINT('Ctrl Pts',(126.916439715656,-33.5918824007403,20.0527490979748));
#25175=CARTESIAN_POINT('Ctrl Pts',(126.939819199682,-33.5417493389165,20.0495243248565));
#25176=CARTESIAN_POINT('Ctrl Pts',(126.952066224576,-33.5163217020307,20.0478899859034));
#25177=CARTESIAN_POINT('Ctrl Pts',(126.984094549459,-33.4518942595872,20.0437504203348));
#25178=CARTESIAN_POINT('Ctrl Pts',(127.004315838557,-33.413118239776,20.0412604214548));
#25179=CARTESIAN_POINT('Ctrl Pts',(127.097667401596,-33.2422563130808,20.0302795296636));
#25180=CARTESIAN_POINT('Ctrl Pts',(127.178825954979,-33.1147464245847,20.022070276748));
#25181=CARTESIAN_POINT('Ctrl Pts',(127.389761482984,-32.8276280513897,20.0030122806015));
#25182=CARTESIAN_POINT('Ctrl Pts',(127.526069272746,-32.6735855359763,19.9923253809962));
#25183=CARTESIAN_POINT('Ctrl Pts',(127.739579145407,-32.4724197106059,19.9763680460375));
#25184=CARTESIAN_POINT('Ctrl Pts',(127.806017957918,-32.4145397079635,19.971490269403));
#25185=CARTESIAN_POINT('Ctrl Pts',(127.894087136384,-32.3436566622624,19.965023333165));
#25186=CARTESIAN_POINT('Ctrl Pts',(127.913716667303,-32.3282120790643,19.9635818384173));
#25187=CARTESIAN_POINT('Ctrl Pts',(127.946046125913,-32.3033486556651,19.9612043081926));
#25188=CARTESIAN_POINT('Ctrl Pts',(127.958644812193,-32.2937989788841,19.9602769608721));
#25189=CARTESIAN_POINT('Ctrl Pts',(127.98251934731,-32.2759639021357,19.9585171207978));
#25190=CARTESIAN_POINT('Ctrl Pts',(127.993780636098,-32.2676594841001,19.9576859968555));
#25191=CARTESIAN_POINT('Ctrl Pts',(128.024187885427,-32.2455255723737,19.9554397952754));
#25192=CARTESIAN_POINT('Ctrl Pts',(128.043427149575,-32.231826324622,19.9540164323293));
#25193=CARTESIAN_POINT('Ctrl Pts',(128.118338628393,-32.1796569639005,19.9484709992904));
#25194=CARTESIAN_POINT('Ctrl Pts',(128.17501187875,-32.1426583185284,19.9442689008102));
#25195=CARTESIAN_POINT('Ctrl Pts',(128.395952137029,-32.0076744539395,19.9279694184905));
#25196=CARTESIAN_POINT('Ctrl Pts',(128.567295312653,-31.9219589279726,19.9155194535873));
#25197=CARTESIAN_POINT('Ctrl Pts',(128.904312611274,-31.7876323888814,19.8922542655064));
#25198=CARTESIAN_POINT('Ctrl Pts',(129.068284640661,-31.7362971708579,19.8814339471127));
#25199=CARTESIAN_POINT('Ctrl Pts',(129.28657457001,-31.6857606861343,19.8678024442814));
#25200=CARTESIAN_POINT('Ctrl Pts',(129.337961581155,-31.6751144883008,19.8646461456914));
#25201=CARTESIAN_POINT('Ctrl Pts',(129.419105452088,-31.6602593331375,19.8597423693043));
#25202=CARTESIAN_POINT('Ctrl Pts',(129.44870480714,-31.6552459141466,19.8579701826528));
#25203=CARTESIAN_POINT('Ctrl Pts',(129.504556779525,-31.6465475122618,19.8546563134145));
#25204=CARTESIAN_POINT('Ctrl Pts',(129.530793436295,-31.6427760230205,19.8531120542259));
#25205=CARTESIAN_POINT('Ctrl Pts',(129.590463085674,-31.6349117549119,19.849626977559));
#25206=CARTESIAN_POINT('Ctrl Pts',(129.623918525166,-31.6310087233696,19.8476921580684));
#25207=CARTESIAN_POINT('Ctrl Pts',(129.728894506189,-31.6203451188357,19.8416767545401));
#25208=CARTESIAN_POINT('Ctrl Pts',(129.800577317753,-31.6153586754793,19.8376502534484));
#25209=CARTESIAN_POINT('Ctrl Pts',(130.118771119807,-31.6033694477644,19.8200529042631));
#25210=CARTESIAN_POINT('Ctrl Pts',(130.365445416647,-31.6209973013003,19.8072052574937));
#25211=CARTESIAN_POINT('Ctrl Pts',(130.749659797129,-31.691051439037,19.7863666261384));
#25212=CARTESIAN_POINT('Ctrl Pts',(130.889485008773,-31.7258683162843,19.7785838720519));
#25213=CARTESIAN_POINT('Ctrl Pts',(131.053378387976,-31.7779532712119,19.7687876179265));
#25214=CARTESIAN_POINT('Ctrl Pts',(131.079991486189,-31.7867758508939,19.767174955232));
#25215=CARTESIAN_POINT('Ctrl Pts',(131.122056708702,-31.8013026110357,19.7645865013402));
#25216=CARTESIAN_POINT('Ctrl Pts',(131.137582527387,-31.8067912357063,19.7636225203716));
#25217=CARTESIAN_POINT('Ctrl Pts',(131.167377667414,-31.8175691641814,19.761754860786));
#25218=CARTESIAN_POINT('Ctrl Pts',(131.181652359512,-31.8228417868254,19.7608521132334));
#25219=CARTESIAN_POINT('Ctrl Pts',(131.217213496199,-31.836249746466,19.75858402694));
#25220=CARTESIAN_POINT('Ctrl Pts',(131.238454127222,-31.8445038940108,19.7572120807001));
#25221=CARTESIAN_POINT('Ctrl Pts',(131.316530189969,-31.8757541122032,19.7521095308907));
#25222=CARTESIAN_POINT('Ctrl Pts',(131.372819044646,-31.9000756410706,19.7483136772788));
#25223=CARTESIAN_POINT('Ctrl Pts',(131.628583592661,-32.0189197204648,19.7306183394088));
#25224=CARTESIAN_POINT('Ctrl Pts',(131.81918642865,-32.131257330255,19.7161940995058));
#25225=CARTESIAN_POINT('Ctrl Pts',(132.087586577362,-32.327021100415,19.6949713080096));
#25226=CARTESIAN_POINT('Ctrl Pts',(132.17436802999,-32.3971244801238,19.6879360963486));
#25227=CARTESIAN_POINT('Ctrl Pts',(132.314898987542,-32.5225901164289,19.6762947048432));
#25228=CARTESIAN_POINT('Ctrl Pts',(132.370499635818,-32.5757372370219,19.6716149100946));
#25229=CARTESIAN_POINT('Ctrl Pts',(132.448381408971,-32.6554263228917,19.6649479047418));
#25230=CARTESIAN_POINT('Ctrl Pts',(132.472136764199,-32.6804877231172,19.662898119216));
#25231=CARTESIAN_POINT('Ctrl Pts',(132.513504884782,-32.725487837064,19.659298127611));
#25232=CARTESIAN_POINT('Ctrl Pts',(132.531273345969,-32.7452787992734,19.6577414766571));
#25233=CARTESIAN_POINT('Ctrl Pts',(132.568276700126,-32.7874828822709,19.6544764942763));
#25234=CARTESIAN_POINT('Ctrl Pts',(132.58745537382,-32.8099424726989,19.6527705306142));
#25235=CARTESIAN_POINT('Ctrl Pts',(132.638367560109,-32.8711667396767,19.648201926184));
#25236=CARTESIAN_POINT('Ctrl Pts',(132.66953992508,-32.9103896575483,19.6453615107732));
#25237=CARTESIAN_POINT('Ctrl Pts',(132.857026551126,-33.1573429613659,19.6279691685409));
#25238=CARTESIAN_POINT('Ctrl Pts',(132.989880155607,-33.3817870484092,19.6143483000809));
#25239=CARTESIAN_POINT('Ctrl Pts',(133.141855624863,-33.7225250636265,19.5945156606457));
#25240=CARTESIAN_POINT('Ctrl Pts',(133.182727929545,-33.828061850002,19.5884643653526));
#25241=CARTESIAN_POINT('Ctrl Pts',(133.238412522682,-33.9964002044334,19.5786864551119));
#25242=CARTESIAN_POINT('Ctrl Pts',(133.256840896426,-34.0579200994591,19.5750872112681));
#25243=CARTESIAN_POINT('Ctrl Pts',(133.279358338388,-34.1416752618375,19.5701072568024));
#25244=CARTESIAN_POINT('Ctrl Pts',(133.284989508949,-34.1634856037982,19.568803220226));
#25245=CARTESIAN_POINT('Ctrl Pts',(133.294084892809,-34.2002222009744,19.5665921723164));
#25246=CARTESIAN_POINT('Ctrl Pts',(133.297666131027,-34.2151191869144,19.5656915539131));
#25247=CARTESIAN_POINT('Ctrl Pts',(133.304919839925,-34.2462189218737,19.5638021611607));
#25248=CARTESIAN_POINT('Ctrl Pts',(133.308574352005,-34.2624250588927,19.5628125136921));
#25249=CARTESIAN_POINT('Ctrl Pts',(133.318220657547,-34.3067169163491,19.56009516443));
#25250=CARTESIAN_POINT('Ctrl Pts',(133.323974765379,-34.3348523421205,19.5583552412008));
#25251=CARTESIAN_POINT('Ctrl Pts',(133.361079654356,-34.5288034717945,19.5462821732507));
#25252=CARTESIAN_POINT('Ctrl Pts',(133.380364637538,-34.6966727376086,19.5354488214455));
#25253=CARTESIAN_POINT('Ctrl Pts',(133.392591895672,-35.0040449210967,19.5156259006755));
#25254=CARTESIAN_POINT('Ctrl Pts',(133.389577918343,-35.143041951486,19.5066654864244));
#25255=CARTESIAN_POINT('Ctrl Pts',(133.366895798481,-35.4152632785626,19.4893684828256));
#25256=CARTESIAN_POINT('Ctrl Pts',(133.347807510332,-35.548290773347,19.4810359299813));
#25257=CARTESIAN_POINT('Ctrl Pts',(133.312559728758,-35.7204665599387,19.470442131707));
#25258=CARTESIAN_POINT('Ctrl Pts',(133.303499682309,-35.760929759087,19.4679658971067));
#25259=CARTESIAN_POINT('Ctrl Pts',(133.287135994972,-35.8281986772698,19.463870106073));
#25260=CARTESIAN_POINT('Ctrl Pts',(133.280241308915,-35.8550983114437,19.4622378884108));
#25261=CARTESIAN_POINT('Ctrl Pts',(133.265966828475,-35.9080748856431,19.4590335254165));
#25262=CARTESIAN_POINT('Ctrl Pts',(133.258603326212,-35.9341540276346,19.4574609998783));
#25263=CARTESIAN_POINT('Ctrl Pts',(133.239770931259,-35.997918256818,19.4536267231888));
#25264=CARTESIAN_POINT('Ctrl Pts',(133.227956235934,-36.0354975883954,19.4513761799896));
#25265=CARTESIAN_POINT('Ctrl Pts',(133.182620222873,-36.1713745490391,19.4432636047178));
#25266=CARTESIAN_POINT('Ctrl Pts',(133.145240293091,-36.2683280275595,19.4375247484902));
#25267=CARTESIAN_POINT('Ctrl Pts',(133.001654836658,-36.5951626352275,19.4181291648662));
#25268=CARTESIAN_POINT('Ctrl Pts',(132.874215616292,-36.8147592541918,19.4050653273042));
#25269=CARTESIAN_POINT('Ctrl Pts',(132.684973685579,-37.0701485437394,19.3878357314506));
#25270=CARTESIAN_POINT('Ctrl Pts',(132.64493808778,-37.1210611418539,19.384282300992));
#25271=CARTESIAN_POINT('Ctrl Pts',(132.575118169129,-37.2047974169777,19.3781773764767));
#25272=CARTESIAN_POINT('Ctrl Pts',(132.546103134713,-37.2382412021783,19.3756649896913));
#25273=CARTESIAN_POINT('Ctrl Pts',(132.503296749702,-37.2856717708358,19.3719771938113));
#25274=CARTESIAN_POINT('Ctrl Pts',(132.490024696034,-37.3001232649984,19.3708362956679));
#25275=CARTESIAN_POINT('Ctrl Pts',(132.466524232604,-37.325270363624,19.3688187753727));
#25276=CARTESIAN_POINT('Ctrl Pts',(132.456350086203,-37.3360154741698,19.3679460973316));
#25277=CARTESIAN_POINT('Ctrl Pts',(132.433566989721,-37.3597637180413,19.3659932756243));
#25278=CARTESIAN_POINT('Ctrl Pts',(132.420924136429,-37.3727324736671,19.3649106909307));
#25279=CARTESIAN_POINT('Ctrl Pts',(132.382829563148,-37.4111876060401,19.3616536556656));
#25280=CARTESIAN_POINT('Ctrl Pts',(132.357075676757,-37.4363695182129,19.3594582224381));
#25281=CARTESIAN_POINT('Ctrl Pts',(132.221050747283,-37.5651979253716,19.3479188110186));
#25282=CARTESIAN_POINT('Ctrl Pts',(132.104337796046,-37.6617779950932,19.338213299181));
#25283=CARTESIAN_POINT('Ctrl Pts',(131.873603281396,-37.8280250444343,19.3198917442089));
#25284=CARTESIAN_POINT('Ctrl Pts',(131.761140078117,-37.8993970237987,19.311300125933));
#25285=CARTESIAN_POINT('Ctrl Pts',(131.519302174393,-38.0335977579744,19.2937374923244));
#25286=CARTESIAN_POINT('Ctrl Pts',(131.389530159568,-38.0951912403951,19.2848084469085));
#25287=CARTESIAN_POINT('Ctrl Pts',(131.217036963647,-38.1640175037994,19.2736058749596));
#25288=CARTESIAN_POINT('Ctrl Pts',(131.177553856138,-38.1789232284152,19.2710841962039));
#25289=CARTESIAN_POINT('Ctrl Pts',(131.11150664511,-38.2024579999321,19.2669344698561));
#25290=CARTESIAN_POINT('Ctrl Pts',(131.085096661619,-38.2115026962444,19.2652930449604));
#25291=CARTESIAN_POINT('Ctrl Pts',(131.032940975786,-38.2286477430164,19.2620855692815));
#25292=CARTESIAN_POINT('Ctrl Pts',(131.00720434663,-38.2367688786307,19.2605189453443));
#25293=CARTESIAN_POINT('Ctrl Pts',(130.950131819949,-38.2540313280403,19.2570790482898));
#25294=CARTESIAN_POINT('Ctrl Pts',(130.918755139911,-38.2630291841523,19.255210457974));
#25295=CARTESIAN_POINT('Ctrl Pts',(130.808842249527,-38.2928376302635,19.2487384844376));
#25296=CARTESIAN_POINT('Ctrl Pts',(130.729689180986,-38.3112777789999,19.2442088981335));
#25297=CARTESIAN_POINT('Ctrl Pts',(130.375391617486,-38.3804944914267,19.2243845332523));
#25298=CARTESIAN_POINT('Ctrl Pts',(130.095274566259,-38.3999375058523,19.2100008401026));
#25299=CARTESIAN_POINT('Ctrl Pts',(129.749160724202,-38.3811181684098,19.1912382798433));
#25300=CARTESIAN_POINT('Ctrl Pts',(129.68248675719,-38.3755095696038,19.1875726372736));
#25301=CARTESIAN_POINT('Ctrl Pts',(129.57101034035,-38.3628002734263,19.1812957669168));
#25302=CARTESIAN_POINT('Ctrl Pts',(129.526104361182,-38.3567663490817,19.1787265817193));
#25303=CARTESIAN_POINT('Ctrl Pts',(129.461771722245,-38.346805534286,19.1749703479391));
#25304=CARTESIAN_POINT('Ctrl Pts',(129.442235769276,-38.3436052376457,19.1738196095493));
#25305=CARTESIAN_POINT('Ctrl Pts',(129.408000973724,-38.3376886648702,19.1717835957511));
#25306=CARTESIAN_POINT('Ctrl Pts',(129.393290319951,-38.3350460001238,19.1709023209343));
#25307=CARTESIAN_POINT('Ctrl Pts',(129.360859320256,-38.3289983217153,19.1689449474997));
#25308=CARTESIAN_POINT('Ctrl Pts',(129.343148608262,-38.3255491052591,19.1678665778649));
#25309=CARTESIAN_POINT('Ctrl Pts',(129.291571789138,-38.3150762837749,19.1647002700099));
#25310=CARTESIAN_POINT('Ctrl Pts',(129.257785559828,-38.3076757433622,19.1625934596495));
#25311=CARTESIAN_POINT('Ctrl Pts',(129.040876746305,-38.2566734787021,19.1488818486681));
#25312=CARTESIAN_POINT('Ctrl Pts',(128.861554201773,-38.198401280825,19.1367078875408));
#25313=CARTESIAN_POINT('Ctrl Pts',(128.543155738256,-38.0647495209478,19.1144548503293));
#25314=CARTESIAN_POINT('Ctrl Pts',(128.402693473605,-37.9939445685754,19.1043858766844));
#25315=CARTESIAN_POINT('Ctrl Pts',(128.185598444882,-37.8648669016545,19.0886317187811));
#25316=CARTESIAN_POINT('Ctrl Pts',(128.105648162496,-37.8126409525438,19.0827810643623));
#25317=CARTESIAN_POINT('Ctrl Pts',(127.99768399278,-37.7354204714346,19.0748136808338));
#25318=CARTESIAN_POINT('Ctrl Pts',(127.967724036539,-37.7132359136485,19.0725949619642));
#25319=CARTESIAN_POINT('Ctrl Pts',(127.916708654769,-37.6741411594073,19.0688019835447));
#25320=CARTESIAN_POINT('Ctrl Pts',(127.895478596384,-37.6574656148347,19.0672189120923));
#25321=CARTESIAN_POINT('Ctrl Pts',(127.852329832161,-37.6227322081549,19.0639908557788));
#25322=CARTESIAN_POINT('Ctrl Pts',(127.830434271734,-37.6046489221274,19.0623470507372));
#25323=CARTESIAN_POINT('Ctrl Pts',(127.774749822837,-37.5574703614813,19.0581497415298));
#25324=CARTESIAN_POINT('Ctrl Pts',(127.741302544589,-37.5279792455196,19.0556123537418));
#25325=CARTESIAN_POINT('Ctrl Pts',(127.579355106281,-37.3794060904274,19.0432269759379));
#25326=CARTESIAN_POINT('Ctrl Pts',(127.459633297536,-37.2511421956431,19.0337712314917));
#25327=CARTESIAN_POINT('Ctrl Pts',(127.251118128711,-36.9898163153125,19.0159729204797));
#25328=CARTESIAN_POINT('Ctrl Pts',(127.160765286253,-36.8586187859908,19.0076254218208));
#25329=CARTESIAN_POINT('Ctrl Pts',(127.043624510451,-36.6599302610241,18.9951758156346));
#25330=CARTESIAN_POINT('Ctrl Pts',(127.009248391523,-36.597162568518,18.991266872403));
#25331=CARTESIAN_POINT('Ctrl Pts',(126.955399758409,-36.4909964981786,18.9846197088263));
#25332=CARTESIAN_POINT('Ctrl Pts',(126.934807506673,-36.4481904925946,18.9819302521196));
#25333=CARTESIAN_POINT('Ctrl Pts',(126.906767803111,-36.3866239408624,18.9780295146676));
#25334=CARTESIAN_POINT('Ctrl Pts',(126.898577132215,-36.3682059528073,18.9768585037977));
#25335=CARTESIAN_POINT('Ctrl Pts',(126.884587547551,-36.335977041105,18.9748004777273));
#25336=CARTESIAN_POINT('Ctrl Pts',(126.878715131583,-36.3221989878863,18.9739177819017));
#25337=CARTESIAN_POINT('Ctrl Pts',(126.86606734434,-36.2919704569789,18.971974445059));
#25338=CARTESIAN_POINT('Ctrl Pts',(126.859330139233,-36.275505525923,18.9709117730339));
#25339=CARTESIAN_POINT('Ctrl Pts',(126.84032528591,-36.2279963339575,18.9678350794381));
#25340=CARTESIAN_POINT('Ctrl Pts',(126.828386516974,-36.1968237252505,18.9658036888101));
#25341=CARTESIAN_POINT('Ctrl Pts',(126.745804919668,-35.971282022719,18.9510410006886));
#25342=CARTESIAN_POINT('Ctrl Pts',(126.692625240065,-35.7709965558779,18.9376147101442));
#25343=CARTESIAN_POINT('Ctrl Pts',(126.626335021558,-35.3803631093282,18.9121058551246));
#25344=CARTESIAN_POINT('Ctrl Pts',(126.610349291643,-35.1912478961659,18.9000493839968));
#25345=CARTESIAN_POINT('Ctrl Pts',(126.6102214509,-34.9461491383693,18.8850413354147));
#25346=CARTESIAN_POINT('Ctrl Pts',(126.611561328262,-34.8905356796344,18.8816747745842));
#25347=CARTESIAN_POINT('Ctrl Pts',(126.615917247258,-34.8011660559186,18.8763257076945));
#25348=CARTESIAN_POINT('Ctrl Pts',(126.618071693678,-34.7673799872712,18.8743174906237));
#25349=CARTESIAN_POINT('Ctrl Pts',(126.62281608338,-34.7071907034308,18.8707636366067));
#25350=CARTESIAN_POINT('Ctrl Pts',(126.62521050149,-34.6807753285021,18.8692121256732));
#25351=CARTESIAN_POINT('Ctrl Pts',(126.63096475465,-34.6246315717396,18.8659308985182));
#25352=CARTESIAN_POINT('Ctrl Pts',(126.634408622081,-34.5949139585812,18.8642039126751));
#25353=CARTESIAN_POINT('Ctrl Pts',(126.644909082024,-34.5137188526947,18.8595098343058));
#25354=CARTESIAN_POINT('Ctrl Pts',(126.652756627622,-34.4623508299043,18.8565672043406));
#25355=CARTESIAN_POINT('Ctrl Pts',(126.690906854619,-34.2460638648988,18.8442656239512));
#25356=CARTESIAN_POINT('Ctrl Pts',(126.732242904627,-34.0833276277052,18.8352430382239));
#25357=CARTESIAN_POINT('Ctrl Pts',(126.796849932018,-33.8902596431973,18.8244142701401));
#25358=CARTESIAN_POINT('Ctrl Pts',(126.808780054898,-33.856405717364,18.8225099732079));
#25359=CARTESIAN_POINT('Ctrl Pts',(126.821241893434,-33.8227566256554,18.8206072661261));
#25360=CARTESIAN_POINT('',(126.610251372999,-34.9977875375927,19.2361966383981));
#25361=CARTESIAN_POINT('Ctrl Pts',(126.821241915874,-33.8227565650612,19.1602708352289));
#25362=CARTESIAN_POINT('Ctrl Pts',(126.816736953399,-33.8349207321845,19.1610465414327));
#25363=CARTESIAN_POINT('Ctrl Pts',(126.812301909871,-33.8471104990182,19.1618260822225));
#25364=CARTESIAN_POINT('Ctrl Pts',(126.792726924733,-33.901889116889,19.1653381032647));
#25365=CARTESIAN_POINT('Ctrl Pts',(126.778370469,-33.9447508173432,19.1681101177204));
#25366=CARTESIAN_POINT('Ctrl Pts',(126.744968324843,-34.0515173590052,19.1750527022559));
#25367=CARTESIAN_POINT('Ctrl Pts',(126.726943361646,-34.1157207046637,19.1792602750059));
#25368=CARTESIAN_POINT('Ctrl Pts',(126.644210410436,-34.4477444133355,19.2010559226414));
#25369=CARTESIAN_POINT('Ctrl Pts',(126.610430890917,-34.7222374851469,19.2190847940162));
#25370=CARTESIAN_POINT('Ctrl Pts',(126.610250724596,-34.9977836064225,19.2361975235207));
#25371=CARTESIAN_POINT('Ctrl Pts',(126.610250722074,-34.9977874673202,19.2361977633008));
#25372=CARTESIAN_POINT('Ctrl Pts',(126.610215475891,-35.0517869964763,19.2395513902642));
#25373=CARTESIAN_POINT('Ctrl Pts',(126.611470566682,-35.1057822568918,19.2428715249805));
#25374=CARTESIAN_POINT('Ctrl Pts',(126.615959723836,-35.2009458075462,19.2486631010251));
#25375=CARTESIAN_POINT('Ctrl Pts',(126.618656669346,-35.2421266443502,19.2511495142746));
#25376=CARTESIAN_POINT('Ctrl Pts',(126.624315591746,-35.3096122172126,19.2551925444575));
#25377=CARTESIAN_POINT('Ctrl Pts',(126.626834810277,-35.3359488228297,19.2567624477098));
#25378=CARTESIAN_POINT('Ctrl Pts',(126.63235118281,-35.3872720625358,19.259806964583));
#25379=CARTESIAN_POINT('Ctrl Pts',(126.635318754657,-35.4122600810101,19.2612823870852));
#25380=CARTESIAN_POINT('Ctrl Pts',(126.642207569199,-35.4652234956728,19.2643958356638));
#25381=CARTESIAN_POINT('Ctrl Pts',(126.646200829735,-35.4931876975554,19.2660315094045));
#25382=CARTESIAN_POINT('Ctrl Pts',(126.657283866026,-35.5644258418229,19.2701792150951));
#25383=CARTESIAN_POINT('Ctrl Pts',(126.664864716015,-35.607618769188,19.2726758952135));
#25384=CARTESIAN_POINT('Ctrl Pts',(126.703952801223,-35.8074716358138,19.2841596591186));
#25385=CARTESIAN_POINT('Ctrl Pts',(126.745674981425,-35.9619323369152,19.2928266039349));
#25386=CARTESIAN_POINT('Ctrl Pts',(126.868023081428,-36.3139368607722,19.3127242568782));
#25387=CARTESIAN_POINT('Ctrl Pts',(126.95667909956,-36.5079444781437,19.3237971593411));
#25388=CARTESIAN_POINT('Ctrl Pts',(127.099974271123,-36.7566333809814,19.3395269336545));
#25389=CARTESIAN_POINT('Ctrl Pts',(127.139114944674,-36.8196827234399,19.3436637006914));
#25390=CARTESIAN_POINT('Ctrl Pts',(127.193423675289,-36.9010771644574,19.3492720263093));
#25391=CARTESIAN_POINT('Ctrl Pts',(127.20676318801,-36.9206231010795,19.3506399324129));
#25392=CARTESIAN_POINT('Ctrl Pts',(127.22919845104,-36.9527686144097,19.352927674653));
#25393=CARTESIAN_POINT('Ctrl Pts',(127.238178441058,-36.9654485876958,19.3538400724683));
#25394=CARTESIAN_POINT('Ctrl Pts',(127.255549040383,-36.989622196841,19.3555996164857));
#25395=CARTESIAN_POINT('Ctrl Pts',(127.263925392552,-37.0011255038456,19.3564457149268));
#25396=CARTESIAN_POINT('Ctrl Pts',(127.287153991146,-37.0326070235525,19.3587847830008));
#25397=CARTESIAN_POINT('Ctrl Pts',(127.302153977148,-37.0524744913238,19.3602872315245));
#25398=CARTESIAN_POINT('Ctrl Pts',(127.366005101649,-37.1351359174747,19.3666433956339));
#25399=CARTESIAN_POINT('Ctrl Pts',(127.416837337539,-37.1963613758636,19.3716086362371));
#25400=CARTESIAN_POINT('Ctrl Pts',(127.604929047678,-37.4073411404047,19.3894983438435));
#25401=CARTESIAN_POINT('Ctrl Pts',(127.753436768156,-37.5464900332526,19.4027441967379));
#25402=CARTESIAN_POINT('Ctrl Pts',(127.998979629321,-37.7382629343204,19.4226268813693));
#25403=CARTESIAN_POINT('Ctrl Pts',(128.087609881186,-37.8008808645023,19.4294621294333));
#25404=CARTESIAN_POINT('Ctrl Pts',(128.242748668098,-37.8996840911201,19.4408189327648));
#25405=CARTESIAN_POINT('Ctrl Pts',(128.307740578387,-37.938087721698,19.4454093261073));
#25406=CARTESIAN_POINT('Ctrl Pts',(128.404055015417,-37.9907425050132,19.4519751671637));
#25407=CARTESIAN_POINT('Ctrl Pts',(128.434394333691,-38.0067357969035,19.4540105471248));
#25408=CARTESIAN_POINT('Ctrl Pts',(128.4886603915,-38.0342978672481,19.4575944719336));
#25409=CARTESIAN_POINT('Ctrl Pts',(128.512489906022,-38.046050679056,19.4591492635014));
#25410=CARTESIAN_POINT('Ctrl Pts',(128.563207636043,-38.0703277368329,19.4624194715049));
#25411=CARTESIAN_POINT('Ctrl Pts',(128.590127115723,-38.0827817372623,19.4641323985691));
#25412=CARTESIAN_POINT('Ctrl Pts',(128.663505249134,-38.1155670848793,19.4687425015449));
#25413=CARTESIAN_POINT('Ctrl Pts',(128.710263188707,-38.1352122435713,19.4716167221714));
#25414=CARTESIAN_POINT('Ctrl Pts',(128.994746451094,-38.24729468547,19.488759843582));
#25415=CARTESIAN_POINT('Ctrl Pts',(129.2418378593,-38.3137076845742,19.5021404355514));
#25416=CARTESIAN_POINT('Ctrl Pts',(129.608486885277,-38.3690525909381,19.5218420282797));
#25417=CARTESIAN_POINT('Ctrl Pts',(129.723721208312,-38.3804533564389,19.5280267362175));
#25418=CARTESIAN_POINT('Ctrl Pts',(129.904345972995,-38.3890256963134,19.5379927647802));
#25419=CARTESIAN_POINT('Ctrl Pts',(129.96945784759,-38.3902375944467,19.5416407478837));
#25420=CARTESIAN_POINT('Ctrl Pts',(130.057194919791,-38.3893430343751,19.546677926323));
#25421=CARTESIAN_POINT('Ctrl Pts',(130.079826484096,-38.3888855301423,19.5479881717945));
#25422=CARTESIAN_POINT('Ctrl Pts',(130.117785664961,-38.3877377353283,19.5502066176384));
#25423=CARTESIAN_POINT('Ctrl Pts',(130.133116700031,-38.3871699638146,19.5511083250721));
#25424=CARTESIAN_POINT('Ctrl Pts',(130.165000628942,-38.3857723676685,19.5529963594252));
#25425=CARTESIAN_POINT('Ctrl Pts',(130.181551997265,-38.384925195643,19.5539835157157));
#25426=CARTESIAN_POINT('Ctrl Pts',(130.226577344332,-38.3822894214789,19.5566869006675));
#25427=CARTESIAN_POINT('Ctrl Pts',(130.255035401087,-38.3802626896993,19.5584151511606));
#25428=CARTESIAN_POINT('Ctrl Pts',(130.447526910326,-38.3641092582399,19.5702227641813));
#25429=CARTESIAN_POINT('Ctrl Pts',(130.610355108811,-38.3384080562368,19.580779689856));
#25430=CARTESIAN_POINT('Ctrl Pts',(130.901331910001,-38.2704759623411,19.6000305194481));
#25431=CARTESIAN_POINT('Ctrl Pts',(131.03008708596,-38.2322338275067,19.6086933463872));
#25432=CARTESIAN_POINT('Ctrl Pts',(131.24561578217,-38.1540269935091,19.6232464342937));
#25433=CARTESIAN_POINT('Ctrl Pts',(131.33359304085,-38.1178481068058,19.6292040888516));
#25434=CARTESIAN_POINT('Ctrl Pts',(131.482487280298,-38.0491607839702,19.6392901065023));
#25435=CARTESIAN_POINT('Ctrl Pts',(131.544145142191,-38.0184046826063,19.6434682179105));
#25436=CARTESIAN_POINT('Ctrl Pts',(131.634037660264,-37.9700885165434,19.6495637788521));
#25437=CARTESIAN_POINT('Ctrl Pts',(131.663017663586,-37.953959586572,19.6515296541311));
#25438=CARTESIAN_POINT('Ctrl Pts',(131.714477138844,-37.9243222509504,19.6550229906314));
#25439=CARTESIAN_POINT('Ctrl Pts',(131.737045050106,-37.9109735550463,19.6565559228395));
#25440=CARTESIAN_POINT('Ctrl Pts',(131.785329582839,-37.8816522399491,19.6598386467291));
#25441=CARTESIAN_POINT('Ctrl Pts',(131.810991827585,-37.8655941857449,19.6615852008343));
#25442=CARTESIAN_POINT('Ctrl Pts',(131.880374477991,-37.820873889295,19.6663149917191));
#25443=CARTESIAN_POINT('Ctrl Pts',(131.923653335046,-37.7915400644277,19.6692736329023));
#25444=CARTESIAN_POINT('Ctrl Pts',(132.19678451895,-37.5970456909897,19.6880408864379));
#25445=CARTESIAN_POINT('Ctrl Pts',(132.405854894409,-37.4046571971606,19.7027322568091));
#25446=CARTESIAN_POINT('Ctrl Pts',(132.678034171645,-37.0827219615734,19.7252541804833));
#25447=CARTESIAN_POINT('Ctrl Pts',(132.760899595045,-36.9715535676053,19.732759928562));
#25448=CARTESIAN_POINT('Ctrl Pts',(132.851975043394,-36.8323262813569,19.7422393238943));
#25449=CARTESIAN_POINT('Ctrl Pts',(132.866937901877,-36.8088250910627,19.7438420925372));
#25450=CARTESIAN_POINT('Ctrl Pts',(132.890261159672,-36.7711762818887,19.7464183398467));
#25451=CARTESIAN_POINT('Ctrl Pts',(132.898811596143,-36.7571472044543,19.7473801985655));
#25452=CARTESIAN_POINT('Ctrl Pts',(132.915095311493,-36.7299874554653,19.7492470089152));
#25453=CARTESIAN_POINT('Ctrl Pts',(132.922842582926,-36.7168658870126,19.7501510729468));
#25454=CARTESIAN_POINT('Ctrl Pts',(132.942010626481,-36.6838951754522,19.7524273234342));
#25455=CARTESIAN_POINT('Ctrl Pts',(132.953319110528,-36.663981867943,19.7538062173939));
#25456=CARTESIAN_POINT('Ctrl Pts',(132.994555940667,-36.5896225385892,19.7589660681125));
#25457=CARTESIAN_POINT('Ctrl Pts',(133.023185928337,-36.5344741632048,19.7628140964044));
#25458=CARTESIAN_POINT('Ctrl Pts',(133.146196207625,-36.2807052601986,19.7805163880707));
#25459=CARTESIAN_POINT('Ctrl Pts',(133.222627618009,-36.0739774251647,19.7948847781485));
#25460=CARTESIAN_POINT('Ctrl Pts',(133.306791367939,-35.7536137909025,19.8160443970512));
#25461=CARTESIAN_POINT('Ctrl Pts',(133.329761767628,-35.6445873435912,19.8230704295038));
#25462=CARTESIAN_POINT('Ctrl Pts',(133.359441774787,-35.4587570945061,19.8346988025996));
#25463=CARTESIAN_POINT('Ctrl Pts',(133.368976469921,-35.3824997584737,19.8393745347971));
#25464=CARTESIAN_POINT('Ctrl Pts',(133.379027746316,-35.2716026918333,19.846036959189));
#25465=CARTESIAN_POINT('Ctrl Pts',(133.381618337571,-35.2371794337575,19.8480861046058));
#25466=CARTESIAN_POINT('Ctrl Pts',(133.385273222976,-35.1761747302857,19.8516853912278));
#25467=CARTESIAN_POINT('Ctrl Pts',(133.386551252857,-35.1496094964039,19.8532419683326));
#25468=CARTESIAN_POINT('Ctrl Pts',(133.38858862795,-35.0935129065476,19.8565072071534));
#25469=CARTESIAN_POINT('Ctrl Pts',(133.389274857872,-35.0639810186423,19.8582134956124));
#25470=CARTESIAN_POINT('Ctrl Pts',(133.390084291149,-34.9843243198225,19.862783990647));
#25471=CARTESIAN_POINT('Ctrl Pts',(133.389481931877,-34.934198598235,19.8656259392149));
#25472=CARTESIAN_POINT('Ctrl Pts',(133.378887229694,-34.6245070176078,19.8830073997862));
#25473=CARTESIAN_POINT('Ctrl Pts',(133.340200084402,-34.3667953565156,19.8966177603642));
#25474=CARTESIAN_POINT('Ctrl Pts',(133.242930759682,-34.0067102163326,19.9164445520153));
#25475=CARTESIAN_POINT('Ctrl Pts',(133.207947955851,-33.8989588864861,19.9225016021018));
#25476=CARTESIAN_POINT('Ctrl Pts',(133.144767409337,-33.7331254185884,19.9322876449867));
#25477=CARTESIAN_POINT('Ctrl Pts',(133.120191439165,-33.6737505543854,19.9358890130272));
#25478=CARTESIAN_POINT('Ctrl Pts',(133.0847400329,-33.5945493176286,19.940871467982));
#25479=CARTESIAN_POINT('Ctrl Pts',(133.075330590271,-33.5740777044597,19.9421757830238));
#25480=CARTESIAN_POINT('Ctrl Pts',(133.059180465775,-33.5398442833371,19.944387167526));
#25481=CARTESIAN_POINT('Ctrl Pts',(133.052549081894,-33.526031229869,19.9452878396822));
#25482=CARTESIAN_POINT('Ctrl Pts',(133.038533552067,-33.4973374092028,19.9471771878438));
#25483=CARTESIAN_POINT('Ctrl Pts',(133.031133375043,-33.4824653394593,19.9481667350843));
#25484=CARTESIAN_POINT('Ctrl Pts',(133.010645971728,-33.4420397476596,19.9508835030708));
#25485=CARTESIAN_POINT('Ctrl Pts',(132.997343219713,-33.4165977075638,19.9526229367354));
#25486=CARTESIAN_POINT('Ctrl Pts',(132.903711935006,-33.2429329749408,19.9646854283372));
#25487=CARTESIAN_POINT('Ctrl Pts',(132.812752087564,-33.1007256279803,19.975507785595));
#25488=CARTESIAN_POINT('Ctrl Pts',(132.628351199254,-32.8549073312108,19.9953099050514));
#25489=CARTESIAN_POINT('Ctrl Pts',(132.538360600551,-32.7491376420928,20.0042604378855));
#25490=CARTESIAN_POINT('Ctrl Pts',(132.348833986512,-32.552249048837,20.0215666835943));
#25491=CARTESIAN_POINT('Ctrl Pts',(132.249834291612,-32.4609532288098,20.0299172091076));
#25492=CARTESIAN_POINT('Ctrl Pts',(132.113543338317,-32.3495169244659,20.0405294674718));
#25493=CARTESIAN_POINT('Ctrl Pts',(132.080947640085,-32.32384919615,20.0430071540465));
#25494=CARTESIAN_POINT('Ctrl Pts',(132.025756807603,-32.2820070427779,20.047104668851));
#25495=CARTESIAN_POINT('Ctrl Pts',(132.003419919627,-32.2655009502264,20.0487371809818));
#25496=CARTESIAN_POINT('Ctrl Pts',(131.958896197835,-32.233438088688,20.0519416361506));
#25497=CARTESIAN_POINT('Ctrl Pts',(131.936720725371,-32.2178691588593,20.0535139656573));
#25498=CARTESIAN_POINT('Ctrl Pts',(131.881871312146,-32.1803341880507,20.0573468988262));
#25499=CARTESIAN_POINT('Ctrl Pts',(131.848996377523,-32.1586680052232,20.059596313516));
#25500=CARTESIAN_POINT('Ctrl Pts',(131.728203232173,-32.0820439890653,20.0676980424927));
#25501=CARTESIAN_POINT('Ctrl Pts',(131.638149869025,-32.0305520112295,20.0734276424108));
#25502=CARTESIAN_POINT('Ctrl Pts',(131.320431579276,-31.8677429578912,20.0928257013155));
#25503=CARTESIAN_POINT('Ctrl Pts',(131.082767847086,-31.7778611938597,20.1058991359685));
#25504=CARTESIAN_POINT('Ctrl Pts',(130.774551535498,-31.6992923746749,20.1231399609527));
#25505=CARTESIAN_POINT('Ctrl Pts',(130.711340740496,-31.685095110012,20.12669429097));
#25506=CARTESIAN_POINT('Ctrl Pts',(130.604299290924,-31.6642559542592,20.132800595864));
#25507=CARTESIAN_POINT('Ctrl Pts',(130.560673648247,-31.6566467957303,20.1353134399064));
#25508=CARTESIAN_POINT('Ctrl Pts',(130.497520420058,-31.6469023953297,20.1390017846809));
#25509=CARTESIAN_POINT('Ctrl Pts',(130.478102053031,-31.6440785912536,20.1401427597984));
#25510=CARTESIAN_POINT('Ctrl Pts',(130.443998655354,-31.6394212933619,20.1421603478744));
#25511=CARTESIAN_POINT('Ctrl Pts',(130.429324437796,-31.637515120602,20.1430330152535));
#25512=CARTESIAN_POINT('Ctrl Pts',(130.396663856719,-31.633489816429,20.1449857148189));
#25513=CARTESIAN_POINT('Ctrl Pts',(130.37867291998,-31.6314187231879,20.1460681865974));
#25514=CARTESIAN_POINT('Ctrl Pts',(130.324860217061,-31.6256604072789,20.1493246429877));
#25515=CARTESIAN_POINT('Ctrl Pts',(130.288996457512,-31.622399864992,20.1515196012223));
#25516=CARTESIAN_POINT('Ctrl Pts',(130.102285991814,-31.608420468476,20.163051833763));
#25517=CARTESIAN_POINT('Ctrl Pts',(129.95090766196,-31.6072346191829,20.1727501719458));
#25518=CARTESIAN_POINT('Ctrl Pts',(129.618366999672,-31.6268922275347,20.1942113124854));
#25519=CARTESIAN_POINT('Ctrl Pts',(129.437908711403,-31.6522301535943,20.2059498770714));
#25520=CARTESIAN_POINT('Ctrl Pts',(129.191875936219,-31.7072407972895,20.2217316454497));
#25521=CARTESIAN_POINT('Ctrl Pts',(129.123893920941,-31.7246730224662,20.2260710565437));
#25522=CARTESIAN_POINT('Ctrl Pts',(129.00347524158,-31.759569315421,20.233713825701));
#25523=CARTESIAN_POINT('Ctrl Pts',(128.95083325386,-31.7762285612515,20.2370397591887));
#25524=CARTESIAN_POINT('Ctrl Pts',(128.869706038507,-31.8041002413739,20.242143843824));
#25525=CARTESIAN_POINT('Ctrl Pts',(128.840927851766,-31.8144244549056,20.2439501682841));
#25526=CARTESIAN_POINT('Ctrl Pts',(128.787528839335,-31.8344008765015,20.2472949916082));
#25527=CARTESIAN_POINT('Ctrl Pts',(128.762873868321,-31.8439545125429,20.2488365679187));
#25528=CARTESIAN_POINT('Ctrl Pts',(128.70782595241,-31.8660294172508,20.2522734077765));
#25529=CARTESIAN_POINT('Ctrl Pts',(128.677498050859,-31.8787063441986,20.2541633595127));
#25530=CARTESIAN_POINT('Ctrl Pts',(128.585707950495,-31.9186522942257,20.2598765308522));
#25531=CARTESIAN_POINT('Ctrl Pts',(128.524866718545,-31.9473112970534,20.2636534655531));
#25532=CARTESIAN_POINT('Ctrl Pts',(128.196759698843,-32.1139666567642,20.284048415187));
#25533=CARTESIAN_POINT('Ctrl Pts',(127.947944877892,-32.2852396274746,20.2994742431764));
#25534=CARTESIAN_POINT('Ctrl Pts',(127.674358370537,-32.5329245619873,20.3194330101063));
#25535=CARTESIAN_POINT('Ctrl Pts',(127.625123851497,-32.5802825491507,20.3231721618661));
#25536=CARTESIAN_POINT('Ctrl Pts',(127.545198565302,-32.6619519237733,20.3295612709896));
#25537=CARTESIAN_POINT('Ctrl Pts',(127.513714554314,-32.6954603175193,20.3321672065368));
#25538=CARTESIAN_POINT('Ctrl Pts',(127.469589160205,-32.7443798235453,20.3359676562647));
#25539=CARTESIAN_POINT('Ctrl Pts',(127.456385795957,-32.7592795493614,20.3371246720448));
#25540=CARTESIAN_POINT('Ctrl Pts',(127.433494644613,-32.7855747906894,20.3391674752441));
#25541=CARTESIAN_POINT('Ctrl Pts',(127.423749829932,-32.7969194756355,20.340049163677));
#25542=CARTESIAN_POINT('Ctrl Pts',(127.402465624827,-32.8220323876268,20.3420020647311));
#25543=CARTESIAN_POINT('Ctrl Pts',(127.390960555121,-32.8358278963901,20.3430754724506));
#25544=CARTESIAN_POINT('Ctrl Pts',(127.357195558682,-32.8769754180763,20.3462771949156));
#25545=CARTESIAN_POINT('Ctrl Pts',(127.33525286723,-32.9045832876639,20.3484254983314));
#25546=CARTESIAN_POINT('Ctrl Pts',(127.202225284048,-33.0774251784764,20.3618501159945));
#25547=CARTESIAN_POINT('Ctrl Pts',(127.102619442563,-33.2310981983309,20.3736613701719));
#25548=CARTESIAN_POINT('Ctrl Pts',(126.941073417759,-33.5309001692829,20.3956112185553));
#25549=CARTESIAN_POINT('Ctrl Pts',(126.876029076999,-33.6748218847371,20.4057322719259));
#25550=CARTESIAN_POINT('Ctrl Pts',(126.821241916136,-33.8227565643555,20.4155868599104));
#25551=CARTESIAN_POINT('Origin',(130.,-35.,23.));
#25552=CARTESIAN_POINT('',(126.821241920569,-33.8227565523843,21.6644320182169));
#25553=CARTESIAN_POINT('',(126.821241906568,-33.8227565901911,21.3230638867798));
#25554=CARTESIAN_POINT('',(126.821241915871,-33.8227565650715,23.));
#25555=CARTESIAN_POINT('',(126.610249333224,-35.0010395456522,20.1438703980445));
#25556=CARTESIAN_POINT('Ctrl Pts',(126.821241906568,-33.8227565901911,21.3230638867798));
#25557=CARTESIAN_POINT('Ctrl Pts',(126.859773755242,-33.7187140236256,21.3161349444083));
#25558=CARTESIAN_POINT('Ctrl Pts',(126.903393986687,-33.6166164168015,21.3090328813153));
#25559=CARTESIAN_POINT('Ctrl Pts',(127.06846590041,-33.277377232492,21.2847520991139));
#25560=CARTESIAN_POINT('Ctrl Pts',(127.212817793153,-33.0524426550774,21.2675617727641));
#25561=CARTESIAN_POINT('Ctrl Pts',(127.416488571569,-32.8048198627095,21.2480209965305));
#25562=CARTESIAN_POINT('Ctrl Pts',(127.451946182574,-32.763759989001,21.2447532248313));
#25563=CARTESIAN_POINT('Ctrl Pts',(127.508984933493,-32.7008282369973,21.2396985833579));
#25564=CARTESIAN_POINT('Ctrl Pts',(127.529902661678,-32.6783699499337,21.237885059339));
#25565=CARTESIAN_POINT('Ctrl Pts',(127.569397916283,-32.6371040792032,21.2345334744583));
#25566=CARTESIAN_POINT('Ctrl Pts',(127.587895871424,-32.6182239078389,21.2329922324592));
#25567=CARTESIAN_POINT('Ctrl Pts',(127.629779312757,-32.576463503472,21.2295643934529));
#25568=CARTESIAN_POINT('Ctrl Pts',(127.653279184206,-32.5537014131698,21.2276829775776));
#25569=CARTESIAN_POINT('Ctrl Pts',(127.725452292415,-32.4857914491748,21.2220260037073));
#25570=CARTESIAN_POINT('Ctrl Pts',(127.775126953947,-32.4417285833791,21.2182953501243));
#25571=CARTESIAN_POINT('Ctrl Pts',(127.895317455162,-32.3412666949094,21.2096092682179));
#25572=CARTESIAN_POINT('Ctrl Pts',(127.966855911994,-32.2861691340578,21.2046998713434));
#25573=CARTESIAN_POINT('Ctrl Pts',(128.153666406531,-32.1538293958193,21.1923918187075));
#25574=CARTESIAN_POINT('Ctrl Pts',(128.271635314369,-32.0806865297782,21.1850855022926));
#25575=CARTESIAN_POINT('Ctrl Pts',(128.542146797576,-31.9351237791153,21.1687632961399));
#25576=CARTESIAN_POINT('Ctrl Pts',(128.696273499869,-31.8664577763994,21.159740764265));
#25577=CARTESIAN_POINT('Ctrl Pts',(128.881867984865,-31.7998421691392,21.148517695639));
#25578=CARTESIAN_POINT('Ctrl Pts',(128.909011560901,-31.790487037579,21.1468674532568));
#25579=CARTESIAN_POINT('Ctrl Pts',(128.952042324984,-31.7762652523802,21.1442326366521));
#25580=CARTESIAN_POINT('Ctrl Pts',(128.967852670224,-31.7711684968163,21.1432606068666));
#25581=CARTESIAN_POINT('Ctrl Pts',(128.998317355534,-31.7615942611086,21.1413789191015));
#25582=CARTESIAN_POINT('Ctrl Pts',(129.012965587288,-31.7570996186416,21.1404702201279));
#25583=CARTESIAN_POINT('Ctrl Pts',(129.049226690899,-31.746241744309,21.1382118162415));
#25584=CARTESIAN_POINT('Ctrl Pts',(129.070873310223,-31.7399944469147,21.1368558427123));
#25585=CARTESIAN_POINT('Ctrl Pts',(129.154482959024,-31.7167647389613,21.1315927905092));
#25586=CARTESIAN_POINT('Ctrl Pts',(129.216858517564,-31.701330392302,21.127612585129));
#25587=CARTESIAN_POINT('Ctrl Pts',(129.390256962549,-31.6636193953959,21.1164675636157));
#25588=CARTESIAN_POINT('Ctrl Pts',(129.502014204305,-31.645118503067,21.1091966671459));
#25589=CARTESIAN_POINT('Ctrl Pts',(129.872525306431,-31.6027048368204,21.085168803525));
#25590=CARTESIAN_POINT('Ctrl Pts',(130.133153666791,-31.6029165292737,21.06847297977));
#25591=CARTESIAN_POINT('Ctrl Pts',(130.44101147656,-31.638686877902,21.0496515724498));
#25592=CARTESIAN_POINT('Ctrl Pts',(130.490663489561,-31.6455750464352,21.0466407698371));
#25593=CARTESIAN_POINT('Ctrl Pts',(130.569306660171,-31.6582687938726,21.0419094301623));
#25594=CARTESIAN_POINT('Ctrl Pts',(130.598404659501,-31.6633565558373,21.0401670069435));
#25595=CARTESIAN_POINT('Ctrl Pts',(130.653568123068,-31.6737466964143,21.0368782908773));
#25596=CARTESIAN_POINT('Ctrl Pts',(130.679644788603,-31.6789767613357,21.0353298748655));
#25597=CARTESIAN_POINT('Ctrl Pts',(130.739419842849,-31.6916990958462,21.0317935427955));
#25598=CARTESIAN_POINT('Ctrl Pts',(130.773071029569,-31.69940037501,21.0298123358701));
#25599=CARTESIAN_POINT('Ctrl Pts',(130.881222139028,-31.7258962530373,21.0234712052757));
#25600=CARTESIAN_POINT('Ctrl Pts',(130.955204878489,-31.7467104886632,21.0191744895268));
#25601=CARTESIAN_POINT('Ctrl Pts',(131.134528011522,-31.8038067201689,21.0088040968927));
#25602=CARTESIAN_POINT('Ctrl Pts',(131.238910812551,-31.8428006836137,21.0028073761437));
#25603=CARTESIAN_POINT('Ctrl Pts',(131.543193959248,-31.9738907795177,20.9851390168922));
#25604=CARTESIAN_POINT('Ctrl Pts',(131.736232105777,-32.0803650125761,20.9737018556521));
#25605=CARTESIAN_POINT('Ctrl Pts',(131.96877421985,-32.2398936285405,20.9581398140606));
#25606=CARTESIAN_POINT('Ctrl Pts',(132.018989343203,-32.2764104219727,20.9546589659596));
#25607=CARTESIAN_POINT('Ctrl Pts',(132.086309201272,-32.3282509280813,20.9497831011088));
#25608=CARTESIAN_POINT('Ctrl Pts',(132.104305545333,-32.3424019684997,20.9484584067004));
#25609=CARTESIAN_POINT('Ctrl Pts',(132.134037985052,-32.3662727742873,20.9462315983099));
#25610=CARTESIAN_POINT('Ctrl Pts',(132.145854732596,-32.3758916409401,20.9453363219601));
#25611=CARTESIAN_POINT('Ctrl Pts',(132.170279451822,-32.3960487399837,20.9434635057661));
#25612=CARTESIAN_POINT('Ctrl Pts',(132.182876218778,-32.4065994423888,20.9424851545431));
#25613=CARTESIAN_POINT('Ctrl Pts',(132.216630748349,-32.4352914511176,20.9398309037964));
#25614=CARTESIAN_POINT('Ctrl Pts',(132.237641853639,-32.4536024188978,20.9381436735157));
#25615=CARTESIAN_POINT('Ctrl Pts',(132.361954231143,-32.5646660703355,20.9279617628552));
#25616=CARTESIAN_POINT('Ctrl Pts',(132.459695164844,-32.663427345246,20.9191248187912));
#25617=CARTESIAN_POINT('Ctrl Pts',(132.73710780747,-32.9804847354087,20.8920502522279));
#25618=CARTESIAN_POINT('Ctrl Pts',(132.895850796657,-33.2155391924482,20.8737600413138));
#25619=CARTESIAN_POINT('Ctrl Pts',(133.047270541718,-33.5143047745597,20.8533746700617));
#25620=CARTESIAN_POINT('Ctrl Pts',(133.069862239451,-33.5615653141194,20.850222740593));
#25621=CARTESIAN_POINT('Ctrl Pts',(133.103777922287,-33.6369573581211,20.8453061307776));
#25622=CARTESIAN_POINT('Ctrl Pts',(133.115834630705,-33.6647482343102,20.8435171145053));
#25623=CARTESIAN_POINT('Ctrl Pts',(133.137628115932,-33.7168857587398,20.8402030236323));
#25624=CARTESIAN_POINT('Ctrl Pts',(133.147457988454,-33.7411907936983,20.8386749405761));
#25625=CARTESIAN_POINT('Ctrl Pts',(133.169070401186,-33.7964653693545,20.8352365975405));
#25626=CARTESIAN_POINT('Ctrl Pts',(133.180682916066,-33.8274987790066,20.8333320435934));
#25627=CARTESIAN_POINT('Ctrl Pts',(133.214972881802,-33.9233963337106,20.8275217668704));
#25628=CARTESIAN_POINT('Ctrl Pts',(133.236135386097,-33.9887855175925,20.8236647656838));
#25629=CARTESIAN_POINT('Ctrl Pts',(133.281714492032,-34.145757323562,20.8146143503214));
#25630=CARTESIAN_POINT('Ctrl Pts',(133.304307540692,-34.2378098354776,20.8094728603572));
#25631=CARTESIAN_POINT('Ctrl Pts',(133.34959295557,-34.4626452836973,20.7971677094481));
#25632=CARTESIAN_POINT('Ctrl Pts',(133.368287519213,-34.5960659019881,20.7900769695353));
#25633=CARTESIAN_POINT('Ctrl Pts',(133.392115984737,-34.8945444133617,20.7741590735634));
#25634=CARTESIAN_POINT('Ctrl Pts',(133.393230285814,-35.0595655312461,20.7653209861682));
#25635=CARTESIAN_POINT('Ctrl Pts',(133.380455323631,-35.2524706642951,20.7543152395594));
#25636=CARTESIAN_POINT('Ctrl Pts',(133.378209849686,-35.2809229952767,20.7526744686298));
#25637=CARTESIAN_POINT('Ctrl Pts',(133.374092816968,-35.3258488454448,20.7500513369237));
#25638=CARTESIAN_POINT('Ctrl Pts',(133.372459156744,-35.3423434218908,20.7490813338481));
#25639=CARTESIAN_POINT('Ctrl Pts',(133.369080721447,-35.3740795281454,20.747200562248));
#25640=CARTESIAN_POINT('Ctrl Pts',(133.367353347112,-35.3893222344036,20.7462907117488));
#25641=CARTESIAN_POINT('Ctrl Pts',(133.362821873032,-35.427020157652,20.7440250845846));
#25642=CARTESIAN_POINT('Ctrl Pts',(133.359896273264,-35.4494598279762,20.742662950993));
#25643=CARTESIAN_POINT('Ctrl Pts',(133.347689641711,-35.5362946605122,20.7373437950091));
#25644=CARTESIAN_POINT('Ctrl Pts',(133.336780582456,-35.600443273135,20.7333117251082));
#25645=CARTESIAN_POINT('Ctrl Pts',(133.30138720749,-35.7775627861017,20.7219627776854));
#25646=CARTESIAN_POINT('Ctrl Pts',(133.272961033268,-35.889654426404,20.7145357285367));
#25647=CARTESIAN_POINT('Ctrl Pts',(133.163544255588,-36.2440162374779,20.6906368715027));
#25648=CARTESIAN_POINT('Ctrl Pts',(133.060888270915,-36.4787127307769,20.6742375603121));
#25649=CARTESIAN_POINT('Ctrl Pts',(132.907423420061,-36.7435199997241,20.6556429101796));
#25650=CARTESIAN_POINT('Ctrl Pts',(132.881033665064,-36.7867899621619,20.6525977792643));
#25651=CARTESIAN_POINT('Ctrl Pts',(132.837679534634,-36.8544161171508,20.6478257097789));
#25652=CARTESIAN_POINT('Ctrl Pts',(132.821349335328,-36.8791679777266,20.6460762313326));
#25653=CARTESIAN_POINT('Ctrl Pts',(132.789774194258,-36.9256871430759,20.6427817354166));
#25654=CARTESIAN_POINT('Ctrl Pts',(132.774594061156,-36.9474955411837,20.6412344855192));
#25655=CARTESIAN_POINT('Ctrl Pts',(132.739229954676,-36.9970481342958,20.6377112186631));
#25656=CARTESIAN_POINT('Ctrl Pts',(132.718877890896,-37.0246691414448,20.635741730824));
#25657=CARTESIAN_POINT('Ctrl Pts',(132.652379795883,-37.112106342507,20.6294842577165));
#25658=CARTESIAN_POINT('Ctrl Pts',(132.604650864281,-37.1706927015846,20.6252570643444));
#25659=CARTESIAN_POINT('Ctrl Pts',(132.483623205743,-37.3095060094869,20.6151012301935));
#25660=CARTESIAN_POINT('Ctrl Pts',(132.408348446616,-37.387899103388,20.6092450690748));
#25661=CARTESIAN_POINT('Ctrl Pts',(132.181212029347,-37.6027579474692,20.5925577769525));
#25662=CARTESIAN_POINT('Ctrl Pts',(132.020640756066,-37.7292923828891,20.5819272899538));
#25663=CARTESIAN_POINT('Ctrl Pts',(131.783848104023,-37.8834808987926,20.5664898418752));
#25664=CARTESIAN_POINT('Ctrl Pts',(131.716552258405,-37.9240421868466,20.5621233185625));
#25665=CARTESIAN_POINT('Ctrl Pts',(131.626240949896,-37.9742831916333,20.5562100665069));
#25666=CARTESIAN_POINT('Ctrl Pts',(131.60443729217,-37.9861013093735,20.554778459207));
#25667=CARTESIAN_POINT('Ctrl Pts',(131.569938356575,-38.0043136657504,20.5525039863005));
#25668=CARTESIAN_POINT('Ctrl Pts',(131.55732874817,-38.0108693428522,20.5516707183298));
#25669=CARTESIAN_POINT('Ctrl Pts',(131.530832264893,-38.0244337657655,20.5499149730549));
#25670=CARTESIAN_POINT('Ctrl Pts',(131.516937833453,-38.0314264966941,20.5489914849855));
#25671=CARTESIAN_POINT('Ctrl Pts',(131.481708786511,-38.0488535843119,20.5466438550995));
#25672=CARTESIAN_POINT('Ctrl Pts',(131.460311943731,-38.059159699008,20.5452123530944));
#25673=CARTESIAN_POINT('Ctrl Pts',(131.370888872964,-38.1010797669131,20.5392117878531));
#25674=CARTESIAN_POINT('Ctrl Pts',(131.301935019881,-38.1306541806046,20.5345422854971));
#25675=CARTESIAN_POINT('Ctrl Pts',(131.094226399504,-38.2116918228963,20.5204653533826));
#25676=CARTESIAN_POINT('Ctrl Pts',(130.953021865792,-38.2563848872775,20.5108880952779));
#25677=CARTESIAN_POINT('Ctrl Pts',(130.610081511397,-38.3407059093794,20.4881481229481));
#25678=CARTESIAN_POINT('Ctrl Pts',(130.40674676347,-38.3715121055298,20.4750991709274));
#25679=CARTESIAN_POINT('Ctrl Pts',(130.148966182982,-38.386889557602,20.4593751703967));
#25680=CARTESIAN_POINT('Ctrl Pts',(130.096012796522,-38.3888041866135,20.4561857195452));
#25681=CARTESIAN_POINT('Ctrl Pts',(130.012615779515,-38.3898630236812,20.4512243572008));
#25682=CARTESIAN_POINT('Ctrl Pts',(129.982193071018,-38.3898397426532,20.4494273683715));
#25683=CARTESIAN_POINT('Ctrl Pts',(129.925322634463,-38.3890305651922,20.4460912071455));
#25684=CARTESIAN_POINT('Ctrl Pts',(129.898876014868,-38.388344563187,20.4445490925656));
#25685=CARTESIAN_POINT('Ctrl Pts',(129.83938678588,-38.3861043241054,20.4411000398793));
#25686=CARTESIAN_POINT('Ctrl Pts',(129.806353198417,-38.3843758841064,20.4391985895675));
#25687=CARTESIAN_POINT('Ctrl Pts',(129.705107801927,-38.3775910757621,20.433409050608));
#25688=CARTESIAN_POINT('Ctrl Pts',(129.637017468586,-38.3709534906077,20.4295691577197));
#25689=CARTESIAN_POINT('Ctrl Pts',(129.475809481098,-38.350296836443,20.4205684371169));
#25690=CARTESIAN_POINT('Ctrl Pts',(129.382982726584,-38.3344498597171,20.4154587048134));
#25691=CARTESIAN_POINT('Ctrl Pts',(129.077947882023,-38.2691991019591,20.3987181821178));
#25692=CARTESIAN_POINT('Ctrl Pts',(128.869863147881,-38.2032210988882,20.3874080410901));
#25693=CARTESIAN_POINT('Ctrl Pts',(128.588471843518,-38.0831420843416,20.3707764216785));
#25694=CARTESIAN_POINT('Ctrl Pts',(128.50877501658,-38.0453936494679,20.3658989754533));
#25695=CARTESIAN_POINT('Ctrl Pts',(128.407858305335,-37.9926828868083,20.359392964211));
#25696=CARTESIAN_POINT('Ctrl Pts',(128.38520702745,-37.9805217006054,20.3579104618822));
#25697=CARTESIAN_POINT('Ctrl Pts',(128.348716749315,-37.9603924757447,20.3554824904944));
#25698=CARTESIAN_POINT('Ctrl Pts',(128.334791467079,-37.9525820062384,20.3545464262084));
#25699=CARTESIAN_POINT('Ctrl Pts',(128.307236798478,-37.9368701011722,20.3526741810172));
#25700=CARTESIAN_POINT('Ctrl Pts',(128.293606329227,-37.9289714682675,20.3517381721666));
#25701=CARTESIAN_POINT('Ctrl Pts',(128.258733684731,-37.9084373067436,20.3493189972118));
#25702=CARTESIAN_POINT('Ctrl Pts',(128.237574069281,-37.8956641222464,20.3478275881173));
#25703=CARTESIAN_POINT('Ctrl Pts',(128.144209710245,-37.8379015087755,20.3411481912208));
#25704=CARTESIAN_POINT('Ctrl Pts',(128.073578741764,-37.7904375032694,20.3358306400722));
#25705=CARTESIAN_POINT('Ctrl Pts',(127.85126862087,-37.6285798321187,20.3183957051997));
#25706=CARTESIAN_POINT('Ctrl Pts',(127.707392184788,-37.5040823930608,20.3060271150506));
#25707=CARTESIAN_POINT('Ctrl Pts',(127.457056991398,-37.2477101688592,20.2831229962828));
#25708=CARTESIAN_POINT('Ctrl Pts',(127.348543251883,-37.1186199206653,20.2725675785924));
#25709=CARTESIAN_POINT('Ctrl Pts',(127.224081370735,-36.9459330465488,20.2597014097012));
#25710=CARTESIAN_POINT('Ctrl Pts',(127.198809954639,-36.9093753609102,20.2570417276768));
#25711=CARTESIAN_POINT('Ctrl Pts',(127.158595581403,-36.8486834884419,20.2527279720168));
#25712=CARTESIAN_POINT('Ctrl Pts',(127.143224528853,-36.8248407303131,20.2510582692216));
#25713=CARTESIAN_POINT('Ctrl Pts',(127.113803744457,-36.7779217975867,20.2478198728546));
#25714=CARTESIAN_POINT('Ctrl Pts',(127.099727051058,-36.7548651308258,20.246250281829));
#25715=CARTESIAN_POINT('Ctrl Pts',(127.066833631517,-36.6995108419458,20.2425322135636));
#25716=CARTESIAN_POINT('Ctrl Pts',(127.048272330219,-36.6670650759384,20.2403929232357));
#25717=CARTESIAN_POINT('Ctrl Pts',(126.983872086,-36.550042217053,20.2328116610712));
#25718=CARTESIAN_POINT('Ctrl Pts',(126.941099300056,-36.4638262121703,20.2274748578003));
#25719=CARTESIAN_POINT('Ctrl Pts',(126.837415130847,-36.2303731777448,20.2135375041085));
#25720=CARTESIAN_POINT('Ctrl Pts',(126.783113675241,-36.0804660023441,20.2051145483497));
#25721=CARTESIAN_POINT('Ctrl Pts',(126.71186937848,-35.8299646754079,20.191305205481));
#25722=CARTESIAN_POINT('Ctrl Pts',(126.688561079136,-35.7314474332906,20.1859351981973));
#25723=CARTESIAN_POINT('Ctrl Pts',(126.651263933784,-35.5349233021026,20.1751127654718));
#25724=CARTESIAN_POINT('Ctrl Pts',(126.637091279735,-35.4370558995753,20.1696699745491));
#25725=CARTESIAN_POINT('Ctrl Pts',(126.624573230346,-35.3124074518496,20.1625185518193));
#25726=CARTESIAN_POINT('Ctrl Pts',(126.622238982669,-35.2860676689685,20.160995002182));
#25727=CARTESIAN_POINT('Ctrl Pts',(126.61897784093,-35.2436272081478,20.158516461183));
#25728=CARTESIAN_POINT('Ctrl Pts',(126.617857237862,-35.2275420176978,20.1575716104813));
#25729=CARTESIAN_POINT('Ctrl Pts',(126.615979816103,-35.1975036991971,20.1557959404069));
#25730=CARTESIAN_POINT('Ctrl Pts',(126.615194438922,-35.1835527391387,20.1549667072676));
#25731=CARTESIAN_POINT('Ctrl Pts',(126.613711948982,-35.1539593154366,20.1531986225364));
#25732=CARTESIAN_POINT('Ctrl Pts',(126.613036921538,-35.1383160148335,20.1522586297319));
#25733=CARTESIAN_POINT('Ctrl Pts',(126.611002640217,-35.0821388850985,20.1488650590904));
#25734=CARTESIAN_POINT('Ctrl Pts',(126.610262546074,-35.0415878496477,20.1463819526198));
#25735=CARTESIAN_POINT('Ctrl Pts',(126.610250158162,-35.0010354991548,20.1438715788674));
#25736=CARTESIAN_POINT('Ctrl Pts',(126.610250159373,-35.0010394571165,20.143871823883));
#25737=CARTESIAN_POINT('Ctrl Pts',(126.610149230195,-34.6719016210195,20.1234967188205));
#25738=CARTESIAN_POINT('Ctrl Pts',(126.657981717222,-34.3444712680937,20.1016491473991));
#25739=CARTESIAN_POINT('Ctrl Pts',(126.773063007837,-33.9595473749733,20.0765392240846));
#25740=CARTESIAN_POINT('Ctrl Pts',(126.796058758342,-33.8907553870495,20.072064610877));
#25741=CARTESIAN_POINT('Ctrl Pts',(126.82124191022,-33.822756580328,20.0676573852273));
#25742=CARTESIAN_POINT('Ctrl Pts',(126.821241916136,-33.8227565643555,20.4155868599104));
#25743=CARTESIAN_POINT('Ctrl Pts',(126.820287593857,-33.8253333972916,20.4157585142308));
#25744=CARTESIAN_POINT('Ctrl Pts',(126.819336383827,-33.8279114475735,20.4159300917818));
#25745=CARTESIAN_POINT('Ctrl Pts',(126.78505051154,-33.9211850399282,20.4221320307644));
#25746=CARTESIAN_POINT('Ctrl Pts',(126.755603743355,-34.0132692357797,20.4280574555847));
#25747=CARTESIAN_POINT('Ctrl Pts',(126.720262735379,-34.1426028844148,20.43610650087));
#25748=CARTESIAN_POINT('Ctrl Pts',(126.710994121633,-34.1788746506242,20.4383349228403));
#25749=CARTESIAN_POINT('Ctrl Pts',(126.696072440349,-34.2415819426616,20.4421392521894));
#25750=CARTESIAN_POINT('Ctrl Pts',(126.690131375848,-34.2679446585663,20.4437241091623));
#25751=CARTESIAN_POINT('Ctrl Pts',(126.67860493898,-34.3221035893835,20.4469513216356));
#25752=CARTESIAN_POINT('Ctrl Pts',(126.673051753885,-34.3499045196963,20.4485925544366));
#25753=CARTESIAN_POINT('Ctrl Pts',(126.659707166987,-34.4213674361841,20.4527739451933));
#25754=CARTESIAN_POINT('Ctrl Pts',(126.652422558014,-34.4651192841586,20.4552982355576));
#25755=CARTESIAN_POINT('Ctrl Pts',(126.622062488983,-34.6725089710146,20.4671127850266));
#25756=CARTESIAN_POINT('Ctrl Pts',(126.610113321141,-34.8375542996702,20.4760588099895));
#25757=CARTESIAN_POINT('Ctrl Pts',(126.610434020515,-35.2220294011891,20.4965625636002));
#25758=CARTESIAN_POINT('Ctrl Pts',(126.631878462955,-35.440678979504,20.5079616797009));
#25759=CARTESIAN_POINT('Ctrl Pts',(126.686426697232,-35.7173448321876,20.5235153390101));
#25760=CARTESIAN_POINT('Ctrl Pts',(126.700289207335,-35.7786265741539,20.5270362472441));
#25761=CARTESIAN_POINT('Ctrl Pts',(126.721539861997,-35.8617615159784,20.5319595795821));
#25762=CARTESIAN_POINT('Ctrl Pts',(126.727460774096,-35.8839800561133,20.5332898991135));
#25763=CARTESIAN_POINT('Ctrl Pts',(126.737685090256,-35.9208361511508,20.5355234339344));
#25764=CARTESIAN_POINT('Ctrl Pts',(126.741862229316,-35.9355084429598,20.5364197197017));
#25765=CARTESIAN_POINT('Ctrl Pts',(126.750734759437,-35.9658930418776,20.5382915112906));
#25766=CARTESIAN_POINT('Ctrl Pts',(126.755445330979,-35.9816001970923,20.5392677917796));
#25767=CARTESIAN_POINT('Ctrl Pts',(126.768423509854,-36.0237610047166,20.5419105051132));
#25768=CARTESIAN_POINT('Ctrl Pts',(126.776901727913,-36.0501479074717,20.5435881087229));
#25769=CARTESIAN_POINT('Ctrl Pts',(126.828423407328,-36.2039958022773,20.5534961823521));
#25770=CARTESIAN_POINT('Ctrl Pts',(126.878697446336,-36.3288971841403,20.5620484418298));
#25771=CARTESIAN_POINT('Ctrl Pts',(127.060272170925,-36.712427684662,20.5893018835114));
#25772=CARTESIAN_POINT('Ctrl Pts',(127.217403975416,-36.9574532626752,20.6080878925377));
#25773=CARTESIAN_POINT('Ctrl Pts',(127.436522120658,-37.218461883155,20.6288049802505));
#25774=CARTESIAN_POINT('Ctrl Pts',(127.470098427761,-37.25667685306,20.6318631997782));
#25775=CARTESIAN_POINT('Ctrl Pts',(127.52480459498,-37.316184532881,20.6366678748007));
#25776=CARTESIAN_POINT('Ctrl Pts',(127.545377853937,-37.33797632362,20.6384368539857));
#25777=CARTESIAN_POINT('Ctrl Pts',(127.584692667842,-37.3785286395582,20.6417479216268));
#25778=CARTESIAN_POINT('Ctrl Pts',(127.603370509505,-37.3973475221807,20.6432925386918));
#25779=CARTESIAN_POINT('Ctrl Pts',(127.646331585218,-37.4396290764838,20.6467826823124));
#25780=CARTESIAN_POINT('Ctrl Pts',(127.670748638937,-37.4629521415749,20.6487221399036));
#25781=CARTESIAN_POINT('Ctrl Pts',(127.748549328397,-37.5350750509929,20.6547694761412));
#25782=CARTESIAN_POINT('Ctrl Pts',(127.803150163531,-37.5825350826226,20.6588224105451));
#25783=CARTESIAN_POINT('Ctrl Pts',(127.938266990732,-37.6925923117058,20.6684504514533));
#25784=CARTESIAN_POINT('Ctrl Pts',(128.020170538602,-37.7533749370772,20.6739634071083));
#25785=CARTESIAN_POINT('Ctrl Pts',(128.144188316743,-37.8370120573627,20.6819655826703));
#25786=CARTESIAN_POINT('Ctrl Pts',(128.184241343463,-37.8628124305117,20.6845005365484));
#25787=CARTESIAN_POINT('Ctrl Pts',(128.402282279954,-37.9968473667998,20.6980904430487));
#25788=CARTESIAN_POINT('Ctrl Pts',(128.589400201139,-38.0893346173491,20.7089922971266));
#25789=CARTESIAN_POINT('Ctrl Pts',(128.827700399478,-38.180932354407,20.7232391805213));
#25790=CARTESIAN_POINT('Ctrl Pts',(128.87194446919,-38.1968902496851,20.7258999659437));
#25791=CARTESIAN_POINT('Ctrl Pts',(128.934236314361,-38.2179035177958,20.7296863015));
#25792=CARTESIAN_POINT('Ctrl Pts',(128.952017549844,-38.2237382079705,20.7307716347112));
#25793=CARTESIAN_POINT('Ctrl Pts',(128.984257072195,-38.2340222921873,20.7327491497458));
#25794=CARTESIAN_POINT('Ctrl Pts',(128.998698807387,-38.2385227801463,20.7336384855201));
#25795=CARTESIAN_POINT('Ctrl Pts',(129.02910307024,-38.2477748656496,20.7355189673773));
#25796=CARTESIAN_POINT('Ctrl Pts',(129.045071095319,-38.2525056783061,20.7365111641546));
#25797=CARTESIAN_POINT('Ctrl Pts',(129.088851164086,-38.2651261249449,20.7392427823008));
#25798=CARTESIAN_POINT('Ctrl Pts',(129.116729684759,-38.2727777563369,20.7409946300442));
#25799=CARTESIAN_POINT('Ctrl Pts',(129.323955843639,-38.3268132221219,20.7540907523586));
#25800=CARTESIAN_POINT('Ctrl Pts',(129.506725061284,-38.3587780848658,20.7660344910275));
#25801=CARTESIAN_POINT('Ctrl Pts',(129.924822853205,-38.3970285891289,20.7930980191956));
#25802=CARTESIAN_POINT('Ctrl Pts',(130.160096080795,-38.3940912060254,20.808111416691));
#25803=CARTESIAN_POINT('Ctrl Pts',(130.444922949057,-38.3608272616754,20.8255602516092));
#25804=CARTESIAN_POINT('Ctrl Pts',(130.49649707673,-38.3535961915296,20.8286933374334));
#25805=CARTESIAN_POINT('Ctrl Pts',(130.577715390762,-38.3402939434571,20.8335874604137));
#25806=CARTESIAN_POINT('Ctrl Pts',(130.607478426116,-38.3350095579873,20.8353724645112));
#25807=CARTESIAN_POINT('Ctrl Pts',(130.662924281831,-38.3243983165584,20.838682939486));
#25808=CARTESIAN_POINT('Ctrl Pts',(130.68862346733,-38.3191701595135,20.8402113598081));
#25809=CARTESIAN_POINT('Ctrl Pts',(130.746741669479,-38.3066427120293,20.8436553956946));
#25810=CARTESIAN_POINT('Ctrl Pts',(130.779119478534,-38.2991638480062,20.845565225006));
#25811=CARTESIAN_POINT('Ctrl Pts',(130.878617047122,-38.2746346837263,20.8514108523649));
#25812=CARTESIAN_POINT('Ctrl Pts',(130.9453302802,-38.2560024246874,20.8552970258375));
#25813=CARTESIAN_POINT('Ctrl Pts',(131.102856956312,-38.2067565479753,20.864432441114));
#25814=CARTESIAN_POINT('Ctrl Pts',(131.193035764187,-38.1743106875792,20.8696283227387));
#25815=CARTESIAN_POINT('Ctrl Pts',(131.405175393261,-38.0876641796424,20.8819172570561));
#25816=CARTESIAN_POINT('Ctrl Pts',(131.525545902882,-38.0299996908448,20.888942274422));
#25817=CARTESIAN_POINT('Ctrl Pts',(131.774703126616,-37.8920189123316,20.9040844365503));
#25818=CARTESIAN_POINT('Ctrl Pts',(131.902121670271,-37.8098521388453,20.9122038045981));
#25819=CARTESIAN_POINT('Ctrl Pts',(132.0525130592,-37.6979424448265,20.9227842417959));
#25820=CARTESIAN_POINT('Ctrl Pts',(132.081073188371,-37.6759741144796,20.9248416205529));
#25821=CARTESIAN_POINT('Ctrl Pts',(132.123456332016,-37.6422843108382,20.9279768837471));
#25822=CARTESIAN_POINT('Ctrl Pts',(132.137545233771,-37.6308997538443,20.9290330893307));
#25823=CARTESIAN_POINT('Ctrl Pts',(132.162976895045,-37.6100105352697,20.9309665950521));
#25824=CARTESIAN_POINT('Ctrl Pts',(132.174349628666,-37.6005437335457,20.9318413113802));
#25825=CARTESIAN_POINT('Ctrl Pts',(132.200655042083,-37.578353602582,20.9338879865361));
#25826=CARTESIAN_POINT('Ctrl Pts',(132.215539574857,-37.565574841197,20.9350637486538));
#25827=CARTESIAN_POINT('Ctrl Pts',(132.263636356245,-37.5235518172059,20.9389186129392));
#25828=CARTESIAN_POINT('Ctrl Pts',(132.296385770554,-37.4937873456795,20.9416309347357));
#25829=CARTESIAN_POINT('Ctrl Pts',(132.375570207479,-37.4189376058717,20.9483882534124));
#25830=CARTESIAN_POINT('Ctrl Pts',(132.421314034323,-37.3731477959729,20.9524679640954));
#25831=CARTESIAN_POINT('Ctrl Pts',(132.639045064265,-37.1423460921838,20.972660057934));
#25832=CARTESIAN_POINT('Ctrl Pts',(132.791314782899,-36.9397904969845,20.9891813928842));
#25833=CARTESIAN_POINT('Ctrl Pts',(132.972656275966,-36.6323598482052,21.0115501811179));
#25834=CARTESIAN_POINT('Ctrl Pts',(133.021477092835,-36.540118042203,21.0179694783276));
#25835=CARTESIAN_POINT('Ctrl Pts',(133.082792203004,-36.4100896863981,21.0266180496944));
#25836=CARTESIAN_POINT('Ctrl Pts',(133.098990987637,-36.3741236284215,21.0289699883953));
#25837=CARTESIAN_POINT('Ctrl Pts',(133.124285881217,-36.3152376850167,21.0327572776763));
#25838=CARTESIAN_POINT('Ctrl Pts',(133.133765804597,-36.2924876654957,21.0342053433743));
#25839=CARTESIAN_POINT('Ctrl Pts',(133.153224587626,-36.2443172414362,21.0372404632677));
#25840=CARTESIAN_POINT('Ctrl Pts',(133.163146112001,-36.2188754798109,21.0388255311379));
#25841=CARTESIAN_POINT('Ctrl Pts',(133.186503883485,-36.1567724118986,21.0426527227575));
#25842=CARTESIAN_POINT('Ctrl Pts',(133.199616413212,-36.1199930350217,21.044884154967));
#25843=CARTESIAN_POINT('Ctrl Pts',(133.247159301728,-35.9789838942373,21.0533150691245));
#25844=CARTESIAN_POINT('Ctrl Pts',(133.277156909894,-35.8733262245528,21.0593735941721));
#25845=CARTESIAN_POINT('Ctrl Pts',(133.348234777279,-35.5670892124865,21.0764258355136));
#25846=CARTESIAN_POINT('Ctrl Pts',(133.376353233746,-35.3640124893995,21.087105006235));
#25847=CARTESIAN_POINT('Ctrl Pts',(133.392305716176,-35.0256567040839,21.1052179492294));
#25848=CARTESIAN_POINT('Ctrl Pts',(133.390663907451,-34.8914297655106,21.1124954389765));
#25849=CARTESIAN_POINT('Ctrl Pts',(133.379068377582,-34.729646136544,21.1217343647834));
#25850=CARTESIAN_POINT('Ctrl Pts',(133.376711765118,-34.7016514480393,21.1233501728052));
#25851=CARTESIAN_POINT('Ctrl Pts',(133.372421166223,-34.6572871173794,21.1259425081241));
#25852=CARTESIAN_POINT('Ctrl Pts',(133.370715210553,-34.6408961335983,21.1269071644245));
#25853=CARTESIAN_POINT('Ctrl Pts',(133.367184962585,-34.6092220824792,21.1287857067231));
#25854=CARTESIAN_POINT('Ctrl Pts',(133.365375987353,-34.5939379569628,21.1296987844487));
#25855=CARTESIAN_POINT('Ctrl Pts',(133.360616237692,-34.5559412934743,21.1319843497481));
#25856=CARTESIAN_POINT('Ctrl Pts',(133.357539253476,-34.5332455351663,21.1333634378651));
#25857=CARTESIAN_POINT('Ctrl Pts',(133.344508280128,-34.4439373361143,21.1388404313999));
#25858=CARTESIAN_POINT('Ctrl Pts',(133.332800420255,-34.3776002467393,21.1430189259567));
#25859=CARTESIAN_POINT('Ctrl Pts',(133.294264914669,-34.1917846567766,21.1549567697375));
#25860=CARTESIAN_POINT('Ctrl Pts',(133.262929354052,-34.0733486064671,21.162838424998));
#25861=CARTESIAN_POINT('Ctrl Pts',(133.150438565884,-33.7255368893349,21.1864011314886));
#25862=CARTESIAN_POINT('Ctrl Pts',(133.050935071364,-33.5028864628366,21.2019842645644));
#25863=CARTESIAN_POINT('Ctrl Pts',(132.902563947965,-33.2483811352218,21.219900462612));
#25864=CARTESIAN_POINT('Ctrl Pts',(132.875673876993,-33.2045762881228,21.2229914967536));
#25865=CARTESIAN_POINT('Ctrl Pts',(132.831481069952,-33.1361263791028,21.2278353957712));
#25866=CARTESIAN_POINT('Ctrl Pts',(132.81482911876,-33.1110725149671,21.2296114125014));
#25867=CARTESIAN_POINT('Ctrl Pts',(132.784383061657,-33.0665614495388,21.2327732546111));
#25868=CARTESIAN_POINT('Ctrl Pts',(132.77071311444,-33.0470221345846,21.234163548169));
#25869=CARTESIAN_POINT('Ctrl Pts',(132.738068487334,-33.001393846203,21.237416552046));
#25870=CARTESIAN_POINT('Ctrl Pts',(132.718925151498,-32.9754280149584,21.2392727411446));
#25871=CARTESIAN_POINT('Ctrl Pts',(132.660760526403,-32.8988473454725,21.2447657551839));
#25872=CARTESIAN_POINT('Ctrl Pts',(132.620674489013,-32.8490571835975,21.2483615817674));
#25873=CARTESIAN_POINT('Ctrl Pts',(132.472469089335,-32.6752725775131,21.2610464877853));
#25874=CARTESIAN_POINT('Ctrl Pts',(132.356761512215,-32.5580453977352,21.269845693574));
#25875=CARTESIAN_POINT('Ctrl Pts',(132.073651224566,-32.3101616406124,21.2898223389195));
#25876=CARTESIAN_POINT('Ctrl Pts',(131.901600002336,-32.1858998320389,21.3009073687721));
#25877=CARTESIAN_POINT('Ctrl Pts',(131.680813906284,-32.055981768142,21.3152499794785));
#25878=CARTESIAN_POINT('Ctrl Pts',(131.64208752184,-32.0342072019635,21.3177707359521));
#25879=CARTESIAN_POINT('Ctrl Pts',(131.585817718685,-32.0040084913975,21.3214566269803));
#25880=CARTESIAN_POINT('Ctrl Pts',(131.56861074205,-31.9949636844864,21.322586812008));
#25881=CARTESIAN_POINT('Ctrl Pts',(131.538038788806,-31.9792277283836,21.3246018904176));
#25882=CARTESIAN_POINT('Ctrl Pts',(131.524705897415,-31.9724762020515,21.3254831165395));
#25883=CARTESIAN_POINT('Ctrl Pts',(131.495161865255,-31.9577603219726,21.3274414986867));
#25884=CARTESIAN_POINT('Ctrl Pts',(131.478931653073,-31.9498373166076,21.3285209416322));
#25885=CARTESIAN_POINT('Ctrl Pts',(131.430378892346,-31.9266142257537,21.3317590492175));
#25886=CARTESIAN_POINT('Ctrl Pts',(131.397877670878,-31.9116959846269,21.3339383548076));
#25887=CARTESIAN_POINT('Ctrl Pts',(131.233519125562,-31.8393804535754,21.3449957003125));
#25888=CARTESIAN_POINT('Ctrl Pts',(131.098348199541,-31.7899049800216,21.3542004646612));
#25889=CARTESIAN_POINT('Ctrl Pts',(130.699241030071,-31.6719890429284,21.3809974654698));
#25890=CARTESIAN_POINT('Ctrl Pts',(130.429625960381,-31.6265648421354,21.3985436677035));
#25891=CARTESIAN_POINT('Ctrl Pts',(130.109125059716,-31.6116615507698,21.4180011702165));
#25892=CARTESIAN_POINT('Ctrl Pts',(130.060752571116,-31.6104491134969,21.4209044068304));
#25893=CARTESIAN_POINT('Ctrl Pts',(129.983190022656,-31.6101660959475,21.4255079706179));
#25894=CARTESIAN_POINT('Ctrl Pts',(129.954010476047,-31.6104363826967,21.4272281844018));
#25895=CARTESIAN_POINT('Ctrl Pts',(129.898156769915,-31.6116751597812,21.4304995703979));
#25896=CARTESIAN_POINT('Ctrl Pts',(129.871483563404,-31.6125819785923,21.4320525129762));
#25897=CARTESIAN_POINT('Ctrl Pts',(129.809612709081,-31.6154172887375,21.4356343324276));
#25898=CARTESIAN_POINT('Ctrl Pts',(129.774428565088,-31.6175799920439,21.4376558776803));
#25899=CARTESIAN_POINT('Ctrl Pts',(129.658128238933,-31.626551594448,21.4442926742673));
#25900=CARTESIAN_POINT('Ctrl Pts',(129.57722098049,-31.6357334005355,21.4488357700602));
#25901=CARTESIAN_POINT('Ctrl Pts',(129.376603024897,-31.6658533143611,21.4599866375184));
#25902=CARTESIAN_POINT('Ctrl Pts',(129.257539108534,-31.6903304809292,21.4664997638447));
#25903=CARTESIAN_POINT('Ctrl Pts',(128.962595429627,-31.7676866294816,21.4827179892139));
#25904=CARTESIAN_POINT('Ctrl Pts',(128.789230696818,-31.8285510376674,21.4923211826765));
#25905=CARTESIAN_POINT('Ctrl Pts',(128.55041494736,-31.9348428776452,21.5066067726672));
#25906=CARTESIAN_POINT('Ctrl Pts',(128.480298371473,-31.9689951799723,21.5109421688899));
#25907=CARTESIAN_POINT('Ctrl Pts',(128.389567187416,-32.0171283052853,21.5168194241486));
#25908=CARTESIAN_POINT('Ctrl Pts',(128.3678358013,-32.0289635910794,21.5182479330366));
#25909=CARTESIAN_POINT('Ctrl Pts',(128.333839870898,-32.0479638940704,21.5205186715805));
#25910=CARTESIAN_POINT('Ctrl Pts',(128.321487030528,-32.0549701288763,21.5213513578358));
#25911=CARTESIAN_POINT('Ctrl Pts',(128.295687957207,-32.0698177857296,21.5231071599524));
#25912=CARTESIAN_POINT('Ctrl Pts',(128.282251179972,-32.0776745033739,21.52403130068));
#25913=CARTESIAN_POINT('Ctrl Pts',(128.248406194686,-32.097778317842,21.5263827223055));
#25914=CARTESIAN_POINT('Ctrl Pts',(128.228072201531,-32.1101482117179,21.5278174099003));
#25915=CARTESIAN_POINT('Ctrl Pts',(128.143777184807,-32.1626520101382,21.5338517000191));
#25916=CARTESIAN_POINT('Ctrl Pts',(128.081039854025,-32.2047009002592,21.5385530978229));
#25917=CARTESIAN_POINT('Ctrl Pts',(127.898206825027,-32.3362992590072,21.5527791308458));
#25918=CARTESIAN_POINT('Ctrl Pts',(127.782586113114,-32.431749755275,21.5624770742481));
#25919=CARTESIAN_POINT('Ctrl Pts',(127.526206777901,-32.6736612024014,21.5851702616093));
#25920=CARTESIAN_POINT('Ctrl Pts',(127.391514919853,-32.8257572873833,21.5980547467719));
#25921=CARTESIAN_POINT('Ctrl Pts',(127.239764229064,-33.0316724069148,21.6136300876327));
#25922=CARTESIAN_POINT('Ctrl Pts',(127.209320179376,-33.0750787970273,21.6168214262843));
#25923=CARTESIAN_POINT('Ctrl Pts',(127.16302275823,-33.1444971020334,21.6217850418477));
#25924=CARTESIAN_POINT('Ctrl Pts',(127.146481326923,-33.170037664999,21.6235824336054));
#25925=CARTESIAN_POINT('Ctrl Pts',(127.116205688537,-33.2181932713178,21.6269189698705));
#25926=CARTESIAN_POINT('Ctrl Pts',(127.102388120413,-33.2407529158776,21.6284610623735));
#25927=CARTESIAN_POINT('Ctrl Pts',(127.071895827569,-33.2918710649817,21.6319095880549));
#25928=CARTESIAN_POINT('Ctrl Pts',(127.055371941876,-33.3205166827609,21.6338105410874));
#25929=CARTESIAN_POINT('Ctrl Pts',(127.005990138883,-33.4090943123837,21.6395967470595));
#25930=CARTESIAN_POINT('Ctrl Pts',(126.974522390244,-33.4697836568545,21.6434338885759));
#25931=CARTESIAN_POINT('Ctrl Pts',(126.904172418033,-33.6161294763308,21.6524266251195));
#25932=CARTESIAN_POINT('Ctrl Pts',(126.866977252481,-33.7025347427677,21.6575312572186));
#25933=CARTESIAN_POINT('Ctrl Pts',(126.829305917559,-33.8011517640883,21.6631969367738));
#25934=CARTESIAN_POINT('Ctrl Pts',(126.825246120578,-33.8119445294727,21.6638149053911));
#25935=CARTESIAN_POINT('Ctrl Pts',(126.821241920569,-33.8227565523843,21.6644320182169));
#25936=CARTESIAN_POINT('Origin',(130.,-35.,23.));
#25937=CARTESIAN_POINT('',(126.821241915871,-33.8227565650708,22.910437866903));
#25938=CARTESIAN_POINT('',(126.82124189288,-33.8227566271494,22.5700841492926));
#25939=CARTESIAN_POINT('',(126.821241915871,-33.8227565650715,23.));
#25940=CARTESIAN_POINT('Ctrl Pts',(126.82124189288,-33.8227566271494,22.5700841492926));
#25941=CARTESIAN_POINT('Ctrl Pts',(126.875221356717,-33.6770028584336,22.5618222215772));
#25942=CARTESIAN_POINT('Ctrl Pts',(126.939173664941,-33.5351017100661,22.5536556010467));
#25943=CARTESIAN_POINT('Ctrl Pts',(127.044327726873,-33.3390072460445,22.5416122053039));
#25944=CARTESIAN_POINT('Ctrl Pts',(127.077738565226,-33.2809064246452,22.5379406552031));
#25945=CARTESIAN_POINT('Ctrl Pts',(127.136615781811,-33.1852015218415,22.5316547567207));
#25946=CARTESIAN_POINT('Ctrl Pts',(127.161156104269,-33.147048941982,22.5290826089747));
#25947=CARTESIAN_POINT('Ctrl Pts',(127.197499573133,-33.092963378713,22.5253228145811));
#25948=CARTESIAN_POINT('Ctrl Pts',(127.208689415927,-33.0766221120918,22.5241715736982));
#25949=CARTESIAN_POINT('Ctrl Pts',(127.228574699369,-33.0481213398838,22.5221350008219));
#25950=CARTESIAN_POINT('Ctrl Pts',(127.237208371548,-33.0359198319151,22.5212536770162));
#25951=CARTESIAN_POINT('Ctrl Pts',(127.25643899417,-33.0091199319431,22.519296588666));
#25952=CARTESIAN_POINT('Ctrl Pts',(127.267071805655,-32.9945489558439,22.5182185586158));
#25953=CARTESIAN_POINT('Ctrl Pts',(127.299060536642,-32.9514391369945,22.5149889810653));
#25954=CARTESIAN_POINT('Ctrl Pts',(127.320750228251,-32.9231523797288,22.5128169463551));
#25955=CARTESIAN_POINT('Ctrl Pts',(127.432642462585,-32.7818976367237,22.5017215039121));
#25956=CARTESIAN_POINT('Ctrl Pts',(127.529554033828,-32.6744478246296,22.4924672381036));
#25957=CARTESIAN_POINT('Ctrl Pts',(127.721678552639,-32.4870342214296,22.4751843327712));
#25958=CARTESIAN_POINT('Ctrl Pts',(127.815015076258,-32.4054695775771,22.4671815930314));
#25959=CARTESIAN_POINT('Ctrl Pts',(127.995772758507,-32.2641967550436,22.4525565229874));
#25960=CARTESIAN_POINT('Ctrl Pts',(128.081933114347,-32.2031144807136,22.4459119587034));
#25961=CARTESIAN_POINT('Ctrl Pts',(128.233179187261,-32.1061725446786,22.4348282356796));
#25962=CARTESIAN_POINT('Ctrl Pts',(128.296845796887,-32.0682496432615,22.4303246455869));
#25963=CARTESIAN_POINT('Ctrl Pts',(128.391527846991,-32.0159787804679,22.4238573207223));
#25964=CARTESIAN_POINT('Ctrl Pts',(128.421594965392,-31.9999661702924,22.4218361685239));
#25965=CARTESIAN_POINT('Ctrl Pts',(128.475512611406,-31.9722867029102,22.4182680576704));
#25966=CARTESIAN_POINT('Ctrl Pts',(128.499268091112,-31.9604419063832,22.4167150472767));
#25967=CARTESIAN_POINT('Ctrl Pts',(128.549973947418,-31.9358986805628,22.4134393429106));
#25968=CARTESIAN_POINT('Ctrl Pts',(128.576957639627,-31.9232739850169,22.4117192621436));
#25969=CARTESIAN_POINT('Ctrl Pts',(128.650893790988,-31.8898627437939,22.4070663652008));
#25970=CARTESIAN_POINT('Ctrl Pts',(128.698158637001,-31.8697842294994,22.4041572684698));
#25971=CARTESIAN_POINT('Ctrl Pts',(128.977721208215,-31.7584517649315,22.3872945684435));
#25972=CARTESIAN_POINT('Ctrl Pts',(129.219065434033,-31.6920034490645,22.3741831590362));
#25973=CARTESIAN_POINT('Ctrl Pts',(129.582798735268,-31.6339266193383,22.3546218455725));
#25974=CARTESIAN_POINT('Ctrl Pts',(129.700961062595,-31.6213790619869,22.3482831836327));
#25975=CARTESIAN_POINT('Ctrl Pts',(129.885572754549,-31.61153641757,22.3381009691775));
#25976=CARTESIAN_POINT('Ctrl Pts',(129.951699729036,-31.6099491172216,22.3343977877195));
#25977=CARTESIAN_POINT('Ctrl Pts',(130.040585416341,-31.6104165625916,22.3292958785399));
#25978=CARTESIAN_POINT('Ctrl Pts',(130.063342108821,-31.6107654592859,22.3279787206335));
#25979=CARTESIAN_POINT('Ctrl Pts',(130.101451985475,-31.6117336865038,22.325752033465));
#25980=CARTESIAN_POINT('Ctrl Pts',(130.116808051709,-31.6122283151603,22.3248491091045));
#25981=CARTESIAN_POINT('Ctrl Pts',(130.148676924486,-31.6134717700329,22.3229625404597));
#25982=CARTESIAN_POINT('Ctrl Pts',(130.165188343072,-31.6142370038163,22.3219781148505));
#25983=CARTESIAN_POINT('Ctrl Pts',(130.209977563612,-31.6166411954713,22.3192899832394));
#25984=CARTESIAN_POINT('Ctrl Pts',(130.238240876734,-31.6185138551292,22.3175744716415));
#25985=CARTESIAN_POINT('Ctrl Pts',(130.418759564762,-31.6327489157916,22.3065084140503));
#25986=CARTESIAN_POINT('Ctrl Pts',(130.570043585579,-31.6550364373433,22.2967454988852));
#25987=CARTESIAN_POINT('Ctrl Pts',(130.905315344659,-31.7278378878598,22.2746608816278));
#25988=CARTESIAN_POINT('Ctrl Pts',(131.087619518073,-31.7838322343053,22.2623521568806));
#25989=CARTESIAN_POINT('Ctrl Pts',(131.362576995636,-31.8943574607892,22.2437822505309));
#25990=CARTESIAN_POINT('Ctrl Pts',(131.458987260906,-31.9384658433892,22.2372640026014));
#25991=CARTESIAN_POINT('Ctrl Pts',(131.58749118131,-32.0047092228763,22.2285739755291));
#25992=CARTESIAN_POINT('Ctrl Pts',(131.621497940462,-32.0229814068246,22.2262737573928));
#25993=CARTESIAN_POINT('Ctrl Pts',(131.678945818758,-32.0551252569402,22.2223856046329));
#25994=CARTESIAN_POINT('Ctrl Pts',(131.702544840901,-32.0687055003295,22.2207876772764));
#25995=CARTESIAN_POINT('Ctrl Pts',(131.750090236053,-32.0968337793337,22.2175658640644));
#25996=CARTESIAN_POINT('Ctrl Pts',(131.774024992314,-32.1113973387821,22.215942694943));
#25997=CARTESIAN_POINT('Ctrl Pts',(131.833983331831,-32.1489065021916,22.2118715301933));
#25998=CARTESIAN_POINT('Ctrl Pts',(131.869759457529,-32.1722396148944,22.2094377336443));
#25999=CARTESIAN_POINT('Ctrl Pts',(132.017878554505,-32.2728830341861,22.1993285089663));
#26000=CARTESIAN_POINT('Ctrl Pts',(132.125949432966,-32.3562630461693,22.1918781044542));
#26001=CARTESIAN_POINT('Ctrl Pts',(132.39383308219,-32.5900218777712,22.1727849839951));
#26002=CARTESIAN_POINT('Ctrl Pts',(132.544583463436,-32.7497737115449,22.1614079093625));
#26003=CARTESIAN_POINT('Ctrl Pts',(132.716442449432,-32.9714269845317,22.1461691520912));
#26004=CARTESIAN_POINT('Ctrl Pts',(132.75270557425,-33.0209145157086,22.1427952045048));
#26005=CARTESIAN_POINT('Ctrl Pts',(132.811836850997,-33.1063810954357,22.1369668667414));
#26006=CARTESIAN_POINT('Ctrl Pts',(132.835406014853,-33.1418580735475,22.1345471040134));
#26007=CARTESIAN_POINT('Ctrl Pts',(132.868690455659,-33.1940670644545,22.1309711652016));
#26008=CARTESIAN_POINT('Ctrl Pts',(132.87894164973,-33.2104543489647,22.1298466606475));
#26009=CARTESIAN_POINT('Ctrl Pts',(132.896855656515,-33.2396435157445,22.127838350852));
#26010=CARTESIAN_POINT('Ctrl Pts',(132.904574953705,-33.2524096677341,22.1269581315384));
#26011=CARTESIAN_POINT('Ctrl Pts',(132.92163476998,-33.2810484332341,22.1249790993513));
#26012=CARTESIAN_POINT('Ctrl Pts',(132.930930293566,-33.2969463313673,22.1238776689857));
#26013=CARTESIAN_POINT('Ctrl Pts',(132.958808882547,-33.3455306645392,22.1205049494262));
#26014=CARTESIAN_POINT('Ctrl Pts',(132.976977472753,-33.3784502287916,22.1182105201633));
#26015=CARTESIAN_POINT('Ctrl Pts',(133.096987633331,-33.604713198634,22.1024129100212));
#26016=CARTESIAN_POINT('Ctrl Pts',(133.180468150924,-33.8072004344837,22.0881766317165));
#26017=CARTESIAN_POINT('Ctrl Pts',(133.302260934746,-34.2088278577358,22.0612052177804));
#26018=CARTESIAN_POINT('Ctrl Pts',(133.343396063065,-34.4061945576884,22.0484936598183));
#26019=CARTESIAN_POINT('Ctrl Pts',(133.372016960801,-34.6508073356001,22.0335998169214));
#26020=CARTESIAN_POINT('Ctrl Pts',(133.376359421202,-34.6956461724549,22.0309027334509));
#26021=CARTESIAN_POINT('Ctrl Pts',(133.381987648654,-34.7689668518173,22.0265444658337));
#26022=CARTESIAN_POINT('Ctrl Pts',(133.383810041427,-34.7974007679625,22.0248670226781));
#26023=CARTESIAN_POINT('Ctrl Pts',(133.386658289675,-34.8527689791085,22.0216243055483));
#26024=CARTESIAN_POINT('Ctrl Pts',(133.387721816002,-34.8796991129522,22.0200579919012));
#26025=CARTESIAN_POINT('Ctrl Pts',(133.389483026834,-34.9436213208268,22.0163645832592));
#26026=CARTESIAN_POINT('Ctrl Pts',(133.389896494211,-34.9806181651762,22.0142463385183));
#26027=CARTESIAN_POINT('Ctrl Pts',(133.389250312565,-35.1049616979434,22.0071858335102));
#26028=CARTESIAN_POINT('Ctrl Pts',(133.385420458441,-35.1922619273485,22.0023271882629));
#26029=CARTESIAN_POINT('Ctrl Pts',(133.355756761783,-35.5510255332498,21.9826167083828));
#26030=CARTESIAN_POINT('Ctrl Pts',(133.300598417627,-35.8190074566996,21.9685856390136));
#26031=CARTESIAN_POINT('Ctrl Pts',(133.192848217436,-36.1404078295949,21.9502306191092));
#26032=CARTESIAN_POINT('Ctrl Pts',(133.169909743399,-36.2026974248961,21.9465927620871));
#26033=CARTESIAN_POINT('Ctrl Pts',(133.128355873861,-36.3060720986387,21.9403584028179));
#26034=CARTESIAN_POINT('Ctrl Pts',(133.110721785273,-36.3475326983147,21.9378032073753));
#26035=CARTESIAN_POINT('Ctrl Pts',(133.084175471041,-36.4066474069874,21.9340638251363));
#26036=CARTESIAN_POINT('Ctrl Pts',(133.075926200067,-36.4245958145135,21.9329155017651));
#26037=CARTESIAN_POINT('Ctrl Pts',(133.061161509957,-36.4559940228749,21.9308820597518));
#26038=CARTESIAN_POINT('Ctrl Pts',(133.054713288279,-36.4694744294754,21.9300009033708));
#26039=CARTESIAN_POINT('Ctrl Pts',(133.040267886372,-36.4991674397782,21.928041626554));
#26040=CARTESIAN_POINT('Ctrl Pts',(133.032230127418,-36.5153587876941,21.92696120431));
#26041=CARTESIAN_POINT('Ctrl Pts',(133.00787023519,-36.5634597327342,21.9237171615184));
#26042=CARTESIAN_POINT('Ctrl Pts',(132.991171580083,-36.5951746129659,21.9215327926247));
#26043=CARTESIAN_POINT('Ctrl Pts',(132.902689659023,-36.7569477101237,21.910177445218));
#26044=CARTESIAN_POINT('Ctrl Pts',(132.822920521991,-36.8824413110184,21.9006575252438));
#26045=CARTESIAN_POINT('Ctrl Pts',(132.660089189368,-37.10487387355,21.8829012027134));
#26046=CARTESIAN_POINT('Ctrl Pts',(132.579277157378,-37.203156791653,21.8746901900265));
#26047=CARTESIAN_POINT('Ctrl Pts',(132.424599185356,-37.3710663485271,21.8601615846144));
#26048=CARTESIAN_POINT('Ctrl Pts',(132.35276543755,-37.4423624399458,21.8538059980752));
#26049=CARTESIAN_POINT('Ctrl Pts',(132.224571909779,-37.5586831918333,21.8431392994375));
#26050=CARTESIAN_POINT('Ctrl Pts',(132.169770335166,-37.6053172003812,21.8387701607497));
#26051=CARTESIAN_POINT('Ctrl Pts',(132.087177910723,-37.6711849288741,21.8324559468023));
#26052=CARTESIAN_POINT('Ctrl Pts',(132.060520357714,-37.691801726297,21.8304572525341));
#26053=CARTESIAN_POINT('Ctrl Pts',(132.012352182321,-37.7279197844041,21.8269139170658));
#26054=CARTESIAN_POINT('Ctrl Pts',(131.990959078749,-37.743572426924,21.8253635315419));
#26055=CARTESIAN_POINT('Ctrl Pts',(131.944960207124,-37.7764069097351,21.8220782134291));
#26056=CARTESIAN_POINT('Ctrl Pts',(131.920305332038,-37.7935162521357,21.8203460988291));
#26057=CARTESIAN_POINT('Ctrl Pts',(131.853100999014,-37.8388427298664,21.8156992605478));
#26058=CARTESIAN_POINT('Ctrl Pts',(131.81013515642,-37.8664302633139,21.8128076563953));
#26059=CARTESIAN_POINT('Ctrl Pts',(131.556047448402,-38.0215825434769,21.796128483962));
#26060=CARTESIAN_POINT('Ctrl Pts',(131.332133877025,-38.1267675299052,21.7831600961581));
#26061=CARTESIAN_POINT('Ctrl Pts',(130.984873325064,-38.2457550638413,21.7636703318022));
#26062=CARTESIAN_POINT('Ctrl Pts',(130.868981081366,-38.2786841910303,21.7572477596199));
#26063=CARTESIAN_POINT('Ctrl Pts',(130.686565101661,-38.320162695996,21.7469481127064));
#26064=CARTESIAN_POINT('Ctrl Pts',(130.62112184417,-38.3330254208299,21.7432153061226));
#26065=CARTESIAN_POINT('Ctrl Pts',(130.532829948524,-38.3476884982262,21.738078679639));
#26066=CARTESIAN_POINT('Ctrl Pts',(130.510276984202,-38.3512002885019,21.7367578531742));
#26067=CARTESIAN_POINT('Ctrl Pts',(130.472474772301,-38.3566961551044,21.7345267823099));
#26068=CARTESIAN_POINT('Ctrl Pts',(130.457243920226,-38.358804769317,21.7336232023414));
#26069=CARTESIAN_POINT('Ctrl Pts',(130.425633665275,-38.3629620146003,21.7317373686895));
#26070=CARTESIAN_POINT('Ctrl Pts',(130.409252914079,-38.3649947334059,21.730754358794));
#26071=CARTESIAN_POINT('Ctrl Pts',(130.364829497876,-38.3701781574071,21.7280741321064));
#26072=CARTESIAN_POINT('Ctrl Pts',(130.336761875379,-38.3730983830254,21.7263652211955));
#26073=CARTESIAN_POINT('Ctrl Pts',(130.169925087337,-38.3883534954738,21.7161282559049));
#26074=CARTESIAN_POINT('Ctrl Pts',(130.03054997845,-38.3924730763807,21.707257317377));
#26075=CARTESIAN_POINT('Ctrl Pts',(129.690938800354,-38.3815802011859,21.6854173459184));
#26076=CARTESIAN_POINT('Ctrl Pts',(129.491494345156,-38.3573854308202,21.6724217762087));
#26077=CARTESIAN_POINT('Ctrl Pts',(129.189017913185,-38.2931034686713,21.6530219697648));
#26078=CARTESIAN_POINT('Ctrl Pts',(129.083826055173,-38.2654022024886,21.6463283351088));
#26079=CARTESIAN_POINT('Ctrl Pts',(128.943019507733,-38.2209800141382,21.6374505728627));
#26080=CARTESIAN_POINT('Ctrl Pts',(128.906103917149,-38.2086307923856,21.6351305758812));
#26081=CARTESIAN_POINT('Ctrl Pts',(128.843686141581,-38.1865479364285,21.6312192195372));
#26082=CARTESIAN_POINT('Ctrl Pts',(128.818074539928,-38.1771373533466,21.6296175757162));
#26083=CARTESIAN_POINT('Ctrl Pts',(128.769531062382,-38.1586325591241,21.6265872255135));
#26084=CARTESIAN_POINT('Ctrl Pts',(128.746579498941,-38.1495952985207,21.625156771354));
#26085=CARTESIAN_POINT('Ctrl Pts',(128.692955588167,-38.1278016771449,21.6218190166652));
#26086=CARTESIAN_POINT('Ctrl Pts',(128.66236777198,-38.1148432638927,21.6199185044834));
#26087=CARTESIAN_POINT('Ctrl Pts',(128.553199733295,-38.066689891399,21.613142722471));
#26088=CARTESIAN_POINT('Ctrl Pts',(128.475773598282,-38.0289525256209,21.6083515493266));
#26089=CARTESIAN_POINT('Ctrl Pts',(128.158332900447,-37.8589738130607,21.5886247714017));
#26090=CARTESIAN_POINT('Ctrl Pts',(127.933388876429,-37.7008476361053,21.5745269229572));
#26091=CARTESIAN_POINT('Ctrl Pts',(127.680569480258,-37.4728658379607,21.556094613114));
#26092=CARTESIAN_POINT('Ctrl Pts',(127.632527933754,-37.4269113128627,21.5524513776684));
#26093=CARTESIAN_POINT('Ctrl Pts',(127.554209658539,-37.3474558258223,21.5462087867545));
#26094=CARTESIAN_POINT('Ctrl Pts',(127.523194235355,-37.3147077676494,21.5436508801519));
#26095=CARTESIAN_POINT('Ctrl Pts',(127.47954294819,-37.2667359445908,21.5399082327382));
#26096=CARTESIAN_POINT('Ctrl Pts',(127.466371359267,-37.2520038771194,21.5387594418239));
#26097=CARTESIAN_POINT('Ctrl Pts',(127.443466599012,-37.225930226349,21.5367254987961));
#26098=CARTESIAN_POINT('Ctrl Pts',(127.433678447333,-37.2146381372794,21.5358443163057));
#26099=CARTESIAN_POINT('Ctrl Pts',(127.412219409588,-37.1895486347702,21.5338853933744));
#26100=CARTESIAN_POINT('Ctrl Pts',(127.400584124366,-37.1757225653415,21.5328053569752));
#26101=CARTESIAN_POINT('Ctrl Pts',(127.366922352102,-37.1350672420323,21.5296296648581));
#26102=CARTESIAN_POINT('Ctrl Pts',(127.345197386002,-37.1079926251747,21.5275149789163));
#26103=CARTESIAN_POINT('Ctrl Pts',(127.209833924155,-36.9338847728349,21.5139424984479));
#26104=CARTESIAN_POINT('Ctrl Pts',(127.108039954802,-36.7780591445625,21.5019308223391));
#26105=CARTESIAN_POINT('Ctrl Pts',(126.94398907362,-36.4752471499145,21.479735322859));
#26106=CARTESIAN_POINT('Ctrl Pts',(126.878317469425,-36.3306624840133,21.4695661429436));
#26107=CARTESIAN_POINT('Ctrl Pts',(126.78954259032,-36.0920526132474,21.4536822123608));
#26108=CARTESIAN_POINT('Ctrl Pts',(126.75991016541,-36.000717862271,21.4477983459049));
#26109=CARTESIAN_POINT('Ctrl Pts',(126.724185279051,-35.8722601470201,21.439794623547));
#26110=CARTESIAN_POINT('Ctrl Pts',(126.71477369126,-35.8361148951158,21.4375715375384));
#26111=CARTESIAN_POINT('Ctrl Pts',(126.699588536887,-35.7735752404079,21.4337734125112));
#26112=CARTESIAN_POINT('Ctrl Pts',(126.693529755223,-35.7472543487111,21.4321895004332));
#26113=CARTESIAN_POINT('Ctrl Pts',(126.681751699707,-35.6931366803916,21.4289617190237));
#26114=CARTESIAN_POINT('Ctrl Pts',(126.676065601144,-35.6653348204779,21.4273190042138));
#26115=CARTESIAN_POINT('Ctrl Pts',(126.662364005628,-35.5937757870995,21.4231286326974));
#26116=CARTESIAN_POINT('Ctrl Pts',(126.654859375633,-35.549925611132,21.4205969821994));
#26117=CARTESIAN_POINT('Ctrl Pts',(126.622801563957,-35.3375467408126,21.4084916433636));
#26118=CARTESIAN_POINT('Ctrl Pts',(126.610107772386,-35.1674705458382,21.3992861357667));
#26119=CARTESIAN_POINT('Ctrl Pts',(126.610452580932,-34.758004344421,21.377469519136));
#26120=CARTESIAN_POINT('Ctrl Pts',(126.63595943991,-34.5195817834189,21.3650620872863));
#26121=CARTESIAN_POINT('Ctrl Pts',(126.695861222004,-34.2416344671744,21.3491545163103));
#26122=CARTESIAN_POINT('Ctrl Pts',(126.706275168305,-34.1976112711154,21.3465892521772));
#26123=CARTESIAN_POINT('Ctrl Pts',(126.722452827094,-34.1348567950213,21.3428498373894));
#26124=CARTESIAN_POINT('Ctrl Pts',(126.727503287372,-34.1159448761843,21.3417120500325));
#26125=CARTESIAN_POINT('Ctrl Pts',(126.73670109481,-34.0826619933657,21.3396887658171));
#26126=CARTESIAN_POINT('Ctrl Pts',(126.740780196718,-34.0682730948824,21.3388070536722));
#26127=CARTESIAN_POINT('Ctrl Pts',(126.74996678249,-34.0366663850937,21.3368544382099));
#26128=CARTESIAN_POINT('Ctrl Pts',(126.755115877096,-34.0194621038904,21.3357813445513));
#26129=CARTESIAN_POINT('Ctrl Pts',(126.770773309181,-33.968621374732,21.3325815004086));
#26130=CARTESIAN_POINT('Ctrl Pts',(126.781669436654,-33.9351079565262,21.3304347946027));
#26131=CARTESIAN_POINT('Ctrl Pts',(126.802146273574,-33.87531394158,21.3265447011104));
#26132=CARTESIAN_POINT('Ctrl Pts',(126.811532548339,-33.8489735142301,21.3248098602003));
#26133=CARTESIAN_POINT('Ctrl Pts',(126.821241906568,-33.8227565901911,21.3230638867798));
#26134=CARTESIAN_POINT('',(126.610250132114,-34.9990536039932,21.7310836956603));
#26135=CARTESIAN_POINT('Ctrl Pts',(126.821241920569,-33.8227565523843,21.6644320182169));
#26136=CARTESIAN_POINT('Ctrl Pts',(126.752438318367,-34.0085380123179,21.6750357805896));
#26137=CARTESIAN_POINT('Ctrl Pts',(126.700049022576,-34.2000063967079,21.6853623555409));
#26138=CARTESIAN_POINT('Ctrl Pts',(126.647643744624,-34.4888977139629,21.7012706745202));
#26139=CARTESIAN_POINT('Ctrl Pts',(126.634581709237,-34.5834969871236,21.7065349591291));
#26140=CARTESIAN_POINT('Ctrl Pts',(126.623044381903,-34.7045978728204,21.7134816678112));
#26141=CARTESIAN_POINT('Ctrl Pts',(126.62086188101,-34.7307099210969,21.7149917963618));
#26142=CARTESIAN_POINT('Ctrl Pts',(126.617829448334,-34.7728750299003,21.7174537985805));
#26143=CARTESIAN_POINT('Ctrl Pts',(126.616790572028,-34.7889139135047,21.7183957745052));
#26144=CARTESIAN_POINT('Ctrl Pts',(126.615063215451,-34.8188851141068,21.7201672184858));
#26145=CARTESIAN_POINT('Ctrl Pts',(126.614346600264,-34.8328154512365,21.7209951189075));
#26146=CARTESIAN_POINT('Ctrl Pts',(126.613006262979,-34.8624320673733,21.7227643873754));
#26147=CARTESIAN_POINT('Ctrl Pts',(126.612405494094,-34.878119100501,21.7237069409951));
#26148=CARTESIAN_POINT('Ctrl Pts',(126.610814475245,-34.9288816874263,21.7267733351668));
#26149=CARTESIAN_POINT('Ctrl Pts',(126.610259927971,-34.9639673342148,21.7289179407535));
#26150=CARTESIAN_POINT('Ctrl Pts',(126.610250132114,-34.9990536039932,21.7310836956603));
#26151=CARTESIAN_POINT('Ctrl Pts',(126.610250133167,-34.9990498377178,21.7310834631812));
#26152=CARTESIAN_POINT('Ctrl Pts',(126.610184089431,-35.2346640589123,21.7456271095323));
#26153=CARTESIAN_POINT('Ctrl Pts',(126.634683158631,-35.4696432505531,21.7610327902304));
#26154=CARTESIAN_POINT('Ctrl Pts',(126.718321766228,-35.8658252201045,21.7869870984347));
#26155=CARTESIAN_POINT('Ctrl Pts',(126.765653934861,-36.0286318897158,21.7976574643732));
#26156=CARTESIAN_POINT('Ctrl Pts',(126.84323383648,-36.2361045111181,21.8111301719299));
#26157=CARTESIAN_POINT('Ctrl Pts',(126.862633153511,-36.284545326814,21.8142680560725));
#26158=CARTESIAN_POINT('Ctrl Pts',(126.894920506843,-36.3600676098888,21.8191500380044));
#26159=CARTESIAN_POINT('Ctrl Pts',(126.907062139507,-36.3874574010428,21.8209184799051));
#26160=CARTESIAN_POINT('Ctrl Pts',(126.930631104539,-36.438778181232,21.8242290802648));
#26161=CARTESIAN_POINT('Ctrl Pts',(126.941979169833,-36.4627428797727,21.8257737592733));
#26162=CARTESIAN_POINT('Ctrl Pts',(126.9684206794,-36.5169287455225,21.8292647617316));
#26163=CARTESIAN_POINT('Ctrl Pts',(126.983687137532,-36.5470626454893,21.8312050042061));
#26164=CARTESIAN_POINT('Ctrl Pts',(127.033086036067,-36.6410573286293,21.8372577575565));
#26165=CARTESIAN_POINT('Ctrl Pts',(127.068816559942,-36.7040575944839,21.8413151773829));
#26166=CARTESIAN_POINT('Ctrl Pts',(127.259517253358,-37.0165298934346,21.86153893919));
#26167=CARTESIAN_POINT('Ctrl Pts',(127.444403973806,-37.2462318720692,21.876612247925));
#26168=CARTESIAN_POINT('Ctrl Pts',(127.705596352677,-37.4961412204957,21.8961677318682));
#26169=CARTESIAN_POINT('Ctrl Pts',(127.756017916026,-37.5415649840546,21.8998833870045));
#26170=CARTESIAN_POINT('Ctrl Pts',(127.842670409812,-37.6150388843688,21.9062366530857));
#26171=CARTESIAN_POINT('Ctrl Pts',(127.878169076405,-37.6439236826234,21.9088308794442));
#26172=CARTESIAN_POINT('Ctrl Pts',(127.929905028485,-37.6843075076711,21.9126172452596));
#26173=CARTESIAN_POINT('Ctrl Pts',(127.945677144192,-37.6963971423887,21.9137722667569));
#26174=CARTESIAN_POINT('Ctrl Pts',(127.973501542113,-37.7173392611635,21.9158129146997));
#26175=CARTESIAN_POINT('Ctrl Pts',(127.985507525298,-37.7262517708347,21.9166944735153));
#26176=CARTESIAN_POINT('Ctrl Pts',(128.012087314788,-37.7457115335876,21.9186488036377));
#26177=CARTESIAN_POINT('Ctrl Pts',(128.026686161449,-37.7562222574362,21.919723794173));
#26178=CARTESIAN_POINT('Ctrl Pts',(128.07025576623,-37.7870674627045,21.922935036427));
#26179=CARTESIAN_POINT('Ctrl Pts',(128.09946126998,-37.8070643334998,21.9250914465276));
#26180=CARTESIAN_POINT('Ctrl Pts',(128.277547850465,-37.9249461814373,21.9382382221361));
#26181=CARTESIAN_POINT('Ctrl Pts',(128.433634347324,-38.0114184188415,21.9497358629018));
#26182=CARTESIAN_POINT('Ctrl Pts',(128.744644839366,-38.1529732583397,21.9717619954101));
#26183=CARTESIAN_POINT('Ctrl Pts',(128.898230702646,-38.2098706163406,21.982264450798));
#26184=CARTESIAN_POINT('Ctrl Pts',(129.149140857578,-38.2826794501964,21.9985772580142));
#26185=CARTESIAN_POINT('Ctrl Pts',(129.244086022803,-38.3058346205192,22.0045691858803));
#26186=CARTESIAN_POINT('Ctrl Pts',(129.376758062242,-38.332174384776,22.0126906453767));
#26187=CARTESIAN_POINT('Ctrl Pts',(129.413729974842,-38.338877696407,22.0149275165718));
#26188=CARTESIAN_POINT('Ctrl Pts',(129.477495112424,-38.349346976491,22.0187416739526));
#26189=CARTESIAN_POINT('Ctrl Pts',(129.504235419351,-38.3534093204029,22.0203280312455));
#26190=CARTESIAN_POINT('Ctrl Pts',(129.559055753787,-38.3610674581038,22.0235543816657));
#26191=CARTESIAN_POINT('Ctrl Pts',(129.587137979988,-38.3646324181504,22.0251933020372));
#26192=CARTESIAN_POINT('Ctrl Pts',(129.659117206343,-38.3728552213844,22.0293606838535));
#26193=CARTESIAN_POINT('Ctrl Pts',(129.703067210523,-38.3770082313533,22.0318734930034));
#26194=CARTESIAN_POINT('Ctrl Pts',(129.905948185439,-38.3921876985808,22.0433434210747));
#26195=CARTESIAN_POINT('Ctrl Pts',(130.065457276097,-38.3928610287155,22.0519832784894));
#26196=CARTESIAN_POINT('Ctrl Pts',(130.421778521114,-38.3692170374748,22.0710499266387));
#26197=CARTESIAN_POINT('Ctrl Pts',(130.617585439835,-38.3388772972301,22.0813628826014));
#26198=CARTESIAN_POINT('Ctrl Pts',(130.893765739832,-38.2709473694263,22.0968450230371));
#26199=CARTESIAN_POINT('Ctrl Pts',(130.97708041638,-38.2470333255409,22.1016466470498));
#26200=CARTESIAN_POINT('Ctrl Pts',(131.082990115519,-38.2121885400554,22.1080256693629));
#26201=CARTESIAN_POINT('Ctrl Pts',(131.106512734401,-38.2041617154124,22.1094602958369));
#26202=CARTESIAN_POINT('Ctrl Pts',(131.144824577782,-38.1906160617389,22.1118293987248));
#26203=CARTESIAN_POINT('Ctrl Pts',(131.159667724175,-38.1852511545534,22.1127553058751));
#26204=CARTESIAN_POINT('Ctrl Pts',(131.189419802427,-38.1742620395046,22.1146284459386));
#26205=CARTESIAN_POINT('Ctrl Pts',(131.204327580887,-38.168635986816,22.1155757562416));
#26206=CARTESIAN_POINT('Ctrl Pts',(131.243044621624,-38.1537118546385,22.118057807387));
#26207=CARTESIAN_POINT('Ctrl Pts',(131.266788925926,-38.1442493738683,22.1196015817096));
#26208=CARTESIAN_POINT('Ctrl Pts',(131.370984535479,-38.1013539880753,22.1264645161839));
#26209=CARTESIAN_POINT('Ctrl Pts',(131.450231376754,-38.0650973466966,22.1319178141608));
#26210=CARTESIAN_POINT('Ctrl Pts',(131.723347585185,-37.9271788971476,22.1513397242616));
#26211=CARTESIAN_POINT('Ctrl Pts',(131.908696543025,-37.8098375472863,22.1656310211412));
#26212=CARTESIAN_POINT('Ctrl Pts',(132.155851447953,-37.6175554713786,22.1854998369281));
#26213=CARTESIAN_POINT('Ctrl Pts',(132.227814251974,-37.5565871750673,22.1914047018569));
#26214=CARTESIAN_POINT('Ctrl Pts',(132.347496579117,-37.4462937303417,22.2014131162497));
#26215=CARTESIAN_POINT('Ctrl Pts',(132.396431872003,-37.3983762203588,22.2055653630469));
#26216=CARTESIAN_POINT('Ctrl Pts',(132.466815181706,-37.3251500712227,22.2116312171359));
#26217=CARTESIAN_POINT('Ctrl Pts',(132.489395533275,-37.3009584937079,22.2135925654058));
#26218=CARTESIAN_POINT('Ctrl Pts',(132.529385012088,-37.256837698431,22.2170952399564));
#26219=CARTESIAN_POINT('Ctrl Pts',(132.546921646025,-37.2370281903119,22.2186418000029));
#26220=CARTESIAN_POINT('Ctrl Pts',(132.584114913181,-37.1940100310811,22.221945859541));
#26221=CARTESIAN_POINT('Ctrl Pts',(132.603694834624,-37.1707379380984,22.2237001723004));
#26222=CARTESIAN_POINT('Ctrl Pts',(132.656489993688,-37.1062449985358,22.2284746855898));
#26223=CARTESIAN_POINT('Ctrl Pts',(132.689057713821,-37.0645038422921,22.231469478068));
#26224=CARTESIAN_POINT('Ctrl Pts',(132.844899887195,-36.8548171161176,22.2460848468508));
#26225=CARTESIAN_POINT('Ctrl Pts',(132.95349031581,-36.6765163826288,22.2571554977244));
#26226=CARTESIAN_POINT('Ctrl Pts',(133.109050969757,-36.3584690494355,22.2759260114666));
#26227=CARTESIAN_POINT('Ctrl Pts',(133.164561654783,-36.2235934840538,22.2836297957879));
#26228=CARTESIAN_POINT('Ctrl Pts',(133.235043387952,-36.015102509684,22.2956898279514));
#26229=CARTESIAN_POINT('Ctrl Pts',(133.256538817358,-35.9438708586632,22.2998369770416));
#26230=CARTESIAN_POINT('Ctrl Pts',(133.281765082318,-35.8491077454208,22.3054573913496));
#26231=CARTESIAN_POINT('Ctrl Pts',(133.287617573049,-35.8261577601654,22.3068264433262));
#26232=CARTESIAN_POINT('Ctrl Pts',(133.296911331859,-35.7880496705314,22.3091155769322));
#26233=CARTESIAN_POINT('Ctrl Pts',(133.30048980961,-35.772925364493,22.3100282012526));
#26234=CARTESIAN_POINT('Ctrl Pts',(133.30714427166,-35.7439114195566,22.3117877077815));
#26235=CARTESIAN_POINT('Ctrl Pts',(133.310237046073,-35.7300261065887,22.3126335368375));
#26236=CARTESIAN_POINT('Ctrl Pts',(133.318496705012,-35.6918115979305,22.3149709715902));
#26237=CARTESIAN_POINT('Ctrl Pts',(133.32348325711,-35.6674448506925,22.31647203487));
#26238=CARTESIAN_POINT('Ctrl Pts',(133.343247215751,-35.5651497581732,22.3228119759294));
#26239=CARTESIAN_POINT('Ctrl Pts',(133.355554311687,-35.4867746852462,22.3277616891127));
#26240=CARTESIAN_POINT('Ctrl Pts',(133.389576254935,-35.2062005783271,22.3456483341834));
#26241=CARTESIAN_POINT('Ctrl Pts',(133.395841705234,-35.0025635363479,22.3589089253334));
#26242=CARTESIAN_POINT('Ctrl Pts',(133.377406421914,-34.6912917783067,22.3788084560034));
#26243=CARTESIAN_POINT('Ctrl Pts',(133.365796517691,-34.5833564213881,22.3856462795732));
#26244=CARTESIAN_POINT('Ctrl Pts',(133.337363583791,-34.4015794389906,22.3970067562618));
#26245=CARTESIAN_POINT('Ctrl Pts',(133.323210122675,-34.3274089813116,22.4015983082196));
#26246=CARTESIAN_POINT('Ctrl Pts',(133.299040697024,-34.2203130049996,22.4081654582626));
#26247=CARTESIAN_POINT('Ctrl Pts',(133.290982980952,-34.1869732602412,22.4102010227236));
#26248=CARTESIAN_POINT('Ctrl Pts',(133.27578758345,-34.1280328666723,22.4137851487468));
#26249=CARTESIAN_POINT('Ctrl Pts',(133.268852340374,-34.102383483895,22.415339959633));
#26250=CARTESIAN_POINT('Ctrl Pts',(133.253539150372,-34.0482817653181,22.4186100854218));
#26251=CARTESIAN_POINT('Ctrl Pts',(133.245087880979,-34.0198523954727,22.4203229126016));
#26252=CARTESIAN_POINT('Ctrl Pts',(133.22118078816,-33.9431320120994,22.4249324364401));
#26253=CARTESIAN_POINT('Ctrl Pts',(133.205012576533,-33.8950699691313,22.4278061878758));
#26254=CARTESIAN_POINT('Ctrl Pts',(133.101021658256,-33.6074632293198,22.4449529549382));
#26255=CARTESIAN_POINT('Ctrl Pts',(132.987465500873,-33.3781014703135,22.4583370456428));
#26256=CARTESIAN_POINT('Ctrl Pts',(132.786568812553,-33.0663962690906,22.4780405459557));
#26257=CARTESIAN_POINT('Ctrl Pts',(132.718961467793,-32.9724313426805,22.484223325471));
#26258=CARTESIAN_POINT('Ctrl Pts',(132.606013255887,-32.8312819245049,22.4941866409162));
#26259=CARTESIAN_POINT('Ctrl Pts',(132.56388549353,-32.7816372559472,22.4978339253717));
#26260=CARTESIAN_POINT('Ctrl Pts',(132.505221491868,-32.7164101360827,22.5028702813325));
#26261=CARTESIAN_POINT('Ctrl Pts',(132.48991772378,-32.6997332634724,22.504180435362));
#26262=CARTESIAN_POINT('Ctrl Pts',(132.463963288543,-32.6720126012728,22.5063987698874));
#26263=CARTESIAN_POINT('Ctrl Pts',(132.453402267455,-32.6608852693096,22.5073004588663));
#26264=CARTESIAN_POINT('Ctrl Pts',(132.43127524936,-32.6378864522204,22.5091885071081));
#26265=CARTESIAN_POINT('Ctrl Pts',(132.419697236351,-32.6260275886735,22.5101756963591));
#26266=CARTESIAN_POINT('Ctrl Pts',(132.387951484392,-32.593985271296,22.5128792674677));
#26267=CARTESIAN_POINT('Ctrl Pts',(132.367615562871,-32.573971229243,22.5146076738232));
#26268=CARTESIAN_POINT('Ctrl Pts',(132.228191839359,-32.440176985522,22.5264194278298));
#26269=CARTESIAN_POINT('Ctrl Pts',(132.101210164485,-32.3349598785437,22.5369806949257));
#26270=CARTESIAN_POINT('Ctrl Pts',(131.857699811985,-32.1614437715059,22.5562448387764));
#26271=CARTESIAN_POINT('Ctrl Pts',(131.743758974418,-32.0900588672015,22.564916675378));
#26272=CARTESIAN_POINT('Ctrl Pts',(131.501385953946,-31.9575708947373,22.5824483428808));
#26273=CARTESIAN_POINT('Ctrl Pts',(131.372732145685,-31.8973963736867,22.5912730949246));
#26274=CARTESIAN_POINT('Ctrl Pts',(131.20151557434,-31.8300574594483,22.6023697703212));
#26275=CARTESIAN_POINT('Ctrl Pts',(131.162075298258,-31.8153875234316,22.6048838840267));
#26276=CARTESIAN_POINT('Ctrl Pts',(131.096054612181,-31.7922208365859,22.6090246050085));
#26277=CARTESIAN_POINT('Ctrl Pts',(131.069624960091,-31.7833114250413,22.6106644701131));
#26278=CARTESIAN_POINT('Ctrl Pts',(131.017394951661,-31.7664196716079,22.6138713167247));
#26279=CARTESIAN_POINT('Ctrl Pts',(130.991603251331,-31.7584174726705,22.6154388399871));
#26280=CARTESIAN_POINT('Ctrl Pts',(130.934363486134,-31.7414052271095,22.6188836228549));
#26281=CARTESIAN_POINT('Ctrl Pts',(130.902874869762,-31.7325404221423,22.6207561490613));
#26282=CARTESIAN_POINT('Ctrl Pts',(130.792298283057,-31.7031310555451,22.6272580668999));
#26283=CARTESIAN_POINT('Ctrl Pts',(130.712597352665,-31.6849905237577,22.6318127169709));
#26284=CARTESIAN_POINT('Ctrl Pts',(130.402046100968,-31.626026246427,22.6491671950613));
#26285=CARTESIAN_POINT('Ctrl Pts',(130.16787032721,-31.6063056199236,22.6613775133596));
#26286=CARTESIAN_POINT('Ctrl Pts',(129.794148306511,-31.6136354855097,22.6813427723163));
#26287=CARTESIAN_POINT('Ctrl Pts',(129.655082326422,-31.6249646710824,22.6888930026413));
#26288=CARTESIAN_POINT('Ctrl Pts',(129.489518815417,-31.6487924752175,22.6984232724398));
#26289=CARTESIAN_POINT('Ctrl Pts',(129.461964281328,-31.6531058617174,22.7000277088801));
#26290=CARTESIAN_POINT('Ctrl Pts',(129.418261448175,-31.6605007170222,22.7026060143201));
#26291=CARTESIAN_POINT('Ctrl Pts',(129.402076358949,-31.6633605980633,22.7035682313963));
#26292=CARTESIAN_POINT('Ctrl Pts',(129.370930258535,-31.6690979562435,22.7054351844467));
#26293=CARTESIAN_POINT('Ctrl Pts',(129.355966803847,-31.6719587781506,22.7063390254833));
#26294=CARTESIAN_POINT('Ctrl Pts',(129.318578828497,-31.6793684630758,22.7086138914072));
#26295=CARTESIAN_POINT('Ctrl Pts',(129.296180327208,-31.6840436639568,22.7099916068013));
#26296=CARTESIAN_POINT('Ctrl Pts',(129.213281287075,-31.7022247781861,22.7151416750835));
#26297=CARTESIAN_POINT('Ctrl Pts',(129.153110397447,-31.7171620856801,22.7189807864738));
#26298=CARTESIAN_POINT('Ctrl Pts',(128.88137091605,-31.79258857924,22.7366818667814));
#26299=CARTESIAN_POINT('Ctrl Pts',(128.675592610951,-31.8719392858899,22.7510597656125));
#26300=CARTESIAN_POINT('Ctrl Pts',(128.379428962843,-32.0206447529596,22.7722301399837));
#26301=CARTESIAN_POINT('Ctrl Pts',(128.282418347726,-32.075495799312,22.7792577344384));
#26302=CARTESIAN_POINT('Ctrl Pts',(128.123337052652,-32.1760940192633,22.7908883247868));
#26303=CARTESIAN_POINT('Ctrl Pts',(128.059807978172,-32.2193588625678,22.7955647500366));
#26304=CARTESIAN_POINT('Ctrl Pts',(127.96994591637,-32.2851377427901,22.8022279586107));
#26305=CARTESIAN_POINT('Ctrl Pts',(127.942403843196,-32.3059519592587,22.8042772157689));
#26306=CARTESIAN_POINT('Ctrl Pts',(127.894213799616,-32.3435405479725,22.8078766282606));
#26307=CARTESIAN_POINT('Ctrl Pts',(127.873436663713,-32.3601437958476,22.809433221016));
#26308=CARTESIAN_POINT('Ctrl Pts',(127.830000691357,-32.3956996143193,22.8126984237339));
#26309=CARTESIAN_POINT('Ctrl Pts',(127.807389772795,-32.4147073725196,22.8144046613531));
#26310=CARTESIAN_POINT('Ctrl Pts',(127.74709185758,-32.4667566890721,22.8189748495515));
#26311=CARTESIAN_POINT('Ctrl Pts',(127.709883722034,-32.5003431101859,22.8218165475283));
#26312=CARTESIAN_POINT('Ctrl Pts',(127.484500773233,-32.713046583648,22.839199802642));
#26313=CARTESIAN_POINT('Ctrl Pts',(127.316692922024,-32.9124736538238,22.852811895961));
#26314=CARTESIAN_POINT('Ctrl Pts',(127.110821566848,-33.2235236397755,22.8726396482673));
#26315=CARTESIAN_POINT('Ctrl Pts',(127.053113162414,-33.3209897680172,22.8786957461462));
#26316=CARTESIAN_POINT('Ctrl Pts',(126.970468588516,-33.4780039889782,22.8884804441466));
#26317=CARTESIAN_POINT('Ctrl Pts',(126.942169452699,-33.535690019088,22.8920814618493));
#26318=CARTESIAN_POINT('Ctrl Pts',(126.906184193166,-33.6146421368958,22.8970635057497));
#26319=CARTESIAN_POINT('Ctrl Pts',(126.897045104032,-33.6352349981405,22.8983677763938));
#26320=CARTESIAN_POINT('Ctrl Pts',(126.88203673246,-33.6699831214862,22.9005791083759));
#26321=CARTESIAN_POINT('Ctrl Pts',(126.876056756953,-33.6840902604301,22.9014797731322));
#26322=CARTESIAN_POINT('Ctrl Pts',(126.863793172486,-33.7135755935075,22.9033691318452));
#26323=CARTESIAN_POINT('Ctrl Pts',(126.857526693039,-33.7289600682777,22.9043586973535));
#26324=CARTESIAN_POINT('Ctrl Pts',(126.841006257433,-33.7703874720365,22.9070322637399));
#26325=CARTESIAN_POINT('Ctrl Pts',(126.83096158199,-33.7965118086049,22.9087275643847));
#26326=CARTESIAN_POINT('Ctrl Pts',(126.821241915871,-33.8227565650702,22.910437866903));
#26327=CARTESIAN_POINT('Origin',(130.,-35.,23.));
#26328=CARTESIAN_POINT('',(126.821241975209,-33.8227564048483,24.1659080048185));
#26329=CARTESIAN_POINT('',(126.821241884814,-33.8227566489294,23.8178897147876));
#26330=CARTESIAN_POINT('',(126.821241915871,-33.8227565650715,23.));
#26331=CARTESIAN_POINT('',(126.610250686307,-35.0021570388984,22.6387449561209));
#26332=CARTESIAN_POINT('Ctrl Pts',(126.821241884814,-33.8227566489294,23.8178897147877));
#26333=CARTESIAN_POINT('Ctrl Pts',(126.830547911808,-33.7976287866224,23.8162401981369));
#26334=CARTESIAN_POINT('Ctrl Pts',(126.840153848162,-33.772605981515,23.8145990229724));
#26335=CARTESIAN_POINT('Ctrl Pts',(126.869647419057,-33.6984204307351,23.8097378524965));
#26336=CARTESIAN_POINT('Ctrl Pts',(126.890390936526,-33.6496116843828,23.8065455595275));
#26337=CARTESIAN_POINT('Ctrl Pts',(126.924828262693,-33.573588468545,23.8015808094579));
#26338=CARTESIAN_POINT('Ctrl Pts',(126.937757555136,-33.5460390753756,23.7997832184751));
#26339=CARTESIAN_POINT('Ctrl Pts',(126.962616483277,-33.4948733609272,23.7964465035576));
#26340=CARTESIAN_POINT('Ctrl Pts',(126.974454927409,-33.4712155483715,23.7949044286691));
#26341=CARTESIAN_POINT('Ctrl Pts',(127.001709970506,-33.4183062597122,23.7914561874206));
#26342=CARTESIAN_POINT('Ctrl Pts',(127.01728016263,-33.3891366690291,23.7895554972374));
#26343=CARTESIAN_POINT('Ctrl Pts',(127.066323880393,-33.3004068760858,23.7837710257596));
#26344=CARTESIAN_POINT('Ctrl Pts',(127.101174120129,-33.2416252539697,23.779935312226));
#26345=CARTESIAN_POINT('Ctrl Pts',(127.272238238132,-32.9720186516412,23.7622517386775));
#26346=CARTESIAN_POINT('Ctrl Pts',(127.429811750342,-32.7756957429772,23.7491758103101));
#26347=CARTESIAN_POINT('Ctrl Pts',(127.709944854719,-32.4966192310434,23.7280812087678));
#26348=CARTESIAN_POINT('Ctrl Pts',(127.818672898893,-32.4013327739757,23.7202756841766));
#26349=CARTESIAN_POINT('Ctrl Pts',(127.955551913448,-32.2960330648351,23.71044126171));
#26350=CARTESIAN_POINT('Ctrl Pts',(127.978185726328,-32.2790677889654,23.708814703716));
#26351=CARTESIAN_POINT('Ctrl Pts',(128.014370942396,-32.2526457729037,23.7062091070921));
#26352=CARTESIAN_POINT('Ctrl Pts',(128.027784226679,-32.2430011022744,23.7052421480911));
#26353=CARTESIAN_POINT('Ctrl Pts',(128.053810504954,-32.2245743181905,23.7033626815613));
#26354=CARTESIAN_POINT('Ctrl Pts',(128.066413574875,-32.2157793248051,23.7024510298915));
#26355=CARTESIAN_POINT('Ctrl Pts',(128.097847635245,-32.194159568455,23.7001742193603));
#26356=CARTESIAN_POINT('Ctrl Pts',(128.116748788784,-32.1814384946211,23.6988025668957));
#26357=CARTESIAN_POINT('Ctrl Pts',(128.191179995932,-32.1324268431552,23.6933954198613));
#26358=CARTESIAN_POINT('Ctrl Pts',(128.247639251099,-32.0975809670038,23.6892818135176));
#26359=CARTESIAN_POINT('Ctrl Pts',(128.408439617249,-32.0047395670314,23.6776073996966));
#26360=CARTESIAN_POINT('Ctrl Pts',(128.514874052137,-31.9505659714966,23.6699297714933));
#26361=CARTESIAN_POINT('Ctrl Pts',(128.851013931739,-31.8012543832227,23.646223659805));
#26362=CARTESIAN_POINT('Ctrl Pts',(129.088528188507,-31.7256453661697,23.630283015533));
#26363=CARTESIAN_POINT('Ctrl Pts',(129.382064835819,-31.6666611377677,23.6120818757022));
#26364=CARTESIAN_POINT('Ctrl Pts',(129.432149513526,-31.6577645082902,23.609023733643));
#26365=CARTESIAN_POINT('Ctrl Pts',(129.512032838721,-31.645422364358,23.6042191544235));
#26366=CARTESIAN_POINT('Ctrl Pts',(129.541708179297,-31.6412395504485,23.6024501949986));
#26367=CARTESIAN_POINT('Ctrl Pts',(129.597735958085,-31.6340986888464,23.5991391497192));
#26368=CARTESIAN_POINT('Ctrl Pts',(129.624075048423,-31.6310552860772,23.5975945354879));
#26369=CARTESIAN_POINT('Ctrl Pts',(129.684031498166,-31.6248394167985,23.5941043790031));
#26370=CARTESIAN_POINT('Ctrl Pts',(129.717666261645,-31.6218595597769,23.5921649060012));
#26371=CARTESIAN_POINT('Ctrl Pts',(129.823470678403,-31.614077182643,23.5861174438135));
#26372=CARTESIAN_POINT('Ctrl Pts',(129.895754954031,-31.6110813062142,23.5820644024377));
#26373=CARTESIAN_POINT('Ctrl Pts',(130.070020760732,-31.6094404171182,23.5724360378762));
#26374=CARTESIAN_POINT('Ctrl Pts',(130.171953638521,-31.6130794192745,23.5669228717045));
#26375=CARTESIAN_POINT('Ctrl Pts',(130.321071319966,-31.6251534497163,23.5589195841914));
#26376=CARTESIAN_POINT('Ctrl Pts',(130.368484631765,-31.6300007121009,23.5563837374015));
#26377=CARTESIAN_POINT('Ctrl Pts',(130.622554238047,-31.6614015264397,23.5427907337562));
#26378=CARTESIAN_POINT('Ctrl Pts',(130.826512211952,-31.7059636903256,23.5318866740389));
#26379=CARTESIAN_POINT('Ctrl Pts',(131.069853690381,-31.7831652559476,23.5176394498414));
#26380=CARTESIAN_POINT('Ctrl Pts',(131.114336748879,-31.7983026606069,23.5149811738008));
#26381=CARTESIAN_POINT('Ctrl Pts',(131.176068908901,-31.8207521442701,23.5111978460947));
#26382=CARTESIAN_POINT('Ctrl Pts',(131.193595648791,-31.827290684641,23.5101129280441));
#26383=CARTESIAN_POINT('Ctrl Pts',(131.225193703566,-31.8393775585697,23.5081359280701));
#26384=CARTESIAN_POINT('Ctrl Pts',(131.2392839456,-31.8448757354378,23.5072466869939));
#26385=CARTESIAN_POINT('Ctrl Pts',(131.268814488704,-31.85662723395,23.5053660668784));
#26386=CARTESIAN_POINT('Ctrl Pts',(131.284246079543,-31.8629002989227,23.5043736330825));
#26387=CARTESIAN_POINT('Ctrl Pts',(131.326347231351,-31.8803774465944,23.5016406775824));
#26388=CARTESIAN_POINT('Ctrl Pts',(131.352920002706,-31.891809336757,23.4998877101594));
#26389=CARTESIAN_POINT('Ctrl Pts',(131.547656144271,-31.9785571740614,23.4868507326663));
#26390=CARTESIAN_POINT('Ctrl Pts',(131.709562378444,-32.0671274624447,23.4749736608001));
#26391=CARTESIAN_POINT('Ctrl Pts',(132.060360576384,-32.2979854492503,23.4479034754087));
#26392=CARTESIAN_POINT('Ctrl Pts',(132.243241443606,-32.4477720307668,23.4328169775543));
#26393=CARTESIAN_POINT('Ctrl Pts',(132.445692207619,-32.6522993780657,23.4153071852525));
#26394=CARTESIAN_POINT('Ctrl Pts',(132.481416759889,-32.6900909333667,23.4121787034557));
#26395=CARTESIAN_POINT('Ctrl Pts',(132.536501879554,-32.7511167322913,23.4072900800265));
#26396=CARTESIAN_POINT('Ctrl Pts',(132.556444254683,-32.7738125420433,23.4055060611986));
#26397=CARTESIAN_POINT('Ctrl Pts',(132.591569510411,-32.8148820662251,23.4023370114084));
#26398=CARTESIAN_POINT('Ctrl Pts',(132.606866858328,-32.8331547961255,23.400947396156));
#26399=CARTESIAN_POINT('Ctrl Pts',(132.642304240279,-32.8764033710224,23.3977048811682));
#26400=CARTESIAN_POINT('Ctrl Pts',(132.662285086708,-32.9015070743428,23.3958583601764));
#26401=CARTESIAN_POINT('Ctrl Pts',(132.720419446321,-32.9767134287119,23.3904273342128));
#26402=CARTESIAN_POINT('Ctrl Pts',(132.75753757047,-33.0276010159845,23.3868823979259));
#26403=CARTESIAN_POINT('Ctrl Pts',(132.881115753394,-33.2073354686621,23.374760947598));
#26404=CARTESIAN_POINT('Ctrl Pts',(132.960137982987,-33.3410657717112,23.3664375811743));
#26405=CARTESIAN_POINT('Ctrl Pts',(133.11643160582,-33.6525444661945,23.3479161257107));
#26406=CARTESIAN_POINT('Ctrl Pts',(133.188190100291,-33.832431516262,23.3377982930934));
#26407=CARTESIAN_POINT('Ctrl Pts',(133.263078529485,-34.0796982057225,23.3235692996567));
#26408=CARTESIAN_POINT('Ctrl Pts',(133.280137473007,-34.1424838427764,23.3199279111274));
#26409=CARTESIAN_POINT('Ctrl Pts',(133.300835350781,-34.2283567038766,23.3148621135368));
#26410=CARTESIAN_POINT('Ctrl Pts',(133.306058540883,-34.2510512372541,23.3135153055207));
#26411=CARTESIAN_POINT('Ctrl Pts',(133.314032361246,-34.2874070501608,23.3113423995842));
#26412=CARTESIAN_POINT('Ctrl Pts',(133.316933395637,-34.3010350235389,23.3105244510493));
#26413=CARTESIAN_POINT('Ctrl Pts',(133.322963780649,-34.330246748709,23.3087630818801));
#26414=CARTESIAN_POINT('Ctrl Pts',(133.326067685264,-34.3458353146965,23.3078182419956));
#26415=CARTESIAN_POINT('Ctrl Pts',(133.333842216942,-34.386367277142,23.3053498720477));
#26416=CARTESIAN_POINT('Ctrl Pts',(133.338342488312,-34.4113418708958,23.3038174829395));
#26417=CARTESIAN_POINT('Ctrl Pts',(133.358026144364,-34.5280729063963,23.296609143737));
#26418=CARTESIAN_POINT('Ctrl Pts',(133.369708432472,-34.6203725044751,23.2907782567168));
#26419=CARTESIAN_POINT('Ctrl Pts',(133.397431156424,-34.9466605214832,23.2699568352102));
#26420=CARTESIAN_POINT('Ctrl Pts',(133.392988439629,-35.1817277983134,23.2546334935683));
#26421=CARTESIAN_POINT('Ctrl Pts',(133.349461587637,-35.5350428979376,23.2321773893474));
#26422=CARTESIAN_POINT('Ctrl Pts',(133.328135175159,-35.6547406614057,23.2246606915477));
#26423=CARTESIAN_POINT('Ctrl Pts',(133.291035715214,-35.8131322441544,23.2148573409886));
#26424=CARTESIAN_POINT('Ctrl Pts',(133.280916644145,-35.8530453232092,23.2123989176489));
#26425=CARTESIAN_POINT('Ctrl Pts',(133.263503255684,-35.9168280787533,23.208487940403));
#26426=CARTESIAN_POINT('Ctrl Pts',(133.256668392898,-35.940817864531,23.2070210011448));
#26427=CARTESIAN_POINT('Ctrl Pts',(133.241875138925,-35.9906470159029,23.2039817436943));
#26428=CARTESIAN_POINT('Ctrl Pts',(133.233871138667,-36.0164710753585,23.2024110098273));
#26429=CARTESIAN_POINT('Ctrl Pts',(133.214027460683,-36.0778864706726,23.1986845092971));
#26430=CARTESIAN_POINT('Ctrl Pts',(133.201904200699,-36.1133828675132,23.1965380448515));
#26431=CARTESIAN_POINT('Ctrl Pts',(133.156263131924,-36.2401015902052,23.1888946129706));
#26432=CARTESIAN_POINT('Ctrl Pts',(133.119414173454,-36.3300775879569,23.1835052320613));
#26433=CARTESIAN_POINT('Ctrl Pts',(133.010920902795,-36.5655786732497,23.1693643398103));
#26434=CARTESIAN_POINT('Ctrl Pts',(132.932619025583,-36.7077558594452,23.160797815657));
#26435=CARTESIAN_POINT('Ctrl Pts',(132.746190528454,-36.9953624870278,23.1426212160717));
#26436=CARTESIAN_POINT('Ctrl Pts',(132.635989208321,-37.1388270564738,23.1330308783856));
#26437=CARTESIAN_POINT('Ctrl Pts',(132.491583098022,-37.2986143742496,23.1208643112932));
#26438=CARTESIAN_POINT('Ctrl Pts',(132.4678717687,-37.3240531648718,23.1188775247553));
#26439=CARTESIAN_POINT('Ctrl Pts',(132.431242187615,-37.3621586535904,23.1158165038008));
#26440=CARTESIAN_POINT('Ctrl Pts',(132.418606292562,-37.3750948716228,23.1147619946361));
#26441=CARTESIAN_POINT('Ctrl Pts',(132.395340799283,-37.3985351414718,23.1128216177442));
#26442=CARTESIAN_POINT('Ctrl Pts',(132.384744390141,-37.4090708866835,23.1119382005952));
#26443=CARTESIAN_POINT('Ctrl Pts',(132.359985474236,-37.4333646391614,23.1098749922807));
#26444=CARTESIAN_POINT('Ctrl Pts',(132.345772098309,-37.4470692934874,23.1086913862744));
#26445=CARTESIAN_POINT('Ctrl Pts',(132.298775093558,-37.4915984898068,23.1047828808652));
#26446=CARTESIAN_POINT('Ctrl Pts',(132.265498565563,-37.5218932969624,23.1020235296191));
#26447=CARTESIAN_POINT('Ctrl Pts',(132.181758654428,-37.5951347013873,23.095120398463));
#26448=CARTESIAN_POINT('Ctrl Pts',(132.130620880852,-37.6372805544383,23.0909401093218));
#26449=CARTESIAN_POINT('Ctrl Pts',(131.864087685929,-37.8441336498446,23.069453858277));
#26450=CARTESIAN_POINT('Ctrl Pts',(131.630684552988,-37.9840940142984,23.0517111109592));
#26451=CARTESIAN_POINT('Ctrl Pts',(131.302187293109,-38.1309051340909,23.0293243240089));
#26452=CARTESIAN_POINT('Ctrl Pts',(131.219887275039,-38.1638798759714,23.0239010450524));
#26453=CARTESIAN_POINT('Ctrl Pts',(131.101390762603,-38.2060447563607,23.0163527060142));
#26454=CARTESIAN_POINT('Ctrl Pts',(131.066194793751,-38.2179206668567,23.0141422165452));
#26455=CARTESIAN_POINT('Ctrl Pts',(131.005113457647,-38.2374186595166,23.0103587117697));
#26456=CARTESIAN_POINT('Ctrl Pts',(130.979319730512,-38.2453144019889,23.0087770036859));
#26457=CARTESIAN_POINT('Ctrl Pts',(130.926140346136,-38.2609014181675,23.0055477475181));
#26458=CARTESIAN_POINT('Ctrl Pts',(130.89874657401,-38.2685575820333,23.0039014302249));
#26459=CARTESIAN_POINT('Ctrl Pts',(130.827959044338,-38.2873844311032,22.9996893054904));
#26460=CARTESIAN_POINT('Ctrl Pts',(130.784433627119,-38.2980413468147,22.9971398414552));
#26461=CARTESIAN_POINT('Ctrl Pts',(130.552377577873,-38.3500046256461,22.9837410651453));
#26462=CARTESIAN_POINT('Ctrl Pts',(130.36078205061,-38.3760182465848,22.9733791174867));
#26463=CARTESIAN_POINT('Ctrl Pts',(129.965421590042,-38.3956364624001,22.9523541217555));
#26464=CARTESIAN_POINT('Ctrl Pts',(129.762370688194,-38.3874859997452,22.9417399257189));
#26465=CARTESIAN_POINT('Ctrl Pts',(129.508132125618,-38.3543023849092,22.9275033880633));
#26466=CARTESIAN_POINT('Ctrl Pts',(129.455153527463,-38.3461052247901,22.9244825521568));
#26467=CARTESIAN_POINT('Ctrl Pts',(129.381102230195,-38.3328424087904,22.9201564105175));
#26468=CARTESIAN_POINT('Ctrl Pts',(129.359847429409,-38.3288252590359,22.9189025926186));
#26469=CARTESIAN_POINT('Ctrl Pts',(129.323754363032,-38.3216452308235,22.916750648339));
#26470=CARTESIAN_POINT('Ctrl Pts',(129.308895902455,-38.3185855905414,22.9158581143804));
#26471=CARTESIAN_POINT('Ctrl Pts',(129.277451050542,-38.3118901530993,22.9139544251808));
#26472=CARTESIAN_POINT('Ctrl Pts',(129.260870901783,-38.3082293632031,22.912942011824));
#26473=CARTESIAN_POINT('Ctrl Pts',(129.214640505371,-38.2976571116272,22.9100962666));
#26474=CARTESIAN_POINT('Ctrl Pts',(129.185055544493,-38.2904706891914,22.9082488171383));
#26475=CARTESIAN_POINT('Ctrl Pts',(128.983414280014,-38.2386043229692,22.8954950754344));
#26476=CARTESIAN_POINT('Ctrl Pts',(128.815020202468,-38.1808515946106,22.8840477355071));
#26477=CARTESIAN_POINT('Ctrl Pts',(128.431649475386,-38.0146856757006,22.8571141772499));
#26478=CARTESIAN_POINT('Ctrl Pts',(128.222087469648,-37.896051324041,22.8417341823877));
#26479=CARTESIAN_POINT('Ctrl Pts',(127.984789883333,-37.7261700232894,22.8239819014037));
#26480=CARTESIAN_POINT('Ctrl Pts',(127.943468278206,-37.6951349737892,22.8208736145039));
#26481=CARTESIAN_POINT('Ctrl Pts',(127.879190504197,-37.6445189738938,22.8160091072229));
#26482=CARTESIAN_POINT('Ctrl Pts',(127.855759641064,-37.6255564918252,22.8142294019036));
#26483=CARTESIAN_POINT('Ctrl Pts',(127.814256013385,-37.5910415913594,22.8110642528796));
#26484=CARTESIAN_POINT('Ctrl Pts',(127.79608875507,-37.5756064471289,22.8096742873531));
#26485=CARTESIAN_POINT('Ctrl Pts',(127.753786027696,-37.5388901366872,22.8064261919594));
#26486=CARTESIAN_POINT('Ctrl Pts',(127.729787526294,-37.5174542223757,22.8045745168159));
#26487=CARTESIAN_POINT('Ctrl Pts',(127.659368595675,-37.4527286879265,22.7991104899942));
#26488=CARTESIAN_POINT('Ctrl Pts',(127.61385359762,-37.4084724288458,22.7955384650104));
#26489=CARTESIAN_POINT('Ctrl Pts',(127.45639460684,-37.2465200337467,22.7829898299827));
#26490=CARTESIAN_POINT('Ctrl Pts',(127.351691651454,-37.122086135163,22.7742953230129));
#26491=CARTESIAN_POINT('Ctrl Pts',(127.134824245472,-36.8231754321495,22.7546852202155));
#26492=CARTESIAN_POINT('Ctrl Pts',(127.028934115131,-36.6449781200022,22.7438586818861));
#26493=CARTESIAN_POINT('Ctrl Pts',(126.919040066319,-36.4143742294821,22.7296222409634));
#26494=CARTESIAN_POINT('Ctrl Pts',(126.899073250631,-36.3700442982055,22.7268747045796));
#26495=CARTESIAN_POINT('Ctrl Pts',(126.872653691574,-36.3078492724187,22.7229847289986));
#26496=CARTESIAN_POINT('Ctrl Pts',(126.865386487054,-36.2903343525093,22.7218854437274));
#26497=CARTESIAN_POINT('Ctrl Pts',(126.852564786459,-36.2586847341258,22.7198905983247));
#26498=CARTESIAN_POINT('Ctrl Pts',(126.846957496691,-36.2445716729039,22.7189980600518));
#26499=CARTESIAN_POINT('Ctrl Pts',(126.835445788105,-36.2150205281709,22.7171220809651));
#26500=CARTESIAN_POINT('Ctrl Pts',(126.829559191831,-36.1995763004391,22.71613772376));
#26501=CARTESIAN_POINT('Ctrl Pts',(126.813893304726,-36.1575539784773,22.7134499742199));
#26502=CARTESIAN_POINT('Ctrl Pts',(126.804333979025,-36.1308959523763,22.7117347816865));
#26503=CARTESIAN_POINT('Ctrl Pts',(126.744820610243,-35.9581489655936,22.7005690518424));
#26504=CARTESIAN_POINT('Ctrl Pts',(126.704567254605,-35.8089231302589,22.6906971957163));
#26505=CARTESIAN_POINT('Ctrl Pts',(126.63195401171,-35.4416684464721,22.6665957114359));
#26506=CARTESIAN_POINT('Ctrl Pts',(126.61039070071,-35.2221872513799,22.6523831461664));
#26507=CARTESIAN_POINT('Ctrl Pts',(126.610250686307,-35.0021570388984,22.6387449561209));
#26508=CARTESIAN_POINT('Ctrl Pts',(126.610250683868,-35.0021532034418,22.6387447183869));
#26509=CARTESIAN_POINT('Ctrl Pts',(126.610218691316,-34.9517879050375,22.6356229144437));
#26510=CARTESIAN_POINT('Ctrl Pts',(126.61130919799,-34.901425866968,22.6325306774218));
#26511=CARTESIAN_POINT('Ctrl Pts',(126.615250248782,-34.8117907148621,22.6270802631384));
#26512=CARTESIAN_POINT('Ctrl Pts',(126.617663286356,-34.7725089830984,22.624709880538));
#26513=CARTESIAN_POINT('Ctrl Pts',(126.622844410456,-34.706866888933,22.6207784648604));
#26514=CARTESIAN_POINT('Ctrl Pts',(126.625238527359,-34.6804816760169,22.6192062325317));
#26515=CARTESIAN_POINT('Ctrl Pts',(126.630507076093,-34.6291164756261,22.6161605211917));
#26516=CARTESIAN_POINT('Ctrl Pts',(126.63335059779,-34.6041351162239,22.6146861925193));
#26517=CARTESIAN_POINT('Ctrl Pts',(126.63997234392,-34.5512079497467,22.6115765120531));
#26518=CARTESIAN_POINT('Ctrl Pts',(126.643821893556,-34.5232728855082,22.6099434891408));
#26519=CARTESIAN_POINT('Ctrl Pts',(126.654511184851,-34.4522671855163,22.6058119415004));
#26520=CARTESIAN_POINT('Ctrl Pts',(126.661834404157,-34.4092738814656,22.6033285227861));
#26521=CARTESIAN_POINT('Ctrl Pts',(126.699004926034,-34.2139065936132,22.5921111504173));
#26522=CARTESIAN_POINT('Ctrl Pts',(126.738470590289,-34.0635469347733,22.5836776502972));
#26523=CARTESIAN_POINT('Ctrl Pts',(126.798698643084,-33.8850238155912,22.5736077440637));
#26524=CARTESIAN_POINT('Ctrl Pts',(126.80974403253,-33.8538028132203,22.571843975796));
#26525=CARTESIAN_POINT('Ctrl Pts',(126.82124189288,-33.8227566271494,22.5700841492926));
#26526=CARTESIAN_POINT('Ctrl Pts',(126.821241915871,-33.8227565650702,22.910437866903));
#26527=CARTESIAN_POINT('Ctrl Pts',(126.82099104874,-33.8234339491151,22.9104820102593));
#26528=CARTESIAN_POINT('Ctrl Pts',(126.820740398121,-33.8241114133797,22.9105261636133));
#26529=CARTESIAN_POINT('Ctrl Pts',(126.762030822358,-33.982948999682,22.9208794240525));
#26530=CARTESIAN_POINT('Ctrl Pts',(126.715459369069,-34.1452369403566,22.9317036970583));
#26531=CARTESIAN_POINT('Ctrl Pts',(126.652004459477,-34.4505819230391,22.9518005612867));
#26532=CARTESIAN_POINT('Ctrl Pts',(126.631773965391,-34.592579412559,22.9610437876921));
#26533=CARTESIAN_POINT('Ctrl Pts',(126.61374749444,-34.8228406799421,22.9756516692902));
#26534=CARTESIAN_POINT('Ctrl Pts',(126.610297960021,-34.9104825912722,22.981125822323));
#26535=CARTESIAN_POINT('Ctrl Pts',(126.610215302828,-35.0631810994019,22.9904959503338));
#26536=CARTESIAN_POINT('Ctrl Pts',(126.612050631295,-35.1281876952586,22.9944324614789));
#26537=CARTESIAN_POINT('Ctrl Pts',(126.617604134591,-35.2255152586737,23.0002495803037));
#26538=CARTESIAN_POINT('Ctrl Pts',(126.619919010954,-35.2578983126503,23.002172388253));
#26539=CARTESIAN_POINT('Ctrl Pts',(126.624960736115,-35.3165642123053,23.0056339323517));
#26540=CARTESIAN_POINT('Ctrl Pts',(126.627530335416,-35.3428576282269,23.0071773747259));
#26541=CARTESIAN_POINT('Ctrl Pts',(126.63377052809,-35.3998227684592,23.0105049966958));
#26542=CARTESIAN_POINT('Ctrl Pts',(126.637553537661,-35.4304799441682,23.0122855648604));
#26543=CARTESIAN_POINT('Ctrl Pts',(126.649479605335,-35.5173422938289,23.0173041973384));
#26544=CARTESIAN_POINT('Ctrl Pts',(126.658616919227,-35.573401768844,23.020511566431));
#26545=CARTESIAN_POINT('Ctrl Pts',(126.682685868905,-35.7008157627025,23.0277482778569));
#26546=CARTESIAN_POINT('Ctrl Pts',(126.698519070877,-35.7719717129499,23.0317510149133));
#26547=CARTESIAN_POINT('Ctrl Pts',(126.765572759789,-36.0332711437679,23.0463955384083));
#26548=CARTESIAN_POINT('Ctrl Pts',(126.83103182175,-36.2193483948337,23.056693662574));
#26549=CARTESIAN_POINT('Ctrl Pts',(126.971707682056,-36.5299015523981,23.0748827619362));
#26550=CARTESIAN_POINT('Ctrl Pts',(127.039439883645,-36.657174828069,23.0826679670223));
#26551=CARTESIAN_POINT('Ctrl Pts',(127.129901141975,-36.8038119459335,23.0924796146608));
#26552=CARTESIAN_POINT('Ctrl Pts',(127.145050909777,-36.8276954266485,23.0941060009977));
#26553=CARTESIAN_POINT('Ctrl Pts',(127.16952014108,-36.8652243165318,23.0967113875397));
#26554=CARTESIAN_POINT('Ctrl Pts',(127.178643900167,-36.8789964650642,23.0976783114826));
#26555=CARTESIAN_POINT('Ctrl Pts',(127.196449364859,-36.9054514201454,23.0995577678874));
#26556=CARTESIAN_POINT('Ctrl Pts',(127.205117237884,-36.9181427449747,23.1004694452645));
#26557=CARTESIAN_POINT('Ctrl Pts',(127.226849237619,-36.9495022665738,23.1027464050047));
#26558=CARTESIAN_POINT('Ctrl Pts',(127.240015752354,-36.968098353516,23.1041181827489));
#26559=CARTESIAN_POINT('Ctrl Pts',(127.292254643203,-37.0403242169623,23.1095264794334));
#26560=CARTESIAN_POINT('Ctrl Pts',(127.332708699814,-37.092931859177,23.1136411504478));
#26561=CARTESIAN_POINT('Ctrl Pts',(127.450208391119,-37.2367888088423,23.125319848251));
#26562=CARTESIAN_POINT('Ctrl Pts',(127.530569280683,-37.325203390577,23.133000784026));
#26563=CARTESIAN_POINT('Ctrl Pts',(127.791954538115,-37.5839183108784,23.1567044608626));
#26564=CARTESIAN_POINT('Ctrl Pts',(127.987184666386,-37.7387423425457,23.1726391825686));
#26565=CARTESIAN_POINT('Ctrl Pts',(128.24068951947,-37.8978991404231,23.1908356517705));
#26566=CARTESIAN_POINT('Ctrl Pts',(128.284377223569,-37.9239753254123,23.1938943767824));
#26567=CARTESIAN_POINT('Ctrl Pts',(128.354709767108,-37.9638358993376,23.1986996561776));
#26568=CARTESIAN_POINT('Ctrl Pts',(128.380977789022,-37.9782663338575,23.2004687438768));
#26569=CARTESIAN_POINT('Ctrl Pts',(128.430838771203,-38.0048029920779,23.2037799058657));
#26570=CARTESIAN_POINT('Ctrl Pts',(128.454388967973,-38.0169843519115,23.2053245103925));
#26571=CARTESIAN_POINT('Ctrl Pts',(128.508246765071,-38.0440461773995,23.2088144805509));
#26572=CARTESIAN_POINT('Ctrl Pts',(128.53863886894,-38.0587527859887,23.2107537796421));
#26573=CARTESIAN_POINT('Ctrl Pts',(128.634795987094,-38.1035223903969,23.2168000227788));
#26574=CARTESIAN_POINT('Ctrl Pts',(128.701308082851,-38.1319376661058,23.2208520521741));
#26575=CARTESIAN_POINT('Ctrl Pts',(128.863624578295,-38.1952214841995,23.2304773877655));
#26576=CARTESIAN_POINT('Ctrl Pts',(128.96019232814,-38.2279391751071,23.2359885935928));
#26577=CARTESIAN_POINT('Ctrl Pts',(129.10371966805,-38.2694560289283,23.2439815973126));
#26578=CARTESIAN_POINT('Ctrl Pts',(129.149620329422,-38.2816940240597,23.2465091996543));
#26579=CARTESIAN_POINT('Ctrl Pts',(129.397783530491,-38.342302626394,23.2600735243816));
#26580=CARTESIAN_POINT('Ctrl Pts',(129.603896497924,-38.3729420110107,23.2709571366214));
#26581=CARTESIAN_POINT('Ctrl Pts',(129.858832844804,-38.3871410868485,23.2852012808286));
#26582=CARTESIAN_POINT('Ctrl Pts',(129.906218652212,-38.3887840753286,23.2878828898149));
#26583=CARTESIAN_POINT('Ctrl Pts',(129.972394059845,-38.3896895837878,23.2916941549857));
#26584=CARTESIAN_POINT('Ctrl Pts',(129.991168634878,-38.3897904854055,23.292782899158));
#26585=CARTESIAN_POINT('Ctrl Pts',(130.025083617667,-38.3896910075231,23.2947646364064));
#26586=CARTESIAN_POINT('Ctrl Pts',(130.040223947393,-38.3895451527241,23.295654740488));
#26587=CARTESIAN_POINT('Ctrl Pts',(130.071983152491,-38.389026379111,23.2975340552605));
#26588=CARTESIAN_POINT('Ctrl Pts',(130.088600907703,-38.3886326484421,23.2985242831775));
#26589=CARTESIAN_POINT('Ctrl Pts',(130.133961883737,-38.3872240069773,23.3012448645861));
#26590=CARTESIAN_POINT('Ctrl Pts',(130.162695517743,-38.385965491429,23.3029874856713));
#26591=CARTESIAN_POINT('Ctrl Pts',(130.376393709729,-38.373879337996,23.3160743407193));
#26592=CARTESIAN_POINT('Ctrl Pts',(130.560194154702,-38.3482689477335,23.3280194918785));
#26593=CARTESIAN_POINT('Ctrl Pts',(130.970179870068,-38.2564294129084,23.3551025273855));
#26594=CARTESIAN_POINT('Ctrl Pts',(131.193471606607,-38.1813893440609,23.3701339875679));
#26595=CARTESIAN_POINT('Ctrl Pts',(131.454584943649,-38.0622372677699,23.3875979139282));
#26596=CARTESIAN_POINT('Ctrl Pts',(131.501437119071,-38.0395396804537,23.390729885767));
#26597=CARTESIAN_POINT('Ctrl Pts',(131.574638243906,-38.0019714971347,23.3956226789002));
#26598=CARTESIAN_POINT('Ctrl Pts',(131.601341372054,-37.9878126392964,23.3974074453966));
#26599=CARTESIAN_POINT('Ctrl Pts',(131.650855045311,-37.9607043782557,23.4007177068324));
#26600=CARTESIAN_POINT('Ctrl Pts',(131.673711392157,-37.9478437931481,23.4022461477179));
#26601=CARTESIAN_POINT('Ctrl Pts',(131.725188957321,-37.9180871450768,23.4056905240933));
#26602=CARTESIAN_POINT('Ctrl Pts',(131.753715784527,-37.9010326754021,23.4076006685354));
#26603=CARTESIAN_POINT('Ctrl Pts',(131.840921846817,-37.8471409244757,23.4134484137288));
#26604=CARTESIAN_POINT('Ctrl Pts',(131.898727851236,-37.8089211699321,23.4173363355261));
#26605=CARTESIAN_POINT('Ctrl Pts',(132.033624581195,-37.7136625089983,23.4264768559567));
#26606=CARTESIAN_POINT('Ctrl Pts',(132.109547061533,-37.6550717503198,23.4316760074138));
#26607=CARTESIAN_POINT('Ctrl Pts',(132.284852332273,-37.5075123022938,23.4439640120745));
#26608=CARTESIAN_POINT('Ctrl Pts',(132.381667757404,-37.4157456970804,23.450985117923));
#26609=CARTESIAN_POINT('Ctrl Pts',(132.576399169963,-37.2080538013853,23.4661215911864));
#26610=CARTESIAN_POINT('Ctrl Pts',(132.672442355327,-37.0907839315999,23.4742392434749));
#26611=CARTESIAN_POINT('Ctrl Pts',(132.781228110879,-36.9381623548048,23.4848176505006));
#26612=CARTESIAN_POINT('Ctrl Pts',(132.801670091542,-36.9084935418959,23.4868748943246));
#26613=CARTESIAN_POINT('Ctrl Pts',(132.831672365347,-36.8634282308166,23.4900099925321));
#26614=CARTESIAN_POINT('Ctrl Pts',(132.841589026969,-36.8482707934181,23.4910661714537));
#26615=CARTESIAN_POINT('Ctrl Pts',(132.859385644309,-36.8205872077836,23.4929996534261));
#26616=CARTESIAN_POINT('Ctrl Pts',(132.867305736671,-36.8080878937493,23.4938743731124));
#26617=CARTESIAN_POINT('Ctrl Pts',(132.885535456707,-36.7788971489478,23.4959210893217));
#26618=CARTESIAN_POINT('Ctrl Pts',(132.895782244796,-36.7621677242874,23.4970968896798));
#26619=CARTESIAN_POINT('Ctrl Pts',(132.928669921785,-36.7074121168421,23.5009520140095));
#26620=CARTESIAN_POINT('Ctrl Pts',(132.950710589783,-36.6690327342506,23.5036645635286));
#26621=CARTESIAN_POINT('Ctrl Pts',(133.003118944002,-36.5734899177844,23.5104225855791));
#26622=CARTESIAN_POINT('Ctrl Pts',(133.032612369083,-36.5158678354111,23.5145027804693));
#26623=CARTESIAN_POINT('Ctrl Pts',(133.16907408796,-36.2293157499042,23.5347007294079));
#26624=CARTESIAN_POINT('Ctrl Pts',(133.251876674452,-35.9897301058736,23.5512275691034));
#26625=CARTESIAN_POINT('Ctrl Pts',(133.330131363948,-35.6414774120627,23.5735961284351));
#26626=CARTESIAN_POINT('Ctrl Pts',(133.348281278378,-35.5387801430027,23.5800105924801));
#26627=CARTESIAN_POINT('Ctrl Pts',(133.366735839005,-35.3962950804308,23.5886539906304));
#26628=CARTESIAN_POINT('Ctrl Pts',(133.371118217657,-35.3571024501742,23.5910053908385));
#26629=CARTESIAN_POINT('Ctrl Pts',(133.377126574664,-35.2933060891642,23.5947920565171));
#26630=CARTESIAN_POINT('Ctrl Pts',(133.379169700171,-35.2687462530776,23.5962400288211));
#26631=CARTESIAN_POINT('Ctrl Pts',(133.382911860536,-35.2169288547645,23.5992751419442));
#26632=CARTESIAN_POINT('Ctrl Pts',(133.384549702556,-35.1896685501678,23.600860294272));
#26633=CARTESIAN_POINT('Ctrl Pts',(133.387728805286,-35.1233840794671,23.6046880573141));
#26634=CARTESIAN_POINT('Ctrl Pts',(133.388925475389,-35.0843468399124,23.6069199685269));
#26635=CARTESIAN_POINT('Ctrl Pts',(133.390915102305,-34.9354668633698,23.6153556218887));
#26636=CARTESIAN_POINT('Ctrl Pts',(133.38704388264,-34.8256250878844,23.6214181905919));
#26637=CARTESIAN_POINT('Ctrl Pts',(133.360687703521,-34.5119756760426,23.6384903743963));
#26638=CARTESIAN_POINT('Ctrl Pts',(133.32505315594,-34.309774675517,23.6491843918476));
#26639=CARTESIAN_POINT('Ctrl Pts',(133.236339528424,-33.9829444446467,23.6672950312395));
#26640=CARTESIAN_POINT('Ctrl Pts',(133.193694996535,-33.856059111773,23.6745531928376));
#26641=CARTESIAN_POINT('Ctrl Pts',(133.133168268083,-33.7059944809986,23.6837701862437));
#26642=CARTESIAN_POINT('Ctrl Pts',(133.122340989274,-33.6800832157172,23.6853853654109));
#26643=CARTESIAN_POINT('Ctrl Pts',(133.104652142154,-33.6391871403826,23.6879769248676));
#26644=CARTESIAN_POINT('Ctrl Pts',(133.098000835993,-33.624112156426,23.6889414463183));
#26645=CARTESIAN_POINT('Ctrl Pts',(133.08492401723,-33.5950495375422,23.6908199358509));
#26646=CARTESIAN_POINT('Ctrl Pts',(133.078512709476,-33.5810562175969,23.6917330984575));
#26647=CARTESIAN_POINT('Ctrl Pts',(133.062321912723,-33.5463444490477,23.6940191830544));
#26648=CARTESIAN_POINT('Ctrl Pts',(133.052427333971,-33.5256807449137,23.6953987119341));
#26649=CARTESIAN_POINT('Ctrl Pts',(133.012595449593,-33.4446163945177,23.7008798788137));
#26650=CARTESIAN_POINT('Ctrl Pts',(132.981070231003,-33.3850174768372,23.7050622552517));
#26651=CARTESIAN_POINT('Ctrl Pts',(132.887254895,-33.219775821444,23.717015986941));
#26652=CARTESIAN_POINT('Ctrl Pts',(132.820980027847,-33.1165170455659,23.7249099819555));
#26653=CARTESIAN_POINT('Ctrl Pts',(132.607218004869,-32.8201421700877,23.7484644145453));
#26654=CARTESIAN_POINT('Ctrl Pts',(132.444403485207,-32.6390061985273,23.7640263896184));
#26655=CARTESIAN_POINT('Ctrl Pts',(132.22533177626,-32.4424723667827,23.7819255359141));
#26656=CARTESIAN_POINT('Ctrl Pts',(132.186278816788,-32.4090089777049,23.7850183720514));
#26657=CARTESIAN_POINT('Ctrl Pts',(132.123191479038,-32.3573936646943,23.7898644242251));
#26658=CARTESIAN_POINT('Ctrl Pts',(132.099651846995,-32.3386521255418,23.7916408268109));
#26659=CARTESIAN_POINT('Ctrl Pts',(132.057014879181,-32.3056237435785,23.7948030142445));
#26660=CARTESIAN_POINT('Ctrl Pts',(132.038010638914,-32.2912205141639,23.7961932728847));
#26661=CARTESIAN_POINT('Ctrl Pts',(131.992950259457,-32.2578121311745,23.7994457596723));
#26662=CARTESIAN_POINT('Ctrl Pts',(131.966771507508,-32.2389757363414,23.8013014736034));
#26663=CARTESIAN_POINT('Ctrl Pts',(131.887964141413,-32.1839611926456,23.8067914299035));
#26664=CARTESIAN_POINT('Ctrl Pts',(131.834576422565,-32.1488926305017,23.8103847450437));
#26665=CARTESIAN_POINT('Ctrl Pts',(131.640206361493,-32.0289393970981,23.823070345762));
#26666=CARTESIAN_POINT('Ctrl Pts',(131.494072041906,-31.9528319911576,23.8318724069918));
#26667=CARTESIAN_POINT('Ctrl Pts',(131.148558022859,-31.8037431645573,23.8518497691372));
#26668=CARTESIAN_POINT('Ctrl Pts',(130.94672145762,-31.7382605386934,23.862932748559));
#26669=CARTESIAN_POINT('Ctrl Pts',(130.69672555456,-31.6823267289896,23.8772749766537));
#26670=CARTESIAN_POINT('Ctrl Pts',(130.653146080762,-31.6734729460076,23.8797980181451));
#26671=CARTESIAN_POINT('Ctrl Pts',(130.59027762137,-31.6619832897281,23.8834866588573));
#26672=CARTESIAN_POINT('Ctrl Pts',(130.571118738339,-31.658651982187,23.8846172366288));
#26673=CARTESIAN_POINT('Ctrl Pts',(130.537186083,-31.6530522021898,23.8866327371998));
#26674=CARTESIAN_POINT('Ctrl Pts',(130.522424344964,-31.6507163093001,23.8875139866667));
#26675=CARTESIAN_POINT('Ctrl Pts',(130.489795206329,-31.6457740501232,23.8894720630821));
#26676=CARTESIAN_POINT('Ctrl Pts',(130.471922353268,-31.6432127968506,23.8905511718802));
#26677=CARTESIAN_POINT('Ctrl Pts',(130.418619126482,-31.6360083307154,23.8937872588269));
#26678=CARTESIAN_POINT('Ctrl Pts',(130.383135930791,-31.6317825835941,23.8959648414437));
#26679=CARTESIAN_POINT('Ctrl Pts',(130.204804610918,-31.6133991009827,23.9070041884261));
#26680=CARTESIAN_POINT('Ctrl Pts',(130.061235112937,-31.6077655870104,23.9161915897613));
#26681=CARTESIAN_POINT('Ctrl Pts',(129.645035363894,-31.6178668901878,23.9429982833793));
#26682=CARTESIAN_POINT('Ctrl Pts',(129.374061635519,-31.6573851642018,23.9605728054815));
#26683=CARTESIAN_POINT('Ctrl Pts',(129.064104621089,-31.7416507753097,23.9800511756094));
#26684=CARTESIAN_POINT('Ctrl Pts',(129.01775224568,-31.7553228912587,23.9829506436435));
#26685=CARTESIAN_POINT('Ctrl Pts',(128.94391420433,-31.778829633505,23.9875497270389));
#26686=CARTESIAN_POINT('Ctrl Pts',(128.916236970659,-31.7880358791561,23.9892691602955));
#26687=CARTESIAN_POINT('Ctrl Pts',(128.863465654284,-31.8063489317281,23.992539963171));
#26688=CARTESIAN_POINT('Ctrl Pts',(128.838353690229,-31.8153971400255,23.9940930904858));
#26689=CARTESIAN_POINT('Ctrl Pts',(128.780307724944,-31.8370899247414,23.9976766400935));
#26690=CARTESIAN_POINT('Ctrl Pts',(128.747458711238,-31.8499539935427,23.9996997071762));
#26691=CARTESIAN_POINT('Ctrl Pts',(128.639332609322,-31.8942563683168,24.0063479059001));
#26692=CARTESIAN_POINT('Ctrl Pts',(128.564987141215,-31.9278999425594,24.0109005240269));
#26693=CARTESIAN_POINT('Ctrl Pts',(128.382783596397,-32.0184119673033,24.0220822268754));
#26694=CARTESIAN_POINT('Ctrl Pts',(128.276642139766,-32.0784770439541,24.0286159209385));
#26695=CARTESIAN_POINT('Ctrl Pts',(128.018536703292,-32.2435092327085,24.0449091424842));
#26696=CARTESIAN_POINT('Ctrl Pts',(127.871492782923,-32.3554040474251,24.0545660389377));
#26697=CARTESIAN_POINT('Ctrl Pts',(127.677338622234,-32.5298761191181,24.0688423294303));
#26698=CARTESIAN_POINT('Ctrl Pts',(127.622140874676,-32.5829662446655,24.0731025600854));
#26699=CARTESIAN_POINT('Ctrl Pts',(127.551643713595,-32.655525190657,24.0788927647717));
#26700=CARTESIAN_POINT('Ctrl Pts',(127.534688736915,-32.6733605913742,24.0803136059769));
#26701=CARTESIAN_POINT('Ctrl Pts',(127.508275595749,-32.7017581716639,24.0825751061112));
#26702=CARTESIAN_POINT('Ctrl Pts',(127.498686610119,-32.712198147149,24.0834063553604));
#26703=CARTESIAN_POINT('Ctrl Pts',(127.478688857615,-32.7342466413048,24.0851623302159));
#26704=CARTESIAN_POINT('Ctrl Pts',(127.468294282524,-32.7458672867926,24.0860881158017));
#26705=CARTESIAN_POINT('Ctrl Pts',(127.442149843759,-32.7755044848018,24.0884490725075));
#26706=CARTESIAN_POINT('Ctrl Pts',(127.426510093778,-32.7936166809816,24.0898917674628));
#26707=CARTESIAN_POINT('Ctrl Pts',(127.361504641657,-32.8705301557401,24.0960119500959));
#26708=CARTESIAN_POINT('Ctrl Pts',(127.313955328994,-32.9308306329129,24.1007947299246));
#26709=CARTESIAN_POINT('Ctrl Pts',(127.177005913177,-33.1171881710146,24.1154076957921));
#26710=CARTESIAN_POINT('Ctrl Pts',(127.094135743321,-33.2477938054022,24.1254203025004));
#26711=CARTESIAN_POINT('Ctrl Pts',(126.943698634776,-33.5250954934791,24.145719522381));
#26712=CARTESIAN_POINT('Ctrl Pts',(126.87712746268,-33.6718560792905,24.1559689145811));
#26713=CARTESIAN_POINT('Ctrl Pts',(126.821241975209,-33.8227564048483,24.1659080048185));
#26714=CARTESIAN_POINT('Origin',(130.,-35.,23.));
#26715=CARTESIAN_POINT('',(126.82124193643,-33.8227565095591,25.4139334024237));
#26716=CARTESIAN_POINT('',(126.821241914321,-33.8227565692546,25.0733699431874));
#26717=CARTESIAN_POINT('',(126.821241915871,-33.8227565650715,23.));
#26718=CARTESIAN_POINT('Ctrl Pts',(126.821241914321,-33.8227565692547,25.0733699431874));
#26719=CARTESIAN_POINT('Ctrl Pts',(126.875893823826,-33.6751870906752,25.0637024941563));
#26720=CARTESIAN_POINT('Ctrl Pts',(126.940754520208,-33.5316051062762,25.0536068363797));
#26721=CARTESIAN_POINT('Ctrl Pts',(127.101016925518,-33.2339431825994,25.0318253550778));
#26722=CARTESIAN_POINT('Ctrl Pts',(127.199275152069,-33.0819255671996,25.0201687247304));
#26723=CARTESIAN_POINT('Ctrl Pts',(127.351719310163,-32.8829491129561,25.004479979221));
#26724=CARTESIAN_POINT('Ctrl Pts',(127.395957199737,-32.8287659827226,25.0001555604634));
#26725=CARTESIAN_POINT('Ctrl Pts',(127.477971830063,-32.7344291177899,24.9925360805312));
#26726=CARTESIAN_POINT('Ctrl Pts',(127.515110482934,-32.6937558387858,24.9892186467732));
#26727=CARTESIAN_POINT('Ctrl Pts',(127.5743647106,-32.6319561938971,24.9841245811721));
#26728=CARTESIAN_POINT('Ctrl Pts',(127.595801592221,-32.6101949593467,24.9823199540119));
#26729=CARTESIAN_POINT('Ctrl Pts',(127.636339655425,-32.5701411510711,24.9789767193885));
#26730=CARTESIAN_POINT('Ctrl Pts',(127.655366285614,-32.5517767556746,24.9774350589407));
#26731=CARTESIAN_POINT('Ctrl Pts',(127.698547872695,-32.5110632957582,24.9739960620206));
#26732=CARTESIAN_POINT('Ctrl Pts',(127.722817473349,-32.488839379671,24.9721040686612));
#26733=CARTESIAN_POINT('Ctrl Pts',(127.797803243295,-32.4221554057985,24.9663773758941));
#26734=CARTESIAN_POINT('Ctrl Pts',(127.849527337279,-32.3788511162025,24.962589296921));
#26735=CARTESIAN_POINT('Ctrl Pts',(128.138556389407,-32.1511899503183,24.9422015487431));
#26736=CARTESIAN_POINT('Ctrl Pts',(128.398253180408,-31.9974863518289,24.9267899944319));
#26737=CARTESIAN_POINT('Ctrl Pts',(128.73765046983,-31.853328512598,24.9068475310897));
#26738=CARTESIAN_POINT('Ctrl Pts',(128.801289414047,-31.8285398040028,24.90310930642));
#26739=CARTESIAN_POINT('Ctrl Pts',(128.908947636574,-31.7903079811134,24.8967216121689));
#26740=CARTESIAN_POINT('Ctrl Pts',(128.952571523532,-31.7758084303568,24.8941161392245));
#26741=CARTESIAN_POINT('Ctrl Pts',(129.015488887375,-31.7563077811375,24.8903162476382));
#26742=CARTESIAN_POINT('Ctrl Pts',(129.034554340259,-31.7505822093758,24.8891593123638));
#26743=CARTESIAN_POINT('Ctrl Pts',(129.068029895214,-31.7408497325236,24.8871165984788));
#26744=CARTESIAN_POINT('Ctrl Pts',(129.082417819552,-31.7367697486889,24.8862349176171));
#26745=CARTESIAN_POINT('Ctrl Pts',(129.114147808661,-31.7279985209001,24.8842819674329));
#26746=CARTESIAN_POINT('Ctrl Pts',(129.131500225542,-31.7233498975141,24.8832085020978));
#26747=CARTESIAN_POINT('Ctrl Pts',(129.183028443219,-31.7099838133465,24.8800064246755));
#26748=CARTESIAN_POINT('Ctrl Pts',(129.217303265452,-31.7016618359966,24.8778578175446));
#26749=CARTESIAN_POINT('Ctrl Pts',(129.429346921317,-31.6536683997751,24.8644762127533));
#26750=CARTESIAN_POINT('Ctrl Pts',(129.60993242284,-31.6278467096305,24.8527123825411));
#26751=CARTESIAN_POINT('Ctrl Pts',(129.952361894427,-31.6067648088782,24.830599611446));
#26752=CARTESIAN_POINT('Ctrl Pts',(130.113534106895,-31.6083289931502,24.8202714235265));
#26753=CARTESIAN_POINT('Ctrl Pts',(130.37047077841,-31.6291655068897,24.8041823743001));
#26754=CARTESIAN_POINT('Ctrl Pts',(130.466573076162,-31.6411183266721,24.7982465083586));
#26755=CARTESIAN_POINT('Ctrl Pts',(130.598976278609,-31.6633796476745,24.7901860889087));
#26756=CARTESIAN_POINT('Ctrl Pts',(130.635808668836,-31.6702018884951,24.7879563372232));
#26757=CARTESIAN_POINT('Ctrl Pts',(130.69901025272,-31.6829953075673,24.7841504652557));
#26758=CARTESIAN_POINT('Ctrl Pts',(130.725434415827,-31.6886739160363,24.7825653762343));
#26759=CARTESIAN_POINT('Ctrl Pts',(130.779424149527,-31.7009537286371,24.7793383136194));
#26760=CARTESIAN_POINT('Ctrl Pts',(130.806980541334,-31.7075858732133,24.7776974547774));
#26761=CARTESIAN_POINT('Ctrl Pts',(130.877402580308,-31.7254720023353,24.7735183119634));
#26762=CARTESIAN_POINT('Ctrl Pts',(130.920137270263,-31.7372225704428,24.7709958610612));
#26763=CARTESIAN_POINT('Ctrl Pts',(131.120039856985,-31.7964290345649,24.7592437544084));
#26764=CARTESIAN_POINT('Ctrl Pts',(131.273862044502,-31.8544253801053,24.7503533319201));
#26765=CARTESIAN_POINT('Ctrl Pts',(131.598557818831,-32.0045904945581,24.7312714924699));
#26766=CARTESIAN_POINT('Ctrl Pts',(131.766936535618,-32.1007253521701,24.7211695281631));
#26767=CARTESIAN_POINT('Ctrl Pts',(131.97405619726,-32.2437540348335,24.707461954135));
#26768=CARTESIAN_POINT('Ctrl Pts',(132.021067230905,-32.27803815241,24.7042548591645));
#26769=CARTESIAN_POINT('Ctrl Pts',(132.099657977262,-32.3385113590126,24.6986854124545));
#26770=CARTESIAN_POINT('Ctrl Pts',(132.131687867204,-32.3640956135696,24.696353762319));
#26771=CARTESIAN_POINT('Ctrl Pts',(132.177907122695,-32.4024072023963,24.6928845204022));
#26772=CARTESIAN_POINT('Ctrl Pts',(132.192466739078,-32.4146842865059,24.6917760069932));
#26773=CARTESIAN_POINT('Ctrl Pts',(132.218239271372,-32.4367906989044,24.6897840875354));
#26774=CARTESIAN_POINT('Ctrl Pts',(132.229491936485,-32.4465722892715,24.6889040128183));
#26775=CARTESIAN_POINT('Ctrl Pts',(132.254690087242,-32.4687698094187,24.6869095918574));
#26776=CARTESIAN_POINT('Ctrl Pts',(132.268597683253,-32.4812268495621,24.6857923943984));
#26777=CARTESIAN_POINT('Ctrl Pts',(132.311200168924,-32.5200249839481,24.6823210563346));
#26778=CARTESIAN_POINT('Ctrl Pts',(132.33954353939,-32.5467454166296,24.6799418583471));
#26779=CARTESIAN_POINT('Ctrl Pts',(132.522818156495,-32.7255905571389,24.6641284709953));
#26780=CARTESIAN_POINT('Ctrl Pts',(132.663279390932,-32.8918055326581,24.6499832656876));
#26781=CARTESIAN_POINT('Ctrl Pts',(132.901022739427,-33.2351546624578,24.6231467391655));
#26782=CARTESIAN_POINT('Ctrl Pts',(133.000333295119,-33.4098322665787,24.6104795577287));
#26783=CARTESIAN_POINT('Ctrl Pts',(133.102325110033,-33.6332479227907,24.595627456806));
#26784=CARTESIAN_POINT('Ctrl Pts',(133.120206079079,-33.6745768051963,24.592931450274));
#26785=CARTESIAN_POINT('Ctrl Pts',(133.148047433661,-33.7426162389387,24.5885744644279));
#26786=CARTESIAN_POINT('Ctrl Pts',(133.158503311044,-33.7691167905398,24.5868972443618));
#26787=CARTESIAN_POINT('Ctrl Pts',(133.178198952359,-33.8209398414679,24.5836546561143));
#26788=CARTESIAN_POINT('Ctrl Pts',(133.187473171261,-33.8462468711979,24.5820882523075));
#26789=CARTESIAN_POINT('Ctrl Pts',(133.208762993143,-33.9065583755539,24.5783941555274));
#26790=CARTESIAN_POINT('Ctrl Pts',(133.22050925611,-33.9416546801746,24.5762753221904));
#26791=CARTESIAN_POINT('Ctrl Pts',(133.258073864831,-34.0603148072602,24.5692081477171));
#26792=CARTESIAN_POINT('Ctrl Pts',(133.281233625542,-34.1446865133921,24.5643436643755));
#26793=CARTESIAN_POINT('Ctrl Pts',(133.363018642583,-34.4952495192453,24.5446347664032));
#26794=CARTESIAN_POINT('Ctrl Pts',(133.392701213385,-34.7671127671767,24.5306096205587));
#26795=CARTESIAN_POINT('Ctrl Pts',(133.388743834586,-35.1059422768452,24.512261459041));
#26796=CARTESIAN_POINT('Ctrl Pts',(133.386020594541,-35.1722561925368,24.5086240818133));
#26797=CARTESIAN_POINT('Ctrl Pts',(133.378184404678,-35.2833805420892,24.5023904569481));
#26798=CARTESIAN_POINT('Ctrl Pts',(133.374120284345,-35.328247328336,24.4998355034537));
#26799=CARTESIAN_POINT('Ctrl Pts',(133.366989895216,-35.3926503278033,24.4960964126159));
#26800=CARTESIAN_POINT('Ctrl Pts',(133.364644737093,-35.4122632493966,24.4949481309856));
#26801=CARTESIAN_POINT('Ctrl Pts',(133.360224512184,-35.4466761811227,24.4929147336864));
#26802=CARTESIAN_POINT('Ctrl Pts',(133.358222779718,-35.4614847046468,24.4920335796212));
#26803=CARTESIAN_POINT('Ctrl Pts',(133.353583152089,-35.4941779998795,24.4900742711456));
#26804=CARTESIAN_POINT('Ctrl Pts',(133.350900104469,-35.5120549883257,24.4889938144035));
#26805=CARTESIAN_POINT('Ctrl Pts',(133.342470802727,-35.5653130324419,24.4857495627475));
#26806=CARTESIAN_POINT('Ctrl Pts',(133.336306366831,-35.600624256997,24.4835650157044));
#26807=CARTESIAN_POINT('Ctrl Pts',(133.298062712453,-35.8008908889849,24.4710090214047));
#26808=CARTESIAN_POINT('Ctrl Pts',(133.254313802097,-35.9633675392982,24.4601891807129));
#26809=CARTESIAN_POINT('Ctrl Pts',(133.143508726153,-36.2792846214322,24.4386090022506));
#26810=CARTESIAN_POINT('Ctrl Pts',(133.076771357625,-36.4323764362759,24.4278799010688));
#26811=CARTESIAN_POINT('Ctrl Pts',(132.966652538034,-36.6414029314021,24.4130971627072));
#26812=CARTESIAN_POINT('Ctrl Pts',(132.932390765654,-36.7018567028678,24.408802411961));
#26813=CARTESIAN_POINT('Ctrl Pts',(132.867823011802,-36.8080372920871,24.4012290523111));
#26814=CARTESIAN_POINT('Ctrl Pts',(132.83822028184,-36.854161220482,24.3979284696695));
#26815=CARTESIAN_POINT('Ctrl Pts',(132.790425001181,-36.9248020701622,24.3928542677881));
#26816=CARTESIAN_POINT('Ctrl Pts',(132.77299872563,-36.9498238010583,24.3910530048198));
#26817=CARTESIAN_POINT('Ctrl Pts',(132.739830679199,-36.9961042974664,24.3877128970109));
#26818=CARTESIAN_POINT('Ctrl Pts',(132.724173212354,-37.0174203539709,24.3861710478909));
#26819=CARTESIAN_POINT('Ctrl Pts',(132.688433988152,-37.0649008242302,24.3827276787155));
#26820=CARTESIAN_POINT('Ctrl Pts',(132.668216474972,-37.0909599887926,24.3808315648287));
#26821=CARTESIAN_POINT('Ctrl Pts',(132.60524933025,-37.169720102317,24.3750775487913));
#26822=CARTESIAN_POINT('Ctrl Pts',(132.561293723805,-37.2214375316467,24.3712669486538));
#26823=CARTESIAN_POINT('Ctrl Pts',(132.347635325388,-37.4580445608414,24.3536058901353));
#26824=CARTESIAN_POINT('Ctrl Pts',(132.159302421337,-37.6250318853284,24.3405293951551));
#26825=CARTESIAN_POINT('Ctrl Pts',(131.835327009499,-37.853623356693,24.319380312681));
#26826=CARTESIAN_POINT('Ctrl Pts',(131.711126149247,-37.9297832738017,24.3115164386881));
#26827=CARTESIAN_POINT('Ctrl Pts',(131.557593852507,-38.010829658664,24.3016273679988));
#26828=CARTESIAN_POINT('Ctrl Pts',(131.532595599175,-38.0236310065254,24.3000120262671));
#26829=CARTESIAN_POINT('Ctrl Pts',(131.492683211789,-38.0434476193215,24.2974202679454));
#26830=CARTESIAN_POINT('Ctrl Pts',(131.477871480686,-38.0506675407377,24.2964557133605));
#26831=CARTESIAN_POINT('Ctrl Pts',(131.449285421754,-38.0643446684004,24.2945878106088));
#26832=CARTESIAN_POINT('Ctrl Pts',(131.435519313781,-38.0708176024146,24.293685405137));
#26833=CARTESIAN_POINT('Ctrl Pts',(131.401050533551,-38.0867426863635,24.2914194736652));
#26834=CARTESIAN_POINT('Ctrl Pts',(131.380295537576,-38.096079323376,24.290049366698));
#26835=CARTESIAN_POINT('Ctrl Pts',(131.303481589911,-38.1297082112448,24.2849619131463));
#26836=CARTESIAN_POINT('Ctrl Pts',(131.246865642598,-38.1526913697427,24.2811797928546));
#26837=CARTESIAN_POINT('Ctrl Pts',(131.005648120923,-38.2430996373723,24.2650188323532));
#26838=CARTESIAN_POINT('Ctrl Pts',(130.815989725741,-38.295934006517,24.2522227774963));
#26839=CARTESIAN_POINT('Ctrl Pts',(130.436596013824,-38.3668506153915,24.22746015288));
#26840=CARTESIAN_POINT('Ctrl Pts',(130.247752227897,-38.3859911698679,24.2155250057647));
#26841=CARTESIAN_POINT('Ctrl Pts',(130.013594167302,-38.3900172877107,24.2013666171102));
#26842=CARTESIAN_POINT('Ctrl Pts',(129.968901205641,-38.3899019400603,24.1986914613154));
#26843=CARTESIAN_POINT('Ctrl Pts',(129.895811383336,-38.3882676041646,24.194359290837));
#26844=CARTESIAN_POINT('Ctrl Pts',(129.867409328543,-38.3872750718854,24.19268638746));
#26845=CARTESIAN_POINT('Ctrl Pts',(129.812067007864,-38.3846439238437,24.1894462423995));
#26846=CARTESIAN_POINT('Ctrl Pts',(129.78512728165,-38.383040507796,24.1878780440071));
#26847=CARTESIAN_POINT('Ctrl Pts',(129.721087736956,-38.3784608990628,24.1841703699146));
#26848=CARTESIAN_POINT('Ctrl Pts',(129.684011738647,-38.3751950566755,24.1820399390979));
#26849=CARTESIAN_POINT('Ctrl Pts',(129.558351692207,-38.3620374467854,24.1748675314108));
#26850=CARTESIAN_POINT('Ctrl Pts',(129.470103729425,-38.3492627171622,24.1699131452475));
#26851=CARTESIAN_POINT('Ctrl Pts',(129.116415008417,-38.2837311780441,24.1502346186156));
#26852=CARTESIAN_POINT('Ctrl Pts',(128.857250454102,-38.2027686380154,24.136305727162));
#26853=CARTESIAN_POINT('Ctrl Pts',(128.550083629725,-38.0647236722473,24.1180690686392));
#26854=CARTESIAN_POINT('Ctrl Pts',(128.490504203096,-38.035821179182,24.114439550148));
#26855=CARTESIAN_POINT('Ctrl Pts',(128.391938754509,-37.9843871964846,24.1082179562922));
#26856=CARTESIAN_POINT('Ctrl Pts',(128.352485094035,-37.9627895879264,24.105666967951));
#26857=CARTESIAN_POINT('Ctrl Pts',(128.296350961136,-37.9305928932128,24.101932653028));
#26858=CARTESIAN_POINT('Ctrl Pts',(128.279313696641,-37.9206220840956,24.1007850558861));
#26859=CARTESIAN_POINT('Ctrl Pts',(128.249534572845,-37.9028432863217,24.0987523915376));
#26860=CARTESIAN_POINT('Ctrl Pts',(128.236755746736,-37.8950989702657,24.0978712751555));
#26861=CARTESIAN_POINT('Ctrl Pts',(128.208622689531,-37.8777942101719,24.0959114462088));
#26862=CARTESIAN_POINT('Ctrl Pts',(128.193293694891,-37.8681953349207,24.094830422724));
#26863=CARTESIAN_POINT('Ctrl Pts',(128.148705998996,-37.8397756721785,24.0916490542294));
#26864=CARTESIAN_POINT('Ctrl Pts',(128.119660164121,-37.8206271015588,24.0895295815972));
#26865=CARTESIAN_POINT('Ctrl Pts',(127.938696991767,-37.6972891528411,24.0760509020725));
#26866=CARTESIAN_POINT('Ctrl Pts',(127.795199817523,-37.5813146465733,24.064147854628));
#26867=CARTESIAN_POINT('Ctrl Pts',(127.546280292757,-37.344171767919,24.0419897502178));
#26868=CARTESIAN_POINT('Ctrl Pts',(127.438627527818,-37.2260414121756,24.0317521288504));
#26869=CARTESIAN_POINT('Ctrl Pts',(127.279996660215,-37.0251581944908,24.0157797971023));
#26870=CARTESIAN_POINT('Ctrl Pts',(127.223545049045,-36.9470450692669,24.0098734487436));
#26871=CARTESIAN_POINT('Ctrl Pts',(127.149901694267,-36.835413580024,24.0018452035483));
#26872=CARTESIAN_POINT('Ctrl Pts',(127.129827417018,-36.8038605472737,23.9996192278667));
#26873=CARTESIAN_POINT('Ctrl Pts',(127.096156422575,-36.7489503658316,23.9958177452791));
#26874=CARTESIAN_POINT('Ctrl Pts',(127.082309647367,-36.7257514228154,23.9942333238592));
#26875=CARTESIAN_POINT('Ctrl Pts',(127.054498125793,-36.6778641500091,23.9910058591832));
#26876=CARTESIAN_POINT('Ctrl Pts',(127.040562909077,-36.6531610849346,23.9893639531585));
#26877=CARTESIAN_POINT('Ctrl Pts',(127.005606757017,-36.5893351944016,23.9851784729584));
#26878=CARTESIAN_POINT('Ctrl Pts',(126.985041316327,-36.5499682727796,23.9826508294941));
#26879=CARTESIAN_POINT('Ctrl Pts',(126.890676103926,-36.3603423899407,23.9707124635746));
#26880=CARTESIAN_POINT('Ctrl Pts',(126.827297129446,-36.2051519913493,23.9616560414043));
#26881=CARTESIAN_POINT('Ctrl Pts',(126.716772248405,-35.8644194912719,23.9425605862669));
#26882=CARTESIAN_POINT('Ctrl Pts',(126.673334495947,-35.678303230035,23.9325962202296));
#26883=CARTESIAN_POINT('Ctrl Pts',(126.633472967456,-35.4051767320333,23.9175602303984));
#26884=CARTESIAN_POINT('Ctrl Pts',(126.624349200229,-35.3203933316099,23.9128332486971));
#26885=CARTESIAN_POINT('Ctrl Pts',(126.616713742662,-35.2106912823588,23.906540464242));
#26886=CARTESIAN_POINT('Ctrl Pts',(126.6152666468,-35.1860020620336,23.9051127202299));
#26887=CARTESIAN_POINT('Ctrl Pts',(126.613340081839,-35.1455607975624,23.902752056321));
#26888=CARTESIAN_POINT('Ctrl Pts',(126.612700055594,-35.1298168536005,23.9018275870525));
#26889=CARTESIAN_POINT('Ctrl Pts',(126.61169766522,-35.1000461078001,23.9000682245249));
#26890=CARTESIAN_POINT('Ctrl Pts',(126.611312582627,-35.0860203886457,23.8992346436669));
#26891=CARTESIAN_POINT('Ctrl Pts',(126.610508419963,-35.0481653627905,23.8969728779139));
#26892=CARTESIAN_POINT('Ctrl Pts',(126.610253568687,-35.0243338132724,23.8955362101897));
#26893=CARTESIAN_POINT('Ctrl Pts',(126.610238801731,-34.924681597953,23.8894808002329));
#26894=CARTESIAN_POINT('Ctrl Pts',(126.612771476117,-34.8488871420349,23.8847594083724));
#26895=CARTESIAN_POINT('Ctrl Pts',(126.627938209812,-34.6226659146988,23.870439178431));
#26896=CARTESIAN_POINT('Ctrl Pts',(126.64807845332,-34.4729315193651,23.8606648240289));
#26897=CARTESIAN_POINT('Ctrl Pts',(126.712848075336,-34.154161297163,23.8397259590213));
#26898=CARTESIAN_POINT('Ctrl Pts',(126.760697730583,-33.9862362059936,23.8286213181425));
#26899=CARTESIAN_POINT('Ctrl Pts',(126.821241884814,-33.8227566489294,23.8178897147877));
#26900=CARTESIAN_POINT('',(126.610251398414,-35.0029526077136,24.2343658980132));
#26901=CARTESIAN_POINT('Ctrl Pts',(126.821241975209,-33.8227564048483,24.1659080048185));
#26902=CARTESIAN_POINT('Ctrl Pts',(126.807344274267,-33.8602825622005,24.168379675193));
#26903=CARTESIAN_POINT('Ctrl Pts',(126.794107430046,-33.8980646848755,24.1708330162916));
#26904=CARTESIAN_POINT('Ctrl Pts',(126.765504500368,-33.984591761951,24.1763714619477));
#26905=CARTESIAN_POINT('Ctrl Pts',(126.750567979835,-34.0334561579263,24.1794422012933));
#26906=CARTESIAN_POINT('Ctrl Pts',(126.728693599679,-34.1112684560801,24.1842446403351));
#26907=CARTESIAN_POINT('Ctrl Pts',(126.721022952137,-34.1400006244833,24.1859993724584));
#26908=CARTESIAN_POINT('Ctrl Pts',(126.707220319802,-34.1945733341013,24.18929825462));
#26909=CARTESIAN_POINT('Ctrl Pts',(126.701012019139,-34.2203920872161,24.1908447176221));
#26910=CARTESIAN_POINT('Ctrl Pts',(126.687513281788,-34.2795811411885,24.1943586620257));
#26911=CARTESIAN_POINT('Ctrl Pts',(126.68042248472,-34.3129943001812,24.1963197433085));
#26912=CARTESIAN_POINT('Ctrl Pts',(126.666629190672,-34.3831999981619,24.200396128665));
#26913=CARTESIAN_POINT('Ctrl Pts',(126.660028074952,-34.4200078597816,24.2025081495119));
#26914=CARTESIAN_POINT('Ctrl Pts',(126.624735767856,-34.6374461818767,24.2148510598649));
#26915=CARTESIAN_POINT('Ctrl Pts',(126.610091916046,-34.8200503077089,24.2246539376064));
#26916=CARTESIAN_POINT('Ctrl Pts',(126.610251286801,-35.0029536196393,24.2343661467437));
#26917=CARTESIAN_POINT('Ctrl Pts',(126.610251285911,-35.0029525974854,24.2343660924671));
#26918=CARTESIAN_POINT('Ctrl Pts',(126.610436908779,-35.2160581364856,24.2456820473744));
#26919=CARTESIAN_POINT('Ctrl Pts',(126.630718128161,-35.4286581131638,24.256828764692));
#26920=CARTESIAN_POINT('Ctrl Pts',(126.679338029607,-35.6823917574262,24.2712824344637));
#26921=CARTESIAN_POINT('Ctrl Pts',(126.688746957028,-35.7266755192801,24.2738495722609));
#26922=CARTESIAN_POINT('Ctrl Pts',(126.703539186111,-35.790027097529,24.2776033371392));
#26923=CARTESIAN_POINT('Ctrl Pts',(126.70820759982,-35.809258589989,24.2787537191822));
#26924=CARTESIAN_POINT('Ctrl Pts',(126.716696964117,-35.8429410666196,24.2807893716379));
#26925=CARTESIAN_POINT('Ctrl Pts',(126.720445514594,-35.8574093727653,24.2816706474096));
#26926=CARTESIAN_POINT('Ctrl Pts',(126.728932152827,-35.8892952204943,24.283628383695));
#26927=CARTESIAN_POINT('Ctrl Pts',(126.733713681397,-35.9066997864303,24.2847071204101));
#26928=CARTESIAN_POINT('Ctrl Pts',(126.748366571423,-35.9584152443109,24.2879409581653));
#26929=CARTESIAN_POINT('Ctrl Pts',(126.758640964347,-35.9926082401722,24.2901166231013));
#26930=CARTESIAN_POINT('Ctrl Pts',(126.813623987023,-36.1656258332153,24.3012952896008));
#26931=CARTESIAN_POINT('Ctrl Pts',(126.866715971581,-36.3016144375825,24.310634954532));
#26932=CARTESIAN_POINT('Ctrl Pts',(127.007142546088,-36.6024585349234,24.33201609475));
#26933=CARTESIAN_POINT('Ctrl Pts',(127.09966384379,-36.7644062583769,24.3440425930186));
#26934=CARTESIAN_POINT('Ctrl Pts',(127.245174344422,-36.9764555324361,24.3601500718101));
#26935=CARTESIAN_POINT('Ctrl Pts',(127.287155274596,-37.0336950100936,24.3645411782755));
#26936=CARTESIAN_POINT('Ctrl Pts',(127.365224917559,-37.1334162901762,24.3722641494602));
#26937=CARTESIAN_POINT('Ctrl Pts',(127.400621643439,-37.1764047211051,24.3756192960652));
#26938=CARTESIAN_POINT('Ctrl Pts',(127.4571331044,-37.2416898593376,24.3807577874005));
#26939=CARTESIAN_POINT('Ctrl Pts',(127.477517480785,-37.2646031676762,24.3825699209641));
#26940=CARTESIAN_POINT('Ctrl Pts',(127.516045575909,-37.3067453557586,24.3859201979737));
#26941=CARTESIAN_POINT('Ctrl Pts',(127.5341085714,-37.3260445477324,24.3874615025292));
#26942=CARTESIAN_POINT('Ctrl Pts',(127.575048705052,-37.368773608732,24.3908910641822));
#26943=CARTESIAN_POINT('Ctrl Pts',(127.598043483406,-37.3920874131044,24.3927741151482));
#26944=CARTESIAN_POINT('Ctrl Pts',(127.668784765945,-37.4617613650883,24.3984418093849));
#26945=CARTESIAN_POINT('Ctrl Pts',(127.717563220923,-37.5070533783992,24.4021812866695));
#26946=CARTESIAN_POINT('Ctrl Pts',(127.994709762611,-37.7495927033872,24.4226007048005));
#26947=CARTESIAN_POINT('Ctrl Pts',(128.247267861713,-37.9170822870038,24.438074685957));
#26948=CARTESIAN_POINT('Ctrl Pts',(128.580138633457,-38.0788101621423,24.4580884341411));
#26949=CARTESIAN_POINT('Ctrl Pts',(128.642513248589,-38.1068162304265,24.4618306913904));
#26950=CARTESIAN_POINT('Ctrl Pts',(128.748207332888,-38.1504819626931,24.4682245354235));
#26951=CARTESIAN_POINT('Ctrl Pts',(128.791077272663,-38.1671796432037,24.4708320158464));
#26952=CARTESIAN_POINT('Ctrl Pts',(128.852969817343,-38.1898469155771,24.4746343234939));
#26953=CARTESIAN_POINT('Ctrl Pts',(128.871727626187,-38.1965298361735,24.4757916019916));
#26954=CARTESIAN_POINT('Ctrl Pts',(128.904675415796,-38.2079421462605,24.4778346895675));
#26955=CARTESIAN_POINT('Ctrl Pts',(128.918839524934,-38.2127434965227,24.4787163955311));
#26956=CARTESIAN_POINT('Ctrl Pts',(128.950082689076,-38.2231042910342,24.4806691102535));
#26957=CARTESIAN_POINT('Ctrl Pts',(128.967174210528,-38.2286217628435,24.4817423109499));
#26958=CARTESIAN_POINT('Ctrl Pts',(129.017936985997,-38.2445646445416,24.4849427891844));
#26959=CARTESIAN_POINT('Ctrl Pts',(129.051726924969,-38.2546006607534,24.4870900332582));
#26960=CARTESIAN_POINT('Ctrl Pts',(129.260748089142,-38.3131511867445,24.5004504183648));
#26961=CARTESIAN_POINT('Ctrl Pts',(129.439479775454,-38.3480250414412,24.5121927155569));
#26962=CARTESIAN_POINT('Ctrl Pts',(129.780321718107,-38.3864633883233,24.5343008154518));
#26963=CARTESIAN_POINT('Ctrl Pts',(129.941610093308,-38.393079903419,24.5446453280976));
#26964=CARTESIAN_POINT('Ctrl Pts',(130.199598421458,-38.3852548527202,24.5607553870761));
#26965=CARTESIAN_POINT('Ctrl Pts',(130.296265384888,-38.3781680730078,24.5666965482075));
#26966=CARTESIAN_POINT('Ctrl Pts',(130.429717795511,-38.3626108013519,24.5747627404839));
#26967=CARTESIAN_POINT('Ctrl Pts',(130.466858644995,-38.3576557238271,24.5769931711046));
#26968=CARTESIAN_POINT('Ctrl Pts',(130.530638399757,-38.3480678690337,24.5807998359523));
#26969=CARTESIAN_POINT('Ctrl Pts',(130.557317476455,-38.3437303809341,24.582385048631));
#26970=CARTESIAN_POINT('Ctrl Pts',(130.611856980228,-38.3341924288818,24.5856120503617));
#26971=CARTESIAN_POINT('Ctrl Pts',(130.639709824671,-38.328960727939,24.5872527286439));
#26972=CARTESIAN_POINT('Ctrl Pts',(130.710925686642,-38.3146571614297,24.5914307620992));
#26973=CARTESIAN_POINT('Ctrl Pts',(130.754183103735,-38.3050832865524,24.5939523013676));
#26974=CARTESIAN_POINT('Ctrl Pts',(130.956302146785,-38.2561745746636,24.60567449531));
#26975=CARTESIAN_POINT('Ctrl Pts',(131.112374188894,-38.2062155656347,24.6145382953326));
#26976=CARTESIAN_POINT('Ctrl Pts',(131.444234180228,-38.0728204255457,24.6336181954355));
#26977=CARTESIAN_POINT('Ctrl Pts',(131.617675828643,-37.9851558799842,24.643742371876));
#26978=CARTESIAN_POINT('Ctrl Pts',(131.855722522548,-37.837970750278,24.6589832866789));
#26979=CARTESIAN_POINT('Ctrl Pts',(131.927036456209,-37.7900380419107,24.6637449353574));
#26980=CARTESIAN_POINT('Ctrl Pts',(132.01648080816,-37.724853153555,24.6700777814639));
#26981=CARTESIAN_POINT('Ctrl Pts',(132.036352872599,-37.7100344019353,24.6715087414383));
#26982=CARTESIAN_POINT('Ctrl Pts',(132.068597202239,-37.6854346659395,24.6738733484276));
#26983=CARTESIAN_POINT('Ctrl Pts',(132.081067271454,-37.6757826374976,24.6747984894508));
#26984=CARTESIAN_POINT('Ctrl Pts',(132.104497549176,-37.6573843796994,24.6765579523125));
#26985=CARTESIAN_POINT('Ctrl Pts',(132.115471735024,-37.6486564516115,24.6773909484308));
#26986=CARTESIAN_POINT('Ctrl Pts',(132.144912126016,-37.624942402806,24.6796490180205));
#26987=CARTESIAN_POINT('Ctrl Pts',(132.163274940736,-37.6098299000797,24.6810825273098));
#26988=CARTESIAN_POINT('Ctrl Pts',(132.23430205968,-37.5501103188006,24.6867209725807));
#26989=CARTESIAN_POINT('Ctrl Pts',(132.285755218997,-37.5040946695482,24.6910092465469));
#26990=CARTESIAN_POINT('Ctrl Pts',(132.490152603477,-37.3097467928741,24.7087768763713));
#26991=CARTESIAN_POINT('Ctrl Pts',(132.630356267499,-37.1487244476289,24.7226868440036));
#26992=CARTESIAN_POINT('Ctrl Pts',(132.818737611109,-36.886071096317,24.7433266411604));
#26993=CARTESIAN_POINT('Ctrl Pts',(132.878555831865,-36.7934507277802,24.7502762127446));
#26994=CARTESIAN_POINT('Ctrl Pts',(132.971973488392,-36.6320532235835,24.761795943397));
#26995=CARTESIAN_POINT('Ctrl Pts',(133.007949488169,-36.5647572969367,24.7664376519188));
#26996=CARTESIAN_POINT('Ctrl Pts',(133.056823734463,-36.4654074726031,24.7730615990404));
#26997=CARTESIAN_POINT('Ctrl Pts',(133.071550122843,-36.4342839253048,24.7751052801298));
#26998=CARTESIAN_POINT('Ctrl Pts',(133.096802757864,-36.3787401695698,24.7786984590859));
#26999=CARTESIAN_POINT('Ctrl Pts',(133.10752046497,-36.354410719046,24.7802543177324));
#27000=CARTESIAN_POINT('Ctrl Pts',(133.129558762794,-36.302744142241,24.7835214811389));
#27001=CARTESIAN_POINT('Ctrl Pts',(133.140809930037,-36.2753797134425,24.785230367012));
#27002=CARTESIAN_POINT('Ctrl Pts',(133.170237565398,-36.201055413356,24.789816358468));
#27003=CARTESIAN_POINT('Ctrl Pts',(133.187728689355,-36.1538312258618,24.7926709342583));
#27004=CARTESIAN_POINT('Ctrl Pts',(133.288341765249,-35.8624092958261,24.809961079061));
#27005=CARTESIAN_POINT('Ctrl Pts',(133.344416872628,-35.6097770377765,24.8234833202264));
#27006=CARTESIAN_POINT('Ctrl Pts',(133.383194451374,-35.2396592722044,24.843261552494));
#27007=CARTESIAN_POINT('Ctrl Pts',(133.389346167686,-35.1255821806748,24.8493672058927));
#27008=CARTESIAN_POINT('Ctrl Pts',(133.389948327781,-34.9468387208198,24.8592218536625));
#27009=CARTESIAN_POINT('Ctrl Pts',(133.38832025085,-34.8822689723597,24.8628410605483));
#27010=CARTESIAN_POINT('Ctrl Pts',(133.383635962622,-34.7952509000251,24.8678444621272));
#27011=CARTESIAN_POINT('Ctrl Pts',(133.382197634648,-34.7727256666619,24.8691510549399));
#27012=CARTESIAN_POINT('Ctrl Pts',(133.379404898653,-34.7349290769522,24.8713651491035));
#27013=CARTESIAN_POINT('Ctrl Pts',(133.378171607038,-34.719649058839,24.8722662164328));
#27014=CARTESIAN_POINT('Ctrl Pts',(133.37538729903,-34.6878444364612,24.8741550497788));
#27015=CARTESIAN_POINT('Ctrl Pts',(133.373818514529,-34.6713221640996,24.8751436708627));
#27016=CARTESIAN_POINT('Ctrl Pts',(133.369211997512,-34.6263212130996,24.8778552538438));
#27017=CARTESIAN_POINT('Ctrl Pts',(133.365934628095,-34.5978690739955,24.8795903544918));
#27018=CARTESIAN_POINT('Ctrl Pts',(133.341066605702,-34.4036612151039,24.8915599551861));
#27019=CARTESIAN_POINT('Ctrl Pts',(133.307602806705,-34.2396713050136,24.9022858505088));
#27020=CARTESIAN_POINT('Ctrl Pts',(133.225082045367,-33.94743475074,24.921852633121));
#27021=CARTESIAN_POINT('Ctrl Pts',(133.180070812314,-33.8183907355127,24.9306636078335));
#27022=CARTESIAN_POINT('Ctrl Pts',(133.074268950022,-33.5653417371081,24.9480500195027));
#27023=CARTESIAN_POINT('Ctrl Pts',(133.013441517617,-33.4416189047824,24.9566063656474));
#27024=CARTESIAN_POINT('Ctrl Pts',(132.924580152183,-33.2856549758569,24.9674294865618));
#27025=CARTESIAN_POINT('Ctrl Pts',(132.903244286699,-33.2497655089816,24.9699234195639));
#27026=CARTESIAN_POINT('Ctrl Pts',(132.866592293773,-33.1906277679722,24.9740401973353));
#27027=CARTESIAN_POINT('Ctrl Pts',(132.851643500477,-33.1671583080248,24.9756759810408));
#27028=CARTESIAN_POINT('Ctrl Pts',(132.821594120495,-33.1212388382192,24.9788814389872));
#27029=CARTESIAN_POINT('Ctrl Pts',(132.806510407494,-33.0987803181955,24.9804515695561));
#27030=CARTESIAN_POINT('Ctrl Pts',(132.772485110212,-33.0494066604086,24.9839100793754));
#27031=CARTESIAN_POINT('Ctrl Pts',(132.753417030398,-33.0225817775156,24.9857935849184));
#27032=CARTESIAN_POINT('Ctrl Pts',(132.684874284082,-32.9290704242584,24.9923802708236));
#27033=CARTESIAN_POINT('Ctrl Pts',(132.633341511965,-32.8639257547196,24.9970059992321));
#27034=CARTESIAN_POINT('Ctrl Pts',(132.399444397277,-32.5895933458376,25.016784667415));
#27035=CARTESIAN_POINT('Ctrl Pts',(132.194194887457,-32.4013671084972,25.0310555234053));
#27036=CARTESIAN_POINT('Ctrl Pts',(131.913981377329,-32.2015122943597,25.0496878314616));
#27037=CARTESIAN_POINT('Ctrl Pts',(131.858522721635,-32.1643782775739,25.0533447439061));
#27038=CARTESIAN_POINT('Ctrl Pts',(131.763700145047,-32.1048640154398,25.0596082609953));
#27039=CARTESIAN_POINT('Ctrl Pts',(131.72491749436,-32.0815912208658,25.0621730545131));
#27040=CARTESIAN_POINT('Ctrl Pts',(131.668519435158,-32.0492646132009,25.0659239968495));
#27041=CARTESIAN_POINT('Ctrl Pts',(131.651270674401,-32.0395774714856,25.0670739757018));
#27042=CARTESIAN_POINT('Ctrl Pts',(131.620843336266,-32.0228377050667,25.0691091952802));
#27043=CARTESIAN_POINT('Ctrl Pts',(131.607701369389,-32.0157203974954,25.0699904477118));
#27044=CARTESIAN_POINT('Ctrl Pts',(131.578579657438,-32.0001971218945,25.0719484855451));
#27045=CARTESIAN_POINT('Ctrl Pts',(131.562579757073,-31.9918318675765,25.0730275521562));
#27046=CARTESIAN_POINT('Ctrl Pts',(131.515691762351,-31.9677923402809,25.0761976641346));
#27047=CARTESIAN_POINT('Ctrl Pts',(131.484630182155,-31.9524636453704,25.0783076441454));
#27048=CARTESIAN_POINT('Ctrl Pts',(131.284132859435,-31.8573120526994,25.0919648560047));
#27049=CARTESIAN_POINT('Ctrl Pts',(131.108573072493,-31.7911776983037,25.1040752045084));
#27050=CARTESIAN_POINT('Ctrl Pts',(130.776820086821,-31.6966960226035,25.1263051174737));
#27051=CARTESIAN_POINT('Ctrl Pts',(130.622334867936,-31.6641382866081,25.1364127535991));
#27052=CARTESIAN_POINT('Ctrl Pts',(130.371391545657,-31.6292994034178,25.152217049404));
#27053=CARTESIAN_POINT('Ctrl Pts',(130.276128787727,-31.6201612841146,25.1580805728196));
#27054=CARTESIAN_POINT('Ctrl Pts',(130.143348421782,-31.6130769276361,25.1660620960981));
#27055=CARTESIAN_POINT('Ctrl Pts',(130.106065846671,-31.6117044297849,25.1682825608067));
#27056=CARTESIAN_POINT('Ctrl Pts',(130.041771982493,-31.6103998468723,25.1720776447012));
#27057=CARTESIAN_POINT('Ctrl Pts',(130.01477076835,-31.610174638156,25.1736610993292));
#27058=CARTESIAN_POINT('Ctrl Pts',(129.959379982093,-31.610374499745,25.1768891850223));
#27059=CARTESIAN_POINT('Ctrl Pts',(129.930992620713,-31.610833572886,25.1785326457682));
#27060=CARTESIAN_POINT('Ctrl Pts',(129.858083340608,-31.6129290946049,25.1827275098656));
#27061=CARTESIAN_POINT('Ctrl Pts',(129.813581149839,-31.6150867177881,25.1852628376556));
#27062=CARTESIAN_POINT('Ctrl Pts',(129.596223322366,-31.629924850698,25.1975409740153));
#27063=CARTESIAN_POINT('Ctrl Pts',(129.424465534204,-31.6549721786094,25.2069008791239));
#27064=CARTESIAN_POINT('Ctrl Pts',(129.098110558649,-31.7284587366632,25.2247156401648));
#27065=CARTESIAN_POINT('Ctrl Pts',(128.943590608699,-31.7750375258261,25.2331693424943));
#27066=CARTESIAN_POINT('Ctrl Pts',(128.726189794318,-31.8578795882111,25.2457275605851));
#27067=CARTESIAN_POINT('Ctrl Pts',(128.660228530845,-31.8854335000244,25.2496323604552));
#27068=CARTESIAN_POINT('Ctrl Pts',(128.551996450094,-31.9347196780033,25.2562732651985));
#27069=CARTESIAN_POINT('Ctrl Pts',(128.509221941368,-31.9552934379189,25.2589607293781));
#27070=CARTESIAN_POINT('Ctrl Pts',(128.448922566152,-31.9858716083388,25.2628591117792));
#27071=CARTESIAN_POINT('Ctrl Pts',(128.431031519794,-31.995145755242,25.2640298306471));
#27072=CARTESIAN_POINT('Ctrl Pts',(128.399989054328,-32.0115899916525,25.2660875674119));
#27073=CARTESIAN_POINT('Ctrl Pts',(128.386800772914,-32.018688602625,25.2669702711297));
#27074=CARTESIAN_POINT('Ctrl Pts',(128.35804650642,-32.0344122935125,25.2689139020258));
#27075=CARTESIAN_POINT('Ctrl Pts',(128.342501352489,-32.0430725537307,25.2699768640977));
#27076=CARTESIAN_POINT('Ctrl Pts',(128.297975204728,-32.0683396623369,25.273055167941));
#27077=CARTESIAN_POINT('Ctrl Pts',(128.269171318839,-32.0852525606394,25.275087904618));
#27078=CARTESIAN_POINT('Ctrl Pts',(128.024560012043,-32.2337862826416,25.2926777341158));
#27079=CARTESIAN_POINT('Ctrl Pts',(127.823859975425,-32.388734247844,25.3092496628992));
#27080=CARTESIAN_POINT('Ctrl Pts',(127.558345411499,-32.6457766427049,25.3328979198023));
#27081=CARTESIAN_POINT('Ctrl Pts',(127.478684074648,-32.731296726382,25.3402832421547));
#27082=CARTESIAN_POINT('Ctrl Pts',(127.352597774039,-32.8815198785215,25.3524186652358));
#27083=CARTESIAN_POINT('Ctrl Pts',(127.30374974135,-32.9440494506282,25.357251122086));
#27084=CARTESIAN_POINT('Ctrl Pts',(127.23661886655,-33.0364956829248,25.3640902712282));
#27085=CARTESIAN_POINT('Ctrl Pts',(127.216537573947,-33.0650680757396,25.3661641698332));
#27086=CARTESIAN_POINT('Ctrl Pts',(127.181918826337,-33.1159794398359,25.3697912596576));
#27087=CARTESIAN_POINT('Ctrl Pts',(127.167196842172,-33.1381887040619,25.3713512277966));
#27088=CARTESIAN_POINT('Ctrl Pts',(127.136820122179,-33.1852089601518,25.3746084524684));
#27089=CARTESIAN_POINT('Ctrl Pts',(127.121222471287,-33.2100543166143,25.3763035354955));
#27090=CARTESIAN_POINT('Ctrl Pts',(127.080368775087,-33.277045452513,25.3808072147052));
#27091=CARTESIAN_POINT('Ctrl Pts',(127.05570273539,-33.3195438646867,25.3835947092113));
#27092=CARTESIAN_POINT('Ctrl Pts',(126.95028996597,-33.5106161476536,25.3958450224807));
#27093=CARTESIAN_POINT('Ctrl Pts',(126.879871394148,-33.6644469814127,25.4049493855538));
#27094=CARTESIAN_POINT('Ctrl Pts',(126.82124193643,-33.822756509559,25.4139334024237));
#27095=CARTESIAN_POINT('Origin',(130.,-35.,23.));
#27096=CARTESIAN_POINT('',(126.821241917671,-33.8227565602112,26.6607167036746));
#27097=CARTESIAN_POINT('',(126.821241846765,-33.8227567516686,26.3195780637354));
#27098=CARTESIAN_POINT('',(126.821241915871,-33.8227565650715,23.));
#27099=CARTESIAN_POINT('',(126.61025105039,-34.9973314581693,25.1397298775655));
#27100=CARTESIAN_POINT('Ctrl Pts',(126.821241846765,-33.8227567516686,26.3195780637354));
#27101=CARTESIAN_POINT('Ctrl Pts',(126.872641896856,-33.6839678237783,26.3116709482775));
#27102=CARTESIAN_POINT('Ctrl Pts',(126.933097475216,-33.5486368529399,26.3038949810359));
#27103=CARTESIAN_POINT('Ctrl Pts',(127.064470118871,-33.2997532174182,26.2888430489513));
#27104=CARTESIAN_POINT('Ctrl Pts',(127.13359097118,-33.1856496796866,26.2816081180484));
#27105=CARTESIAN_POINT('Ctrl Pts',(127.225173164613,-33.0528151267007,26.2724174983671));
#27106=CARTESIAN_POINT('Ctrl Pts',(127.241391093988,-33.0299061716714,26.2708030971816));
#27107=CARTESIAN_POINT('Ctrl Pts',(127.26757610129,-32.9938753525737,26.2682124992475));
#27108=CARTESIAN_POINT('Ctrl Pts',(127.277357937171,-32.9806197395715,26.2672481463267));
#27109=CARTESIAN_POINT('Ctrl Pts',(127.296466445943,-32.9551165399456,26.2653697269105));
#27110=CARTESIAN_POINT('Ctrl Pts',(127.305780551951,-32.9428603414275,26.2644564624457));
#27111=CARTESIAN_POINT('Ctrl Pts',(127.329168992009,-32.9125153694444,26.2621697457715));
#27112=CARTESIAN_POINT('Ctrl Pts',(127.343343799958,-32.8945052534146,26.2607896789041));
#27113=CARTESIAN_POINT('Ctrl Pts',(127.399973941049,-32.8240349162805,26.2553033936031));
#27114=CARTESIAN_POINT('Ctrl Pts',(127.443806997026,-32.7727066538227,26.2511162532689));
#27115=CARTESIAN_POINT('Ctrl Pts',(127.571665839718,-32.6317330599146,26.2391429971847));
#27116=CARTESIAN_POINT('Ctrl Pts',(127.659073905266,-32.5452988957365,26.2312338308905));
#27117=CARTESIAN_POINT('Ctrl Pts',(127.932361624292,-32.3029553962049,26.2076894962586));
#27118=CARTESIAN_POINT('Ctrl Pts',(128.130507823779,-32.1620057896263,26.1921534497731));
#27119=CARTESIAN_POINT('Ctrl Pts',(128.386902966921,-32.0182269213214,26.1742752335936));
#27120=CARTESIAN_POINT('Ctrl Pts',(128.43235239155,-31.994083477423,26.1711802157235));
#27121=CARTESIAN_POINT('Ctrl Pts',(128.505227863689,-31.9574735806384,26.166331559897));
#27122=CARTESIAN_POINT('Ctrl Pts',(128.532299237725,-31.9443224463463,26.1645546933086));
#27123=CARTESIAN_POINT('Ctrl Pts',(128.581126425488,-31.9214010727991,26.1613920947902));
#27124=CARTESIAN_POINT('Ctrl Pts',(128.602816715877,-31.9114967235814,26.1600018822684));
#27125=CARTESIAN_POINT('Ctrl Pts',(128.654075351643,-31.8887412183173,26.1567500320226));
#27126=CARTESIAN_POINT('Ctrl Pts',(128.683726379171,-31.876081271332,26.1548948999792));
#27127=CARTESIAN_POINT('Ctrl Pts',(128.772584788656,-31.8396316836202,26.1494086693622));
#27128=CARTESIAN_POINT('Ctrl Pts',(128.832289555741,-31.8170879635669,26.1458184115659));
#27129=CARTESIAN_POINT('Ctrl Pts',(129.048072915008,-31.7425008865129,26.133137551249));
#27130=CARTESIAN_POINT('Ctrl Pts',(129.207262065151,-31.7001457085345,26.1243371640464));
#27131=CARTESIAN_POINT('Ctrl Pts',(129.576727174316,-31.6301356227021,26.1043737983293));
#27132=CARTESIAN_POINT('Ctrl Pts',(129.787758316995,-31.6102976643573,26.0933029327255));
#27133=CARTESIAN_POINT('Ctrl Pts',(130.043951014271,-31.6102400261106,26.0789629364333));
#27134=CARTESIAN_POINT('Ctrl Pts',(130.088658298929,-31.6111146840661,26.0764263702882));
#27135=CARTESIAN_POINT('Ctrl Pts',(130.152805593533,-31.613639817594,26.0727214602308));
#27136=CARTESIAN_POINT('Ctrl Pts',(130.172270775874,-31.6145742402129,26.0715885649613));
#27137=CARTESIAN_POINT('Ctrl Pts',(130.206651730642,-31.6165219658253,26.0695705714045));
#27138=CARTESIAN_POINT('Ctrl Pts',(130.221570520848,-31.6174661807976,26.0686891822981));
#27139=CARTESIAN_POINT('Ctrl Pts',(130.254463019463,-31.6197665029575,26.0667328999854));
#27140=CARTESIAN_POINT('Ctrl Pts',(130.272432231053,-31.6211672769704,26.0656557547198));
#27141=CARTESIAN_POINT('Ctrl Pts',(130.325829951156,-31.625758566004,26.0624315179375));
#27142=CARTESIAN_POINT('Ctrl Pts',(130.361219290762,-31.6293634399044,26.0602640352331));
#27143=CARTESIAN_POINT('Ctrl Pts',(130.537598092024,-31.6501394461733,26.0493296501669));
#27144=CARTESIAN_POINT('Ctrl Pts',(130.677457965805,-31.6756020497781,26.0402434210629));
#27145=CARTESIAN_POINT('Ctrl Pts',(131.082481233426,-31.7759636241809,26.013379422321));
#27146=CARTESIAN_POINT('Ctrl Pts',(131.340658093015,-31.8744821345834,25.9956387661412));
#27147=CARTESIAN_POINT('Ctrl Pts',(131.626496728509,-32.0255734220944,25.976038353868));
#27148=CARTESIAN_POINT('Ctrl Pts',(131.668417347394,-32.048883434574,25.973161199341));
#27149=CARTESIAN_POINT('Ctrl Pts',(131.73495049132,-32.0877503226696,25.9685886514542));
#27150=CARTESIAN_POINT('Ctrl Pts',(131.759880726629,-32.1027476296637,25.966873845163));
#27151=CARTESIAN_POINT('Ctrl Pts',(131.807327002476,-32.1321283534849,25.9636064649977));
#27152=CARTESIAN_POINT('Ctrl Pts',(131.829872018882,-32.1464605961522,25.9620522088917));
#27153=CARTESIAN_POINT('Ctrl Pts',(131.881927614971,-32.1804238689389,25.9584582225732));
#27154=CARTESIAN_POINT('Ctrl Pts',(131.9113047065,-32.2002543757691,25.9564259898748));
#27155=CARTESIAN_POINT('Ctrl Pts',(132.008132127398,-32.2678505364383,25.9497086975587));
#27156=CARTESIAN_POINT('Ctrl Pts',(132.074148411893,-32.3176232250213,25.9450983415721));
#27157=CARTESIAN_POINT('Ctrl Pts',(132.23475817385,-32.4481928430184,25.9337285281904));
#27158=CARTESIAN_POINT('Ctrl Pts',(132.326848966293,-32.5318751176796,25.9270690867836));
#27159=CARTESIAN_POINT('Ctrl Pts',(132.548147210143,-32.7563882352958,25.91031167277));
#27160=CARTESIAN_POINT('Ctrl Pts',(132.670423627442,-32.9034131784751,25.9003206459875));
#27161=CARTESIAN_POINT('Ctrl Pts',(132.818660588792,-33.1158027922413,25.8860841678037));
#27162=CARTESIAN_POINT('Ctrl Pts',(132.855957423047,-33.1728293435759,25.8822769506339));
#27163=CARTESIAN_POINT('Ctrl Pts',(132.903863713192,-33.2511314865916,25.877015743733));
#27164=CARTESIAN_POINT('Ctrl Pts',(132.916006803609,-33.2714544276159,25.8756472564802));
#27165=CARTESIAN_POINT('Ctrl Pts',(132.934991466135,-33.3039969862346,25.8734485363741));
#27166=CARTESIAN_POINT('Ctrl Pts',(132.941972125748,-33.3161350633563,25.8726268169666));
#27167=CARTESIAN_POINT('Ctrl Pts',(132.956666799108,-33.342056698505,25.8708678041221));
#27168=CARTESIAN_POINT('Ctrl Pts',(132.964360024048,-33.3558515349639,25.8699291995874));
#27169=CARTESIAN_POINT('Ctrl Pts',(132.983937628066,-33.391540524465,25.8674954835977));
#27170=CARTESIAN_POINT('Ctrl Pts',(132.995677373985,-33.413512482222,25.8659919482933));
#27171=CARTESIAN_POINT('Ctrl Pts',(133.047471513738,-33.5130746602782,25.8591622912028));
#27172=CARTESIAN_POINT('Ctrl Pts',(133.084758293183,-33.5920605612015,25.8536996380028));
#27173=CARTESIAN_POINT('Ctrl Pts',(133.197750322388,-33.8575126747524,25.8353926787601));
#27174=CARTESIAN_POINT('Ctrl Pts',(133.259911396775,-34.0492819644057,25.8222756581342));
#27175=CARTESIAN_POINT('Ctrl Pts',(133.339300697521,-34.3969760994267,25.799544777836));
#27176=CARTESIAN_POINT('Ctrl Pts',(133.363441043687,-34.5507319297071,25.7898326576385));
#27177=CARTESIAN_POINT('Ctrl Pts',(133.380761554616,-34.7494214907845,25.7777827414339));
#27178=CARTESIAN_POINT('Ctrl Pts',(133.383727489832,-34.7932953183525,25.7751519298529));
#27179=CARTESIAN_POINT('Ctrl Pts',(133.387196737493,-34.8654542344397,25.7708725235286));
#27180=CARTESIAN_POINT('Ctrl Pts',(133.388201083338,-34.893708924528,25.7692087800152));
#27181=CARTESIAN_POINT('Ctrl Pts',(133.389474857267,-34.9490315743568,25.7659734802388));
#27182=CARTESIAN_POINT('Ctrl Pts',(133.389773780234,-34.9760966626119,25.764401138764));
#27183=CARTESIAN_POINT('Ctrl Pts',(133.389713358641,-35.0408493910121,25.7606628942086));
#27184=CARTESIAN_POINT('Ctrl Pts',(133.389049714405,-35.0785335624023,25.75850645419));
#27185=CARTESIAN_POINT('Ctrl Pts',(133.384378890436,-35.2147093735066,25.7507755481));
#27186=CARTESIAN_POINT('Ctrl Pts',(133.376704821279,-35.3130295338046,25.7453121235378));
#27187=CARTESIAN_POINT('Ctrl Pts',(133.344606796192,-35.5758836534239,25.7308795366582));
#27188=CARTESIAN_POINT('Ctrl Pts',(133.31234735193,-35.7391851584835,25.7221063009621));
#27189=CARTESIAN_POINT('Ctrl Pts',(133.222074825556,-36.0671943225409,25.7040584589812));
#27190=CARTESIAN_POINT('Ctrl Pts',(133.163073370296,-36.2311069985198,25.6948028366459));
#27191=CARTESIAN_POINT('Ctrl Pts',(133.077155047246,-36.422248743592,25.6829698820208));
#27192=CARTESIAN_POINT('Ctrl Pts',(133.062035677305,-36.4545143429691,25.6809346394649));
#27193=CARTESIAN_POINT('Ctrl Pts',(133.038501848042,-36.5027431138328,25.6778264552161));
#27194=CARTESIAN_POINT('Ctrl Pts',(133.030463491483,-36.5188881926641,25.6767746393246));
#27195=CARTESIAN_POINT('Ctrl Pts',(133.015527904107,-36.5482958286826,25.6748366393828));
#27196=CARTESIAN_POINT('Ctrl Pts',(133.008671241512,-36.5615779991443,25.6739528607498));
#27197=CARTESIAN_POINT('Ctrl Pts',(132.992524138716,-36.5923557180179,25.6718853637653));
#27198=CARTESIAN_POINT('Ctrl Pts',(132.983167970902,-36.6098156009669,25.670697773503));
#27199=CARTESIAN_POINT('Ctrl Pts',(132.951874885448,-36.66700306412,25.6667618066143));
#27200=CARTESIAN_POINT('Ctrl Pts',(132.929294007879,-36.7063706360173,25.6639783386855));
#27201=CARTESIAN_POINT('Ctrl Pts',(132.871407254879,-36.8027538960762,25.6570000068675));
#27202=CARTESIAN_POINT('Ctrl Pts',(132.835187255167,-36.8591970183983,25.6527676909545));
#27203=CARTESIAN_POINT('Ctrl Pts',(132.638126155383,-37.1471235644097,25.6305395744156));
#27204=CARTESIAN_POINT('Ctrl Pts',(132.450512860566,-37.3589983418362,25.6120928473726));
#27205=CARTESIAN_POINT('Ctrl Pts',(132.178893386909,-37.5979223458838,25.5896843228841));
#27206=CARTESIAN_POINT('Ctrl Pts',(132.11711062319,-37.6485129955901,25.5848154736091));
#27207=CARTESIAN_POINT('Ctrl Pts',(132.02790930571,-37.7164372301631,25.5780964472045));
#27208=CARTESIAN_POINT('Ctrl Pts',(132.001944748504,-37.7356287594849,25.5761757371733));
#27209=CARTESIAN_POINT('Ctrl Pts',(131.95385080078,-37.7701255791025,25.57268060927));
#27210=CARTESIAN_POINT('Ctrl Pts',(131.931806011754,-37.7855438016303,25.5711020002461));
#27211=CARTESIAN_POINT('Ctrl Pts',(131.886414002077,-37.8164931018334,25.5678980516255));
#27212=CARTESIAN_POINT('Ctrl Pts',(131.86305290564,-37.8320001976431,25.566273683678));
#27213=CARTESIAN_POINT('Ctrl Pts',(131.803536961595,-37.8704516787979,25.5621951352898));
#27214=CARTESIAN_POINT('Ctrl Pts',(131.767134263767,-37.8930045173811,25.5597552639241));
#27215=CARTESIAN_POINT('Ctrl Pts',(131.599397881863,-37.9925757431818,25.5487446477152));
#27216=CARTESIAN_POINT('Ctrl Pts',(131.463389495656,-38.0613855047465,25.5404629722138));
#27217=CARTESIAN_POINT('Ctrl Pts',(131.280208020721,-38.139052949277,25.5298183173276));
#27218=CARTESIAN_POINT('Ctrl Pts',(131.236840002805,-38.156392385583,25.5273328398893));
#27219=CARTESIAN_POINT('Ctrl Pts',(131.000206013559,-38.2453774246887,25.5139075857791));
#27220=CARTESIAN_POINT('Ctrl Pts',(130.801087671491,-38.3001712553871,25.5031209759358));
#27221=CARTESIAN_POINT('Ctrl Pts',(130.549510224445,-38.3452795554704,25.4888867510208));
#27222=CARTESIAN_POINT('Ctrl Pts',(130.500589435965,-38.3529489248003,25.4860899342451));
#27223=CARTESIAN_POINT('Ctrl Pts',(130.432615073598,-38.3620846430312,25.4821425964938));
#27224=CARTESIAN_POINT('Ctrl Pts',(130.413688609792,-38.364465878408,25.4810369740353));
#27225=CARTESIAN_POINT('Ctrl Pts',(130.379632988619,-38.3684588944788,25.4790342045704));
#27226=CARTESIAN_POINT('Ctrl Pts',(130.364510881969,-38.3701288313052,25.4781401594019));
#27227=CARTESIAN_POINT('Ctrl Pts',(130.332991860657,-38.373394859023,25.4762659897216));
#27228=CARTESIAN_POINT('Ctrl Pts',(130.316593843099,-38.3749732988077,25.4752850075943));
#27229=CARTESIAN_POINT('Ctrl Pts',(130.272228509807,-38.3789176468158,25.4726160941092));
#27230=CARTESIAN_POINT('Ctrl Pts',(130.244242845664,-38.3810557739627,25.4709166274426));
#27231=CARTESIAN_POINT('Ctrl Pts',(130.071585019871,-38.3920922331794,25.4603468307246));
#27232=CARTESIAN_POINT('Ctrl Pts',(129.926503670802,-38.3920502235697,25.4511040990249));
#27233=CARTESIAN_POINT('Ctrl Pts',(129.533170004118,-38.3666884914843,25.4257534726648));
#27234=CARTESIAN_POINT('Ctrl Pts',(129.286944170252,-38.3232671306737,25.4096260701744));
#27235=CARTESIAN_POINT('Ctrl Pts',(128.981116253666,-38.2337428355661,25.3900195338736));
#27236=CARTESIAN_POINT('Ctrl Pts',(128.915153730744,-38.2122151910756,25.3858112077257));
#27237=CARTESIAN_POINT('Ctrl Pts',(128.818617880988,-38.1773962360449,25.3796809771827));
#27238=CARTESIAN_POINT('Ctrl Pts',(128.787508108005,-38.165655395324,25.3777098414903));
#27239=CARTESIAN_POINT('Ctrl Pts',(128.731952973321,-38.1437497222584,25.374196584072));
#27240=CARTESIAN_POINT('Ctrl Pts',(128.70744474499,-38.1337527901405,25.3726490947544));
#27241=CARTESIAN_POINT('Ctrl Pts',(128.655135577234,-38.1116977441667,25.3693503150698));
#27242=CARTESIAN_POINT('Ctrl Pts',(128.62737403661,-38.0995517768112,25.367602111026));
#27243=CARTESIAN_POINT('Ctrl Pts',(128.550732498311,-38.0647886014754,25.3627802649627));
#27244=CARTESIAN_POINT('Ctrl Pts',(128.502221982979,-38.041375826811,25.3597334638496));
#27245=CARTESIAN_POINT('Ctrl Pts',(128.291878573805,-37.933603155817,25.346514604831));
#27246=CARTESIAN_POINT('Ctrl Pts',(128.136447880491,-37.8374087380429,25.3367462433169));
#27247=CARTESIAN_POINT('Ctrl Pts',(127.817084479054,-37.6021428356282,25.3156905409571));
#27248=CARTESIAN_POINT('Ctrl Pts',(127.65710613106,-37.4590846297011,25.3044810377785));
#27249=CARTESIAN_POINT('Ctrl Pts',(127.483221020712,-37.271120485721,25.2901125714594));
#27250=CARTESIAN_POINT('Ctrl Pts',(127.455310362949,-37.2398033422622,25.2877282205396));
#27251=CARTESIAN_POINT('Ctrl Pts',(127.415472560754,-37.1933974190403,25.2841951278275));
#27252=CARTESIAN_POINT('Ctrl Pts',(127.403080300457,-37.1787111691146,25.2830770027148));
#27253=CARTESIAN_POINT('Ctrl Pts',(127.381292617278,-37.1524402806168,25.2810752821355));
#27254=CARTESIAN_POINT('Ctrl Pts',(127.371847779662,-37.1408978043242,25.2801951712567));
#27255=CARTESIAN_POINT('Ctrl Pts',(127.350848889111,-37.1148868195185,25.2782102224457));
#27256=CARTESIAN_POINT('Ctrl Pts',(127.339337091931,-37.1003858509212,25.2771026760653));
#27257=CARTESIAN_POINT('Ctrl Pts',(127.304488491964,-37.0557421895858,25.2736919179755));
#27258=CARTESIAN_POINT('Ctrl Pts',(127.281541624904,-37.0253004817645,25.2713648353679));
#27259=CARTESIAN_POINT('Ctrl Pts',(127.22812133883,-36.9518883980091,25.2657622338185));
#27260=CARTESIAN_POINT('Ctrl Pts',(127.198126974572,-36.908582371011,25.2624646658873));
#27261=CARTESIAN_POINT('Ctrl Pts',(127.105441547351,-36.7678666961246,25.25181438779));
#27262=CARTESIAN_POINT('Ctrl Pts',(127.04672991839,-36.6679374232611,25.2443498360029));
#27263=CARTESIAN_POINT('Ctrl Pts',(126.889102808978,-36.365136342913,25.2223446256813));
#27264=CARTESIAN_POINT('Ctrl Pts',(126.805169692314,-36.1551469310553,25.2078959013107));
#27265=CARTESIAN_POINT('Ctrl Pts',(126.728060203813,-35.8874784752449,25.190873112828));
#27266=CARTESIAN_POINT('Ctrl Pts',(126.714597682359,-35.8362656003739,25.1876734303632));
#27267=CARTESIAN_POINT('Ctrl Pts',(126.694675858038,-35.7525511772749,25.1825340661964));
#27268=CARTESIAN_POINT('Ctrl Pts',(126.687483913848,-35.7202348599203,25.1805718226491));
#27269=CARTESIAN_POINT('Ctrl Pts',(126.675398087947,-35.6619117131779,25.177068185866));
#27270=CARTESIAN_POINT('Ctrl Pts',(126.670333204605,-35.6359434567092,25.1755215465766));
#27271=CARTESIAN_POINT('Ctrl Pts',(126.661092781109,-35.585425978005,25.1725376881475));
#27272=CARTESIAN_POINT('Ctrl Pts',(126.656882713319,-35.5608848788984,25.1710994834994));
#27273=CARTESIAN_POINT('Ctrl Pts',(126.648205463771,-35.5067299420334,25.1679495856491));
#27274=CARTESIAN_POINT('Ctrl Pts',(126.643859535123,-35.4770986343486,25.1662416958792));
#27275=CARTESIAN_POINT('Ctrl Pts',(126.632370063276,-35.39081213588,25.1613104073976));
#27276=CARTESIAN_POINT('Ctrl Pts',(126.626264485296,-35.3340279736208,25.1581178992765));
#27277=CARTESIAN_POINT('Ctrl Pts',(126.613962667415,-35.18405197675,25.1497989695217));
#27278=CARTESIAN_POINT('Ctrl Pts',(126.610177537892,-35.0907116357337,25.1447368543743));
#27279=CARTESIAN_POINT('Ctrl Pts',(126.61025105039,-34.9973314581693,25.1397298775655));
#27280=CARTESIAN_POINT('Ctrl Pts',(126.610251047991,-34.9973345073913,25.1397300410625));
#27281=CARTESIAN_POINT('Ctrl Pts',(126.610442852642,-34.7534135092292,25.1266511724115));
#27282=CARTESIAN_POINT('Ctrl Pts',(126.636961587853,-34.5102363678044,25.1140470393936));
#27283=CARTESIAN_POINT('Ctrl Pts',(126.703286733997,-34.2086073460077,25.0970240520163));
#27284=CARTESIAN_POINT('Ctrl Pts',(126.719048765736,-34.1456121463358,25.0933861108642));
#27285=CARTESIAN_POINT('Ctrl Pts',(126.742725428392,-34.0613420215835,25.0883607212718));
#27286=CARTESIAN_POINT('Ctrl Pts',(126.749059650024,-34.0396338110871,25.0870517513496));
#27287=CARTESIAN_POINT('Ctrl Pts',(126.76005363156,-34.0033115697369,25.0848348292149));
#27288=CARTESIAN_POINT('Ctrl Pts',(126.764596378906,-33.9886624206434,25.0839333494163));
#27289=CARTESIAN_POINT('Ctrl Pts',(126.774256935561,-33.9582410629125,25.0820450494289));
#27290=CARTESIAN_POINT('Ctrl Pts',(126.779391261301,-33.9424749045304,25.0810573909748));
#27291=CARTESIAN_POINT('Ctrl Pts',(126.793686010773,-33.8996492424574,25.0783511872542));
#27292=CARTESIAN_POINT('Ctrl Pts',(126.803072976973,-33.87266744937,25.0766205799485));
#27293=CARTESIAN_POINT('Ctrl Pts',(126.815585988529,-33.8381138444426,25.0743741277453));
#27294=CARTESIAN_POINT('Ctrl Pts',(126.818400150778,-33.8304298155902,25.0738726265239));
#27295=CARTESIAN_POINT('Ctrl Pts',(126.821241914321,-33.8227565692546,25.0733699431874));
#27296=CARTESIAN_POINT('Ctrl Pts',(126.82124193643,-33.822756509559,25.4139334024237));
#27297=CARTESIAN_POINT('Ctrl Pts',(126.787245704209,-33.9145521305829,25.4191427755899));
#27298=CARTESIAN_POINT('Ctrl Pts',(126.757213458934,-34.007853458936,25.4243154379788));
#27299=CARTESIAN_POINT('Ctrl Pts',(126.688840402644,-34.2568461875151,25.4380514877741));
#27300=CARTESIAN_POINT('Ctrl Pts',(126.657434412747,-34.4140822036232,25.4466549067327));
#27301=CARTESIAN_POINT('Ctrl Pts',(126.633676902108,-34.6011478868738,25.4573910116902));
#27302=CARTESIAN_POINT('Ctrl Pts',(126.630448555809,-34.6294097141762,25.4590264691335));
#27303=CARTESIAN_POINT('Ctrl Pts',(126.625904661282,-34.6741783018617,25.4616430471889));
#27304=CARTESIAN_POINT('Ctrl Pts',(126.624353671105,-34.6906604279019,25.4626119143837));
#27305=CARTESIAN_POINT('Ctrl Pts',(126.62161264791,-34.7222695651522,25.4644817185376));
#27306=CARTESIAN_POINT('Ctrl Pts',(126.620403354746,-34.7373942550521,25.4653816259913));
#27307=CARTESIAN_POINT('Ctrl Pts',(126.617650048824,-34.775006758323,25.4676317779128));
#27308=CARTESIAN_POINT('Ctrl Pts',(126.616228745331,-34.7975026245944,25.4689884097207));
#27309=CARTESIAN_POINT('Ctrl Pts',(126.611870212197,-34.8794711854176,25.4739669495039));
#27310=CARTESIAN_POINT('Ctrl Pts',(126.610275975973,-34.9390014906017,25.4776502533167));
#27311=CARTESIAN_POINT('Ctrl Pts',(126.610205881268,-35.1016313215704,25.4878440348002));
#27312=CARTESIAN_POINT('Ctrl Pts',(126.614864498925,-35.2046670969959,25.4944453108071));
#27313=CARTESIAN_POINT('Ctrl Pts',(126.648420621211,-35.573262356808,25.5182665406884));
#27314=CARTESIAN_POINT('Ctrl Pts',(126.703976296854,-35.8354551113146,25.5355024212253));
#27315=CARTESIAN_POINT('Ctrl Pts',(126.806981263004,-36.139261775208,25.5550454646257));
#27316=CARTESIAN_POINT('Ctrl Pts',(126.825421536744,-36.1896798391686,25.5582781045745));
#27317=CARTESIAN_POINT('Ctrl Pts',(126.856231318259,-36.2680922630069,25.5632909305051));
#27318=CARTESIAN_POINT('Ctrl Pts',(126.867795010541,-36.2963917261077,25.5650970584487));
#27319=CARTESIAN_POINT('Ctrl Pts',(126.890071584234,-36.3488696711284,25.5684416982363));
#27320=CARTESIAN_POINT('Ctrl Pts',(126.900687555886,-36.3730865133278,25.5699832846886));
#27321=CARTESIAN_POINT('Ctrl Pts',(126.925135306658,-36.4271274583494,25.5734203754036));
#27322=CARTESIAN_POINT('Ctrl Pts',(126.939119878457,-36.4568797667438,25.5753105642273));
#27323=CARTESIAN_POINT('Ctrl Pts',(126.983028987265,-36.5468725830967,25.581025302252));
#27324=CARTESIAN_POINT('Ctrl Pts',(127.014316359812,-36.6064317326092,25.5848035277591));
#27325=CARTESIAN_POINT('Ctrl Pts',(127.169687276383,-36.8819563252734,25.602333395267));
#27326=CARTESIAN_POINT('Ctrl Pts',(127.315548276213,-37.0847431046058,25.615321886196));
#27327=CARTESIAN_POINT('Ctrl Pts',(127.581383177703,-37.3796194675264,25.6364866707286));
#27328=CARTESIAN_POINT('Ctrl Pts',(127.687531428811,-37.4828967243146,25.6444716831675));
#27329=CARTESIAN_POINT('Ctrl Pts',(127.821605610217,-37.5972685753959,25.6545070952492));
#27330=CARTESIAN_POINT('Ctrl Pts',(127.843367470255,-37.6153665499935,25.6561346450307));
#27331=CARTESIAN_POINT('Ctrl Pts',(127.878189225958,-37.6435955003439,25.6587414669841));
#27332=CARTESIAN_POINT('Ctrl Pts',(127.891101444329,-37.6539074940926,25.6597086402304));
#27333=CARTESIAN_POINT('Ctrl Pts',(127.916165677873,-37.6736259505897,25.6615882001489));
#27334=CARTESIAN_POINT('Ctrl Pts',(127.928307079374,-37.6830448401183,25.6624997266158));
#27335=CARTESIAN_POINT('Ctrl Pts',(127.958599366436,-37.7062163824547,25.6647757545627));
#27336=CARTESIAN_POINT('Ctrl Pts',(127.976825445937,-37.7198691728403,25.6661467400372));
#27337=CARTESIAN_POINT('Ctrl Pts',(128.048604903044,-37.7725170478575,25.6715476500428));
#27338=CARTESIAN_POINT('Ctrl Pts',(128.103156292401,-37.8101203495046,25.6756554669053));
#27339=CARTESIAN_POINT('Ctrl Pts',(128.258750879866,-37.9107793199093,25.6873065634296));
#27340=CARTESIAN_POINT('Ctrl Pts',(128.362065870056,-37.9701437677219,25.6949661824686));
#27341=CARTESIAN_POINT('Ctrl Pts',(128.69037029607,-38.1364393504687,25.7186855316003));
#27342=CARTESIAN_POINT('Ctrl Pts',(128.924208465432,-38.2241419275337,25.7346584128665));
#27343=CARTESIAN_POINT('Ctrl Pts',(129.215397390698,-38.2980974281019,25.7529214078871));
#27344=CARTESIAN_POINT('Ctrl Pts',(129.265507339742,-38.3096176312419,25.7560120066338));
#27345=CARTESIAN_POINT('Ctrl Pts',(129.345051031264,-38.3260088820693,25.7608379839455));
#27346=CARTESIAN_POINT('Ctrl Pts',(129.374318694114,-38.3316386694311,25.7625967798613));
#27347=CARTESIAN_POINT('Ctrl Pts',(129.429784510833,-38.3415511038982,25.7658990934757));
#27348=CARTESIAN_POINT('Ctrl Pts',(129.455965969773,-38.3459134054856,25.7674449860698));
#27349=CARTESIAN_POINT('Ctrl Pts',(129.515836818474,-38.3551676237021,25.7709519192941));
#27350=CARTESIAN_POINT('Ctrl Pts',(129.549554353529,-38.3598605043914,25.7729066570245));
#27351=CARTESIAN_POINT('Ctrl Pts',(129.656724560794,-38.3731343402817,25.7790601601875));
#27352=CARTESIAN_POINT('Ctrl Pts',(129.730392340303,-38.3798204234853,25.7832010664015));
#27353=CARTESIAN_POINT('Ctrl Pts',(129.909322663475,-38.3901718880995,25.793093815337));
#27354=CARTESIAN_POINT('Ctrl Pts',(130.014652084743,-38.3913529945894,25.7987784469583));
#27355=CARTESIAN_POINT('Ctrl Pts',(130.243976267176,-38.3832384183336,25.8110392872419));
#27356=CARTESIAN_POINT('Ctrl Pts',(130.367746534448,-38.3720304194298,25.8175820577195));
#27357=CARTESIAN_POINT('Ctrl Pts',(130.633803881423,-38.3331122438844,25.8318931334268));
#27358=CARTESIAN_POINT('Ctrl Pts',(130.775484373895,-38.30302297775,25.839670564831));
#27359=CARTESIAN_POINT('Ctrl Pts',(130.949123615791,-38.2543571550464,25.849852613178));
#27360=CARTESIAN_POINT('Ctrl Pts',(130.983297503208,-38.2441951143609,25.8518889890201));
#27361=CARTESIAN_POINT('Ctrl Pts',(131.034511437505,-38.2280824924763,25.8549985616961));
#27362=CARTESIAN_POINT('Ctrl Pts',(131.051675651107,-38.2225314250919,25.8560506046008));
#27363=CARTESIAN_POINT('Ctrl Pts',(131.082979757373,-38.2121306554416,25.8579888070591));
#27364=CARTESIAN_POINT('Ctrl Pts',(131.097133038533,-38.2073240515501,25.8588725574213));
#27365=CARTESIAN_POINT('Ctrl Pts',(131.129963181995,-38.1959318593251,25.8609397007394));
#27366=CARTESIAN_POINT('Ctrl Pts',(131.148614570608,-38.1892760571265,25.8621269608499));
#27367=CARTESIAN_POINT('Ctrl Pts',(131.20978244548,-38.1668419737231,25.8660606346946));
#27368=CARTESIAN_POINT('Ctrl Pts',(131.252039042161,-38.150374496244,25.8688420860223));
#27369=CARTESIAN_POINT('Ctrl Pts',(131.355864450288,-38.1074947884238,25.8758141153587));
#27370=CARTESIAN_POINT('Ctrl Pts',(131.417004005171,-38.0800959418345,25.8800420658591));
#27371=CARTESIAN_POINT('Ctrl Pts',(131.730130198394,-37.9284761305506,25.902205670715));
#27372=CARTESIAN_POINT('Ctrl Pts',(131.966816192955,-37.775066412917,25.9205910798073));
#27373=CARTESIAN_POINT('Ctrl Pts',(132.243504116812,-37.5423576745732,25.9429952833657));
#27374=CARTESIAN_POINT('Ctrl Pts',(132.303285096733,-37.488327278408,25.9479098378704));
#27375=CARTESIAN_POINT('Ctrl Pts',(132.384333435747,-37.4096490778797,25.9546800258246));
#27376=CARTESIAN_POINT('Ctrl Pts',(132.407254642719,-37.3867508889208,25.9566076214498));
#27377=CARTESIAN_POINT('Ctrl Pts',(132.448619636211,-37.344225244498,25.9601112747249));
#27378=CARTESIAN_POINT('Ctrl Pts',(132.467164330396,-37.3247000556938,25.9616916011689));
#27379=CARTESIAN_POINT('Ctrl Pts',(132.504512491792,-37.2844268648241,25.9648950353677));
#27380=CARTESIAN_POINT('Ctrl Pts',(132.523295508523,-37.2636626885251,25.9665172218916));
#27381=CARTESIAN_POINT('Ctrl Pts',(132.57001493324,-37.2107113104227,25.9705823091845));
#27382=CARTESIAN_POINT('Ctrl Pts',(132.597606007651,-37.178225083099,25.9730111013198));
#27383=CARTESIAN_POINT('Ctrl Pts',(132.719058181566,-37.0296343572002,25.983845785645));
#27384=CARTESIAN_POINT('Ctrl Pts',(132.805803945586,-36.9079213311702,25.991974752014));
#27385=CARTESIAN_POINT('Ctrl Pts',(132.95191839456,-36.6712789097517,26.0068650138268));
#27386=CARTESIAN_POINT('Ctrl Pts',(133.013286259049,-36.557915786643,26.0136509503787));
#27387=CARTESIAN_POINT('Ctrl Pts',(133.131480819086,-36.3063245018191,26.0284346286501));
#27388=CARTESIAN_POINT('Ctrl Pts',(133.185920499401,-36.1672866050858,26.0364382882537));
#27389=CARTESIAN_POINT('Ctrl Pts',(133.241874119128,-35.990931202135,26.0468825855411));
#27390=CARTESIAN_POINT('Ctrl Pts',(133.252180903041,-35.9565623926181,26.0489316085174));
#27391=CARTESIAN_POINT('Ctrl Pts',(133.266858868967,-35.9046354168717,26.0520566529567));
#27392=CARTESIAN_POINT('Ctrl Pts',(133.271638495118,-35.8871942473503,26.0531112051102));
#27393=CARTESIAN_POINT('Ctrl Pts',(133.280112292474,-35.8552728907168,26.0550516230709));
#27394=CARTESIAN_POINT('Ctrl Pts',(133.28385059507,-35.8408053353152,26.0559350376184));
#27395=CARTESIAN_POINT('Ctrl Pts',(133.292305973281,-35.8071655649761,26.0579981896492));
#27396=CARTESIAN_POINT('Ctrl Pts',(133.296951319751,-35.7879764113146,26.0591817411637));
#27397=CARTESIAN_POINT('Ctrl Pts',(133.311632555241,-35.7249270985144,26.063089860786));
#27398=CARTESIAN_POINT('Ctrl Pts',(133.320962456073,-35.6809092679978,26.0658488717137));
#27399=CARTESIAN_POINT('Ctrl Pts',(133.341856309441,-35.5716553671269,26.0727509408532));
#27400=CARTESIAN_POINT('Ctrl Pts',(133.352388946846,-35.5062419553376,26.0769304949928));
#27401=CARTESIAN_POINT('Ctrl Pts',(133.396218345873,-35.1718750901233,26.0984066332734));
#27402=CARTESIAN_POINT('Ctrl Pts',(133.399095101174,-34.8998871634906,26.1161397992864));
#27403=CARTESIAN_POINT('Ctrl Pts',(133.3598719393,-34.5422434304771,26.1385264779311));
#27404=CARTESIAN_POINT('Ctrl Pts',(133.346736299976,-34.4544371706386,26.1439575261338));
#27405=CARTESIAN_POINT('Ctrl Pts',(133.323232021166,-34.3307356436352,26.1515144021166));
#27406=CARTESIAN_POINT('Ctrl Pts',(133.315695641226,-34.294345392661,26.1537259288782));
#27407=CARTESIAN_POINT('Ctrl Pts',(133.301657845245,-34.2317628841904,26.1575106399686));
#27408=CARTESIAN_POINT('Ctrl Pts',(133.295439369463,-34.2055113481075,26.1590925318514));
#27409=CARTESIAN_POINT('Ctrl Pts',(133.282023542729,-34.1517458184858,26.1623216706012));
#27410=CARTESIAN_POINT('Ctrl Pts',(133.274791990878,-34.1242425110012,26.1639676929666));
#27411=CARTESIAN_POINT('Ctrl Pts',(133.255284206633,-34.0536729326261,26.1681780231017));
#27412=CARTESIAN_POINT('Ctrl Pts',(133.242498966873,-34.010752357864,26.1707260154638));
#27413=CARTESIAN_POINT('Ctrl Pts',(133.170367075123,-33.7850488893111,26.1840770287661));
#27414=CARTESIAN_POINT('Ctrl Pts',(133.096406190468,-33.607300057701,26.194397302453));
#27415=CARTESIAN_POINT('Ctrl Pts',(132.914920076432,-33.2581089971184,26.2153015438782));
#27416=CARTESIAN_POINT('Ctrl Pts',(132.806343645562,-33.0880989341488,26.225838038678));
#27417=CARTESIAN_POINT('Ctrl Pts',(132.649533434162,-32.8849496238822,26.2400688177508));
#27418=CARTESIAN_POINT('Ctrl Pts',(132.614665041127,-32.841993619884,26.2431830582179));
#27419=CARTESIAN_POINT('Ctrl Pts',(132.5645435767,-32.7832453219295,26.2476217727078));
#27420=CARTESIAN_POINT('Ctrl Pts',(132.550162989169,-32.7667168263191,26.2488911814358));
#27421=CARTESIAN_POINT('Ctrl Pts',(132.525525832908,-32.7389480703399,26.2510613402408));
#27422=CARTESIAN_POINT('Ctrl Pts',(132.515351710289,-32.7276350800774,26.2519562511849));
#27423=CARTESIAN_POINT('Ctrl Pts',(132.493744968918,-32.7039326497257,26.2538548752673));
#27424=CARTESIAN_POINT('Ctrl Pts',(132.482295699705,-32.691559556845,26.2548597208605));
#27425=CARTESIAN_POINT('Ctrl Pts',(132.450306886043,-32.6575027692292,26.2576625587953));
#27426=CARTESIAN_POINT('Ctrl Pts',(132.429572798851,-32.6360048657712,26.2594740222598));
#27427=CARTESIAN_POINT('Ctrl Pts',(132.381780701611,-32.5877450553072,26.263631896904));
#27428=CARTESIAN_POINT('Ctrl Pts',(132.354550832211,-32.5611594183934,26.2659884990843));
#27429=CARTESIAN_POINT('Ctrl Pts',(132.261969026402,-32.4737638090419,26.2739434100994));
#27430=CARTESIAN_POINT('Ctrl Pts',(132.19466592247,-32.4150796904743,26.2796323149203));
#27431=CARTESIAN_POINT('Ctrl Pts',(131.895107286787,-32.1740230585245,26.304315104801));
#27432=CARTESIAN_POINT('Ctrl Pts',(131.641836126465,-32.0197297813164,26.3234667522904));
#27433=CARTESIAN_POINT('Ctrl Pts',(131.325760037249,-31.8798566150797,26.3444598076618));
#27434=CARTESIAN_POINT('Ctrl Pts',(131.279320405142,-31.8605296424742,26.3474813287574));
#27435=CARTESIAN_POINT('Ctrl Pts',(131.20491671409,-31.8314900428239,26.3522253915821));
#27436=CARTESIAN_POINT('Ctrl Pts',(131.177227330573,-31.821098376524,26.3539700227239));
#27437=CARTESIAN_POINT('Ctrl Pts',(131.124393203832,-31.8020550600788,26.3572605397195));
#27438=CARTESIAN_POINT('Ctrl Pts',(131.099275881102,-31.7933343622869,26.3588085829967));
#27439=CARTESIAN_POINT('Ctrl Pts',(131.041381834062,-31.7739938264764,26.3623407796383));
#27440=CARTESIAN_POINT('Ctrl Pts',(131.00854032239,-31.7635762795696,26.3643182808736));
#27441=CARTESIAN_POINT('Ctrl Pts',(130.902357678865,-31.7316677434358,26.3706328335647));
#27442=CARTESIAN_POINT('Ctrl Pts',(130.828444487925,-31.712154803958,26.3749074503057));
#27443=CARTESIAN_POINT('Ctrl Pts',(130.646218320187,-31.6705837248991,26.3852093804827));
#27444=CARTESIAN_POINT('Ctrl Pts',(130.53736446586,-31.6512909229631,26.3911611840199));
#27445=CARTESIAN_POINT('Ctrl Pts',(130.214716711872,-31.6102473811741,26.4085103118073));
#27446=CARTESIAN_POINT('Ctrl Pts',(129.999598238162,-31.6034556349267,26.4196843782863));
#27447=CARTESIAN_POINT('Ctrl Pts',(129.71816053168,-31.6213172038474,26.4351933914901));
#27448=CARTESIAN_POINT('Ctrl Pts',(129.651167112662,-31.62757574472,26.4389545883871));
#27449=CARTESIAN_POINT('Ctrl Pts',(129.561017366068,-31.6387123269632,26.4441616456333));
#27450=CARTESIAN_POINT('Ctrl Pts',(129.537657362573,-31.6418457759108,26.4455242355563));
#27451=CARTESIAN_POINT('Ctrl Pts',(129.500493436248,-31.6472259555943,26.4477159235646));
#27452=CARTESIAN_POINT('Ctrl Pts',(129.48666703266,-31.6493150178924,26.4485366073992));
#27453=CARTESIAN_POINT('Ctrl Pts',(129.457225277952,-31.6539499434106,26.4502961979962));
#27454=CARTESIAN_POINT('Ctrl Pts',(129.441614118659,-31.6565196929192,26.4512364455543));
#27455=CARTESIAN_POINT('Ctrl Pts',(129.401348776475,-31.6634376212321,26.4536793171709));
#27456=CARTESIAN_POINT('Ctrl Pts',(129.376724159326,-31.6679497391838,26.4551904792097));
#27457=CARTESIAN_POINT('Ctrl Pts',(129.265017159348,-31.6897000566389,26.4621171818812));
#27458=CARTESIAN_POINT('Ctrl Pts',(129.178588425886,-31.7100811540554,26.4676738549862));
#27459=CARTESIAN_POINT('Ctrl Pts',(128.891699580637,-31.7897429491614,26.486577467915));
#27460=CARTESIAN_POINT('Ctrl Pts',(128.695934086685,-31.8641593476491,26.5002117283727));
#27461=CARTESIAN_POINT('Ctrl Pts',(128.376302451349,-32.0208042372218,26.5228489240746));
#27462=CARTESIAN_POINT('Ctrl Pts',(128.248674742486,-32.093994163338,26.5320101448521));
#27463=CARTESIAN_POINT('Ctrl Pts',(128.08995362208,-32.1992824965346,26.5435127862868));
#27464=CARTESIAN_POINT('Ctrl Pts',(128.05418420511,-32.224014255096,26.5461135739441));
#27465=CARTESIAN_POINT('Ctrl Pts',(127.996039462624,-32.2658930370188,26.550357273483));
#27466=CARTESIAN_POINT('Ctrl Pts',(127.973385336374,-32.2826424973632,26.5520148398546));
#27467=CARTESIAN_POINT('Ctrl Pts',(127.929334782069,-32.3160688672133,26.5552471647612));
#27468=CARTESIAN_POINT('Ctrl Pts',(127.907924570049,-32.3327240059741,26.556822589318));
#27469=CARTESIAN_POINT('Ctrl Pts',(127.856984947556,-32.3733410045625,26.5605829652382));
#27470=CARTESIAN_POINT('Ctrl Pts',(127.827653992501,-32.3975465456926,26.5627581497772));
#27471=CARTESIAN_POINT('Ctrl Pts',(127.721750973548,-32.4879819031902,26.570656733372));
#27472=CARTESIAN_POINT('Ctrl Pts',(127.647745972011,-32.5571416221869,26.576262294808));
#27473=CARTESIAN_POINT('Ctrl Pts',(127.399746765793,-32.8106409177155,26.5955676588138));
#27474=CARTESIAN_POINT('Ctrl Pts',(127.243428179312,-33.011051966476,26.608651887737));
#27475=CARTESIAN_POINT('Ctrl Pts',(127.058954235618,-33.3116519519306,26.6277292490004));
#27476=CARTESIAN_POINT('Ctrl Pts',(127.010755401214,-33.3985373091709,26.6331964845641));
#27477=CARTESIAN_POINT('Ctrl Pts',(126.954607499484,-33.5111436573751,26.6403786564727));
#27478=CARTESIAN_POINT('Ctrl Pts',(126.943050346605,-33.5350196536688,26.6419068503812));
#27479=CARTESIAN_POINT('Ctrl Pts',(126.924912940587,-33.5736391716766,26.6443911186429));
#27480=CARTESIAN_POINT('Ctrl Pts',(126.91815552176,-33.5882988191386,26.645336967813));
#27481=CARTESIAN_POINT('Ctrl Pts',(126.905070274942,-33.6172278897419,26.6472101219333));
#27482=CARTESIAN_POINT('Ctrl Pts',(126.898735850074,-33.6314937507399,26.6481370260561));
#27483=CARTESIAN_POINT('Ctrl Pts',(126.88290537347,-33.6678202079074,26.6505044378755));
#27484=CARTESIAN_POINT('Ctrl Pts',(126.8735449547,-33.6899386704676,26.6519525488066));
#27485=CARTESIAN_POINT('Ctrl Pts',(126.849381463222,-33.748770663097,26.6558182816861));
#27486=CARTESIAN_POINT('Ctrl Pts',(126.834986479187,-33.7856438997939,26.6582553902751));
#27487=CARTESIAN_POINT('Ctrl Pts',(126.821241917671,-33.8227565602112,26.6607167036746));
#27488=CARTESIAN_POINT('Origin',(130.,-35.,23.));
#27489=CARTESIAN_POINT('',(126.821241915871,-33.8227565650715,27.9134201656876));
#27490=CARTESIAN_POINT('',(126.821241909639,-33.8227565818973,27.5681924492054));
#27491=CARTESIAN_POINT('',(126.821241915871,-33.8227565650715,23.));
#27492=CARTESIAN_POINT('Ctrl Pts',(126.821241909639,-33.8227565818973,27.5681924492054));
#27493=CARTESIAN_POINT('Ctrl Pts',(126.830994690413,-33.796422409788,27.5664434765392));
#27494=CARTESIAN_POINT('Ctrl Pts',(126.841075512034,-33.770207282694,27.5647030610561));
#27495=CARTESIAN_POINT('Ctrl Pts',(126.878262909731,-33.676977887363,27.5585167549009));
#27496=CARTESIAN_POINT('Ctrl Pts',(126.907185575693,-33.6107087819299,27.5541258504753));
#27497=CARTESIAN_POINT('Ctrl Pts',(126.952692476912,-33.5149203903061,27.5477868022147));
#27498=CARTESIAN_POINT('Ctrl Pts',(126.967633039461,-33.4846467977137,27.5457844326971));
#27499=CARTESIAN_POINT('Ctrl Pts',(126.995110796069,-33.4310038762966,27.5422370537086));
#27500=CARTESIAN_POINT('Ctrl Pts',(127.007474510898,-33.407549303618,27.5406862497125));
#27501=CARTESIAN_POINT('Ctrl Pts',(127.03439841979,-33.3578944622786,27.5374025701998));
#27502=CARTESIAN_POINT('Ctrl Pts',(127.049033564782,-33.3317372775957,27.5356724784264));
#27503=CARTESIAN_POINT('Ctrl Pts',(127.089444626059,-33.2617073529145,27.5310372553567));
#27504=CARTESIAN_POINT('Ctrl Pts',(127.115865074307,-33.2182143731757,27.528155039862));
#27505=CARTESIAN_POINT('Ctrl Pts',(127.276916839641,-32.9660679721129,27.5113907461457));
#27506=CARTESIAN_POINT('Ctrl Pts',(127.433164698986,-32.7721245466826,27.4983412475447));
#27507=CARTESIAN_POINT('Ctrl Pts',(127.6938938942,-32.5127222757983,27.4788112128993));
#27508=CARTESIAN_POINT('Ctrl Pts',(127.782970553315,-32.4330069977381,27.4724364634655));
#27509=CARTESIAN_POINT('Ctrl Pts',(127.927791128568,-32.3165766608859,27.4622037115341));
#27510=CARTESIAN_POINT('Ctrl Pts',(127.980726504992,-32.2765199054924,27.4584877494638));
#27511=CARTESIAN_POINT('Ctrl Pts',(128.053367195339,-32.224834226741,27.4533708578985));
#27512=CARTESIAN_POINT('Ctrl Pts',(128.072066789466,-32.2118110142414,27.4520521103479));
#27513=CARTESIAN_POINT('Ctrl Pts',(128.103595706058,-32.1903217208418,27.4498235219002));
#27514=CARTESIAN_POINT('Ctrl Pts',(128.116354260353,-32.1817523176812,27.4489203116299));
#27515=CARTESIAN_POINT('Ctrl Pts',(128.142946284133,-32.1641527806685,27.4470340585967));
#27516=CARTESIAN_POINT('Ctrl Pts',(128.156788093335,-32.1551365943247,27.4460502453972));
#27517=CARTESIAN_POINT('Ctrl Pts',(128.194502751086,-32.1309610563538,27.443365535753));
#27518=CARTESIAN_POINT('Ctrl Pts',(128.218499785379,-32.1159990208538,27.4416528820377));
#27519=CARTESIAN_POINT('Ctrl Pts',(128.366369978479,-32.0263523719625,27.4310858609728));
#27520=CARTESIAN_POINT('Ctrl Pts',(128.494721781097,-31.9593656735746,27.4218618191689));
#27521=CARTESIAN_POINT('Ctrl Pts',(128.856277882206,-31.7991842829979,27.3964273346959));
#27522=CARTESIAN_POINT('Ctrl Pts',(129.096214989827,-31.7233360766284,27.3801975822387));
#27523=CARTESIAN_POINT('Ctrl Pts',(129.409307172233,-31.6614154860398,27.3605736877328));
#27524=CARTESIAN_POINT('Ctrl Pts',(129.476658769481,-31.6501970910915,27.3564345310392));
#27525=CARTESIAN_POINT('Ctrl Pts',(129.577059300003,-31.6365763450943,27.3503837246341));
#27526=CARTESIAN_POINT('Ctrl Pts',(129.609875655481,-31.6326121948958,27.3484246787697));
#27527=CARTESIAN_POINT('Ctrl Pts',(129.669050647453,-31.6263406641625,27.3449244911459));
#27528=CARTESIAN_POINT('Ctrl Pts',(129.695387918909,-31.6238607364222,27.343378147041));
#27529=CARTESIAN_POINT('Ctrl Pts',(129.752086981207,-31.6191908297352,27.3400728226625));
#27530=CARTESIAN_POINT('Ctrl Pts',(129.782454829864,-31.6171009922646,27.3383170530493));
#27531=CARTESIAN_POINT('Ctrl Pts',(129.86582498547,-31.6124909845331,27.3335341136556));
#27532=CARTESIAN_POINT('Ctrl Pts',(129.9188658456,-31.6108057094804,27.3305325064398));
#27533=CARTESIAN_POINT('Ctrl Pts',(130.164975732085,-31.6087673880729,27.3167653520169));
#27534=CARTESIAN_POINT('Ctrl Pts',(130.35781472556,-31.6236626908488,27.3064610251735));
#27535=CARTESIAN_POINT('Ctrl Pts',(130.70331540003,-31.6802994820465,27.287889929921));
#27536=CARTESIAN_POINT('Ctrl Pts',(130.856318214848,-31.7164382169579,27.2796161127852));
#27537=CARTESIAN_POINT('Ctrl Pts',(131.080200314196,-31.7860353878578,27.2667911049631));
#27538=CARTESIAN_POINT('Ctrl Pts',(131.153330248597,-31.8115475777353,27.2624808425103));
#27539=CARTESIAN_POINT('Ctrl Pts',(131.24789027011,-31.8482146700501,27.2566707961217));
#27540=CARTESIAN_POINT('Ctrl Pts',(131.27017012622,-31.8571273215863,27.2552842540382));
#27541=CARTESIAN_POINT('Ctrl Pts',(131.306778848797,-31.8722248149294,27.2529738928787));
#27542=CARTESIAN_POINT('Ctrl Pts',(131.321163441263,-31.8782735999672,27.2520578237541));
#27543=CARTESIAN_POINT('Ctrl Pts',(131.348522531862,-31.890001186762,27.2502987669395));
#27544=CARTESIAN_POINT('Ctrl Pts',(131.361504125982,-31.8956623675598,27.2494569130484));
#27545=CARTESIAN_POINT('Ctrl Pts',(131.39688129249,-31.9113546817793,27.2471437447665));
#27546=CARTESIAN_POINT('Ctrl Pts',(131.419203573381,-31.9215477284648,27.2456632882036));
#27547=CARTESIAN_POINT('Ctrl Pts',(131.51009030064,-31.9642480191422,27.2395554289301));
#27548=CARTESIAN_POINT('Ctrl Pts',(131.57766057147,-31.9988088587972,27.2348267945692));
#27549=CARTESIAN_POINT('Ctrl Pts',(131.824595584461,-32.1357553206266,27.2169825853644));
#27550=CARTESIAN_POINT('Ctrl Pts',(131.995651137573,-32.2521964279902,27.2035098746665));
#27551=CARTESIAN_POINT('Ctrl Pts',(132.239222285499,-32.4528093100334,27.1833680636472));
#27552=CARTESIAN_POINT('Ctrl Pts',(132.320007305528,-32.5261636749289,27.1764933248361));
#27553=CARTESIAN_POINT('Ctrl Pts',(132.450678501914,-32.6568572817911,27.1650801803098));
#27554=CARTESIAN_POINT('Ctrl Pts',(132.502428549926,-32.7122072594907,27.160472005428));
#27555=CARTESIAN_POINT('Ctrl Pts',(132.574882752124,-32.7951047301561,27.1538860261557));
#27556=CARTESIAN_POINT('Ctrl Pts',(132.59708822907,-32.821303784652,27.1518477678726));
#27557=CARTESIAN_POINT('Ctrl Pts',(132.635764219446,-32.8683672425936,27.14826064464));
#27558=CARTESIAN_POINT('Ctrl Pts',(132.652394390311,-32.8890960962418,27.1467054933274));
#27559=CARTESIAN_POINT('Ctrl Pts',(132.687049828737,-32.933348993048,27.1434363795027));
#27560=CARTESIAN_POINT('Ctrl Pts',(132.705013905189,-32.9569182542266,27.141724881642));
#27561=CARTESIAN_POINT('Ctrl Pts',(132.752799486374,-33.0213492718809,27.1371232775701));
#27562=CARTESIAN_POINT('Ctrl Pts',(132.782019764605,-33.062648684945,27.1342559765518));
#27563=CARTESIAN_POINT('Ctrl Pts',(132.974684132486,-33.3483099866243,27.1149359097818));
#27564=CARTESIAN_POINT('Ctrl Pts',(133.10665403177,-33.6123652264817,27.0997163155911));
#27565=CARTESIAN_POINT('Ctrl Pts',(133.232303184815,-33.9749724160016,27.0791816976117));
#27566=CARTESIAN_POINT('Ctrl Pts',(133.25831508641,-34.060933199699,27.0743268618067));
#27567=CARTESIAN_POINT('Ctrl Pts',(133.290484324365,-34.1847843619575,27.0672264698843));
#27568=CARTESIAN_POINT('Ctrl Pts',(133.299459800818,-34.2219071846226,27.0650848523721));
#27569=CARTESIAN_POINT('Ctrl Pts',(133.314351099898,-34.2883970378607,27.0612127434705));
#27570=CARTESIAN_POINT('Ctrl Pts',(133.320508548394,-34.3177061928561,27.0594934216268));
#27571=CARTESIAN_POINT('Ctrl Pts',(133.3295269608,-34.3636510038532,27.0567734091824));
#27572=CARTESIAN_POINT('Ctrl Pts',(133.332653519902,-34.3802336589864,27.05578665987));
#27573=CARTESIAN_POINT('Ctrl Pts',(133.338362279986,-34.4118047435323,27.0538973080747));
#27574=CARTESIAN_POINT('Ctrl Pts',(133.340967615793,-34.4267882348552,27.0529959536205));
#27575=CARTESIAN_POINT('Ctrl Pts',(133.34650445416,-34.4599517555191,27.0509911964642));
#27576=CARTESIAN_POINT('Ctrl Pts',(133.349388806334,-34.4781391383884,27.0498853343631));
#27577=CARTESIAN_POINT('Ctrl Pts',(133.358842373799,-34.5410587327454,27.0460395179882));
#27578=CARTESIAN_POINT('Ctrl Pts',(133.364664480301,-34.5858965116578,27.0432639821675));
#27579=CARTESIAN_POINT('Ctrl Pts',(133.392456374922,-34.8395695690365,27.0274133846477));
#27580=CARTESIAN_POINT('Ctrl Pts',(133.395879099278,-35.0499676985824,27.0137349000843));
#27581=CARTESIAN_POINT('Ctrl Pts',(133.364753837455,-35.4556344683181,26.9876028523466));
#27582=CARTESIAN_POINT('Ctrl Pts',(133.332614428017,-35.6502864669629,26.9751760355249));
#27583=CARTESIAN_POINT('Ctrl Pts',(133.272601936296,-35.8845902202759,26.9605506438904));
#27584=CARTESIAN_POINT('Ctrl Pts',(133.260590714406,-35.9278856474808,26.9578608371576));
#27585=CARTESIAN_POINT('Ctrl Pts',(133.239568290055,-35.9982047324122,26.953511229768));
#27586=CARTESIAN_POINT('Ctrl Pts',(133.231071230352,-36.025375137211,26.9518352933306));
#27587=CARTESIAN_POINT('Ctrl Pts',(133.213861833918,-36.0780649773579,26.9485934408178));
#27588=CARTESIAN_POINT('Ctrl Pts',(133.205185302647,-36.1035937749889,26.9470265124761));
#27589=CARTESIAN_POINT('Ctrl Pts',(133.183858764982,-36.1639684117867,26.9433284271286));
#27590=CARTESIAN_POINT('Ctrl Pts',(133.170939802831,-36.1987159876285,26.9412061841352));
#27591=CARTESIAN_POINT('Ctrl Pts',(133.125426933817,-36.3152416350341,26.9341034775999));
#27592=CARTESIAN_POINT('Ctrl Pts',(133.09021738324,-36.3959628675105,26.9292081541935));
#27593=CARTESIAN_POINT('Ctrl Pts',(132.933585480935,-36.7199980722284,26.9095083337712));
#27594=CARTESIAN_POINT('Ctrl Pts',(132.786260944704,-36.9496301319206,26.8955150832843));
#27595=CARTESIAN_POINT('Ctrl Pts',(132.570860801857,-37.210311453422,26.8772038588778));
#27596=CARTESIAN_POINT('Ctrl Pts',(132.52713451787,-37.2601752661838,26.873569072913));
#27597=CARTESIAN_POINT('Ctrl Pts',(132.45131084207,-37.3416890094502,26.8673394145487));
#27598=CARTESIAN_POINT('Ctrl Pts',(132.419992910924,-37.3740400525759,26.8647857679079));
#27599=CARTESIAN_POINT('Ctrl Pts',(132.374025576047,-37.4196689113159,26.8610482507724));
#27600=CARTESIAN_POINT('Ctrl Pts',(132.359888633793,-37.4334585822378,26.859900194323));
#27601=CARTESIAN_POINT('Ctrl Pts',(132.334844298097,-37.4574642374002,26.8578670379586));
#27602=CARTESIAN_POINT('Ctrl Pts',(132.323988590493,-37.467732844832,26.8569858960968));
#27603=CARTESIAN_POINT('Ctrl Pts',(132.2998481233,-37.4902671688812,26.8550264158087));
#27604=CARTESIAN_POINT('Ctrl Pts',(132.286533072077,-37.5024984396797,26.8539457722239));
#27605=CARTESIAN_POINT('Ctrl Pts',(132.246519125892,-37.5386694969125,26.8507003892999));
#27606=CARTESIAN_POINT('Ctrl Pts',(132.219538308561,-37.562292035229,26.8485148773444));
#27607=CARTESIAN_POINT('Ctrl Pts',(132.078641501372,-37.6817562380133,26.8371386478315));
#27608=CARTESIAN_POINT('Ctrl Pts',(131.958883665927,-37.7704394633191,26.8275975467818));
#27609=CARTESIAN_POINT('Ctrl Pts',(131.726035903215,-37.9202039314815,26.8097642153179));
#27610=CARTESIAN_POINT('Ctrl Pts',(131.614535293586,-37.98329830662,26.8014972020417));
#27611=CARTESIAN_POINT('Ctrl Pts',(131.364972910286,-38.1064181195044,26.7837926976329));
#27612=CARTESIAN_POINT('Ctrl Pts',(131.225931158269,-38.1638721465648,26.7744242765136));
#27613=CARTESIAN_POINT('Ctrl Pts',(131.043074643412,-38.2255576705999,26.7627783238998));
#27614=CARTESIAN_POINT('Ctrl Pts',(131.002374441645,-38.2384367719991,26.7602266865295));
#27615=CARTESIAN_POINT('Ctrl Pts',(130.934579756203,-38.2584889681723,26.7560414116201));
#27616=CARTESIAN_POINT('Ctrl Pts',(130.907621091163,-38.2661006876111,26.7543939169789));
#27617=CARTESIAN_POINT('Ctrl Pts',(130.854576924671,-38.2803700868507,26.7511841091669));
#27618=CARTESIAN_POINT('Ctrl Pts',(130.828500400175,-38.28705290115,26.7496210990796));
#27619=CARTESIAN_POINT('Ctrl Pts',(130.770907154633,-38.3010838094103,26.7462004809165));
#27620=CARTESIAN_POINT('Ctrl Pts',(130.739359042992,-38.3082926813406,26.7443473595146));
#27621=CARTESIAN_POINT('Ctrl Pts',(130.629177908061,-38.3318146524044,26.7379423714849));
#27622=CARTESIAN_POINT('Ctrl Pts',(130.550069534292,-38.3457851949272,26.7334625747005));
#27623=CARTESIAN_POINT('Ctrl Pts',(130.191966373627,-38.3959798531437,26.7135917969621));
#27624=CARTESIAN_POINT('Ctrl Pts',(129.90964159175,-38.4001994052375,26.6991313994537));
#27625=CARTESIAN_POINT('Ctrl Pts',(129.563437805498,-38.3621880918611,26.6802803767095));
#27626=CARTESIAN_POINT('Ctrl Pts',(129.497063482505,-38.3529016199872,26.6766089048678));
#27627=CARTESIAN_POINT('Ctrl Pts',(129.386294668133,-38.3340408512872,26.670323126022));
#27628=CARTESIAN_POINT('Ctrl Pts',(129.341737353693,-38.3255304105277,26.6677510175765));
#27629=CARTESIAN_POINT('Ctrl Pts',(129.277991335347,-38.3120236715448,26.6639912705699));
#27630=CARTESIAN_POINT('Ctrl Pts',(129.258653031287,-38.3077487727487,26.6628400365185));
#27631=CARTESIAN_POINT('Ctrl Pts',(129.224787165396,-38.2999505392557,26.6608034710753));
#27632=CARTESIAN_POINT('Ctrl Pts',(129.210243718083,-38.2965001901647,26.6599221477652));
#27633=CARTESIAN_POINT('Ctrl Pts',(129.178199944245,-38.2886737614959,26.6579650546773));
#27634=CARTESIAN_POINT('Ctrl Pts',(129.160711652075,-38.2842541737943,26.6568870193113));
#27635=CARTESIAN_POINT('Ctrl Pts',(129.108772226055,-38.2706862705814,26.6536574094168));
#27636=CARTESIAN_POINT('Ctrl Pts',(129.074430239311,-38.2611341626483,26.6514853470934));
#27637=CARTESIAN_POINT('Ctrl Pts',(128.901591868381,-38.2101098613569,26.6403892496618));
#27638=CARTESIAN_POINT('Ctrl Pts',(128.765708177188,-38.1603516915279,26.631134310759));
#27639=CARTESIAN_POINT('Ctrl Pts',(128.520061010398,-38.0521356138726,26.6138492845831));
#27640=CARTESIAN_POINT('Ctrl Pts',(128.409514105401,-37.9960152615364,26.6058450916093));
#27641=CARTESIAN_POINT('Ctrl Pts',(128.210943111251,-37.8811139433955,26.5912199342369));
#27642=CARTESIAN_POINT('Ctrl Pts',(128.12211323902,-37.8240195418498,26.5845766547595));
#27643=CARTESIAN_POINT('Ctrl Pts',(127.975712549297,-37.7199544202773,26.5734947773514));
#27644=CARTESIAN_POINT('Ctrl Pts',(127.91675866483,-37.6750698194147,26.5689917772688));
#27645=CARTESIAN_POINT('Ctrl Pts',(127.832909850094,-37.6067768373599,26.5625251229662));
#27646=CARTESIAN_POINT('Ctrl Pts',(127.806825414567,-37.5848695445709,26.5605040682418));
#27647=CARTESIAN_POINT('Ctrl Pts',(127.761008902725,-37.5451971367022,26.5569360654727));
#27648=CARTESIAN_POINT('Ctrl Pts',(127.741147306139,-37.5275866286352,26.5553830670236));
#27649=CARTESIAN_POINT('Ctrl Pts',(127.699437937586,-37.4897202052171,26.5521073236154));
#27650=CARTESIAN_POINT('Ctrl Pts',(127.67764613392,-37.469405820383,26.5503871927245));
#27651=CARTESIAN_POINT('Ctrl Pts',(127.619029212581,-37.4133006200849,26.5457339955877));
#27652=CARTESIAN_POINT('Ctrl Pts',(127.582744288737,-37.3769554031527,26.5428246541864));
#27653=CARTESIAN_POINT('Ctrl Pts',(127.37506018272,-37.159249778047,26.5259640357805));
#27654=CARTESIAN_POINT('Ctrl Pts',(127.223284317831,-36.9602371688749,26.5128546183194));
#27655=CARTESIAN_POINT('Ctrl Pts',(127.033529265057,-36.6445557707527,26.4932943162819));
#27656=CARTESIAN_POINT('Ctrl Pts',(126.97773452637,-36.539617010713,26.486954496472));
#27657=CARTESIAN_POINT('Ctrl Pts',(126.899623154708,-36.3720216719875,26.4767706597061));
#27658=CARTESIAN_POINT('Ctrl Pts',(126.873443784974,-36.3112685252105,26.473067067287));
#27659=CARTESIAN_POINT('Ctrl Pts',(126.840668249408,-36.2286358233001,26.4679646764145));
#27660=CARTESIAN_POINT('Ctrl Pts',(126.832490101244,-36.2073955761962,26.4666474674454));
#27661=CARTESIAN_POINT('Ctrl Pts',(126.819150756607,-36.1716822147994,26.4644207193171));
#27662=CARTESIAN_POINT('Ctrl Pts',(126.81387279523,-36.1572530188819,26.4635177858885));
#27663=CARTESIAN_POINT('Ctrl Pts',(126.803120698791,-36.1272271302625,26.4616312276648));
#27664=CARTESIAN_POINT('Ctrl Pts',(126.797662295291,-36.1116255977065,26.460646821896));
#27665=CARTESIAN_POINT('Ctrl Pts',(126.783160633895,-36.0691827653424,26.457958801183));
#27666=CARTESIAN_POINT('Ctrl Pts',(126.774339539014,-36.0422676092873,26.4562433822108));
#27667=CARTESIAN_POINT('Ctrl Pts',(126.72019381854,-35.8697823310236,26.4451953637472));
#27668=CARTESIAN_POINT('Ctrl Pts',(126.684400509325,-35.721416265381,26.4354519754617));
#27669=CARTESIAN_POINT('Ctrl Pts',(126.62660463481,-35.3833111756366,26.413372798666));
#27670=CARTESIAN_POINT('Ctrl Pts',(126.610389780889,-35.1930722355296,26.4010493342579));
#27671=CARTESIAN_POINT('Ctrl Pts',(126.610175022661,-34.8983352556159,26.3825794060772));
#27672=CARTESIAN_POINT('Ctrl Pts',(126.614897717059,-34.7942452572275,26.3761707671459));
#27673=CARTESIAN_POINT('Ctrl Pts',(126.628005360703,-34.6512718640806,26.3675336110191));
#27674=CARTESIAN_POINT('Ctrl Pts',(126.632289101672,-34.6120790515124,26.3651828664172));
#27675=CARTESIAN_POINT('Ctrl Pts',(126.640359982631,-34.5485232826407,26.3613969628748));
#27676=CARTESIAN_POINT('Ctrl Pts',(126.643730790616,-34.5241120776792,26.3599491071496));
#27677=CARTESIAN_POINT('Ctrl Pts',(126.651397939722,-34.4727286025183,26.3569140105945));
#27678=CARTESIAN_POINT('Ctrl Pts',(126.655754678625,-34.4457670354514,26.3553287608552));
#27679=CARTESIAN_POINT('Ctrl Pts',(126.6671336537,-34.3803768772537,26.351500319755));
#27680=CARTESIAN_POINT('Ctrl Pts',(126.674495322243,-34.3420108566249,26.3492678374341));
#27681=CARTESIAN_POINT('Ctrl Pts',(126.705097450401,-34.1961921307263,26.3408264962036));
#27682=CARTESIAN_POINT('Ctrl Pts',(126.7328975702,-34.0897611642596,26.3347590711471));
#27683=CARTESIAN_POINT('Ctrl Pts',(126.782934654739,-33.9303456417629,26.3256968410527));
#27684=CARTESIAN_POINT('Ctrl Pts',(126.801414529506,-33.8762938999873,26.3226281947471));
#27685=CARTESIAN_POINT('Ctrl Pts',(126.821241846765,-33.8227567516686,26.3195780637354));
#27686=CARTESIAN_POINT('',(126.610250231881,-34.9987461903623,26.7339821967504));
#27687=CARTESIAN_POINT('Ctrl Pts',(126.821241917671,-33.8227565602112,26.6607167036746));
#27688=CARTESIAN_POINT('Ctrl Pts',(126.808026128393,-33.8584414453932,26.6630833269527));
#27689=CARTESIAN_POINT('Ctrl Pts',(126.795411679185,-33.8943476869306,26.6654723265988));
#27690=CARTESIAN_POINT('Ctrl Pts',(126.733599981728,-34.080243728041,26.6778554664346));
#27691=CARTESIAN_POINT('Ctrl Pts',(126.694320202069,-34.2333191535549,26.6880905081309));
#27692=CARTESIAN_POINT('Ctrl Pts',(126.628948778195,-34.5897919147975,26.7113996454761));
#27693=CARTESIAN_POINT('Ctrl Pts',(126.610336083526,-34.7939598524325,26.7243514856095));
#27694=CARTESIAN_POINT('Ctrl Pts',(126.610250297903,-34.9985788622999,26.7367448338284));
#27695=CARTESIAN_POINT('Ctrl Pts',(126.610250231881,-34.9987461903623,26.7339821967504));
#27696=CARTESIAN_POINT('Ctrl Pts',(126.610210918892,-35.1050312211208,26.7401898652714));
#27697=CARTESIAN_POINT('Ctrl Pts',(126.615174777716,-35.2112871242203,26.7463975337923));
#27698=CARTESIAN_POINT('Ctrl Pts',(126.625107297085,-35.3170241415319,26.7526052023133));
#27699=CARTESIAN_POINT('Ctrl Pts',(126.63504515388,-35.4228179786101,26.7588162066412));
#27700=CARTESIAN_POINT('Ctrl Pts',(126.649956949814,-35.5280919745356,26.7650272109691));
#27701=CARTESIAN_POINT('Ctrl Pts',(126.669756487617,-35.6323631952676,26.771238215297));
#27702=CARTESIAN_POINT('Ctrl Pts',(126.689810649996,-35.7379753571683,26.777529093931));
#27703=CARTESIAN_POINT('Ctrl Pts',(126.714879066237,-35.8425583544692,26.783819972565));
#27704=CARTESIAN_POINT('Ctrl Pts',(126.744819612008,-35.9456245048278,26.790110851199));
#27705=CARTESIAN_POINT('Ctrl Pts',(126.774450142078,-36.0476234694036,26.7963365917036));
#27706=CARTESIAN_POINT('Ctrl Pts',(126.808852175912,-36.1481364947945,26.8025623322082));
#27707=CARTESIAN_POINT('Ctrl Pts',(126.847839093249,-36.2467103434447,26.8087880727127));
#27708=CARTESIAN_POINT('Ctrl Pts',(126.887437873914,-36.3468312167672,26.8151115204114));
#27709=CARTESIAN_POINT('Ctrl Pts',(126.931766482523,-36.4449511376652,26.8214349681101));
#27710=CARTESIAN_POINT('Ctrl Pts',(126.980581021134,-36.540621333283,26.8277584158088));
#27711=CARTESIAN_POINT('Ctrl Pts',(127.029395559746,-36.6362915289008,26.8340818635075));
#27712=CARTESIAN_POINT('Ctrl Pts',(127.082695759616,-36.7295116605695,26.8404053112062));
#27713=CARTESIAN_POINT('Ctrl Pts',(127.140192688407,-36.8198646111885,26.8467287589049));
#27714=CARTESIAN_POINT('Ctrl Pts',(127.195672875856,-36.9070483746075,26.8528304076544));
#27715=CARTESIAN_POINT('Ctrl Pts',(127.255237266505,-36.991840115881,26.8589320564039));
#27716=CARTESIAN_POINT('Ctrl Pts',(127.318653174035,-37.0738332289239,26.8650337051533));
#27717=CARTESIAN_POINT('Ctrl Pts',(127.381985666394,-37.1557184909589,26.8711273279974));
#27718=CARTESIAN_POINT('Ctrl Pts',(127.449159344426,-37.2348121076691,26.8772209508415));
#27719=CARTESIAN_POINT('Ctrl Pts',(127.519897363522,-37.3107349426182,26.8833145736856));
#27720=CARTESIAN_POINT('Ctrl Pts',(127.590562576443,-37.3865796349879,26.8894019247485));
#27721=CARTESIAN_POINT('Ctrl Pts',(127.664784545446,-37.4592597237484,26.8954892758114));
#27722=CARTESIAN_POINT('Ctrl Pts',(127.742245693181,-37.5284284748709,26.9015766268743));
#27723=CARTESIAN_POINT('Ctrl Pts',(127.819651737321,-37.5975480213678,26.9076596475738));
#27724=CARTESIAN_POINT('Ctrl Pts',(127.900292059853,-37.6631609133593,26.9137426682733));
#27725=CARTESIAN_POINT('Ctrl Pts',(127.983812297837,-37.7249572862979,26.9198256889727));
#27726=CARTESIAN_POINT('Ctrl Pts',(128.067301613337,-37.7867307797833,26.9259064574982));
#27727=CARTESIAN_POINT('Ctrl Pts',(128.153668381677,-37.8446903083731,26.9319872260236));
#27728=CARTESIAN_POINT('Ctrl Pts',(128.242525864358,-37.8985668398449,26.938067994549));
#27729=CARTESIAN_POINT('Ctrl Pts',(128.33137346955,-37.9524373823466,26.9441480871301));
#27730=CARTESIAN_POINT('Ctrl Pts',(128.422710872761,-38.0022256084781,26.9502281797111));
#27731=CARTESIAN_POINT('Ctrl Pts',(128.516123897908,-38.0477068061314,26.9563082722921));
#27732=CARTESIAN_POINT('Ctrl Pts',(128.609550740135,-38.0931947310841,26.9623892642031));
#27733=CARTESIAN_POINT('Ctrl Pts',(128.705053429628,-38.1343741745972,26.9684702561141));
#27734=CARTESIAN_POINT('Ctrl Pts',(128.802195670963,-38.1710676201936,26.974551248025));
#27735=CARTESIAN_POINT('Ctrl Pts',(128.89943874179,-38.2077991520172,26.9806385517455));
#27736=CARTESIAN_POINT('Ctrl Pts',(128.998324362134,-38.2400352355096,26.986725855466));
#27737=CARTESIAN_POINT('Ctrl Pts',(129.098398877858,-38.2676475451083,26.9928131591865));
#27738=CARTESIAN_POINT('Ctrl Pts',(129.198527160484,-38.2952746899358,26.9989037334245));
#27739=CARTESIAN_POINT('Ctrl Pts',(129.299845193629,-38.3182730178205,27.0049943076626));
#27740=CARTESIAN_POINT('Ctrl Pts',(129.401888827044,-38.3365653129057,27.0110848819006));
#27741=CARTESIAN_POINT('Ctrl Pts',(129.504099053358,-38.3548874713577,27.0171853993991));
#27742=CARTESIAN_POINT('Ctrl Pts',(129.60703682202,-38.3684881927925,27.0232859168975));
#27743=CARTESIAN_POINT('Ctrl Pts',(129.710232315234,-38.3773421134622,27.0293864343959));
#27744=CARTESIAN_POINT('Ctrl Pts',(129.791551230606,-38.3843190773123,27.0341936934217));
#27745=CARTESIAN_POINT('Ctrl Pts',(129.873030044153,-38.3883495206598,27.0390009524475));
#27746=CARTESIAN_POINT('Ctrl Pts',(129.954440018181,-38.389443811388,27.0438082114734));
#27747=CARTESIAN_POINT('Ctrl Pts',(130.057770259678,-38.3908327483895,27.0499098623092));
#27748=CARTESIAN_POINT('Ctrl Pts',(130.16133869337,-38.3874945526483,27.0560115131451));
#27749=CARTESIAN_POINT('Ctrl Pts',(130.264677695181,-38.3794009498983,27.062113163981));
#27750=CARTESIAN_POINT('Ctrl Pts',(130.367880768739,-38.3713179931702,27.0682067889339));
#27751=CARTESIAN_POINT('Ctrl Pts',(130.470854587525,-38.358492097902,27.0743004138869));
#27752=CARTESIAN_POINT('Ctrl Pts',(130.573130296352,-38.340946980409,27.0803940388398));
#27753=CARTESIAN_POINT('Ctrl Pts',(130.675300739611,-38.3234199209353,27.0864813920309));
#27754=CARTESIAN_POINT('Ctrl Pts',(130.776774082327,-38.3011833697077,27.092568745222));
#27755=CARTESIAN_POINT('Ctrl Pts',(130.877086241575,-38.274312872549,27.0986560984131));
#27756=CARTESIAN_POINT('Ctrl Pts',(130.977327042043,-38.2474614901803,27.1047391212609));
#27757=CARTESIAN_POINT('Ctrl Pts',(131.076407889687,-38.2159828274786,27.1108221441086));
#27758=CARTESIAN_POINT('Ctrl Pts',(131.173875373655,-38.1800034071721,27.1169051669564));
#27759=CARTESIAN_POINT('Ctrl Pts',(131.271306771517,-38.1440373077922,27.1229859376417));
#27760=CARTESIAN_POINT('Ctrl Pts',(131.367125592008,-38.1035739105461,27.129066708327));
#27761=CARTESIAN_POINT('Ctrl Pts',(131.460894828175,-38.0587891989333,27.1351474790123));
#27762=CARTESIAN_POINT('Ctrl Pts',(131.554653641,-38.0140094655672,27.141227573762));
#27763=CARTESIAN_POINT('Ctrl Pts',(131.646362936558,-37.9649095573695,27.1473076685118));
#27764=CARTESIAN_POINT('Ctrl Pts',(131.735607735692,-37.911712700509,27.1533877632616));
#27765=CARTESIAN_POINT('Ctrl Pts',(131.824865735456,-37.8585079750444,27.1594687573475));
#27766=CARTESIAN_POINT('Ctrl Pts',(131.911658147093,-37.8012053159886,27.1655497514335));
#27767=CARTESIAN_POINT('Ctrl Pts',(131.995597339505,-37.7400723204073,27.1716307455195));
#27768=CARTESIAN_POINT('Ctrl Pts',(132.079623657122,-37.6788758714532,27.177718051411));
#27769=CARTESIAN_POINT('Ctrl Pts',(132.160790494676,-37.6138413984369,27.1838053573026));
#27770=CARTESIAN_POINT('Ctrl Pts',(132.238741847519,-37.5452779814131,27.1898926631942));
#27771=CARTESIAN_POINT('Ctrl Pts',(132.316735081181,-37.4766777274143,27.1959832396044));
#27772=CARTESIAN_POINT('Ctrl Pts',(132.391509081025,-37.4045450497778,27.2020738160146));
#27773=CARTESIAN_POINT('Ctrl Pts',(132.462744835503,-37.3292258236812,27.2081643924249));
#27774=CARTESIAN_POINT('Ctrl Pts',(132.534096886719,-37.2537836343285,27.2142649120746));
#27775=CARTESIAN_POINT('Ctrl Pts',(132.601898873521,-37.1751448282075,27.2203654317244));
#27776=CARTESIAN_POINT('Ctrl Pts',(132.665872045227,-37.0936884441047,27.2264659513742));
#27777=CARTESIAN_POINT('Ctrl Pts',(132.716283198907,-37.0295004386057,27.2312731889301));
#27778=CARTESIAN_POINT('Ctrl Pts',(132.7643176392,-36.963563539714,27.236080426486));
#27779=CARTESIAN_POINT('Ctrl Pts',(132.80985865339,-36.8960747375742,27.2408876640418));
#27780=CARTESIAN_POINT('Ctrl Pts',(132.867662092612,-36.8104138241755,27.2469893038236));
#27781=CARTESIAN_POINT('Ctrl Pts',(132.921642478689,-36.7219624582929,27.2530909436055));
#27782=CARTESIAN_POINT('Ctrl Pts',(132.971519829462,-36.6310962465826,27.2591925833873));
#27783=CARTESIAN_POINT('Ctrl Pts',(133.021331573161,-36.5403495573827,27.2652861972671));
#27784=CARTESIAN_POINT('Ctrl Pts',(133.067050806911,-36.4471947089995,27.271379811147));
#27785=CARTESIAN_POINT('Ctrl Pts',(133.108440357057,-36.3520368371902,27.2774734250269));
#27786=CARTESIAN_POINT('Ctrl Pts',(133.149787307592,-36.25697690528,27.2835607671405));
#27787=CARTESIAN_POINT('Ctrl Pts',(133.186813266121,-36.1599184395919,27.2896481092541));
#27788=CARTESIAN_POINT('Ctrl Pts',(133.219327023633,-36.0612909956297,27.2957354513678));
#27789=CARTESIAN_POINT('Ctrl Pts',(133.25181765209,-35.9627337114954,27.3018184631768));
#27790=CARTESIAN_POINT('Ctrl Pts',(133.279802328967,-35.8626100736336,27.3079014749858));
#27791=CARTESIAN_POINT('Ctrl Pts',(133.303138330882,-35.7613686554859,27.3139844867949));
#27792=CARTESIAN_POINT('Ctrl Pts',(133.326465693026,-35.6601647203073,27.3200652464689));
#27793=CARTESIAN_POINT('Ctrl Pts',(133.345147704808,-35.5578442436962,27.3261460061429));
#27794=CARTESIAN_POINT('Ctrl Pts',(133.359092002414,-35.4548691919879,27.3322267658169));
#27795=CARTESIAN_POINT('Ctrl Pts',(133.373034750068,-35.3519055862728,27.3383068495957));
#27796=CARTESIAN_POINT('Ctrl Pts',(133.382240773313,-35.2482879740206,27.3443869333746));
#27797=CARTESIAN_POINT('Ctrl Pts',(133.386669295573,-35.1444857948878,27.3504670171535));
#27798=CARTESIAN_POINT('Ctrl Pts',(133.391098472917,-35.0406682609339,27.356548000322));
#27799=CARTESIAN_POINT('Ctrl Pts',(133.390748726998,-34.9366665332639,27.3626289834905));
#27800=CARTESIAN_POINT('Ctrl Pts',(133.385631382985,-34.8329515009179,27.368709966659));
#27801=CARTESIAN_POINT('Ctrl Pts',(133.380508727258,-34.7291288141581,27.374797261783));
#27802=CARTESIAN_POINT('Ctrl Pts',(133.370608611621,-34.6255938450878,27.3808845569071));
#27803=CARTESIAN_POINT('Ctrl Pts',(133.355994392891,-34.5228137707522,27.3869718520312));
#27804=CARTESIAN_POINT('Ctrl Pts',(133.341372322225,-34.4199784746777,27.3930624177408));
#27805=CARTESIAN_POINT('Ctrl Pts',(133.322031182985,-34.3178993015912,27.3991529834504));
#27806=CARTESIAN_POINT('Ctrl Pts',(133.298085384627,-34.2170326582749,27.40524354916));
#27807=CARTESIAN_POINT('Ctrl Pts',(133.27410049235,-34.1160013400358,27.4113440583296));
#27808=CARTESIAN_POINT('Ctrl Pts',(133.245496041031,-34.0161869176726,27.4174445674992));
#27809=CARTESIAN_POINT('Ctrl Pts',(133.212436246745,-33.9180303039832,27.4235450766689));
#27810=CARTESIAN_POINT('Ctrl Pts',(133.186384340782,-33.8406805525787,27.428352423316));
#27811=CARTESIAN_POINT('Ctrl Pts',(133.157566757318,-33.7643599812258,27.4331597699631));
#27812=CARTESIAN_POINT('Ctrl Pts',(133.126084283109,-33.6892742020556,27.4379671166102));
#27813=CARTESIAN_POINT('Ctrl Pts',(133.08612560333,-33.5939726515496,27.4440687725343));
#27814=CARTESIAN_POINT('Ctrl Pts',(133.041737391341,-33.5003389802669,27.4501704284584));
#27815=CARTESIAN_POINT('Ctrl Pts',(132.993080319246,-33.4088132526192,27.4562720843826));
#27816=CARTESIAN_POINT('Ctrl Pts',(132.944487249362,-33.317407915463,27.4623657143518));
#27817=CARTESIAN_POINT('Ctrl Pts',(132.891636681597,-33.2281053841537,27.4684593443211));
#27818=CARTESIAN_POINT('Ctrl Pts',(132.834737451366,-33.1413261059775,27.4745529742904));
#27819=CARTESIAN_POINT('Ctrl Pts',(132.777896784393,-33.054636144953,27.4806403324205));
#27820=CARTESIAN_POINT('Ctrl Pts',(132.717015974492,-32.9704646286416,27.4867276905507));
#27821=CARTESIAN_POINT('Ctrl Pts',(132.652349477154,-32.8892069467753,27.4928150486808));
#27822=CARTESIAN_POINT('Ctrl Pts',(132.587728982838,-32.8080070707148,27.4988980763325));
#27823=CARTESIAN_POINT('Ctrl Pts',(132.519328422117,-32.72971724075,27.5049811039842));
#27824=CARTESIAN_POINT('Ctrl Pts',(132.447444734549,-32.6547027195202,27.5110641316358));
#27825=CARTESIAN_POINT('Ctrl Pts',(132.375587661986,-32.579715972488,27.5171449070407));
#27826=CARTESIAN_POINT('Ctrl Pts',(132.300250321271,-32.5080024325567,27.5232256824457));
#27827=CARTESIAN_POINT('Ctrl Pts',(132.221768458665,-32.4398925845622,27.5293064578506));
#27828=CARTESIAN_POINT('Ctrl Pts',(132.143295321211,-32.3717903086199,27.5353865572307));
#27829=CARTESIAN_POINT('Ctrl Pts',(132.06167868008,-32.3072912083081,27.5414666566108));
#27830=CARTESIAN_POINT('Ctrl Pts',(131.977288810259,-32.2466867190011,27.5475467559908));
#27831=CARTESIAN_POINT('Ctrl Pts',(131.892886459244,-32.1860732663394,27.5536277546127));
#27832=CARTESIAN_POINT('Ctrl Pts',(131.805710412133,-32.1293558186036,27.5597087532345));
#27833=CARTESIAN_POINT('Ctrl Pts',(131.716160716455,-32.0767830292987,27.5657897518564));
#27834=CARTESIAN_POINT('Ctrl Pts',(131.626518074739,-32.0241556732814,27.5718770621103));
#27835=CARTESIAN_POINT('Ctrl Pts',(131.534497233888,-31.9756817838379,27.5779643723642));
#27836=CARTESIAN_POINT('Ctrl Pts',(131.440523658722,-31.9315644619509,27.5840516826181));
#27837=CARTESIAN_POINT('Ctrl Pts',(131.346499595917,-31.8874234378751,27.5901422633012));
#27838=CARTESIAN_POINT('Ctrl Pts',(131.25052110427,-31.8476438074137,27.5962328439843));
#27839=CARTESIAN_POINT('Ctrl Pts',(131.153032625976,-31.8123800687763,27.6023234246674));
#27840=CARTESIAN_POINT('Ctrl Pts',(131.055384994923,-31.7770587610663,27.6084239483995));
#27841=CARTESIAN_POINT('Ctrl Pts',(130.956222861508,-31.7462681998162,27.6145244721317));
#27842=CARTESIAN_POINT('Ctrl Pts',(130.856005011475,-31.7201127332132,27.6206249958638));
#27843=CARTESIAN_POINT('Ctrl Pts',(130.777033700421,-31.6995023181207,27.6254321869687));
#27844=CARTESIAN_POINT('Ctrl Pts',(130.697407165734,-31.6817690097786,27.6302393780737));
#27845=CARTESIAN_POINT('Ctrl Pts',(130.617352600343,-31.6669412202377,27.6350465691787));
#27846=CARTESIAN_POINT('Ctrl Pts',(130.515741023193,-31.6481206186452,27.6411482358038));
#27847=CARTESIAN_POINT('Ctrl Pts',(130.413096306608,-31.633919041833,27.6472499024289));
#27848=CARTESIAN_POINT('Ctrl Pts',(130.309874584419,-31.6244433341401,27.653351569054));
#27849=CARTESIAN_POINT('Ctrl Pts',(130.206788633678,-31.6149800902052,27.6594452099254));
#27850=CARTESIAN_POINT('Ctrl Pts',(130.103127608539,-31.6102303962829,27.6655388507969));
#27851=CARTESIAN_POINT('Ctrl Pts',(129.999357636771,-31.6102500608644,27.6716324916684));
#27852=CARTESIAN_POINT('Ctrl Pts',(129.895694466417,-31.6102697052069,27.6777198608849));
#27853=CARTESIAN_POINT('Ctrl Pts',(129.79192299789,-31.6150489470218,27.6838072301015));
#27854=CARTESIAN_POINT('Ctrl Pts',(129.688513408595,-31.6245917038268,27.689894599318));
#27855=CARTESIAN_POINT('Ctrl Pts',(129.585177379706,-31.6341276723923,27.6959776382848));
#27856=CARTESIAN_POINT('Ctrl Pts',(129.482203142843,-31.6484203783877,27.7020606772516));
#27857=CARTESIAN_POINT('Ctrl Pts',(129.380058966024,-31.667421692309,27.7081437162183));
#27858=CARTESIAN_POINT('Ctrl Pts',(129.277952605832,-31.6864159714132,27.7142245030741));
#27859=CARTESIAN_POINT('Ctrl Pts',(129.176676115,-31.7101153156768,27.72030528993));
#27860=CARTESIAN_POINT('Ctrl Pts',(129.076689946649,-31.7384200748898,27.7263860767858));
#27861=CARTESIAN_POINT('Ctrl Pts',(128.976714892158,-31.7667216879166,27.7324661877381));
#27862=CARTESIAN_POINT('Ctrl Pts',(128.878030286519,-31.7996275814483,27.7385462986903));
#27863=CARTESIAN_POINT('Ctrl Pts',(128.781082850265,-31.8369878209873,27.7446264096426));
#27864=CARTESIAN_POINT('Ctrl Pts',(128.684121073889,-31.8743535867208,27.7507074199434));
#27865=CARTESIAN_POINT('Ctrl Pts',(128.58889737658,-31.9161748536409,27.7567884302442));
#27866=CARTESIAN_POINT('Ctrl Pts',(128.495839017465,-31.962253334934,27.762869440545));
#27867=CARTESIAN_POINT('Ctrl Pts',(128.402684069356,-32.0083796429266,27.7689567625697));
#27868=CARTESIAN_POINT('Ctrl Pts',(128.311699331944,-32.0587717996961,27.7750440845944));
#27869=CARTESIAN_POINT('Ctrl Pts',(128.223287898296,-32.1131852899503,27.7811314066191));
#27870=CARTESIAN_POINT('Ctrl Pts',(128.134828964388,-32.1676280146015,27.7872219991414));
#27871=CARTESIAN_POINT('Ctrl Pts',(128.048946441808,-32.2260961355533,27.7933125916637));
#27872=CARTESIAN_POINT('Ctrl Pts',(127.966013176318,-32.2883026231553,27.7994031841859));
#27873=CARTESIAN_POINT('Ctrl Pts',(127.882944520295,-32.3506106643308,27.8055037197457));
#27874=CARTESIAN_POINT('Ctrl Pts',(127.802835070017,-32.4166689917352,27.8116042553054));
#27875=CARTESIAN_POINT('Ctrl Pts',(127.726023589787,-32.4861510888093,27.8177047908651));
#27876=CARTESIAN_POINT('Ctrl Pts',(127.665497969812,-32.5409013291376,27.8225118678258));
#27877=CARTESIAN_POINT('Ctrl Pts',(127.607019413902,-32.5977766009208,27.8273189447864));
#27878=CARTESIAN_POINT('Ctrl Pts',(127.550736213157,-32.6566024739796,27.8321260217471));
#27879=CARTESIAN_POINT('Ctrl Pts',(127.480210872341,-32.7303138957067,27.8381495018707));
#27880=CARTESIAN_POINT('Ctrl Pts',(127.412881597948,-32.8073526954095,27.8441729819944));
#27881=CARTESIAN_POINT('Ctrl Pts',(127.349084152318,-32.8874067521153,27.850196462118));
#27882=CARTESIAN_POINT('Ctrl Pts',(127.285385722298,-32.9673365624479,27.856210593614));
#27883=CARTESIAN_POINT('Ctrl Pts',(127.225208491823,-33.0502719824567,27.8622247251101));
#27884=CARTESIAN_POINT('Ctrl Pts',(127.168851233696,-33.1358643489396,27.8682388566061));
#27885=CARTESIAN_POINT('Ctrl Pts',(127.112544514999,-33.2213799588598,27.8742475948168));
#27886=CARTESIAN_POINT('Ctrl Pts',(127.060051206712,-33.3095474187509,27.8802563330275));
#27887=CARTESIAN_POINT('Ctrl Pts',(127.011629294196,-33.3999857540655,27.8862650712381));
#27888=CARTESIAN_POINT('Ctrl Pts',(126.96323952536,-33.4903640541445,27.8922698206976));
#27889=CARTESIAN_POINT('Ctrl Pts',(126.918915988411,-33.58300984726,27.8982745701571));
#27890=CARTESIAN_POINT('Ctrl Pts',(126.878872257577,-33.6775149611506,27.9042793196166));
#27891=CARTESIAN_POINT('Ctrl Pts',(126.858553142843,-33.7254690406571,27.9073262683069));
#27892=CARTESIAN_POINT('Ctrl Pts',(126.839335262333,-33.7739014433273,27.9103732169973));
#27893=CARTESIAN_POINT('Ctrl Pts',(126.821241915871,-33.8227565650715,27.9134201656876));
#27894=CARTESIAN_POINT('Origin',(130.,-35.,23.));
#27895=CARTESIAN_POINT('',(126.821241931958,-33.822756521634,29.1634528404117));
#27896=CARTESIAN_POINT('',(126.821241915871,-33.8227565650717,28.8235739384178));
#27897=CARTESIAN_POINT('',(126.821241915871,-33.8227565650715,23.));
#27898=CARTESIAN_POINT('',(132.573234427015,-32.7934484719078,30.));
#27899=CARTESIAN_POINT('Ctrl Pts',(132.573234427015,-32.7934484719079,29.9999999999999));
#27900=CARTESIAN_POINT('Ctrl Pts',(132.579611511435,-32.8008852949168,29.9994250391984));
#27901=CARTESIAN_POINT('Ctrl Pts',(132.585956399471,-32.8083498133881,29.9988519729851));
#27902=CARTESIAN_POINT('Ctrl Pts',(132.600007252001,-32.825026072687,29.9975804179708));
#27903=CARTESIAN_POINT('Ctrl Pts',(132.607696829063,-32.8342515035189,29.9968828466264));
#27904=CARTESIAN_POINT('Ctrl Pts',(132.637470118023,-32.8703599354667,29.9941745295691));
#27905=CARTESIAN_POINT('Ctrl Pts',(132.659189092145,-32.8975421629648,29.9921828548663));
#27906=CARTESIAN_POINT('Ctrl Pts',(132.802145611422,-33.0822183703115,29.9789321000128));
#27907=CARTESIAN_POINT('Ctrl Pts',(132.909756478062,-33.2497897358446,29.9682440386));
#27908=CARTESIAN_POINT('Ctrl Pts',(133.073150607209,-33.5613965661057,29.9491490506503));
#27909=CARTESIAN_POINT('Ctrl Pts',(133.134966297491,-33.7016099934545,29.9408058913643));
#27910=CARTESIAN_POINT('Ctrl Pts',(133.20739195755,-33.9015492648347,29.9288672165697));
#27911=CARTESIAN_POINT('Ctrl Pts',(133.226208331665,-33.9581091836126,29.9254867018423));
#27912=CARTESIAN_POINT('Ctrl Pts',(133.253211617292,-34.0470408397768,29.9201490433486));
#27913=CARTESIAN_POINT('Ctrl Pts',(133.262428340742,-34.0790883825275,29.9182211637458));
#27914=CARTESIAN_POINT('Ctrl Pts',(133.278849847665,-34.1395311560066,29.9145740152084));
#27915=CARTESIAN_POINT('Ctrl Pts',(133.286162290575,-34.1678940680356,29.9128580448567));
#27916=CARTESIAN_POINT('Ctrl Pts',(133.30192669742,-34.2324914783355,29.9089376781382));
#27917=CARTESIAN_POINT('Ctrl Pts',(133.310151375338,-34.2687770764245,29.9067268805151));
#27918=CARTESIAN_POINT('Ctrl Pts',(133.333562014955,-34.3805648282459,29.8998854252298));
#27919=CARTESIAN_POINT('Ctrl Pts',(133.346772919315,-34.4564511986565,29.8951981720216));
#27920=CARTESIAN_POINT('Ctrl Pts',(133.393620096028,-34.7930443915162,29.8741973720993));
#27921=CARTESIAN_POINT('Ctrl Pts',(133.399446949911,-35.0566731102899,29.8571068577239));
#27922=CARTESIAN_POINT('Ctrl Pts',(133.364491187454,-35.4273159581913,29.8329885651439));
#27923=CARTESIAN_POINT('Ctrl Pts',(133.348928839309,-35.5357967083164,29.8259326655496));
#27924=CARTESIAN_POINT('Ctrl Pts',(133.316043062173,-35.7059224879963,29.8150225986625));
#27925=CARTESIAN_POINT('Ctrl Pts',(133.302181718188,-35.7681569793268,29.8110656306506));
#27926=CARTESIAN_POINT('Ctrl Pts',(133.281035730172,-35.851892579397,29.8058180836199));
#27927=CARTESIAN_POINT('Ctrl Pts',(133.275279491917,-35.8737624051622,29.8044547156108));
#27928=CARTESIAN_POINT('Ctrl Pts',(133.265241320972,-35.9104068951055,29.8021841213498));
#27929=CARTESIAN_POINT('Ctrl Pts',(133.261076992772,-35.9252126603911,29.801270532542));
#27930=CARTESIAN_POINT('Ctrl Pts',(133.252324285727,-35.9555384341778,29.7994078136172));
#27931=CARTESIAN_POINT('Ctrl Pts',(133.247725271621,-35.9710548565745,29.7984593973338));
#27932=CARTESIAN_POINT('Ctrl Pts',(133.234926992402,-36.0131262363495,29.7958990232918));
#27933=CARTESIAN_POINT('Ctrl Pts',(133.226511783729,-36.039614945532,29.7942991173387));
#27934=CARTESIAN_POINT('Ctrl Pts',(133.171831395826,-36.2046705821193,29.784388228408));
#27935=CARTESIAN_POINT('Ctrl Pts',(133.116969803896,-36.3402439961798,29.7765025398196));
#27936=CARTESIAN_POINT('Ctrl Pts',(132.944943736513,-36.6971282521409,29.7553920149646));
#27937=CARTESIAN_POINT('Ctrl Pts',(132.811778273929,-36.9096690530237,29.7423700365931));
#27938=CARTESIAN_POINT('Ctrl Pts',(132.617151624161,-37.1552087535418,29.7249890956176));
#27939=CARTESIAN_POINT('Ctrl Pts',(132.576475272214,-37.2036746248411,29.7214333632558));
#27940=CARTESIAN_POINT('Ctrl Pts',(132.513621493501,-37.274444459706,29.7160308332342));
#27941=CARTESIAN_POINT('Ctrl Pts',(132.492450045524,-37.2976255756651,29.7142257692305));
#27942=CARTESIAN_POINT('Ctrl Pts',(132.453564677613,-37.339032097701,29.7109345050955));
#27943=CARTESIAN_POINT('Ctrl Pts',(132.43596180134,-37.3573588674686,29.7094531893193));
#27944=CARTESIAN_POINT('Ctrl Pts',(132.39747363265,-37.39653837362,29.7062316254048));
#27945=CARTESIAN_POINT('Ctrl Pts',(132.376518849585,-37.41731960388,29.7044883149132));
#27946=CARTESIAN_POINT('Ctrl Pts',(132.317915794874,-37.4739387567862,29.6996403548318));
#27947=CARTESIAN_POINT('Ctrl Pts',(132.279711736574,-37.5091872258359,29.696510251551));
#27948=CARTESIAN_POINT('Ctrl Pts',(132.016349635554,-37.7411940681912,29.6751226057618));
#27949=CARTESIAN_POINT('Ctrl Pts',(131.766850229018,-37.9082615466856,29.6556005379831));
#27950=CARTESIAN_POINT('Ctrl Pts',(131.382386418046,-38.0977806878159,29.6278685445383));
#27951=CARTESIAN_POINT('Ctrl Pts',(131.262808845141,-38.1484213961159,29.6195585485893));
#27952=CARTESIAN_POINT('Ctrl Pts',(131.108989185093,-38.2033850515808,29.6094929774765));
#27953=CARTESIAN_POINT('Ctrl Pts',(131.077198029626,-38.2142148967209,29.6074453913095));
#27954=CARTESIAN_POINT('Ctrl Pts',(131.029016338119,-38.2298330691815,29.6043969062004));
#27955=CARTESIAN_POINT('Ctrl Pts',(131.012742925569,-38.2349726543789,29.6033766106406));
#27956=CARTESIAN_POINT('Ctrl Pts',(130.982363649703,-38.2443155409405,29.6014901961562));
#27957=CARTESIAN_POINT('Ctrl Pts',(130.968267981001,-38.2485502620121,29.6006222024175));
#27958=CARTESIAN_POINT('Ctrl Pts',(130.935691366313,-38.2581062849303,29.5986319947837));
#27959=CARTESIAN_POINT('Ctrl Pts',(130.917191647699,-38.2633624402099,29.5975134750781));
#27960=CARTESIAN_POINT('Ctrl Pts',(130.856787385743,-38.2799703032837,29.5938963385894));
#27961=CARTESIAN_POINT('Ctrl Pts',(130.81470775166,-38.2906749245336,29.5914311190113));
#27962=CARTESIAN_POINT('Ctrl Pts',(130.564644581916,-38.3491972090907,29.577040756179));
#27963=CARTESIAN_POINT('Ctrl Pts',(130.352708317561,-38.3781001377415,29.5658758599012));
#27964=CARTESIAN_POINT('Ctrl Pts',(129.973222249421,-38.3937242997488,29.5457251332386));
#27965=CARTESIAN_POINT('Ctrl Pts',(129.806731897867,-38.3883215358424,29.5368323424307));
#27966=CARTESIAN_POINT('Ctrl Pts',(129.577289571825,-38.3639065831947,29.5240203610878));
#27967=CARTESIAN_POINT('Ctrl Pts',(129.513467688545,-38.3552700610506,29.520397961575));
#27968=CARTESIAN_POINT('Ctrl Pts',(129.417831613124,-38.3395423952033,29.514862402352));
#27969=CARTESIAN_POINT('Ctrl Pts',(129.385808589249,-38.3338014707419,29.5129906272664));
#27970=CARTESIAN_POINT('Ctrl Pts',(129.330243225254,-38.3230122462417,29.5097089245382));
#27971=CARTESIAN_POINT('Ctrl Pts',(129.306662534691,-38.3181723345035,29.5083055660848));
#27972=CARTESIAN_POINT('Ctrl Pts',(129.253411948365,-38.3066503015099,29.5051114039644));
#27973=CARTESIAN_POINT('Ctrl Pts',(129.223776715518,-38.2998192766703,29.503316056454));
#27974=CARTESIAN_POINT('Ctrl Pts',(129.143583372027,-38.2801943828873,29.4984081103108));
#27975=CARTESIAN_POINT('Ctrl Pts',(129.093223673764,-38.2666314269643,29.4952718898123));
#27976=CARTESIAN_POINT('Ctrl Pts',(128.832934569379,-38.1900472948139,29.4787729263559));
#27977=CARTESIAN_POINT('Ctrl Pts',(128.629193782588,-38.107942874097,29.4648218878101));
#27978=CARTESIAN_POINT('Ctrl Pts',(128.31810376963,-37.9460053142572,29.4422925904713));
#27979=CARTESIAN_POINT('Ctrl Pts',(128.205010172565,-37.8784954791242,29.4338250411977));
#27980=CARTESIAN_POINT('Ctrl Pts',(128.038064456554,-37.7651651766539,29.4211369636581));
#27981=CARTESIAN_POINT('Ctrl Pts',(127.981237953753,-37.7239549659096,29.4167829297808));
#27982=CARTESIAN_POINT('Ctrl Pts',(127.907174969473,-37.6666530958381,29.4111019366394));
#27983=CARTESIAN_POINT('Ctrl Pts',(127.888770577908,-37.6521059056849,29.4096897189001));
#27984=CARTESIAN_POINT('Ctrl Pts',(127.858314424734,-37.6275147922911,29.4073539528856));
#27985=CARTESIAN_POINT('Ctrl Pts',(127.846178886392,-37.6175763077851,29.40642357703));
#27986=CARTESIAN_POINT('Ctrl Pts',(127.821322530603,-37.5969301082211,29.4045194048611));
#27987=CARTESIAN_POINT('Ctrl Pts',(127.808610703635,-37.586212380994,29.4035463339465));
#27988=CARTESIAN_POINT('Ctrl Pts',(127.774414690168,-37.556947517734,29.4009291241242));
#27989=CARTESIAN_POINT('Ctrl Pts',(127.753083287517,-37.5382229960679,29.3992969924296));
#27990=CARTESIAN_POINT('Ctrl Pts',(127.627017702105,-37.4247288287836,29.3896368417002));
#27991=CARTESIAN_POINT('Ctrl Pts',(127.528044719206,-37.3237469682956,29.3819890242514));
#27992=CARTESIAN_POINT('Ctrl Pts',(127.306050963309,-37.0669580246055,29.3638540851373));
#27993=CARTESIAN_POINT('Ctrl Pts',(127.189847421728,-36.9059691949673,29.3534822868552));
#27994=CARTESIAN_POINT('Ctrl Pts',(127.050931797165,-36.6729459682225,29.3387476980586));
#27995=CARTESIAN_POINT('Ctrl Pts',(127.015534118904,-36.6089481059611,29.3347302355318));
#27996=CARTESIAN_POINT('Ctrl Pts',(126.956287445656,-36.4931391872167,29.3274678062916));
#27997=CARTESIAN_POINT('Ctrl Pts',(126.931623991883,-36.4417763002849,29.3242494566258));
#27998=CARTESIAN_POINT('Ctrl Pts',(126.895546432862,-36.3615196467383,29.3192115070047));
#27999=CARTESIAN_POINT('Ctrl Pts',(126.8832148667,-36.3330484013627,29.3174225937205));
#28000=CARTESIAN_POINT('Ctrl Pts',(126.861053491503,-36.2798928078993,29.3140776791192));
#28001=CARTESIAN_POINT('Ctrl Pts',(126.851119654777,-36.2552542751105,29.3125252832496));
#28002=CARTESIAN_POINT('Ctrl Pts',(126.829609979132,-36.2000420030781,29.309041039671));
#28003=CARTESIAN_POINT('Ctrl Pts',(126.818184886186,-36.1694127429295,29.3071044184487));
#28004=CARTESIAN_POINT('Ctrl Pts',(126.785147905498,-36.0767743224212,29.3012339886558));
#28005=CARTESIAN_POINT('Ctrl Pts',(126.764894028021,-36.0143004454116,29.2972572611331));
#28006=CARTESIAN_POINT('Ctrl Pts',(126.661228634267,-35.6597483103477,29.2745808361231));
#28007=CARTESIAN_POINT('Ctrl Pts',(126.615569562297,-35.3581038595991,29.2547105263846));
#28008=CARTESIAN_POINT('Ctrl Pts',(126.609585600672,-34.9859259006388,29.2309812864319));
#28009=CARTESIAN_POINT('Ctrl Pts',(126.610564123725,-34.9173363804271,29.2266491728853));
#28010=CARTESIAN_POINT('Ctrl Pts',(126.615680876302,-34.8027225403464,29.2195243435344));
#28011=CARTESIAN_POINT('Ctrl Pts',(126.61868003125,-34.7566688717514,29.2166924944106));
#28012=CARTESIAN_POINT('Ctrl Pts',(126.624323906089,-34.6907830767939,29.2126987695243));
#28013=CARTESIAN_POINT('Ctrl Pts',(126.62620502512,-34.670892560446,29.2115006421746));
#28014=CARTESIAN_POINT('Ctrl Pts',(126.629803079382,-34.636129328525,29.2094212137074));
#28015=CARTESIAN_POINT('Ctrl Pts',(126.631442851152,-34.6212495352094,29.2085358866884));
#28016=CARTESIAN_POINT('Ctrl Pts',(126.635258901757,-34.5886090202942,29.2066045306057));
#28017=CARTESIAN_POINT('Ctrl Pts',(126.63747728662,-34.5708540696618,29.2055607737064));
#28018=CARTESIAN_POINT('Ctrl Pts',(126.644464713786,-34.5183148045883,29.2024901713332));
#28019=CARTESIAN_POINT('Ctrl Pts',(126.649633822217,-34.4835850871588,29.2004838618329));
#28020=CARTESIAN_POINT('Ctrl Pts',(126.685445527855,-34.2662257532156,29.1880396855573));
#28021=CARTESIAN_POINT('Ctrl Pts',(126.730474293754,-34.0862647071683,29.1782250990549));
#28022=CARTESIAN_POINT('Ctrl Pts',(126.800000382245,-33.8813493953562,29.1667560690774));
#28023=CARTESIAN_POINT('Ctrl Pts',(126.810420543352,-33.851976115516,29.1651051327837));
#28024=CARTESIAN_POINT('Ctrl Pts',(126.821241931958,-33.822756521634,29.1634528404117));
#28025=CARTESIAN_POINT('',(127.462899484434,-32.7519950986681,30.));
#28026=CARTESIAN_POINT('Origin',(130.,-35.,30.));
#28027=CARTESIAN_POINT('Ctrl Pts',(127.462899484433,-32.7519950986684,30.));
#28028=CARTESIAN_POINT('Ctrl Pts',(127.478841211814,-32.7340032496596,29.9985247980324));
#28029=CARTESIAN_POINT('Ctrl Pts',(127.494973853206,-32.7161815072181,29.9970389843388));
#28030=CARTESIAN_POINT('Ctrl Pts',(127.655532556121,-32.54256038369,29.982332718974));
#28031=CARTESIAN_POINT('Ctrl Pts',(127.814107040654,-32.4004994717988,29.968479649082));
#28032=CARTESIAN_POINT('Ctrl Pts',(128.115334933663,-32.1778123164891,29.9444203697092));
#28033=CARTESIAN_POINT('Ctrl Pts',(128.25250588551,-32.0908797629625,29.9341499832904));
#28034=CARTESIAN_POINT('Ctrl Pts',(128.45155791788,-31.9839100841736,29.920297256416));
#28035=CARTESIAN_POINT('Ctrl Pts',(128.508570815153,-31.9553142916071,29.9164394224824));
#28036=CARTESIAN_POINT('Ctrl Pts',(128.595733202631,-31.9146328270807,29.9107021911106));
#28037=CARTESIAN_POINT('Ctrl Pts',(128.625302752653,-31.9013449019518,29.9087829390122));
#28038=CARTESIAN_POINT('Ctrl Pts',(128.677145548552,-31.8789360607914,29.9054637086128));
#28039=CARTESIAN_POINT('Ctrl Pts',(128.699333377025,-31.8696245605349,29.9040574879752));
#28040=CARTESIAN_POINT('Ctrl Pts',(128.749864592398,-31.8490482974775,29.9008864454266));
#28041=CARTESIAN_POINT('Ctrl Pts',(128.778264846292,-31.8379281365532,29.8991264565951));
#28042=CARTESIAN_POINT('Ctrl Pts',(128.856001255967,-31.8086940426138,29.8943666083622));
#28043=CARTESIAN_POINT('Ctrl Pts',(128.90561572349,-31.7913413546243,29.8913912147908));
#28044=CARTESIAN_POINT('Ctrl Pts',(129.145569309334,-31.7136311688059,29.877266612353));
#28045=CARTESIAN_POINT('Ctrl Pts',(129.340591592957,-31.6690148984837,29.8666083712587));
#28046=CARTESIAN_POINT('Ctrl Pts',(129.682440454129,-31.6220280860358,29.8482471185181));
#28047=CARTESIAN_POINT('Ctrl Pts',(129.827576050535,-31.6115189341251,29.8405386994585));
#28048=CARTESIAN_POINT('Ctrl Pts',(130.047103311534,-31.6097657177983,29.8284892634394));
#28049=CARTESIAN_POINT('Ctrl Pts',(130.121271913425,-31.6116082245879,29.824349898015));
#28050=CARTESIAN_POINT('Ctrl Pts',(130.219171643299,-31.6172585246066,29.8187278936532));
#28051=CARTESIAN_POINT('Ctrl Pts',(130.243012368907,-31.6188876062566,29.8173463537531));
#28052=CARTESIAN_POINT('Ctrl Pts',(130.282558175012,-31.6220102489604,29.815031123508));
#28053=CARTESIAN_POINT('Ctrl Pts',(130.298274058582,-31.6233616644061,29.8141048272922));
#28054=CARTESIAN_POINT('Ctrl Pts',(130.328354383573,-31.6261599205397,29.8123190440699));
#28055=CARTESIAN_POINT('Ctrl Pts',(130.342720117328,-31.6275889355883,29.8114605922281));
#28056=CARTESIAN_POINT('Ctrl Pts',(130.382474769113,-31.6318001172697,29.8090702732338));
#28057=CARTESIAN_POINT('Ctrl Pts',(130.407841512791,-31.6347774791618,29.8075284235628));
#28058=CARTESIAN_POINT('Ctrl Pts',(130.518019607285,-31.6489733676891,29.8007660386851));
#28059=CARTESIAN_POINT('Ctrl Pts',(130.602417394555,-31.6631130007462,29.7954173465248));
#28060=CARTESIAN_POINT('Ctrl Pts',(130.879267284407,-31.7203401710726,29.7774942745521));
#28061=CARTESIAN_POINT('Ctrl Pts',(131.068500370582,-31.7770218056226,29.764655914404));
#28062=CARTESIAN_POINT('Ctrl Pts',(131.351308686713,-31.8893971444937,29.7452544606234));
#28063=CARTESIAN_POINT('Ctrl Pts',(131.448955684109,-31.9336641162856,29.7385073746334));
#28064=CARTESIAN_POINT('Ctrl Pts',(131.611006246129,-32.0166007508257,29.7272730573135));
#28065=CARTESIAN_POINT('Ctrl Pts',(131.676519041654,-32.0529171360565,29.7227196617578));
#28066=CARTESIAN_POINT('Ctrl Pts',(131.770213909791,-32.1089924726446,29.7161887391315));
#28067=CARTESIAN_POINT('Ctrl Pts',(131.799380394573,-32.1270551459805,29.7141528423898));
#28068=CARTESIAN_POINT('Ctrl Pts',(131.850747165765,-32.1599555334545,29.7105609147107));
#28069=CARTESIAN_POINT('Ctrl Pts',(131.873055440775,-32.1746184294003,29.7089987569814));
#28070=CARTESIAN_POINT('Ctrl Pts',(131.92000067502,-32.2062752367217,29.705705628646));
#28071=CARTESIAN_POINT('Ctrl Pts',(131.944590573733,-32.2233350529725,29.7039772620414));
#28072=CARTESIAN_POINT('Ctrl Pts',(132.010884456967,-32.2706406563581,29.699305790333));
#28073=CARTESIAN_POINT('Ctrl Pts',(132.052130896932,-32.3015156293555,29.6963864161049));
#28074=CARTESIAN_POINT('Ctrl Pts',(132.289390947357,-32.487703850879,29.6794814776684));
#28075=CARTESIAN_POINT('Ctrl Pts',(132.468434798278,-32.6633820086602,29.6663382243855));
#28076=CARTESIAN_POINT('Ctrl Pts',(132.701678574942,-32.949276153876,29.6467361058599));
#28077=CARTESIAN_POINT('Ctrl Pts',(132.771921928922,-33.045267008513,29.6403887243119));
#28078=CARTESIAN_POINT('Ctrl Pts',(132.873229397983,-33.2001817236004,29.6301914059989));
#28079=CARTESIAN_POINT('Ctrl Pts',(132.907849138409,-33.2566683480162,29.6264815140026));
#28080=CARTESIAN_POINT('Ctrl Pts',(132.95214015839,-33.3339284522975,29.6213691645074));
#28081=CARTESIAN_POINT('Ctrl Pts',(132.963290077767,-33.3538415109323,29.6200481865427));
#28082=CARTESIAN_POINT('Ctrl Pts',(132.981626424686,-33.3873791058198,29.6178153262414));
#28083=CARTESIAN_POINT('Ctrl Pts',(132.98892281339,-33.4009431872959,29.6169100707665));
#28084=CARTESIAN_POINT('Ctrl Pts',(133.003830534246,-33.4291153764499,29.6150244439665));
#28085=CARTESIAN_POINT('Ctrl Pts',(133.011428224115,-33.4437299704328,29.61404333391));
#28086=CARTESIAN_POINT('Ctrl Pts',(133.031760495018,-33.4835466791367,29.6113636421677));
#28087=CARTESIAN_POINT('Ctrl Pts',(133.044286894435,-33.5088529366953,29.6096532817275));
#28088=CARTESIAN_POINT('Ctrl Pts',(133.120046781933,-33.6668399736745,29.5989443660502));
#28089=CARTESIAN_POINT('Ctrl Pts',(133.174905914532,-33.8033496357441,29.5895625758721));
#28090=CARTESIAN_POINT('Ctrl Pts',(133.281471636943,-34.1280523134781,29.5675694911915));
#28091=CARTESIAN_POINT('Ctrl Pts',(133.326152205909,-34.3180385577463,29.5549564921927));
#28092=CARTESIAN_POINT('Ctrl Pts',(133.36972174774,-34.6167908719486,29.536024700485));
#28093=CARTESIAN_POINT('Ctrl Pts',(133.380146996494,-34.7234428212229,29.5294332539337));
#28094=CARTESIAN_POINT('Ctrl Pts',(133.387437586222,-34.8689913901223,29.5206724233102));
#28095=CARTESIAN_POINT('Ctrl Pts',(133.388710411931,-34.9075955279075,29.5183707767972));
#28096=CARTESIAN_POINT('Ctrl Pts',(133.389753696899,-34.9733383841115,29.5144870565039));
#28097=CARTESIAN_POINT('Ctrl Pts',(133.389858524057,-35.0004672928326,29.5128948430668));
#28098=CARTESIAN_POINT('Ctrl Pts',(133.389411253268,-35.0554076119964,29.5096904800148));
#28099=CARTESIAN_POINT('Ctrl Pts',(133.388842527335,-35.0832168233847,29.508078967019));
#28100=CARTESIAN_POINT('Ctrl Pts',(133.386550082098,-35.1531762175458,29.504049492468));
#28101=CARTESIAN_POINT('Ctrl Pts',(133.384381706613,-35.1953077040938,29.5016453560981));
#28102=CARTESIAN_POINT('Ctrl Pts',(133.372460687514,-35.3651135568099,29.4920344302891));
#28103=CARTESIAN_POINT('Ctrl Pts',(133.356264153654,-35.4922341728441,29.4850242839034));
#28104=CARTESIAN_POINT('Ctrl Pts',(133.291253845684,-35.8427573564131,29.4658457972842));
#28105=CARTESIAN_POINT('Ctrl Pts',(133.226999465458,-36.0625712985417,29.4540203849703));
#28106=CARTESIAN_POINT('Ctrl Pts',(133.106509735553,-36.3595900471022,29.4366288513963));
#28107=CARTESIAN_POINT('Ctrl Pts',(133.06842631856,-36.4434836341209,29.4315405041469));
#28108=CARTESIAN_POINT('Ctrl Pts',(133.015626832986,-36.5482363884655,29.4248343268036));
#28109=CARTESIAN_POINT('Ctrl Pts',(133.004024775013,-36.5706292307663,29.4233795411865));
#28110=CARTESIAN_POINT('Ctrl Pts',(132.984749678343,-36.6068366625051,29.4209892164612));
#28111=CARTESIAN_POINT('Ctrl Pts',(132.977227754632,-36.6207311875072,29.4200626952523));
#28112=CARTESIAN_POINT('Ctrl Pts',(132.96289661719,-36.646767279017,29.4183081511374));
#28113=CARTESIAN_POINT('Ctrl Pts',(132.956109213911,-36.6589204729349,29.4174815623257));
#28114=CARTESIAN_POINT('Ctrl Pts',(132.937785525292,-36.6912604355233,29.4152623393041));
#28115=CARTESIAN_POINT('Ctrl Pts',(132.926116282433,-36.7113705295886,29.4138617507756));
#28116=CARTESIAN_POINT('Ctrl Pts',(132.881161450912,-36.7870389964753,29.4085179058602));
#28117=CARTESIAN_POINT('Ctrl Pts',(132.846494536307,-36.8417566178106,29.404501548168));
#28118=CARTESIAN_POINT('Ctrl Pts',(132.702015419951,-37.0559688978315,29.3882595657944));
#28119=CARTESIAN_POINT('Ctrl Pts',(132.58019513135,-37.2069177437768,29.3756533520406));
#28120=CARTESIAN_POINT('Ctrl Pts',(132.326516778446,-37.4713544647548,29.3521492712588));
#28121=CARTESIAN_POINT('Ctrl Pts',(132.197500432843,-37.5867505596752,29.3412452219469));
#28122=CARTESIAN_POINT('Ctrl Pts',(132.018403373966,-37.7238258186841,29.3275226926755));
#28123=CARTESIAN_POINT('Ctrl Pts',(131.975835265241,-37.7548602033877,29.3243539909629));
#28124=CARTESIAN_POINT('Ctrl Pts',(131.907841428439,-37.8020441361666,29.319433933198));
#28125=CARTESIAN_POINT('Ctrl Pts',(131.882895689877,-37.8188675324368,29.3176576704253));
#28126=CARTESIAN_POINT('Ctrl Pts',(131.835529955723,-37.8499016074708,29.3143376830527));
#28127=CARTESIAN_POINT('Ctrl Pts',(131.81316076269,-37.8641853114283,29.312791355883));
#28128=CARTESIAN_POINT('Ctrl Pts',(131.762018393016,-37.8960026539388,29.3093034313769));
#28129=CARTESIAN_POINT('Ctrl Pts',(131.733146691286,-37.9133731054648,29.3073678090876));
#28130=CARTESIAN_POINT('Ctrl Pts',(131.641991147098,-37.9663814352736,29.3013558756328));
#28131=CARTESIAN_POINT('Ctrl Pts',(131.578829922599,-38.0004750980198,29.2973333744503));
#28132=CARTESIAN_POINT('Ctrl Pts',(131.252019648092,-38.1637035901683,29.2771411035599));
#28133=CARTESIAN_POINT('Ctrl Pts',(130.97350536681,-38.2601919036173,29.2620646190058));
#28134=CARTESIAN_POINT('Ctrl Pts',(130.619652660696,-38.3333215818098,29.2425120947366));
#28135=CARTESIAN_POINT('Ctrl Pts',(130.552860181364,-38.3450481139434,29.2387983813863));
#28136=CARTESIAN_POINT('Ctrl Pts',(130.440488133104,-38.3613194147462,29.2324478714702));
#28137=CARTESIAN_POINT('Ctrl Pts',(130.395085801481,-38.366957795219,29.2298542281665));
#28138=CARTESIAN_POINT('Ctrl Pts',(130.32979457595,-38.3737273891108,29.2260671405981));
#28139=CARTESIAN_POINT('Ctrl Pts',(130.309986372578,-38.3756050369781,29.2249106671137));
#28140=CARTESIAN_POINT('Ctrl Pts',(130.275239074104,-38.3785903704842,29.222867023552));
#28141=CARTESIAN_POINT('Ctrl Pts',(130.260307365872,-38.379773587641,29.2219839179486));
#28142=CARTESIAN_POINT('Ctrl Pts',(130.227384564231,-38.3821629799518,29.2200255469682));
#28143=CARTESIAN_POINT('Ctrl Pts',(130.209391632011,-38.3833245891236,29.218948049829));
#28144=CARTESIAN_POINT('Ctrl Pts',(130.156968008969,-38.3862892405329,29.2157893696504));
#28145=CARTESIAN_POINT('Ctrl Pts',(130.122518980383,-38.3877105364792,29.2136894750293));
#28146=CARTESIAN_POINT('Ctrl Pts',(129.895417175012,-38.3936119651958,29.1997121813691));
#28147=CARTESIAN_POINT('Ctrl Pts',(129.70271627876,-38.3821815352064,29.187238437771));
#28148=CARTESIAN_POINT('Ctrl Pts',(129.35955108603,-38.3322630414233,29.1648971983666));
#28149=CARTESIAN_POINT('Ctrl Pts',(129.208735357683,-38.2997059179865,29.1550296461056));
#28150=CARTESIAN_POINT('Ctrl Pts',(128.969964921749,-38.2308420517709,29.139537255849));
#28151=CARTESIAN_POINT('Ctrl Pts',(128.880407351219,-38.2009104150179,29.1337543321659));
#28152=CARTESIAN_POINT('Ctrl Pts',(128.757504127495,-38.1540432216105,29.1258602729314));
#28153=CARTESIAN_POINT('Ctrl Pts',(128.723018091405,-38.1402391639313,29.1236497478761));
#28154=CARTESIAN_POINT('Ctrl Pts',(128.663882468747,-38.1154330487683,29.119865646685));
#28155=CARTESIAN_POINT('Ctrl Pts',(128.639125098898,-38.1046984885592,29.1182833885195));
#28156=CARTESIAN_POINT('Ctrl Pts',(128.588523932318,-38.0820367194559,29.115052520482));
#28157=CARTESIAN_POINT('Ctrl Pts',(128.562696843926,-38.0700773180777,29.113405148314));
#28158=CARTESIAN_POINT('Ctrl Pts',(128.496562655612,-38.0384359410375,29.1091892517985));
#28159=CARTESIAN_POINT('Ctrl Pts',(128.456489418936,-38.0182763569392,29.1066371084714));
#28160=CARTESIAN_POINT('Ctrl Pts',(128.254323285386,-37.9114931952036,29.0937550470773));
#28161=CARTESIAN_POINT('Ctrl Pts',(128.099061997621,-37.8125832459622,29.0838613236284));
#28162=CARTESIAN_POINT('Ctrl Pts',(127.811353882473,-37.5945385142546,29.0646668353547));
#28163=CARTESIAN_POINT('Ctrl Pts',(127.67875235352,-37.4766116070571,29.0553819285376));
#28164=CARTESIAN_POINT('Ctrl Pts',(127.498935781337,-37.2895109809737,29.0412241209243));
#28165=CARTESIAN_POINT('Ctrl Pts',(127.444074416775,-37.2280989948424,29.0366526011648));
#28166=CARTESIAN_POINT('Ctrl Pts',(127.375879868763,-37.1459257648364,29.0305394849632));
#28167=CARTESIAN_POINT('Ctrl Pts',(127.360457617432,-37.1269273114062,29.0291263665175));
#28168=CARTESIAN_POINT('Ctrl Pts',(127.33547836026,-37.0954656031604,29.0267835195185));
#28169=CARTESIAN_POINT('Ctrl Pts',(127.325799585962,-37.0830995635218,29.0258619889336));
#28170=CARTESIAN_POINT('Ctrl Pts',(127.307612767747,-37.0595276165547,29.0241031751704));
#28171=CARTESIAN_POINT('Ctrl Pts',(127.299087894945,-37.0483351280391,29.0232671443138));
#28172=CARTESIAN_POINT('Ctrl Pts',(127.276172238462,-37.0178568884208,29.0209888472522));
#28173=CARTESIAN_POINT('Ctrl Pts',(127.26191701453,-36.9984708126906,29.0195378792274));
#28174=CARTESIAN_POINT('Ctrl Pts',(127.206137943803,-36.9208981563015,29.0137300273212));
#28175=CARTESIAN_POINT('Ctrl Pts',(127.166255116018,-36.8615594071029,29.0092835258124));
#28176=CARTESIAN_POINT('Ctrl Pts',(127.028235051219,-36.6414855896818,28.992899063843));
#28177=CARTESIAN_POINT('Ctrl Pts',(126.941657674828,-36.4739072011151,28.9806426900215));
#28178=CARTESIAN_POINT('Ctrl Pts',(126.798564021562,-36.1293230860652,28.9567220587969));
#28179=CARTESIAN_POINT('Ctrl Pts',(126.741753860513,-35.9531065428809,28.9450926735559));
#28180=CARTESIAN_POINT('Ctrl Pts',(126.689441068281,-35.7297843032429,28.9312280638086));
#28181=CARTESIAN_POINT('Ctrl Pts',(126.680145050042,-35.6862572137455,28.9285642615742));
#28182=CARTESIAN_POINT('Ctrl Pts',(126.666330870643,-35.6147031903601,28.9242462511849));
#28183=CARTESIAN_POINT('Ctrl Pts',(126.661302997939,-35.5867812862212,28.9225763278949));
#28184=CARTESIAN_POINT('Ctrl Pts',(126.652177311346,-35.5321809962047,28.9193391717641));
#28185=CARTESIAN_POINT('Ctrl Pts',(126.648046435952,-35.5055103694541,28.9177710196791));
#28186=CARTESIAN_POINT('Ctrl Pts',(126.638966803628,-35.4418729764437,28.9140590905716));
#28187=CARTESIAN_POINT('Ctrl Pts',(126.634308685247,-35.4048678848587,28.9119244408266));
#28188=CARTESIAN_POINT('Ctrl Pts',(126.620540237047,-35.2787204598076,28.9047217289337));
#28189=CARTESIAN_POINT('Ctrl Pts',(126.6143533784,-35.1892938167239,28.8997423539257));
#28190=CARTESIAN_POINT('Ctrl Pts',(126.603771012355,-34.8297322796127,28.8800693369051));
#28191=CARTESIAN_POINT('Ctrl Pts',(126.628122280371,-34.5597800057159,28.8661652196633));
#28192=CARTESIAN_POINT('Ctrl Pts',(126.697999995049,-34.23085757422,28.8479563580422));
#28193=CARTESIAN_POINT('Ctrl Pts',(126.713643320526,-34.1665475392923,28.8443288430707));
#28194=CARTESIAN_POINT('Ctrl Pts',(126.743057430617,-34.0593878775331,28.838110459357));
#28195=CARTESIAN_POINT('Ctrl Pts',(126.75581773537,-34.0162789525637,28.8355606692214));
#28196=CARTESIAN_POINT('Ctrl Pts',(126.775405901636,-33.9546353599272,28.8318281892463));
#28197=CARTESIAN_POINT('Ctrl Pts',(126.781544843671,-33.9358850175106,28.8306812242449));
#28198=CARTESIAN_POINT('Ctrl Pts',(126.79261855824,-33.9030348773328,28.8286495218307));
#28199=CARTESIAN_POINT('Ctrl Pts',(126.797483389167,-33.8889124525811,28.8277687306515));
#28200=CARTESIAN_POINT('Ctrl Pts',(126.808444380887,-33.8577632314348,28.8258093683885));
#28201=CARTESIAN_POINT('Ctrl Pts',(126.814583478882,-33.8407529771556,28.8247284833112));
#28202=CARTESIAN_POINT('Ctrl Pts',(126.820986072869,-33.8234475577599,28.8236182809077));
#28203=CARTESIAN_POINT('Ctrl Pts',(126.821113966276,-33.8231020508019,28.8235961111341));
#28204=CARTESIAN_POINT('Ctrl Pts',(126.821241915871,-33.8227565650717,28.8235739384178));
#28205=CARTESIAN_POINT('Origin',(-10.,-35.,32.7603849714045));
#28206=CARTESIAN_POINT('',(-7.51282745730981,-31.7594448403263,18.0469656703996));
#28207=CARTESIAN_POINT('',(-7.51282745730979,-31.7594448403263,17.9425398458891));
#28208=CARTESIAN_POINT('',(-7.5128274573098,-31.7594448403263,32.7603849714045));
#28209=CARTESIAN_POINT('',(-14.0827617124838,-35.0055111943466,17.1353849829093));
#28210=CARTESIAN_POINT('Ctrl Pts',(-7.51282745730979,-31.7594448403263,
17.9425398458891));
#28211=CARTESIAN_POINT('Ctrl Pts',(-7.41830337030683,-31.8319934322288,
17.9367380944228));
#28212=CARTESIAN_POINT('Ctrl Pts',(-7.32686995564933,-31.9087474254191,
17.9309363429564));
#28213=CARTESIAN_POINT('Ctrl Pts',(-7.23891895494735,-31.9894092834377,
17.9251345914901));
#28214=CARTESIAN_POINT('Ctrl Pts',(-7.15101699404093,-32.0700261659473,
17.9193360749695));
#28215=CARTESIAN_POINT('Ctrl Pts',(-7.06659388623147,-32.1545463036953,
17.9135375584488));
#28216=CARTESIAN_POINT('Ctrl Pts',(-6.98600812104434,-32.242632060535,17.9077390419282));
#28217=CARTESIAN_POINT('Ctrl Pts',(-6.90544513829122,-32.3306929146151,
17.9019421647084));
#28218=CARTESIAN_POINT('Ctrl Pts',(-6.82871761722978,-32.422317081744,17.8961452874887));
#28219=CARTESIAN_POINT('Ctrl Pts',(-6.75614657546723,-32.5171307001481,
17.8903484102689));
#28220=CARTESIAN_POINT('Ctrl Pts',(-6.6835788188904,-32.6119400264773,17.8845517954654));
#28221=CARTESIAN_POINT('Ctrl Pts',(-6.61516741615517,-32.7099381918354,
17.8787551806619));
#28222=CARTESIAN_POINT('Ctrl Pts',(-6.55119212035181,-32.8107194767969,
17.8729585658584));
#28223=CARTESIAN_POINT('Ctrl Pts',(-6.48720453022862,-32.9115201291928,
17.8671608371024));
#28224=CARTESIAN_POINT('Ctrl Pts',(-6.42765496159749,-33.0151046191435,
17.8613631083465));
#28225=CARTESIAN_POINT('Ctrl Pts',(-6.37277863245117,-33.1210401412491,
17.8555653795906));
#28226=CARTESIAN_POINT('Ctrl Pts',(-6.31784438904388,-33.2270874634253,
17.8497615321459));
#28227=CARTESIAN_POINT('Ctrl Pts',(-6.2675934242897,-33.3354904093112,17.8439576847012));
#28228=CARTESIAN_POINT('Ctrl Pts',(-6.22221405330886,-33.4457933403235,
17.8381538372565));
#28229=CARTESIAN_POINT('Ctrl Pts',(-6.1768101584289,-33.5561558811958,17.8323468532993));
#28230=CARTESIAN_POINT('Ctrl Pts',(-6.13628324099394,-33.6684200677715,
17.826539869342));
#28231=CARTESIAN_POINT('Ctrl Pts',(-6.1007720966111,-33.7821138158952,17.8207328853847));
#28232=CARTESIAN_POINT('Ctrl Pts',(-6.0652035360177,-33.8959913898091,17.8149165124027));
#28233=CARTESIAN_POINT('Ctrl Pts',(-6.03466705613968,-34.0113027473889,
17.8091001394206));
#28234=CARTESIAN_POINT('Ctrl Pts',(-6.00925069731334,-34.127563754131,17.8032837664386));
#28235=CARTESIAN_POINT('Ctrl Pts',(-5.98745130943369,-34.227279799162,17.7982951143837));
#28236=CARTESIAN_POINT('Ctrl Pts',(-5.96941762182638,-34.3276941337255,
17.7933064623287));
#28237=CARTESIAN_POINT('Ctrl Pts',(-5.95517470999492,-34.4284990172053,
17.7883178102738));
#28238=CARTESIAN_POINT('Ctrl Pts',(-5.93851906885877,-34.5463801066818,
17.7824840875517));
#28239=CARTESIAN_POINT('Ctrl Pts',(-5.9269944808512,-34.6651770682635,17.7766503648296));
#28240=CARTESIAN_POINT('Ctrl Pts',(-5.92069314400233,-34.7844064597202,
17.7708166421075));
#28241=CARTESIAN_POINT('Ctrl Pts',(-5.91439976709298,-34.9034852388912,
17.764990288628));
#28242=CARTESIAN_POINT('Ctrl Pts',(-5.9133165382126,-35.0229949586629,17.7591639351485));
#28243=CARTESIAN_POINT('Ctrl Pts',(-5.91748427346542,-35.1424441736183,
17.753337581669));
#28244=CARTESIAN_POINT('Ctrl Pts',(-5.92164781989202,-35.261773334882,17.7475170840274));
#28245=CARTESIAN_POINT('Ctrl Pts',(-5.93105181658592,-35.3810417080726,
17.7416965863859));
#28246=CARTESIAN_POINT('Ctrl Pts',(-5.94568508665268,-35.4997555236408,
17.7358760887443));
#28247=CARTESIAN_POINT('Ctrl Pts',(-5.96083644705803,-35.6226723970781,
17.7298495166177));
#28248=CARTESIAN_POINT('Ctrl Pts',(-5.98159424722097,-35.7449942738863,
17.7238229444911));
#28249=CARTESIAN_POINT('Ctrl Pts',(-6.00788719817211,-35.8661757197485,
17.7177963723644));
#28250=CARTESIAN_POINT('Ctrl Pts',(-6.03325190179439,-35.9830789712902,
17.7119825625667));
#28251=CARTESIAN_POINT('Ctrl Pts',(-6.06376744677097,-36.0989205224302,
17.706168752769));
#28252=CARTESIAN_POINT('Ctrl Pts',(-6.09931751766941,-36.2132193420974,
17.7003549429713));
#28253=CARTESIAN_POINT('Ctrl Pts',(-6.13486190666894,-36.3274998936059,
17.6945420623836));
#28254=CARTESIAN_POINT('Ctrl Pts',(-6.17543910039763,-36.4402378157443,
17.6887291817958));
#28255=CARTESIAN_POINT('Ctrl Pts',(-6.22088278486858,-36.5509668192122,
17.6829163012081));
#28256=CARTESIAN_POINT('Ctrl Pts',(-6.26632982913655,-36.6617040092297,
17.6771029908555));
#28257=CARTESIAN_POINT('Ctrl Pts',(-6.31664392498955,-36.7704316089549,
17.6712896805029));
#28258=CARTESIAN_POINT('Ctrl Pts',(-6.37161068595107,-36.8767034890189,
17.6654763701502));
#28259=CARTESIAN_POINT('Ctrl Pts',(-6.42659435971158,-36.9830080680251,
17.6596612710921));
#28260=CARTESIAN_POINT('Ctrl Pts',(-6.48623335900731,-37.0868550634284,
17.6538461720339));
#28261=CARTESIAN_POINT('Ctrl Pts',(-6.55026775161833,-37.1878236707915,
17.6480310729758));
#28262=CARTESIAN_POINT('Ctrl Pts',(-6.61437088710802,-37.2889006710422,
17.642209731231));
#28263=CARTESIAN_POINT('Ctrl Pts',(-6.68287861686422,-37.3870927713628,
17.6363883894862));
#28264=CARTESIAN_POINT('Ctrl Pts',(-6.75548806402465,-37.4820087222477,
17.6305670477413));
#28265=CARTESIAN_POINT('Ctrl Pts',(-6.82814390425031,-37.5769853187106,
17.6247419865096));
#28266=CARTESIAN_POINT('Ctrl Pts',(-6.90490642128588,-37.6686812851157,
17.6189169252779));
#28267=CARTESIAN_POINT('Ctrl Pts',(-6.98543397023575,-37.7567402221086,
17.6130918640462));
#28268=CARTESIAN_POINT('Ctrl Pts',(-7.06607372756671,-37.8449218618398,
17.6072586860806));
#28269=CARTESIAN_POINT('Ctrl Pts',(-7.15048870197217,-37.9294560696016,
17.6014255081149));
#28270=CARTESIAN_POINT('Ctrl Pts',(-7.23830202914566,-38.0100248035156,
17.5955923301492));
#28271=CARTESIAN_POINT('Ctrl Pts',(-7.26015042859291,-38.0300707115591,
17.5941410060013));
#28272=CARTESIAN_POINT('Ctrl Pts',(-7.28220904940426,-38.0498713440633,
17.5926896818533));
#28273=CARTESIAN_POINT('Ctrl Pts',(-7.3044717991109,-38.0694222124386,17.5912383577053));
#28274=CARTESIAN_POINT('Ctrl Pts',(-7.39387079096929,-38.1479312890683,
17.5854103752055));
#28275=CARTESIAN_POINT('Ctrl Pts',(-7.48684366641138,-38.2226553293975,
17.5795823927056));
#28276=CARTESIAN_POINT('Ctrl Pts',(-7.58303683313338,-38.293252806878,17.5737544102058));
#28277=CARTESIAN_POINT('Ctrl Pts',(-7.67911044836402,-38.363762543888,17.5679336708816));
#28278=CARTESIAN_POINT('Ctrl Pts',(-7.77839606833716,-38.4301556801732,
17.5621129315574));
#28279=CARTESIAN_POINT('Ctrl Pts',(-7.88050527017014,-38.4921293060572,
17.5562921922332));
#28280=CARTESIAN_POINT('Ctrl Pts',(-7.98251404491423,-38.5540419792482,
17.5504771777594));
#28281=CARTESIAN_POINT('Ctrl Pts',(-8.08734053018008,-38.6115435794294,
17.5446621632855));
#28282=CARTESIAN_POINT('Ctrl Pts',(-8.19456589800467,-38.6643734393962,
17.5388471488117));
#28283=CARTESIAN_POINT('Ctrl Pts',(-8.30573107092183,-38.7191444384382,
17.5328184719919));
#28284=CARTESIAN_POINT('Ctrl Pts',(-8.41947443517335,-38.7688935336658,
17.5267897951722));
#28285=CARTESIAN_POINT('Ctrl Pts',(-8.53529918504936,-38.8133812453888,
17.5207611183524));
#28286=CARTESIAN_POINT('Ctrl Pts',(-8.64689736879917,-38.8562455540343,
17.514952434248));
#28287=CARTESIAN_POINT('Ctrl Pts',(-8.76042727961783,-38.8942255869599,
17.5091437501435));
#28288=CARTESIAN_POINT('Ctrl Pts',(-8.87542318440409,-38.9271557119402,
17.5033350660391));
#28289=CARTESIAN_POINT('Ctrl Pts',(-8.990403470318,-38.960081364314,17.4975271708767));
#28290=CARTESIAN_POINT('Ctrl Pts',(-9.1068489625418,-38.9879583606301,17.4917192757142));
#28291=CARTESIAN_POINT('Ctrl Pts',(-9.22427893354455,-39.0106709946164,
17.4859113805518));
#28292=CARTESIAN_POINT('Ctrl Pts',(-9.34172052787383,-39.0333858767201,
17.4801029105185));
#28293=CARTESIAN_POINT('Ctrl Pts',(-9.46014639463344,-39.0509353026474,
17.4742944404853));
#28294=CARTESIAN_POINT('Ctrl Pts',(-9.57906641146543,-39.06325484237,17.468485970452));
#28295=CARTESIAN_POINT('Ctrl Pts',(-9.69802612153923,-39.0755784941209,
17.4626755616619));
#28296=CARTESIAN_POINT('Ctrl Pts',(-9.81747990460743,-39.0826687457922,
17.4568651528717));
#28297=CARTESIAN_POINT('Ctrl Pts',(-9.93693395963507,-39.0845131502485,
17.4510547440815));
#28298=CARTESIAN_POINT('Ctrl Pts',(-10.0565213697727,-39.0863596137455,
17.4452378487162));
#28299=CARTESIAN_POINT('Ctrl Pts',(-10.1761086447797,-39.0829485339201,
17.4394209533509));
#28300=CARTESIAN_POINT('Ctrl Pts',(-10.2952032565593,-39.0743195796742,
17.4336040579856));
#28301=CARTESIAN_POINT('Ctrl Pts',(-10.4143768272869,-39.0656849044882,
17.4277833060567));
#28302=CARTESIAN_POINT('Ctrl Pts',(-10.5330566804442,-39.051825512261,17.4219625541279));
#28303=CARTESIAN_POINT('Ctrl Pts',(-10.6507583154515,-39.0328325795737,
17.416141802199));
#28304=CARTESIAN_POINT('Ctrl Pts',(-10.7686287585406,-39.0138124071582,
17.4103127021281));
#28305=CARTESIAN_POINT('Ctrl Pts',(-10.8855177855614,-38.9896440811116,
17.4044836020572));
#28306=CARTESIAN_POINT('Ctrl Pts',(-11.0009537873615,-38.960469229216,17.3986545019863));
#28307=CARTESIAN_POINT('Ctrl Pts',(-11.0306298219521,-38.9529690221703,
17.3971559697032));
#28308=CARTESIAN_POINT('Ctrl Pts',(-11.0602099213474,-38.9451381902407,
17.39565743742));
#28309=CARTESIAN_POINT('Ctrl Pts',(-11.0896862802715,-38.9369796558514,
17.3941589051369));
#28310=CARTESIAN_POINT('Ctrl Pts',(-11.2031719139894,-38.9055688412473,
17.3883894718687));
#28311=CARTESIAN_POINT('Ctrl Pts',(-11.3155007485516,-38.8691909052908,
17.3826200386006));
#28312=CARTESIAN_POINT('Ctrl Pts',(-11.4262003987351,-38.8279468939169,
17.3768506053324));
#28313=CARTESIAN_POINT('Ctrl Pts',(-11.5367586810991,-38.7867555527722,
17.3710885398581));
#28314=CARTESIAN_POINT('Ctrl Pts',(-11.6456915287877,-38.7407106345995,
17.3653264743838));
#28315=CARTESIAN_POINT('Ctrl Pts',(-11.7525390974166,-38.689963646437,17.3595644089094));
#28316=CARTESIAN_POINT('Ctrl Pts',(-11.8592793964961,-38.6392676056813,
17.3538081282571));
#28317=CARTESIAN_POINT('Ctrl Pts',(-11.9639382054807,-38.5838790596371,
17.3480518476048));
#28318=CARTESIAN_POINT('Ctrl Pts',(-12.0660738167459,-38.5239982950843,
17.3422955669525));
#28319=CARTESIAN_POINT('Ctrl Pts',(-12.1734329020074,-38.46105507648,17.3362448955198));
#28320=CARTESIAN_POINT('Ctrl Pts',(-12.2780034320631,-38.3931481539316,
17.3301942240872));
#28321=CARTESIAN_POINT('Ctrl Pts',(-12.3792994209464,-38.3205661061759,
17.3241435526545));
#28322=CARTESIAN_POINT('Ctrl Pts',(-12.4755642992349,-38.2515890215929,
17.3183934024714));
#28323=CARTESIAN_POINT('Ctrl Pts',(-12.5688717047298,-38.1783903109183,
17.3126432522882));
#28324=CARTESIAN_POINT('Ctrl Pts',(-12.6588334620962,-38.1012625849543,
17.3068931021051));
#28325=CARTESIAN_POINT('Ctrl Pts',(-12.7487854232299,-38.0241432576829,
17.3011435780748));
#28326=CARTESIAN_POINT('Ctrl Pts',(-12.8353921438226,-37.9430960365249,
17.2953940540445));
#28327=CARTESIAN_POINT('Ctrl Pts',(-12.9182989111097,-37.8584535094026,
17.2896445300142));
#28328=CARTESIAN_POINT('Ctrl Pts',(-13.001217134618,-37.7737992862083,17.2838942115033));
#28329=CARTESIAN_POINT('Ctrl Pts',(-13.0804340967645,-37.6855490671484,
17.2781438929923));
#28330=CARTESIAN_POINT('Ctrl Pts',(-13.1556328407124,-37.5940713896532,
17.2723935744814));
#28331=CARTESIAN_POINT('Ctrl Pts',(-13.2308605571474,-37.5025584677418,
17.2666410404943));
#28332=CARTESIAN_POINT('Ctrl Pts',(-13.3020667131398,-37.407815936993,17.2608885065071));
#28333=CARTESIAN_POINT('Ctrl Pts',(-13.3689759047412,-37.3102437865457,
17.25513597252));
#28334=CARTESIAN_POINT('Ctrl Pts',(-13.4359686747336,-37.2125497556341,
17.2493762528604));
#28335=CARTESIAN_POINT('Ctrl Pts',(-13.4986535321635,-37.1120193945602,
17.2436165332008));
#28336=CARTESIAN_POINT('Ctrl Pts',(-13.5567994624573,-37.0090800342106,
17.2378568135413));
#28337=CARTESIAN_POINT('Ctrl Pts',(-13.6149876492351,-36.9060658645764,
17.2320929081115));
#28338=CARTESIAN_POINT('Ctrl Pts',(-13.6686301558586,-36.8006395816176,
17.2263290026817));
#28339=CARTESIAN_POINT('Ctrl Pts',(-13.7175436244579,-36.6932496567998,
17.2205650972519));
#28340=CARTESIAN_POINT('Ctrl Pts',(-13.7665358558739,-36.5856868075665,
17.2147919105047));
#28341=CARTESIAN_POINT('Ctrl Pts',(-13.8107836979585,-36.4761543910992,
17.2090187237575));
#28342=CARTESIAN_POINT('Ctrl Pts',(-13.850153190532,-36.3651173610485,17.2032455370104));
#28343=CARTESIAN_POINT('Ctrl Pts',(-13.8641694595514,-36.325586120421,17.2011901755297));
#28344=CARTESIAN_POINT('Ctrl Pts',(-13.8775678722885,-36.2858642738188,
17.1991348140491));
#28345=CARTESIAN_POINT('Ctrl Pts',(-13.8903439517821,-36.2459730883259,
17.1970794525685));
#28346=CARTESIAN_POINT('Ctrl Pts',(-13.9364879357336,-36.1018961651894,
17.1896560041449));
#28347=CARTESIAN_POINT('Ctrl Pts',(-13.9746350341868,-35.9552204518296,
17.1822325557212));
#28348=CARTESIAN_POINT('Ctrl Pts',(-14.0045492121205,-35.8067283357521,
17.1748091072976));
#28349=CARTESIAN_POINT('Ctrl Pts',(-14.0339663193344,-35.6607036477675,
17.167509011047));
#28350=CARTESIAN_POINT('Ctrl Pts',(-14.0554218917175,-35.5129222631596,
17.1602089147964));
#28351=CARTESIAN_POINT('Ctrl Pts',(-14.0687370244314,-35.3641483571585,
17.1529088185457));
#28352=CARTESIAN_POINT('Ctrl Pts',(-14.0793913123442,-35.2451048551138,
17.1470675453931));
#28353=CARTESIAN_POINT('Ctrl Pts',(-14.0848344029928,-35.1254262216438,
17.1412262722404));
#28354=CARTESIAN_POINT('Ctrl Pts',(-14.0849962778219,-35.0055145427062,
17.1353849990878));
#28355=CARTESIAN_POINT('',(-13.1750507821943,-32.429732011932,17.));
#28356=CARTESIAN_POINT('Ctrl Pts',(-14.0811726754193,-35.0055088132717,
17.1353849714045));
#28357=CARTESIAN_POINT('Ctrl Pts',(-14.0735476212511,-34.0799540937817,
17.090256647603));
#28358=CARTESIAN_POINT('Ctrl Pts',(-13.7580895933996,-33.1499595688096,
17.0451283238015));
#28359=CARTESIAN_POINT('Ctrl Pts',(-13.1750507821943,-32.429732011932,17.));
#28360=CARTESIAN_POINT('',(-11.4626266916477,-31.1858227412875,17.00000010299));
#28361=CARTESIAN_POINT('Origin',(-10.,-35.,17.));
#28362=CARTESIAN_POINT('',(-14.0849987341496,-34.9967841025477,17.2396150285694));
#28363=CARTESIAN_POINT('Ctrl Pts',(-14.0849987341496,-34.9967841025477,
17.2396150285694));
#28364=CARTESIAN_POINT('Ctrl Pts',(-14.0848792956189,-34.8450671234211,
17.2322291344928));
#28365=CARTESIAN_POINT('Ctrl Pts',(-14.0763040577088,-34.6937076409018,
17.2248432404161));
#28366=CARTESIAN_POINT('Ctrl Pts',(-14.0594139179449,-34.5435094274846,
17.2174573463394));
#28367=CARTESIAN_POINT('Ctrl Pts',(-14.0421958750279,-34.3903952839183,
17.2099280633986));
#28368=CARTESIAN_POINT('Ctrl Pts',(-14.0163369470605,-34.2384876988639,
17.2023987804579));
#28369=CARTESIAN_POINT('Ctrl Pts',(-13.9820349515489,-34.0886149855068,
17.1948694975171));
#28370=CARTESIAN_POINT('Ctrl Pts',(-13.9743904293648,-34.0552144423323,
17.1931915260285));
#28371=CARTESIAN_POINT('Ctrl Pts',(-13.9663267596094,-34.0219148823929,
17.1915135545398));
#28372=CARTESIAN_POINT('Ctrl Pts',(-13.9578464551255,-33.9887253401522,
17.1898355830512));
#28373=CARTESIAN_POINT('Ctrl Pts',(-13.9285722574743,-33.8741543101436,
17.1840431885559));
#28374=CARTESIAN_POINT('Ctrl Pts',(-13.8942699070934,-33.7606632797219,
17.1782507940605));
#28375=CARTESIAN_POINT('Ctrl Pts',(-13.8550346975133,-33.6487293087733,
17.1724583995652));
#28376=CARTESIAN_POINT('Ctrl Pts',(-13.8158484446736,-33.5369350063114,
17.1666732326788));
#28377=CARTESIAN_POINT('Ctrl Pts',(-13.7717417078434,-33.4266942862656,
17.1608880657925));
#28378=CARTESIAN_POINT('Ctrl Pts',(-13.7228604057983,-33.3184723020601,
17.1551028989061));
#28379=CARTESIAN_POINT('Ctrl Pts',(-13.6740269923903,-33.2103563421034,
17.1493233997034));
#28380=CARTESIAN_POINT('Ctrl Pts',(-13.620428486564,-33.1042555587027,17.1435439005007));
#28381=CARTESIAN_POINT('Ctrl Pts',(-13.562259834161,-33.0006176268849,17.137764401298));
#28382=CARTESIAN_POINT('Ctrl Pts',(-13.504130973168,-32.8970505906315,17.1319888556754));
#28383=CARTESIAN_POINT('Ctrl Pts',(-13.4414383856446,-32.7959434139872,
17.1262133100527));
#28384=CARTESIAN_POINT('Ctrl Pts',(-13.3744238446957,-32.6977209733941,
17.1204377644301));
#28385=CARTESIAN_POINT('Ctrl Pts',(-13.3074334204694,-32.5995338804036,
17.1146642972703));
#28386=CARTESIAN_POINT('Ctrl Pts',(-13.2361243672596,-32.5042298006227,
17.1088908301104));
#28387=CARTESIAN_POINT('Ctrl Pts',(-13.1607825295344,-32.4122058039732,
17.1031173629506));
#28388=CARTESIAN_POINT('Ctrl Pts',(-13.0854495234263,-32.3201925944339,
17.0973445725602));
#28389=CARTESIAN_POINT('Ctrl Pts',(-13.0060849345761,-32.2314590230699,
17.0915717821698));
#28390=CARTESIAN_POINT('Ctrl Pts',(-12.9230153063086,-32.146369589613,17.0857989917794));
#28391=CARTESIAN_POINT('Ctrl Pts',(-12.839935258194,-32.0612694829545,17.0800254772784));
#28392=CARTESIAN_POINT('Ctrl Pts',(-12.7531495356343,-31.9798147183417,
17.0742519627774));
#28393=CARTESIAN_POINT('Ctrl Pts',(-12.663021482694,-31.9023328805841,17.0684784482765));
#28394=CARTESIAN_POINT('Ctrl Pts',(-12.5728043165972,-31.8247744334812,
17.0626992252743));
#28395=CARTESIAN_POINT('Ctrl Pts',(-12.47923853297,-31.7511970295599,17.0569200022721));
#28396=CARTESIAN_POINT('Ctrl Pts',(-12.3827206515411,-31.6818879921378,
17.0511407792699));
#28397=CARTESIAN_POINT('Ctrl Pts',(-12.2861553775729,-31.6125449223557,
17.045358718534));
#28398=CARTESIAN_POINT('Ctrl Pts',(-12.1866354641117,-31.547474620243,17.039576657798));
#28399=CARTESIAN_POINT('Ctrl Pts',(-12.0845849864714,-31.4869200928277,
17.033794597062));
#28400=CARTESIAN_POINT('Ctrl Pts',(-11.9823703793501,-31.4262681745584,
17.0280032369416));
#28401=CARTESIAN_POINT('Ctrl Pts',(-11.877617440471,-31.37014673806,17.0222118768211));
#28402=CARTESIAN_POINT('Ctrl Pts',(-11.7707738116355,-31.3187522349038,
17.0164205167007));
#28403=CARTESIAN_POINT('Ctrl Pts',(-11.6697948503699,-31.2701787860231,
17.0109470454638));
#28404=CARTESIAN_POINT('Ctrl Pts',(-11.5669488707751,-31.2258272805034,
17.0054735742269));
#28405=CARTESIAN_POINT('Ctrl Pts',(-11.4626266916477,-31.1858227412875,
17.00000010299));
#28406=CARTESIAN_POINT('Ctrl Pts',(-7.51282745730981,-31.7594448403263,
18.0469656703996));
#28407=CARTESIAN_POINT('Ctrl Pts',(-7.41799591346389,-31.8322294097635,
18.041156532831));
#28408=CARTESIAN_POINT('Ctrl Pts',(-7.32640799980818,-31.9091448038285,
18.0353473952624));
#28409=CARTESIAN_POINT('Ctrl Pts',(-7.23842903445172,-31.9898586740419,
18.0295382576938));
#28410=CARTESIAN_POINT('Ctrl Pts',(-7.15040482328216,-32.070614053776,18.0237261326026));
#28411=CARTESIAN_POINT('Ctrl Pts',(-7.06599354704681,-32.1551715127752,
18.0179140075113));
#28412=CARTESIAN_POINT('Ctrl Pts',(-6.98552277878798,-32.2431626666062,
18.01210188242));
#28413=CARTESIAN_POINT('Ctrl Pts',(-6.90492116054487,-32.3312968989904,
18.0062803064873));
#28414=CARTESIAN_POINT('Ctrl Pts',(-6.82827311668664,-32.4228756697515,
18.0004587305545));
#28415=CARTESIAN_POINT('Ctrl Pts',(-6.75586551560998,-32.5174979461858,
17.9946371546218));
#28416=CARTESIAN_POINT('Ctrl Pts',(-6.68752493647219,-32.6068054370391,
17.9891425675228));
#28417=CARTESIAN_POINT('Ctrl Pts',(-6.62296160326281,-32.6988236305518,
17.9836479804239));
#28418=CARTESIAN_POINT('Ctrl Pts',(-6.56237960878621,-32.793194379672,17.978153393325));
#28419=CARTESIAN_POINT('Ctrl Pts',(-6.49815825728457,-32.893234285969,17.9723287285466));
#28420=CARTESIAN_POINT('Ctrl Pts',(-6.43820408463767,-32.9962410126016,
17.9665040637681));
#28421=CARTESIAN_POINT('Ctrl Pts',(-6.38280235811278,-33.1018150196766,
17.9606793989897));
#28422=CARTESIAN_POINT('Ctrl Pts',(-6.32747055204339,-33.2072557857295,
17.9548620853037));
#28423=CARTESIAN_POINT('Ctrl Pts',(-6.27667995239707,-33.3152570295018,
17.9490447716177));
#28424=CARTESIAN_POINT('Ctrl Pts',(-6.23067250817717,-33.4253904422402,
17.9432274579317));
#28425=CARTESIAN_POINT('Ctrl Pts',(-6.18471114847212,-33.5354135370728,
17.9374159713044));
#28426=CARTESIAN_POINT('Ctrl Pts',(-6.14352356912006,-33.6475641775767,
17.9316044846772));
#28427=CARTESIAN_POINT('Ctrl Pts',(-6.10730546100739,-33.7613902042624,
17.9257929980499));
#28428=CARTESIAN_POINT('Ctrl Pts',(-6.06972578762955,-33.8794953491098,
17.9197630373294));
#28429=CARTESIAN_POINT('Ctrl Pts',(-6.03749676689774,-33.9994039233524,
17.9137330766088));
#28430=CARTESIAN_POINT('Ctrl Pts',(-6.01078198013274,-34.1205884979338,
17.9077031158882));
#28431=CARTESIAN_POINT('Ctrl Pts',(-5.98506416668024,-34.2372505663912,
17.9018981882165));
#28432=CARTESIAN_POINT('Ctrl Pts',(-5.9644564835091,-34.3550946687381,17.8960932605447));
#28433=CARTESIAN_POINT('Ctrl Pts',(-5.94905366228232,-34.4736362769607,
17.890288332873));
#28434=CARTESIAN_POINT('Ctrl Pts',(-5.93365313903662,-34.5921601996979,
17.8844842712513));
#28435=CARTESIAN_POINT('Ctrl Pts',(-5.92345598603055,-34.7113810166986,
17.8786802096296));
#28436=CARTESIAN_POINT('Ctrl Pts',(-5.91850534177189,-34.8308067529261,
17.8728761480078));
#28437=CARTESIAN_POINT('Ctrl Pts',(-5.91355426889453,-34.9502428288387,
17.8670715838799));
#28438=CARTESIAN_POINT('Ctrl Pts',(-5.91385062479059,-35.0698834514069,
17.861267019752));
#28439=CARTESIAN_POINT('Ctrl Pts',(-5.91938544634027,-35.1892349451354,
17.8554624556242));
#28440=CARTESIAN_POINT('Ctrl Pts',(-5.92492205202479,-35.3086249114969,
17.8496560204106));
#28441=CARTESIAN_POINT('Ctrl Pts',(-5.93570046273317,-35.427725156134,17.8438495851971));
#28442=CARTESIAN_POINT('Ctrl Pts',(-5.95165976113041,-35.5460460698049,
17.8380431499836));
#28443=CARTESIAN_POINT('Ctrl Pts',(-5.96763667162035,-35.6644975580691,
17.8322303070024));
#28444=CARTESIAN_POINT('Ctrl Pts',(-5.98880582772998,-35.782167593892,17.8264174640213));
#28445=CARTESIAN_POINT('Ctrl Pts',(-6.01505496204245,-35.8985755641333,
17.8206046210402));
#28446=CARTESIAN_POINT('Ctrl Pts',(-6.04132128348752,-36.0150597547633,
17.8147879719867));
#28447=CARTESIAN_POINT('Ctrl Pts',(-6.07267410054133,-36.1302798411067,
17.8089713229333));
#28448=CARTESIAN_POINT('Ctrl Pts',(-6.10895140066696,-36.2437707978677,
17.8031546738798));
#28449=CARTESIAN_POINT('Ctrl Pts',(-6.14528050704745,-36.3574238268174,
17.7973297182875));
#28450=CARTESIAN_POINT('Ctrl Pts',(-6.18654799227187,-36.4693424159406,
17.7915047626952));
#28451=CARTESIAN_POINT('Ctrl Pts',(-6.23254386823653,-36.5790817886474,
17.7856798071029));
#28452=CARTESIAN_POINT('Ctrl Pts',(-6.24466704261493,-36.6080058937677,
17.7841445183208));
#28453=CARTESIAN_POINT('Ctrl Pts',(-6.25711845065319,-36.6367787457519,
17.7826092295387));
#28454=CARTESIAN_POINT('Ctrl Pts',(-6.26989372793288,-36.6653925060134,
17.7810739407566));
#28455=CARTESIAN_POINT('Ctrl Pts',(-6.31836098739686,-36.7739483136465,
17.7752493125997));
#28456=CARTESIAN_POINT('Ctrl Pts',(-6.37164893828561,-36.8805610015775,
17.7694246844429));
#28457=CARTESIAN_POINT('Ctrl Pts',(-6.42957968551216,-36.9847729789305,
17.7636000562861));
#28458=CARTESIAN_POINT('Ctrl Pts',(-6.48743749358682,-37.0888537455947,
17.7577827617726));
#28459=CARTESIAN_POINT('Ctrl Pts',(-6.54992627449195,-37.1905394601524,
17.751965467259));
#28460=CARTESIAN_POINT('Ctrl Pts',(-6.61682033094515,-37.2893930040283,
17.7461481727455));
#28461=CARTESIAN_POINT('Ctrl Pts',(-6.68364757915551,-37.3881478211726,
17.7403366880639));
#28462=CARTESIAN_POINT('Ctrl Pts',(-6.75487112287933,-37.4840757586115,
17.7345252033824));
#28463=CARTESIAN_POINT('Ctrl Pts',(-6.8302199657713,-37.5767653239294,17.7287137187008));
#28464=CARTESIAN_POINT('Ctrl Pts',(-6.90840155476272,-37.672939561268,17.7226837507627));
#28465=CARTESIAN_POINT('Ctrl Pts',(-6.9910244955403,-37.7656267619708,17.7166537828247));
#28466=CARTESIAN_POINT('Ctrl Pts',(-7.07773723570448,-37.8544010468769,
17.7106238148867));
#28467=CARTESIAN_POINT('Ctrl Pts',(-7.16121441223064,-37.9398628445097,
17.7048188467003));
#28468=CARTESIAN_POINT('Ctrl Pts',(-7.248481334466,-38.0216981875071,17.6990138785139));
#28469=CARTESIAN_POINT('Ctrl Pts',(-7.33918460599718,-38.0995622979765,
17.6932089103274));
#28470=CARTESIAN_POINT('Ctrl Pts',(-7.42987458756949,-38.1774149996973,
17.6874047926924));
#28471=CARTESIAN_POINT('Ctrl Pts',(-7.52399960751364,-38.2512973602683,
17.6816006750573));
#28472=CARTESIAN_POINT('Ctrl Pts',(-7.62117176851912,-38.320903678987,17.6757965574222));
#28473=CARTESIAN_POINT('Ctrl Pts',(-7.71835259959821,-38.390516208249,17.6699919219214));
#28474=CARTESIAN_POINT('Ctrl Pts',(-7.81858078047582,-38.4558516993873,
17.6641872864207));
#28475=CARTESIAN_POINT('Ctrl Pts',(-7.92143844123699,-38.5166471029139,
17.6583826509199));
#28476=CARTESIAN_POINT('Ctrl Pts',(-8.02432952738108,-38.5774622629626,
17.6525761291021));
#28477=CARTESIAN_POINT('Ctrl Pts',(-8.12985144163544,-38.6337341935927,
17.6467696072842));
#28478=CARTESIAN_POINT('Ctrl Pts',(-8.23756124598365,-38.685245532979,17.6409630854663));
#28479=CARTESIAN_POINT('Ctrl Pts',(-8.3453903198527,-38.7368139120451,17.6351501339546));
#28480=CARTESIAN_POINT('Ctrl Pts',(-8.45541175130916,-38.7836110012543,
17.6293371824428));
#28481=CARTESIAN_POINT('Ctrl Pts',(-8.56716198730639,-38.8254673216981,
17.623524230931));
#28482=CARTESIAN_POINT('Ctrl Pts',(-8.6789856402559,-38.8673511406385,17.6177074604636));
#28483=CARTESIAN_POINT('Ctrl Pts',(-8.79253997245018,-38.9042876003803,
17.6118906899963));
#28484=CARTESIAN_POINT('Ctrl Pts',(-8.90734721116404,-38.9361573752899,
17.606073919529));
#28485=CARTESIAN_POINT('Ctrl Pts',(-9.02231874944238,-38.968072758736,17.6002488247359));
#28486=CARTESIAN_POINT('Ctrl Pts',(-9.13854637673725,-38.9949068934395,
17.5944237299428));
#28487=CARTESIAN_POINT('Ctrl Pts',(-9.2555429677009,-39.0165916804002,17.5885986351497));
#28488=CARTESIAN_POINT('Ctrl Pts',(-9.28636761622221,-39.0223048890572,
17.5870639194958));
#28489=CARTESIAN_POINT('Ctrl Pts',(-9.31724562117584,-39.027660938676,17.585529203842));
#28490=CARTESIAN_POINT('Ctrl Pts',(-9.34816804465764,-39.0326591849541,
17.5839944881881));
#28491=CARTESIAN_POINT('Ctrl Pts',(-9.46537473536423,-39.0516042688004,
17.5781773845232));
#28492=CARTESIAN_POINT('Ctrl Pts',(-9.58359963525702,-39.0654662622646,
17.5723602808582));
#28493=CARTESIAN_POINT('Ctrl Pts',(-9.70236375059238,-39.0741425678342,
17.5665431771933));
#28494=CARTESIAN_POINT('Ctrl Pts',(-9.82097756406794,-39.0828078931101,
17.5607334353606));
#28495=CARTESIAN_POINT('Ctrl Pts',(-9.9401288311714,-39.0863005533965,17.554923693528));
#28496=CARTESIAN_POINT('Ctrl Pts',(-10.0593293837626,-39.0845691356889,
17.5491139516953));
#28497=CARTESIAN_POINT('Ctrl Pts',(-10.1784103425818,-39.0828394551106,
17.5433100387697));
#28498=CARTESIAN_POINT('Ctrl Pts',(-10.2975400816037,-39.075896128858,17.5375061258441));
#28499=CARTESIAN_POINT('Ctrl Pts',(-10.4162269551722,-39.0637396720002,
17.5317022129185));
#28500=CARTESIAN_POINT('Ctrl Pts',(-10.5395944260109,-39.0511038067876,
17.5256694138644));
#28501=CARTESIAN_POINT('Ctrl Pts',(-10.6624829335618,-39.0328351491251,
17.5196366148103));
#28502=CARTESIAN_POINT('Ctrl Pts',(-10.7843417756888,-39.0089940108348,
17.5136038157562));
#28503=CARTESIAN_POINT('Ctrl Pts',(-10.901445632305,-38.9860831642259,17.5078064191693));
#28504=CARTESIAN_POINT('Ctrl Pts',(-11.0175982323764,-38.9580266446692,
17.5020090225824));
#28505=CARTESIAN_POINT('Ctrl Pts',(-11.132318464172,-38.9249305593469,17.4962116259955));
#28506=CARTESIAN_POINT('Ctrl Pts',(-11.2470221211626,-38.8918392557545,
17.4904150670178));
#28507=CARTESIAN_POINT('Ctrl Pts',(-11.360293428187,-38.8537099477184,17.4846185080401));
#28508=CARTESIAN_POINT('Ctrl Pts',(-11.4716650242463,-38.8106990246424,
17.4788219490624));
#28509=CARTESIAN_POINT('Ctrl Pts',(-11.5830469735196,-38.7676841032282,
17.4730248512308));
#28510=CARTESIAN_POINT('Ctrl Pts',(-11.6925284788183,-38.7197868119969,
17.4672277533992));
#28511=CARTESIAN_POINT('Ctrl Pts',(-11.7996614171169,-38.6672119905646,
17.4614306555676));
#28512=CARTESIAN_POINT('Ctrl Pts',(-11.9068297523597,-38.6146197983027,
17.4556316423629));
#28513=CARTESIAN_POINT('Ctrl Pts',(-12.0116476101418,-38.5573471826325,
17.4498326291582));
#28514=CARTESIAN_POINT('Ctrl Pts',(-12.1136913478998,-38.4956449885269,
17.4440336159536));
#28515=CARTESIAN_POINT('Ctrl Pts',(-12.2158496459546,-38.4338735239122,
17.4382280924359));
#28516=CARTESIAN_POINT('Ctrl Pts',(-12.3152272569984,-38.3676627666107,
17.4324225689182));
#28517=CARTESIAN_POINT('Ctrl Pts',(-12.4114293004768,-38.2973070419362,
17.4266170454005));
#28518=CARTESIAN_POINT('Ctrl Pts',(-12.5076952582291,-38.226904574647,17.4208076648356));
#28519=CARTESIAN_POINT('Ctrl Pts',(-12.6007811283544,-38.1523519114076,
17.4149982842707));
#28520=CARTESIAN_POINT('Ctrl Pts',(-12.6903262170624,-38.0739827334887,
17.4091889037058));
#28521=CARTESIAN_POINT('Ctrl Pts',(-12.7800013460207,-37.9954997453357,
17.4033710865721));
#28522=CARTESIAN_POINT('Ctrl Pts',(-12.8661251357339,-37.9131894620869,
17.3975532694385));
#28523=CARTESIAN_POINT('Ctrl Pts',(-12.9483746417885,-37.8274214350992,
17.3917354523048));
#28524=CARTESIAN_POINT('Ctrl Pts',(-12.971090887545,-37.8037334195407,17.3901286467431));
#28525=CARTESIAN_POINT('Ctrl Pts',(-12.993511849102,-37.7797818359811,17.3885218411814));
#28526=CARTESIAN_POINT('Ctrl Pts',(-13.0156312901188,-37.7555748805025,
17.3869150356197));
#28527=CARTESIAN_POINT('Ctrl Pts',(-13.0950952824613,-37.6686115018474,
17.3811425938679));
#28528=CARTESIAN_POINT('Ctrl Pts',(-13.1709347279013,-37.5780543125062,
17.3753701521162));
#28529=CARTESIAN_POINT('Ctrl Pts',(-13.2428032938079,-37.4842406883529,
17.3695977103644));
#28530=CARTESIAN_POINT('Ctrl Pts',(-13.314557702329,-37.3905760795297,17.3638344376681));
#28531=CARTESIAN_POINT('Ctrl Pts',(-13.3823535340787,-37.2936656586178,
17.3580711649717));
#28532=CARTESIAN_POINT('Ctrl Pts',(-13.4458822746592,-37.1938824829943,
17.3523078922753));
#28533=CARTESIAN_POINT('Ctrl Pts',(-13.509353084695,-37.0941902975851,17.3465498749881));
#28534=CARTESIAN_POINT('Ctrl Pts',(-13.5685643151663,-36.9916309131642,
17.3407918577009));
#28535=CARTESIAN_POINT('Ctrl Pts',(-13.623248700849,-36.8866090882311,17.3350338404137));
#28536=CARTESIAN_POINT('Ctrl Pts',(-13.6778967281546,-36.7816570898684,
17.3292796514983));
#28537=CARTESIAN_POINT('Ctrl Pts',(-13.7280237029789,-36.674246274176,17.323525462583));
#28538=CARTESIAN_POINT('Ctrl Pts',(-13.7734069587951,-36.5648082704653,
17.3177712736676));
#28539=CARTESIAN_POINT('Ctrl Pts',(-13.818771248082,-36.4554160029863,17.3120194895377));
#28540=CARTESIAN_POINT('Ctrl Pts',(-13.8593956025279,-36.3439986168261,
17.3062677054078));
#28541=CARTESIAN_POINT('Ctrl Pts',(-13.8951047222278,-36.2310094243662,
17.3005159212779));
#28542=CARTESIAN_POINT('Ctrl Pts',(-13.9308168475328,-36.1180107217059,
17.2947636530254));
#28543=CARTESIAN_POINT('Ctrl Pts',(-13.9616127765773,-36.0034403426354,
17.289011384773));
#28544=CARTESIAN_POINT('Ctrl Pts',(-13.987366634355,-35.8877681697565,17.2832591165205));
#28545=CARTESIAN_POINT('Ctrl Pts',(-14.013121424051,-35.7720918112122,17.2775066401188));
#28546=CARTESIAN_POINT('Ctrl Pts',(-14.0338336962148,-35.6553139878288,
17.2717541637171));
#28547=CARTESIAN_POINT('Ctrl Pts',(-14.0494286499008,-35.5379150577577,
17.2660016873154));
#28548=CARTESIAN_POINT('Ctrl Pts',(-14.0650341474827,-35.4204367531582,
17.26024532161));
#28549=CARTESIAN_POINT('Ctrl Pts',(-14.0755153712924,-35.3023369175002,
17.2544889559045));
#28550=CARTESIAN_POINT('Ctrl Pts',(-14.0808493937001,-35.1841011296474,
17.2487325901991));
#28551=CARTESIAN_POINT('Ctrl Pts',(-14.0836655963984,-35.1216762053895,
17.2456934029979));
#28552=CARTESIAN_POINT('Ctrl Pts',(-14.0850478813473,-35.0592134171758,
17.2426542157967));
#28553=CARTESIAN_POINT('Ctrl Pts',(-14.08499873415,-34.996784103083,17.2396150285955));
#28554=CARTESIAN_POINT('Origin',(-10.,-35.,32.7603849714045));
#28555=CARTESIAN_POINT('',(-7.51282745730977,-31.7594448403263,19.2967866684593));
#28556=CARTESIAN_POINT('',(-7.51282745730979,-31.7594448403263,19.1927507934385));
#28557=CARTESIAN_POINT('',(-7.5128274573098,-31.7594448403263,32.7603849714045));
#28558=CARTESIAN_POINT('',(-14.0849999333383,-34.9992620122689,18.3853849714444));
#28559=CARTESIAN_POINT('Ctrl Pts',(-7.5128274573098,-31.7594448403263,19.1927507934385));
#28560=CARTESIAN_POINT('Ctrl Pts',(-7.41816098010506,-31.83210271875,19.1869272043147));
#28561=CARTESIAN_POINT('Ctrl Pts',(-7.3267948839667,-31.9088247975322,19.1811036151909));
#28562=CARTESIAN_POINT('Ctrl Pts',(-7.23907769086388,-31.9892637108318,
19.1752800260671));
#28563=CARTESIAN_POINT('Ctrl Pts',(-7.20189342113841,-32.0233626387928,
19.1728113434624));
#28564=CARTESIAN_POINT('Ctrl Pts',(-7.1653643842384,-32.0581290534056,19.1703426608576));
#28565=CARTESIAN_POINT('Ctrl Pts',(-7.12951495513338,-32.093534688458,19.1678739782529));
#28566=CARTESIAN_POINT('Ctrl Pts',(-7.04494813447614,-32.1770546234885,
19.1620504925153));
#28567=CARTESIAN_POINT('Ctrl Pts',(-6.96389309800936,-32.2644031799116,
19.1562270067777));
#28568=CARTESIAN_POINT('Ctrl Pts',(-6.88671566354767,-32.3552531991889,
19.15040352104));
#28569=CARTESIAN_POINT('Ctrl Pts',(-6.80963560306152,-32.4459885939309,
19.1445873827345));
#28570=CARTESIAN_POINT('Ctrl Pts',(-6.73642367590697,-32.5402163562413,
19.1387712444289));
#28571=CARTESIAN_POINT('Ctrl Pts',(-6.66740974472798,-32.6375717597214,
19.1329551061234));
#28572=CARTESIAN_POINT('Ctrl Pts',(-6.59846489787046,-32.734829708501,19.1271447898883));
#28573=CARTESIAN_POINT('Ctrl Pts',(-6.53370992188484,-32.8352087388302,
19.1213344736532));
#28574=CARTESIAN_POINT('Ctrl Pts',(-6.47343477594744,-32.9383107119396,
19.1155241574181));
#28575=CARTESIAN_POINT('Ctrl Pts',(-6.41087650802344,-33.0453180158119,
19.1094937560959));
#28576=CARTESIAN_POINT('Ctrl Pts',(-6.35314444740412,-33.1552582804184,
19.1034633547736));
#28577=CARTESIAN_POINT('Ctrl Pts',(-6.30051393217922,-33.2676525077226,
19.0974329534514));
#28578=CARTESIAN_POINT('Ctrl Pts',(-6.2498612881276,-33.3758229249181,19.0916291764912));
#28579=CARTESIAN_POINT('Ctrl Pts',(-6.20393386227847,-33.4862657887406,
19.0858253995311));
#28580=CARTESIAN_POINT('Ctrl Pts',(-6.16293019111039,-33.5985292433633,
19.0800216225709));
#28581=CARTESIAN_POINT('Ctrl Pts',(-6.12193257350797,-33.7107761240019,
19.0742187024497));
#28582=CARTESIAN_POINT('Ctrl Pts',(-6.08585740503899,-33.8248426774518,
19.0684157823286));
#28583=CARTESIAN_POINT('Ctrl Pts',(-6.05485451372902,-33.9402584786111,
19.0626128622074));
#28584=CARTESIAN_POINT('Ctrl Pts',(-6.02384888208821,-34.0556844813182,
19.0568094291689));
#28585=CARTESIAN_POINT('Ctrl Pts',(-5.99791652494864,-34.1724595744584,
19.0510059961304));
#28586=CARTESIAN_POINT('Ctrl Pts',(-5.97715680626476,-34.2901002615735,
19.0452025630919));
#28587=CARTESIAN_POINT('Ctrl Pts',(-5.95639035287169,-34.4077791127807,
19.039397247348));
#28588=CARTESIAN_POINT('Ctrl Pts',(-5.94079994615834,-34.5263237144956,
19.0335919316042));
#28589=CARTESIAN_POINT('Ctrl Pts',(-5.93043336647939,-34.6452431602693,
19.0277866158603));
#28590=CARTESIAN_POINT('Ctrl Pts',(-5.92005530381182,-34.7642943322906,
19.0219748696083));
#28591=CARTESIAN_POINT('Ctrl Pts',(-5.91491265380358,-34.8837207701175,
19.0161631233563));
#28592=CARTESIAN_POINT('Ctrl Pts',(-5.9150011230657,-35.0030290997907,19.0103513771044));
#28593=CARTESIAN_POINT('Ctrl Pts',(-5.91508965044777,-35.1224158091395,
19.0045358128223));
#28594=CARTESIAN_POINT('Ctrl Pts',(-5.92041612296338,-35.2416838488016,
18.9987202485403));
#28595=CARTESIAN_POINT('Ctrl Pts',(-5.93092429633697,-35.3603441658459,
18.9929046842583));
#28596=CARTESIAN_POINT('Ctrl Pts',(-5.94144752526976,-35.4791744931636,
18.9870807877411));
#28597=CARTESIAN_POINT('Ctrl Pts',(-5.95716721945902,-35.5973949566152,
18.9812568912238));
#28598=CARTESIAN_POINT('Ctrl Pts',(-5.97797589018163,-35.7145257588357,
18.9754329947066));
#28599=CARTESIAN_POINT('Ctrl Pts',(-5.98350027717661,-35.7456222132476,
18.9738868383659));
#28600=CARTESIAN_POINT('Ctrl Pts',(-5.98938307315799,-35.7766419460926,
18.9723406820251));
#28601=CARTESIAN_POINT('Ctrl Pts',(-5.99562167962237,-35.807576168104,18.9707945256844));
#28602=CARTESIAN_POINT('Ctrl Pts',(-6.01911979901596,-35.9240919391059,
18.9649708266736));
#28603=CARTESIAN_POINT('Ctrl Pts',(-6.04774543284499,-36.0397691373127,
18.9591471276627));
#28604=CARTESIAN_POINT('Ctrl Pts',(-6.08142546428526,-36.1541224406657,
18.9533234286519));
#28605=CARTESIAN_POINT('Ctrl Pts',(-6.11506300070686,-36.2683314613219,
18.9475070775617));
#28606=CARTESIAN_POINT('Ctrl Pts',(-6.15374213614125,-36.3812195212681,
18.9416907264714));
#28607=CARTESIAN_POINT('Ctrl Pts',(-6.19733862407877,-36.4923107786506,
18.9358743753812));
#28608=CARTESIAN_POINT('Ctrl Pts',(-6.24089146718125,-36.6032908215792,
18.9300638470923));
#28609=CARTESIAN_POINT('Ctrl Pts',(-6.28935172115923,-36.7124772625115,
18.9242533188033));
#28610=CARTESIAN_POINT('Ctrl Pts',(-6.34254532110293,-36.8194093194809,
18.9184427905143));
#28611=CARTESIAN_POINT('Ctrl Pts',(-6.39775106084799,-36.9303862662133,
18.9124124689561));
#28612=CARTESIAN_POINT('Ctrl Pts',(-6.45805518470405,-37.0389344794742,
18.9063821473978));
#28613=CARTESIAN_POINT('Ctrl Pts',(-6.52320802133764,-37.1445611525692,
18.9003518258395));
#28614=CARTESIAN_POINT('Ctrl Pts',(-6.58591548063397,-37.2462233463577,
18.8945478399627));
#28615=CARTESIAN_POINT('Ctrl Pts',(-6.65311400581338,-37.3451789767769,
18.8887438540858));
#28616=CARTESIAN_POINT('Ctrl Pts',(-6.72453449292813,-37.4410142793483,
18.882939868209));
#28617=CARTESIAN_POINT('Ctrl Pts',(-6.79594441768056,-37.536835408855,18.8771367406825));
#28618=CARTESIAN_POINT('Ctrl Pts',(-6.87157481873301,-37.6295368009083,
18.871333613156));
#28619=CARTESIAN_POINT('Ctrl Pts',(-6.95111436096877,-37.718735250095,18.8655304856295));
#28620=CARTESIAN_POINT('Ctrl Pts',(-7.03066090970844,-37.8079415566224,
18.8597268469153));
#28621=CARTESIAN_POINT('Ctrl Pts',(-7.11411701251287,-37.8936440020054,
18.8539232082011));
#28622=CARTESIAN_POINT('Ctrl Pts',(-7.20113273869939,-37.9754944217087,
18.8481195694869));
#28623=CARTESIAN_POINT('Ctrl Pts',(-7.28817666363465,-38.0573713662659,
18.8423140500167));
#28624=CARTESIAN_POINT('Ctrl Pts',(-7.37878220883528,-38.1353935229219,
18.8365085305465));
#28625=CARTESIAN_POINT('Ctrl Pts',(-7.47256496897134,-38.209251807498,18.8307030110763));
#28626=CARTESIAN_POINT('Ctrl Pts',(-7.56645154505005,-38.2831918519564,
18.8248910649935));
#28627=CARTESIAN_POINT('Ctrl Pts',(-7.66352203557086,-38.3529585709188,
18.8190791189106));
#28628=CARTESIAN_POINT('Ctrl Pts',(-7.76336142554086,-38.418285079867,18.8132671728277));
#28629=CARTESIAN_POINT('Ctrl Pts',(-7.86326636786683,-38.4836544807697,
18.8074514107483));
#28630=CARTESIAN_POINT('Ctrl Pts',(-7.96594347988446,-38.5445776577864,
18.801635648669));
#28631=CARTESIAN_POINT('Ctrl Pts',(-8.07095288110995,-38.6008335442092,
18.7958198865897));
#28632=CARTESIAN_POINT('Ctrl Pts',(-8.17611264840499,-38.6571699851007,
18.7899957967485));
#28633=CARTESIAN_POINT('Ctrl Pts',(-8.2836110039876,-38.7088256198026,18.7841717069073));
#28634=CARTESIAN_POINT('Ctrl Pts',(-8.3929877162259,-38.7556273137519,18.7783476170661));
#28635=CARTESIAN_POINT('Ctrl Pts',(-8.42198752222565,-38.7680361713342,
18.7768034357494));
#28636=CARTESIAN_POINT('Ctrl Pts',(-8.45111928958413,-38.7801040804447,
18.7752592544327));
#28637=CARTESIAN_POINT('Ctrl Pts',(-8.48037427685997,-38.7918284061348,
18.773715073116));
#28638=CARTESIAN_POINT('Ctrl Pts',(-8.59070779361214,-38.8360460320986,
18.7678912813103));
#28639=CARTESIAN_POINT('Ctrl Pts',(-8.70315067803467,-38.8755152456379,
18.7620674895045));
#28640=CARTESIAN_POINT('Ctrl Pts',(-8.81725691625265,-38.9100311760711,
18.7562436976988));
#28641=CARTESIAN_POINT('Ctrl Pts',(-8.93121923080606,-38.9445035711176,
18.7504272515165));
#28642=CARTESIAN_POINT('Ctrl Pts',(-9.04684033888211,-38.9740349923122,
18.7446108053342));
#28643=CARTESIAN_POINT('Ctrl Pts',(-9.16365413058495,-38.9984685301641,
18.7387943591519));
#28644=CARTESIAN_POINT('Ctrl Pts',(-9.28035102411723,-39.0228776168289,
18.7329837336173));
#28645=CARTESIAN_POINT('Ctrl Pts',(-9.39823782950199,-39.0421988859875,
18.7271731080826));
#28646=CARTESIAN_POINT('Ctrl Pts',(-9.51683372619434,-39.0563253508387,
18.7213624825479));
#28647=CARTESIAN_POINT('Ctrl Pts',(-9.63991293020297,-39.0709858416131,
18.7153321966312));
#28648=CARTESIAN_POINT('Ctrl Pts',(-9.76375546640057,-39.0800508870034,
18.7093019107145));
#28649=CARTESIAN_POINT('Ctrl Pts',(-9.8878123230821,-39.0834591861739,18.7032716247979));
#28650=CARTESIAN_POINT('Ctrl Pts',(-10.0072157643847,-39.0867396388697,
18.6974675369808));
#28651=CARTESIAN_POINT('Ctrl Pts',(-10.126817292495,-39.0847800627728,18.6916634491637));
#28652=CARTESIAN_POINT('Ctrl Pts',(-10.2461233180407,-39.0775787315902,
18.6858593613466));
#28653=CARTESIAN_POINT('Ctrl Pts',(-10.3654117315051,-39.0703784634756,
18.6800561303351));
#28654=CARTESIAN_POINT('Ctrl Pts',(-10.4844043217039,-39.0579380037031,
18.6742528993236));
#28655=CARTESIAN_POINT('Ctrl Pts',(-10.6026099100317,-39.0403076982244,
18.6684496683121));
#28656=CARTESIAN_POINT('Ctrl Pts',(-10.7208259397154,-39.0226758354227,
18.6626459246886));
#28657=CARTESIAN_POINT('Ctrl Pts',(-10.8382544254531,-38.999853275678,18.6568421810651));
#28658=CARTESIAN_POINT('Ctrl Pts',(-10.9544123405207,-38.9719418530817,
18.6510384374416));
#28659=CARTESIAN_POINT('Ctrl Pts',(-11.0706079237318,-38.9440213792599,
18.6452328117574));
#28660=CARTESIAN_POINT('Ctrl Pts',(-11.1855317200458,-38.9110088559792,
18.6394271860732));
#28661=CARTESIAN_POINT('Ctrl Pts',(-11.2987144917996,-38.8730563730457,
18.633621560389));
#28662=CARTESIAN_POINT('Ctrl Pts',(-11.4120225795509,-38.8350618691121,
18.6278095067143));
#28663=CARTESIAN_POINT('Ctrl Pts',(-11.5235854076105,-38.792116617767,18.6219974530397));
#28664=CARTESIAN_POINT('Ctrl Pts',(-11.6329522546071,-38.7444214418484,
18.616185399365));
#28665=CARTESIAN_POINT('Ctrl Pts',(-11.7423909255862,-38.6966949432979,
18.6103695287673));
#28666=CARTESIAN_POINT('Ctrl Pts',(-11.8496303775063,-38.6442124868736,
18.6045536581696));
#28667=CARTESIAN_POINT('Ctrl Pts',(-11.9542445799809,-38.5872208074797,
18.5987377875719));
#28668=CARTESIAN_POINT('Ctrl Pts',(-12.0590085890829,-38.530147516497,18.5929135886981));
#28669=CARTESIAN_POINT('Ctrl Pts',(-12.1611394969088,-38.4685523244996,
18.5870893898243));
#28670=CARTESIAN_POINT('Ctrl Pts',(-12.2602402068397,-38.4027252618137,
18.5812651909505));
#28671=CARTESIAN_POINT('Ctrl Pts',(-12.2864981079149,-38.3852836057319,
18.5797220008162));
#28672=CARTESIAN_POINT('Ctrl Pts',(-12.3125434566103,-38.3675450700787,
18.5781788106819));
#28673=CARTESIAN_POINT('Ctrl Pts',(-12.3383692710118,-38.3495155100981,
18.5766356205475));
#28674=CARTESIAN_POINT('Ctrl Pts',(-12.4353485685863,-38.2818121635428,
18.5708407405517));
#28675=CARTESIAN_POINT('Ctrl Pts',(-12.5295492744555,-38.2097788486512,
18.5650458605559));
#28676=CARTESIAN_POINT('Ctrl Pts',(-12.6205578782234,-38.1336721919947,
18.5592509805601));
#28677=CARTESIAN_POINT('Ctrl Pts',(-12.7114513203758,-38.0576618401399,
18.5534634333627));
#28678=CARTESIAN_POINT('Ctrl Pts',(-12.7991603788963,-37.9775886587321,
18.5476758861653));
#28679=CARTESIAN_POINT('Ctrl Pts',(-12.8833004316501,-37.8937525154799,
18.5418883389678));
#28680=CARTESIAN_POINT('Ctrl Pts',(-12.9673565359973,-37.8100000174171,
18.5361065661353));
#28681=CARTESIAN_POINT('Ctrl Pts',(-13.0478504263204,-37.7224923146416,
18.5303247933027));
#28682=CARTESIAN_POINT('Ctrl Pts',(-13.1244310249679,-37.6315690700071,
18.5245430204702));
#28683=CARTESIAN_POINT('Ctrl Pts',(-13.2012298936544,-37.5403866759209,
18.5187447684274));
#28684=CARTESIAN_POINT('Ctrl Pts',(-13.2740928125809,-37.4457695142884,
18.5129465163847));
#28685=CARTESIAN_POINT('Ctrl Pts',(-13.3427031763758,-37.3480972029809,
18.507148264342));
#28686=CARTESIAN_POINT('Ctrl Pts',(-13.4110441711698,-37.2508083598766,
18.501372776635));
#28687=CARTESIAN_POINT('Ctrl Pts',(-13.4751657043617,-37.1504886541793,
18.4955972889281));
#28688=CARTESIAN_POINT('Ctrl Pts',(-13.534796089474,-37.0475452634409,18.4898218012211));
#28689=CARTESIAN_POINT('Ctrl Pts',(-13.5944184924182,-36.9446156527821,
18.4840470866253));
#28690=CARTESIAN_POINT('Ctrl Pts',(-13.6495507358493,-36.8390634126814,
18.4782723720295));
#28691=CARTESIAN_POINT('Ctrl Pts',(-13.6999659003013,-36.7313224242202,
18.4724976574336));
#28692=CARTESIAN_POINT('Ctrl Pts',(-13.7503865306814,-36.6235697546606,
18.4667223167529));
#28693=CARTESIAN_POINT('Ctrl Pts',(-13.7960888906862,-36.5136282391173,
18.4609469760721));
#28694=CARTESIAN_POINT('Ctrl Pts',(-13.8368935305175,-36.4019532928999,
18.4551716353914));
#28695=CARTESIAN_POINT('Ctrl Pts',(-13.8779822997752,-36.2895007356427,
18.4493560800625));
#28696=CARTESIAN_POINT('Ctrl Pts',(-13.9141047250615,-36.1752909100815,
18.4435405247335));
#28697=CARTESIAN_POINT('Ctrl Pts',(-13.945128495028,-36.0598047733983,18.4377249694046));
#28698=CARTESIAN_POINT('Ctrl Pts',(-13.975982656681,-35.9449500044988,18.4319412079722));
#28699=CARTESIAN_POINT('Ctrl Pts',(-14.0017937405414,-35.8288332630182,
18.4261574465398));
#28700=CARTESIAN_POINT('Ctrl Pts',(-14.0224831018297,-35.7119372833998,
18.4203736851074));
#28701=CARTESIAN_POINT('Ctrl Pts',(-14.0433430602509,-35.5940774210066,
18.4145422328303));
#28702=CARTESIAN_POINT('Ctrl Pts',(-14.0589963984069,-35.4754258368058,
18.4087107805531));
#28703=CARTESIAN_POINT('Ctrl Pts',(-14.0694159822337,-35.356480803889,18.4028793282759));
#28704=CARTESIAN_POINT('Ctrl Pts',(-14.0798355660604,-35.2375357709721,
18.3970478759987));
#28705=CARTESIAN_POINT('Ctrl Pts',(-14.0850214380849,-35.1182977151717,
18.3912164237215));
#28706=CARTESIAN_POINT('Ctrl Pts',(-14.0849999333383,-34.9992620122689,
18.3853849714444));
#28707=CARTESIAN_POINT('Ctrl Pts',(-14.0849999333382,-34.9992620114549,
18.3853849714045));
#28708=CARTESIAN_POINT('Ctrl Pts',(-14.0849927683375,-34.9596014672289,
18.3834420369294));
#28709=CARTESIAN_POINT('Ctrl Pts',(-14.0844080317122,-34.9199467334781,
18.3814991024543));
#28710=CARTESIAN_POINT('Ctrl Pts',(-14.0832461448359,-34.8803090618181,
18.3795561679791));
#28711=CARTESIAN_POINT('Ctrl Pts',(-14.0797629590262,-34.7614804750833,
18.3737315030043));
#28712=CARTESIAN_POINT('Ctrl Pts',(-14.0710827252895,-34.6426127214269,
18.3679068380296));
#28713=CARTESIAN_POINT('Ctrl Pts',(-14.0571956019598,-34.5241966294384,
18.3620821730548));
#28714=CARTESIAN_POINT('Ctrl Pts',(-14.0433260050548,-34.4059299860188,
18.3562648591742));
#28715=CARTESIAN_POINT('Ctrl Pts',(-14.024262636187,-34.2881142723218,18.3504475452937));
#28716=CARTESIAN_POINT('Ctrl Pts',(-14.0000476499133,-34.1712396013183,
18.3446302314131));
#28717=CARTESIAN_POINT('Ctrl Pts',(-13.9758569191974,-34.0544820008057,
18.3388187445931));
#28718=CARTESIAN_POINT('Ctrl Pts',(-13.9465249191627,-33.9386639651413,
18.3330072577732));
#28719=CARTESIAN_POINT('Ctrl Pts',(-13.9121454499452,-33.8242691726109,
18.3271957709532));
#28720=CARTESIAN_POINT('Ctrl Pts',(-13.876473537939,-33.7055738853948,18.3211658103056));
#28721=CARTESIAN_POINT('Ctrl Pts',(-13.8353672565244,-33.5884113956389,
18.315135849658));
#28722=CARTESIAN_POINT('Ctrl Pts',(-13.7889894075899,-33.4733093734578,
18.3091058890104));
#28723=CARTESIAN_POINT('Ctrl Pts',(-13.744342338888,-33.3625028567672,18.3033009611517));
#28724=CARTESIAN_POINT('Ctrl Pts',(-13.6948102801032,-33.2536061857114,
18.2974960332931));
#28725=CARTESIAN_POINT('Ctrl Pts',(-13.6405886331091,-33.1470727471169,
18.2916911054345));
#28726=CARTESIAN_POINT('Ctrl Pts',(-13.5863750755856,-33.0405552025272,
18.2858870436284));
#28727=CARTESIAN_POINT('Ctrl Pts',(-13.5274735063545,-32.9364005528948,
18.2800829818223));
#28728=CARTESIAN_POINT('Ctrl Pts',(-13.4641261137532,-32.835039199428,18.2742789200162));
#28729=CARTESIAN_POINT('Ctrl Pts',(-13.400773236667,-32.7336690703071,18.2684743557065));
#28730=CARTESIAN_POINT('Ctrl Pts',(-13.3329739872578,-32.635093064334,18.2626697913969));
#28731=CARTESIAN_POINT('Ctrl Pts',(-13.2610145152082,-32.5397135671631,
18.2568652270872));
#28732=CARTESIAN_POINT('Ctrl Pts',(-13.1890318472518,-32.4443033247147,
18.2510587916947));
#28733=CARTESIAN_POINT('Ctrl Pts',(-13.1128865353371,-32.3520919659564,
18.2452523563022));
#28734=CARTESIAN_POINT('Ctrl Pts',(-13.0329053126748,-32.2634491847677,
18.2394459209098));
#28735=CARTESIAN_POINT('Ctrl Pts',(-12.9528358257594,-32.1747085807572,
18.2336330777547));
#28736=CARTESIAN_POINT('Ctrl Pts',(-12.8689222519123,-32.0895447184489,
18.2278202345997));
#28737=CARTESIAN_POINT('Ctrl Pts',(-12.7815286256401,-32.0082908723031,
18.2220073914446));
#28738=CARTESIAN_POINT('Ctrl Pts',(-12.6940777767297,-31.926983823657,18.21619074222));
#28739=CARTESIAN_POINT('Ctrl Pts',(-12.6031426475152,-31.8495921538102,
18.2103740929954));
#28740=CARTESIAN_POINT('Ctrl Pts',(-12.5091195271677,-31.7764081836582,
18.2045574437708));
#28741=CARTESIAN_POINT('Ctrl Pts',(-12.414962136009,-31.7031197022861,18.1987324880126));
#28742=CARTESIAN_POINT('Ctrl Pts',(-12.3177082834953,-31.6340511495191,
18.1929075322544));
#28743=CARTESIAN_POINT('Ctrl Pts',(-12.2177824212526,-31.5694510450974,
18.1870825764962));
#28744=CARTESIAN_POINT('Ctrl Pts',(-12.1914449027408,-31.5524243574323,
18.1855472894677));
#28745=CARTESIAN_POINT('Ctrl Pts',(-12.1649218871643,-31.5357078392217,
18.1840120024392));
#28746=CARTESIAN_POINT('Ctrl Pts',(-12.1382214026234,-31.5193054955422,
18.1824767154107));
#28747=CARTESIAN_POINT('Ctrl Pts',(-12.0369241125928,-31.4570776748317,
18.1766520864543));
#28748=CARTESIAN_POINT('Ctrl Pts',(-11.9327453225741,-31.3991755625065,
18.170827457498));
#28749=CARTESIAN_POINT('Ctrl Pts',(-11.8260902324513,-31.345876375525,18.1650028285416));
#28750=CARTESIAN_POINT('Ctrl Pts',(-11.7195694289784,-31.2926442961636,
18.159185533224));
#28751=CARTESIAN_POINT('Ctrl Pts',(-11.6105788886912,-31.2440037959266,
18.1533682379065));
#28752=CARTESIAN_POINT('Ctrl Pts',(-11.4995517045763,-31.2001882039629,
18.147550942589));
#28753=CARTESIAN_POINT('Ctrl Pts',(-11.3886354051343,-31.1564163713509,
18.1417394570998));
#28754=CARTESIAN_POINT('Ctrl Pts',(-11.2756868858487,-31.1174600096547,
18.1359279716107));
#28755=CARTESIAN_POINT('Ctrl Pts',(-11.161162156784,-31.0835057199515,18.1301164861215));
#28756=CARTESIAN_POINT('Ctrl Pts',(-11.0423318833288,-31.0482749225214,
18.1240865184849));
#28757=CARTESIAN_POINT('Ctrl Pts',(-10.9218049596498,-31.0184298841488,
18.1180565508483));
#28758=CARTESIAN_POINT('Ctrl Pts',(-10.8001120045011,-30.9941235939868,
18.1120265832116));
#28759=CARTESIAN_POINT('Ctrl Pts',(-10.6829598281673,-30.9707242543323,
18.1062216142141));
#28760=CARTESIAN_POINT('Ctrl Pts',(-10.5647275148102,-30.9524578148195,
18.1004166452166));
#28761=CARTESIAN_POINT('Ctrl Pts',(-10.4459014118456,-30.9394092879343,
18.0946116762191));
#28762=CARTESIAN_POINT('Ctrl Pts',(-10.3270927194324,-30.9263626729359,
18.088807557773));
#28763=CARTESIAN_POINT('Ctrl Pts',(-10.2076908160468,-30.9185324946725,
18.0830034393269));
#28764=CARTESIAN_POINT('Ctrl Pts',(-10.0881884590293,-30.9159520331301,
18.0771993208808));
#28765=CARTESIAN_POINT('Ctrl Pts',(-9.96867543957385,-30.9133713413495,
18.07139468457));
#28766=CARTESIAN_POINT('Ctrl Pts',(-9.84906235675006,-30.9160413064066,
18.0655900482592));
#28767=CARTESIAN_POINT('Ctrl Pts',(-9.72984262241596,-30.9239430829125,
18.0597854119484));
#28768=CARTESIAN_POINT('Ctrl Pts',(-9.61058414560315,-30.9318474272349,
18.0539788893223));
#28769=CARTESIAN_POINT('Ctrl Pts',(-9.49171967855415,-30.9449869373111,
18.0481723666963));
#28770=CARTESIAN_POINT('Ctrl Pts',(-9.37373752527892,-30.9632909056069,
18.0423658440703));
#28771=CARTESIAN_POINT('Ctrl Pts',(-9.255624727833,-30.9816151422796,18.0365528917572));
#28772=CARTESIAN_POINT('Ctrl Pts',(-9.13839659792394,-31.0051151896328,
18.030739939444));
#28773=CARTESIAN_POINT('Ctrl Pts',(-9.02253141690564,-31.0336691805822,
18.0249269871308));
#28774=CARTESIAN_POINT('Ctrl Pts',(-8.90659011559562,-31.0622419307317,
18.0191102158652));
#28775=CARTESIAN_POINT('Ctrl Pts',(-8.79201393718519,-31.0958751223193,
18.0132934445995));
#28776=CARTESIAN_POINT('Ctrl Pts',(-8.67926458013119,-31.1343974660211,
18.0074766733338));
#28777=CARTESIAN_POINT('Ctrl Pts',(-8.56635386875424,-31.172974938611,18.0016515777529));
#28778=CARTESIAN_POINT('Ctrl Pts',(-8.45527557556923,-31.2164553803592,
17.995826482172));
#28779=CARTESIAN_POINT('Ctrl Pts',(-8.3464701931264,-31.2646199419898,17.9900013865911));
#28780=CARTESIAN_POINT('Ctrl Pts',(-8.31780379968252,-31.2773096108531,
17.9884666786748));
#28781=CARTESIAN_POINT('Ctrl Pts',(-8.2892950364283,-31.2903241790584,17.9869319707585));
#28782=CARTESIAN_POINT('Ctrl Pts',(-8.2609516437956,-31.303659131684,17.9853972628422));
#28783=CARTESIAN_POINT('Ctrl Pts',(-8.15351027992575,-31.3542079673793,
17.9795796420018));
#28784=CARTESIAN_POINT('Ctrl Pts',(-8.04809906399801,-31.4095278223734,
17.9737620211614));
#28785=CARTESIAN_POINT('Ctrl Pts',(-7.94517137702572,-31.4694328599776,
17.9679444003209));
#28786=CARTESIAN_POINT('Ctrl Pts',(-7.84238877816553,-31.5292534547165,
17.9621349800692));
#28787=CARTESIAN_POINT('Ctrl Pts',(-7.74208309268596,-31.5936461665222,
17.9563255598174));
#28788=CARTESIAN_POINT('Ctrl Pts',(-7.64468617915615,-31.6623778216608,
17.9505161395657));
#28789=CARTESIAN_POINT('Ctrl Pts',(-7.60011108377388,-31.6938338501174,
17.9478573750068));
#28790=CARTESIAN_POINT('Ctrl Pts',(-7.55614494409697,-31.7261980482037,
17.9451986104479));
#28791=CARTESIAN_POINT('Ctrl Pts',(-7.51282745730979,-31.7594448403263,
17.9425398458891));
#28792=CARTESIAN_POINT('',(-14.0849995332614,-35.001952755595,18.4896150286338));
#28793=CARTESIAN_POINT('Ctrl Pts',(-14.0849995332617,-35.0019527548048,
18.4896150285955));
#28794=CARTESIAN_POINT('Ctrl Pts',(-14.0850575830891,-34.8805173769074,
18.4837275465484));
#28795=CARTESIAN_POINT('Ctrl Pts',(-14.0796963945017,-34.7590902192459,
18.4778400645013));
#28796=CARTESIAN_POINT('Ctrl Pts',(-14.068944624063,-34.6381787094313,18.4719525824541));
#28797=CARTESIAN_POINT('Ctrl Pts',(-14.0581894969497,-34.5172294513599,
18.4660632623505));
#28798=CARTESIAN_POINT('Ctrl Pts',(-14.0420404715241,-34.3967965517054,
18.4601739422469));
#28799=CARTESIAN_POINT('Ctrl Pts',(-14.0205780196417,-34.2773815751216,
18.4542846221433));
#28800=CARTESIAN_POINT('Ctrl Pts',(-13.999104411433,-34.1579045258323,18.4483922407316));
#28801=CARTESIAN_POINT('Ctrl Pts',(-13.9723119464262,-34.039446838248,18.44249985932));
#28802=CARTESIAN_POINT('Ctrl Pts',(-13.9403319704358,-33.9224987411787,
18.4366074779083));
#28803=CARTESIAN_POINT('Ctrl Pts',(-13.9083066257222,-33.805384734484,18.4307067372089));
#28804=CARTESIAN_POINT('Ctrl Pts',(-13.8710791744484,-33.689784973889,18.4248059965095));
#28805=CARTESIAN_POINT('Ctrl Pts',(-13.8288306955208,-33.5761739906022,
18.4189052558101));
#28806=CARTESIAN_POINT('Ctrl Pts',(-13.7865496100022,-33.4624753244695,
18.4129999610287));
#28807=CARTESIAN_POINT('Ctrl Pts',(-13.7392399260949,-33.3507688546655,
18.4070946662472));
#28808=CARTESIAN_POINT('Ctrl Pts',(-13.687129973312,-33.241507020229,18.4011893714658));
#28809=CARTESIAN_POINT('Ctrl Pts',(-13.634928187988,-33.132052635399,18.3952736698773));
#28810=CARTESIAN_POINT('Ctrl Pts',(-13.5779094167131,-33.0250518383686,
18.3893579682888));
#28811=CARTESIAN_POINT('Ctrl Pts',(-13.5163471857879,-32.9209311052778,
18.3834422667002));
#28812=CARTESIAN_POINT('Ctrl Pts',(-13.4777388784652,-32.8556325415087,
18.3797322772875));
#28813=CARTESIAN_POINT('Ctrl Pts',(-13.437344457819,-32.7914661462019,18.3760222878747));
#28814=CARTESIAN_POINT('Ctrl Pts',(-13.3952395708656,-32.7285305953132,
18.3723122984619));
#28815=CARTESIAN_POINT('Ctrl Pts',(-13.3291450185491,-32.629736907412,18.3664885068054));
#28816=CARTESIAN_POINT('Ctrl Pts',(-13.2586283616502,-32.5336711932551,
18.3606647151489));
#28817=CARTESIAN_POINT('Ctrl Pts',(-13.1839420305572,-32.4407543794994,
18.3548409234924));
#28818=CARTESIAN_POINT('Ctrl Pts',(-13.1093499023061,-32.3479547629308,
18.3490244774602));
#28819=CARTESIAN_POINT('Ctrl Pts',(-13.0305988139817,-32.2582964624724,
18.3432080314279));
#28820=CARTESIAN_POINT('Ctrl Pts',(-12.9479848629971,-32.1721721679812,
18.3373915853957));
#28821=CARTESIAN_POINT('Ctrl Pts',(-12.8654535856495,-32.0861340600067,
18.3315809600117));
#28822=CARTESIAN_POINT('Ctrl Pts',(-12.7790674169178,-32.0036232154057,
18.3257703346277));
#28823=CARTESIAN_POINT('Ctrl Pts',(-12.6891627840684,-31.9249994275153,
18.3199597092437));
#28824=CARTESIAN_POINT('Ctrl Pts',(-12.5958594629035,-31.8434034040375,
18.3139294232707));
#28825=CARTESIAN_POINT('Ctrl Pts',(-12.498766690014,-31.7659944728829,18.3078991372978));
#28826=CARTESIAN_POINT('Ctrl Pts',(-12.3983029695353,-31.6931332251936,
18.3018688513249));
#28827=CARTESIAN_POINT('Ctrl Pts',(-12.3016076812011,-31.6230050304569,
18.2960647636591));
#28828=CARTESIAN_POINT('Ctrl Pts',(-12.2017901417147,-31.557089754572,18.2902606759933));
#28829=CARTESIAN_POINT('Ctrl Pts',(-12.0992567518518,-31.4956675257898,
18.2844565883275));
#28830=CARTESIAN_POINT('Ctrl Pts',(-11.9967384980758,-31.4342543642216,
18.2786533574672));
#28831=CARTESIAN_POINT('Ctrl Pts',(-11.8915055413924,-31.3773331404906,
18.272850126607));
#28832=CARTESIAN_POINT('Ctrl Pts',(-11.7839916953017,-31.3251396446811,
18.2670468957467));
#28833=CARTESIAN_POINT('Ctrl Pts',(-11.6764683522758,-31.272941538505,18.2612431522743));
#28834=CARTESIAN_POINT('Ctrl Pts',(-11.5666640865868,-31.225472168885,18.2554394088018));
#28835=CARTESIAN_POINT('Ctrl Pts',(-11.4550350563148,-31.1829202281201,
18.2496356653294));
#28836=CARTESIAN_POINT('Ctrl Pts',(-11.3433698265356,-31.140354488442,18.2438300397958));
#28837=CARTESIAN_POINT('Ctrl Pts',(-11.229879036659,-31.1027094943694,18.2380244142623));
#28838=CARTESIAN_POINT('Ctrl Pts',(-11.1150358409108,-31.0701246745623,
18.2322187887288));
#28839=CARTESIAN_POINT('Ctrl Pts',(-11.0000654907144,-31.0375037768251,
18.2264067352035));
#28840=CARTESIAN_POINT('Ctrl Pts',(-10.8837401387693,-31.0099543481992,
18.2205946816783));
#28841=CARTESIAN_POINT('Ctrl Pts',(-10.7665451741307,-30.987565141212,18.2147826281531));
#28842=CARTESIAN_POINT('Ctrl Pts',(-10.6492732445727,-30.9651612306621,
18.2089667577042));
#28843=CARTESIAN_POINT('Ctrl Pts',(-10.5311309680637,-30.9479243495558,
18.2031508872553));
#28844=CARTESIAN_POINT('Ctrl Pts',(-10.4126092794624,-30.935891416005,18.1973350168064));
#28845=CARTESIAN_POINT('Ctrl Pts',(-10.2939178687895,-30.9238412513935,
18.1915108180794));
#28846=CARTESIAN_POINT('Ctrl Pts',(-10.1748463677846,-30.9170099314566,
18.1856866193525));
#28847=CARTESIAN_POINT('Ctrl Pts',(-10.0558862779217,-30.9153823038208,
18.1798624206255));
#28848=CARTESIAN_POINT('Ctrl Pts',(-10.0243663698065,-30.9149510442817,
18.1783192290481));
#28849=CARTESIAN_POINT('Ctrl Pts',(-9.99285425617415,-30.9148848268477,
18.1767760374708));
#28850=CARTESIAN_POINT('Ctrl Pts',(-9.96135900559659,-30.9151827613036,
18.1752328458934));
#28851=CARTESIAN_POINT('Ctrl Pts',(-9.84254216014076,-30.9163067286177,
18.1694111060503));
#28852=CARTESIAN_POINT('Ctrl Pts',(-9.72358249997705,-30.9226209291842,
18.1635893662072));
#28853=CARTESIAN_POINT('Ctrl Pts',(-9.6049700399353,-30.9341450676824,18.1577676263641));
#28854=CARTESIAN_POINT('Ctrl Pts',(-9.48649777117739,-30.9456555854887,
18.1519527673932));
#28855=CARTESIAN_POINT('Ctrl Pts',(-9.36837228927801,-30.9623637587939,
18.1461379084223));
#28856=CARTESIAN_POINT('Ctrl Pts',(-9.25108406035002,-30.9842373183493,
18.1403230494514));
#28857=CARTESIAN_POINT('Ctrl Pts',(-9.13390674299997,-31.0060901935528,
18.134513689201));
#28858=CARTESIAN_POINT('Ctrl Pts',(-9.0175655031429,-31.033098666387,18.1287043289505));
#28859=CARTESIAN_POINT('Ctrl Pts',(-8.90254549512174,-31.0651787067616,
18.1228949687001));
#28860=CARTESIAN_POINT('Ctrl Pts',(-8.78760708024051,-31.0972359901284,
18.1170897295061));
#28861=CARTESIAN_POINT('Ctrl Pts',(-8.67398842467963,-31.134357574507,18.1112844903121));
#28862=CARTESIAN_POINT('Ctrl Pts',(-8.56216366771447,-31.1764085362634,
18.1054792511181));
#28863=CARTESIAN_POINT('Ctrl Pts',(-8.45038370261397,-31.2184426543347,
18.0996763372365));
#28864=CARTESIAN_POINT('Ctrl Pts',(-8.34039658894526,-31.2654020799654,
18.0938734233548));
#28865=CARTESIAN_POINT('Ctrl Pts',(-8.23265998151875,-31.3171024642172,
18.0880705094732));
#28866=CARTESIAN_POINT('Ctrl Pts',(-8.12494812156206,-31.3687909727128,
18.0822689285409));
#28867=CARTESIAN_POINT('Ctrl Pts',(-8.01948610574778,-31.4252180931851,
18.0764673476085));
#28868=CARTESIAN_POINT('Ctrl Pts',(-7.91670964774879,-31.4861522075911,
18.0706657666762));
#28869=CARTESIAN_POINT('Ctrl Pts',(-7.81391283532173,-31.547098389732,18.0648630367661));
#28870=CARTESIAN_POINT('Ctrl Pts',(-7.71380299386624,-31.612553139466,18.059060306856));
#28871=CARTESIAN_POINT('Ctrl Pts',(-7.61678904282017,-31.6822401332257,
18.053257576946));
#28872=CARTESIAN_POINT('Ctrl Pts',(-7.58172493086275,-31.7074273617101,
18.0511602747638));
#28873=CARTESIAN_POINT('Ctrl Pts',(-7.54706496700791,-31.733167060793,18.0490629725817));
#28874=CARTESIAN_POINT('Ctrl Pts',(-7.51282745730981,-31.7594448403263,
18.0469656703996));
#28875=CARTESIAN_POINT('Ctrl Pts',(-7.51282745730977,-31.7594448403263,
19.2967866684593));
#28876=CARTESIAN_POINT('Ctrl Pts',(-7.41811230182008,-31.8321400800316,
19.2909817497243));
#28877=CARTESIAN_POINT('Ctrl Pts',(-7.32652932999714,-31.9090354648001,
19.2851768309894));
#28878=CARTESIAN_POINT('Ctrl Pts',(-7.23846562792,-31.9898251027854,19.2793719122544));
#28879=CARTESIAN_POINT('Ctrl Pts',(-7.15042629203376,-32.0705923872279,
19.2735685996721));
#28880=CARTESIAN_POINT('Ctrl Pts',(-7.06590459032354,-32.1552515065383,
19.2677652870899));
#28881=CARTESIAN_POINT('Ctrl Pts',(-6.98525340953167,-32.2434572386303,
19.2619619745077));
#28882=CARTESIAN_POINT('Ctrl Pts',(-6.90460550996115,-32.3316593821508,
19.256158898028));
#28883=CARTESIAN_POINT('Ctrl Pts',(-6.82782809357387,-32.4234075500423,
19.2503558215484));
#28884=CARTESIAN_POINT('Ctrl Pts',(-6.75523570142573,-32.5183212039634,
19.2445527450688));
#28885=CARTESIAN_POINT('Ctrl Pts',(-6.68262913065411,-32.6132533962591,
19.2387485351421));
#28886=CARTESIAN_POINT('Ctrl Pts',(-6.61420945765297,-32.7113519797587,
19.2329443252153));
#28887=CARTESIAN_POINT('Ctrl Pts',(-6.55024921419173,-32.8122055590583,
19.2271401152886));
#28888=CARTESIAN_POINT('Ctrl Pts',(-6.48622215928464,-32.9131644877608,
19.2213298424134));
#28889=CARTESIAN_POINT('Ctrl Pts',(-6.4266640565776,-33.0168838145444,19.2155195695383));
#28890=CARTESIAN_POINT('Ctrl Pts',(-6.37180269974769,-33.1229253210269,
19.2097092966631));
#28891=CARTESIAN_POINT('Ctrl Pts',(-6.31691165533461,-33.2290242106335,
19.2038958796266));
#28892=CARTESIAN_POINT('Ctrl Pts',(-6.26672259176406,-33.3374474129976,
19.1980824625901));
#28893=CARTESIAN_POINT('Ctrl Pts',(-6.22141541612506,-33.4477359945864,
19.1922690455535));
#28894=CARTESIAN_POINT('Ctrl Pts',(-6.17603645820562,-33.5581993115407,
19.1864464180481));
#28895=CARTESIAN_POINT('Ctrl Pts',(-6.13555497936683,-33.6705335279456,
19.1806237905427));
#28896=CARTESIAN_POINT('Ctrl Pts',(-6.10010137767713,-33.7842632951152,
19.1748011630372));
#28897=CARTESIAN_POINT('Ctrl Pts',(-6.07133916713093,-33.8765280962299,
19.1700774782701));
#28898=CARTESIAN_POINT('Ctrl Pts',(-6.04588510475766,-33.969711018008,19.1653537935029));
#28899=CARTESIAN_POINT('Ctrl Pts',(-6.02378394272223,-34.0635541308509,
19.1606301087357));
#28900=CARTESIAN_POINT('Ctrl Pts',(-5.99653648754323,-34.179248772017,19.154806505942));
#28901=CARTESIAN_POINT('Ctrl Pts',(-5.97429877815729,-34.2963201807641,
19.1489829031483));
#28902=CARTESIAN_POINT('Ctrl Pts',(-5.95720681340291,-34.4142967898294,
19.1431593003546));
#28903=CARTESIAN_POINT('Ctrl Pts',(-5.9401364129236,-34.532124552341,19.1373430449767));
#28904=CARTESIAN_POINT('Ctrl Pts',(-5.92819890229578,-34.6508548430926,
19.1315267895989));
#28905=CARTESIAN_POINT('Ctrl Pts',(-5.92147985714887,-34.7700033818561,
19.125710534221));
#28906=CARTESIAN_POINT('Ctrl Pts',(-5.91476753790458,-34.8890326504776,
19.1199001010346));
#28907=CARTESIAN_POINT('Ctrl Pts',(-5.91326331491269,-35.0084789288646,
19.1140896678482));
#28908=CARTESIAN_POINT('Ctrl Pts',(-5.91700120472805,-35.1278508420302,
19.1082792346619));
#28909=CARTESIAN_POINT('Ctrl Pts',(-5.92088057325785,-35.2517409688533,
19.1022488772246));
#28910=CARTESIAN_POINT('Ctrl Pts',(-5.93040678586944,-35.3755505462157,
19.0962185197873));
#28911=CARTESIAN_POINT('Ctrl Pts',(-5.94555850193402,-35.498727519554,19.09018816235));
#28912=CARTESIAN_POINT('Ctrl Pts',(-5.96014120915312,-35.6172786942639,
19.0843842694735));
#28913=CARTESIAN_POINT('Ctrl Pts',(-5.97993446342108,-35.7352434801594,
19.078580376597));
#28914=CARTESIAN_POINT('Ctrl Pts',(-6.00486629169651,-35.8521335885747,
19.0727764837204));
#28915=CARTESIAN_POINT('Ctrl Pts',(-6.02979443675131,-35.9690064286191,
19.0669734482627));
#28916=CARTESIAN_POINT('Ctrl Pts',(-6.05985956098728,-36.0848045076697,
19.061170412805));
#28917=CARTESIAN_POINT('Ctrl Pts',(-6.09493856249193,-36.1990496942527,
19.0553673773472));
#28918=CARTESIAN_POINT('Ctrl Pts',(-6.13002066030497,-36.3133049648835,
19.0495638296746));
#28919=CARTESIAN_POINT('Ctrl Pts',(-6.17011739543714,-36.4260066801526,
19.0437602820019));
#28920=CARTESIAN_POINT('Ctrl Pts',(-6.21505597183103,-36.5366924557725,
19.0379567343293));
#28921=CARTESIAN_POINT('Ctrl Pts',(-6.26000912017273,-36.6474141227685,
19.032151304777));
#28922=CARTESIAN_POINT('Ctrl Pts',(-6.30980707868948,-36.756118171914,19.0263458752247));
#28923=CARTESIAN_POINT('Ctrl Pts',(-6.36422941753683,-36.8623633565165,
19.0205404456723));
#28924=CARTESIAN_POINT('Ctrl Pts',(-6.4187120216759,-36.9687261931196,19.0147285874013));
#28925=CARTESIAN_POINT('Ctrl Pts',(-6.47782904156566,-37.0726243664797,
19.0089167291304));
#28926=CARTESIAN_POINT('Ctrl Pts',(-6.54131462508069,-37.1736422146525,
19.0031048708594));
#28927=CARTESIAN_POINT('Ctrl Pts',(-6.60484190473565,-37.2747264094523,
18.9972891954689));
#28928=CARTESIAN_POINT('Ctrl Pts',(-6.67274323037939,-37.3729261765179,
18.9914735200785));
#28929=CARTESIAN_POINT('Ctrl Pts',(-6.74471103920186,-37.4678571234384,
18.985657844688));
#28930=CARTESIAN_POINT('Ctrl Pts',(-6.81678193082489,-37.5629240443177,
18.9798338392384));
#28931=CARTESIAN_POINT('Ctrl Pts',(-6.89293067143959,-37.6547124867205,
18.9740098337888));
#28932=CARTESIAN_POINT('Ctrl Pts',(-6.97281120843644,-37.7428731323617,
18.9681858283392));
#28933=CARTESIAN_POINT('Ctrl Pts',(-6.9940028118998,-37.766261375778,18.9666407709485));
#28934=CARTESIAN_POINT('Ctrl Pts',(-7.01545686835546,-37.7893945098375,
18.9650957135579));
#28935=CARTESIAN_POINT('Ctrl Pts',(-7.03716652044213,-37.8122664831788,
18.9635506561672));
#28936=CARTESIAN_POINT('Ctrl Pts',(-7.11899448754544,-37.8984754686886,
18.9577270296609));
#28937=CARTESIAN_POINT('Ctrl Pts',(-7.20472012898345,-37.9812490979073,
18.9519034031545));
#28938=CARTESIAN_POINT('Ctrl Pts',(-7.29402358378522,-38.0602151288577,
18.9460797766482));
#28939=CARTESIAN_POINT('Ctrl Pts',(-7.38321437281215,-38.1390815357892,
18.940263497264));
#28940=CARTESIAN_POINT('Ctrl Pts',(-7.47597369417695,-38.2141496307771,
18.9344472178798));
#28941=CARTESIAN_POINT('Ctrl Pts',(-7.57194341428716,-38.2850823759194,
18.9286309384956));
#28942=CARTESIAN_POINT('Ctrl Pts',(-7.6678170714414,-38.3559441194045,18.9228204810414));
#28943=CARTESIAN_POINT('Ctrl Pts',(-7.76689440795815,-38.4226785064943,
18.9170100235872));
#28944=CARTESIAN_POINT('Ctrl Pts',(-7.86878309388657,-38.4849877329908,
18.911199566133));
#28945=CARTESIAN_POINT('Ctrl Pts',(-7.97452765582091,-38.5496549902068,
18.9051692176941));
#28946=CARTESIAN_POINT('Ctrl Pts',(-8.08330022028003,-38.6095552419705,
18.8991388692552));
#28947=CARTESIAN_POINT('Ctrl Pts',(-8.19462736983438,-38.6644037258808,
18.8931085208162));
#28948=CARTESIAN_POINT('Ctrl Pts',(-8.30177434702584,-38.7171927290848,
18.8873046031804));
#28949=CARTESIAN_POINT('Ctrl Pts',(-8.41128712709699,-38.7653023007235,
18.8815006855446));
#28950=CARTESIAN_POINT('Ctrl Pts',(-8.52271786244398,-38.8085249751128,
18.8756967679088));
#28951=CARTESIAN_POINT('Ctrl Pts',(-8.63413213865007,-38.8517412651945,
18.8698937075544));
#28952=CARTESIAN_POINT('Ctrl Pts',(-8.74746342615259,-38.8900719458933,
18.8640906472));
#28953=CARTESIAN_POINT('Ctrl Pts',(-8.86224434573965,-38.9233578821207,
18.8582875868457));
#28954=CARTESIAN_POINT('Ctrl Pts',(-8.97703539878588,-38.9566467570044,
18.8524840141668));
#28955=CARTESIAN_POINT('Ctrl Pts',(-9.09327594618063,-38.9848898881663,
18.8466804414879));
#28956=CARTESIAN_POINT('Ctrl Pts',(-9.21048453883426,-39.0079783353432,
18.840876868809));
#28957=CARTESIAN_POINT('Ctrl Pts',(-9.32773113946557,-39.031074269558,18.8350714141686));
#28958=CARTESIAN_POINT('Ctrl Pts',(-9.4459460092339,-39.0490121165882,18.8292659595283));
#28959=CARTESIAN_POINT('Ctrl Pts',(-9.56463926691708,-39.0617343625709,
18.8234605048879));
#28960=CARTESIAN_POINT('Ctrl Pts',(-9.68346396042756,-39.0744706966236,
18.8176486215358));
#28961=CARTESIAN_POINT('Ctrl Pts',(-9.80276769302514,-39.0819798576253,
18.8118367381837));
#28962=CARTESIAN_POINT('Ctrl Pts',(-9.92205708305286,-39.0842563462273,
18.8060248548316));
#28963=CARTESIAN_POINT('Ctrl Pts',(-10.0414248202914,-39.0865343299876,
18.8002091543349));
#28964=CARTESIAN_POINT('Ctrl Pts',(-10.1607777889321,-39.083572807119,18.7943934538383));
#28965=CARTESIAN_POINT('Ctrl Pts',(-10.2796258959687,-39.0754183047024,
18.7885777533416));
#28966=CARTESIAN_POINT('Ctrl Pts',(-10.3986442306876,-39.0672521224865,
18.7827537229418));
#28967=CARTESIAN_POINT('Ctrl Pts',(-10.5171558561783,-39.0538781605604,
18.776929692542));
#28968=CARTESIAN_POINT('Ctrl Pts',(-10.6346789156901,-39.0353943641209,
18.7711056621422));
#28969=CARTESIAN_POINT('Ctrl Pts',(-10.6658518154301,-39.0304915515527,
18.7695608426277));
#28970=CARTESIAN_POINT('Ctrl Pts',(-10.6969552370849,-39.0252295000134,
18.7680160231133));
#28971=CARTESIAN_POINT('Ctrl Pts',(-10.7279803646265,-39.0196106265058,
18.7664712035988));
#28972=CARTESIAN_POINT('Ctrl Pts',(-10.8449353797245,-38.9984292329712,
18.7606477178001));
#28973=CARTESIAN_POINT('Ctrl Pts',(-10.9611538213096,-38.9721050356772,
18.7548242320015));
#28974=CARTESIAN_POINT('Ctrl Pts',(-11.0761490389905,-38.9407014915976,
18.7490007462028));
#28975=CARTESIAN_POINT('Ctrl Pts',(-11.1909991683903,-38.909337569046,18.7431846078362));
#28976=CARTESIAN_POINT('Ctrl Pts',(-11.3046287530725,-38.8729071528003,
18.7373684694695));
#28977=CARTESIAN_POINT('Ctrl Pts',(-11.416559605072,-38.8315250077845,18.7315523311029));
#28978=CARTESIAN_POINT('Ctrl Pts',(-11.5283784120568,-38.790184287121,18.7257420148067));
#28979=CARTESIAN_POINT('Ctrl Pts',(-11.6385014884079,-38.7439018393689,
18.7199316985106));
#28980=CARTESIAN_POINT('Ctrl Pts',(-11.7464647136278,-38.6928425371322,
18.7141213822144));
#28981=CARTESIAN_POINT('Ctrl Pts',(-11.8585174041288,-38.639849194454,18.7080909809151));
#28982=CARTESIAN_POINT('Ctrl Pts',(-11.9682429529133,-38.5817100820163,
18.7020605796157));
#28983=CARTESIAN_POINT('Ctrl Pts',(-12.0751436498692,-38.5186650639706,
18.6960301783164));
#28984=CARTESIAN_POINT('Ctrl Pts',(-12.1780269867652,-38.4579892964976,
18.6902264012956));
#28985=CARTESIAN_POINT('Ctrl Pts',(-12.2782935745585,-38.3927699262819,
18.6844226242748));
#28986=CARTESIAN_POINT('Ctrl Pts',(-12.3755244157646,-38.3232677818837,
18.6786188472541));
#28987=CARTESIAN_POINT('Ctrl Pts',(-12.4727409023177,-38.2537758984187,
18.6728159270726));
#28988=CARTESIAN_POINT('Ctrl Pts',(-12.5669222014561,-38.1800027355907,
18.6670130068911));
#28989=CARTESIAN_POINT('Ctrl Pts',(-12.6576790313083,-38.1022519508487,
18.6612100867096));
#28990=CARTESIAN_POINT('Ctrl Pts',(-12.7484438831084,-38.024494293756,18.6554066536111));
#28991=CARTESIAN_POINT('Ctrl Pts',(-12.8357833536778,-37.9427585814093,
18.6496032205126));
#28992=CARTESIAN_POINT('Ctrl Pts',(-12.9193424301072,-37.8573877538367,
18.6437997874141));
#28993=CARTESIAN_POINT('Ctrl Pts',(-13.0029286141271,-37.7719892309192,
18.6379944716106));
#28994=CARTESIAN_POINT('Ctrl Pts',(-13.0827316794739,-37.682953539143,18.6321891558071));
#28995=CARTESIAN_POINT('Ctrl Pts',(-13.1584350028544,-37.5906588607426,
18.6263838400036));
#28996=CARTESIAN_POINT('Ctrl Pts',(-13.2342221822704,-37.4982619481802,
18.6205720936929));
#28997=CARTESIAN_POINT('Ctrl Pts',(-13.3059002958618,-37.4025991591309,
18.6147603473822));
#28998=CARTESIAN_POINT('Ctrl Pts',(-13.3731943052379,-37.3040801156016,
18.6089486010715));
#28999=CARTESIAN_POINT('Ctrl Pts',(-13.4405325234464,-37.2054963499384,
18.6031330367312));
#29000=CARTESIAN_POINT('Ctrl Pts',(-13.503480686763,-37.1040529390479,18.5973174723909));
#29001=CARTESIAN_POINT('Ctrl Pts',(-13.5618090734252,-37.000185272535,18.5915019080506));
#29002=CARTESIAN_POINT('Ctrl Pts',(-13.6202210299261,-36.896168789903,18.5856780114762));
#29003=CARTESIAN_POINT('Ctrl Pts',(-13.6739998151822,-36.7897214822269,
18.5798541149018));
#29004=CARTESIAN_POINT('Ctrl Pts',(-13.7229632272811,-36.6813000351848,
18.5740302183273));
#29005=CARTESIAN_POINT('Ctrl Pts',(-13.7359622668343,-36.6525157936851,
18.5724840625617));
#29006=CARTESIAN_POINT('Ctrl Pts',(-13.7486221793541,-36.6235924987563,
18.570937906796));
#29007=CARTESIAN_POINT('Ctrl Pts',(-13.760940146646,-36.5945388716951,18.5693917510303));
#29008=CARTESIAN_POINT('Ctrl Pts',(-13.8139041428435,-36.4696159719389,
18.5627436908306));
#29009=CARTESIAN_POINT('Ctrl Pts',(-13.8606921368581,-36.3419281838578,
18.5560956306309));
#29010=CARTESIAN_POINT('Ctrl Pts',(-13.9010386242277,-36.2120736991964,
18.5494475704312));
#29011=CARTESIAN_POINT('Ctrl Pts',(-13.9400043386838,-36.0866632087167,
18.5430270259844));
#29012=CARTESIAN_POINT('Ctrl Pts',(-13.9729620104295,-35.9592321474535,
18.5366064815376));
#29013=CARTESIAN_POINT('Ctrl Pts',(-13.9997194876352,-35.8303427125178,
18.5301859370908));
#29014=CARTESIAN_POINT('Ctrl Pts',(-14.0264024397389,-35.701812261286,18.5237832751867));
#29015=CARTESIAN_POINT('Ctrl Pts',(-14.0469195642965,-35.5718317830148,
18.5173806132826));
#29016=CARTESIAN_POINT('Ctrl Pts',(-14.0611283190673,-35.4409782036222,
18.5109779513786));
#29017=CARTESIAN_POINT('Ctrl Pts',(-14.0752785314931,-35.31066376193,18.5046016694668));
#29018=CARTESIAN_POINT('Ctrl Pts',(-14.0831721511011,-35.1794836454211,
18.498225387555));
#29019=CARTESIAN_POINT('Ctrl Pts',(-14.0847177083086,-35.0480233633797,
18.4918491056432));
#29020=CARTESIAN_POINT('Ctrl Pts',(-14.0848982154794,-35.0326699856684,
18.4911044133067));
#29021=CARTESIAN_POINT('Ctrl Pts',(-14.0849921906863,-35.0173128016336,
18.4903597209703));
#29022=CARTESIAN_POINT('Ctrl Pts',(-14.0849995332614,-35.001952755595,18.4896150286338));
#29023=CARTESIAN_POINT('Origin',(-10.,-35.,32.7603849714045));
#29024=CARTESIAN_POINT('',(-7.51282745730979,-31.7594448403263,20.5469196554144));
#29025=CARTESIAN_POINT('',(-7.51282745730978,-31.7594448403263,20.4426717943404));
#29026=CARTESIAN_POINT('',(-7.5128274573098,-31.7594448403263,32.7603849714045));
#29027=CARTESIAN_POINT('',(-14.0849992317303,-34.9974946531383,19.6353849713615));
#29028=CARTESIAN_POINT('Ctrl Pts',(-7.51282745730978,-31.7594448403263,
20.4426717943404));
#29029=CARTESIAN_POINT('Ctrl Pts',(-7.41801457216884,-31.83221508894,20.4368682884277));
#29030=CARTESIAN_POINT('Ctrl Pts',(-7.32640772298353,-31.9091424187619,
20.4310647825151));
#29031=CARTESIAN_POINT('Ctrl Pts',(-7.23838002126121,-31.9899036405738,
20.4252612766024));
#29032=CARTESIAN_POINT('Ctrl Pts',(-7.15032437497231,-32.070690500194,20.4194559283555));
#29033=CARTESIAN_POINT('Ctrl Pts',(-7.06585043653951,-32.1553133963662,
20.4136505801085));
#29034=CARTESIAN_POINT('Ctrl Pts',(-6.98529490154283,-32.2434118607713,
20.4078452318615));
#29035=CARTESIAN_POINT('Ctrl Pts',(-6.90465041251276,-32.3316076085443,
20.4020334730167));
#29036=CARTESIAN_POINT('Ctrl Pts',(-6.82793323981866,-32.4232862840495,
20.3962217141718));
#29037=CARTESIAN_POINT('Ctrl Pts',(-6.7554402684333,-32.5180537579762,20.390409955327));
#29038=CARTESIAN_POINT('Ctrl Pts',(-6.68290012777349,-32.6128828946118,
20.3845944149231));
#29039=CARTESIAN_POINT('Ctrl Pts',(-6.61458989548414,-32.7108044981316,
20.3787788745193));
#29040=CARTESIAN_POINT('Ctrl Pts',(-6.55076260764328,-32.8113962416261,
20.3729633341154));
#29041=CARTESIAN_POINT('Ctrl Pts',(-6.48684340383313,-32.9121328445987,
20.3671394189075));
#29042=CARTESIAN_POINT('Ctrl Pts',(-6.42742023329891,-33.015546909901,20.3613155036995));
#29043=CARTESIAN_POINT('Ctrl Pts',(-6.37269984728246,-33.1211922391859,
20.3554915884915));
#29044=CARTESIAN_POINT('Ctrl Pts',(-6.35659889460636,-33.1522773716401,
20.3537779568822));
#29045=CARTESIAN_POINT('Ctrl Pts',(-6.34090477651809,-33.1835555567077,
20.3520643252729));
#29046=CARTESIAN_POINT('Ctrl Pts',(-6.32562195109587,-33.215015139075,20.3503506936635));
#29047=CARTESIAN_POINT('Ctrl Pts',(-6.27368491830175,-33.3219271344658,
20.3445271015834));
#29048=CARTESIAN_POINT('Ctrl Pts',(-6.22633417308424,-33.4312802038204,
20.3387035095032));
#29049=CARTESIAN_POINT('Ctrl Pts',(-6.18380574197683,-33.5426440431278,
20.332879917423));
#29050=CARTESIAN_POINT('Ctrl Pts',(-6.14133096681192,-33.6538673803851,
20.3270636726706));
#29051=CARTESIAN_POINT('Ctrl Pts',(-6.10366654908498,-33.767096063685,20.3212474279182));
#29052=CARTESIAN_POINT('Ctrl Pts',(-6.071002103367,-33.8818763358852,20.3154311831658));
#29053=CARTESIAN_POINT('Ctrl Pts',(-6.0383703549341,-33.9965417124183,20.3096207605055));
#29054=CARTESIAN_POINT('Ctrl Pts',(-6.01072873281045,-34.1127551975689,
20.3038103378452));
#29055=CARTESIAN_POINT('Ctrl Pts',(-5.98821810023126,-34.2300448138444,
20.297999915185));
#29056=CARTESIAN_POINT('Ctrl Pts',(-5.96485538495364,-34.3517741299987,
20.2919695537645));
#29057=CARTESIAN_POINT('Ctrl Pts',(-5.94701993528333,-34.4746622366628,
20.2859391923441));
#29058=CARTESIAN_POINT('Ctrl Pts',(-5.93481189984071,-34.5981658173782,
20.2799088309237));
#29059=CARTESIAN_POINT('Ctrl Pts',(-5.92306235444929,-34.7170310463039,
20.2741049482623));
#29060=CARTESIAN_POINT('Ctrl Pts',(-5.91652519881065,-34.8364659100945,
20.2683010656008));
#29061=CARTESIAN_POINT('Ctrl Pts',(-5.91523720607281,-34.9559782173449,
20.2624971829394));
#29062=CARTESIAN_POINT('Ctrl Pts',(-5.91394940358339,-35.0754728715235,
20.256694157565));
#29063=CARTESIAN_POINT('Ctrl Pts',(-5.91790922646807,-35.1950445382098,
20.2508911321906));
#29064=CARTESIAN_POINT('Ctrl Pts',(-5.92710133590371,-35.3141997326585,
20.2450881068162));
#29065=CARTESIAN_POINT('Ctrl Pts',(-5.93629425692309,-35.43336544748,20.2392845690849));
#29066=CARTESIAN_POINT('Ctrl Pts',(-5.95072035158373,-35.5521142098069,
20.2334810313536));
#29067=CARTESIAN_POINT('Ctrl Pts',(-5.97031234403708,-35.6699570100985,
20.2276774936223));
#29068=CARTESIAN_POINT('Ctrl Pts',(-5.98991068998727,-35.7878380256896,
20.2218720738589));
#29069=CARTESIAN_POINT('Ctrl Pts',(-6.01467819849276,-35.9048120923528,
20.2160666540955));
#29070=CARTESIAN_POINT('Ctrl Pts',(-6.04449648579143,-36.020400386654,20.2102612343321));
#29071=CARTESIAN_POINT('Ctrl Pts',(-6.07434779422287,-36.1361166848333,
20.2044493855764));
#29072=CARTESIAN_POINT('Ctrl Pts',(-6.1092609440807,-36.2504437517881,20.1986375368208));
#29073=CARTESIAN_POINT('Ctrl Pts',(-6.14906762696214,-36.3629177738547,
20.1928256880652));
#29074=CARTESIAN_POINT('Ctrl Pts',(-6.18890045518272,-36.4754656697343,
20.1870100220421));
#29075=CARTESIAN_POINT('Ctrl Pts',(-6.23363306476521,-36.5861577191303,
20.1811943560189));
#29076=CARTESIAN_POINT('Ctrl Pts',(-6.28304959839844,-36.6945514781304,
20.1753786899958));
#29077=CARTESIAN_POINT('Ctrl Pts',(-6.33253691615743,-36.8031005000943,
20.1695546936265));
#29078=CARTESIAN_POINT('Ctrl Pts',(-6.38672136438866,-36.9093442984082,
20.1637306972571));
#29079=CARTESIAN_POINT('Ctrl Pts',(-6.44534184579712,-37.012866216806,20.1579067008877));
#29080=CARTESIAN_POINT('Ctrl Pts',(-6.46089433286163,-37.0403314176725,
20.1563615476235));
#29081=CARTESIAN_POINT('Ctrl Pts',(-6.47675883432838,-37.067605196216,20.1548163943593));
#29082=CARTESIAN_POINT('Ctrl Pts',(-6.49292998448124,-37.0946801441388,
20.1532712410951));
#29083=CARTESIAN_POINT('Ctrl Pts',(-6.553878124316,-37.1967240740028,20.1474476468347));
#29084=CARTESIAN_POINT('Ctrl Pts',(-6.6193819464649,-37.2962702709819,20.1416240525744));
#29085=CARTESIAN_POINT('Ctrl Pts',(-6.6892109379969,-37.3928854521102,20.135800458314));
#29086=CARTESIAN_POINT('Ctrl Pts',(-6.75895182974484,-37.4893787386442,
20.1299842113944));
#29087=CARTESIAN_POINT('Ctrl Pts',(-6.83300680024026,-37.5829480363693,
20.1241679644748));
#29088=CARTESIAN_POINT('Ctrl Pts',(-6.91110027968808,-37.6731860238032,
20.1183517175552));
#29089=CARTESIAN_POINT('Ctrl Pts',(-6.9891155869673,-37.7633336823235,20.1125412927432));
#29090=CARTESIAN_POINT('Ctrl Pts',(-7.0711610953141,-37.8501563574677,20.1067308679311));
#29091=CARTESIAN_POINT('Ctrl Pts',(-7.15691927225585,-37.9332775142372,
20.1009204431191));
#29092=CARTESIAN_POINT('Ctrl Pts',(-7.24592356174802,-38.019544967253,20.094890082511));
#29093=CARTESIAN_POINT('Ctrl Pts',(-7.33892687397448,-38.1018247827203,
20.088859721903));
#29094=CARTESIAN_POINT('Ctrl Pts',(-7.43552969293042,-38.1797353732911,
20.082829361295));
#29095=CARTESIAN_POINT('Ctrl Pts',(-7.52850450245271,-38.2547199585896,
20.0770254765332));
#29096=CARTESIAN_POINT('Ctrl Pts',(-7.62481298225817,-38.3256573019792,
20.0712215917715));
#29097=CARTESIAN_POINT('Ctrl Pts',(-7.72406363516667,-38.3922468458574,
20.0654177070097));
#29098=CARTESIAN_POINT('Ctrl Pts',(-7.82329962745752,-38.4588265535903,
20.0596146795575));
#29099=CARTESIAN_POINT('Ctrl Pts',(-7.92547658957685,-38.5210595115568,
20.0538116521054));
#29100=CARTESIAN_POINT('Ctrl Pts',(-8.03017337674044,-38.578688038136,20.0480086246532));
#29101=CARTESIAN_POINT('Ctrl Pts',(-8.13487940727622,-38.6363216525688,
20.0422050848687));
#29102=CARTESIAN_POINT('Ctrl Pts',(-8.24210534743277,-38.6893498304572,
20.0364015450843));
#29103=CARTESIAN_POINT('Ctrl Pts',(-8.35140532536104,-38.7375607819475,
20.0305980052998));
#29104=CARTESIAN_POINT('Ctrl Pts',(-8.46074074771617,-38.7857873675631,
20.0247925835101));
#29105=CARTESIAN_POINT('Ctrl Pts',(-8.57215117204004,-38.8291934552923,
20.0189871617203));
#29106=CARTESIAN_POINT('Ctrl Pts',(-8.68517123033586,-38.8676155841117,
20.0131817399305));
#29107=CARTESIAN_POINT('Ctrl Pts',(-8.79831644740283,-38.9060802617184,
20.0073698891982));
#29108=CARTESIAN_POINT('Ctrl Pts',(-8.91307446965551,-38.9395498320075,
20.0015580384659));
#29109=CARTESIAN_POINT('Ctrl Pts',(-9.02896511595014,-38.9679108172889,
19.9957461877336));
#29110=CARTESIAN_POINT('Ctrl Pts',(-9.14493187956705,-38.9962904301501,
19.9899305197604));
#29111=CARTESIAN_POINT('Ctrl Pts',(-9.26203234915435,-39.0195546963855,
19.9841148517872));
#29112=CARTESIAN_POINT('Ctrl Pts',(-9.37977815200525,-39.0376416209552,
19.978299183814));
#29113=CARTESIAN_POINT('Ctrl Pts',(-9.49769261252338,-39.0557544530175,
19.9724751855482));
#29114=CARTESIAN_POINT('Ctrl Pts',(-9.61625384679987,-39.0686750974766,
19.9666511872824));
#29115=CARTESIAN_POINT('Ctrl Pts',(-9.7349702512338,-39.0763935325566,19.9608271890166));
#29116=CARTESIAN_POINT('Ctrl Pts',(-9.76646625873928,-39.0784412688435,
19.9592820555199));
#29117=CARTESIAN_POINT('Ctrl Pts',(-9.79797320079258,-39.0801231238753,
19.9577369220233));
#29118=CARTESIAN_POINT('Ctrl Pts',(-9.82948194037072,-39.0814395244007,
19.9561917885266));
#29119=CARTESIAN_POINT('Ctrl Pts',(-9.94823818709877,-39.0864010299283,
19.9503681898295));
#29120=CARTESIAN_POINT('Ctrl Pts',(-10.0674026593695,-39.0861831193878,
19.9445445911324));
#29121=CARTESIAN_POINT('Ctrl Pts',(-10.1864866122855,-39.0807410777257,
19.9387209924352));
#29122=CARTESIAN_POINT('Ctrl Pts',(-10.3054203237308,-39.0753059019791,
19.9329047410423));
#29123=CARTESIAN_POINT('Ctrl Pts',(-10.4242733135602,-39.0646597229128,
19.9270884896494));
#29124=CARTESIAN_POINT('Ctrl Pts',(-10.5425538518512,-39.0488097408796,
19.9212722382566));
#29125=CARTESIAN_POINT('Ctrl Pts',(-10.6607159911385,-39.0329756247032,
19.9154618089404));
#29126=CARTESIAN_POINT('Ctrl Pts',(-10.7783064164573,-39.0119481221722,
19.9096513796243));
#29127=CARTESIAN_POINT('Ctrl Pts',(-10.894836144462,-38.9857864060389,19.9038409503081));
#29128=CARTESIAN_POINT('Ctrl Pts',(-11.0157766202502,-38.9586344470429,
19.8978105913769));
#29129=CARTESIAN_POINT('Ctrl Pts',(-11.1355740679262,-38.9259519471033,
19.8917802324456));
#29130=CARTESIAN_POINT('Ctrl Pts',(-11.2536903398068,-38.8878638777451,
19.8857498735144));
#29131=CARTESIAN_POINT('Ctrl Pts',(-11.3673707651204,-38.8512062025995,
19.879945984201));
#29132=CARTESIAN_POINT('Ctrl Pts',(-11.4794935867999,-38.8095417843649,
19.8741420948877));
#29133=CARTESIAN_POINT('Ctrl Pts',(-11.5895928221178,-38.7630333057085,
19.8683382055744));
#29134=CARTESIAN_POINT('Ctrl Pts',(-11.6996757945346,-38.7165316968799,
19.8625351735611));
#29135=CARTESIAN_POINT('Ctrl Pts',(-11.8077353989698,-38.6651876094302,
19.8567321415478));
#29136=CARTESIAN_POINT('Ctrl Pts',(-11.9133252612175,-38.6092120254686,
19.8509291095345));
#29137=CARTESIAN_POINT('Ctrl Pts',(-12.0189244457598,-38.5532314995468,
19.8451255651843));
#29138=CARTESIAN_POINT('Ctrl Pts',(-12.1220530937882,-38.4926188553773,
19.8393220208342));
#29139=CARTESIAN_POINT('Ctrl Pts',(-12.2222896591848,-38.42763091226,19.8335184764841));
#29140=CARTESIAN_POINT('Ctrl Pts',(-12.3225587298375,-38.3626218945006,
19.8277130501292));
#29141=CARTESIAN_POINT('Ctrl Pts',(-12.4199335102169,-38.2932349780552,
19.8219076237743));
#29142=CARTESIAN_POINT('Ctrl Pts',(-12.5140221879713,-38.2197697803396,
19.8161021974194));
#29143=CARTESIAN_POINT('Ctrl Pts',(-12.6082150593581,-38.1462232273962,
19.8102903421458));
#29144=CARTESIAN_POINT('Ctrl Pts',(-12.6991142422774,-38.0685896297487,
19.8044784868722));
#29145=CARTESIAN_POINT('Ctrl Pts',(-12.7863616089684,-37.9872083931436,
19.7986666315986));
#29146=CARTESIAN_POINT('Ctrl Pts',(-12.8736662798165,-37.9057737052613,
19.7928509590927));
#29147=CARTESIAN_POINT('Ctrl Pts',(-12.9573140722942,-37.8205867670632,
19.7870352865868));
#29148=CARTESIAN_POINT('Ctrl Pts',(-13.0369854269177,-37.7320220564061,
19.7812196140809));
#29149=CARTESIAN_POINT('Ctrl Pts',(-13.1167709010918,-37.6433304875448,
19.7753956113296));
#29150=CARTESIAN_POINT('Ctrl Pts',(-13.1925683103788,-37.5512518034839,
19.7695716085784));
#29151=CARTESIAN_POINT('Ctrl Pts',(-13.2640997931654,-37.4561916741691,
19.7637476058271));
#29152=CARTESIAN_POINT('Ctrl Pts',(-13.2830768747935,-37.4309725152294,
19.7622025158708));
#29153=CARTESIAN_POINT('Ctrl Pts',(-13.3017539546748,-37.405543660053,19.7606574259145));
#29154=CARTESIAN_POINT('Ctrl Pts',(-13.3201263815374,-37.3799129838335,
19.7591123359582));
#29155=CARTESIAN_POINT('Ctrl Pts',(-13.3898878294926,-37.2825914324391,
19.7532455164367));
#29156=CARTESIAN_POINT('Ctrl Pts',(-13.4554778697672,-37.1820448960581,
19.7473786969153));
#29157=CARTESIAN_POINT('Ctrl Pts',(-13.5165873062648,-37.0786627233433,
19.7415118773939));
#29158=CARTESIAN_POINT('Ctrl Pts',(-13.5776176346634,-36.975414382122,19.7356526526559));
#29159=CARTESIAN_POINT('Ctrl Pts',(-13.6341786944696,-36.8693380470425,
19.729793427918));
#29160=CARTESIAN_POINT('Ctrl Pts',(-13.6860029550964,-36.7608541152011,
19.72393420318));
#29161=CARTESIAN_POINT('Ctrl Pts',(-13.7377717268428,-36.6524863384548,
19.7180812519869));
#29162=CARTESIAN_POINT('Ctrl Pts',(-13.7848136180123,-36.5417164522241,
19.7122283007938));
#29163=CARTESIAN_POINT('Ctrl Pts',(-13.8269059431142,-36.4289912185024,
19.7063753496006));
#29164=CARTESIAN_POINT('Ctrl Pts',(-13.8694507206623,-36.3150542957704,
19.700459484751));
#29165=CARTESIAN_POINT('Ctrl Pts',(-13.9069386754605,-36.1991200917361,
19.6945436199013));
#29166=CARTESIAN_POINT('Ctrl Pts',(-13.9391887252632,-36.0816733271922,
19.6886277550516));
#29167=CARTESIAN_POINT('Ctrl Pts',(-13.9710477424299,-35.9656506075172,
19.6827836202067));
#29168=CARTESIAN_POINT('Ctrl Pts',(-13.9977950643991,-35.8481522013055,
19.6769394853618));
#29169=CARTESIAN_POINT('Ctrl Pts',(-14.0193056312597,-35.7296624168231,
19.671095350517));
#29170=CARTESIAN_POINT('Ctrl Pts',(-14.041212224163,-35.6089911444811,19.6651436206649));
#29171=CARTESIAN_POINT('Ctrl Pts',(-14.0576872017008,-35.4872920340612,
19.6591918908128));
#29172=CARTESIAN_POINT('Ctrl Pts',(-14.0686527751091,-35.3650884763954,
19.6532401609607));
#29173=CARTESIAN_POINT('Ctrl Pts',(-14.0796183485174,-35.2428849187295,
19.6472884311087));
#29174=CARTESIAN_POINT('Ctrl Pts',(-14.0850744735076,-35.1201773507321,
19.6413367012566));
#29175=CARTESIAN_POINT('Ctrl Pts',(-14.0849992317308,-34.9974946540251,
19.6353849714045));
#29176=CARTESIAN_POINT('Ctrl Pts',(-14.0849992317303,-34.9974946531383,
19.6353849713615));
#29177=CARTESIAN_POINT('Ctrl Pts',(-14.0849166368598,-34.862822689068,19.6288516038181));
#29178=CARTESIAN_POINT('Ctrl Pts',(-14.0781702967129,-34.7283970591762,
19.6223182362747));
#29179=CARTESIAN_POINT('Ctrl Pts',(-14.0648574522931,-34.5948347342912,
19.6157848687313));
#29180=CARTESIAN_POINT('Ctrl Pts',(-14.051492035593,-34.4607449732116,19.6092257009893));
#29181=CARTESIAN_POINT('Ctrl Pts',(-14.0315082632746,-34.3275255447684,
19.6026665332472));
#29182=CARTESIAN_POINT('Ctrl Pts',(-14.0050544114292,-34.1957835108058,
19.5961073655052));
#29183=CARTESIAN_POINT('Ctrl Pts',(-13.9784604821396,-34.063343881366,19.5895134659041));
#29184=CARTESIAN_POINT('Ctrl Pts',(-13.945327873669,-33.9323975267073,19.582919566303));
#29185=CARTESIAN_POINT('Ctrl Pts',(-13.9058559311413,-33.8035408719191,
19.576325666702));
#29186=CARTESIAN_POINT('Ctrl Pts',(-13.8773364431503,-33.7104386432608,
19.5715614055979));
#29187=CARTESIAN_POINT('Ctrl Pts',(-13.8455085702689,-33.6184269108994,
19.5667971444938));
#29188=CARTESIAN_POINT('Ctrl Pts',(-13.81046272572,-33.5277232543104,19.5620328833897));
#29189=CARTESIAN_POINT('Ctrl Pts',(-13.767624377055,-33.4168514828874,19.5562092805936));
#29190=CARTESIAN_POINT('Ctrl Pts',(-13.7198739334846,-33.3076721551263,
19.5503856777975));
#29191=CARTESIAN_POINT('Ctrl Pts',(-13.6673654194799,-33.200651262261,19.5445620750014));
#29192=CARTESIAN_POINT('Ctrl Pts',(-13.6149231534501,-33.0937653935446,
19.5387458196211));
#29193=CARTESIAN_POINT('Ctrl Pts',(-13.5577349352383,-32.9890329066717,
19.5329295642409));
#29194=CARTESIAN_POINT('Ctrl Pts',(-13.4960035835794,-32.8869018140181,
19.5271133088607));
#29195=CARTESIAN_POINT('Ctrl Pts',(-13.4343340262757,-32.784872956693,19.521302875672));
#29196=CARTESIAN_POINT('Ctrl Pts',(-13.3681305927617,-32.6854406606044,
19.5154924424833));
#29197=CARTESIAN_POINT('Ctrl Pts',(-13.2976426612025,-32.589029681017,19.5096820092946));
#29198=CARTESIAN_POINT('Ctrl Pts',(-13.2244867693012,-32.4889695566128,
19.5036516518582));
#29199=CARTESIAN_POINT('Ctrl Pts',(-13.1467158332367,-32.3921643828436,
19.4976212944218));
#29200=CARTESIAN_POINT('Ctrl Pts',(-13.064659181786,-32.2990577385855,19.4915909369854));
#29201=CARTESIAN_POINT('Ctrl Pts',(-12.9856840928256,-32.2094476291906,
19.4857870441068));
#29202=CARTESIAN_POINT('Ctrl Pts',(-12.9027396703876,-32.1232636027136,
19.4799831512281));
#29203=CARTESIAN_POINT('Ctrl Pts',(-12.8161610266563,-32.0408680205266,
19.4741792583494));
#29204=CARTESIAN_POINT('Ctrl Pts',(-12.7295951733336,-31.9584846107775,
19.4683762228896));
#29205=CARTESIAN_POINT('Ctrl Pts',(-12.6393964621359,-31.8798888137317,
19.4625731874298));
#29206=CARTESIAN_POINT('Ctrl Pts',(-12.5459364683641,-31.8054057379608,
19.45677015197));
#29207=CARTESIAN_POINT('Ctrl Pts',(-12.4524682251862,-31.7309160878139,
19.4509666042954));
#29208=CARTESIAN_POINT('Ctrl Pts',(-12.3557384464404,-31.6605401352099,
19.4451630566208));
#29209=CARTESIAN_POINT('Ctrl Pts',(-12.2561508300465,-31.5945619324263,
19.4393595089461));
#29210=CARTESIAN_POINT('Ctrl Pts',(-12.156530921008,-31.5285623353094,19.4335540793919));
#29211=CARTESIAN_POINT('Ctrl Pts',(-12.0540516715701,-31.4669635494739,
19.4277486498377));
#29212=CARTESIAN_POINT('Ctrl Pts',(-11.9491441581158,-31.4100052853962,
19.4219432202834));
#29213=CARTESIAN_POINT('Ctrl Pts',(-11.8441204739503,-31.3529839478376,
19.4161313620106));
#29214=CARTESIAN_POINT('Ctrl Pts',(-11.7366635174216,-31.3006135843589,
19.4103195037378));
#29215=CARTESIAN_POINT('Ctrl Pts',(-11.6272274070774,-31.2530871419719,
19.404507645465));
#29216=CARTESIAN_POINT('Ctrl Pts',(-11.5177194211509,-31.20552948511,19.3986919700729));
#29217=CARTESIAN_POINT('Ctrl Pts',(-11.4062300731225,-31.1628222309038,
19.3928762946807));
#29218=CARTESIAN_POINT('Ctrl Pts',(-11.2932302505084,-31.1251089668005,
19.3870606192885));
#29219=CARTESIAN_POINT('Ctrl Pts',(-11.1800685730566,-31.0873416842563,
19.3812366138372));
#29220=CARTESIAN_POINT('Ctrl Pts',(-11.0653924939827,-31.0545827808194,
19.375412608386));
#29221=CARTESIAN_POINT('Ctrl Pts',(-10.9496848632193,-31.0269251629786,
19.3695886029348));
#29222=CARTESIAN_POINT('Ctrl Pts',(-10.9189886474781,-31.0195878404656,
19.3680435455636));
#29223=CARTESIAN_POINT('Ctrl Pts',(-10.8882198672476,-31.0126092612386,
19.3664984881925));
#29224=CARTESIAN_POINT('Ctrl Pts',(-10.8573875990132,-31.0059905477004,
19.3649534308213));
#29225=CARTESIAN_POINT('Ctrl Pts',(-10.7411646752692,-30.9810411591901,
19.3591293025521));
#29226=CARTESIAN_POINT('Ctrl Pts',(-10.62366441418,-30.9611287597988,19.3533051742829));
#29227=CARTESIAN_POINT('Ctrl Pts',(-10.5053611158976,-30.9463799952957,
19.3474810460137));
#29228=CARTESIAN_POINT('Ctrl Pts',(-10.3872094763206,-30.9316501379454,
19.3416643839755));
#29229=CARTESIAN_POINT('Ctrl Pts',(-10.2682572490579,-30.9220707984628,
19.3358477219373));
#29230=CARTESIAN_POINT('Ctrl Pts',(-10.148990417942,-30.9177179353502,19.3300310598991));
#29231=CARTESIAN_POINT('Ctrl Pts',(-10.0298630331131,-30.9133701615872,
19.3242211986782));
#29232=CARTESIAN_POINT('Ctrl Pts',(-9.91042218245955,-30.9142367134684,
19.3184113374573));
#29233=CARTESIAN_POINT('Ctrl Pts',(-9.79115967193203,-30.9203418381717,
19.3126014762363));
#29234=CARTESIAN_POINT('Ctrl Pts',(-9.67197562219243,-30.9264429464167,
19.3067954372248));
#29235=CARTESIAN_POINT('Ctrl Pts',(-9.55297008553151,-30.9377757534022,
19.3009893982133));
#29236=CARTESIAN_POINT('Ctrl Pts',(-9.43463534023889,-30.954312443911,19.2951833592017));
#29237=CARTESIAN_POINT('Ctrl Pts',(-9.3163505181675,-30.9708421578986,19.2893797696497));
#29238=CARTESIAN_POINT('Ctrl Pts',(-9.19873632821924,-30.992571331977,19.2835761800977));
#29239=CARTESIAN_POINT('Ctrl Pts',(-9.08227975844286,-31.0194203238427,
19.2777725905457));
#29240=CARTESIAN_POINT('Ctrl Pts',(-8.9658448366947,-31.0462643247686,19.2719700798188));
#29241=CARTESIAN_POINT('Ctrl Pts',(-8.85056750435854,-31.0782261572829,
19.2661675690919));
#29242=CARTESIAN_POINT('Ctrl Pts',(-8.73692375970745,-31.115175240605,19.260365058365));
#29243=CARTESIAN_POINT('Ctrl Pts',(-8.62322686242791,-31.1521416054845,
19.2545598337299));
#29244=CARTESIAN_POINT('Ctrl Pts',(-8.51116546951101,-31.1940997595864,
19.2487546090947));
#29245=CARTESIAN_POINT('Ctrl Pts',(-8.40119959948887,-31.2408694782802,
19.2429493844596));
#29246=CARTESIAN_POINT('Ctrl Pts',(-8.29121022613133,-31.2876491932063,
19.2371429190563));
#29247=CARTESIAN_POINT('Ctrl Pts',(-8.18331763951256,-31.3392423514837,
19.2313364536531));
#29248=CARTESIAN_POINT('Ctrl Pts',(-8.07795982296281,-31.3954214451819,
19.2255299882498));
#29249=CARTESIAN_POINT('Ctrl Pts',(-7.97248668849355,-31.4516620289186,
19.2197171674614));
#29250=CARTESIAN_POINT('Ctrl Pts',(-7.86955422295094,-31.5124983750139,
19.2139043466729));
#29251=CARTESIAN_POINT('Ctrl Pts',(-7.76957409372478,-31.5776579252482,
19.2080915258845));
#29252=CARTESIAN_POINT('Ctrl Pts',(-7.68162090265582,-31.6349792191501,
19.2029779484025));
#29253=CARTESIAN_POINT('Ctrl Pts',(-7.59595220320821,-31.6956454061462,
19.1978643709205));
#29254=CARTESIAN_POINT('Ctrl Pts',(-7.5128274573098,-31.7594448403263,19.1927507934385));
#29255=CARTESIAN_POINT('',(-14.0849997388207,-35.001460765222,19.7396150285601));
#29256=CARTESIAN_POINT('Ctrl Pts',(-14.0849997388207,-35.0014607652219,
19.7396150285601));
#29257=CARTESIAN_POINT('Ctrl Pts',(-14.0850418772244,-34.8836215905298,
19.7338448932755));
#29258=CARTESIAN_POINT('Ctrl Pts',(-14.0799808576064,-34.7655803559852,
19.7280747579908));
#29259=CARTESIAN_POINT('Ctrl Pts',(-14.0697904347131,-34.6478199075505,
19.7223046227062));
#29260=CARTESIAN_POINT('Ctrl Pts',(-14.059612412446,-34.530202760656,19.7165415090428));
#29261=CARTESIAN_POINT('Ctrl Pts',(-14.0443174331435,-34.4128661318137,
19.7107783953795));
#29262=CARTESIAN_POINT('Ctrl Pts',(-14.0239312542375,-34.2962939099519,
19.7050152817162));
#29263=CARTESIAN_POINT('Ctrl Pts',(-14.0035643214882,-34.179831741439,19.6992576088855));
#29264=CARTESIAN_POINT('Ctrl Pts',(-13.9781158193059,-34.0641329527669,
19.6934999360549));
#29265=CARTESIAN_POINT('Ctrl Pts',(-13.9476633382702,-33.9496766366128,
19.6877422632243));
#29266=CARTESIAN_POINT('Ctrl Pts',(-13.917229973243,-33.8352921683947,19.6819882046713));
#29267=CARTESIAN_POINT('Ctrl Pts',(-13.8817989824691,-33.7221490230879,
19.6762341461184));
#29268=CARTESIAN_POINT('Ctrl Pts',(-13.8414989710686,-33.6107157759194,
19.6704800875654));
#29269=CARTESIAN_POINT('Ctrl Pts',(-13.8012118048751,-33.4993180469328,
19.6647278630584));
#29270=CARTESIAN_POINT('Ctrl Pts',(-13.7560588442483,-33.3896295240911,
19.6589756385515));
#29271=CARTESIAN_POINT('Ctrl Pts',(-13.7062182517548,-33.2821026601221,
19.6532234140445));
#29272=CARTESIAN_POINT('Ctrl Pts',(-13.6563812419505,-33.1745835255022,
19.6474716030244));
#29273=CARTESIAN_POINT('Ctrl Pts',(-13.6018574456382,-33.0692261185813,
19.6417197920044));
#29274=CARTESIAN_POINT('Ctrl Pts',(-13.5428724621768,-32.9664612822105,
19.6359679809843));
#29275=CARTESIAN_POINT('Ctrl Pts',(-13.4838771573901,-32.8636784638169,
19.6302151634994));
#29276=CARTESIAN_POINT('Ctrl Pts',(-13.4204193215166,-32.7634894786887,
19.6244623460145));
#29277=CARTESIAN_POINT('Ctrl Pts',(-13.3527692482539,-32.6662983549813,
19.6187095285296));
#29278=CARTESIAN_POINT('Ctrl Pts',(-13.2850503479888,-32.5690083492862,
19.6129508581436));
#29279=CARTESIAN_POINT('Ctrl Pts',(-13.2131309321623,-32.47472263748,19.6071921877577));
#29280=CARTESIAN_POINT('Ctrl Pts',(-13.1373232306751,-32.3838142370492,
19.6014335173717));
#29281=CARTESIAN_POINT('Ctrl Pts',(-13.0614743849762,-32.2928564965856,
19.5956717214992));
#29282=CARTESIAN_POINT('Ctrl Pts',(-12.9817333318425,-32.205280024942,19.5899099256267));
#29283=CARTESIAN_POINT('Ctrl Pts',(-12.8984497562577,-32.1214215295654,
19.5841481297542));
#29284=CARTESIAN_POINT('Ctrl Pts',(-12.8150375631549,-32.0374335288036,
19.578377435754));
#29285=CARTESIAN_POINT('Ctrl Pts',(-12.7280722279227,-31.957175253068,19.5726067417539));
#29286=CARTESIAN_POINT('Ctrl Pts',(-12.6379373769759,-31.8809438294328,
19.5668360477537));
#29287=CARTESIAN_POINT('Ctrl Pts',(-12.5752148457861,-31.827896336744,19.5628203697933));
#29288=CARTESIAN_POINT('Ctrl Pts',(-12.5109581856905,-31.7767979505961,
19.5588046918329));
#29289=CARTESIAN_POINT('Ctrl Pts',(-12.4453045397188,-31.7277361493867,
19.5547890138725));
#29290=CARTESIAN_POINT('Ctrl Pts',(-12.3500926002635,-31.6565859615001,
19.5489654151801));
#29291=CARTESIAN_POINT('Ctrl Pts',(-12.2516191999004,-31.5894800129192,
19.5431418164876));
#29292=CARTESIAN_POINT('Ctrl Pts',(-12.1502624676698,-31.526731176524,19.5373182177951));
#29293=CARTESIAN_POINT('Ctrl Pts',(-12.0490336114812,-31.4640615067777,
19.5315019664069));
#29294=CARTESIAN_POINT('Ctrl Pts',(-11.9449290029249,-31.4057382286165,
19.5256857150186));
#29295=CARTESIAN_POINT('Ctrl Pts',(-11.8383585485305,-31.3520330529122,
19.5198694636304));
#29296=CARTESIAN_POINT('Ctrl Pts',(-11.7318947713275,-31.2983816361728,
19.5140590343189));
#29297=CARTESIAN_POINT('Ctrl Pts',(-11.6229704212492,-31.2493393082513,
19.5082486050074));
#29298=CARTESIAN_POINT('Ctrl Pts',(-11.5120224840164,-31.2051333346442,
19.5024381756959));
#29299=CARTESIAN_POINT('Ctrl Pts',(-11.3968750743293,-31.1592541278692,
19.4964078167629));
#29300=CARTESIAN_POINT('Ctrl Pts',(-11.2795482429684,-31.1185848652021,
19.4903774578299));
#29301=CARTESIAN_POINT('Ctrl Pts',(-11.1605567056453,-31.0833262667179,
19.4843470988969));
#29302=CARTESIAN_POINT('Ctrl Pts',(-11.0460338855338,-31.0493918019448,
19.4785432095883));
#29303=CARTESIAN_POINT('Ctrl Pts',(-10.92996956717,-31.0204690622736,19.4727393202796));
#29304=CARTESIAN_POINT('Ctrl Pts',(-10.8128401996152,-30.9966868958462,
19.4669354309709));
#29305=CARTESIAN_POINT('Ctrl Pts',(-10.6957281333917,-30.9729082423135,
19.4611323989623));
#29306=CARTESIAN_POINT('Ctrl Pts',(-10.5775517308993,-30.9542687332049,
19.4553293669537));
#29307=CARTESIAN_POINT('Ctrl Pts',(-10.4587985297507,-30.9408462816618,
19.4495263349451));
#29308=CARTESIAN_POINT('Ctrl Pts',(-10.3400348441456,-30.9274226450803,
19.4437227905996));
#29309=CARTESIAN_POINT('Ctrl Pts',(-10.220694664407,-30.9192170277171,19.4379192462542));
#29310=CARTESIAN_POINT('Ctrl Pts',(-10.1012709185177,-30.9162554926804,
19.4321157019087));
#29311=CARTESIAN_POINT('Ctrl Pts',(-9.98180844524824,-30.9132929972612,
19.4263102755585));
#29312=CARTESIAN_POINT('Ctrl Pts',(-9.86226275993423,-30.9155779763552,
19.4205048492082));
#29313=CARTESIAN_POINT('Ctrl Pts',(-9.74312641610772,-30.9230843813125,
19.4146994228579));
#29314=CARTESIAN_POINT('Ctrl Pts',(-9.62385814090777,-30.9305990988491,
19.4088875675889));
#29315=CARTESIAN_POINT('Ctrl Pts',(-9.50500051979866,-30.9433467583186,
19.4030757123199));
#29316=CARTESIAN_POINT('Ctrl Pts',(-9.38704077165203,-30.9612494525679,
19.3972638570509));
#29317=CARTESIAN_POINT('Ctrl Pts',(-9.26900354742514,-30.9791639053247,
19.3914481845496));
#29318=CARTESIAN_POINT('Ctrl Pts',(-9.15186577032583,-31.0022400570877,
19.3856325120482));
#29319=CARTESIAN_POINT('Ctrl Pts',(-9.0361026309011,-31.030349277097,19.3798168395469));
#29320=CARTESIAN_POINT('Ctrl Pts',(-8.92017367482114,-31.0584987601543,
19.3739928368001));
#29321=CARTESIAN_POINT('Ctrl Pts',(-8.80562367724287,-31.091695587492,19.3681688340534));
#29322=CARTESIAN_POINT('Ctrl Pts',(-8.69291102659217,-31.1297618399386,
19.3623448313066));
#29323=CARTESIAN_POINT('Ctrl Pts',(-8.66300870733518,-31.1398606995342,
19.3607997413058));
#29324=CARTESIAN_POINT('Ctrl Pts',(-8.63323558515604,-31.1503020232743,
19.3592546513049));
#29325=CARTESIAN_POINT('Ctrl Pts',(-8.60359994560332,-31.1610819378266,
19.3577095613041));
#29326=CARTESIAN_POINT('Ctrl Pts',(-8.49191615464733,-31.2017067308648,
19.3518867914478));
#29327=CARTESIAN_POINT('Ctrl Pts',(-8.38182657333516,-31.2472748149992,
19.3460640215914));
#29328=CARTESIAN_POINT('Ctrl Pts',(-8.27379995922212,-31.2976415058481,
19.3402412517351));
#29329=CARTESIAN_POINT('Ctrl Pts',(-8.16589302622355,-31.3479523961729,
19.3344249328408));
#29330=CARTESIAN_POINT('Ctrl Pts',(-8.06004488446533,-31.4030511558678,
19.3286086139465));
#29331=CARTESIAN_POINT('Ctrl Pts',(-7.95670750152521,-31.4627438931176,
19.3227922950522));
#29332=CARTESIAN_POINT('Ctrl Pts',(-7.85348150489727,-31.5223722881742,
19.3169822455088));
#29333=CARTESIAN_POINT('Ctrl Pts',(-7.75276123275879,-31.5865846031199,
19.3111721959653));
#29334=CARTESIAN_POINT('Ctrl Pts',(-7.65497622498272,-31.6551399887882,
19.3053621464219));
#29335=CARTESIAN_POINT('Ctrl Pts',(-7.60686687164105,-31.6888686282556,
19.3025036537677));
#29336=CARTESIAN_POINT('Ctrl Pts',(-7.55946765824416,-31.7236478174602,
19.2996451611135));
#29337=CARTESIAN_POINT('Ctrl Pts',(-7.51282745730977,-31.7594448403263,
19.2967866684593));
#29338=CARTESIAN_POINT('Ctrl Pts',(-7.51282745730979,-31.7594448403263,
20.5469196554144));
#29339=CARTESIAN_POINT('Ctrl Pts',(-7.47644412383199,-31.7873695703737,
20.5446751958479));
#29340=CARTESIAN_POINT('Ctrl Pts',(-7.44055213223825,-31.8158910003058,
20.5424307362813));
#29341=CARTESIAN_POINT('Ctrl Pts',(-7.40517161094806,-31.8449895988491,
20.5401862767148));
#29342=CARTESIAN_POINT('Ctrl Pts',(-7.31337143933769,-31.9204903614861,
20.534362683227));
#29343=CARTESIAN_POINT('Ctrl Pts',(-7.22472119483735,-32.0001228138231,
20.5285390897392));
#29344=CARTESIAN_POINT('Ctrl Pts',(-7.13961488664204,-32.0835943349252,
20.5227154962513));
#29345=CARTESIAN_POINT('Ctrl Pts',(-7.05461595269594,-32.1669605443049,
20.5168992500917));
#29346=CARTESIAN_POINT('Ctrl Pts',(-6.97315235089349,-32.2541559053276,
20.5110830039321));
#29347=CARTESIAN_POINT('Ctrl Pts',(-6.89558569267423,-32.3448471214502,
20.5052667577725));
#29348=CARTESIAN_POINT('Ctrl Pts',(-6.81809667910428,-32.4354475551693,
20.4994563337071));
#29349=CARTESIAN_POINT('Ctrl Pts',(-6.74449711271978,-32.5295365738911,
20.4936459096417));
#29350=CARTESIAN_POINT('Ctrl Pts',(-6.67511189826874,-32.6267439853724,
20.4878354855764));
#29351=CARTESIAN_POINT('Ctrl Pts',(-6.60310030684887,-32.7276309027648,
20.4818051246834));
#29352=CARTESIAN_POINT('Ctrl Pts',(-6.53562873542885,-32.8318766390586,
20.4757747637905));
#29353=CARTESIAN_POINT('Ctrl Pts',(-6.47301484396659,-32.9390291828558,
20.4697444028976));
#29354=CARTESIAN_POINT('Ctrl Pts',(-6.41275248611149,-33.0421574949379,
20.4639405188451));
#29355=CARTESIAN_POINT('Ctrl Pts',(-6.35698974170198,-33.1479778309798,
20.4581366347925));
#29356=CARTESIAN_POINT('Ctrl Pts',(-6.30596534631192,-33.2560582070059,
20.45233275074));
#29357=CARTESIAN_POINT('Ctrl Pts',(-6.25494848776096,-33.3641226184252,
20.4465297239821));
#29358=CARTESIAN_POINT('Ctrl Pts',(-6.20866876061912,-33.4744460367868,
20.4407266972242));
#29359=CARTESIAN_POINT('Ctrl Pts',(-6.16731807849836,-33.5865735644914,
20.4349236704663));
#29360=CARTESIAN_POINT('Ctrl Pts',(-6.12596374553521,-33.6987109919102,
20.4291201313605));
#29361=CARTESIAN_POINT('Ctrl Pts',(-6.0895394641378,-33.8126524622339,20.4233165922547));
#29362=CARTESIAN_POINT('Ctrl Pts',(-6.05818807864224,-33.9279254799027,
20.4175130531489));
#29363=CARTESIAN_POINT('Ctrl Pts',(-6.02682652624944,-34.0432358792983,
20.4117076320214));
#29364=CARTESIAN_POINT('Ctrl Pts',(-6.00054124856552,-34.1598782909817,
20.405902210894));
#29365=CARTESIAN_POINT('Ctrl Pts',(-5.97942439191471,-34.2773681575867,
20.4000967897665));
#29366=CARTESIAN_POINT('Ctrl Pts',(-5.95828415028766,-34.3949881334113,
20.3942849396692));
#29367=CARTESIAN_POINT('Ctrl Pts',(-5.94232382666853,-34.5134570353053,
20.3884730895719));
#29368=CARTESIAN_POINT('Ctrl Pts',(-5.93158393261422,-34.6322831216313,
20.3826612394745));
#29369=CARTESIAN_POINT('Ctrl Pts',(-5.92083698453664,-34.7511872536041,
20.3768455721211));
#29370=CARTESIAN_POINT('Ctrl Pts',(-5.91531731341602,-34.8704486302597,
20.3710299047677));
#29371=CARTESIAN_POINT('Ctrl Pts',(-5.91501330217641,-34.9895750969147,
20.3652142374143));
#29372=CARTESIAN_POINT('Ctrl Pts',(-5.91470885547333,-35.1088721994499,
20.3593902397415));
#29373=CARTESIAN_POINT('Ctrl Pts',(-5.91963496330141,-35.2280335997395,
20.3535662420687));
#29374=CARTESIAN_POINT('Ctrl Pts',(-5.92972813549782,-35.3465717083692,
20.3477422443959));
#29375=CARTESIAN_POINT('Ctrl Pts',(-5.93240591213912,-35.3780205504394,
20.3461971043127));
#29376=CARTESIAN_POINT('Ctrl Pts',(-5.93544710454838,-35.4094255757416,
20.3446519642295));
#29377=CARTESIAN_POINT('Ctrl Pts',(-5.93884992651983,-35.4407778132711,
20.3431068241463));
#29378=CARTESIAN_POINT('Ctrl Pts',(-5.95167507597797,-35.5589435990619,
20.3372832304741));
#29379=CARTESIAN_POINT('Ctrl Pts',(-5.96968252705702,-35.6767397184615,
20.3314596368018));
#29380=CARTESIAN_POINT('Ctrl Pts',(-5.99284352153497,-35.7936762293881,
20.3256360431296));
#29381=CARTESIAN_POINT('Ctrl Pts',(-6.01597529497144,-35.9104652075031,
20.3198197967874));
#29382=CARTESIAN_POINT('Ctrl Pts',(-6.04424760092048,-36.0263963372128,
20.3140035504453));
#29383=CARTESIAN_POINT('Ctrl Pts',(-6.07757990198573,-36.1409844760967,
20.3081873041032));
#29384=CARTESIAN_POINT('Ctrl Pts',(-6.11087883722424,-36.2554579115889,
20.3023768798574));
#29385=CARTESIAN_POINT('Ctrl Pts',(-6.14922757782333,-36.3685906408246,
20.2965664556116));
#29386=CARTESIAN_POINT('Ctrl Pts',(-6.1924946066162,-36.4799079969219,20.2907560313658));
#29387=CARTESIAN_POINT('Ctrl Pts',(-6.23739938196257,-36.5954389452481,
20.2847256705413));
#29388=CARTESIAN_POINT('Ctrl Pts',(-6.28760204993146,-36.7090139340734,
20.2786953097168));
#29389=CARTESIAN_POINT('Ctrl Pts',(-6.34289869087207,-36.82011950563,20.2726649488923));
#29390=CARTESIAN_POINT('Ctrl Pts',(-6.39611860780277,-36.9270523895845,
20.2668610646656));
#29391=CARTESIAN_POINT('Ctrl Pts',(-6.45405658032985,-37.0316975960583,
20.261057180439));
#29392=CARTESIAN_POINT('Ctrl Pts',(-6.51648217566361,-37.1336186556015,
20.2552532962123));
#29393=CARTESIAN_POINT('Ctrl Pts',(-6.57889855005348,-37.2355246602883,
20.2494502692829));
#29394=CARTESIAN_POINT('Ctrl Pts',(-6.64580101578983,-37.3347069701451,
20.2436472423535));
#29395=CARTESIAN_POINT('Ctrl Pts',(-6.71691430969483,-37.4307557158451,
20.2378442154241));
#29396=CARTESIAN_POINT('Ctrl Pts',(-6.78803388214217,-37.5268129416207,
20.2320406761496));
#29397=CARTESIAN_POINT('Ctrl Pts',(-6.86336477893826,-37.6197357249787,
20.2262371368751));
#29398=CARTESIAN_POINT('Ctrl Pts',(-6.9425901204879,-37.709145590156,20.2204335976005));
#29399=CARTESIAN_POINT('Ctrl Pts',(-7.02184115387228,-37.7985844498878,
20.2146281763073));
#29400=CARTESIAN_POINT('Ctrl Pts',(-7.10498887301,-37.8845078203705,20.2088227550141));
#29401=CARTESIAN_POINT('Ctrl Pts',(-7.19167851935393,-37.966573016351,20.2030173337209));
#29402=CARTESIAN_POINT('Ctrl Pts',(-7.27846416642655,-38.0487290919111,
20.197205483463));
#29403=CARTESIAN_POINT('Ctrl Pts',(-7.36879927334768,-38.1270181836673,
20.1913936332051));
#29404=CARTESIAN_POINT('Ctrl Pts',(-7.46229476855321,-38.2011368540391,
20.1855817829472));
#29405=CARTESIAN_POINT('Ctrl Pts',(-7.55585167208242,-38.2753042059362,
20.1797661154361));
#29406=CARTESIAN_POINT('Ctrl Pts',(-7.65257276777595,-38.3452954425188,
20.173950447925));
#29407=CARTESIAN_POINT('Ctrl Pts',(-7.75204006358966,-38.4108504986724,
20.1681347804138));
#29408=CARTESIAN_POINT('Ctrl Pts',(-7.85164983553608,-38.4764994553469,
20.1623107825886));
#29409=CARTESIAN_POINT('Ctrl Pts',(-7.95401330969173,-38.5376993398648,
20.1564867847634));
#29410=CARTESIAN_POINT('Ctrl Pts',(-8.05868787733256,-38.5942359747775,
20.1506627869382));
#29411=CARTESIAN_POINT('Ctrl Pts',(-8.08645861221458,-38.6092354530143,
20.1491176484847));
#29412=CARTESIAN_POINT('Ctrl Pts',(-8.11439191096311,-38.6239069627225,
20.1475725100313));
#29413=CARTESIAN_POINT('Ctrl Pts',(-8.14247929138295,-38.6382470802653,
20.1460273715779));
#29414=CARTESIAN_POINT('Ctrl Pts',(-8.24834003862632,-38.6922946822824,
20.1402037771796));
#29415=CARTESIAN_POINT('Ctrl Pts',(-8.35673235688323,-38.741805317745,20.1343801827814));
#29416=CARTESIAN_POINT('Ctrl Pts',(-8.46723070838592,-38.7865344708169,
20.1285565883832));
#29417=CARTESIAN_POINT('Ctrl Pts',(-8.57758964987418,-38.8312071914463,
20.1227403413106));
#29418=CARTESIAN_POINT('Ctrl Pts',(-8.69004896458759,-38.8711102764148,
20.1169240942381));
#29419=CARTESIAN_POINT('Ctrl Pts',(-8.80415874560844,-38.9060451474983,
20.1111078471656));
#29420=CARTESIAN_POINT('Ctrl Pts',(-8.91815430215916,-38.9409450485985,
20.1052974221859));
#29421=CARTESIAN_POINT('Ctrl Pts',(-9.03379665011463,-38.9708865105447,
20.0994869972062));
#29422=CARTESIAN_POINT('Ctrl Pts',(-9.15061669875019,-38.9957193354336,
20.0936765722265));
#29423=CARTESIAN_POINT('Ctrl Pts',(-9.27185860709382,-39.0214921296951,
20.0876462116758));
#29424=CARTESIAN_POINT('Ctrl Pts',(-9.39436871862172,-39.041761734177,20.0816158511251));
#29425=CARTESIAN_POINT('Ctrl Pts',(-9.51760581090146,-39.0564172426322,
20.0755854905744));
#29426=CARTESIAN_POINT('Ctrl Pts',(-9.63621462391286,-39.0705223503542,
20.0697816056099));
#29427=CARTESIAN_POINT('Ctrl Pts',(-9.75549635563586,-39.0794273897883,
20.0639777206454));
#29428=CARTESIAN_POINT('Ctrl Pts',(-9.87495964064826,-39.0830858316393,
20.0581738356809));
#29429=CARTESIAN_POINT('Ctrl Pts',(-9.99440527963151,-39.0867437330984,
20.0523708080135));
#29430=CARTESIAN_POINT('Ctrl Pts',(-10.1140320105376,-39.0851565656684,
20.046567780346));
#29431=CARTESIAN_POINT('Ctrl Pts',(-10.2333461411369,-39.0783298761155,
20.0407647526786));
#29432=CARTESIAN_POINT('Ctrl Pts',(-10.3526708058821,-39.0715025838399,
20.0349612126666));
#29433=CARTESIAN_POINT('Ctrl Pts',(-10.4716824077565,-39.059434873021,20.0291576726547));
#29434=CARTESIAN_POINT('Ctrl Pts',(-10.589890698599,-39.0421843060042,20.0233541326428));
#29435=CARTESIAN_POINT('Ctrl Pts',(-10.7081373229486,-39.0249281448388,
20.0175487106136));
#29436=CARTESIAN_POINT('Ctrl Pts',(-10.8255797143336,-39.0024858438039,
20.0117432885844));
#29437=CARTESIAN_POINT('Ctrl Pts',(-10.9417367948808,-38.9749662651609,
20.0059378665552));
#29438=CARTESIAN_POINT('Ctrl Pts',(-11.0580225084692,-38.9474162111731,
20.0001260155672));
#29439=CARTESIAN_POINT('Ctrl Pts',(-11.1730196724962,-38.9147777505631,
19.9943141645791));
#29440=CARTESIAN_POINT('Ctrl Pts',(-11.2862612255628,-38.8772099581547,
19.9885023135911));
#29441=CARTESIAN_POINT('Ctrl Pts',(-11.3995771562069,-38.8396174910458,
19.9826866453524));
#29442=CARTESIAN_POINT('Ctrl Pts',(-11.5111347988012,-38.7970893894815,
19.9768709771136));
#29443=CARTESIAN_POINT('Ctrl Pts',(-11.6204875142691,-38.7498326917475,
19.9710553088749));
#29444=CARTESIAN_POINT('Ctrl Pts',(-11.7299968654689,-38.702508303994,19.9652313103314));
#29445=CARTESIAN_POINT('Ctrl Pts',(-11.837294619651,-38.6504419787779,19.9594073117878));
#29446=CARTESIAN_POINT('Ctrl Pts',(-11.9419590228879,-38.5938864970147,
19.9535833132443));
#29447=CARTESIAN_POINT('Ctrl Pts',(-11.9697269311232,-38.5788820888373,
19.9520381818327));
#29448=CARTESIAN_POINT('Ctrl Pts',(-11.9973096492124,-38.5635619394124,
19.950493050421));
#29449=CARTESIAN_POINT('Ctrl Pts',(-12.0246996641969,-38.5479312662171,
19.9489479190094));
#29450=CARTESIAN_POINT('Ctrl Pts',(-12.1279324851569,-38.4890193419862,
19.943124326928));
#29451=CARTESIAN_POINT('Ctrl Pts',(-12.2287584359163,-38.4255030880873,
19.9373007348465));
#29452=CARTESIAN_POINT('Ctrl Pts',(-12.3267397463782,-38.357604377026,19.931477142765));
#29453=CARTESIAN_POINT('Ctrl Pts',(-12.4245974388409,-38.2897913302895,
19.9256608980113));
#29454=CARTESIAN_POINT('Ctrl Pts',(-12.5196172966492,-38.2176070542147,
19.9198446532575));
#29455=CARTESIAN_POINT('Ctrl Pts',(-12.6113866122977,-38.1413189842982,
19.9140284085038));
#29456=CARTESIAN_POINT('Ctrl Pts',(-12.7030640663699,-38.0651072791481,
19.9082179858422));
#29457=CARTESIAN_POINT('Ctrl Pts',(-12.7914971391326,-37.9848002118877,
19.9024075631806));
#29458=CARTESIAN_POINT('Ctrl Pts',(-12.876303071105,-37.9007077831371,19.896597140519));
#29459=CARTESIAN_POINT('Ctrl Pts',(-12.9643191157427,-37.8134322495691,
19.8905667790991));
#29460=CARTESIAN_POINT('Ctrl Pts',(-13.048427633254,-37.7220793771287,19.8845364176792));
#29461=CARTESIAN_POINT('Ctrl Pts',(-13.1282391859743,-37.6270410341932,
19.8785060562593));
#29462=CARTESIAN_POINT('Ctrl Pts',(-13.2050533028845,-37.535571990723,19.8727021735965));
#29463=CARTESIAN_POINT('Ctrl Pts',(-13.2778871054155,-37.4406896514441,
19.8668982909338));
#29464=CARTESIAN_POINT('Ctrl Pts',(-13.3464323293442,-37.3427794742826,
19.861094408271));
#29465=CARTESIAN_POINT('Ctrl Pts',(-13.4149674285101,-37.2448837593589,
19.8552913828954));
#29466=CARTESIAN_POINT('Ctrl Pts',(-13.4792149747097,-37.1439614303904,
19.8494883575197));
#29467=CARTESIAN_POINT('Ctrl Pts',(-13.5389089831636,-37.0404284375796,
19.843685332144));
#29468=CARTESIAN_POINT('Ctrl Pts',(-13.598608262082,-36.9368863037015,19.8378817944115));
#29469=CARTESIAN_POINT('Ctrl Pts',(-13.6537529999346,-36.8307334014606,
19.8320782566789));
#29470=CARTESIAN_POINT('Ctrl Pts',(-13.7041226041859,-36.7224113135831,
19.8262747189463));
#29471=CARTESIAN_POINT('Ctrl Pts',(-13.7545085428211,-36.614054097882,19.8204692991816));
#29472=CARTESIAN_POINT('Ctrl Pts',(-13.8001160960937,-36.5035266676226,
19.8146638794168));
#29473=CARTESIAN_POINT('Ctrl Pts',(-13.840772604059,-36.3912910565048,19.8088584596521));
#29474=CARTESIAN_POINT('Ctrl Pts',(-13.8814741355335,-36.2789311543118,
19.8030466108953));
#29475=CARTESIAN_POINT('Ctrl Pts',(-13.9172135383115,-36.1648596794967,
19.7972347621384));
#29476=CARTESIAN_POINT('Ctrl Pts',(-13.9478678321096,-36.049554467474,19.7914229133815));
#29477=CARTESIAN_POINT('Ctrl Pts',(-13.9785422598863,-35.9341735220908,
19.7856072473571));
#29478=CARTESIAN_POINT('Ctrl Pts',(-14.0041248398133,-35.8175576236468,
19.7797915813328));
#29479=CARTESIAN_POINT('Ctrl Pts',(-14.0245439016398,-35.7001938187202,
19.7739759153084));
#29480=CARTESIAN_POINT('Ctrl Pts',(-14.044992211682,-35.5826619021581,19.7681519189378));
#29481=CARTESIAN_POINT('Ctrl Pts',(-14.0602621890924,-35.4643803443969,
19.7623279225673));
#29482=CARTESIAN_POINT('Ctrl Pts',(-14.0703340625699,-35.3458404532196,
19.7565039261967));
#29483=CARTESIAN_POINT('Ctrl Pts',(-14.0730062119097,-35.314390863165,19.7549587729448));
#29484=CARTESIAN_POINT('Ctrl Pts',(-14.0753127595707,-35.2829230824219,
19.7534136196929));
#29485=CARTESIAN_POINT('Ctrl Pts',(-14.0772539509858,-35.2514462550343,
19.751868466441));
#29486=CARTESIAN_POINT('Ctrl Pts',(-14.0823853229758,-35.1682399781399,
19.7477839871591));
#29487=CARTESIAN_POINT('Ctrl Pts',(-14.0849699104865,-35.0848750437508,
19.7436995078773));
#29488=CARTESIAN_POINT('Ctrl Pts',(-14.0849997388204,-35.0014607659441,
19.7396150285955));
#29489=CARTESIAN_POINT('Origin',(-10.,-35.,32.7603849714045));
#29490=CARTESIAN_POINT('',(-7.51282745730979,-31.7594448403263,21.7969517045595));
#29491=CARTESIAN_POINT('',(-7.5128274573098,-31.7594448403263,21.6925401901332));
#29492=CARTESIAN_POINT('',(-7.5128274573098,-31.7594448403263,32.7603849714045));
#29493=CARTESIAN_POINT('',(-14.084998525967,-35.0034702806205,20.8853849714301));
#29494=CARTESIAN_POINT('Ctrl Pts',(-7.5128274573098,-31.7594448403263,21.6925401901332));
#29495=CARTESIAN_POINT('Ctrl Pts',(-7.41823831723824,-31.8320433613915,
21.6867304612017));
#29496=CARTESIAN_POINT('Ctrl Pts',(-7.32673657161299,-31.9088588456523,
21.6809207322703));
#29497=CARTESIAN_POINT('Ctrl Pts',(-7.2387160725769,-31.9895953640491,21.6751110033388));
#29498=CARTESIAN_POINT('Ctrl Pts',(-7.14889638448983,-32.0719821827907,
21.6691825202445));
#29499=CARTESIAN_POINT('Ctrl Pts',(-7.06270218204445,-32.1584518535685,
21.6632540371501));
#29500=CARTESIAN_POINT('Ctrl Pts',(-6.98051726194745,-32.2486459706896,
21.6573255540558));
#29501=CARTESIAN_POINT('Ctrl Pts',(-6.90006210464625,-32.3369417538096,
21.6515218489557));
#29502=CARTESIAN_POINT('Ctrl Pts',(-6.82344940572467,-32.4288064278047,
21.6457181438557));
#29503=CARTESIAN_POINT('Ctrl Pts',(-6.75100196095492,-32.5238665742167,
21.6399144387556));
#29504=CARTESIAN_POINT('Ctrl Pts',(-6.67856311686816,-32.6189154354525,
21.6341114226492));
#29505=CARTESIAN_POINT('Ctrl Pts',(-6.61028879098722,-32.7171586899447,
21.6283084065428));
#29506=CARTESIAN_POINT('Ctrl Pts',(-6.54646067508267,-32.8181908581983,
21.6225053904363));
#29507=CARTESIAN_POINT('Ctrl Pts',(-6.48262507317079,-32.9192348758938,
21.6167016937298));
#29508=CARTESIAN_POINT('Ctrl Pts',(-6.42323693620976,-33.0230681125113,
21.6108979970233));
#29509=CARTESIAN_POINT('Ctrl Pts',(-6.36853356044624,-33.1292577680517,
21.6050943003168));
#29510=CARTESIAN_POINT('Ctrl Pts',(-6.31177027222353,-33.2394461054181,
21.5990720593799));
#29511=CARTESIAN_POINT('Ctrl Pts',(-6.26005172010707,-33.3521713939478,
21.593049818443));
#29512=CARTESIAN_POINT('Ctrl Pts',(-6.21358913516407,-33.4669253890784,
21.5870275775062));
#29513=CARTESIAN_POINT('Ctrl Pts',(-6.16874567483564,-33.5776804457435,
21.5812151991619));
#29514=CARTESIAN_POINT('Ctrl Pts',(-6.1287980621215,-33.6903247673409,21.5754028208176));
#29515=CARTESIAN_POINT('Ctrl Pts',(-6.09388554052908,-33.8043851667396,
21.5695904424734));
#29516=CARTESIAN_POINT('Ctrl Pts',(-6.05894890485997,-33.9185243476498,
21.5637740495197));
#29517=CARTESIAN_POINT('Ctrl Pts',(-6.02905438772444,-34.0340811599237,
21.557957656566));
#29518=CARTESIAN_POINT('Ctrl Pts',(-6.0042902724017,-34.1505715022579,21.5521412636124));
#29519=CARTESIAN_POINT('Ctrl Pts',(-5.97949171870993,-34.267223842602,21.5463167820561));
#29520=CARTESIAN_POINT('Ctrl Pts',(-5.95983786975095,-34.3848119025423,
21.5404923004999));
#29521=CARTESIAN_POINT('Ctrl Pts',(-5.9453652930546,-34.502845704802,21.5346678189437));
#29522=CARTESIAN_POINT('Ctrl Pts',(-5.94384095292056,-34.515277745463,21.5340543489872));
#29523=CARTESIAN_POINT('Ctrl Pts',(-5.94237404403647,-34.5277147308241,
21.5334408790307));
#29524=CARTESIAN_POINT('Ctrl Pts',(-5.94096457550326,-34.540156088786,21.5328274090742));
#29525=CARTESIAN_POINT('Ctrl Pts',(-5.92758466681395,-34.6582603455175,
21.5270038154231));
#29526=CARTESIAN_POINT('Ctrl Pts',(-5.91934211447388,-34.7771395042762,
21.521180221772));
#29527=CARTESIAN_POINT('Ctrl Pts',(-5.91631621890907,-34.8963092286898,
21.5153566281209));
#29528=CARTESIAN_POINT('Ctrl Pts',(-5.91329414096097,-35.0153286027953,
21.5095403817982));
#29529=CARTESIAN_POINT('Ctrl Pts',(-5.91547563943895,-35.134637408806,21.5037241354755));
#29530=CARTESIAN_POINT('Ctrl Pts',(-5.9228884422849,-35.2537446471277,21.4979078891528));
#29531=CARTESIAN_POINT('Ctrl Pts',(-5.93029382487437,-35.3727326584477,
21.4920974649247));
#29532=CARTESIAN_POINT('Ctrl Pts',(-5.94292006911669,-35.4915190982697,
21.4862870406966));
#29533=CARTESIAN_POINT('Ctrl Pts',(-5.96074286670504,-35.609612016881,21.4804766164685));
#29534=CARTESIAN_POINT('Ctrl Pts',(-5.9792402941338,-35.7321749973018,21.4744462556367));
#29535=CARTESIAN_POINT('Ctrl Pts',(-6.00333545989816,-35.8539904686384,
21.4684158948049));
#29536=CARTESIAN_POINT('Ctrl Pts',(-6.03294191300147,-35.9745127676842,
21.4623855339731));
#29537=CARTESIAN_POINT('Ctrl Pts',(-6.06143646425158,-36.0905087235307,
21.4565816497599));
#29538=CARTESIAN_POINT('Ctrl Pts',(-6.09503569746211,-36.2053064561403,
21.4507777655466));
#29539=CARTESIAN_POINT('Ctrl Pts',(-6.13361042261971,-36.3184296097726,
21.4449738813333));
#29540=CARTESIAN_POINT('Ctrl Pts',(-6.17217944987885,-36.4315360539081,
21.4391708544156));
#29541=CARTESIAN_POINT('Ctrl Pts',(-6.21572237578022,-36.5429680245935,
21.4333678274979));
#29542=CARTESIAN_POINT('Ctrl Pts',(-6.26406044065362,-36.6522652961649,
21.4275648005802));
#29543=CARTESIAN_POINT('Ctrl Pts',(-6.31240277327407,-36.7615722175455,
21.4217612613158));
#29544=CARTESIAN_POINT('Ctrl Pts',(-6.36554092144129,-36.8687436916215,
21.4159577220514));
#29545=CARTESIAN_POINT('Ctrl Pts',(-6.4232486413134,-36.9733410040167,21.4101541827869));
#29546=CARTESIAN_POINT('Ctrl Pts',(-6.48097507512801,-37.0779722361039,
21.4043487615022));
#29547=CARTESIAN_POINT('Ctrl Pts',(-6.54327383057665,-37.1800272889913,
21.3985433402175));
#29548=CARTESIAN_POINT('Ctrl Pts',(-6.60987386278575,-37.2790940686546,
21.3927379189327));
#29549=CARTESIAN_POINT('Ctrl Pts',(-6.67654764837054,-37.3782705556135,
21.3869260686809));
#29550=CARTESIAN_POINT('Ctrl Pts',(-6.74753199064943,-37.4744518247513,
21.381114218429));
#29551=CARTESIAN_POINT('Ctrl Pts',(-6.82251376542751,-37.5672565569304,
21.3753023681772));
#29552=CARTESIAN_POINT('Ctrl Pts',(-6.89754478864049,-37.6601222437593,
21.3694867006707));
#29553=CARTESIAN_POINT('Ctrl Pts',(-6.97657820348194,-37.7496066716158,
21.3636710331642));
#29554=CARTESIAN_POINT('Ctrl Pts',(-7.05926316405889,-37.8353645024474,
21.3578553656577));
#29555=CARTESIAN_POINT('Ctrl Pts',(-7.14206656191993,-37.9212451721183,
21.352031367835));
#29556=CARTESIAN_POINT('Ctrl Pts',(-7.22853165020971,-38.0033883102641,
21.3462073700123));
#29557=CARTESIAN_POINT('Ctrl Pts',(-7.31827350938968,-38.0814879570686,
21.3403833721896));
#29558=CARTESIAN_POINT('Ctrl Pts',(-7.34208251677673,-38.1022082216663,
21.3388382336283));
#29559=CARTESIAN_POINT('Ctrl Pts',(-7.36612200403376,-38.1226441107511,
21.337293095067));
#29560=CARTESIAN_POINT('Ctrl Pts',(-7.39038444532554,-38.1427904252115,
21.3357479565057));
#29561=CARTESIAN_POINT('Ctrl Pts',(-7.4818290593393,-38.2187214466398,21.3299243628435));
#29562=CARTESIAN_POINT('Ctrl Pts',(-7.57673789068995,-38.2907805045122,
21.3241007691813));
#29563=CARTESIAN_POINT('Ctrl Pts',(-7.67474932401576,-38.3586357786808,
21.3182771755191));
#29564=CARTESIAN_POINT('Ctrl Pts',(-7.77263710135612,-38.4264054433393,
21.3124609291855));
#29565=CARTESIAN_POINT('Ctrl Pts',(-7.87361936226491,-38.489981642841,21.306644682852));
#29566=CARTESIAN_POINT('Ctrl Pts',(-7.97730064829635,-38.5490720382401,
21.3008284365185));
#29567=CARTESIAN_POINT('Ctrl Pts',(-8.08087814878458,-38.6081032838252,
21.2950180122798));
#29568=CARTESIAN_POINT('Ctrl Pts',(-8.1871489468936,-38.662657457206,21.2892075880411));
#29569=CARTESIAN_POINT('Ctrl Pts',(-8.29568826514955,-38.7124852202333,
21.2833971638025));
#29570=CARTESIAN_POINT('Ctrl Pts',(-8.40833602135342,-38.7641990672694,
21.2773668029748));
#29571=CARTESIAN_POINT('Ctrl Pts',(-8.52342705879202,-38.8108213702415,
21.271336442147));
#29572=CARTESIAN_POINT('Ctrl Pts',(-8.64045761121957,-38.8521253215737,
21.2653060813193));
#29573=CARTESIAN_POINT('Ctrl Pts',(-8.75309295697439,-38.8918780591524,
21.2595021970962));
#29574=CARTESIAN_POINT('Ctrl Pts',(-8.86752434411707,-38.9267045656859,
21.2536983128731));
#29575=CARTESIAN_POINT('Ctrl Pts',(-8.98328254519098,-38.9564517711059,
21.24789442865));
#29576=CARTESIAN_POINT('Ctrl Pts',(-9.09902364753772,-38.9861945825447,
21.2420914017228));
#29577=CARTESIAN_POINT('Ctrl Pts',(-9.21609077868371,-39.0108594833107,
21.2362883747956));
#29578=CARTESIAN_POINT('Ctrl Pts',(-9.33400102962214,-39.0303437038863,
21.2304853478684));
#29579=CARTESIAN_POINT('Ctrl Pts',(-9.4519216908,-39.0498296447143,21.2246818085947));
#29580=CARTESIAN_POINT('Ctrl Pts',(-9.57068521687892,-39.0641339293542,
21.2188782693211));
#29581=CARTESIAN_POINT('Ctrl Pts',(-9.68980066117877,-39.0732052943836,
21.2130747300474));
#29582=CARTESIAN_POINT('Ctrl Pts',(-9.80895473322567,-39.0822796011508,
21.2072693087538));
#29583=CARTESIAN_POINT('Ctrl Pts',(-9.92846054350984,-39.0861175824163,
21.2014638874602));
#29584=CARTESIAN_POINT('Ctrl Pts',(-10.0478248515515,-39.0847200373556,
21.1956584661665));
#29585=CARTESIAN_POINT('Ctrl Pts',(-10.1673213445136,-39.0833209446431,
21.1898466159063));
#29586=CARTESIAN_POINT('Ctrl Pts',(-10.2866756138942,-39.0766747573613,
21.184034765646));
#29587=CARTESIAN_POINT('Ctrl Pts',(-10.4053970920895,-39.064834338288,21.1782229153857));
#29588=CARTESIAN_POINT('Ctrl Pts',(-10.5241965471874,-39.052986142364,21.1724072478711));
#29589=CARTESIAN_POINT('Ctrl Pts',(-10.642361980158,-39.0359369785404,21.1665915803565));
#29590=CARTESIAN_POINT('Ctrl Pts',(-10.7594122392775,-39.0137909824548,
21.1607759128418));
#29591=CARTESIAN_POINT('Ctrl Pts',(-10.8766301602534,-38.9916132646213,
21.1549519150115));
#29592=CARTESIAN_POINT('Ctrl Pts',(-10.9927293230292,-38.9643242359031,
21.1491279171812));
#29593=CARTESIAN_POINT('Ctrl Pts',(-11.1072428327699,-38.9320781158669,
21.1433039193508));
#29594=CARTESIAN_POINT('Ctrl Pts',(-11.137623893087,-38.9235230438931,21.1417587808797));
#29595=CARTESIAN_POINT('Ctrl Pts',(-11.1678934506138,-38.9146193209484,
21.1402136424085));
#29596=CARTESIAN_POINT('Ctrl Pts',(-11.198043031576,-38.90537039146,21.1386685039373));
#29597=CARTESIAN_POINT('Ctrl Pts',(-11.3116761558621,-38.870511374501,21.1328449101648));
#29598=CARTESIAN_POINT('Ctrl Pts',(-11.4239698392151,-38.8306325165478,
21.1270213163923));
#29599=CARTESIAN_POINT('Ctrl Pts',(-11.5344483324554,-38.7858543705516,
21.1211977226198));
#29600=CARTESIAN_POINT('Ctrl Pts',(-11.6447874406743,-38.7411327188346,
21.1153814761755));
#29601=CARTESIAN_POINT('Ctrl Pts',(-11.7533155387002,-38.6915242253266,
21.1095652297312));
#29602=CARTESIAN_POINT('Ctrl Pts',(-11.8595713467469,-38.6371993905143,
21.1037489832868));
#29603=CARTESIAN_POINT('Ctrl Pts',(-11.9657207921482,-38.582928935159,21.097938558937));
#29604=CARTESIAN_POINT('Ctrl Pts',(-12.06960211107,-38.5239517153247,21.0921281345872));
#29605=CARTESIAN_POINT('Ctrl Pts',(-12.1707739167292,-38.4604863245573,
21.0863177102374));
#29606=CARTESIAN_POINT('Ctrl Pts',(-12.2757752819967,-38.3946186390456,
21.0802873494512));
#29607=CARTESIAN_POINT('Ctrl Pts',(-12.3778575445062,-38.3239164647101,
21.074256988665));
#29608=CARTESIAN_POINT('Ctrl Pts',(-12.4765548626641,-38.2486768094433,
21.0682266278788));
#29609=CARTESIAN_POINT('Ctrl Pts',(-12.5715455007079,-38.1762628574395,
21.0624227435443));
#29610=CARTESIAN_POINT('Ctrl Pts',(-12.663400505583,-38.0996463676855,21.0566188592098));
#29611=CARTESIAN_POINT('Ctrl Pts',(-12.7517346404905,-38.0191358810634,
21.0508149748753));
#29612=CARTESIAN_POINT('Ctrl Pts',(-12.840055727498,-37.9386372867044,21.0450119478368));
#29613=CARTESIAN_POINT('Ctrl Pts',(-12.9248566770818,-37.8542461143283,
21.0392089207983));
#29614=CARTESIAN_POINT('Ctrl Pts',(-13.0057868226452,-37.7663099206005,
21.0334058937598));
#29615=CARTESIAN_POINT('Ctrl Pts',(-13.0867241134889,-37.6783659630319,
21.0276023543751));
#29616=CARTESIAN_POINT('Ctrl Pts',(-13.1637896442939,-37.5868766622893,
21.0217988149904));
#29617=CARTESIAN_POINT('Ctrl Pts',(-13.2366714207157,-37.4922245312817,
21.0159952756057));
#29618=CARTESIAN_POINT('Ctrl Pts',(-13.3095768318412,-37.3975417057001,
21.0101898542013));
#29619=CARTESIAN_POINT('Ctrl Pts',(-13.3782955413343,-37.2996943334015,
21.004384432797));
#29620=CARTESIAN_POINT('Ctrl Pts',(-13.4425578411275,-37.1990953845823,
20.9985790113926));
#29621=CARTESIAN_POINT('Ctrl Pts',(-13.5068913054552,-37.0983850317615,
20.9927671610227));
#29622=CARTESIAN_POINT('Ctrl Pts',(-13.5667582893279,-36.9949173644387,
20.9869553106528));
#29623=CARTESIAN_POINT('Ctrl Pts',(-13.621934094346,-36.889131656665,20.9811434602829));
#29624=CARTESIAN_POINT('Ctrl Pts',(-13.6771461391229,-36.7832764682823,
20.9753277926592));
#29625=CARTESIAN_POINT('Ctrl Pts',(-13.7276606964019,-36.6751005764842,
20.9695121250354));
#29626=CARTESIAN_POINT('Ctrl Pts',(-13.7733011123659,-36.5650634860663,
20.9636964574116));
#29627=CARTESIAN_POINT('Ctrl Pts',(-13.8190069032839,-36.4548687794312,
20.9578724594737));
#29628=CARTESIAN_POINT('Ctrl Pts',(-13.8598244785776,-36.3428079353696,
20.9520484615358));
#29629=CARTESIAN_POINT('Ctrl Pts',(-13.8956268882903,-36.2293559888128,
20.9462244635979));
#29630=CARTESIAN_POINT('Ctrl Pts',(-13.9051254566608,-36.1992565882477,
20.9446793261882));
#29631=CARTESIAN_POINT('Ctrl Pts',(-13.9142713021348,-36.1690593277715,
20.9431341887785));
#29632=CARTESIAN_POINT('Ctrl Pts',(-13.9230626605209,-36.1387731826954,
20.9415890513689));
#29633=CARTESIAN_POINT('Ctrl Pts',(-13.964019680971,-35.9976766412109,20.9343905933257));
#29634=CARTESIAN_POINT('Ctrl Pts',(-13.9973850464863,-35.8542851090668,
20.9271921352824));
#29635=CARTESIAN_POINT('Ctrl Pts',(-14.0229437096185,-35.7093299015557,
20.9199936772392));
#29636=CARTESIAN_POINT('Ctrl Pts',(-14.0481513699877,-35.5663653959087,
20.9128940772094));
#29637=CARTESIAN_POINT('Ctrl Pts',(-14.0657652703003,-35.4218798148452,
20.9057944771795));
#29638=CARTESIAN_POINT('Ctrl Pts',(-14.0756251114202,-35.2765952840546,
20.8986948771497));
#29639=CARTESIAN_POINT('Ctrl Pts',(-14.0817866583225,-35.1858050329981,
20.8942582419098));
#29640=CARTESIAN_POINT('Ctrl Pts',(-14.0849210219501,-35.0947031891774,
20.88982160667));
#29641=CARTESIAN_POINT('Ctrl Pts',(-14.084998525967,-35.0034702806205,20.8853849714301));
#29642=CARTESIAN_POINT('Ctrl Pts',(-14.0849985259674,-35.0034702800941,
20.8853849714045));
#29643=CARTESIAN_POINT('Ctrl Pts',(-14.0851010661903,-34.8827662884805,
20.8795151642127));
#29644=CARTESIAN_POINT('Ctrl Pts',(-14.0798491529874,-34.7619569640071,
20.8736453570208));
#29645=CARTESIAN_POINT('Ctrl Pts',(-14.0692436282641,-34.6415571261249,
20.867775549829));
#29646=CARTESIAN_POINT('Ctrl Pts',(-14.0588381189795,-34.5234279751741,
20.8620164445676));
#29647=CARTESIAN_POINT('Ctrl Pts',(-14.04327920392,-34.4056934318941,20.8562573393062));
#29648=CARTESIAN_POINT('Ctrl Pts',(-14.0226202175467,-34.2888378628019,
20.8504982340449));
#29649=CARTESIAN_POINT('Ctrl Pts',(-14.0019643520304,-34.1719999465367,
20.8447399987847));
#29650=CARTESIAN_POINT('Ctrl Pts',(-13.9762100191969,-34.05604114935,20.8389817635246));
#29651=CARTESIAN_POINT('Ctrl Pts',(-13.9454620141881,-33.9414375339175,
20.8332235282644));
#29652=CARTESIAN_POINT('Ctrl Pts',(-13.9147111095555,-33.82682311104,20.8274647499864));
#29653=CARTESIAN_POINT('Ctrl Pts',(-13.8789657046189,-33.7135645250196,
20.8217059717084));
#29654=CARTESIAN_POINT('Ctrl Pts',(-13.8383807969433,-33.6021238046032,
20.8159471934304));
#29655=CARTESIAN_POINT('Ctrl Pts',(-13.7964261779445,-33.4869220403567,
20.8099940605445));
#29656=CARTESIAN_POINT('Ctrl Pts',(-13.7492997768626,-33.3736634658438,
20.8040409276587));
#29657=CARTESIAN_POINT('Ctrl Pts',(-13.6972267955546,-33.2628359253561,
20.7980877947729));
#29658=CARTESIAN_POINT('Ctrl Pts',(-13.6467793219724,-33.1554679721394,
20.7923204946021));
#29659=CARTESIAN_POINT('Ctrl Pts',(-13.5916897458874,-33.05038188159,20.7865531944314));
#29660=CARTESIAN_POINT('Ctrl Pts',(-13.532208994307,-32.947994975509,20.7807858942606));
#29661=CARTESIAN_POINT('Ctrl Pts',(-13.4698533786046,-32.8406594358778,
20.7747398450172));
#29662=CARTESIAN_POINT('Ctrl Pts',(-13.4026717823479,-32.7362909683151,
20.7686937957739));
#29663=CARTESIAN_POINT('Ctrl Pts',(-13.3310026043436,-32.6353337127924,
20.7626477465305));
#29664=CARTESIAN_POINT('Ctrl Pts',(-13.2593334263393,-32.5343764572698,
20.7566016972871));
#29665=CARTESIAN_POINT('Ctrl Pts',(-13.1831770448846,-32.4368307748664,
20.7505556480437));
#29666=CARTESIAN_POINT('Ctrl Pts',(-13.1029170864551,-32.3430975639694,
20.7445095988004));
#29667=CARTESIAN_POINT('Ctrl Pts',(-13.0256101762356,-32.2528131299729,
20.7386860051282));
#29668=CARTESIAN_POINT('Ctrl Pts',(-12.9442348728726,-32.1657599620686,
20.732862411456));
#29669=CARTESIAN_POINT('Ctrl Pts',(-12.8590915555345,-32.0823261873418,
20.7270388177838));
#29670=CARTESIAN_POINT('Ctrl Pts',(-12.7740556591628,-31.998997676739,20.7212225714418));
#29671=CARTESIAN_POINT('Ctrl Pts',(-12.6852614933123,-31.9192797601209,
20.7154063250997));
#29672=CARTESIAN_POINT('Ctrl Pts',(-12.593049462095,-31.8435273663266,20.7095900787576));
#29673=CARTESIAN_POINT('Ctrl Pts',(-12.5009297356559,-31.767850801118,20.7037796545119));
#29674=CARTESIAN_POINT('Ctrl Pts',(-12.4053992638164,-31.6961321195937,
20.6979692302662));
#29675=CARTESIAN_POINT('Ctrl Pts',(-12.3068346109939,-31.6286888192395,
20.6921588060204));
#29676=CARTESIAN_POINT('Ctrl Pts',(-12.2045390821434,-31.5586926504347,
20.6861284451959));
#29677=CARTESIAN_POINT('Ctrl Pts',(-12.0989754538823,-31.4933022356453,
20.6800980843714));
#29678=CARTESIAN_POINT('Ctrl Pts',(-11.9906019499155,-31.432826205945,20.6740677235469));
#29679=CARTESIAN_POINT('Ctrl Pts',(-11.8862985278559,-31.3746214176948,
20.6682638393203));
#29680=CARTESIAN_POINT('Ctrl Pts',(-11.7793928683359,-31.3209687582943,
20.6624599550937));
#29681=CARTESIAN_POINT('Ctrl Pts',(-11.6703216060448,-31.2720983472763,
20.6566560708672));
#29682=CARTESIAN_POINT('Ctrl Pts',(-11.5612664547734,-31.2232351549531,
20.6508530439378));
#29683=CARTESIAN_POINT('Ctrl Pts',(-11.4500467094183,-31.1791529731452,
20.6450500170085));
#29684=CARTESIAN_POINT('Ctrl Pts',(-11.3371209849973,-31.140034654109,20.6392469900792));
#29685=CARTESIAN_POINT('Ctrl Pts',(-11.2241852904441,-31.1009128813441,
20.6334434508047));
#29686=CARTESIAN_POINT('Ctrl Pts',(-11.1095437032182,-31.0667559763748,
20.6276399115302));
#29687=CARTESIAN_POINT('Ctrl Pts',(-10.9936714594704,-31.0376973827541,
20.6218363722558));
#29688=CARTESIAN_POINT('Ctrl Pts',(-10.877761639734,-31.0086293657775,20.6160309509626));
#29689=CARTESIAN_POINT('Ctrl Pts',(-10.7606207656496,-30.9846630475094,
20.6102255296695));
#29690=CARTESIAN_POINT('Ctrl Pts',(-10.6427351271284,-30.9658809442017,
20.6044201083764));
#29691=CARTESIAN_POINT('Ctrl Pts',(-10.5247189412156,-30.9470780414597,
20.5986082581185));
#29692=CARTESIAN_POINT('Ctrl Pts',(-10.4059567480696,-30.9334708775643,
20.5927964078607));
#29693=CARTESIAN_POINT('Ctrl Pts',(-10.2869409962033,-30.9250902016489,
20.5869845576029));
#29694=CARTESIAN_POINT('Ctrl Pts',(-10.1678470741772,-30.9167040212623,
20.5811688900919));
#29695=CARTESIAN_POINT('Ctrl Pts',(-10.0484996690212,-30.9135511760909,
20.5753532225808));
#29696=CARTESIAN_POINT('Ctrl Pts',(-9.92939060816214,-30.9156102886987,
20.5695375550698));
#29697=CARTESIAN_POINT('Ctrl Pts',(-9.81011093646856,-30.9176723507623,
20.5637135572446));
#29698=CARTESIAN_POINT('Ctrl Pts',(-9.69107069661965,-30.9249612466002,
20.5578895594195));
#29699=CARTESIAN_POINT('Ctrl Pts',(-9.57275612268976,-30.9374038264552,
20.5520655615944));
#29700=CARTESIAN_POINT('Ctrl Pts',(-9.54136661957653,-30.9407049108958,
20.5505204231402));
#29701=CARTESIAN_POINT('Ctrl Pts',(-9.51002813342651,-30.9443684696613,
20.5489752846861));
#29702=CARTESIAN_POINT('Ctrl Pts',(-9.47874959801868,-30.9483925389502,
20.547430146232));
#29703=CARTESIAN_POINT('Ctrl Pts',(-9.3608661673276,-30.96355856533,20.5416067846362));
#29704=CARTESIAN_POINT('Ctrl Pts',(-9.24345509214536,-30.9838981280243,
20.5357834230404));
#29705=CARTESIAN_POINT('Ctrl Pts',(-9.12700558914339,-31.0093727612551,
20.5299600614446));
#29706=CARTESIAN_POINT('Ctrl Pts',(-9.01069687702149,-31.0348165949037,
20.5241437404646));
#29707=CARTESIAN_POINT('Ctrl Pts',(-8.89534782060662,-31.0653830669002,
20.5183274194846));
#29708=CARTESIAN_POINT('Ctrl Pts',(-8.78144188802837,-31.1009820303379,
20.5125110985045));
#29709=CARTESIAN_POINT('Ctrl Pts',(-8.66746504168588,-31.1366031564184,
20.5066911564909));
#29710=CARTESIAN_POINT('Ctrl Pts',(-8.55493352306209,-31.1772629828042,
20.5008712144772));
#29711=CARTESIAN_POINT('Ctrl Pts',(-8.44432160893254,-31.2228198687955,
20.4950512724635));
#29712=CARTESIAN_POINT('Ctrl Pts',(-8.33397539404962,-31.2682673232633,
20.4892453104466));
#29713=CARTESIAN_POINT('Ctrl Pts',(-8.22553995871077,-31.3185882042552,
20.4834393484298));
#29714=CARTESIAN_POINT('Ctrl Pts',(-8.11947019380578,-31.3735923218679,
20.4776333864129));
#29715=CARTESIAN_POINT('Ctrl Pts',(-8.01301732572882,-31.4287951035576,
20.4718064544008));
#29716=CARTESIAN_POINT('Ctrl Pts',(-7.90894763984181,-31.4887148755145,
20.4659795223887));
#29717=CARTESIAN_POINT('Ctrl Pts',(-7.80769898378764,-31.5531113661282,
20.4601525903766));
#29718=CARTESIAN_POINT('Ctrl Pts',(-7.70645032773347,-31.617507856742,20.4543256583645));
#29719=CARTESIAN_POINT('Ctrl Pts',(-7.60802305871064,-31.6863808514964,
20.4484987263525));
#29720=CARTESIAN_POINT('Ctrl Pts',(-7.51282745730978,-31.7594448403263,
20.4426717943404));
#29721=CARTESIAN_POINT('',(-14.0849985032409,-34.9965030699667,20.9896150285484));
#29722=CARTESIAN_POINT('Ctrl Pts',(-14.0849985032409,-34.9965030699667,
20.9896150285484));
#29723=CARTESIAN_POINT('Ctrl Pts',(-14.0848731076929,-34.8500201203563,
20.9824905060981));
#29724=CARTESIAN_POINT('Ctrl Pts',(-14.0768649533835,-34.7038771885051,
20.9753659836478));
#29725=CARTESIAN_POINT('Ctrl Pts',(-14.0611057921053,-34.5588143867611,
20.9682414611975));
#29726=CARTESIAN_POINT('Ctrl Pts',(-14.0451084213714,-34.4115588711768,
20.9610092471901));
#29727=CARTESIAN_POINT('Ctrl Pts',(-14.0211239958772,-34.2654163151662,
20.9537770331828));
#29728=CARTESIAN_POINT('Ctrl Pts',(-13.9893392113733,-34.1211384314923,
20.9465448191755));
#29729=CARTESIAN_POINT('Ctrl Pts',(-13.9714671903031,-34.0400135342429,
20.9424782734009));
#29730=CARTESIAN_POINT('Ctrl Pts',(-13.9511298671933,-33.9594777773168,
20.9384117276262));
#29731=CARTESIAN_POINT('Ctrl Pts',(-13.928367028479,-33.8796618860545,20.9343451818516));
#29732=CARTESIAN_POINT('Ctrl Pts',(-13.8957689635323,-33.7653596393175,
20.9285215881894));
#29733=CARTESIAN_POINT('Ctrl Pts',(-13.8581254755735,-33.6522969933898,
20.9226979945272));
#29734=CARTESIAN_POINT('Ctrl Pts',(-13.8155476565818,-33.5409519951856,
20.9168744008649));
#29735=CARTESIAN_POINT('Ctrl Pts',(-13.773023555835,-33.4297474752401,20.9110581545314));
#29736=CARTESIAN_POINT('Ctrl Pts',(-13.7255776507743,-33.3202566708117,
20.9052419081978));
#29737=CARTESIAN_POINT('Ctrl Pts',(-13.6733712581103,-33.2129441530581,
20.8994256618642));
#29738=CARTESIAN_POINT('Ctrl Pts',(-13.6212171243352,-33.1057390557306,
20.8936152376256));
#29739=CARTESIAN_POINT('Ctrl Pts',(-13.5643121604877,-33.0007082723686,
20.8878048133869));
#29740=CARTESIAN_POINT('Ctrl Pts',(-13.502866161484,-32.8982974390436,20.8819943891482));
#29741=CARTESIAN_POINT('Ctrl Pts',(-13.4390943041823,-32.7920101436161,
20.8759640283205));
#29742=CARTESIAN_POINT('Ctrl Pts',(-13.3704310041942,-32.6885454768558,
20.8699336674928));
#29743=CARTESIAN_POINT('Ctrl Pts',(-13.2971639702753,-32.5883750803414,
20.8639033066651));
#29744=CARTESIAN_POINT('Ctrl Pts',(-13.2266485576182,-32.49196668944,20.8580994224419));
#29745=CARTESIAN_POINT('Ctrl Pts',(-13.1518692340175,-32.3986099506225,
20.8522955382188));
#29746=CARTESIAN_POINT('Ctrl Pts',(-13.0731268378526,-32.3086961452727,
20.8464916539957));
#29747=CARTESIAN_POINT('Ctrl Pts',(-12.9943960727838,-32.2187956211559,
20.8406886270685));
#29748=CARTESIAN_POINT('Ctrl Pts',(-12.9117036682537,-32.1323373262523,
20.8348856001413));
#29749=CARTESIAN_POINT('Ctrl Pts',(-12.8253901565031,-32.0496787524855,
20.8290825732141));
#29750=CARTESIAN_POINT('Ctrl Pts',(-12.7390690241739,-31.9670128808329,
20.8232790339404));
#29751=CARTESIAN_POINT('Ctrl Pts',(-12.6491264439008,-31.8881476797638,
20.8174754946667));
#29752=CARTESIAN_POINT('Ctrl Pts',(-12.5559386644153,-31.8134026699712,
20.811671955393));
#29753=CARTESIAN_POINT('Ctrl Pts',(-12.4627206652216,-31.7386334212452,
20.8058665340994));
#29754=CARTESIAN_POINT('Ctrl Pts',(-12.3662556922375,-31.6679872764169,
20.8000611128057));
#29755=CARTESIAN_POINT('Ctrl Pts',(-12.2669512843041,-31.601742082391,20.7942556915121));
#29756=CARTESIAN_POINT('Ctrl Pts',(-12.1675369059325,-31.5354235279458,
20.7884438412518));
#29757=CARTESIAN_POINT('Ctrl Pts',(-12.0652771559888,-31.473515879256,20.7826319909915));
#29758=CARTESIAN_POINT('Ctrl Pts',(-11.9606067648305,-31.4162525041933,
20.7768201407312));
#29759=CARTESIAN_POINT('Ctrl Pts',(-11.8558676255988,-31.3589515182392,
20.7710044732166));
#29760=CARTESIAN_POINT('Ctrl Pts',(-11.7487150575697,-31.3063010604908,
20.7651888057019));
#29761=CARTESIAN_POINT('Ctrl Pts',(-11.6396049709043,-31.2584868649989,
20.7593731381873));
#29762=CARTESIAN_POINT('Ctrl Pts',(-11.5303385958221,-31.2106041808352,
20.7535491403569));
#29763=CARTESIAN_POINT('Ctrl Pts',(-11.4191094850817,-31.1675717325015,
20.7477251425266));
#29764=CARTESIAN_POINT('Ctrl Pts',(-11.3063900618776,-31.1295258680328,
20.7419011446962));
#29765=CARTESIAN_POINT('Ctrl Pts',(-11.2764849825327,-31.119432092148,20.7403560062252));
#29766=CARTESIAN_POINT('Ctrl Pts',(-11.2464750655715,-31.1096890290316,
20.7388108677542));
#29767=CARTESIAN_POINT('Ctrl Pts',(-11.2163692495621,-31.1002986205711,
20.7372657292832));
#29768=CARTESIAN_POINT('Ctrl Pts',(-11.1028985208735,-31.0649055759061,
20.731442004453));
#29769=CARTESIAN_POINT('Ctrl Pts',(-10.9876987634977,-31.0344121023845,
20.7256182796227));
#29770=CARTESIAN_POINT('Ctrl Pts',(-10.8712307300107,-31.0089873446599,
20.7197945547924));
#29771=CARTESIAN_POINT('Ctrl Pts',(-10.7549102796124,-30.9835948040524,
20.7139782095261));
#29772=CARTESIAN_POINT('Ctrl Pts',(-10.6373251451302,-30.9632582903934,
20.7081618642598));
#29773=CARTESIAN_POINT('Ctrl Pts',(-10.5189523332168,-30.9480975485769,
20.7023455189935));
#29774=CARTESIAN_POINT('Ctrl Pts',(-10.4006986643929,-30.9329520661564,
20.6965350279206));
#29775=CARTESIAN_POINT('Ctrl Pts',(-10.2816592980966,-30.9229720433083,
20.6907245368478));
#29776=CARTESIAN_POINT('Ctrl Pts',(-10.1623219706432,-30.9182262951204,
20.6849140457749));
#29777=CARTESIAN_POINT('Ctrl Pts',(-10.0430738621628,-30.9134840949487,
20.6791078987414));
#29778=CARTESIAN_POINT('Ctrl Pts',(-9.92352864244225,-30.9139683984217,
20.6733017517079));
#29779=CARTESIAN_POINT('Ctrl Pts',(-9.80417911364261,-30.9196961901758,
20.6674956046744));
#29780=CARTESIAN_POINT('Ctrl Pts',(-9.68487740632811,-30.9254216868934,
20.661691784073));
#29781=CARTESIAN_POINT('Ctrl Pts',(-9.56577164121818,-30.9363864744827,
20.6558879634716));
#29782=CARTESIAN_POINT('Ctrl Pts',(-9.44735408758601,-30.9525554363905,
20.6500841428702));
#29783=CARTESIAN_POINT('Ctrl Pts',(-9.32895603536141,-30.9687217355384,
20.6442812780619));
#29784=CARTESIAN_POINT('Ctrl Pts',(-9.21124637356511,-30.9900904489027,
20.6384784132535));
#29785=CARTESIAN_POINT('Ctrl Pts',(-9.0947110799995,-31.0165747187472,20.6326755484451));
#29786=CARTESIAN_POINT('Ctrl Pts',(-8.97816747584504,-31.0430608772888,
20.6268722698117));
#29787=CARTESIAN_POINT('Ctrl Pts',(-8.86279880443876,-31.0746632265921,
20.6210689911782));
#29788=CARTESIAN_POINT('Ctrl Pts',(-8.74907907121573,-31.1112441796984,
20.6152657125448));
#29789=CARTESIAN_POINT('Ctrl Pts',(-8.63525960069849,-31.1478572159374,
20.6094573441763));
#29790=CARTESIAN_POINT('Ctrl Pts',(-8.52309234690806,-31.1894574539382,
20.6036489758079));
#29791=CARTESIAN_POINT('Ctrl Pts',(-8.41303458871639,-31.235857895431,20.5978406074394));
#29792=CARTESIAN_POINT('Ctrl Pts',(-8.30292908366268,-31.2822784670401,
20.5920297191999));
#29793=CARTESIAN_POINT('Ctrl Pts',(-8.19493526746047,-31.3335032179248,
20.5862188309604));
#29794=CARTESIAN_POINT('Ctrl Pts',(-8.08948741778155,-31.3892983129058,
20.5804079427208));
#29795=CARTESIAN_POINT('Ctrl Pts',(-7.98388384719028,-31.4451758037168,
20.574588473208));
#29796=CARTESIAN_POINT('Ctrl Pts',(-7.8808341093746,-31.5056369195399,20.5687690036951));
#29797=CARTESIAN_POINT('Ctrl Pts',(-7.78074545052058,-31.5704031950366,
20.5629495341823));
#29798=CARTESIAN_POINT('Ctrl Pts',(-7.6888465203333,-31.6298699867642,20.5576062412596));
#29799=CARTESIAN_POINT('Ctrl Pts',(-7.59944376850164,-31.6929655797273,
20.552262948337));
#29800=CARTESIAN_POINT('Ctrl Pts',(-7.51282745730979,-31.7594448403263,
20.5469196554144));
#29801=CARTESIAN_POINT('Ctrl Pts',(-7.51282745730979,-31.7594448403263,
21.7969517045595));
#29802=CARTESIAN_POINT('Ctrl Pts',(-7.41803123744738,-31.8322022980998,
21.7911462658977));
#29803=CARTESIAN_POINT('Ctrl Pts',(-7.32646761151655,-31.9090941156954,
21.7853408272359));
#29804=CARTESIAN_POINT('Ctrl Pts',(-7.23850334801992,-31.989790498802,21.7795353885741));
#29805=CARTESIAN_POINT('Ctrl Pts',(-7.15044160797137,-32.0705763046453,
21.7737235166845));
#29806=CARTESIAN_POINT('Ctrl Pts',(-7.06598749294522,-32.1551748152077,
21.7679116447949));
#29807=CARTESIAN_POINT('Ctrl Pts',(-6.98547103052354,-32.2432192520646,
21.7620997729053));
#29808=CARTESIAN_POINT('Ctrl Pts',(-6.90490156944531,-32.3313216427452,
21.7562840754452));
#29809=CARTESIAN_POINT('Ctrl Pts',(-6.82827518425165,-32.4228741645268,
21.7504683779852));
#29810=CARTESIAN_POINT('Ctrl Pts',(-6.75588066911818,-32.5174781437017,
21.7446526805251));
#29811=CARTESIAN_POINT('Ctrl Pts',(-6.68338258582743,-32.612217464066,21.738828663083));
#29812=CARTESIAN_POINT('Ctrl Pts',(-6.61512868904173,-32.7100166212431,
21.7330046456408));
#29813=CARTESIAN_POINT('Ctrl Pts',(-6.55136372612828,-32.810449166944,21.7271806281987));
#29814=CARTESIAN_POINT('Ctrl Pts',(-6.53487643022944,-32.8364173636337,
21.7256747495076));
#29815=CARTESIAN_POINT('Ctrl Pts',(-6.51868899898723,-32.8625614964342,
21.7241688708165));
#29816=CARTESIAN_POINT('Ctrl Pts',(-6.50280514828376,-32.8888739570719,
21.7226629921254));
#29817=CARTESIAN_POINT('Ctrl Pts',(-6.44137849223948,-32.990630546166,21.7168393984561));
#29818=CARTESIAN_POINT('Ctrl Pts',(-6.38429762830078,-33.0952344137322,
21.7110158047867));
#29819=CARTESIAN_POINT('Ctrl Pts',(-6.33183666579974,-33.2022784549245,
21.7051922111174));
#29820=CARTESIAN_POINT('Ctrl Pts',(-6.27944189059527,-33.3091874441587,
21.6993759647765));
#29821=CARTESIAN_POINT('Ctrl Pts',(-6.23165560181353,-33.4185301202355,
21.6935597184356));
#29822=CARTESIAN_POINT('Ctrl Pts',(-6.1887078171446,-33.5298718093631,21.6877434720947));
#29823=CARTESIAN_POINT('Ctrl Pts',(-6.14580302344499,-33.6411020448458,
21.6819330478485));
#29824=CARTESIAN_POINT('Ctrl Pts',(-6.10772724468424,-33.7543269338045,
21.6761226236022));
#29825=CARTESIAN_POINT('Ctrl Pts',(-6.07466360223702,-33.8690892323454,
21.670312199356));
#29826=CARTESIAN_POINT('Ctrl Pts',(-6.04034843251884,-33.9881955213142,
21.664281838531));
#29827=CARTESIAN_POINT('Ctrl Pts',(-6.011432532949,-34.108957505296,21.6582514777061));
#29828=CARTESIAN_POINT('Ctrl Pts',(-5.98806495335417,-34.2308432009695,
21.6522211168811));
#29829=CARTESIAN_POINT('Ctrl Pts',(-5.96557496798386,-34.3481513501263,
21.64641723265));
#29830=CARTESIAN_POINT('Ctrl Pts',(-5.94822415578494,-34.4664998916385,
21.6406133484188));
#29831=CARTESIAN_POINT('Ctrl Pts',(-5.93609381245938,-34.5854020032983,
21.6348094641876));
#29832=CARTESIAN_POINT('Ctrl Pts',(-5.92396526091524,-34.7042865518447,
21.6290064372522));
#29833=CARTESIAN_POINT('Ctrl Pts',(-5.91705568616423,-34.8237241018089,
21.6232034103168));
#29834=CARTESIAN_POINT('Ctrl Pts',(-5.91539460443504,-34.9432218129771,
21.6174003833814));
#29835=CARTESIAN_POINT('Ctrl Pts',(-5.91373337604969,-35.0627300745444,
21.6115968440994));
#29836=CARTESIAN_POINT('Ctrl Pts',(-5.91732156768746,-35.1822980995589,
21.6057933048173));
#29837=CARTESIAN_POINT('Ctrl Pts',(-5.92613656673855,-35.3014327904114,
21.5999897655353));
#29838=CARTESIAN_POINT('Ctrl Pts',(-5.93495442439102,-35.4206061152548,
21.5941843442331));
#29839=CARTESIAN_POINT('Ctrl Pts',(-5.94900243029894,-35.5393454194489,
21.588378922931));
#29840=CARTESIAN_POINT('Ctrl Pts',(-5.96820615034603,-35.6571631105687,
21.5825735016289));
#29841=CARTESIAN_POINT('Ctrl Pts',(-5.98743113673578,-35.7751112738776,
21.5767616513599));
#29842=CARTESIAN_POINT('Ctrl Pts',(-6.01182316813919,-35.8921353836473,
21.5709498010909));
#29843=CARTESIAN_POINT('Ctrl Pts',(-6.0412567294959,-36.0077582637907,21.565137950822));
#29844=CARTESIAN_POINT('Ctrl Pts',(-6.07070962297388,-36.1234570856632,
21.5593222832985));
#29845=CARTESIAN_POINT('Ctrl Pts',(-6.10521052322106,-36.2377524550219,
21.5535066157751));
#29846=CARTESIAN_POINT('Ctrl Pts',(-6.14458462288469,-36.3501841614768,
21.5476909482517));
#29847=CARTESIAN_POINT('Ctrl Pts',(-6.18401512169475,-36.4627769142116,
21.5418669504124));
#29848=CARTESIAN_POINT('Ctrl Pts',(-6.22833260108735,-36.5735002981215,
21.5360429525732));
#29849=CARTESIAN_POINT('Ctrl Pts',(-6.27731485981466,-36.6819156777447,
21.530218954734));
#29850=CARTESIAN_POINT('Ctrl Pts',(-6.29031012021684,-36.710678869284,21.5286738163416));
#29851=CARTESIAN_POINT('Ctrl Pts',(-6.30363347546049,-36.7392797521074,
21.5271286779493));
#29852=CARTESIAN_POINT('Ctrl Pts',(-6.3172802545401,-36.7677104616989,21.525583539557));
#29853=CARTESIAN_POINT('Ctrl Pts',(-6.36871467403733,-36.8748652002055,
21.5197599458878));
#29854=CARTESIAN_POINT('Ctrl Pts',(-6.42491268003565,-36.979946017943,21.5139363522187));
#29855=CARTESIAN_POINT('Ctrl Pts',(-6.48568403854074,-37.0825004977269,
21.5081127585495));
#29856=CARTESIAN_POINT('Ctrl Pts',(-6.54637872494984,-37.1849255898006,
21.5022965122088));
#29857=CARTESIAN_POINT('Ctrl Pts',(-6.61163508121168,-37.2848303352914,
21.4964802658682));
#29858=CARTESIAN_POINT('Ctrl Pts',(-6.68121564602919,-37.3817840816998,
21.4906640195275));
#29859=CARTESIAN_POINT('Ctrl Pts',(-6.75072656031707,-37.4786407768727,
21.4848535952815));
#29860=CARTESIAN_POINT('Ctrl Pts',(-6.82455283531835,-37.5725520196744,
21.4790431710355));
#29861=CARTESIAN_POINT('Ctrl Pts',(-6.90241242590179,-37.6631140082228,
21.4732327467896));
#29862=CARTESIAN_POINT('Ctrl Pts',(-6.98321916307485,-37.7571039554041,
21.4672023859645));
#29863=CARTESIAN_POINT('Ctrl Pts',(-7.06837035901945,-37.8474857005277,
21.4611720251395));
#29864=CARTESIAN_POINT('Ctrl Pts',(-7.15750278192183,-37.9338429687388,
21.4551416643144));
#29865=CARTESIAN_POINT('Ctrl Pts',(-7.24328774218333,-38.0169569981856,
21.4493377800836));
#29866=CARTESIAN_POINT('Ctrl Pts',(-7.33275996413809,-38.096343076676,21.4435338958528));
#29867=CARTESIAN_POINT('Ctrl Pts',(-7.42555684708142,-38.1716663526277,
21.4377300116219));
#29868=CARTESIAN_POINT('Ctrl Pts',(-7.51834002293257,-38.2469785025258,
21.4319269846869));
#29869=CARTESIAN_POINT('Ctrl Pts',(-7.61444656619898,-38.3182287860612,
21.4261239577518));
#29870=CARTESIAN_POINT('Ctrl Pts',(-7.71348045926837,-38.3851223596574,
21.4203209308168));
#29871=CARTESIAN_POINT('Ctrl Pts',(-7.81252309599461,-38.4520218392564,
21.4145173915352));
#29872=CARTESIAN_POINT('Ctrl Pts',(-7.91449325799974,-38.5145636155634,
21.4087138522535));
#29873=CARTESIAN_POINT('Ctrl Pts',(-8.01896613726248,-38.5724963029634,
21.4029103129719));
#29874=CARTESIAN_POINT('Ctrl Pts',(-8.12347289586164,-38.6304477772583,
21.3971048916702));
#29875=CARTESIAN_POINT('Ctrl Pts',(-8.23048362888832,-38.683786992155,21.3912994703684));
#29876=CARTESIAN_POINT('Ctrl Pts',(-8.33954972603607,-38.7323089217927,
21.3854940490667));
#29877=CARTESIAN_POINT('Ctrl Pts',(-8.4487366037914,-38.7808845849763,21.3796821987982));
#29878=CARTESIAN_POINT('Ctrl Pts',(-8.5599830157061,-38.8246321483105,21.3738703485297));
#29879=CARTESIAN_POINT('Ctrl Pts',(-8.67282106268532,-38.8633950184195,
21.3680584982612));
#29880=CARTESIAN_POINT('Ctrl Pts',(-8.7857332222997,-38.9021833481896,21.3622428307383));
#29881=CARTESIAN_POINT('Ctrl Pts',(-8.90023870817414,-38.9359803492066,
21.3564271632153));
#29882=CARTESIAN_POINT('Ctrl Pts',(-9.0158567905939,-38.9646799547227,21.3506114956924));
#29883=CARTESIAN_POINT('Ctrl Pts',(-9.13164048343237,-38.9934206693247,
21.3447874978537));
#29884=CARTESIAN_POINT('Ctrl Pts',(-9.24853955488159,-39.017049334478,21.338963500015));
#29885=CARTESIAN_POINT('Ctrl Pts',(-9.36606534026731,-39.035511348911,21.3331395021762));
#29886=CARTESIAN_POINT('Ctrl Pts',(-9.39724557222105,-39.0404094220485,
21.3315943637803));
#29887=CARTESIAN_POINT('Ctrl Pts',(-9.42846990349015,-39.0449441143995,
21.3300492253844));
#29888=CARTESIAN_POINT('Ctrl Pts',(-9.45972919594527,-39.0491150216172,
21.3285040869885));
#29889=CARTESIAN_POINT('Ctrl Pts',(-9.57754480302673,-39.0648350820324,
21.3226804933035));
#29890=CARTESIAN_POINT('Ctrl Pts',(-9.69623706723093,-39.0754341682929,
21.3168568996185));
#29891=CARTESIAN_POINT('Ctrl Pts',(-9.81532332052963,-39.0808233880015,
21.3110333059335));
#29892=CARTESIAN_POINT('Ctrl Pts',(-9.93425932883225,-39.0862058084089,
21.3052170595769));
#29893=CARTESIAN_POINT('Ctrl Pts',(-10.0535879332335,-39.0863914175503,
21.2994008132203));
#29894=CARTESIAN_POINT('Ctrl Pts',(-10.172818780773,-39.0813427531895,21.2935845668637));
#29895=CARTESIAN_POINT('Ctrl Pts',(-10.2919302775763,-39.0762991425695,
21.2877741426018));
#29896=CARTESIAN_POINT('Ctrl Pts',(-10.4109438065621,-39.0660316990324,
21.2819637183399));
#29897=CARTESIAN_POINT('Ctrl Pts',(-10.5293670326174,-39.0505549675048,
21.276153294078));
#29898=CARTESIAN_POINT('Ctrl Pts',(-10.6522728223295,-39.0344924097286,
21.2701229332589));
#29899=CARTESIAN_POINT('Ctrl Pts',(-10.7745422900069,-39.0128183870614,
21.2640925724398));
#29900=CARTESIAN_POINT('Ctrl Pts',(-10.8956281649261,-38.9856085093987,
21.2580622116207));
#29901=CARTESIAN_POINT('Ctrl Pts',(-11.0121665318719,-38.9594205274418,
21.252258327374));
#29902=CARTESIAN_POINT('Ctrl Pts',(-11.127608170754,-38.9281050992437,21.2464544431272));
#29903=CARTESIAN_POINT('Ctrl Pts',(-11.2414742568698,-38.891781940131,21.2406505588804));
#29904=CARTESIAN_POINT('Ctrl Pts',(-11.3553235237461,-38.8554641463376,
21.2348475319295));
#29905=CARTESIAN_POINT('Ctrl Pts',(-11.4675973117569,-38.8141402167147,
21.2290445049786));
#29906=CARTESIAN_POINT('Ctrl Pts',(-11.5778319398096,-38.7679797464578,
21.2232414780276));
#29907=CARTESIAN_POINT('Ctrl Pts',(-11.6880763004256,-38.7218152007149,
21.2174379387301));
#29908=CARTESIAN_POINT('Ctrl Pts',(-11.7962807664614,-38.6708134230554,
21.2116343994327));
#29909=CARTESIAN_POINT('Ctrl Pts',(-11.902002221956,-38.6151919102137,21.2058308601352));
#29910=CARTESIAN_POINT('Ctrl Pts',(-12.0077579616846,-38.5595523599646,
21.2000254388177));
#29911=CARTESIAN_POINT('Ctrl Pts',(-12.1110287282994,-38.499290285125,21.1942200175002));
#29912=CARTESIAN_POINT('Ctrl Pts',(-12.2113971322542,-38.4346685027027,
21.1884145961827));
#29913=CARTESIAN_POINT('Ctrl Pts',(-12.3118766849232,-38.3699751576396,
21.1826027458986));
#29914=CARTESIAN_POINT('Ctrl Pts',(-12.4094471157842,-38.3009126891299,
21.1767908956145));
#29915=CARTESIAN_POINT('Ctrl Pts',(-12.5037209694124,-38.2277865956913,
21.1709790453304));
#29916=CARTESIAN_POINT('Ctrl Pts',(-12.598056742612,-38.1546124726434,21.1651633777919));
#29917=CARTESIAN_POINT('Ctrl Pts',(-12.6890913158667,-38.077369672845,21.1593477102534));
#29918=CARTESIAN_POINT('Ctrl Pts',(-12.7764724594871,-37.9964021228316,
21.153532042715));
#29919=CARTESIAN_POINT('Ctrl Pts',(-12.8639787671569,-37.9153185955488,
21.147708044861));
#29920=CARTESIAN_POINT('Ctrl Pts',(-12.9478209140806,-37.8304999584517,
21.1418840470069));
#29921=CARTESIAN_POINT('Ctrl Pts',(-13.0276853651523,-37.7423249861463,
21.1360600491529));
#29922=CARTESIAN_POINT('Ctrl Pts',(-13.0488738375391,-37.7189316873654,
21.1345149109086));
#29923=CARTESIAN_POINT('Ctrl Pts',(-13.0697825624144,-37.6953023131244,
21.1329697726644));
#29924=CARTESIAN_POINT('Ctrl Pts',(-13.0904061924061,-37.6714442846405,
21.1314246344201));
#29925=CARTESIAN_POINT('Ctrl Pts',(-13.1692726209871,-37.5802092547126,
21.125515900844));
#29926=CARTESIAN_POINT('Ctrl Pts',(-13.2442376687118,-37.4853140263686,
21.119607167268));
#29927=CARTESIAN_POINT('Ctrl Pts',(-13.314940660894,-37.3871307912956,21.113698433692));
#29928=CARTESIAN_POINT('Ctrl Pts',(-13.3839459164573,-37.2913051547967,
21.1079315819947));
#29929=CARTESIAN_POINT('Ctrl Pts',(-13.4488911827427,-37.1923479648596,
21.1021647302974));
#29930=CARTESIAN_POINT('Ctrl Pts',(-13.5094788137209,-37.0906418765642,
21.0963978786002));
#29931=CARTESIAN_POINT('Ctrl Pts',(-13.5700104610653,-36.9890297658072,
21.090636355537));
#29932=CARTESIAN_POINT('Ctrl Pts',(-13.6261922654264,-36.8846741604791,
21.0848748324737));
#29933=CARTESIAN_POINT('Ctrl Pts',(-13.6777687647333,-36.777988164514,21.0791133094105));
#29934=CARTESIAN_POINT('Ctrl Pts',(-13.7293102997855,-36.6713744921147,
21.0733556921448));
#29935=CARTESIAN_POINT('Ctrl Pts',(-13.7762525571488,-36.5624339432972,
21.067598074879));
#29936=CARTESIAN_POINT('Ctrl Pts',(-13.8183854556858,-36.4516051501037,
21.0618404576133));
#29937=CARTESIAN_POINT('Ctrl Pts',(-13.8624295242089,-36.3357491057475,
21.0558216718618));
#29938=CARTESIAN_POINT('Ctrl Pts',(-13.9012174237302,-36.2178298958137,
21.0498028861103));
#29939=CARTESIAN_POINT('Ctrl Pts',(-13.9345650358115,-36.0983728779288,
21.0437841003588));
#29940=CARTESIAN_POINT('Ctrl Pts',(-13.9664521067682,-35.9841477755052,
21.0380289222111));
#29941=CARTESIAN_POINT('Ctrl Pts',(-13.9933652579074,-35.8685171612166,
21.0322737440633));
#29942=CARTESIAN_POINT('Ctrl Pts',(-14.0151946311413,-35.7519555000491,
21.0265185659155));
#29943=CARTESIAN_POINT('Ctrl Pts',(-14.0370247942173,-35.6353896213848,
21.0207631795308));
#29944=CARTESIAN_POINT('Ctrl Pts',(-14.0537707443996,-35.517893038846,21.0150077931461));
#29945=CARTESIAN_POINT('Ctrl Pts',(-14.0653740111778,-35.3999489332902,
21.0092524067614));
#29946=CARTESIAN_POINT('Ctrl Pts',(-14.0769833472101,-35.2819431353887,
21.0034940099398));
#29947=CARTESIAN_POINT('Ctrl Pts',(-14.0834446009025,-35.1634897617954,
20.9977356131181));
#29948=CARTESIAN_POINT('Ctrl Pts',(-14.0847513050877,-35.0450752214036,
20.9919772162965));
#29949=CARTESIAN_POINT('Ctrl Pts',(-14.0849299821657,-35.0288833668764,
20.9911898203962));
#29950=CARTESIAN_POINT('Ctrl Pts',(-14.0850123618426,-35.0126922365669,
20.9904024244958));
#29951=CARTESIAN_POINT('Ctrl Pts',(-14.0849985032417,-34.9965030709352,
20.9896150285955));
#29952=CARTESIAN_POINT('Origin',(-10.,-35.,32.7603849714045));
#29953=CARTESIAN_POINT('',(-7.5128274573098,-31.7594448403263,23.0467784921743));
#29954=CARTESIAN_POINT('',(-7.5128274573098,-31.7594448403263,22.9427600101556));
#29955=CARTESIAN_POINT('',(-7.5128274573098,-31.7594448403263,32.7603849714045));
#29956=CARTESIAN_POINT('',(-14.084999774902,-34.998643884102,22.1353849714381));
#29957=CARTESIAN_POINT('Ctrl Pts',(-7.5128274573098,-31.7594448403263,22.9427600101556));
#29958=CARTESIAN_POINT('Ctrl Pts',(-7.41810522499216,-31.8321455115984,
22.9369372163922));
#29959=CARTESIAN_POINT('Ctrl Pts',(-7.32667862096095,-31.9089218128983,
22.9311144226289));
#29960=CARTESIAN_POINT('Ctrl Pts',(-7.23889864961535,-31.9894279060444,
22.9252916288655));
#29961=CARTESIAN_POINT('Ctrl Pts',(-7.1740346877293,-32.0489169224724,22.9209889449281));
#29962=CARTESIAN_POINT('Ctrl Pts',(-7.11116115321496,-32.1104417111689,
22.9166862609907));
#29963=CARTESIAN_POINT('Ctrl Pts',(-7.05040557842172,-32.1738510746611,
22.9123835770532));
#29964=CARTESIAN_POINT('Ctrl Pts',(-6.96817416518498,-32.2596743359857,
22.9065599833816));
#29965=CARTESIAN_POINT('Ctrl Pts',(-6.88955900838773,-32.3492279583017,
22.9007363897099));
#29966=CARTESIAN_POINT('Ctrl Pts',(-6.81491676329803,-32.4421747957923,
22.8949127960382));
#29967=CARTESIAN_POINT('Ctrl Pts',(-6.74036869048768,-32.5350043670414,
22.8890965496949));
#29968=CARTESIAN_POINT('Ctrl Pts',(-6.66978381322937,-32.6312183229924,
22.8832803033517));
#29969=CARTESIAN_POINT('Ctrl Pts',(-6.60348180785171,-32.7304429572259,
22.8774640570084));
#29970=CARTESIAN_POINT('Ctrl Pts',(-6.53724617114727,-32.8295682670529,
22.8716536327598));
#29971=CARTESIAN_POINT('Ctrl Pts',(-6.47528510307415,-32.9316979222035,
22.8658432085113));
#29972=CARTESIAN_POINT('Ctrl Pts',(-6.41787746912875,-33.0364259184272,
22.8600327842627));
#29973=CARTESIAN_POINT('Ctrl Pts',(-6.35829683750231,-33.1451180859168,
22.8540024234386));
#29974=CARTESIAN_POINT('Ctrl Pts',(-6.30362144545683,-33.2566088367515,
22.8479720626146));
#29975=CARTESIAN_POINT('Ctrl Pts',(-6.25411329246123,-33.3704117776922,
22.8419417017905));
#29976=CARTESIAN_POINT('Ctrl Pts',(-6.20646447061099,-33.4799407285985,
22.836137817557));
#29977=CARTESIAN_POINT('Ctrl Pts',(-6.16360194235758,-33.5916109199821,
22.8303339333235));
#29978=CARTESIAN_POINT('Ctrl Pts',(-6.12571170368782,-33.7049651753491,
22.8245300490901));
#29979=CARTESIAN_POINT('Ctrl Pts',(-6.08782706181152,-33.8183026870804,
22.8187270221524));
#29980=CARTESIAN_POINT('Ctrl Pts',(-6.05491337832605,-33.933323380932,22.8129239952147));
#29981=CARTESIAN_POINT('Ctrl Pts',(-6.02710744688961,-34.0495528623643,
22.807120968277));
#29982=CARTESIAN_POINT('Ctrl Pts',(-5.9992990604802,-34.1657926056442,22.8013174289927));
#29983=CARTESIAN_POINT('Ctrl Pts',(-5.97659941775086,-34.2832409515463,
22.7955138897084));
#29984=CARTESIAN_POINT('Ctrl Pts',(-5.95909450684952,-34.401411831535,22.7897103504241));
#29985=CARTESIAN_POINT('Ctrl Pts',(-5.94158391930971,-34.519621032962,22.7839049291197));
#29986=CARTESIAN_POINT('Ctrl Pts',(-5.92927147367318,-34.6385528307428,
22.7780995078153));
#29987=CARTESIAN_POINT('Ctrl Pts',(-5.92219138970122,-34.7577151722184,
22.7722940865109));
#29988=CARTESIAN_POINT('Ctrl Pts',(-5.9151034651916,-34.8770094749575,22.7664822362398));
#29989=CARTESIAN_POINT('Ctrl Pts',(-5.91325949261094,-34.996534423144,22.7606703859686));
#29990=CARTESIAN_POINT('Ctrl Pts',(-5.91664156972958,-35.1157969340679,
22.7548585356975));
#29991=CARTESIAN_POINT('Ctrl Pts',(-5.92002586821463,-35.2351377772491,
22.7490428681719));
#29992=CARTESIAN_POINT('Ctrl Pts',(-5.92864302289948,-35.3542154335524,
22.7432272006463));
#29993=CARTESIAN_POINT('Ctrl Pts',(-5.9424233196004,-35.4725425723439,22.7374115331207));
#29994=CARTESIAN_POINT('Ctrl Pts',(-5.95622335508832,-35.5910392019845,
22.7315875352794));
#29995=CARTESIAN_POINT('Ctrl Pts',(-5.975201229148,-35.7087827666983,22.725763537438));
#29996=CARTESIAN_POINT('Ctrl Pts',(-5.999236257892,-35.8252966011283,22.7199395395967));
#29997=CARTESIAN_POINT('Ctrl Pts',(-6.00561288201903,-35.8562083564531,
22.7183944012261));
#29998=CARTESIAN_POINT('Ctrl Pts',(-6.01234519332932,-35.8870336423358,
22.7168492628555));
#29999=CARTESIAN_POINT('Ctrl Pts',(-6.01943035767116,-35.9177637618527,
22.7153041244849));
#30000=CARTESIAN_POINT('Ctrl Pts',(-6.04613419145459,-36.0335849290314,
22.7094805308136));
#30001=CARTESIAN_POINT('Ctrl Pts',(-6.07794029159739,-36.1484264116932,
22.7036569371423));
#30002=CARTESIAN_POINT('Ctrl Pts',(-6.11476218449411,-36.2618051026062,
22.6978333434711));
#30003=CARTESIAN_POINT('Ctrl Pts',(-6.15153762110352,-36.3750407494597,
22.6920170971283));
#30004=CARTESIAN_POINT('Ctrl Pts',(-6.19331613887172,-36.486816890333,22.6862008507854));
#30005=CARTESIAN_POINT('Ctrl Pts',(-6.23996041545217,-36.5966613049214,
22.6803846044426));
#30006=CARTESIAN_POINT('Ctrl Pts',(-6.28655800085441,-36.7063957646448,
22.6745741801945));
#30007=CARTESIAN_POINT('Ctrl Pts',(-6.33801149682606,-36.8142019711841,
22.6687637559463));
#30008=CARTESIAN_POINT('Ctrl Pts',(-6.39413419703498,-36.9196241327425,
22.6629533316982));
#30009=CARTESIAN_POINT('Ctrl Pts',(-6.45238125753123,-37.0290367411715,
22.6569229708739));
#30010=CARTESIAN_POINT('Ctrl Pts',(-6.5156578460597,-37.1358808302093,22.6508926100497));
#30011=CARTESIAN_POINT('Ctrl Pts',(-6.58370077591591,-37.2396706480022,
22.6448622492255));
#30012=CARTESIAN_POINT('Ctrl Pts',(-6.64918828143554,-37.3395625292006,
22.6390583649924));
#30013=CARTESIAN_POINT('Ctrl Pts',(-6.71909033052298,-37.4366250425797,
22.6332544807594));
#30014=CARTESIAN_POINT('Ctrl Pts',(-6.79312651017591,-37.5304520189609,
22.6274505965263));
#30015=CARTESIAN_POINT('Ctrl Pts',(-6.86715175389339,-37.6242651360944,
22.6216475695891));
#30016=CARTESIAN_POINT('Ctrl Pts',(-6.94530966089996,-37.7148433461959,
22.6158445426518));
#30017=CARTESIAN_POINT('Ctrl Pts',(-7.02727844659211,-37.8018121931893,
22.6100415157145));
#30018=CARTESIAN_POINT('Ctrl Pts',(-7.10925446927085,-37.8887887186224,
22.6042379764306));
#30019=CARTESIAN_POINT('Ctrl Pts',(-7.19504175951718,-37.9721549501883,
22.5984344371467));
#30020=CARTESIAN_POINT('Ctrl Pts',(-7.28428091920406,-38.0515725248142,
22.5926308978629));
#30021=CARTESIAN_POINT('Ctrl Pts',(-7.37354901810982,-38.1310158536335,
22.5868254765589));
#30022=CARTESIAN_POINT('Ctrl Pts',(-7.46627090781355,-38.2065077075568,
22.5810200552549));
#30023=CARTESIAN_POINT('Ctrl Pts',(-7.56205380769615,-38.2777497408178,
22.5752146339509));
#30024=CARTESIAN_POINT('Ctrl Pts',(-7.65794277827479,-38.3490706680365,
22.5694027836801));
#30025=CARTESIAN_POINT('Ctrl Pts',(-7.7568991974959,-38.4161321366073,22.5635909334094));
#30026=CARTESIAN_POINT('Ctrl Pts',(-7.85850085185827,-38.4786788294564,
22.5577790831387));
#30027=CARTESIAN_POINT('Ctrl Pts',(-7.96016923873276,-38.5412666033093,
22.5519634156135));
#30028=CARTESIAN_POINT('Ctrl Pts',(-8.06448596486752,-38.599333497768,22.5461477480883));
#30029=CARTESIAN_POINT('Ctrl Pts',(-8.17100522620586,-38.6526706828612,
22.540332080563));
#30030=CARTESIAN_POINT('Ctrl Pts',(-8.27767706488404,-38.7060842677126,
22.5345080827221));
#30031=CARTESIAN_POINT('Ctrl Pts',(-8.38655736429783,-38.7547544550232,
22.5286840848811));
#30032=CARTESIAN_POINT('Ctrl Pts',(-8.4971813007853,-38.7985208907272,22.5228600870402));
#30033=CARTESIAN_POINT('Ctrl Pts',(-8.52653043416117,-38.8101323646961,
22.5213149486656));
#30034=CARTESIAN_POINT('Ctrl Pts',(-8.55600222174986,-38.8213989527676,
22.519769810291));
#30035=CARTESIAN_POINT('Ctrl Pts',(-8.58558783611663,-38.8323182580076,
22.5182246719164));
#30036=CARTESIAN_POINT('Ctrl Pts',(-8.69709538742309,-38.8734728872202,
22.5124010782454));
#30037=CARTESIAN_POINT('Ctrl Pts',(-8.81058043544505,-38.9098231007045,
22.5065774845743));
#30038=CARTESIAN_POINT('Ctrl Pts',(-8.92559152155281,-38.9411764007008,
22.5007538909033));
#30039=CARTESIAN_POINT('Ctrl Pts',(-9.04045750409189,-38.972490143852,22.4949376445607));
#30040=CARTESIAN_POINT('Ctrl Pts',(-9.15684530480536,-38.9988194062653,
22.4891213982181));
#30041=CARTESIAN_POINT('Ctrl Pts',(-9.27428469714738,-39.0200201864177,
22.4833051518755));
#30042=CARTESIAN_POINT('Ctrl Pts',(-9.39160653200965,-39.0411997444721,
22.4774947276276));
#30043=CARTESIAN_POINT('Ctrl Pts',(-9.50997746485374,-39.0572609608792,
22.4716843033797));
#30044=CARTESIAN_POINT('Ctrl Pts',(-9.62891393896168,-39.068110142966,22.4658738791318));
#30045=CARTESIAN_POINT('Ctrl Pts',(-9.75235240462994,-39.079369989036,22.4598435183075));
#30046=CARTESIAN_POINT('Ctrl Pts',(-9.87639963886841,-39.0850153142075,
22.4538131574831));
#30047=CARTESIAN_POINT('Ctrl Pts',(-10.0005051034775,-39.0849999687724,
22.4477827966588));
#30048=CARTESIAN_POINT('Ctrl Pts',(-10.1199496558406,-39.0849851996514,
22.441978912426));
#30049=CARTESIAN_POINT('Ctrl Pts',(-10.2394476985915,-39.0797272772861,
22.4361750281932));
#30050=CARTESIAN_POINT('Ctrl Pts',(-10.3585058113548,-39.0692380838708,
22.4303711439604));
#30051=CARTESIAN_POINT('Ctrl Pts',(-10.4775463379617,-39.0587504398216,
22.4245681170234));
#30052=CARTESIAN_POINT('Ctrl Pts',(-10.5961466571589,-39.0430330972343,
22.4187650900863));
#30053=CARTESIAN_POINT('Ctrl Pts',(-10.7138171940898,-39.0221499242845,
22.4129620631493));
#30054=CARTESIAN_POINT('Ctrl Pts',(-10.8314981200985,-39.0012649075689,
22.4071585238657));
#30055=CARTESIAN_POINT('Ctrl Pts',(-10.9482486985517,-38.9752132250327,
22.401354984582));
#30056=CARTESIAN_POINT('Ctrl Pts',(-11.0635889233761,-38.944109988587,22.3955514452984));
#30057=CARTESIAN_POINT('Ctrl Pts',(-11.1789665516905,-38.9129966657244,
22.3897460239947));
#30058=CARTESIAN_POINT('Ctrl Pts',(-11.292932522737,-38.8768286372834,22.3839406026909));
#30059=CARTESIAN_POINT('Ctrl Pts',(-11.4050220006962,-38.8357708713581,
22.3781351813872));
#30060=CARTESIAN_POINT('Ctrl Pts',(-11.5172356073774,-38.7946676377574,
22.3723233311167));
#30061=CARTESIAN_POINT('Ctrl Pts',(-11.6275681893694,-38.7486639985343,
22.3665114808462));
#30062=CARTESIAN_POINT('Ctrl Pts',(-11.735574764776,-38.6979731253584,22.3606996305757));
#30063=CARTESIAN_POINT('Ctrl Pts',(-11.8436522794811,-38.6472489581448,
22.3548839630508));
#30064=CARTESIAN_POINT('Ctrl Pts',(-11.9494003842303,-38.5918316149719,
22.3490682955258));
#30065=CARTESIAN_POINT('Ctrl Pts',(-12.0524000461147,-38.531979480505,22.3432526280009));
#30066=CARTESIAN_POINT('Ctrl Pts',(-12.1555472438929,-38.4720416143183,
22.3374286301602));
#30067=CARTESIAN_POINT('Ctrl Pts',(-12.2559377985724,-38.4076564975345,
22.3316046323195));
#30068=CARTESIAN_POINT('Ctrl Pts',(-12.3531827952385,-38.339124994994,22.3257806344788));
#30069=CARTESIAN_POINT('Ctrl Pts',(-12.3789824229897,-38.3209432137672,
22.3242354961018));
#30070=CARTESIAN_POINT('Ctrl Pts',(-12.4045608326993,-38.302469794208,22.3226903577249));
#30071=CARTESIAN_POINT('Ctrl Pts',(-12.4299111807624,-38.283710805416,22.321145219348));
#30072=CARTESIAN_POINT('Ctrl Pts',(-12.5246533662664,-38.2136025926385,
22.3153705535969));
#30073=CARTESIAN_POINT('Ctrl Pts',(-12.6165244936633,-38.1392680574621,
22.3095958878458));
#30074=CARTESIAN_POINT('Ctrl Pts',(-12.705119863426,-38.0609723168461,22.3038212220948));
#30075=CARTESIAN_POINT('Ctrl Pts',(-12.7936030129361,-37.9827757503496,
22.2980538708845));
#30076=CARTESIAN_POINT('Ctrl Pts',(-12.8788183458607,-37.9006282274634,
22.2922865196743));
#30077=CARTESIAN_POINT('Ctrl Pts',(-12.9603911014523,-37.8148373889875,
22.286519168464));
#30078=CARTESIAN_POINT('Ctrl Pts',(-13.0418827354362,-37.7291318668737,
22.280757552708));
#30079=CARTESIAN_POINT('Ctrl Pts',(-13.1197387110851,-37.6397905343191,
22.2749959369519));
#30080=CARTESIAN_POINT('Ctrl Pts',(-13.1936188085971,-37.5471599685483,
22.2692343211959));
#30081=CARTESIAN_POINT('Ctrl Pts',(-13.2674469120441,-37.4545945927248,
22.2634767602507));
#30082=CARTESIAN_POINT('Ctrl Pts',(-13.3373044441074,-37.3587449120252,
22.2577191993056));
#30083=CARTESIAN_POINT('Ctrl Pts',(-13.4028898721003,-37.2599923713051,
22.2519616383604));
#30084=CARTESIAN_POINT('Ctrl Pts',(-13.4684512490783,-37.1612760444041,
22.2462061887865));
#30085=CARTESIAN_POINT('Ctrl Pts',(-13.5297434061283,-37.0596593195178,
22.2404507392125));
#30086=CARTESIAN_POINT('Ctrl Pts',(-13.586507122281,-36.955554054949,22.2346952896386));
#30087=CARTESIAN_POINT('Ctrl Pts',(-13.6432640019227,-36.851461328615,22.2289405332397));
#30088=CARTESIAN_POINT('Ctrl Pts',(-13.6954933261915,-36.7448810238551,
22.2231857768409));
#30089=CARTESIAN_POINT('Ctrl Pts',(-13.7429813543258,-36.63625046407,22.217431020442));
#30090=CARTESIAN_POINT('Ctrl Pts',(-13.7904753584461,-36.5276062340037,
22.2116755398534));
#30091=CARTESIAN_POINT('Ctrl Pts',(-13.8332267144446,-36.4169116175228,
22.2059200592648));
#30092=CARTESIAN_POINT('Ctrl Pts',(-13.8710697362876,-36.3046241208862,
22.2001645786762));
#30093=CARTESIAN_POINT('Ctrl Pts',(-13.9089487815479,-36.1922297358682,
22.1944036193476));
#30094=CARTESIAN_POINT('Ctrl Pts',(-13.9419100289835,-36.0782398375382,
22.1886426600189));
#30095=CARTESIAN_POINT('Ctrl Pts',(-13.9698376062256,-35.9631273956215,
22.1828817006903));
#30096=CARTESIAN_POINT('Ctrl Pts',(-13.9977791248229,-35.8479574899511,
22.1771178655096));
#30097=CARTESIAN_POINT('Ctrl Pts',(-14.0206818886153,-35.7316643327201,
22.171354030329));
#30098=CARTESIAN_POINT('Ctrl Pts',(-14.0384814547981,-35.6147296472856,
22.1655901951483));
#30099=CARTESIAN_POINT('Ctrl Pts',(-14.0563077963075,-35.4976190606882,
22.159817689612));
#30100=CARTESIAN_POINT('Ctrl Pts',(-14.0690155630157,-35.3798654318944,
22.1540451840757));
#30101=CARTESIAN_POINT('Ctrl Pts',(-14.0765923082484,-35.2619544852256,
22.1482726785393));
#30102=CARTESIAN_POINT('Ctrl Pts',(-14.0822309269687,-35.1742050821785,
22.1439767761723));
#30103=CARTESIAN_POINT('Ctrl Pts',(-14.085028897281,-35.0863686218627,22.1396808738052));
#30104=CARTESIAN_POINT('Ctrl Pts',(-14.084999774902,-34.998643884102,22.1353849714381));
#30105=CARTESIAN_POINT('Ctrl Pts',(-14.0849997749018,-34.9986438834154,
22.1353849714045));
#30106=CARTESIAN_POINT('Ctrl Pts',(-14.0849741968582,-34.9215957126599,
22.1316119031962));
#30107=CARTESIAN_POINT('Ctrl Pts',(-14.0827689216963,-34.8445868960997,
22.1278388349879));
#30108=CARTESIAN_POINT('Ctrl Pts',(-14.0783897720535,-34.7677030624194,
22.1240657667795));
#30109=CARTESIAN_POINT('Ctrl Pts',(-14.0716307137146,-34.6490356590298,
22.1182421731102));
#30110=CARTESIAN_POINT('Ctrl Pts',(-14.0596772245187,-34.5304721392025,
22.1124185794409));
#30111=CARTESIAN_POINT('Ctrl Pts',(-14.0425329433292,-34.4125032748195,
22.1065949857715));
#30112=CARTESIAN_POINT('Ctrl Pts',(-14.025410292197,-34.2946832456818,22.1007787394306));
#30113=CARTESIAN_POINT('Ctrl Pts',(-14.0031099329978,-34.1774567802964,
22.0949624930897));
#30114=CARTESIAN_POINT('Ctrl Pts',(-13.9756874615845,-34.0613125079135,
22.0891462467488));
#30115=CARTESIAN_POINT('Ctrl Pts',(-13.9482924402164,-33.9452844965879,
22.0833358225026));
#30116=CARTESIAN_POINT('Ctrl Pts',(-13.9157855999802,-33.8303369183369,
22.0775253982564));
#30117=CARTESIAN_POINT('Ctrl Pts',(-13.8782739859287,-33.7169505504195,
22.0717149740101));
#30118=CARTESIAN_POINT('Ctrl Pts',(-13.8393424796786,-33.5992722738948,
22.0656846131852));
#30119=CARTESIAN_POINT('Ctrl Pts',(-13.7950198958776,-33.4832761765968,
22.0596542523602));
#30120=CARTESIAN_POINT('Ctrl Pts',(-13.7454836013007,-33.3694854823133,
22.0536238915353));
#30121=CARTESIAN_POINT('Ctrl Pts',(-13.697807694782,-33.2599683181874,22.0478200073041));
#30122=CARTESIAN_POINT('Ctrl Pts',(-13.6453028057686,-33.1524942999704,
22.0420161230729));
#30123=CARTESIAN_POINT('Ctrl Pts',(-13.5881767206801,-33.0475111213712,
22.0362122388418));
#30124=CARTESIAN_POINT('Ctrl Pts',(-13.5310590737252,-32.9425434499099,
22.0304092119063));
#30125=CARTESIAN_POINT('Ctrl Pts',(-13.4693217832893,-32.84006624496,22.0246061849709));
#30126=CARTESIAN_POINT('Ctrl Pts',(-13.4032187691399,-32.7405029299922,
22.0188031580355));
#30127=CARTESIAN_POINT('Ctrl Pts',(-13.3371099187855,-32.6409308246247,
22.0129996187535));
#30128=CARTESIAN_POINT('Ctrl Pts',(-13.266634804225,-32.5442734609492,22.0071960794715));
#30129=CARTESIAN_POINT('Ctrl Pts',(-13.1920905142082,-32.4509250405094,
22.0013925401894));
#30130=CARTESIAN_POINT('Ctrl Pts',(-13.1175220503471,-32.357546348265,21.9955871188873));
#30131=CARTESIAN_POINT('Ctrl Pts',(-13.0388820413454,-32.2674790522316,
21.9897816975851));
#30132=CARTESIAN_POINT('Ctrl Pts',(-12.9565072374636,-32.1810835495132,
21.983976276283));
#30133=CARTESIAN_POINT('Ctrl Pts',(-12.8740412111105,-32.0945923717715,
21.978164426014));
#30134=CARTESIAN_POINT('Ctrl Pts',(-12.7878324161339,-32.0117813994789,
21.9723525757451));
#30135=CARTESIAN_POINT('Ctrl Pts',(-12.698253880029,-31.9329735901189,21.9665407254761));
#30136=CARTESIAN_POINT('Ctrl Pts',(-12.6086165082604,-31.8541140193662,
21.9607250579527));
#30137=CARTESIAN_POINT('Ctrl Pts',(-12.51560530498,-31.7792631032794,21.9549093904292));
#30138=CARTESIAN_POINT('Ctrl Pts',(-12.4196244006124,-31.7087019642759,
21.9490937229058));
#30139=CARTESIAN_POINT('Ctrl Pts',(-12.3235060139627,-31.6380397540596,
21.9432697250666));
#30140=CARTESIAN_POINT('Ctrl Pts',(-12.2244097740045,-31.5716798116975,
21.9374457272273));
#30141=CARTESIAN_POINT('Ctrl Pts',(-12.1227667446957,-31.5098586923143,
21.9316217293881));
#30142=CARTESIAN_POINT('Ctrl Pts',(-12.0958002946327,-31.4934572121535,
21.9300765909958));
#30143=CARTESIAN_POINT('Ctrl Pts',(-12.0686547041485,-31.4773749483047,
21.9285314526034));
#30144=CARTESIAN_POINT('Ctrl Pts',(-12.0413382690486,-31.4616157541446,
21.9269863142111));
#30145=CARTESIAN_POINT('Ctrl Pts',(-11.9383832073534,-31.4022196872316,
21.9211627205419));
#30146=CARTESIAN_POINT('Ctrl Pts',(-11.8326676330743,-31.3472250375885,
21.9153391268728));
#30147=CARTESIAN_POINT('Ctrl Pts',(-11.7246040083446,-31.2968977850454,
21.9095155332036));
#30148=CARTESIAN_POINT('Ctrl Pts',(-11.6166767219297,-31.2466340278071,
21.903699286863));
#30149=CARTESIAN_POINT('Ctrl Pts',(-11.5064076441365,-31.2010261262243,
21.8978830405223));
#30150=CARTESIAN_POINT('Ctrl Pts',(-11.3942359259922,-31.1602954302873,
21.8920667941816));
#30151=CARTESIAN_POINT('Ctrl Pts',(-11.2821764923571,-31.1196055060018,
21.8862563699356));
#30152=CARTESIAN_POINT('Ctrl Pts',(-11.1682185888553,-31.0837832135761,
21.8804459456896));
#30153=CARTESIAN_POINT('Ctrl Pts',(-11.0528230019126,-31.053002568199,21.8746355214437));
#30154=CARTESIAN_POINT('Ctrl Pts',(-10.9330594532589,-31.0210568117114,
21.8686051606186));
#30155=CARTESIAN_POINT('Ctrl Pts',(-10.8117476384181,-30.9945421063119,
21.8625747997936));
#30156=CARTESIAN_POINT('Ctrl Pts',(-10.689422392675,-30.9735969197709,21.8565444389685));
#30157=CARTESIAN_POINT('Ctrl Pts',(-10.571691201226,-30.9534383519167,21.8507405547377));
#30158=CARTESIAN_POINT('Ctrl Pts',(-10.4530217657443,-30.9384385838515,
21.8449366705069));
#30159=CARTESIAN_POINT('Ctrl Pts',(-10.3339024252768,-30.9286692383946,
21.8391327862761));
#30160=CARTESIAN_POINT('Ctrl Pts',(-10.21480068001,-30.9189013359745,21.833329759341));
#30161=CARTESIAN_POINT('Ctrl Pts',(-10.0952495687778,-30.9143623530944,
21.827526732406));
#30162=CARTESIAN_POINT('Ctrl Pts',(-9.97574242032107,-30.9150720239118,
21.8217237054709));
#30163=CARTESIAN_POINT('Ctrl Pts',(-9.85622472063311,-30.9157817573857,
21.8159201661893));
#30164=CARTESIAN_POINT('Ctrl Pts',(-9.73675139978788,-30.9217410634859,
21.8101166269077));
#30165=CARTESIAN_POINT('Ctrl Pts',(-9.61781500981382,-30.9329175526827,
21.8043130876261));
#30166=CARTESIAN_POINT('Ctrl Pts',(-9.49884005015554,-30.9440976662846,
21.7985076663243));
#30167=CARTESIAN_POINT('Ctrl Pts',(-9.38040277399139,-30.9604982895504,
21.7927022450226));
#30168=CARTESIAN_POINT('Ctrl Pts',(-9.26298920128755,-30.9820353308446,
21.7868968237208));
#30169=CARTESIAN_POINT('Ctrl Pts',(-9.14544560391974,-31.0035962224185,
21.7810849734524));
#30170=CARTESIAN_POINT('Ctrl Pts',(-9.02892837476259,-31.0303048122552,
21.7752731231839));
#30171=CARTESIAN_POINT('Ctrl Pts',(-8.9139121062226,-31.0620261444507,21.7694612729154));
#30172=CARTESIAN_POINT('Ctrl Pts',(-8.79882029437999,-31.0937683113873,
21.7636456053925));
#30173=CARTESIAN_POINT('Ctrl Pts',(-8.68523179408255,-31.1305296521297,
21.7578299378695));
#30174=CARTESIAN_POINT('Ctrl Pts',(-8.57360325758762,-31.1721262647215,
21.7520142703466));
#30175=CARTESIAN_POINT('Ctrl Pts',(-8.46181482526753,-31.2137824599693,
21.7461902725079));
#30176=CARTESIAN_POINT('Ctrl Pts',(-8.35199233491958,-31.260287592335,21.7403662746692));
#30177=CARTESIAN_POINT('Ctrl Pts',(-8.24456992798524,-31.3114108032655,
21.7345422768305));
#30178=CARTESIAN_POINT('Ctrl Pts',(-8.21607017744642,-31.3249740699977,
21.7329971384346));
#30179=CARTESIAN_POINT('Ctrl Pts',(-8.18773921196682,-31.338862147366,21.7314520000386));
#30180=CARTESIAN_POINT('Ctrl Pts',(-8.15958480185818,-31.353070209279,21.7299068616426));
#30181=CARTESIAN_POINT('Ctrl Pts',(-8.05345316483866,-31.4066293093942,
21.7240822655402));
#30182=CARTESIAN_POINT('Ctrl Pts',(-7.94949028075317,-31.4649115462035,
21.7182576694377));
#30183=CARTESIAN_POINT('Ctrl Pts',(-7.84814493422774,-31.5277176416786,
21.7124330733352));
#30184=CARTESIAN_POINT('Ctrl Pts',(-7.74693946603362,-31.590437051261,21.7066165164256));
#30185=CARTESIAN_POINT('Ctrl Pts',(-7.64834469086719,-31.6576676818168,
21.700799959516));
#30186=CARTESIAN_POINT('Ctrl Pts',(-7.55278652953408,-31.7291635274795,
21.6949834026064));
#30187=CARTESIAN_POINT('Ctrl Pts',(-7.53940697095604,-31.7391740053057,
21.6941689984486));
#30188=CARTESIAN_POINT('Ctrl Pts',(-7.52608690363846,-31.7492680251774,
21.6933545942909));
#30189=CARTESIAN_POINT('Ctrl Pts',(-7.5128274573098,-31.7594448403263,21.6925401901332));
#30190=CARTESIAN_POINT('',(-14.0849992774348,-35.002429682444,22.2396150286382));
#30191=CARTESIAN_POINT('Ctrl Pts',(-14.0849992774354,-35.0024296815638,
22.2396150285955));
#30192=CARTESIAN_POINT('Ctrl Pts',(-14.085070989627,-34.8818606921073,22.233766442302));
#30193=CARTESIAN_POINT('Ctrl Pts',(-14.0798004648248,-34.7612723331048,
22.2279178560085));
#30194=CARTESIAN_POINT('Ctrl Pts',(-14.0692091476505,-34.6411658981124,
22.2220692697149));
#30195=CARTESIAN_POINT('Ctrl Pts',(-14.0586166826974,-34.5210464472109,
22.2162200496114));
#30196=CARTESIAN_POINT('Ctrl Pts',(-14.0427023124912,-34.4014094220384,
22.2103708295078));
#30197=CARTESIAN_POINT('Ctrl Pts',(-14.0215393834306,-34.2827510979325,
22.2045216094042));
#30198=CARTESIAN_POINT('Ctrl Pts',(-14.0003694708715,-34.1640536180835,
22.1986704591321));
#30199=CARTESIAN_POINT('Ctrl Pts',(-13.9739476225001,-34.0463358750017,
22.19281930886));
#30200=CARTESIAN_POINT('Ctrl Pts',(-13.9423982256987,-33.9300835406406,
22.1869681585879));
#30201=CARTESIAN_POINT('Ctrl Pts',(-13.9108091820572,-33.8136851167132,
22.1811096554139));
#30202=CARTESIAN_POINT('Ctrl Pts',(-13.8740798226738,-33.6987561662509,
22.1752511522399));
#30203=CARTESIAN_POINT('Ctrl Pts',(-13.832384485157,-33.5857672900376,22.169392649066));
#30204=CARTESIAN_POINT('Ctrl Pts',(-13.7906628672974,-33.4727071975545,
22.1635304533095));
#30205=CARTESIAN_POINT('Ctrl Pts',(-13.7439691883523,-33.3615899841287,
22.1576682575531));
#30206=CARTESIAN_POINT('Ctrl Pts',(-13.6925253126231,-33.2528646830776,
22.1518060617967));
#30207=CARTESIAN_POINT('Ctrl Pts',(-13.6409886366956,-33.143943251207,22.145933291158));
#30208=CARTESIAN_POINT('Ctrl Pts',(-13.5846848248018,-33.0374227087693,
22.1400605205193));
#30209=CARTESIAN_POINT('Ctrl Pts',(-13.5238813533309,-32.9337267345176,
22.1341877498806));
#30210=CARTESIAN_POINT('Ctrl Pts',(-13.4639491572571,-32.8315166581756,
22.1283991323412));
#30211=CARTESIAN_POINT('Ctrl Pts',(-13.3996456789967,-32.7320509915328,
22.1226105148018));
#30212=CARTESIAN_POINT('Ctrl Pts',(-13.3312658119027,-32.635704525562,22.1168218972623));
#30213=CARTESIAN_POINT('Ctrl Pts',(-13.2624727782426,-32.5387759125325,
22.1109983035913));
#30214=CARTESIAN_POINT('Ctrl Pts',(-13.1893348551765,-32.4446959552913,
22.1051747099203));
#30215=CARTESIAN_POINT('Ctrl Pts',(-13.1121159531807,-32.3538784430873,
22.0993511162492));
#30216=CARTESIAN_POINT('Ctrl Pts',(-13.0349944742999,-32.263175510665,22.0935348699066));
#30217=CARTESIAN_POINT('Ctrl Pts',(-12.9538025194292,-32.1757271448803,
22.087718623564));
#30218=CARTESIAN_POINT('Ctrl Pts',(-12.8688468720517,-32.0919177066804,
22.0819023772214));
#30219=CARTESIAN_POINT('Ctrl Pts',(-12.7839762657458,-32.0081921621904,
22.0760919529735));
#30220=CARTESIAN_POINT('Ctrl Pts',(-12.6953497508832,-31.9280985839322,
22.0702815287256));
#30221=CARTESIAN_POINT('Ctrl Pts',(-12.6033135194904,-31.8519873381388,
22.0644711044777));
#30222=CARTESIAN_POINT('Ctrl Pts',(-12.5077935263662,-31.7729951242591,
22.0584407436534));
#30223=CARTESIAN_POINT('Ctrl Pts',(-12.4086008771729,-31.6982930201086,
22.052410382829));
#30224=CARTESIAN_POINT('Ctrl Pts',(-12.3061638909232,-31.6282299740045,
22.0463800220047));
#30225=CARTESIAN_POINT('Ctrl Pts',(-12.2075740342512,-31.5607982198471,
22.0405761377719));
#30226=CARTESIAN_POINT('Ctrl Pts',(-12.105979502287,-31.4976636093401,22.0347722535391));
#30227=CARTESIAN_POINT('Ctrl Pts',(-12.0017942403327,-31.4390949437859,
22.0289683693063));
#30228=CARTESIAN_POINT('Ctrl Pts',(-11.8976243676558,-31.38053492945,22.0231653423693));
#30229=CARTESIAN_POINT('Ctrl Pts',(-11.7908648818679,-31.3265397188664,
22.0173623154322));
#30230=CARTESIAN_POINT('Ctrl Pts',(-11.6819559081383,-31.2773330362388,
22.0115592884952));
#30231=CARTESIAN_POINT('Ctrl Pts',(-11.573037318885,-31.2281220091757,22.0057557492116));
#30232=CARTESIAN_POINT('Ctrl Pts',(-11.4619692365034,-31.1837005187882,
21.9999522099279));
#30233=CARTESIAN_POINT('Ctrl Pts',(-11.3492128233251,-31.1442445931601,
21.9941486706443));
#30234=CARTESIAN_POINT('Ctrl Pts',(-11.2364198445569,-31.1047758724355,
21.9883432493405));
#30235=CARTESIAN_POINT('Ctrl Pts',(-11.1219378313496,-31.0702760537414,
21.9825378280368));
#30236=CARTESIAN_POINT('Ctrl Pts',(-11.0062435766426,-31.0408714513841,
21.976732406733));
#30237=CARTESIAN_POINT('Ctrl Pts',(-10.8904212012571,-31.0114342861514,
21.9709205564625));
#30238=CARTESIAN_POINT('Ctrl Pts',(-10.7733843007257,-30.9871037007735,
21.965108706192));
#30239=CARTESIAN_POINT('Ctrl Pts',(-10.6556204998703,-30.9679550151133,
21.9592968559216));
#30240=CARTESIAN_POINT('Ctrl Pts',(-10.5377793511181,-30.9487937524935,
21.9534811883966));
#30241=CARTESIAN_POINT('Ctrl Pts',(-10.4192107558225,-30.9348212154259,
21.9476655208716));
#30242=CARTESIAN_POINT('Ctrl Pts',(-10.3004064516107,-30.9260607559966,
21.9418498533467));
#30243=CARTESIAN_POINT('Ctrl Pts',(-10.1814319730621,-30.9172877481552,
21.936025855506));
#30244=CARTESIAN_POINT('Ctrl Pts',(-10.0622215184187,-30.913741731258,21.9302018576653));
#30245=CARTESIAN_POINT('Ctrl Pts',(-9.94326595421711,-30.9153939910869,
21.9243778598246));
#30246=CARTESIAN_POINT('Ctrl Pts',(-9.91170639454354,-30.9158323446269,
21.9228327214477));
#30247=CARTESIAN_POINT('Ctrl Pts',(-9.88016474084331,-30.916636306858,21.9212875830708));
#30248=CARTESIAN_POINT('Ctrl Pts',(-9.84865006826418,-30.9178047329698,
21.9197424446939));
#30249=CARTESIAN_POINT('Ctrl Pts',(-9.72988906658467,-30.9222078710662,
21.913919690835));
#30250=CARTESIAN_POINT('Ctrl Pts',(-9.61112888813309,-30.9318049790338,
21.908096936976));
#30251=CARTESIAN_POINT('Ctrl Pts',(-9.49286006789792,-30.9466021550719,
21.9022741831171));
#30252=CARTESIAN_POINT('Ctrl Pts',(-9.37473174463704,-30.9613817528637,
21.8964583463755));
#30253=CARTESIAN_POINT('Ctrl Pts',(-9.25709402033374,-30.9813490857124,
21.8906425096338));
#30254=CARTESIAN_POINT('Ctrl Pts',(-9.14043642792352,-31.0064582804785,
21.8848266728922));
#30255=CARTESIAN_POINT('Ctrl Pts',(-9.02388987404794,-31.0315435754868,
21.8790163718553));
#30256=CARTESIAN_POINT('Ctrl Pts',(-8.9083219934234,-31.0617609132255,21.8732060708184));
#30257=CARTESIAN_POINT('Ctrl Pts',(-8.79421556330646,-31.0970128244859,
21.8673957697815));
#30258=CARTESIAN_POINT('Ctrl Pts',(-8.67893007358786,-31.132628993084,21.861525431013));
#30259=CARTESIAN_POINT('Ctrl Pts',(-8.5651368289882,-31.1733843249257,21.8556550922445));
#30260=CARTESIAN_POINT('Ctrl Pts',(-8.4533218646113,-31.2191255316381,21.849784753476));
#30261=CARTESIAN_POINT('Ctrl Pts',(-8.34277849542931,-31.2643465548582,
21.8439811740595));
#30262=CARTESIAN_POINT('Ctrl Pts',(-8.23416902713381,-31.314440469642,21.8381775946431));
#30263=CARTESIAN_POINT('Ctrl Pts',(-8.12794568099241,-31.3692097793063,
21.8323740152266));
#30264=CARTESIAN_POINT('Ctrl Pts',(-8.01988948276489,-31.4249241170376,
21.8264702967821));
#30265=CARTESIAN_POINT('Ctrl Pts',(-7.91430292008785,-31.4854765379561,
21.8205665783376));
#30266=CARTESIAN_POINT('Ctrl Pts',(-7.81163757497356,-31.5506094890934,
21.814662859893));
#30267=CARTESIAN_POINT('Ctrl Pts',(-7.70897222985925,-31.6157424402308,
21.8087591414485));
#30268=CARTESIAN_POINT('Ctrl Pts',(-7.60922847440342,-31.6854556776709,
21.802855423004));
#30269=CARTESIAN_POINT('Ctrl Pts',(-7.51282745730979,-31.7594448403263,
21.7969517045595));
#30270=CARTESIAN_POINT('Ctrl Pts',(-7.5128274573098,-31.7594448403263,23.0467784921743));
#30271=CARTESIAN_POINT('Ctrl Pts',(-7.41657407421678,-31.8333206917696,
23.0408768761477));
#30272=CARTESIAN_POINT('Ctrl Pts',(-7.32354678406087,-31.9115410529426,
23.0349752601211));
#30273=CARTESIAN_POINT('Ctrl Pts',(-7.23415358548507,-31.9937866657014,
23.0290736440946));
#30274=CARTESIAN_POINT('Ctrl Pts',(-7.1462441309189,-32.074667169736,23.0232699828069));
#30275=CARTESIAN_POINT('Ctrl Pts',(-7.06184936093566,-32.1594400346389,
23.0174663215192));
#30276=CARTESIAN_POINT('Ctrl Pts',(-6.98132346380725,-32.2477614620387,
23.0116626602315));
#30277=CARTESIAN_POINT('Ctrl Pts',(-6.90080651065365,-32.3360730796177,
23.0058596435538));
#30278=CARTESIAN_POINT('Ctrl Pts',(-6.82415785080753,-32.4279321741339,
23.0000566268762));
#30279=CARTESIAN_POINT('Ctrl Pts',(-6.75169352034171,-32.5229594241898,
22.9942536101985));
#30280=CARTESIAN_POINT('Ctrl Pts',(-6.67922013687654,-32.6179985460402,
22.9884498685475));
#30281=CARTESIAN_POINT('Ctrl Pts',(-6.61093236983824,-32.7162062857298,
22.9826461268965));
#30282=CARTESIAN_POINT('Ctrl Pts',(-6.54710441122387,-32.8171722346895,
22.9768423852455));
#30283=CARTESIAN_POINT('Ctrl Pts',(-6.48139054620653,-32.9211213956109,
22.9708671621031));
#30284=CARTESIAN_POINT('Ctrl Pts',(-6.42040438537492,-33.0279939058608,
22.9648919389606));
#30285=CARTESIAN_POINT('Ctrl Pts',(-6.36439501581763,-33.1373133921703,
22.9589167158182));
#30286=CARTESIAN_POINT('Ctrl Pts',(-6.30991131226698,-33.2436550727046,
22.9531042546369));
#30287=CARTESIAN_POINT('Ctrl Pts',(-6.26013688993258,-33.3523117422711,
22.9472917934555));
#30288=CARTESIAN_POINT('Ctrl Pts',(-6.21525217972208,-33.4628243636781,
22.9414793322742));
#30289=CARTESIAN_POINT('Ctrl Pts',(-6.16848216054422,-33.5779788873091,
22.9354227281512));
#30290=CARTESIAN_POINT('Ctrl Pts',(-6.12702175079582,-33.695148202419,22.9293661240282));
#30291=CARTESIAN_POINT('Ctrl Pts',(-6.09101724819159,-33.8137964567308,
22.9233095199051));
#30292=CARTESIAN_POINT('Ctrl Pts',(-6.05501274558735,-33.9324447110427,
22.9172529157821));
#30293=CARTESIAN_POINT('Ctrl Pts',(-6.02446420547396,-34.0525714086231,
22.9111963116591));
#30294=CARTESIAN_POINT('Ctrl Pts',(-5.99945759808046,-34.1736311414121,
22.9051397075361));
#30295=CARTESIAN_POINT('Ctrl Pts',(-5.97541304809779,-34.2900334486156,
22.8993161138646));
#30296=CARTESIAN_POINT('Ctrl Pts',(-5.95641431380095,-34.4076737573629,
22.8934925201932));
#30297=CARTESIAN_POINT('Ctrl Pts',(-5.94258432963637,-34.526076928302,22.8876689265217));
#30298=CARTESIAN_POINT('Ctrl Pts',(-5.92877179405107,-34.6443307160538,
22.8818526801787));
#30299=CARTESIAN_POINT('Ctrl Pts',(-5.92011508514747,-34.7633450496746,
22.8760364338357));
#30300=CARTESIAN_POINT('Ctrl Pts',(-5.91668638256212,-34.8826334730583,
22.8702201874927));
#30301=CARTESIAN_POINT('Ctrl Pts',(-5.91326111212698,-35.0018024880719,
22.8644097632444));
#30302=CARTESIAN_POINT('Ctrl Pts',(-5.91505344874563,-35.1212446412101,
22.858599338996));
#30303=CARTESIAN_POINT('Ctrl Pts',(-5.92208383683804,-35.2404678070397,
22.8527889147477));
#30304=CARTESIAN_POINT('Ctrl Pts',(-5.92938033966113,-35.3642038162922,
22.8467585539235));
#30305=CARTESIAN_POINT('Ctrl Pts',(-5.94231932317023,-35.4877034872365,
22.8407281930994));
#30306=CARTESIAN_POINT('Ctrl Pts',(-5.96086422097446,-35.6104155622162,
22.8346978322752));
#30307=CARTESIAN_POINT('Ctrl Pts',(-5.97871264549017,-35.7285190551857,
22.828893948042));
#30308=CARTESIAN_POINT('Ctrl Pts',(-6.0017534391838,-35.8458926032994,22.8230900638088));
#30309=CARTESIAN_POINT('Ctrl Pts',(-6.0299011822913,-35.9620500910181,22.8172861795755));
#30310=CARTESIAN_POINT('Ctrl Pts',(-6.05804476767621,-36.0781904210341,
22.8114831526381));
#30311=CARTESIAN_POINT('Ctrl Pts',(-6.09129370616843,-36.1931146511285,
22.8056801257006));
#30312=CARTESIAN_POINT('Ctrl Pts',(-6.12951174889391,-36.3063482300098,
22.7998770987631));
#30313=CARTESIAN_POINT('Ctrl Pts',(-6.16773316587283,-36.4195918062318,
22.7940735594791));
#30314=CARTESIAN_POINT('Ctrl Pts',(-6.21092442877709,-36.5311440475486,
22.788270020195));
#30315=CARTESIAN_POINT('Ctrl Pts',(-6.25890004806749,-36.6405475152066,
22.782466480911));
#30316=CARTESIAN_POINT('Ctrl Pts',(-6.30689122529183,-36.7499864611335,
22.7766610596068));
#30317=CARTESIAN_POINT('Ctrl Pts',(-6.35966968060255,-36.857274873811,22.7708556383026));
#30318=CARTESIAN_POINT('Ctrl Pts',(-6.41700289212973,-36.9619777585369,
22.7650502169985));
#30319=CARTESIAN_POINT('Ctrl Pts',(-6.47439959488187,-37.0667965920162,
22.7592383667275));
#30320=CARTESIAN_POINT('Ctrl Pts',(-6.53636092581258,-37.1690238239168,
22.7534265164566));
#30321=CARTESIAN_POINT('Ctrl Pts',(-6.60260966410572,-37.2682512880129,
22.7476146661857));
#30322=CARTESIAN_POINT('Ctrl Pts',(-6.66890191492579,-37.3675439252401,
22.7417989986603));
#30323=CARTESIAN_POINT('Ctrl Pts',(-6.73948694036625,-37.4638325422618,
22.735983331135));
#30324=CARTESIAN_POINT('Ctrl Pts',(-6.81404668775415,-37.5567413815616,
22.7301676636096));
#30325=CARTESIAN_POINT('Ctrl Pts',(-6.88871323392924,-37.6497833027415,
22.7243436657685));
#30326=CARTESIAN_POINT('Ctrl Pts',(-6.96736559735218,-37.7394354776297,
22.7185196679274));
#30327=CARTESIAN_POINT('Ctrl Pts',(-7.04964821814089,-37.8253582716676,
22.7126956700862));
#30328=CARTESIAN_POINT('Ctrl Pts',(-7.07147824594466,-37.8481540572764,
22.7111505317134));
#30329=CARTESIAN_POINT('Ctrl Pts',(-7.09356361386344,-37.8706875610459,
22.7096053933405));
#30330=CARTESIAN_POINT('Ctrl Pts',(-7.11589729903294,-37.8929529222361,
22.7080602549676));
#30331=CARTESIAN_POINT('Ctrl Pts',(-7.20007248353159,-37.9768705951097,
22.7022366612962));
#30332=CARTESIAN_POINT('Ctrl Pts',(-7.28804902917364,-38.0572467206924,
22.6964130676248));
#30333=CARTESIAN_POINT('Ctrl Pts',(-7.3794969313009,-38.1337180260736,22.6905894739534));
#30334=CARTESIAN_POINT('Ctrl Pts',(-7.47082945831606,-38.2100928515441,
22.6847732276105));
#30335=CARTESIAN_POINT('Ctrl Pts',(-7.56562432034595,-38.2825723958907,
22.6789569812675));
#30336=CARTESIAN_POINT('Ctrl Pts',(-7.66351422578759,-38.3508296326288,
22.6731407349246));
#30337=CARTESIAN_POINT('Ctrl Pts',(-7.76130614289356,-38.4190185434961,
22.6673303106763));
#30338=CARTESIAN_POINT('Ctrl Pts',(-7.86218660699052,-38.4829933227464,
22.661519886428));
#30339=CARTESIAN_POINT('Ctrl Pts',(-7.96575522545239,-38.5424671060189,
22.6557094621798));
#30340=CARTESIAN_POINT('Ctrl Pts',(-8.07324413034172,-38.6041920950022,
22.6496791013556));
#30341=CARTESIAN_POINT('Ctrl Pts',(-8.18362837108424,-38.6610683238982,
22.6436487405314));
#30342=CARTESIAN_POINT('Ctrl Pts',(-8.29642684731877,-38.7128241964122,
22.6376183797072));
#30343=CARTESIAN_POINT('Ctrl Pts',(-8.4049890572478,-38.7626363222892,22.631814495474));
#30344=CARTESIAN_POINT('Ctrl Pts',(-8.51578703002208,-38.8077055712258,
22.6260106112409));
#30345=CARTESIAN_POINT('Ctrl Pts',(-8.62836736862794,-38.8478369150154,
22.6202067270077));
#30346=CARTESIAN_POINT('Ctrl Pts',(-8.74093107791384,-38.8879623309764,
22.6144037000703));
#30347=CARTESIAN_POINT('Ctrl Pts',(-8.85527624493528,-38.9231511552279,
22.6086006731329));
#30348=CARTESIAN_POINT('Ctrl Pts',(-8.97093128201469,-38.9532572106636,
22.6027976461955));
#30349=CARTESIAN_POINT('Ctrl Pts',(-9.08659653022495,-38.9833659241494,
22.5969941069114));
#30350=CARTESIAN_POINT('Ctrl Pts',(-9.2035714832416,-39.0083908737143,22.5911905676274));
#30351=CARTESIAN_POINT('Ctrl Pts',(-9.32137187388081,-39.0282364461933,
22.5853870283434));
#30352=CARTESIAN_POINT('Ctrl Pts',(-9.43921046581199,-39.0480884543599,
22.5795816070393));
#30353=CARTESIAN_POINT('Ctrl Pts',(-9.55787462526471,-39.0627576772715,
22.5737761857352));
#30354=CARTESIAN_POINT('Ctrl Pts',(-9.67687307520163,-39.0722001412591,
22.5679707644311));
#30355=CARTESIAN_POINT('Ctrl Pts',(-9.79600330490789,-39.0816530619015,
22.5621589141603));
#30356=CARTESIAN_POINT('Ctrl Pts',(-9.91546815674197,-39.0858676376544,
22.5563470638894));
#30357=CARTESIAN_POINT('Ctrl Pts',(-10.034774289896,-39.0848519861511,22.5505352136186));
#30358=CARTESIAN_POINT('Ctrl Pts',(-10.1541587839587,-39.0838356675624,
22.5447195460932));
#30359=CARTESIAN_POINT('Ctrl Pts',(-10.2733839448912,-39.0775823016864,
22.5389038785679));
#30360=CARTESIAN_POINT('Ctrl Pts',(-10.3919611550581,-39.0661519220174,
22.5330882110426));
#30361=CARTESIAN_POINT('Ctrl Pts',(-10.5107082142745,-39.0547051695637,
22.5272642132015));
#30362=CARTESIAN_POINT('Ctrl Pts',(-10.6288050673409,-39.0380666591211,
22.5214402153605));
#30363=CARTESIAN_POINT('Ctrl Pts',(-10.7457727487356,-39.0163475954209,
22.5156162175194));
#30364=CARTESIAN_POINT('Ctrl Pts',(-10.7768049121916,-39.0105854094323,
22.514071079146));
#30365=CARTESIAN_POINT('Ctrl Pts',(-10.8077576788359,-39.0044658909878,
22.5125259407726));
#30366=CARTESIAN_POINT('Ctrl Pts',(-10.8386222972362,-38.9979917011643,
22.5109808023992));
#30367=CARTESIAN_POINT('Ctrl Pts',(-10.9549503876449,-38.9735906173943,
22.5051572087275));
#30368=CARTESIAN_POINT('Ctrl Pts',(-11.0704001978095,-38.9440688376194,
22.4993336150558));
#30369=CARTESIAN_POINT('Ctrl Pts',(-11.1844870002162,-38.9095032352358,
22.4935100213841));
#30370=CARTESIAN_POINT('Ctrl Pts',(-11.2984298651754,-38.8749812424938,
22.4876937750409));
#30371=CARTESIAN_POINT('Ctrl Pts',(-11.411012755344,-38.8354282014154,22.4818775286977));
#30372=CARTESIAN_POINT('Ctrl Pts',(-11.521760819328,-38.7909720400919,22.4760612823544));
#30373=CARTESIAN_POINT('Ctrl Pts',(-11.6323980238884,-38.7465603796313,
22.4702508581059));
#30374=CARTESIAN_POINT('Ctrl Pts',(-11.7412036793262,-38.6972555141252,
22.4644404338573));
#30375=CARTESIAN_POINT('Ctrl Pts',(-11.8477183799131,-38.6432350718189,
22.4586300096088));
#30376=CARTESIAN_POINT('Ctrl Pts',(-11.9582648822223,-38.5871698440405,
22.4525996487847));
#30377=CARTESIAN_POINT('Ctrl Pts',(-12.0663431391598,-38.5260251272257,
22.4465692879606));
#30378=CARTESIAN_POINT('Ctrl Pts',(-12.1714622737272,-38.4600544206384,
22.4405389271365));
#30379=CARTESIAN_POINT('Ctrl Pts',(-12.2726335478099,-38.3965613138407,
22.4347350429031));
#30380=CARTESIAN_POINT('Ctrl Pts',(-12.3710635802308,-38.3285984071227,
22.4289311586696));
#30381=CARTESIAN_POINT('Ctrl Pts',(-12.4663407192961,-38.2564380013048,
22.4231272744361));
#30382=CARTESIAN_POINT('Ctrl Pts',(-12.5616037849091,-38.1842882543505,
22.4173242474984));
#30383=CARTESIAN_POINT('Ctrl Pts',(-12.653714557903,-38.1079424877804,22.4115212205607));
#30384=CARTESIAN_POINT('Ctrl Pts',(-12.7422922727754,-38.0277149949551,
22.405718193623));
#30385=CARTESIAN_POINT('Ctrl Pts',(-12.8308778081336,-37.9474804188814,
22.3999146543387));
#30386=CARTESIAN_POINT('Ctrl Pts',(-12.9159293625085,-37.8633637092838,
22.3941111150545));
#30387=CARTESIAN_POINT('Ctrl Pts',(-12.9971015101761,-37.7757174816072,
22.3883075757702));
#30388=CARTESIAN_POINT('Ctrl Pts',(-13.0782999810252,-37.6880428312805,
22.3825021544657));
#30389=CARTESIAN_POINT('Ctrl Pts',(-13.1556162658785,-37.5968366859967,
22.3766967331613));
#30390=CARTESIAN_POINT('Ctrl Pts',(-13.2287442862499,-37.5024858309306,
22.3708913118569));
#30391=CARTESIAN_POINT('Ctrl Pts',(-13.3019532891348,-37.4080304910262,
22.3650794615857));
#30392=CARTESIAN_POINT('Ctrl Pts',(-13.3709645191656,-37.3104238129581,
22.3592676113146));
#30393=CARTESIAN_POINT('Ctrl Pts',(-13.4355143342349,-37.210082862534,22.3534557610435));
#30394=CARTESIAN_POINT('Ctrl Pts',(-13.5001065459694,-37.1096760076348,
22.3476400935178));
#30395=CARTESIAN_POINT('Ctrl Pts',(-13.5602313018458,-37.0065316557953,
22.3418244259922));
#30396=CARTESIAN_POINT('Ctrl Pts',(-13.615670969756,-36.9010913808819,22.3360087584666));
#30397=CARTESIAN_POINT('Ctrl Pts',(-13.6711900490038,-36.7955000741607,
22.3301847606253));
#30398=CARTESIAN_POINT('Ctrl Pts',(-13.7220104723456,-36.6876066484729,
22.3243607627839));
#30399=CARTESIAN_POINT('Ctrl Pts',(-13.7679626967566,-36.5778726551438,
22.3185367649426));
#30400=CARTESIAN_POINT('Ctrl Pts',(-13.7801540723524,-36.5487596286159,
22.316991626572));
#30401=CARTESIAN_POINT('Ctrl Pts',(-13.7920030629536,-36.5195171306536,
22.3154464882014));
#30402=CARTESIAN_POINT('Ctrl Pts',(-13.8035070969918,-36.4901539394079,
22.3139013498308));
#30403=CARTESIAN_POINT('Ctrl Pts',(-13.852406599943,-36.3653415951289,22.3073335234437));
#30404=CARTESIAN_POINT('Ctrl Pts',(-13.8952013288729,-36.2380114730684,
22.3007656970567));
#30405=CARTESIAN_POINT('Ctrl Pts',(-13.9316569522707,-36.1087373943643,
22.2941978706696));
#30406=CARTESIAN_POINT('Ctrl Pts',(-13.9679980306451,-35.9798694999738,
22.2876506806552));
#30407=CARTESIAN_POINT('Ctrl Pts',(-13.9980396583831,-35.8490700313153,
22.2811034906407));
#30408=CARTESIAN_POINT('Ctrl Pts',(-14.0215963303967,-35.7169295330366,
22.2745563006263));
#30409=CARTESIAN_POINT('Ctrl Pts',(-14.0450149575283,-35.5855633936945,
22.268047477919));
#30410=CARTESIAN_POINT('Ctrl Pts',(-14.0620243166783,-35.4528720959649,
22.2615386552118));
#30411=CARTESIAN_POINT('Ctrl Pts',(-14.0724898512344,-35.319454866284,22.2550298325046));
#30412=CARTESIAN_POINT('Ctrl Pts',(-14.0807516711158,-35.2141311377364,
22.2498915645492));
#30413=CARTESIAN_POINT('Ctrl Pts',(-14.0849362747585,-35.1083554128431,
22.2447532965937));
#30414=CARTESIAN_POINT('Ctrl Pts',(-14.0849992774348,-35.002429682444,22.2396150286382));
#30415=CARTESIAN_POINT('Origin',(-10.,-35.,32.7603849714045));
#30416=CARTESIAN_POINT('',(-7.51282745730979,-31.7594448403263,24.2969436976378));
#30417=CARTESIAN_POINT('',(-7.51282745730979,-31.7594448403263,24.1926554185755));
#30418=CARTESIAN_POINT('',(-7.5128274573098,-31.7594448403263,32.7603849714045));
#30419=CARTESIAN_POINT('',(-14.0849994926668,-34.9979640942378,23.3853849713652));
#30420=CARTESIAN_POINT('Ctrl Pts',(-7.51282745730979,-31.7594448403263,
24.1926554185755));
#30421=CARTESIAN_POINT('Ctrl Pts',(-7.41801607719479,-31.832213933811,24.1868522096254));
#30422=CARTESIAN_POINT('Ctrl Pts',(-7.32640223554429,-31.90914642333,24.1810490006754));
#30423=CARTESIAN_POINT('Ctrl Pts',(-7.23836090041157,-31.9899211831541,
24.1752457917253));
#30424=CARTESIAN_POINT('Ctrl Pts',(-7.15029814958328,-32.070715591109,24.1694411711683));
#30425=CARTESIAN_POINT('Ctrl Pts',(-7.06580993423397,-32.1553538520102,
24.1636365506114));
#30426=CARTESIAN_POINT('Ctrl Pts',(-6.98523507237383,-32.2434772935535,
24.1578319300544));
#30427=CARTESIAN_POINT('Ctrl Pts',(-6.90457409534944,-32.3316949178787,
24.152021105753));
#30428=CARTESIAN_POINT('Ctrl Pts',(-6.82783509921019,-32.4234048588342,
24.1462102814516));
#30429=CARTESIAN_POINT('Ctrl Pts',(-6.75531735975733,-32.5182144403458,
24.1403994571501));
#30430=CARTESIAN_POINT('Ctrl Pts',(-6.68275726123609,-32.6130794020386,
24.1345852386295));
#30431=CARTESIAN_POINT('Ctrl Pts',(-6.61442356434731,-32.7110472762526,
24.1287710201089));
#30432=CARTESIAN_POINT('Ctrl Pts',(-6.55057188569452,-32.811696848186,24.1229568015883));
#30433=CARTESIAN_POINT('Ctrl Pts',(-6.48662276134335,-32.9125000240345,
24.1171337098384));
#30434=CARTESIAN_POINT('Ctrl Pts',(-6.42716951938448,-33.0159927176018,
24.1113106180885));
#30435=CARTESIAN_POINT('Ctrl Pts',(-6.37242173268631,-33.1217292755001,
24.1054875263386));
#30436=CARTESIAN_POINT('Ctrl Pts',(-6.33911654257133,-33.1860529016281,
24.101945115047));
#30437=CARTESIAN_POINT('Ctrl Pts',(-6.30755179619556,-33.2512065136336,
24.0984027037555));
#30438=CARTESIAN_POINT('Ctrl Pts',(-6.2777657820977,-33.317086625201,24.0948602924639));
#30439=CARTESIAN_POINT('Ctrl Pts',(-6.22879867214836,-33.4253911017918,
24.0890366987924));
#30440=CARTESIAN_POINT('Ctrl Pts',(-6.18448346565954,-33.5360091682236,
24.0832131051209));
#30441=CARTESIAN_POINT('Ctrl Pts',(-6.14504422535159,-33.6485041711108,
24.0773895114494));
#30442=CARTESIAN_POINT('Ctrl Pts',(-6.10565474350347,-33.7608572448422,
24.0715732651064));
#30443=CARTESIAN_POINT('Ctrl Pts',(-6.07112912604358,-33.8750821631195,
24.0657570187633));
#30444=CARTESIAN_POINT('Ctrl Pts',(-6.04164439422476,-33.9907201090739,
24.0599407724202));
#30445=CARTESIAN_POINT('Ctrl Pts',(-6.01218917678524,-34.1062423008062,
24.0541303481719));
#30446=CARTESIAN_POINT('Ctrl Pts',(-5.98776490699332,-34.2231743129421,
24.0483199239235));
#30447=CARTESIAN_POINT('Ctrl Pts',(-5.96849937054934,-34.341040460469,24.0425094996752));
#30448=CARTESIAN_POINT('Ctrl Pts',(-5.94850459370308,-34.4633680854682,
24.036479138851));
#30449=CARTESIAN_POINT('Ctrl Pts',(-5.93406695235356,-34.5867015380663,
24.0304487780268));
#30450=CARTESIAN_POINT('Ctrl Pts',(-5.92527156445518,-34.7104949455321,
24.0244184172027));
#30451=CARTESIAN_POINT('Ctrl Pts',(-5.91680649666943,-34.8296391604019,
24.0186145329694));
#30452=CARTESIAN_POINT('Ctrl Pts',(-5.91356755497437,-34.9492089610531,
24.0128106487361));
#30453=CARTESIAN_POINT('Ctrl Pts',(-5.91557791684955,-35.0687113285635,
24.0070067645029));
#30454=CARTESIAN_POINT('Ctrl Pts',(-5.91758798177279,-35.1881960442961,
24.0012037375654));
#30455=CARTESIAN_POINT('Ctrl Pts',(-5.92484580141723,-35.3076129385274,
23.9954007106278));
#30456=CARTESIAN_POINT('Ctrl Pts',(-5.93732242544666,-35.4264691374782,
23.9895976836903));
#30457=CARTESIAN_POINT('Ctrl Pts',(-5.94980015103154,-35.5453358301887,
23.9837941444062));
#30458=CARTESIAN_POINT('Ctrl Pts',(-5.96749755448325,-35.6636413230681,
23.9779906051221));
#30459=CARTESIAN_POINT('Ctrl Pts',(-5.99033389170718,-35.7808986489986,
23.972187065838));
#30460=CARTESIAN_POINT('Ctrl Pts',(-6.01317763448897,-35.8981940001126,
23.9663816445338));
#30461=CARTESIAN_POINT('Ctrl Pts',(-6.04116354730942,-36.0144401076764,
23.9605762232295));
#30462=CARTESIAN_POINT('Ctrl Pts',(-6.07416007869851,-36.1291615970779,
23.9547708019253));
#30463=CARTESIAN_POINT('Ctrl Pts',(-6.10719315069184,-36.2440101299099,
23.9489589516543));
#30464=CARTESIAN_POINT('Ctrl Pts',(-6.1452478041883,-36.3573302817817,23.9431471013834));
#30465=CARTESIAN_POINT('Ctrl Pts',(-6.18814299626949,-36.4686630597624,
23.9373352511124));
#30466=CARTESIAN_POINT('Ctrl Pts',(-6.23106636214315,-36.5800689617095,
23.931519583587));
#30467=CARTESIAN_POINT('Ctrl Pts',(-6.27883643523255,-36.689484516827,23.9257039160616));
#30468=CARTESIAN_POINT('Ctrl Pts',(-6.33122523149382,-36.7964734058628,
23.9198882485362));
#30469=CARTESIAN_POINT('Ctrl Pts',(-6.38368906904874,-36.9036155449295,
23.914064250695));
#30470=CARTESIAN_POINT('Ctrl Pts',(-6.44078463980518,-37.0083237229024,
23.9082402528538));
#30471=CARTESIAN_POINT('Ctrl Pts',(-6.50223944854652,-37.1101886467081,
23.9024162550126));
#30472=CARTESIAN_POINT('Ctrl Pts',(-6.51854374428008,-37.1372139662335,
23.9008711166403));
#30473=CARTESIAN_POINT('Ctrl Pts',(-6.53515464754064,-37.1640393303594,
23.8993259782679));
#30474=CARTESIAN_POINT('Ctrl Pts',(-6.55206659039437,-37.1906574818819,
23.8977808398955));
#30475=CARTESIAN_POINT('Ctrl Pts',(-6.6158073434136,-37.290980728992,23.891957246224));
#30476=CARTESIAN_POINT('Ctrl Pts',(-6.68403312025819,-37.3886814839584,
23.8861336525526));
#30477=CARTESIAN_POINT('Ctrl Pts',(-6.75650153965794,-37.4833329897053,
23.8803100588811));
#30478=CARTESIAN_POINT('Ctrl Pts',(-6.82887852938234,-37.5778650785184,
23.8744938125381));
#30479=CARTESIAN_POINT('Ctrl Pts',(-6.90548726917389,-37.6693552485029,
23.8686775661951));
#30480=CARTESIAN_POINT('Ctrl Pts',(-6.9860410544455,-37.7574039374948,23.8628613198521));
#30481=CARTESIAN_POINT('Ctrl Pts',(-7.06651420493347,-37.8453644892631,
23.8570508956037));
#30482=CARTESIAN_POINT('Ctrl Pts',(-7.15092427078452,-37.9298901137794,
23.8512404713554));
#30483=CARTESIAN_POINT('Ctrl Pts',(-7.23894345024624,-38.0106131815731,
23.8454300471071));
#30484=CARTESIAN_POINT('Ctrl Pts',(-7.33029433770584,-38.0943917844471,
23.8393996862829));
#30485=CARTESIAN_POINT('Ctrl Pts',(-7.42553268961703,-38.1740739175939,
23.8333693254587));
#30486=CARTESIAN_POINT('Ctrl Pts',(-7.52424861234076,-38.2492891632638,
23.8273389646346));
#30487=CARTESIAN_POINT('Ctrl Pts',(-7.61925715398036,-38.3216796206792,
23.8215350804014));
#30488=CARTESIAN_POINT('Ctrl Pts',(-7.7174864152581,-38.3899323876538,23.8157311961681));
#30489=CARTESIAN_POINT('Ctrl Pts',(-7.8185367544231,-38.4537578241963,23.8099273119349));
#30490=CARTESIAN_POINT('Ctrl Pts',(-7.91957216737257,-38.5175738330394,
23.8041242849974));
#30491=CARTESIAN_POINT('Ctrl Pts',(-8.02342748437325,-38.5769635939781,
23.7983212580599));
#30492=CARTESIAN_POINT('Ctrl Pts',(-8.12967461049804,-38.6316811447847,
23.7925182311225));
#30493=CARTESIAN_POINT('Ctrl Pts',(-8.23593111713296,-38.6864035265787,
23.7867146918384));
#30494=CARTESIAN_POINT('Ctrl Pts',(-8.34457948971135,-38.7364526911092,
23.7809111525543));
#30495=CARTESIAN_POINT('Ctrl Pts',(-8.45516818201529,-38.7816292327702,
23.7751076132703));
#30496=CARTESIAN_POINT('Ctrl Pts',(-8.56579273694218,-38.8268204246566,
23.7693021919661));
#30497=CARTESIAN_POINT('Ctrl Pts',(-8.67835848515975,-38.8671356968,23.763496770662));
#30498=CARTESIAN_POINT('Ctrl Pts',(-8.79239572533486,-38.9024244920063,
23.7576913493578));
#30499=CARTESIAN_POINT('Ctrl Pts',(-8.90655925119832,-38.937752366287,23.7518794990869));
#30500=CARTESIAN_POINT('Ctrl Pts',(-9.02219713140498,-38.9680425319197,
23.746067648816));
#30501=CARTESIAN_POINT('Ctrl Pts',(-9.13882623637793,-38.9931948047709,
23.7402557985451));
#30502=CARTESIAN_POINT('Ctrl Pts',(-9.25553194397294,-39.0183635977698,
23.7344401310197));
#30503=CARTESIAN_POINT('Ctrl Pts',(-9.37322977127301,-39.0383877090656,
23.7286244634944));
#30504=CARTESIAN_POINT('Ctrl Pts',(-9.49142982089655,-39.0532186436123,
23.722808795969));
#30505=CARTESIAN_POINT('Ctrl Pts',(-9.6097991793283,-39.0680708218714,23.7169847981279));
#30506=CARTESIAN_POINT('Ctrl Pts',(-9.72867179037029,-39.0777149433081,
23.7111608002867));
#30507=CARTESIAN_POINT('Ctrl Pts',(-9.84755596115319,-39.0821545555038,
23.7053368024456));
#30508=CARTESIAN_POINT('Ctrl Pts',(-9.87909657967911,-39.0833324088188,
23.7037916640728));
#30509=CARTESIAN_POINT('Ctrl Pts',(-9.91063803235721,-39.0841442161781,
23.7022465256999));
#30510=CARTESIAN_POINT('Ctrl Pts',(-9.94217119733299,-39.084590656306,23.700701387327));
#30511=CARTESIAN_POINT('Ctrl Pts',(-10.0610190256045,-39.0862732796548,
23.6948777936556));
#30512=CARTESIAN_POINT('Ctrl Pts',(-10.1801320038195,-39.0827672038154,
23.6890541999841));
#30513=CARTESIAN_POINT('Ctrl Pts',(-10.2990203400898,-39.0740412168034,
23.6832306063127));
#30514=CARTESIAN_POINT('Ctrl Pts',(-10.4177586810645,-39.0653262389201,
23.6774143599696));
#30515=CARTESIAN_POINT('Ctrl Pts',(-10.5362725401565,-39.0514044782802,
23.6715981136266));
#30516=CARTESIAN_POINT('Ctrl Pts',(-10.6540705740894,-39.0322967009026,
23.6657818672836));
#30517=CARTESIAN_POINT('Ctrl Pts',(-10.7717506915403,-39.0132080505157,
23.6599714430353));
#30518=CARTESIAN_POINT('Ctrl Pts',(-10.8887160085574,-38.9889437757082,
23.654161018787));
#30519=CARTESIAN_POINT('Ctrl Pts',(-11.0044793614783,-38.9595765193218,
23.6483505945386));
#30520=CARTESIAN_POINT('Ctrl Pts',(-11.1246245967473,-38.9290976515391,
23.6423202337145));
#30521=CARTESIAN_POINT('Ctrl Pts',(-11.2434746293564,-38.893121885162,23.6362898728903));
#30522=CARTESIAN_POINT('Ctrl Pts',(-11.3604949638244,-38.8517889938843,
23.6302595120661));
#30523=CARTESIAN_POINT('Ctrl Pts',(-11.4731204756289,-38.8120084031377,
23.6244556278329));
#30524=CARTESIAN_POINT('Ctrl Pts',(-11.584050823736,-38.7672659642261,23.6186517435996));
#30525=CARTESIAN_POINT('Ctrl Pts',(-11.692824692563,-38.7177371558852,23.6128478593664));
#30526=CARTESIAN_POINT('Ctrl Pts',(-11.8015824943263,-38.6682156634789,
23.6070448324289));
#30527=CARTESIAN_POINT('Ctrl Pts',(-11.9081840787501,-38.613909376808,23.6012418054915));
#30528=CARTESIAN_POINT('Ctrl Pts',(-12.012189064078,-38.5550415145825,23.595438778554));
#30529=CARTESIAN_POINT('Ctrl Pts',(-12.1162032319582,-38.4961684549405,
23.5896352392699));
#30530=CARTESIAN_POINT('Ctrl Pts',(-12.2176199895532,-38.4327332201492,
23.5838316999859));
#30531=CARTESIAN_POINT('Ctrl Pts',(-12.3160250385777,-38.3650041635459,
23.5780281607018));
#30532=CARTESIAN_POINT('Ctrl Pts',(-12.414461999212,-38.2972531431993,23.5722227393977));
#30533=CARTESIAN_POINT('Ctrl Pts',(-12.5098849727227,-38.2252057631901,
23.5664173180935));
#30534=CARTESIAN_POINT('Ctrl Pts',(-12.601910564254,-38.1491723381903,23.5606118967893));
#30535=CARTESIAN_POINT('Ctrl Pts',(-12.6940380656104,-38.0730547132098,
23.5548000465184));
#30536=CARTESIAN_POINT('Ctrl Pts',(-12.7827603601641,-37.9929424924071,
23.5489881962475));
#30537=CARTESIAN_POINT('Ctrl Pts',(-12.8677288227596,-37.9091848341268,
23.5431763459766));
#30538=CARTESIAN_POINT('Ctrl Pts',(-12.9527530930979,-37.8253721633667,
23.5373606784512));
#30539=CARTESIAN_POINT('Ctrl Pts',(-13.0340183439926,-37.7379095851885,
23.5315450109258));
#30540=CARTESIAN_POINT('Ctrl Pts',(-13.1112154716858,-37.6471802524087,
23.5257293434004));
#30541=CARTESIAN_POINT('Ctrl Pts',(-13.1885231759284,-37.5563209596571,
23.5199053455592));
#30542=CARTESIAN_POINT('Ctrl Pts',(-13.2617508764712,-37.4621858938875,
23.5140813477181));
#30543=CARTESIAN_POINT('Ctrl Pts',(-13.330632012287,-37.3651882374832,23.508257349877));
#30544=CARTESIAN_POINT('Ctrl Pts',(-13.3489065530774,-37.3394542305226,
23.5067122115042));
#30545=CARTESIAN_POINT('Ctrl Pts',(-13.3668754008444,-37.3135188728409,
23.5051670731314));
#30546=CARTESIAN_POINT('Ctrl Pts',(-13.3845341229849,-37.2873901657458,
23.5036219347586));
#30547=CARTESIAN_POINT('Ctrl Pts',(-13.4520539487644,-37.1874845362861,
23.4977139492936));
#30548=CARTESIAN_POINT('Ctrl Pts',(-13.5152498617656,-37.084434171241,23.4918059638286));
#30549=CARTESIAN_POINT('Ctrl Pts',(-13.5738211458681,-36.9786428220743,
23.4858979783636));
#30550=CARTESIAN_POINT('Ctrl Pts',(-13.6323130634339,-36.872994824605,23.4799979984656));
#30551=CARTESIAN_POINT('Ctrl Pts',(-13.6861926320066,-36.7646135732612,
23.4740980185677));
#30552=CARTESIAN_POINT('Ctrl Pts',(-13.7352017518379,-36.6539325479193,
23.4681980386698));
#30553=CARTESIAN_POINT('Ctrl Pts',(-13.7841547944734,-36.5433781659767,
23.4623048096446));
#30554=CARTESIAN_POINT('Ctrl Pts',(-13.8282483207181,-36.4305296035672,
23.4564115806194));
#30555=CARTESIAN_POINT('Ctrl Pts',(-13.8672698330024,-36.3158453703796,
23.4505183515942));
#30556=CARTESIAN_POINT('Ctrl Pts',(-13.9062483904799,-36.201287381379,23.4446316098243));
#30557=CARTESIAN_POINT('Ctrl Pts',(-13.9401659294039,-36.0848981168257,
23.4387448680545));
#30558=CARTESIAN_POINT('Ctrl Pts',(-13.9688580865626,-35.9671558761266,
23.4328581262846));
#30559=CARTESIAN_POINT('Ctrl Pts',(-13.9975315945567,-35.8494901648578,
23.4269752107456));
#30560=CARTESIAN_POINT('Ctrl Pts',(-14.020986387276,-35.7304736079701,23.4210922952066));
#30561=CARTESIAN_POINT('Ctrl Pts',(-14.0391079923918,-35.6105993987847,
23.4152093796675));
#30562=CARTESIAN_POINT('Ctrl Pts',(-14.0572220478134,-35.4907751307399,
23.409328915027));
#30563=CARTESIAN_POINT('Ctrl Pts',(-14.0700072787421,-35.370094309224,23.4034484503864));
#30564=CARTESIAN_POINT('Ctrl Pts',(-14.0774004327815,-35.2490596530013,
23.3975679857458));
#30565=CARTESIAN_POINT('Ctrl Pts',(-14.0825060895164,-35.1654740271091,
23.3935069809654));
#30566=CARTESIAN_POINT('Ctrl Pts',(-14.0850412353373,-35.0817198648656,
23.3894459761849));
#30567=CARTESIAN_POINT('Ctrl Pts',(-14.0849994926672,-34.9979640950489,
23.3853849714045));
#30568=CARTESIAN_POINT('Ctrl Pts',(-14.0849994926668,-34.9979640942378,
23.3853849713652));
#30569=CARTESIAN_POINT('Ctrl Pts',(-14.0849319581215,-34.8624575358837,
23.3788147639339));
#30570=CARTESIAN_POINT('Ctrl Pts',(-14.0781173618785,-34.7271788853858,
23.3722445565027));
#30571=CARTESIAN_POINT('Ctrl Pts',(-14.0646509392799,-34.5927681964646,
23.3656743490714));
#30572=CARTESIAN_POINT('Ctrl Pts',(-14.0514755036666,-34.4612618988816,
23.3592461128904));
#30573=CARTESIAN_POINT('Ctrl Pts',(-14.0319329338457,-34.330586641113,23.3528178767094));
#30574=CARTESIAN_POINT('Ctrl Pts',(-14.006163324473,-34.2013258376235,23.3463896405285));
#30575=CARTESIAN_POINT('Ctrl Pts',(-13.9795400103922,-34.0677828366469,
23.3397484474721));
#30576=CARTESIAN_POINT('Ctrl Pts',(-13.9462701124896,-33.9357499211005,
23.3331072544157));
#30577=CARTESIAN_POINT('Ctrl Pts',(-13.9065621511345,-33.8058487703296,
23.3264660613593));
#30578=CARTESIAN_POINT('Ctrl Pts',(-13.8668541897794,-33.6759476195587,
23.3198248683029));
#30579=CARTESIAN_POINT('Ctrl Pts',(-13.8207083428049,-33.5481784751292,
23.3131836752465));
#30580=CARTESIAN_POINT('Ctrl Pts',(-13.7683854637982,-33.4231372931563,
23.3065424821901));
#30581=CARTESIAN_POINT('Ctrl Pts',(-13.7225040710322,-33.3134899707813,
23.3007188885187));
#30582=CARTESIAN_POINT('Ctrl Pts',(-13.671759167446,-33.2056699869793,23.2948952948472));
#30583=CARTESIAN_POINT('Ctrl Pts',(-13.6163175769508,-33.1001389043836,
23.2890717011758));
#30584=CARTESIAN_POINT('Ctrl Pts',(-13.5609459342572,-32.994740964924,23.2832554548328));
#30585=CARTESIAN_POINT('Ctrl Pts',(-13.500889578707,-32.8916265412277,23.2774392084898));
#30586=CARTESIAN_POINT('Ctrl Pts',(-13.4363636137902,-32.7912378774936,
23.2716229621468));
#30587=CARTESIAN_POINT('Ctrl Pts',(-13.3719022397202,-32.6909497033657,
23.2658125378984));
#30588=CARTESIAN_POINT('Ctrl Pts',(-13.3029803764778,-32.5933822027107,
23.2600021136501));
#30589=CARTESIAN_POINT('Ctrl Pts',(-13.2298590274944,-32.4989530867029,
23.2541916894018));
#30590=CARTESIAN_POINT('Ctrl Pts',(-13.1539698842108,-32.4009496333409,
23.2481613285776));
#30591=CARTESIAN_POINT('Ctrl Pts',(-13.0735572636369,-32.3063272444996,
23.2421309677534));
#30592=CARTESIAN_POINT('Ctrl Pts',(-12.9889626109017,-32.2155202441692,
23.2361006069293));
#30593=CARTESIAN_POINT('Ctrl Pts',(-12.9075449999923,-32.1281235969616,
23.230296722696));
#30594=CARTESIAN_POINT('Ctrl Pts',(-12.822254116813,-32.0442612501225,23.2244928384628));
#30595=CARTESIAN_POINT('Ctrl Pts',(-12.7334349445223,-31.9642861788264,
23.2186889542296));
#30596=CARTESIAN_POINT('Ctrl Pts',(-12.6446288917731,-31.8843229207035,
23.2128859272921));
#30597=CARTESIAN_POINT('Ctrl Pts',(-12.5522958897155,-31.8082460693974,
23.2070829003546));
#30598=CARTESIAN_POINT('Ctrl Pts',(-12.4568163427328,-31.7363703552515,
23.2012798734172));
#30599=CARTESIAN_POINT('Ctrl Pts',(-12.3613283659046,-31.6644882952318,
23.1954763341331));
#30600=CARTESIAN_POINT('Ctrl Pts',(-12.2626936180526,-31.5968083554396,
23.1896727948491));
#30601=CARTESIAN_POINT('Ctrl Pts',(-12.1613234809668,-31.5336033391111,
23.183869255565));
#30602=CARTESIAN_POINT('Ctrl Pts',(-12.0599204707276,-31.4703778261329,
23.1780638342609));
#30603=CARTESIAN_POINT('Ctrl Pts',(-11.9557806534257,-31.4116303385939,
23.1722584129567));
#30604=CARTESIAN_POINT('Ctrl Pts',(-11.849341555226,-31.3575885992774,23.1664529916525));
#30605=CARTESIAN_POINT('Ctrl Pts',(-11.7427845855771,-31.3034870137366,
23.1606411413816));
#30606=CARTESIAN_POINT('Ctrl Pts',(-11.6339236168275,-31.254101763351,23.1548292911107));
#30607=CARTESIAN_POINT('Ctrl Pts',(-11.5232179180481,-31.209613189378,23.1490174408398));
#30608=CARTESIAN_POINT('Ctrl Pts',(-11.4124395071714,-31.1650953950707,
23.1432017733144));
#30609=CARTESIAN_POINT('Ctrl Pts',(-11.2998143375937,-31.1254808174257,
23.137386105789));
#30610=CARTESIAN_POINT('Ctrl Pts',(-11.1858170787973,-31.0908999941633,
23.1315704382637));
#30611=CARTESIAN_POINT('Ctrl Pts',(-11.0716565312373,-31.0562696376056,
23.1257464404226));
#30612=CARTESIAN_POINT('Ctrl Pts',(-10.9561203658598,-31.0266875277412,
23.1199224425814));
#30613=CARTESIAN_POINT('Ctrl Pts',(-10.8396938113801,-31.0022332105124,
23.1140984447403));
#30614=CARTESIAN_POINT('Ctrl Pts',(-10.8088052118552,-30.9957453468553,
23.1125533063674));
#30615=CARTESIAN_POINT('Ctrl Pts',(-10.7778539682478,-30.9896181299179,
23.1110081679946));
#30616=CARTESIAN_POINT('Ctrl Pts',(-10.7468491860047,-30.9838524313262,
23.1094630296217));
#30617=CARTESIAN_POINT('Ctrl Pts',(-10.6299803966585,-30.9621193254829,
23.1036388167762));
#30618=CARTESIAN_POINT('Ctrl Pts',(-10.5119736988937,-30.9454566791178,
23.0978146039308));
#30619=CARTESIAN_POINT('Ctrl Pts',(-10.3933067302598,-30.9339780108892,
23.0919903910854));
#30620=CARTESIAN_POINT('Ctrl Pts',(-10.2747924252673,-30.9225141098305,
23.0861736710204));
#30621=CARTESIAN_POINT('Ctrl Pts',(-10.1556199421272,-30.9162209598722,
23.0803569509554));
#30622=CARTESIAN_POINT('Ctrl Pts',(-10.0362771935465,-30.9151610845434,
23.0745402308903));
#30623=CARTESIAN_POINT('Ctrl Pts',(-9.91707555089145,-30.9141024623673,
23.0687303882744));
#30624=CARTESIAN_POINT('Ctrl Pts',(-9.79770444961418,-30.9182647993533,
23.0629205456584));
#30625=CARTESIAN_POINT('Ctrl Pts',(-9.67865617645128,-30.9276587634302,
23.0571107030424));
#30626=CARTESIAN_POINT('Ctrl Pts',(-9.55968699035048,-30.9370464868367,
23.0513047200656));
#30627=CARTESIAN_POINT('Ctrl Pts',(-9.44104061140693,-30.9516588936954,
23.0454987370889));
#30628=CARTESIAN_POINT('Ctrl Pts',(-9.32320835253115,-30.9714545967662,
23.0396927541121));
#30629=CARTESIAN_POINT('Ctrl Pts',(-9.20542656315506,-30.9912418210109,
23.0338892579336));
#30630=CARTESIAN_POINT('Ctrl Pts',(-9.08845860212028,-31.0162078574589,
23.0280857617551));
#30631=CARTESIAN_POINT('Ctrl Pts',(-8.97278905483393,-31.0462596602545,
23.0222822655766));
#30632=CARTESIAN_POINT('Ctrl Pts',(-8.85714175272616,-31.0763056835883,
23.016479885507));
#30633=CARTESIAN_POINT('Ctrl Pts',(-8.74279276210235,-31.1114354233229,
23.0106775054373));
#30634=CARTESIAN_POINT('Ctrl Pts',(-8.6302142686793,-31.1515052227825,23.0048751253677));
#30635=CARTESIAN_POINT('Ctrl Pts',(-8.51759076243682,-31.1915910435495,
22.9990704253036));
#30636=CARTESIAN_POINT('Ctrl Pts',(-8.40673955371437,-31.2366207361975,
22.9932657252394));
#30637=CARTESIAN_POINT('Ctrl Pts',(-8.2981153940833,-31.2864015041817,22.9874610251753));
#30638=CARTESIAN_POINT('Ctrl Pts',(-8.18946829498385,-31.3361927849686,
22.981655099263));
#30639=CARTESIAN_POINT('Ctrl Pts',(-8.08304954846559,-31.3907369597228,
22.9758491733506));
#30640=CARTESIAN_POINT('Ctrl Pts',(-7.97929057964607,-31.4497945920704,
22.9700432474382));
#30641=CARTESIAN_POINT('Ctrl Pts',(-7.87543494661103,-31.5089072438516,
22.9642319125932));
#30642=CARTESIAN_POINT('Ctrl Pts',(-7.7742443891795,-31.5725415388876,22.9584205777482));
#30643=CARTESIAN_POINT('Ctrl Pts',(-7.67612259938703,-31.6404138905335,
22.9526092429032));
#30644=CARTESIAN_POINT('Ctrl Pts',(-7.62068930273178,-31.6787579546953,
22.9493261653207));
#30645=CARTESIAN_POINT('Ctrl Pts',(-7.56623488510624,-31.7184538738265,
22.9460430877381));
#30646=CARTESIAN_POINT('Ctrl Pts',(-7.5128274573098,-31.7594448403263,22.9427600101556));
#30647=CARTESIAN_POINT('',(-14.0849999165586,-35.0008256610752,23.4896150285502));
#30648=CARTESIAN_POINT('Ctrl Pts',(-14.0849999165586,-35.0008256610752,
23.4896150285502));
#30649=CARTESIAN_POINT('Ctrl Pts',(-14.0850238118884,-34.8826023086252,
23.4838237303793));
#30650=CARTESIAN_POINT('Ctrl Pts',(-14.0799112176567,-34.7641789032605,
23.4780324322084));
#30651=CARTESIAN_POINT('Ctrl Pts',(-14.0696361080072,-34.6460410357058,
23.4722411340375));
#30652=CARTESIAN_POINT('Ctrl Pts',(-14.0593738341097,-34.5280507469535,
23.4664570704042));
#30653=CARTESIAN_POINT('Ctrl Pts',(-14.043961904424,-34.4103456948312,23.4606730067709));
#30654=CARTESIAN_POINT('Ctrl Pts',(-14.023426288869,-34.2934124979611,23.4548889431376));
#30655=CARTESIAN_POINT('Ctrl Pts',(-14.0029108151613,-34.1765939921055,
23.4491105526591));
#30656=CARTESIAN_POINT('Ctrl Pts',(-13.9772817220656,-34.0605462405772,
23.4433321621806));
#30657=CARTESIAN_POINT('Ctrl Pts',(-13.9466168096245,-33.9457510929628,
23.4375537717021));
#30658=CARTESIAN_POINT('Ctrl Pts',(-13.9159728587045,-33.8310344155189,
23.4317793311404));
#30659=CARTESIAN_POINT('Ctrl Pts',(-13.8803000416625,-33.7175690370024,
23.4260048905788));
#30660=CARTESIAN_POINT('Ctrl Pts',(-13.8397271776587,-33.6058263375213,
23.4202304500171));
#30661=CARTESIAN_POINT('Ctrl Pts',(-13.7991689235688,-33.4941238755552,
23.4144580887782));
#30662=CARTESIAN_POINT('Ctrl Pts',(-13.7537142708979,-33.3841432475838,
23.4086857275393));
#30663=CARTESIAN_POINT('Ctrl Pts',(-13.7035416294541,-33.2763398249944,
23.4029133663003));
#30664=CARTESIAN_POINT('Ctrl Pts',(-13.6533748668638,-33.1685490340008,
23.3971416814234));
#30665=CARTESIAN_POINT('Ctrl Pts',(-13.5984913891949,-33.0629353158317,
23.3913699965464));
#30666=CARTESIAN_POINT('Ctrl Pts',(-13.5391171100777,-32.9599325792623,
23.3855983116695));
#30667=CARTESIAN_POINT('Ctrl Pts',(-13.4797353646703,-32.8569168901429,
23.3798259010056));
#30668=CARTESIAN_POINT('Ctrl Pts',(-13.4158619018825,-32.7565131933414,
23.3740534903418));
#30669=CARTESIAN_POINT('Ctrl Pts',(-13.3477674386447,-32.6591287569048,
23.3682810796779));
#30670=CARTESIAN_POINT('Ctrl Pts',(-13.2796050587149,-32.561647190269,23.3625029116732));
#30671=CARTESIAN_POINT('Ctrl Pts',(-13.2072135061458,-32.467191238724,23.3567247436684));
#30672=CARTESIAN_POINT('Ctrl Pts',(-13.1309056247077,-32.3761373951417,
23.3509465756637));
#30673=CARTESIAN_POINT('Ctrl Pts',(-13.0545602420009,-32.285038803434,23.3451655679964));
#30674=CARTESIAN_POINT('Ctrl Pts',(-12.974294975624,-32.197345955219,23.3393845603292));
#30675=CARTESIAN_POINT('Ctrl Pts',(-12.8904603476396,-32.1133992346147,
23.3336035526619));
#30676=CARTESIAN_POINT('Ctrl Pts',(-12.8064891229381,-32.0293157346542,
23.327813125657));
#30677=CARTESIAN_POINT('Ctrl Pts',(-12.7189372206995,-31.9489908384761,
23.3220226986521));
#30678=CARTESIAN_POINT('Ctrl Pts',(-12.6281895523734,-31.8727256793183,
23.3162322716472));
#30679=CARTESIAN_POINT('Ctrl Pts',(-12.539728024013,-31.7983818128125,23.3105877186558));
#30680=CARTESIAN_POINT('Ctrl Pts',(-12.4482301579867,-31.7278957223736,
23.3049431656644));
#30681=CARTESIAN_POINT('Ctrl Pts',(-12.3540776653063,-31.6615058266179,
23.2992986126729));
#30682=CARTESIAN_POINT('Ctrl Pts',(-12.2569387313005,-31.5930100967772,
23.2934750190015));
#30683=CARTESIAN_POINT('Ctrl Pts',(-12.1566511797001,-31.5286470550448,
23.28765142533));
#30684=CARTESIAN_POINT('Ctrl Pts',(-12.0536016281221,-31.4687190209537,
23.2818278316586));
#30685=CARTESIAN_POINT('Ctrl Pts',(-11.9506820888601,-31.4088665949791,
23.2760115853156));
#30686=CARTESIAN_POINT('Ctrl Pts',(-11.8450078304297,-31.3534382509536,
23.2701953389725));
#30687=CARTESIAN_POINT('Ctrl Pts',(-11.7369961000552,-31.3026942852405,
23.2643790926295));
#30688=CARTESIAN_POINT('Ctrl Pts',(-11.6290924900188,-31.2520011145171,
23.2585686683812));
#30689=CARTESIAN_POINT('Ctrl Pts',(-11.5188564302838,-31.2059831663772,
23.2527582441329));
#30690=CARTESIAN_POINT('Ctrl Pts',(-11.406731010566,-31.164855561532,23.2469478198845));
#30691=CARTESIAN_POINT('Ctrl Pts',(-11.2903614117966,-31.1221711917768,
23.2409174590603));
#30692=CARTESIAN_POINT('Ctrl Pts',(-11.1719569820493,-31.0847549248091,
23.2348870982362));
#30693=CARTESIAN_POINT('Ctrl Pts',(-11.0520377807444,-31.0527932017835,
23.228856737412));
#30694=CARTESIAN_POINT('Ctrl Pts',(-10.9366222721191,-31.022031835135,23.2230528531788));
#30695=CARTESIAN_POINT('Ctrl Pts',(-10.8198041478446,-30.9963228131414,
23.2172489689455));
#30696=CARTESIAN_POINT('Ctrl Pts',(-10.7020632302898,-30.9757817876418,
23.2114450847123));
#30697=CARTESIAN_POINT('Ctrl Pts',(-10.5843397043275,-30.9552437962714,
23.2056420577748));
#30698=CARTESIAN_POINT('Ctrl Pts',(-10.4656940583079,-30.9398723534558,
23.1998390308374));
#30699=CARTESIAN_POINT('Ctrl Pts',(-10.3466157934321,-30.9297318894521,
23.1940360038999));
#30700=CARTESIAN_POINT('Ctrl Pts',(-10.2275270151908,-30.9195905301514,
23.1882324646158));
#30701=CARTESIAN_POINT('Ctrl Pts',(-10.1080059490354,-30.9146811025631,
23.1824289253318));
#30702=CARTESIAN_POINT('Ctrl Pts',(-9.98854605372797,-30.9150160579122,
23.1766253860477));
#30703=CARTESIAN_POINT('Ctrl Pts',(-9.86904741896954,-30.9153511218835,
23.1708199647435));
#30704=CARTESIAN_POINT('Ctrl Pts',(-9.74961040263558,-30.9209339499408,
23.1650145434394));
#30705=CARTESIAN_POINT('Ctrl Pts',(-9.63072665119035,-30.9317249117275,
23.1592091221352));
#30706=CARTESIAN_POINT('Ctrl Pts',(-9.51171124699436,-30.9425278235055,
23.1533972718643));
#30707=CARTESIAN_POINT('Ctrl Pts',(-9.39325073757438,-30.9585503445543,
23.1475854215933));
#30708=CARTESIAN_POINT('Ctrl Pts',(-9.27583000575991,-30.9797011529686,
23.1417735713224));
#30709=CARTESIAN_POINT('Ctrl Pts',(-9.15833215137828,-31.0008658533474,
23.135957903797));
#30710=CARTESIAN_POINT('Ctrl Pts',(-9.0418758320683,-31.0271654593759,23.1301422362716));
#30711=CARTESIAN_POINT('Ctrl Pts',(-8.92693250720849,-31.0584582767762,
23.1243265687463));
#30712=CARTESIAN_POINT('Ctrl Pts',(-8.81182453844754,-31.0897959177584,
23.1185025709051));
#30713=CARTESIAN_POINT('Ctrl Pts',(-8.69823427728588,-31.1261409215892,
23.112678573064));
#30714=CARTESIAN_POINT('Ctrl Pts',(-8.58661502727573,-31.1673027879994,
23.1068545752229));
#30715=CARTESIAN_POINT('Ctrl Pts',(-8.55700183183212,-31.1782232555237,
23.1053094368501));
#30716=CARTESIAN_POINT('Ctrl Pts',(-8.52752724292256,-31.1894825129037,
23.1037642984773));
#30717=CARTESIAN_POINT('Ctrl Pts',(-8.49819943683016,-31.2010764592502,
23.1022191601045));
#30718=CARTESIAN_POINT('Ctrl Pts',(-8.38767210566969,-31.2447704179209,
23.0963960166999));
#30719=CARTESIAN_POINT('Ctrl Pts',(-8.27887501034288,-31.2933624204465,
23.0905728732953));
#30720=CARTESIAN_POINT('Ctrl Pts',(-8.17227282463346,-31.3466948700626,
23.0847497298907));
#30721=CARTESIAN_POINT('Ctrl Pts',(-8.06578901651658,-31.399968096062,23.078933052861));
#30722=CARTESIAN_POINT('Ctrl Pts',(-7.96149563547643,-31.4579711253596,
23.0731163758314));
#30723=CARTESIAN_POINT('Ctrl Pts',(-7.85983920555744,-31.5204976255316,
23.0672996988017));
#30724=CARTESIAN_POINT('Ctrl Pts',(-7.75829239057437,-31.5829567041119,
23.0614892938266));
#30725=CARTESIAN_POINT('Ctrl Pts',(-7.6593772139506,-31.6499293338582,23.0556788888515));
#30726=CARTESIAN_POINT('Ctrl Pts',(-7.56351647800449,-31.7211628513992,
23.0498684838764));
#30727=CARTESIAN_POINT('Ctrl Pts',(-7.54652346404085,-31.733790254541,23.0488384866424));
#30728=CARTESIAN_POINT('Ctrl Pts',(-7.52962636762599,-31.746551435824,23.0478084894084));
#30729=CARTESIAN_POINT('Ctrl Pts',(-7.5128274573098,-31.7594448403263,23.0467784921743));
#30730=CARTESIAN_POINT('Ctrl Pts',(-7.51282745730979,-31.7594448403263,
24.2969436976378));
#30731=CARTESIAN_POINT('Ctrl Pts',(-7.44658657932097,-31.8102856638332,
24.2928610902636));
#30732=CARTESIAN_POINT('Ctrl Pts',(-7.38197060909365,-31.8631081695722,
24.2887784828894));
#30733=CARTESIAN_POINT('Ctrl Pts',(-7.31909951636833,-31.9177933883558,
24.2846958755152));
#30734=CARTESIAN_POINT('Ctrl Pts',(-7.22941768704527,-31.9957985612396,
24.2788722818435));
#30735=CARTESIAN_POINT('Ctrl Pts',(-7.14299859653699,-32.0778469307783,
24.2730486881718));
#30736=CARTESIAN_POINT('Ctrl Pts',(-7.0602280293541,-32.1636351150452,24.2672250945002));
#30737=CARTESIAN_POINT('Ctrl Pts',(-6.97756188953619,-32.2493150647749,
24.2614088481569));
#30738=CARTESIAN_POINT('Ctrl Pts',(-6.89853539850233,-32.3387251533123,
24.2555926018137));
#30739=CARTESIAN_POINT('Ctrl Pts',(-6.82350083292988,-32.4315222326049,
24.2497763554704));
#30740=CARTESIAN_POINT('Ctrl Pts',(-6.74854137737154,-32.5242264215092,
24.2439659312219));
#30741=CARTESIAN_POINT('Ctrl Pts',(-6.67756615311754,-32.6203105406969,
24.2381555069733));
#30742=CARTESIAN_POINT('Ctrl Pts',(-6.61088972602085,-32.7193955733602,
24.2323450827247));
#30743=CARTESIAN_POINT('Ctrl Pts',(-6.54168945825155,-32.8222311794476,
24.2263147219007));
#30744=CARTESIAN_POINT('Ctrl Pts',(-6.47712016569874,-32.9282990467605,
24.2202843610766));
#30745=CARTESIAN_POINT('Ctrl Pts',(-6.41748691440709,-33.0371385704651,
24.2142540002525));
#30746=CARTESIAN_POINT('Ctrl Pts',(-6.36009325305609,-33.1418905105289,
24.208450116019));
#30747=CARTESIAN_POINT('Ctrl Pts',(-6.30727177640957,-33.2492092860382,
24.2026462317856));
#30748=CARTESIAN_POINT('Ctrl Pts',(-6.25924920886292,-33.3586564897599,
24.1968423475521));
#30749=CARTESIAN_POINT('Ctrl Pts',(-6.21123373476303,-33.4680875269592,
24.1910393206144));
#30750=CARTESIAN_POINT('Ctrl Pts',(-6.1680159241084,-33.5796459933206,24.1852362936767));
#30751=CARTESIAN_POINT('Ctrl Pts',(-6.12977506487752,-33.6928718687305,
24.179433266739));
#30752=CARTESIAN_POINT('Ctrl Pts',(-6.09153082937867,-33.8061077408011,
24.1736297274547));
#30753=CARTESIAN_POINT('Ctrl Pts',(-6.05826454962939,-33.9210109277316,
24.1678261881704));
#30754=CARTESIAN_POINT('Ctrl Pts',(-6.03010597741508,-34.037105172179,24.1620226488861));
#30755=CARTESIAN_POINT('Ctrl Pts',(-6.00193827370416,-34.153237064636,24.1562172275817));
#30756=CARTESIAN_POINT('Ctrl Pts',(-5.97888166787577,-34.2705603861392,
24.1504118062773));
#30757=CARTESIAN_POINT('Ctrl Pts',(-5.96101490017246,-34.3885882211053,
24.1446063849729));
#30758=CARTESIAN_POINT('Ctrl Pts',(-5.94312834667766,-34.5067467609741,
24.1387945347017));
#30759=CARTESIAN_POINT('Ctrl Pts',(-5.93044316449474,-34.6256109676421,
24.1329826844306));
#30760=CARTESIAN_POINT('Ctrl Pts',(-5.92298628051657,-34.7446881688134,
24.1271708341594));
#30761=CARTESIAN_POINT('Ctrl Pts',(-5.91552449881696,-34.8638435805297,
24.1213551666338));
#30762=CARTESIAN_POINT('Ctrl Pts',(-5.91329786176668,-34.9832118580281,
24.1155394991082));
#30763=CARTESIAN_POINT('Ctrl Pts',(-5.9162811760783,-35.1023013545734,24.1097238315826));
#30764=CARTESIAN_POINT('Ctrl Pts',(-5.91926876366553,-35.221561433963,24.1038998337412));
#30765=CARTESIAN_POINT('Ctrl Pts',(-5.92748116972549,-35.3405415294495,
24.0980758358999));
#30766=CARTESIAN_POINT('Ctrl Pts',(-5.94084147361191,-35.4587559892262,
24.0922518380585));
#30767=CARTESIAN_POINT('Ctrl Pts',(-5.94438603505235,-35.4901189297243,
24.0907066996879));
#30768=CARTESIAN_POINT('Ctrl Pts',(-5.94829266398164,-35.5214280420674,
24.0891615613173));
#30769=CARTESIAN_POINT('Ctrl Pts',(-5.95255932733317,-35.5526744079856,
24.0876164229467));
#30770=CARTESIAN_POINT('Ctrl Pts',(-5.9686402908021,-35.6704412968797,24.0817928292753));
#30771=CARTESIAN_POINT('Ctrl Pts',(-5.98989138186709,-35.7876956583138,
24.0759692356039));
#30772=CARTESIAN_POINT('Ctrl Pts',(-6.01627033365602,-35.9039485303328,
24.0701456419325));
#30773=CARTESIAN_POINT('Ctrl Pts',(-6.04261600447901,-36.020054732086,24.0643293955896));
#30774=CARTESIAN_POINT('Ctrl Pts',(-6.07407657866469,-36.1351615628471,
24.0585131492466));
#30775=CARTESIAN_POINT('Ctrl Pts',(-6.11055816232707,-36.2487862873044,
24.0526969029036));
#30776=CARTESIAN_POINT('Ctrl Pts',(-6.1470032277229,-36.3622972727855,24.0468864786554));
#30777=CARTESIAN_POINT('Ctrl Pts',(-6.18845917976378,-36.4743287168403,
24.0410760544071));
#30778=CARTESIAN_POINT('Ctrl Pts',(-6.23478145327106,-36.5844097624568,
24.0352656301588));
#30779=CARTESIAN_POINT('Ctrl Pts',(-6.28285712064225,-36.6986576033384,
24.0292352693346));
#30780=CARTESIAN_POINT('Ctrl Pts',(-6.33617468997626,-36.8108040380477,
24.0232049085104));
#30781=CARTESIAN_POINT('Ctrl Pts',(-6.39451615077476,-36.9203414313543,
24.0171745476863));
#30782=CARTESIAN_POINT('Ctrl Pts',(-6.4506665361896,-37.0257650317805,24.0113706634531));
#30783=CARTESIAN_POINT('Ctrl Pts',(-6.51147005382736,-37.128771634547,24.0055667792199));
#30784=CARTESIAN_POINT('Ctrl Pts',(-6.57668431458383,-37.2289312950344,
23.9997628949867));
#30785=CARTESIAN_POINT('Ctrl Pts',(-6.64188894249658,-37.3290761608688,
23.9939598680493));
#30786=CARTESIAN_POINT('Ctrl Pts',(-6.71150279512863,-37.4263745786108,
23.9881568411119));
#30787=CARTESIAN_POINT('Ctrl Pts',(-6.78523940407023,-37.5204244306976,
23.9823538141745));
#30788=CARTESIAN_POINT('Ctrl Pts',(-6.8589825231833,-37.6144825864027,23.9765502748905));
#30789=CARTESIAN_POINT('Ctrl Pts',(-6.93684887036415,-37.7052912848328,
23.9707467356065));
#30790=CARTESIAN_POINT('Ctrl Pts',(-7.01851124291595,-37.7924809384097,
23.9649431963225));
#30791=CARTESIAN_POINT('Ctrl Pts',(-7.10020009762288,-37.8796988665745,
23.9591377750184));
#30792=CARTESIAN_POINT('Ctrl Pts',(-7.1856871469023,-37.9632951179562,23.9533323537143));
#30793=CARTESIAN_POINT('Ctrl Pts',(-7.27460831114308,-38.0429369271001,
23.9475269324102));
#30794=CARTESIAN_POINT('Ctrl Pts',(-7.36362794734274,-38.1226669321761,
23.9417150821393));
#30795=CARTESIAN_POINT('Ctrl Pts',(-7.45608898519387,-38.1984334812067,
23.9359032318685));
#30796=CARTESIAN_POINT('Ctrl Pts',(-7.55159412814588,-38.2699439883078,
23.9300913815976));
#30797=CARTESIAN_POINT('Ctrl Pts',(-7.64716199938854,-38.3415014638939,
23.9242757140723));
#30798=CARTESIAN_POINT('Ctrl Pts',(-7.74577762104494,-38.4087971008214,
23.918460046547));
#30799=CARTESIAN_POINT('Ctrl Pts',(-7.84701598392944,-38.4715824671963,
23.9126443790216));
#30800=CARTESIAN_POINT('Ctrl Pts',(-7.94839935983691,-38.5344577668288,
23.9068203811806));
#30801=CARTESIAN_POINT('Ctrl Pts',(-8.05241262046843,-38.5928097020728,
23.9009963833395));
#30802=CARTESIAN_POINT('Ctrl Pts',(-8.1586074155696,-38.6464363905058,23.8951723854985));
#30803=CARTESIAN_POINT('Ctrl Pts',(-8.1867814735695,-38.660663843262,23.8936272471251));
#30804=CARTESIAN_POINT('Ctrl Pts',(-8.21510898346397,-38.6745589665825,
23.8920821087517));
#30805=CARTESIAN_POINT('Ctrl Pts',(-8.24358137181638,-38.688118572195,23.8905369703783));
#30806=CARTESIAN_POINT('Ctrl Pts',(-8.35089319804208,-38.7392244373991,
23.8847133767068));
#30807=CARTESIAN_POINT('Ctrl Pts',(-8.46061043672435,-38.7857252081772,
23.8788897830354));
#30808=CARTESIAN_POINT('Ctrl Pts',(-8.57230096503302,-38.8273882041876,
23.8730661893639));
#30809=CARTESIAN_POINT('Ctrl Pts',(-8.68385057915002,-38.86899863614,23.8672499430209));
#30810=CARTESIAN_POINT('Ctrl Pts',(-8.79736815192777,-38.90578329173,23.8614336966779));
#30811=CARTESIAN_POINT('Ctrl Pts',(-8.91239846827213,-38.9375560831794,
23.8556174503349));
#30812=CARTESIAN_POINT('Ctrl Pts',(-9.0273136386351,-38.9692970698893,23.8498070260865));
#30813=CARTESIAN_POINT('Ctrl Pts',(-9.14373814878656,-38.9960360648753,
23.8439966018382));
#30814=CARTESIAN_POINT('Ctrl Pts',(-9.26119894214271,-39.0176358716177,
23.8381861775899));
#30815=CARTESIAN_POINT('Ctrl Pts',(-9.38310586947834,-39.0400532757214,
23.8321558167657));
#30816=CARTESIAN_POINT('Ctrl Pts',(-9.50612866105545,-39.0569345899521,
23.8261254559415));
#30817=CARTESIAN_POINT('Ctrl Pts',(-9.62972324000022,-39.0681838848562,
23.8200950951174));
#30818=CARTESIAN_POINT('Ctrl Pts',(-9.74867609356334,-39.0790107005698,
23.8142912108841));
#30819=CARTESIAN_POINT('Ctrl Pts',(-9.86815811762749,-39.0846208606733,
23.8084873266509));
#30820=CARTESIAN_POINT('Ctrl Pts',(-9.9876768500406,-39.0849814124394,23.8026834424177));
#30821=CARTESIAN_POINT('Ctrl Pts',(-10.1071779282588,-39.085341910948,23.7968804154802));
#30822=CARTESIAN_POINT('Ctrl Pts',(-10.2267152958181,-39.0804543419597,
23.7910773885428));
#30823=CARTESIAN_POINT('Ctrl Pts',(-10.3457956016437,-39.070337873185,23.7852743616053));
#30824=CARTESIAN_POINT('Ctrl Pts',(-10.4648864210151,-39.0602205112318,
23.7794708223212));
#30825=CARTESIAN_POINT('Ctrl Pts',(-10.5835196915284,-39.0448733661736,
23.7736672830372));
#30826=CARTESIAN_POINT('Ctrl Pts',(-10.7012069401969,-39.0243675064561,
23.7678637437531));
#30827=CARTESIAN_POINT('Ctrl Pts',(-10.8189323534677,-39.0038549969274,
23.762058322449));
#30828=CARTESIAN_POINT('Ctrl Pts',(-10.9357107327008,-38.9781805157537,
23.7562529011448));
#30829=CARTESIAN_POINT('Ctrl Pts',(-11.0510641872897,-38.9474661587146,
23.7504474798406));
#30830=CARTESIAN_POINT('Ctrl Pts',(-11.1665453851525,-38.916717788368,23.7446356295697));
#30831=CARTESIAN_POINT('Ctrl Pts',(-11.2805981137806,-38.8809185067376,
23.7388237792988));
#30832=CARTESIAN_POINT('Ctrl Pts',(-11.3927598792847,-38.8402402162697,
23.7330119290279));
#30833=CARTESIAN_POINT('Ctrl Pts',(-11.5049953132385,-38.7995352080822,
23.7271962615025));
#30834=CARTESIAN_POINT('Ctrl Pts',(-11.6153369340792,-38.7539449646672,
23.7213805939771));
#30835=CARTESIAN_POINT('Ctrl Pts',(-11.7233439859836,-38.7036887701283,
23.7155649264518));
#30836=CARTESIAN_POINT('Ctrl Pts',(-11.8315057463271,-38.6533605890174,
23.7097409286107));
#30837=CARTESIAN_POINT('Ctrl Pts',(-11.937325902232,-38.5983533046048,23.7039169307695));
#30838=CARTESIAN_POINT('Ctrl Pts',(-12.0403898357863,-38.5389312395157,
23.6980929329284));
#30839=CARTESIAN_POINT('Ctrl Pts',(-12.0677332591422,-38.523166241748,23.6965477945556));
#30840=CARTESIAN_POINT('Ctrl Pts',(-12.094882848487,-38.5070907303515,23.6950026561827));
#30841=CARTESIAN_POINT('Ctrl Pts',(-12.1218312375957,-38.4907101282065,
23.6934575178098));
#30842=CARTESIAN_POINT('Ctrl Pts',(-12.2233991431152,-38.4289719870394,
23.6876339241383));
#30843=CARTESIAN_POINT('Ctrl Pts',(-12.3224340400302,-38.3626976832686,
23.6818103304668));
#30844=CARTESIAN_POINT('Ctrl Pts',(-12.4185044472203,-38.292121085072,23.6759867367953));
#30845=CARTESIAN_POINT('Ctrl Pts',(-12.5144536473216,-38.2216335297374,
23.6701704904523));
#30846=CARTESIAN_POINT('Ctrl Pts',(-12.6074454705769,-38.1468547157318,
23.6643542441092));
#30847=CARTESIAN_POINT('Ctrl Pts',(-12.6970747462037,-38.0680633652828,
23.6585379977662));
#30848=CARTESIAN_POINT('Ctrl Pts',(-12.7866143024312,-37.9893508854102,
23.6527275735178));
#30849=CARTESIAN_POINT('Ctrl Pts',(-12.8727977022076,-37.9066341276154,
23.6469171492694));
#30850=CARTESIAN_POINT('Ctrl Pts',(-12.9552508859334,-37.8202335366401,
23.641106725021));
#30851=CARTESIAN_POINT('Ctrl Pts',(-13.040825093205,-37.7305625045902,23.6350763641969));
#30852=CARTESIAN_POINT('Ctrl Pts',(-13.1223807507815,-37.6369235130602,
23.6290460033727));
#30853=CARTESIAN_POINT('Ctrl Pts',(-13.1995393829107,-37.5397190272161,
23.6230156425486));
#30854=CARTESIAN_POINT('Ctrl Pts',(-13.2738002408485,-37.4461651588414,
23.6172117583153));
#30855=CARTESIAN_POINT('Ctrl Pts',(-13.3439881105524,-37.3493091269306,
23.611407874082));
#30856=CARTESIAN_POINT('Ctrl Pts',(-13.4098054814972,-37.249544749133,23.6056039898487));
#30857=CARTESIAN_POINT('Ctrl Pts',(-13.4756131305124,-37.1497951076009,
23.5998009629112));
#30858=CARTESIAN_POINT('Ctrl Pts',(-13.5370513397981,-37.0471383152607,
23.5939979359737));
#30859=CARTESIAN_POINT('Ctrl Pts',(-13.5938657035847,-36.9419975037567,
23.5881949090362));
#30860=CARTESIAN_POINT('Ctrl Pts',(-13.6506850834855,-36.8368474094186,
23.5823913697521));
#30861=CARTESIAN_POINT('Ctrl Pts',(-13.7028796120812,-36.7292132191305,
23.576587830468));
#30862=CARTESIAN_POINT('Ctrl Pts',(-13.7502409658695,-36.6195424347372,
23.5707842911839));
#30863=CARTESIAN_POINT('Ctrl Pts',(-13.7976176783925,-36.5098360853874,
23.5649788698797));
#30864=CARTESIAN_POINT('Ctrl Pts',(-13.8401579372119,-36.3980922031405,
23.5591734485755));
#30865=CARTESIAN_POINT('Ctrl Pts',(-13.8777018974908,-36.2847774103697,
23.5533680272713));
#30866=CARTESIAN_POINT('Ctrl Pts',(-13.9152874342306,-36.1713371319542,
23.5475561770003));
#30867=CARTESIAN_POINT('Ctrl Pts',(-13.9478654997089,-36.0563228583936,
23.5417443267294));
#30868=CARTESIAN_POINT('Ctrl Pts',(-13.975326345867,-35.9402156368918,23.5359324764584));
#30869=CARTESIAN_POINT('Ctrl Pts',(-14.0028052284563,-35.8240321555435,
23.530116808933));
#30870=CARTESIAN_POINT('Ctrl Pts',(-14.0251601218921,-35.7067546968224,
23.5243011414076));
#30871=CARTESIAN_POINT('Ctrl Pts',(-14.0423328227829,-35.5888720997399,
23.5184854738822));
#30872=CARTESIAN_POINT('Ctrl Pts',(-14.0595301217134,-35.4708206485661,
23.512661476041));
#30873=CARTESIAN_POINT('Ctrl Pts',(-14.0715303713908,-35.3521627337771,
23.5068374781998));
#30874=CARTESIAN_POINT('Ctrl Pts',(-14.0783273651944,-35.2333900218666,
23.5010134803587));
#30875=CARTESIAN_POINT('Ctrl Pts',(-14.0801306446992,-35.2018789739962,
23.4994683419862));
#30876=CARTESIAN_POINT('Ctrl Pts',(-14.0815679668199,-35.1703598310385,
23.4979232036138));
#30877=CARTESIAN_POINT('Ctrl Pts',(-14.0826398292009,-35.1388417265166,
23.4963780652414));
#30878=CARTESIAN_POINT('Ctrl Pts',(-14.0842036685506,-35.0928570432686,
23.4941237196927));
#30879=CARTESIAN_POINT('Ctrl Pts',(-14.0849906149495,-35.0468457909019,
23.4918693741441));
#30880=CARTESIAN_POINT('Ctrl Pts',(-14.0849999165584,-35.0008256619994,
23.4896150285955));
#30881=CARTESIAN_POINT('Origin',(-10.,-35.,32.7603849714045));
#30882=CARTESIAN_POINT('',(-7.5128274573098,-31.7594448403263,25.5469376127646));
#30883=CARTESIAN_POINT('',(-7.5128274573098,-31.7594448403263,25.442544535095));
#30884=CARTESIAN_POINT('',(-7.5128274573098,-31.7594448403263,32.7603849714045));
#30885=CARTESIAN_POINT('',(-14.0849984277889,-35.0035839868969,24.6353849714293));
#30886=CARTESIAN_POINT('Ctrl Pts',(-7.5128274573098,-31.7594448403263,25.442544535095));
#30887=CARTESIAN_POINT('Ctrl Pts',(-7.41827395874041,-31.8320160060276,
25.4367332032128));
#30888=CARTESIAN_POINT('Ctrl Pts',(-7.32679695411755,-31.908807538792,25.4309218713305));
#30889=CARTESIAN_POINT('Ctrl Pts',(-7.23879181561765,-31.9895258907441,
25.4251105394482));
#30890=CARTESIAN_POINT('Ctrl Pts',(-7.15085584740807,-32.0701807996754,
25.4193037751573));
#30891=CARTESIAN_POINT('Ctrl Pts',(-7.06638661541144,-32.1547561116215,
25.4134970108664));
#30892=CARTESIAN_POINT('Ctrl Pts',(-6.98574673250876,-32.2429178032894,
25.4076902465755));
#30893=CARTESIAN_POINT('Ctrl Pts',(-6.90514184249712,-32.3310412380507,
25.4018860020734));
#30894=CARTESIAN_POINT('Ctrl Pts',(-6.82836327281571,-32.4227476575573,
25.3960817575712));
#30895=CARTESIAN_POINT('Ctrl Pts',(-6.75573670076481,-32.517666290517,25.3902775130691));
#30896=CARTESIAN_POINT('Ctrl Pts',(-6.68312451340452,-32.6125661235371,
25.3844744181774));
#30897=CARTESIAN_POINT('Ctrl Pts',(-6.61466293637587,-32.7106765806863,
25.3786713232856));
#30898=CARTESIAN_POINT('Ctrl Pts',(-6.55063685704201,-32.811594437038,25.3728682283939));
#30899=CARTESIAN_POINT('Ctrl Pts',(-6.48660834875909,-32.9125161218974,
25.3670649133509));
#30900=CARTESIAN_POINT('Ctrl Pts',(-6.42701589139308,-33.0162450728324,
25.3612615983078));
#30901=CARTESIAN_POINT('Ctrl Pts',(-6.37210024043593,-33.1223503163383,
25.3554582832648));
#30902=CARTESIAN_POINT('Ctrl Pts',(-6.31716954611168,-33.2284846258773,
25.3496533784856));
#30903=CARTESIAN_POINT('Ctrl Pts',(-6.2669183936464,-33.3369961600095,25.3438484737064));
#30904=CARTESIAN_POINT('Ctrl Pts',(-6.22154062098647,-33.447431250751,25.3380435689272));
#30905=CARTESIAN_POINT('Ctrl Pts',(-6.17611367088984,-33.557986023759,25.3322323731751));
#30906=CARTESIAN_POINT('Ctrl Pts',(-6.13557080051017,-33.6704681372962,
25.326421177423));
#30907=CARTESIAN_POINT('Ctrl Pts',(-6.10005697200426,-33.7844057509237,
25.3206099816709));
#30908=CARTESIAN_POINT('Ctrl Pts',(-6.06452142162713,-33.8984130539729,
25.3147952315274));
#30909=CARTESIAN_POINT('Ctrl Pts',(-6.03402114392668,-34.0138772360793,
25.3089804813839));
#30910=CARTESIAN_POINT('Ctrl Pts',(-6.00865026741219,-34.1303148200807,
25.3031657312405));
#30911=CARTESIAN_POINT('Ctrl Pts',(-5.98324158955583,-34.2469258902807,
25.297342317409));
#30912=CARTESIAN_POINT('Ctrl Pts',(-5.9629776421869,-34.3645128566708,25.2915189035776));
#30913=CARTESIAN_POINT('Ctrl Pts',(-5.94790090175037,-34.4825853713273,
25.2856954897461));
#30914=CARTESIAN_POINT('Ctrl Pts',(-5.9406875692008,-34.5390761172393,25.2829093291223));
#30915=CARTESIAN_POINT('Ctrl Pts',(-5.93466085033665,-34.5956779772144,
25.2801231684984));
#30916=CARTESIAN_POINT('Ctrl Pts',(-5.92982117855723,-34.6523372877647,
25.2773370078746));
#30917=CARTESIAN_POINT('Ctrl Pts',(-5.91970536480497,-34.7707657802292,
25.2715134142015));
#30918=CARTESIAN_POINT('Ctrl Pts',(-5.91474633401457,-34.8898271180746,
25.2656898205283));
#30919=CARTESIAN_POINT('Ctrl Pts',(-5.91500999150824,-35.0090349611213,
25.2598662268552));
#30920=CARTESIAN_POINT('Ctrl Pts',(-5.91527331635881,-35.1280924057676,
25.2540499805105));
#30921=CARTESIAN_POINT('Ctrl Pts',(-5.9207462228401,-35.2472955832397,25.2482337341658));
#30922=CARTESIAN_POINT('Ctrl Pts',(-5.93144287956194,-35.3661529157781,
25.2424174878211));
#30923=CARTESIAN_POINT('Ctrl Pts',(-5.94212882887143,-35.4848912714712,
25.236607063571));
#30924=CARTESIAN_POINT('Ctrl Pts',(-5.95802808957765,-35.6032840665822,
25.230796639321));
#30925=CARTESIAN_POINT('Ctrl Pts',(-5.97910278763899,-35.7208402094968,
25.2249862150709));
#30926=CARTESIAN_POINT('Ctrl Pts',(-6.0009752066032,-35.84284609552,25.2189558542474));
#30927=CARTESIAN_POINT('Ctrl Pts',(-6.02842260533274,-35.9639502916357,
25.2129254934239));
#30928=CARTESIAN_POINT('Ctrl Pts',(-6.06134350857702,-36.0836097279794,
25.2068951326003));
#30929=CARTESIAN_POINT('Ctrl Pts',(-6.09302803242764,-36.1987752274389,
25.2010912483653));
#30930=CARTESIAN_POINT('Ctrl Pts',(-6.12978223035001,-36.3126020999863,
25.1952873641303));
#30931=CARTESIAN_POINT('Ctrl Pts',(-6.17146381683887,-36.4246177361756,
25.1894834798954));
#30932=CARTESIAN_POINT('Ctrl Pts',(-6.21313924651174,-36.5366168264576,
25.1836804529561));
#30933=CARTESIAN_POINT('Ctrl Pts',(-6.25974047496469,-36.6468048298346,
25.1778774260169));
#30934=CARTESIAN_POINT('Ctrl Pts',(-6.31107611100897,-36.7547266286323,
25.1720743990777));
#30935=CARTESIAN_POINT('Ctrl Pts',(-6.36241627945318,-36.8626579557965,
25.1662708597918));
#30936=CARTESIAN_POINT('Ctrl Pts',(-6.41849151115981,-36.9683223118065,
25.160467320506));
#30937=CARTESIAN_POINT('Ctrl Pts',(-6.47906354243825,-37.0712873923752,
25.1546637812202));
#30938=CARTESIAN_POINT('Ctrl Pts',(-6.53965521652011,-37.1742858633189,
25.1488583599142));
#30939=CARTESIAN_POINT('Ctrl Pts',(-6.60474638338353,-37.2745829661884,
25.1430529386083));
#30940=CARTESIAN_POINT('Ctrl Pts',(-6.67405472993515,-37.3717742431634,
25.1372475173023));
#30941=CARTESIAN_POINT('Ctrl Pts',(-6.74343982906545,-37.4690731504816,
25.1314356670296));
#30942=CARTESIAN_POINT('Ctrl Pts',(-6.8170511926523,-37.5632590338801,25.1256238167569));
#30943=CARTESIAN_POINT('Ctrl Pts',(-6.89456529351481,-37.6539593598541,
25.1198119664842));
#30944=CARTESIAN_POINT('Ctrl Pts',(-6.97213030605494,-37.7447192582891,
25.113996298957));
#30945=CARTESIAN_POINT('Ctrl Pts',(-7.05360288281086,-37.8319887422407,
25.1081806314299));
#30946=CARTESIAN_POINT('Ctrl Pts',(-7.13862278213925,-37.9154322864899,
25.1023649639027));
#30947=CARTESIAN_POINT('Ctrl Pts',(-7.22376446329271,-37.9989953546056,
25.0965409660598));
#30948=CARTESIAN_POINT('Ctrl Pts',(-7.31246330611885,-38.0787212727478,
25.0907169682169));
#30949=CARTESIAN_POINT('Ctrl Pts',(-7.40432609491705,-38.1543148191757,
25.084892970374));
#30950=CARTESIAN_POINT('Ctrl Pts',(-7.42869779323927,-38.1743701988648,
25.083347832018));
#30951=CARTESIAN_POINT('Ctrl Pts',(-7.45329203647413,-38.1941349514844,
25.0818026936621));
#30952=CARTESIAN_POINT('Ctrl Pts',(-7.47810115818965,-38.2136040875745,
25.0802575553061));
#30953=CARTESIAN_POINT('Ctrl Pts',(-7.57160621141045,-38.2869828483039,
25.0744339616351));
#30954=CARTESIAN_POINT('Ctrl Pts',(-7.66846731883909,-38.3563955273518,
25.0686103679641));
#30955=CARTESIAN_POINT('Ctrl Pts',(-7.76831384647973,-38.4215204094358,
25.062786774293));
#30956=CARTESIAN_POINT('Ctrl Pts',(-7.86803440289478,-38.4865631268076,
25.0569705279504));
#30957=CARTESIAN_POINT('Ctrl Pts',(-7.97073254893948,-38.5473285858543,
25.0511542816078));
#30958=CARTESIAN_POINT('Ctrl Pts',(-8.07600490987609,-38.6035354713363,
25.0453380352652));
#30959=CARTESIAN_POINT('Ctrl Pts',(-8.18117189259851,-38.6596860934158,
25.0395276110173));
#30960=CARTESIAN_POINT('Ctrl Pts',(-8.28890760584245,-38.7112870285497,
25.0337171867694));
#30961=CARTESIAN_POINT('Ctrl Pts',(-8.39878055358211,-38.7581007549576,
25.0279067625215));
#30962=CARTESIAN_POINT('Ctrl Pts',(-8.51281241966153,-38.8066864777424,
25.0218764016972));
#30963=CARTESIAN_POINT('Ctrl Pts',(-8.62914613917075,-38.8501151747488,
25.0158460408728));
#30964=CARTESIAN_POINT('Ctrl Pts',(-8.74727187910843,-38.8881740258285,
25.0098156800485));
#30965=CARTESIAN_POINT('Ctrl Pts',(-8.86096128169724,-38.9248035364225,
25.0040117958157));
#30966=CARTESIAN_POINT('Ctrl Pts',(-8.97631010603435,-38.9564591313934,
24.9982079115829));
#30967=CARTESIAN_POINT('Ctrl Pts',(-9.09284507948462,-38.9830007469475,
24.9924040273501));
#30968=CARTESIAN_POINT('Ctrl Pts',(-9.20936283947303,-39.0095384420213,
24.9866010004131));
#30969=CARTESIAN_POINT('Ctrl Pts',(-9.32706600210986,-39.0309635692546,
24.980797973476));
#30970=CARTESIAN_POINT('Ctrl Pts',(-9.44546900642645,-39.0471867237831,
24.974994946539));
#30971=CARTESIAN_POINT('Ctrl Pts',(-9.56388246449013,-39.0634113106466,
24.9691914072554));
#30972=CARTESIAN_POINT('Ctrl Pts',(-9.68299548250737,-39.0744329562123,
24.9633878679718));
#30973=CARTESIAN_POINT('Ctrl Pts',(-9.80231588616976,-39.080213963892,24.9575843286881));
#30974=CARTESIAN_POINT('Ctrl Pts',(-9.92167498404754,-39.085996846285,24.9517789073844));
#30975=CARTESIAN_POINT('Ctrl Pts',(-10.0412411936723,-39.0865356911639,
24.9459734860807));
#30976=CARTESIAN_POINT('Ctrl Pts',(-10.1605214844387,-39.0818449080083,
24.9401680647769));
#30977=CARTESIAN_POINT('Ctrl Pts',(-10.2799338670867,-39.0771489302446,
24.9343562145064));
#30978=CARTESIAN_POINT('Ctrl Pts',(-10.3990592905948,-39.0672117805131,
24.9285443642359));
#30979=CARTESIAN_POINT('Ctrl Pts',(-10.5174088328726,-39.0520998383141,
24.9227325139655));
#30980=CARTESIAN_POINT('Ctrl Pts',(-10.6358361077652,-39.0369779705104,
24.9169168464405));
#30981=CARTESIAN_POINT('Ctrl Pts',(-10.7534860850764,-39.016674610663,24.9111011789156));
#30982=CARTESIAN_POINT('Ctrl Pts',(-10.8698806698468,-38.9913071317836,
24.9052855113906));
#30983=CARTESIAN_POINT('Ctrl Pts',(-10.9864419772915,-38.96590331673,24.8994615135499));
#30984=CARTESIAN_POINT('Ctrl Pts',(-11.1017439096846,-38.9354210084424,
24.8936375157092));
#30985=CARTESIAN_POINT('Ctrl Pts',(-11.215324005556,-38.9000272513816,24.8878135178685));
#30986=CARTESIAN_POINT('Ctrl Pts',(-11.2454574241779,-38.8906370946827,
24.8862683794916));
#30987=CARTESIAN_POINT('Ctrl Pts',(-11.2754697617168,-38.8809014966569,
24.8847232411146));
#30988=CARTESIAN_POINT('Ctrl Pts',(-11.3053526426733,-38.8708241342466,
24.8831781027377));
#30989=CARTESIAN_POINT('Ctrl Pts',(-11.4179805852676,-38.8328427697088,
24.8773545090664));
#30990=CARTESIAN_POINT('Ctrl Pts',(-11.529131078261,-38.7898804367481,24.8715309153951));
#30991=CARTESIAN_POINT('Ctrl Pts',(-11.6383318802172,-38.7420707703441,
24.8657073217238));
#30992=CARTESIAN_POINT('Ctrl Pts',(-11.7473949091413,-38.6943214229359,
24.859891075381));
#30993=CARTESIAN_POINT('Ctrl Pts',(-11.8545127688016,-38.6417370682555,
24.8540748290381));
#30994=CARTESIAN_POINT('Ctrl Pts',(-11.9592290599098,-38.5845008705265,
24.8482585826953));
#30995=CARTESIAN_POINT('Ctrl Pts',(-12.0638405294327,-38.5273219665473,
24.8424481584471));
#30996=CARTESIAN_POINT('Ctrl Pts',(-12.1660548565831,-38.4655006778096,
24.836637734199));
#30997=CARTESIAN_POINT('Ctrl Pts',(-12.2654368545928,-38.3992676943502,
24.8308273099508));
#30998=CARTESIAN_POINT('Ctrl Pts',(-12.3685806667888,-38.3305276554705,
24.8247969491266));
#30999=CARTESIAN_POINT('Ctrl Pts',(-12.4686730836362,-38.2570355191049,
24.8187665883024));
#31000=CARTESIAN_POINT('Ctrl Pts',(-12.5652566366224,-38.179101034611,24.8127362274781));
#31001=CARTESIAN_POINT('Ctrl Pts',(-12.6582128919258,-38.1040934622701,
24.8069323432451));
#31002=CARTESIAN_POINT('Ctrl Pts',(-12.7479187422822,-38.0249714780818,
24.801128459012));
#31003=CARTESIAN_POINT('Ctrl Pts',(-12.8339976115558,-37.9420541357521,
24.795324574779));
#31004=CARTESIAN_POINT('Ctrl Pts',(-12.9200637660598,-37.8591490412006,
24.7895215478417));
#31005=CARTESIAN_POINT('Ctrl Pts',(-13.0025037108978,-37.7724499866039,
24.7837185209044));
#31006=CARTESIAN_POINT('Ctrl Pts',(-13.0809765035836,-37.6823140726555,
24.7779154939671));
#31007=CARTESIAN_POINT('Ctrl Pts',(-13.1594562245964,-37.5921702006485,
24.7721119546833));
#31008=CARTESIAN_POINT('Ctrl Pts',(-13.2339678289217,-37.4985891739701,
24.7663084153994));
#31009=CARTESIAN_POINT('Ctrl Pts',(-13.3042099961916,-37.4019619691135,
24.7605048761155));
#31010=CARTESIAN_POINT('Ctrl Pts',(-13.3744749421769,-37.3053034291816,
24.7546994548116));
#31011=CARTESIAN_POINT('Ctrl Pts',(-13.4404674576149,-37.2055970765999,
24.7488940335076));
#31012=CARTESIAN_POINT('Ctrl Pts',(-13.5019293327585,-37.1032631666926,
24.7430886122036));
#31013=CARTESIAN_POINT('Ctrl Pts',(-13.56345927124,-37.0008159314518,24.7372767619329));
#31014=CARTESIAN_POINT('Ctrl Pts',(-13.62044834417,-36.8957356809831,24.7314649116622));
#31015=CARTESIAN_POINT('Ctrl Pts',(-13.6726840601652,-36.7884677224396,
24.7256530613915));
#31016=CARTESIAN_POINT('Ctrl Pts',(-13.7249540848592,-36.681129309725,24.7198373938663));
#31017=CARTESIAN_POINT('Ctrl Pts',(-13.772464372894,-36.5716007010673,24.7140217263411));
#31018=CARTESIAN_POINT('Ctrl Pts',(-13.8150510174271,-36.460346100905,24.7082060588159));
#31019=CARTESIAN_POINT('Ctrl Pts',(-13.8576986627298,-36.3489321405416,
24.702382060975));
#31020=CARTESIAN_POINT('Ctrl Pts',(-13.8954084592957,-36.2357876401169,
24.6965580631341));
#31021=CARTESIAN_POINT('Ctrl Pts',(-13.928066613758,-36.1213909567496,24.6907340652932));
#31022=CARTESIAN_POINT('Ctrl Pts',(-13.936731000161,-36.09104089306,24.6891889269185));
#31023=CARTESIAN_POINT('Ctrl Pts',(-13.9450400971673,-36.0606027397414,
24.6876437885439));
#31024=CARTESIAN_POINT('Ctrl Pts',(-13.9529923889216,-36.0300855173858,
24.6860986501693));
#31025=CARTESIAN_POINT('Ctrl Pts',(-13.9915465443555,-35.882132478129,24.6786075385624));
#31026=CARTESIAN_POINT('Ctrl Pts',(-14.0218101378458,-35.7319372299034,
24.6711164269556));
#31027=CARTESIAN_POINT('Ctrl Pts',(-14.0435706506774,-35.5803114620445,
24.6636253153487));
#31028=CARTESIAN_POINT('Ctrl Pts',(-14.0649246235175,-35.4315184370933,
24.6562741561627));
#31029=CARTESIAN_POINT('Ctrl Pts',(-14.0780902876876,-35.281347638357,24.6489229969766));
#31030=CARTESIAN_POINT('Ctrl Pts',(-14.0829121862388,-35.1305874399128,
24.6415718377906));
#31031=CARTESIAN_POINT('Ctrl Pts',(-14.0842649181091,-35.0882932848111,
24.6395095490035));
#31032=CARTESIAN_POINT('Ctrl Pts',(-14.0849612552969,-35.0459528838747,
24.6374472602164));
#31033=CARTESIAN_POINT('Ctrl Pts',(-14.0849984277889,-35.0035839868969,
24.6353849714293));
#31034=CARTESIAN_POINT('Ctrl Pts',(-14.0849984277894,-35.0035839863873,
24.6353849714045));
#31035=CARTESIAN_POINT('Ctrl Pts',(-14.0851020062225,-34.8855261338036,
24.6296385535608));
#31036=CARTESIAN_POINT('Ctrl Pts',(-14.0800834836686,-34.7673454041044,
24.6238921357172));
#31037=CARTESIAN_POINT('Ctrl Pts',(-14.0699376947858,-34.64952580614,24.6181457178735));
#31038=CARTESIAN_POINT('Ctrl Pts',(-14.0597976023172,-34.5317723586983,
24.6124025263907));
#31039=CARTESIAN_POINT('Ctrl Pts',(-14.0445360024405,-34.4143800553256,
24.606659334908));
#31040=CARTESIAN_POINT('Ctrl Pts',(-14.024199795063,-34.2978312101673,24.6009161434252));
#31041=CARTESIAN_POINT('Ctrl Pts',(-14.003869129897,-34.1813141279799,24.5951745171302));
#31042=CARTESIAN_POINT('Ctrl Pts',(-13.9784666777729,-34.065640458642,24.5894328908351));
#31043=CARTESIAN_POINT('Ctrl Pts',(-13.9480909112641,-33.9512849975357,
24.5836912645401));
#31044=CARTESIAN_POINT('Ctrl Pts',(-13.9177158689797,-33.8369322629124,
24.577949775138));
#31045=CARTESIAN_POINT('Ctrl Pts',(-13.8823678558292,-33.7238980779719,
24.5722082857358));
#31046=CARTESIAN_POINT('Ctrl Pts',(-13.8421957448839,-33.612643932512,24.5664667963337));
#31047=CARTESIAN_POINT('Ctrl Pts',(-13.8020146008844,-33.5013647705742,
24.5607240159069));
#31048=CARTESIAN_POINT('Ctrl Pts',(-13.7570073454803,-33.391866836607,24.5549812354801));
#31049=CARTESIAN_POINT('Ctrl Pts',(-13.7073714148722,-33.284592703703,24.5492384550533));
#31050=CARTESIAN_POINT('Ctrl Pts',(-13.657683486109,-33.1772061913812,24.5434896585413));
#31051=CARTESIAN_POINT('Ctrl Pts',(-13.6033573785645,-33.0720485102435,
24.5377408620293));
#31052=CARTESIAN_POINT('Ctrl Pts',(-13.5446370465651,-32.9695386711099,
24.5319920655174));
#31053=CARTESIAN_POINT('Ctrl Pts',(-13.4858820406438,-32.866968300674,24.5262398743835));
#31054=CARTESIAN_POINT('Ctrl Pts',(-13.4227278681906,-32.7670492372735,
24.5204876832497));
#31055=CARTESIAN_POINT('Ctrl Pts',(-13.3554614679228,-32.6701709639363,
24.5147354921159));
#31056=CARTESIAN_POINT('Ctrl Pts',(-13.2880945699607,-32.5731479520216,
24.5089747070638));
#31057=CARTESIAN_POINT('Ctrl Pts',(-13.216603432795,-32.4791751304297,24.5032139220117));
#31058=CARTESIAN_POINT('Ctrl Pts',(-13.1413149418207,-32.3886085248868,
24.4974531369597));
#31059=CARTESIAN_POINT('Ctrl Pts',(-13.1045735045829,-32.3444112350974,
24.49464182384));
#31060=CARTESIAN_POINT('Ctrl Pts',(-13.0669282755438,-32.3010245830022,
24.4918305107204));
#31061=CARTESIAN_POINT('Ctrl Pts',(-13.0284202510578,-32.2584865889471,
24.4890191976008));
#31062=CARTESIAN_POINT('Ctrl Pts',(-12.9486514461778,-32.1703697615308,
24.4831956039294));
#31063=CARTESIAN_POINT('Ctrl Pts',(-12.8649049617741,-32.0855952341254,
24.477372010258));
#31064=CARTESIAN_POINT('Ctrl Pts',(-12.777491772723,-32.0045426972737,24.4715484165866));
#31065=CARTESIAN_POINT('Ctrl Pts',(-12.690188868394,-31.9235924202366,24.4657321702437));
#31066=CARTESIAN_POINT('Ctrl Pts',(-12.599228757394,-31.8463550690208,24.4599159239007));
#31067=CARTESIAN_POINT('Ctrl Pts',(-12.5049615082197,-31.773176044105,24.4540996775577));
#31068=CARTESIAN_POINT('Ctrl Pts',(-12.4107886210817,-31.7000702717967,
24.4482892533095));
#31069=CARTESIAN_POINT('Ctrl Pts',(-12.3133155022263,-31.6310149930897,
24.4424788290612));
#31070=CARTESIAN_POINT('Ctrl Pts',(-12.2129273337946,-31.566317193545,24.4366684048129));
#31071=CARTESIAN_POINT('Ctrl Pts',(-12.1087392655482,-31.4991704484687,
24.4306380439887));
#31072=CARTESIAN_POINT('Ctrl Pts',(-12.001411434772,-31.4367178844015,24.4246076831645));
#31073=CARTESIAN_POINT('Ctrl Pts',(-11.891410407136,-31.379255370538,24.4185773223403));
#31074=CARTESIAN_POINT('Ctrl Pts',(-11.7855405846588,-31.3239509222747,
24.4127734381071));
#31075=CARTESIAN_POINT('Ctrl Pts',(-11.6771951282978,-31.273268676305,24.406969553874));
#31076=CARTESIAN_POINT('Ctrl Pts',(-11.5668168564593,-31.2274266159139,
24.4011656696408));
#31077=CARTESIAN_POINT('Ctrl Pts',(-11.4564548886719,-31.1815913268852,
24.3953626427034));
#31078=CARTESIAN_POINT('Ctrl Pts',(-11.3440610795513,-31.1405949582078,
24.389559615766));
#31079=CARTESIAN_POINT('Ctrl Pts',(-11.2300989151555,-31.1046076373575,
24.3837565888286));
#31080=CARTESIAN_POINT('Ctrl Pts',(-11.1161266890924,-31.0686171392032,
24.3779530495446));
#31081=CARTESIAN_POINT('Ctrl Pts',(-11.0005862218465,-31.0376366911359,
24.3721495102606));
#31082=CARTESIAN_POINT('Ctrl Pts',(-10.8839562508819,-31.0117865720944,
24.3663459709766));
#31083=CARTESIAN_POINT('Ctrl Pts',(-10.7672884581778,-30.9859280701607,
24.3605405496725));
#31084=CARTESIAN_POINT('Ctrl Pts',(-10.6495308575516,-30.9652032943032,
24.3547351283683));
#31085=CARTESIAN_POINT('Ctrl Pts',(-10.5311718307159,-30.949681310532,24.3489297070642));
#31086=CARTESIAN_POINT('Ctrl Pts',(-10.4126817322134,-30.9341421376005,
24.3431178567934));
#31087=CARTESIAN_POINT('Ctrl Pts',(-10.2935892831711,-30.9238173105511,
24.3373060065225));
#31088=CARTESIAN_POINT('Ctrl Pts',(-10.174387593082,-30.9187239780457,24.3314941562517));
#31089=CARTESIAN_POINT('Ctrl Pts',(-10.0551076106827,-30.9136273002122,
24.3256784887263));
#31090=CARTESIAN_POINT('Ctrl Pts',(-9.93571865174241,-30.9137689594669,
24.319862821201));
#31091=CARTESIAN_POINT('Ctrl Pts',(-9.81671176650925,-30.9191140148904,
24.3140471536757));
#31092=CARTESIAN_POINT('Ctrl Pts',(-9.69753441676367,-30.9244667265287,
24.3082231558346));
#31093=CARTESIAN_POINT('Ctrl Pts',(-9.57874063835113,-30.935037674659,24.3023991579936));
#31094=CARTESIAN_POINT('Ctrl Pts',(-9.46081446167688,-30.9507403201001,
24.2965751601525));
#31095=CARTESIAN_POINT('Ctrl Pts',(-9.42952800419933,-30.9549063175294,
24.2950300217791));
#31096=CARTESIAN_POINT('Ctrl Pts',(-9.39830254646571,-30.9594332434406,
24.2934848834058));
#31097=CARTESIAN_POINT('Ctrl Pts',(-9.36714696466196,-30.964318888259,24.2919397450324));
#31098=CARTESIAN_POINT('Ctrl Pts',(-9.24972281422751,-30.9827326895398,
24.2861161798703));
#31099=CARTESIAN_POINT('Ctrl Pts',(-9.13291364202334,-31.0063053837757,
24.2802926147083));
#31100=CARTESIAN_POINT('Ctrl Pts',(-9.01720746820394,-31.0349850139696,
24.2744690495462));
#31101=CARTESIAN_POINT('Ctrl Pts',(-8.90164192701255,-31.0636297861119,
24.2686525625136));
#31102=CARTESIAN_POINT('Ctrl Pts',(-8.78717711113497,-31.0973690534386,
24.2628360754809));
#31103=CARTESIAN_POINT('Ctrl Pts',(-8.67429385790801,-31.1360993510677,
24.2570195884483));
#31104=CARTESIAN_POINT('Ctrl Pts',(-8.56153930379801,-31.1747854919688,
24.2512097328399));
#31105=CARTESIAN_POINT('Ctrl Pts',(-8.4503631069613,-31.2184512041946,24.2453998772315));
#31106=CARTESIAN_POINT('Ctrl Pts',(-8.34123302693219,-31.2669426566071,
24.2395900216232));
#31107=CARTESIAN_POINT('Ctrl Pts',(-8.23217569903826,-31.3154017819409,
24.2337840391852));
#31108=CARTESIAN_POINT('Ctrl Pts',(-8.12516214700283,-31.3686800843982,
24.2279780567473));
#31109=CARTESIAN_POINT('Ctrl Pts',(-8.02064187895397,-31.4265749722921,
24.2221720743094));
#31110=CARTESIAN_POINT('Ctrl Pts',(-7.91616129546325,-31.4844478784873,
24.2163682963037));
#31111=CARTESIAN_POINT('Ctrl Pts',(-7.81417247073959,-31.5469336882283,
24.210564518298));
#31112=CARTESIAN_POINT('Ctrl Pts',(-7.71510143287545,-31.6137833002077,
24.2047607402923));
#31113=CARTESIAN_POINT('Ctrl Pts',(-7.64622177178903,-31.6602608451711,
24.2007256330533));
#31114=CARTESIAN_POINT('Ctrl Pts',(-7.57875203275188,-31.7088467835586,
24.1966905258144));
#31115=CARTESIAN_POINT('Ctrl Pts',(-7.51282745730979,-31.7594448403263,
24.1926554185755));
#31116=CARTESIAN_POINT('',(-14.084998667809,-34.9967009094586,24.7396150285614));
#31117=CARTESIAN_POINT('Ctrl Pts',(-14.084998667809,-34.9967009094586,24.7396150285614));
#31118=CARTESIAN_POINT('Ctrl Pts',(-14.0848838734084,-34.854560229187,24.7327077308575));
#31119=CARTESIAN_POINT('Ctrl Pts',(-14.0773464015934,-34.7127316992153,
24.7258004331536));
#31120=CARTESIAN_POINT('Ctrl Pts',(-14.0625068059482,-34.5719071927434,
24.7188931354498));
#31121=CARTESIAN_POINT('Ctrl Pts',(-14.0474942948948,-34.4294417569901,
24.7119053518465));
#31122=CARTESIAN_POINT('Ctrl Pts',(-14.0250085659472,-34.2880039250404,
24.7049175682433));
#31123=CARTESIAN_POINT('Ctrl Pts',(-13.9952238380687,-34.1482890844142,
24.6979297846401));
#31124=CARTESIAN_POINT('Ctrl Pts',(-13.9681220732687,-34.0211595445654,
24.6915714499774));
#31125=CARTESIAN_POINT('Ctrl Pts',(-13.9349776994646,-33.8954563163519,
24.6852131153147));
#31126=CARTESIAN_POINT('Ctrl Pts',(-13.8959562242754,-33.7716881102385,
24.6788547806521));
#31127=CARTESIAN_POINT('Ctrl Pts',(-13.8602164861204,-33.658328908492,24.673031186981));
#31128=CARTESIAN_POINT('Ctrl Pts',(-13.8194674520747,-33.5463480602667,
24.66720759331));
#31129=CARTESIAN_POINT('Ctrl Pts',(-13.7738333631692,-33.4362203649393,
24.661383999639));
#31130=CARTESIAN_POINT('Ctrl Pts',(-13.7282568484454,-33.3262316120577,
24.6555677532964));
#31131=CARTESIAN_POINT('Ctrl Pts',(-13.677807692304,-33.2180917356995,24.6497515069538));
#31132=CARTESIAN_POINT('Ctrl Pts',(-13.6226599695282,-33.1122606787011,
24.6439352606112));
#31133=CARTESIAN_POINT('Ctrl Pts',(-13.5675674499272,-33.0065355591748,
24.6381248363633));
#31134=CARTESIAN_POINT('Ctrl Pts',(-13.5077859079211,-32.9031150213197,
24.6323144121154));
#31135=CARTESIAN_POINT('Ctrl Pts',(-13.4435373555386,-32.802438742376,24.6265039878675));
#31136=CARTESIAN_POINT('Ctrl Pts',(-13.3768568625529,-32.6979516580294,
24.6204736270431));
#31137=CARTESIAN_POINT('Ctrl Pts',(-13.3053646778812,-32.5964211032718,
24.6144432662188));
#31138=CARTESIAN_POINT('Ctrl Pts',(-13.2293614153236,-32.4983106009699,
24.6084129053945));
#31139=CARTESIAN_POINT('Ctrl Pts',(-13.1562125358369,-32.403884742556,24.6026090211617));
#31140=CARTESIAN_POINT('Ctrl Pts',(-13.0788855771601,-32.3126270336723,
24.5968051369289));
#31141=CARTESIAN_POINT('Ctrl Pts',(-12.9976920602387,-32.2249203052918,
24.5910012526961));
#31142=CARTESIAN_POINT('Ctrl Pts',(-12.9165105364681,-32.137226532133,24.585198225759));
#31143=CARTESIAN_POINT('Ctrl Pts',(-12.8314638675763,-32.0530829959458,
24.579395198822));
#31144=CARTESIAN_POINT('Ctrl Pts',(-12.7429023208597,-31.9728376557868,
24.573592171885));
#31145=CARTESIAN_POINT('Ctrl Pts',(-12.6543329550848,-31.8925852308035,
24.5677886326013));
#31146=CARTESIAN_POINT('Ctrl Pts',(-12.5622483970904,-31.8162319603357,
24.5619850933177));
#31147=CARTESIAN_POINT('Ctrl Pts',(-12.4670335692747,-31.7440868610984,
24.5561815540341));
#31148=CARTESIAN_POINT('Ctrl Pts',(-12.3717878644006,-31.6719183660468,
24.5503761327304));
#31149=CARTESIAN_POINT('Ctrl Pts',(-12.2734101961745,-31.603961002706,24.5445707114266));
#31150=CARTESIAN_POINT('Ctrl Pts',(-12.1723156152313,-31.5404812664444,
24.5387652901229));
#31151=CARTESIAN_POINT('Ctrl Pts',(-12.0711090813969,-31.4769312322505,
24.5329534398524));
#31152=CARTESIAN_POINT('Ctrl Pts',(-11.9671799751828,-31.4178689401148,
24.5271415895819));
#31153=CARTESIAN_POINT('Ctrl Pts',(-11.8609693010197,-31.36351567298,24.5213297393114));
#31154=CARTESIAN_POINT('Ctrl Pts',(-11.7546888671157,-31.3091267063276,
24.5155140717865));
#31155=CARTESIAN_POINT('Ctrl Pts',(-11.646124251332,-31.2594530937943,24.5096984042615));
#31156=CARTESIAN_POINT('Ctrl Pts',(-11.5357363154174,-31.2146679181995,
24.5038827367366));
#31157=CARTESIAN_POINT('Ctrl Pts',(-11.4251902607043,-31.1698185926765,
24.4980587388959));
#31158=CARTESIAN_POINT('Ctrl Pts',(-11.3128160564153,-31.1298718163044,
24.4922347410552));
#31159=CARTESIAN_POINT('Ctrl Pts',(-11.1990897082743,-31.0949508490275,
24.4864107432145));
#31160=CARTESIAN_POINT('Ctrl Pts',(-11.1689174881278,-31.0856861260357,
24.4848656048375));
#31161=CARTESIAN_POINT('Ctrl Pts',(-11.138650147959,-31.0767748751365,24.4833204664606));
#31162=CARTESIAN_POINT('Ctrl Pts',(-11.1082966765157,-31.0682187908247,
24.4817753280836));
#31163=CARTESIAN_POINT('Ctrl Pts',(-10.9938903537229,-31.0359697564614,
24.475951493395));
#31164=CARTESIAN_POINT('Ctrl Pts',(-10.8778908004923,-31.0086663255076,
24.4701276587064));
#31165=CARTESIAN_POINT('Ctrl Pts',(-10.7607632878861,-30.986464872484,24.4643038240178));
#31166=CARTESIAN_POINT('Ctrl Pts',(-10.6437847222405,-30.9642916522716,
24.458487395296));
#31167=CARTESIAN_POINT('Ctrl Pts',(-10.5256814480284,-30.9472075803738,
24.4526709665742));
#31168=CARTESIAN_POINT('Ctrl Pts',(-10.4069336155649,-30.9353191967236,
24.4468545378524));
#31169=CARTESIAN_POINT('Ctrl Pts',(-10.2883058386614,-30.9234428323796,
24.4410439896137));
#31170=CARTESIAN_POINT('Ctrl Pts',(-10.1690352039896,-30.9167517461939,
24.4352334413749));
#31171=CARTESIAN_POINT('Ctrl Pts',(-10.0496111757909,-30.9153012679958,
24.4294228931361));
#31172=CARTESIAN_POINT('Ctrl Pts',(-9.93027871601185,-30.9138519019524,
24.4236168001374));
#31173=CARTESIAN_POINT('Ctrl Pts',(-9.81079350370928,-30.9176351517055,
24.4178107071387));
#31174=CARTESIAN_POINT('Ctrl Pts',(-9.69164860837947,-30.9266543948143,
24.41200461414));
#31175=CARTESIAN_POINT('Ctrl Pts',(-9.57255221940145,-30.9356699660027,
24.4062008849218));
#31176=CARTESIAN_POINT('Ctrl Pts',(-9.45379627834284,-30.9499172604491,
24.4003971557037));
#31177=CARTESIAN_POINT('Ctrl Pts',(-9.33587187471168,-30.9693475921135,
24.3945934264856));
#31178=CARTESIAN_POINT('Ctrl Pts',(-9.21796765035289,-30.9887745988516,
24.388790690404));
#31179=CARTESIAN_POINT('Ctrl Pts',(-9.10089508298854,-31.0133828117266,
24.3829879543224));
#31180=CARTESIAN_POINT('Ctrl Pts',(-8.98513753636315,-31.0430720021839,
24.3771852182408));
#31181=CARTESIAN_POINT('Ctrl Pts',(-8.86937247998878,-31.0727631187218,
24.3713821057078));
#31182=CARTESIAN_POINT('Ctrl Pts',(-8.75492300914663,-31.1075357657944,
24.3655789931748));
#31183=CARTESIAN_POINT('Ctrl Pts',(-8.64225911212408,-31.1472393428361,
24.3597758806418));
#31184=CARTESIAN_POINT('Ctrl Pts',(-8.52950544824127,-31.1869745543725,
24.3539681443811));
#31185=CARTESIAN_POINT('Ctrl Pts',(-8.41854058517941,-31.2316484066746,
24.3481604081203));
#31186=CARTESIAN_POINT('Ctrl Pts',(-8.30981632203141,-31.2810614236413,
24.3423526718595));
#31187=CARTESIAN_POINT('Ctrl Pts',(-8.20104516977009,-31.3304957507783,
24.3365424309176));
#31188=CARTESIAN_POINT('Ctrl Pts',(-8.09451690735335,-31.3846731312039,
24.3307321899758));
#31189=CARTESIAN_POINT('Ctrl Pts',(-7.99065905712731,-31.4433479260271,
24.3249219490339));
#31190=CARTESIAN_POINT('Ctrl Pts',(-7.8866674396989,-31.5020982930207,24.3191042245973));
#31191=CARTESIAN_POINT('Ctrl Pts',(-7.78535345118204,-31.5653574290668,
24.3132865001607));
#31192=CARTESIAN_POINT('Ctrl Pts',(-7.68711615261122,-31.6328360140189,
24.3074687757241));
#31193=CARTESIAN_POINT('Ctrl Pts',(-7.62787447660817,-31.6735287501286,
24.303960416362));
#31194=CARTESIAN_POINT('Ctrl Pts',(-7.56975108065747,-31.7157551433316,
24.3004520569999));
#31195=CARTESIAN_POINT('Ctrl Pts',(-7.51282745730979,-31.7594448403263,
24.2969436976378));
#31196=CARTESIAN_POINT('Ctrl Pts',(-7.5128274573098,-31.7594448403263,25.5469376127646));
#31197=CARTESIAN_POINT('Ctrl Pts',(-7.41802267680316,-31.8322088685169,
25.5411329166442));
#31198=CARTESIAN_POINT('Ctrl Pts',(-7.32644265542362,-31.9091144685266,
25.5353282205238));
#31199=CARTESIAN_POINT('Ctrl Pts',(-7.23845612486566,-31.9898338209149,
25.5295235244034));
#31200=CARTESIAN_POINT('Ctrl Pts',(-7.1503751931797,-32.0706397774443,25.5237126003995));
#31201=CARTESIAN_POINT('Ctrl Pts',(-7.06589575190499,-32.1552673801606,
25.5179016763955));
#31202=CARTESIAN_POINT('Ctrl Pts',(-6.98535008939967,-32.243351506536,25.5120907523916));
#31203=CARTESIAN_POINT('Ctrl Pts',(-6.90475677099751,-32.3314877490392,
25.5062763902784));
#31204=CARTESIAN_POINT('Ctrl Pts',(-6.8281021292086,-32.4230842760319,25.5004620281651));
#31205=CARTESIAN_POINT('Ctrl Pts',(-6.75567743765626,-32.5177437458096,
25.4946476660519));
#31206=CARTESIAN_POINT('Ctrl Pts',(-6.68314294086342,-32.6125467316399,
25.4888244886103));
#31207=CARTESIAN_POINT('Ctrl Pts',(-6.61485143510181,-32.7104215998079,
25.4830013111688));
#31208=CARTESIAN_POINT('Ctrl Pts',(-6.55105043615599,-32.8109426900923,
25.4771781337273));
#31209=CARTESIAN_POINT('Ctrl Pts',(-6.51450889549698,-32.8685153859499,
25.4738429527935));
#31210=CARTESIAN_POINT('Ctrl Pts',(-6.47943954707083,-32.9269556736248,
25.4705077718596));
#31211=CARTESIAN_POINT('Ctrl Pts',(-6.44588189144434,-32.9861803778797,
25.4671725909258));
#31212=CARTESIAN_POINT('Ctrl Pts',(-6.38728652428349,-33.0895932422775,
25.4613489972415));
#31213=CARTESIAN_POINT('Ctrl Pts',(-6.33311386295757,-33.1957323819947,
25.4555254035572));
#31214=CARTESIAN_POINT('Ctrl Pts',(-6.28362667866039,-33.3041832833601,
25.4497018098729));
#31215=CARTESIAN_POINT('Ctrl Pts',(-6.23420192979541,-33.4124973578078,
25.4438855635169));
#31216=CARTESIAN_POINT('Ctrl Pts',(-6.1894510682932,-33.5231170245795,25.4380693171609));
#31217=CARTESIAN_POINT('Ctrl Pts',(-6.14959202975056,-33.6356014282331,
25.4322530708049));
#31218=CARTESIAN_POINT('Ctrl Pts',(-6.10977289032432,-33.7479732343811,
25.4264426465434));
#31219=CARTESIAN_POINT('Ctrl Pts',(-6.07483596799803,-33.8622056813432,
25.420632222282));
#31220=CARTESIAN_POINT('Ctrl Pts',(-6.04495169710551,-33.9778366462393,
25.4148217980205));
#31221=CARTESIAN_POINT('Ctrl Pts',(-6.01393624484356,-34.0978444819544,
25.4087914372012));
#31222=CARTESIAN_POINT('Ctrl Pts',(-5.9883636943945,-34.219358393308,25.4027610763819));
#31223=CARTESIAN_POINT('Ctrl Pts',(-5.96836835913738,-34.3418424866376,
25.3967307155626));
#31224=CARTESIAN_POINT('Ctrl Pts',(-5.9491239698242,-34.4597265604176,25.3909268313159));
#31225=CARTESIAN_POINT('Ctrl Pts',(-5.9350455056025,-34.5785088186769,25.3851229470693));
#31226=CARTESIAN_POINT('Ctrl Pts',(-5.92620079771629,-34.6977003812893,
25.3793190628226));
#31227=CARTESIAN_POINT('Ctrl Pts',(-5.91735739628789,-34.8168743380351,
25.3735160358716));
#31228=CARTESIAN_POINT('Ctrl Pts',(-5.91374624398939,-34.9364570717935,
25.3677130089207));
#31229=CARTESIAN_POINT('Ctrl Pts',(-5.91538324624638,-35.055955115541,25.3619099819697));
#31230=CARTESIAN_POINT('Ctrl Pts',(-5.91702039303356,-35.1754637097173,
25.3561064426721));
#31231=CARTESIAN_POINT('Ctrl Pts',(-5.92390661004875,-35.2948871906974,
25.3503029033744));
#31232=CARTESIAN_POINT('Ctrl Pts',(-5.9360056866268,-35.4137332726169,25.3444993640768));
#31233=CARTESIAN_POINT('Ctrl Pts',(-5.94810868679438,-35.5326178949358,
25.338693942759));
#31234=CARTESIAN_POINT('Ctrl Pts',(-5.96542786715174,-35.6509243397802,
25.3328885214412));
#31235=CARTESIAN_POINT('Ctrl Pts',(-5.98787536717209,-35.7681672543499,
25.3270831001234));
#31236=CARTESIAN_POINT('Ctrl Pts',(-6.01034772572099,-35.8855400045957,
25.3212712498389));
#31237=CARTESIAN_POINT('Ctrl Pts',(-6.03795966314973,-36.0018464723642,
25.3154593995543));
#31238=CARTESIAN_POINT('Ctrl Pts',(-6.07057254486996,-36.1166131267678,
25.3096475492698));
#31239=CARTESIAN_POINT('Ctrl Pts',(-6.10320684690608,-36.2314551605266,
25.3038318817307));
#31240=CARTESIAN_POINT('Ctrl Pts',(-6.1408485062443,-36.3447549801565,25.2980162141917));
#31241=CARTESIAN_POINT('Ctrl Pts',(-6.18331008292999,-36.4560573741911,
25.2922005466526));
#31242=CARTESIAN_POINT('Ctrl Pts',(-6.22583248123856,-36.5675191968847,
25.2863765487979));
#31243=CARTESIAN_POINT('Ctrl Pts',(-6.27318841536203,-36.6769775099537,
25.2805525509432));
#31244=CARTESIAN_POINT('Ctrl Pts',(-6.32514366484224,-36.7839999764436,
25.2747285530885));
#31245=CARTESIAN_POINT('Ctrl Pts',(-6.33892767454405,-36.8123936177247,
25.2731834148448));
#31246=CARTESIAN_POINT('Ctrl Pts',(-6.35303517529878,-36.8406159585932,
25.2716382766011));
#31247=CARTESIAN_POINT('Ctrl Pts',(-6.36746128086554,-36.8686592664231,
25.2700931383574));
#31248=CARTESIAN_POINT('Ctrl Pts',(-6.42183297051223,-36.9743539061123,
25.2642695446883));
#31249=CARTESIAN_POINT('Ctrl Pts',(-6.48090920439806,-37.0778439671083,
25.2584459510193));
#31250=CARTESIAN_POINT('Ctrl Pts',(-6.54448733684962,-37.1786824538715,
25.2526223573502));
#31251=CARTESIAN_POINT('Ctrl Pts',(-6.6079852560432,-37.279393717905,25.2468061110096));
#31252=CARTESIAN_POINT('Ctrl Pts',(-6.67597356092467,-37.3774597191691,
25.2409898646691));
#31253=CARTESIAN_POINT('Ctrl Pts',(-6.74820299708228,-37.472456521724,25.2351736183285));
#31254=CARTESIAN_POINT('Ctrl Pts',(-6.82036013117569,-37.5673582319552,
25.2293631940825));
#31255=CARTESIAN_POINT('Ctrl Pts',(-6.89674970512961,-37.659196532226,25.2235527698366));
#31256=CARTESIAN_POINT('Ctrl Pts',(-6.97707863859834,-37.7475755572471,
25.2177423455907));
#31257=CARTESIAN_POINT('Ctrl Pts',(-7.06044818839508,-37.8392999112166,
25.2117119847656));
#31258=CARTESIAN_POINT('Ctrl Pts',(-7.14806097694068,-37.9272975549707,
25.2056816239406));
#31259=CARTESIAN_POINT('Ctrl Pts',(-7.23954242393988,-38.011162395284,25.1996512631155));
#31260=CARTESIAN_POINT('Ctrl Pts',(-7.32758818820707,-38.0918776026046,
25.1938473788847));
#31261=CARTESIAN_POINT('Ctrl Pts',(-7.41921694001888,-38.1687645312801,
25.1880434946539));
#31262=CARTESIAN_POINT('Ctrl Pts',(-7.51405697676403,-38.2414984629372,
25.182239610423));
#31263=CARTESIAN_POINT('Ctrl Pts',(-7.60888300462153,-38.3142216510149,
25.176436583488));
#31264=CARTESIAN_POINT('Ctrl Pts',(-7.70691905016476,-38.3827928135887,
25.170633556553));
#31265=CARTESIAN_POINT('Ctrl Pts',(-7.80776111059125,-38.4469281471716,
25.1648305296179));
#31266=CARTESIAN_POINT('Ctrl Pts',(-7.90861207431753,-38.511069143234,25.1590269903362));
#31267=CARTESIAN_POINT('Ctrl Pts',(-8.01226920092535,-38.5707733124886,
25.1532234510546));
#31268=CARTESIAN_POINT('Ctrl Pts',(-8.11830090735696,-38.6258010873111,
25.1474199117729));
#31269=CARTESIAN_POINT('Ctrl Pts',(-8.22436699863475,-38.6808467069994,
25.1416144904711));
#31270=CARTESIAN_POINT('Ctrl Pts',(-8.33280883894015,-38.731212728281,25.1358090691693));
#31271=CARTESIAN_POINT('Ctrl Pts',(-8.44317233125726,-38.7767065824389,
25.1300036478676));
#31272=CARTESIAN_POINT('Ctrl Pts',(-8.55365804092722,-38.8222508168294,
25.124191797599));
#31273=CARTESIAN_POINT('Ctrl Pts',(-8.66606927263863,-38.8629119585548,
25.1183799473305));
#31274=CARTESIAN_POINT('Ctrl Pts',(-8.77993398439098,-38.8985463852,25.1125680970619));
#31275=CARTESIAN_POINT('Ctrl Pts',(-8.89387348309799,-38.9342042167281,
25.1067524295389));
#31276=CARTESIAN_POINT('Ctrl Pts',(-9.00926796929501,-38.9648286535075,
25.1009367620158));
#31277=CARTESIAN_POINT('Ctrl Pts',(-9.1256339694926,-38.9903269345625,25.0951210944928));
#31278=CARTESIAN_POINT('Ctrl Pts',(-9.24216665142073,-39.0158617391519,
25.089297096654));
#31279=CARTESIAN_POINT('Ctrl Pts',(-9.35967322399059,-39.0362556628802,
25.0834730988152));
#31280=CARTESIAN_POINT('Ctrl Pts',(-9.47766370192668,-39.0514676096095,
25.0776491009763));
#31281=CARTESIAN_POINT('Ctrl Pts',(-9.50896721934635,-39.0555034220561,
25.0761039625805));
#31282=CARTESIAN_POINT('Ctrl Pts',(-9.54030479206342,-39.0591747752014,
25.0745588241847));
#31283=CARTESIAN_POINT('Ctrl Pts',(-9.5716672742707,-39.0624815170126,25.0730136857889));
#31284=CARTESIAN_POINT('Ctrl Pts',(-9.68987180102332,-39.0749445563952,
25.0671900921193));
#31285=CARTESIAN_POINT('Ctrl Pts',(-9.80881134156663,-39.0822643809811,
25.0613664984498));
#31286=CARTESIAN_POINT('Ctrl Pts',(-9.92800095875183,-39.0843654510902,
25.0555429047802));
#31287=CARTESIAN_POINT('Ctrl Pts',(-10.0470402005301,-39.0864638703873,
25.0497266584391));
#31288=CARTESIAN_POINT('Ctrl Pts',(-10.1663284867357,-39.0833566239609,
25.043910412098));
#31289=CARTESIAN_POINT('Ctrl Pts',(-10.2853746173914,-39.0750197947677,
25.0380941657569));
#31290=CARTESIAN_POINT('Ctrl Pts',(-10.4043015822128,-39.0666913107866,
25.0322837415105));
#31291=CARTESIAN_POINT('Ctrl Pts',(-10.5229864687091,-39.0531436864692,
25.0264733172641));
#31292=CARTESIAN_POINT('Ctrl Pts',(-10.6409375306042,-39.034405046827,25.0206628930177));
#31293=CARTESIAN_POINT('Ctrl Pts',(-10.7633532842126,-39.0149571109073,
25.0146325321928));
#31294=CARTESIAN_POINT('Ctrl Pts',(-10.8849781138591,-38.9899174057335,
25.008602171368));
#31295=CARTESIAN_POINT('Ctrl Pts',(-11.0052670436135,-38.9593766139412,
25.0025718105431));
#31296=CARTESIAN_POINT('Ctrl Pts',(-11.1210383950901,-38.9299828139616,
24.9967679263119));
#31297=CARTESIAN_POINT('Ctrl Pts',(-11.2355719480392,-38.8954937836691,
24.9909640420807));
#31298=CARTESIAN_POINT('Ctrl Pts',(-11.34839236355,-38.8560424056175,24.9851601578495));
#31299=CARTESIAN_POINT('Ctrl Pts',(-11.4611961142788,-38.8165968549562,
24.9793571309141));
#31300=CARTESIAN_POINT('Ctrl Pts',(-11.5722868454571,-38.7721905489741,
24.9735541039786));
#31301=CARTESIAN_POINT('Ctrl Pts',(-11.6812057324157,-38.723005813223,24.9677510770432));
#31302=CARTESIAN_POINT('Ctrl Pts',(-11.7901342357727,-38.6738167349743,
24.9619475377612));
#31303=CARTESIAN_POINT('Ctrl Pts',(-11.8968901414922,-38.6198485562083,
24.9561439984792));
#31304=CARTESIAN_POINT('Ctrl Pts',(-12.001036504013,-38.5613309182955,24.9503404591972));
#31305=CARTESIAN_POINT('Ctrl Pts',(-12.1052166399838,-38.5027943037957,
24.9445350378952));
#31306=CARTESIAN_POINT('Ctrl Pts',(-12.206785193959,-38.4397054959587,24.9387296165931));
#31307=CARTESIAN_POINT('Ctrl Pts',(-12.3053321875756,-38.372338729269,24.932924195291));
#31308=CARTESIAN_POINT('Ctrl Pts',(-12.4039883128662,-38.3048973601207,
24.9271123450222));
#31309=CARTESIAN_POINT('Ctrl Pts',(-12.4996158614001,-38.2331688063547,
24.9213004947534));
#31310=CARTESIAN_POINT('Ctrl Pts',(-12.5918359553017,-38.1574691417028,
24.9154886444846));
#31311=CARTESIAN_POINT('Ctrl Pts',(-12.6841166198558,-38.081719757105,24.9096729769614));
#31312=CARTESIAN_POINT('Ctrl Pts',(-12.7729850694245,-38.0019943392835,
24.9038573094381));
#31313=CARTESIAN_POINT('Ctrl Pts',(-12.8580986988468,-37.9186464033264,
24.8980416419149));
#31314=CARTESIAN_POINT('Ctrl Pts',(-12.9433342443526,-37.835179080451,24.8922176440759));
#31315=CARTESIAN_POINT('Ctrl Pts',(-13.0248039568207,-37.7480791799022,
24.8863936462369));
#31316=CARTESIAN_POINT('Ctrl Pts',(-13.1022048725458,-37.6577339838203,
24.8805696483979));
#31317=CARTESIAN_POINT('Ctrl Pts',(-13.1227397576548,-37.6337649105307,
24.8790245100054));
#31318=CARTESIAN_POINT('Ctrl Pts',(-13.1429884873955,-37.6095675710598,
24.877479371613));
#31319=CARTESIAN_POINT('Ctrl Pts',(-13.1629459212134,-37.5851495313578,
24.8759342332205));
#31320=CARTESIAN_POINT('Ctrl Pts',(-13.2378042578983,-37.4935599084697,
24.8701385737653));
#31321=CARTESIAN_POINT('Ctrl Pts',(-13.3088098080699,-37.3985584740394,
24.8643429143101));
#31322=CARTESIAN_POINT('Ctrl Pts',(-13.3756340199529,-37.3005042845726,
24.8585472548549));
#31323=CARTESIAN_POINT('Ctrl Pts',(-13.4423779072389,-37.2025679590211,
24.8527585619467));
#31324=CARTESIAN_POINT('Ctrl Pts',(-13.5049502169776,-37.1015865095326,
24.8469698690384));
#31325=CARTESIAN_POINT('Ctrl Pts',(-13.5630617794871,-36.9979528912259,
24.8411811761302));
#31326=CARTESIAN_POINT('Ctrl Pts',(-13.6211175348196,-36.8944187969974,
24.8353980423671));
#31327=CARTESIAN_POINT('Ctrl Pts',(-13.6747208597772,-36.7882379551329,
24.829614908604));
#31328=CARTESIAN_POINT('Ctrl Pts',(-13.7236255579147,-36.6798326417964,
24.8238317748409));
#31329=CARTESIAN_POINT('Ctrl Pts',(-13.7724951073974,-36.5715052412387,
24.8180527975164));
#31330=CARTESIAN_POINT('Ctrl Pts',(-13.8166725773331,-36.460956923271,24.8122738201918));
#31331=CARTESIAN_POINT('Ctrl Pts',(-13.8559577878748,-36.3486343233536,
24.8064948428673));
#31332=CARTESIAN_POINT('Ctrl Pts',(-13.8952293775639,-36.236350667598,24.8007178692128));
#31333=CARTESIAN_POINT('Ctrl Pts',(-13.92961193999,-36.1222943399894,24.7949408955583));
#31334=CARTESIAN_POINT('Ctrl Pts',(-13.9589537101831,-36.006931239275,24.7891639219038));
#31335=CARTESIAN_POINT('Ctrl Pts',(-13.9882886312204,-35.8915950674005,
24.7833882967497));
#31336=CARTESIAN_POINT('Ctrl Pts',(-14.0125850024543,-35.7749531295744,
24.7776126715957));
#31337=CARTESIAN_POINT('Ctrl Pts',(-14.0317413883318,-35.6574848877446,
24.7718370464417));
#31338=CARTESIAN_POINT('Ctrl Pts',(-14.0509049499055,-35.5399726440644,
24.7660592578247));
#31339=CARTESIAN_POINT('Ctrl Pts',(-14.0649246106826,-35.4216338849925,
24.7602814692077));
#31340=CARTESIAN_POINT('Ctrl Pts',(-14.0737504068468,-35.3029564700018,
24.7545036805907));
#31341=CARTESIAN_POINT('Ctrl Pts',(-14.0813314046055,-35.2010174267331,
24.7495407965923));
#31342=CARTESIAN_POINT('Ctrl Pts',(-14.0850811474127,-35.0988287954618,
24.7445779125939));
#31343=CARTESIAN_POINT('Ctrl Pts',(-14.0849986678096,-34.9967009101602,
24.7396150285955));
#31344=CARTESIAN_POINT('Origin',(-10.,-35.,32.7603849714045));
#31345=CARTESIAN_POINT('',(-7.5128274573098,-31.7594448403263,26.796772721093));
#31346=CARTESIAN_POINT('',(-7.51282745730979,-31.7594448403263,26.6927653424671));
#31347=CARTESIAN_POINT('',(-7.5128274573098,-31.7594448403263,32.7603849714045));
#31348=CARTESIAN_POINT('',(-14.0849995364304,-34.9980538850391,25.8853849714457));
#31349=CARTESIAN_POINT('Ctrl Pts',(-7.51282745730979,-31.7594448403263,
26.6927653424671));
#31350=CARTESIAN_POINT('Ctrl Pts',(-7.41550409810477,-31.8341419137751,
26.6867866480316));
#31351=CARTESIAN_POINT('Ctrl Pts',(-7.32165094663543,-31.9131486832113,
26.680807953596));
#31352=CARTESIAN_POINT('Ctrl Pts',(-7.23165018155787,-31.9960918318412,
26.6748292591604));
#31353=CARTESIAN_POINT('Ctrl Pts',(-7.14164941648032,-32.079034980471,26.6688505647248));
#31354=CARTESIAN_POINT('Ctrl Pts',(-7.05550131791785,-32.165914133754,26.6628718702893));
#31355=CARTESIAN_POINT('Ctrl Pts',(-6.97354327202869,-32.2563191377791,
26.6568931758537));
#31356=CARTESIAN_POINT('Ctrl Pts',(-6.89371140426106,-32.3443788303763,
26.6510695823501));
#31357=CARTESIAN_POINT('Ctrl Pts',(-6.81759735210981,-32.4360676753925,
26.6452459888466));
#31358=CARTESIAN_POINT('Ctrl Pts',(-6.74554833174319,-32.5310388137963,
26.639422395343));
#31359=CARTESIAN_POINT('Ctrl Pts',(-6.67359021195502,-32.625890131953,26.6336061491707));
#31360=CARTESIAN_POINT('Ctrl Pts',(-6.60568716782213,-32.7240151844941,
26.6277899029984));
#31361=CARTESIAN_POINT('Ctrl Pts',(-6.5421484417945,-32.8250315861108,26.6219736568261));
#31362=CARTESIAN_POINT('Ctrl Pts',(-6.47867331841221,-32.9259468697044,
26.616163232751));
#31363=CARTESIAN_POINT('Ctrl Pts',(-6.41955403829092,-33.0297474009458,
26.610352808676));
#31364=CARTESIAN_POINT('Ctrl Pts',(-6.3650581573562,-33.1360196351363,26.6045423846009));
#31365=CARTESIAN_POINT('Ctrl Pts',(-6.3084994923243,-33.2463144976595,26.5985120237128));
#31366=CARTESIAN_POINT('Ctrl Pts',(-6.25692142388314,-33.3592715215538,
26.5924816628246));
#31367=CARTESIAN_POINT('Ctrl Pts',(-6.21057243011051,-33.4743972690896,
26.5864513019365));
#31368=CARTESIAN_POINT('Ctrl Pts',(-6.16596412375978,-33.5851993425957,
26.5806474178819));
#31369=CARTESIAN_POINT('Ctrl Pts',(-6.12619937404884,-33.6980097669418,
26.5748435338272));
#31370=CARTESIAN_POINT('Ctrl Pts',(-6.09145149069811,-33.8123664073318,
26.5690396497726));
#31371=CARTESIAN_POINT('Ctrl Pts',(-6.05670873999147,-33.9267061559898,
26.5632366230155));
#31372=CARTESIAN_POINT('Ctrl Pts',(-6.02698150062196,-34.0425912758967,
26.5574335962583));
#31373=CARTESIAN_POINT('Ctrl Pts',(-6.00239342359869,-34.1595437784673,
26.5516305695011));
#31374=CARTESIAN_POINT('Ctrl Pts',(-5.97780317571153,-34.2765066066915,
26.5458270303988));
#31375=CARTESIAN_POINT('Ctrl Pts',(-5.95835307631765,-34.3945366053273,
26.5400234912965));
#31376=CARTESIAN_POINT('Ctrl Pts',(-5.94411566812738,-34.513145518178,26.5342199521942));
#31377=CARTESIAN_POINT('Ctrl Pts',(-5.92987364291467,-34.6317928944909,
26.5284145310731));
#31378=CARTESIAN_POINT('Ctrl Pts',(-5.92084771939816,-34.7510191531632,
26.522609109952));
#31379=CARTESIAN_POINT('Ctrl Pts',(-5.91705852648728,-34.8703314846627,
26.5168036888309));
#31380=CARTESIAN_POINT('Ctrl Pts',(-5.91326513739649,-34.9897759435095,
26.510991838744));
#31381=CARTESIAN_POINT('Ctrl Pts',(-5.91472006756795,-35.1093062570726,
26.5051799886571));
#31382=CARTESIAN_POINT('Ctrl Pts',(-5.92139181534436,-35.2284300244276,
26.4993681385702));
#31383=CARTESIAN_POINT('Ctrl Pts',(-5.92806794515974,-35.3476320328986,
26.4935524712297));
#31384=CARTESIAN_POINT('Ctrl Pts',(-5.93996767580205,-35.4664265580115,
26.4877368038892));
#31385=CARTESIAN_POINT('Ctrl Pts',(-5.95700787211379,-35.5843283784398,
26.4819211365486));
#31386=CARTESIAN_POINT('Ctrl Pts',(-5.97407247666817,-35.7023990805048,
26.4760971388921));
#31387=CARTESIAN_POINT('Ctrl Pts',(-5.99629216755737,-35.8195741258997,
26.4702731412356));
#31388=CARTESIAN_POINT('Ctrl Pts',(-6.02353315362947,-35.9353803609848,
26.4644491435791));
#31389=CARTESIAN_POINT('Ctrl Pts',(-6.03076034401834,-35.966104421669,26.4629040034811));
#31390=CARTESIAN_POINT('Ctrl Pts',(-6.03834070087973,-35.9967322307021,
26.4613588633832));
#31391=CARTESIAN_POINT('Ctrl Pts',(-6.0462711511454,-36.0272551726494,26.4598137232852));
#31392=CARTESIAN_POINT('Ctrl Pts',(-6.07616081668759,-36.1422953652745,
26.4539901295173));
#31393=CARTESIAN_POINT('Ctrl Pts',(-6.11112377217277,-36.2562154530518,
26.4481665357494));
#31394=CARTESIAN_POINT('Ctrl Pts',(-6.15106024591779,-36.3685348988775,
26.4423429419815));
#31395=CARTESIAN_POINT('Ctrl Pts',(-6.19094633387794,-36.4807126370635,
26.4365266955409));
#31396=CARTESIAN_POINT('Ctrl Pts',(-6.23579332401346,-36.591293368582,26.4307104491003));
#31397=CARTESIAN_POINT('Ctrl Pts',(-6.28545091568015,-36.6998088422463,
26.4248942026596));
#31398=CARTESIAN_POINT('Ctrl Pts',(-6.33505879983332,-36.8082156913439,
26.4190837783127));
#31399=CARTESIAN_POINT('Ctrl Pts',(-6.38946753686421,-36.9145610261199,
26.4132733539657));
#31400=CARTESIAN_POINT('Ctrl Pts',(-6.44847791428129,-37.0183943803559,
26.4074629296187));
#31401=CARTESIAN_POINT('Ctrl Pts',(-6.50972195512672,-37.1261580393306,
26.4014325688311));
#31402=CARTESIAN_POINT('Ctrl Pts',(-6.57592273228872,-37.2312153708464,
26.3954022080435));
#31403=CARTESIAN_POINT('Ctrl Pts',(-6.64680375531957,-37.3330880704896,
26.3893718472559));
#31404=CARTESIAN_POINT('Ctrl Pts',(-6.71502276801676,-37.4311348352412,
26.3835679629221));
#31405=CARTESIAN_POINT('Ctrl Pts',(-6.78757656904055,-37.5262314933653,
26.3777640785882));
#31406=CARTESIAN_POINT('Ctrl Pts',(-6.86417364421405,-37.6179797681339,
26.3719601942544));
#31407=CARTESIAN_POINT('Ctrl Pts',(-6.94075940518792,-37.70971449071,26.3661571672157));
#31408=CARTESIAN_POINT('Ctrl Pts',(-7.02138699097805,-37.7981015001445,
26.3603541401771));
#31409=CARTESIAN_POINT('Ctrl Pts',(-7.1057244066607,-37.8827753623549,26.3545511131384));
#31410=CARTESIAN_POINT('Ctrl Pts',(-7.19006926846154,-37.9674567003882,
26.3487475737528));
#31411=CARTESIAN_POINT('Ctrl Pts',(-7.27812432320579,-38.0484239500613,
26.3429440343671));
#31412=CARTESIAN_POINT('Ctrl Pts',(-7.36952097272954,-38.1253487944692,
26.3371404949814));
#31413=CARTESIAN_POINT('Ctrl Pts',(-7.46094726112563,-38.2022985847111,
26.3313350735753));
#31414=CARTESIAN_POINT('Ctrl Pts',(-7.55571698716796,-38.2752030997859,
26.3255296521691));
#31415=CARTESIAN_POINT('Ctrl Pts',(-7.65342928716088,-38.3437749460222,
26.319724230763));
#31416=CARTESIAN_POINT('Ctrl Pts',(-7.75124979447971,-38.4124227292298,
26.3139123803902));
#31417=CARTESIAN_POINT('Ctrl Pts',(-7.85201904580789,-38.4767280316185,
26.3081005300173));
#31418=CARTESIAN_POINT('Ctrl Pts',(-7.95530794312085,-38.5364472840034,
26.3022886796444));
#31419=CARTESIAN_POINT('Ctrl Pts',(-8.05866468113677,-38.5962057603144,
26.296473012017));
#31420=CARTESIAN_POINT('Ctrl Pts',(-8.1645439996482,-38.6513719996173,26.2906573443896));
#31421=CARTESIAN_POINT('Ctrl Pts',(-8.27249450183565,-38.7017495530913,
26.2848416767622));
#31422=CARTESIAN_POINT('Ctrl Pts',(-8.38059963144689,-38.7521992669644,
26.2790176788196));
#31423=CARTESIAN_POINT('Ctrl Pts',(-8.49078149029422,-38.7978464485358,
26.273193680877));
#31424=CARTESIAN_POINT('Ctrl Pts',(-8.60257100685233,-38.8385436312631,
26.2673696829345));
#31425=CARTESIAN_POINT('Ctrl Pts',(-8.63222935586338,-38.8493408087289,
26.2658245455286));
#31426=CARTESIAN_POINT('Ctrl Pts',(-8.66200079536442,-38.8597898475114,
26.2642794081227));
#31427=CARTESIAN_POINT('Ctrl Pts',(-8.69187643515746,-38.8698885951799,
26.2627342707168));
#31428=CARTESIAN_POINT('Ctrl Pts',(-8.80447715652083,-38.9079505841522,
26.2569106770561));
#31429=CARTESIAN_POINT('Ctrl Pts',(-8.91892204726395,-38.941155419342,26.2510870833954));
#31430=CARTESIAN_POINT('Ctrl Pts',(-9.03475450883762,-38.9693231339601,
26.2452634897346));
#31431=CARTESIAN_POINT('Ctrl Pts',(-9.1504408305565,-38.9974553108224,26.2394472434023));
#31432=CARTESIAN_POINT('Ctrl Pts',(-9.26751084787404,-39.0205629115739,
26.2336309970699));
#31433=CARTESIAN_POINT('Ctrl Pts',(-9.38549053968945,-39.0385149650817,
26.2278147507376));
#31434=CARTESIAN_POINT('Ctrl Pts',(-9.50335213318378,-39.0564490484851,
26.2220043264999));
#31435=CARTESIAN_POINT('Ctrl Pts',(-9.62212118830161,-39.0692377902069,
26.2161939022621));
#31436=CARTESIAN_POINT('Ctrl Pts',(-9.74131174708171,-39.0768008766436,
26.2103834780244));
#31437=CARTESIAN_POINT('Ctrl Pts',(-9.8650139153479,-39.0846502415646,26.2043531171962));
#31438=CARTESIAN_POINT('Ctrl Pts',(-9.98916969180361,-39.0868704250354,
26.1983227563681));
#31439=CARTESIAN_POINT('Ctrl Pts',(-10.1132274744215,-39.0834304866174,
26.1922923955399));
#31440=CARTESIAN_POINT('Ctrl Pts',(-10.2326261352612,-39.0801197387399,
26.186488511317));
#31441=CARTESIAN_POINT('Ctrl Pts',(-10.3519335851697,-39.0715663581694,
26.1806846270941));
#31442=CARTESIAN_POINT('Ctrl Pts',(-10.4706569195449,-39.0577958381472,
26.1748807428712));
#31443=CARTESIAN_POINT('Ctrl Pts',(-10.5893627172164,-39.0440273521778,
26.1690777159439));
#31444=CARTESIAN_POINT('Ctrl Pts',(-10.7074841654304,-39.0250433063251,
26.1632746890167));
#31445=CARTESIAN_POINT('Ctrl Pts',(-10.8245336381544,-39.0009210539014,
26.1574716620894));
#31446=CARTESIAN_POINT('Ctrl Pts',(-10.9415934451254,-38.9767966717347,
26.1516681228155));
#31447=CARTESIAN_POINT('Ctrl Pts',(-11.0575806884786,-38.9475332634557,
26.1458645835415));
#31448=CARTESIAN_POINT('Ctrl Pts',(-11.1720187213541,-38.9132591425557,
26.1400610442675));
#31449=CARTESIAN_POINT('Ctrl Pts',(-11.2864938651518,-38.8789739069571,
26.1342556229733));
#31450=CARTESIAN_POINT('Ctrl Pts',(-11.3994184083611,-38.8396748442417,
26.1284502016791));
#31451=CARTESIAN_POINT('Ctrl Pts',(-11.510332244344,-38.7955396864866,26.1226447803849));
#31452=CARTESIAN_POINT('Ctrl Pts',(-11.6213689071394,-38.7513556531273,
26.1168329301237));
#31453=CARTESIAN_POINT('Ctrl Pts',(-11.7303900384525,-38.7023249856986,
26.1110210798625));
#31454=CARTESIAN_POINT('Ctrl Pts',(-11.8369567081506,-38.648673053643,26.1052092296012));
#31455=CARTESIAN_POINT('Ctrl Pts',(-11.943593371412,-38.5949858827091,26.0993935620854));
#31456=CARTESIAN_POINT('Ctrl Pts',(-12.0477720070184,-38.5366716013178,
26.0935778945696));
#31457=CARTESIAN_POINT('Ctrl Pts',(-12.1490808715626,-38.4740000586476,
26.0877622270538));
#31458=CARTESIAN_POINT('Ctrl Pts',(-12.2505348501211,-38.4112387457567,
26.0819382292219));
#31459=CARTESIAN_POINT('Ctrl Pts',(-12.3491105167004,-38.3441079433072,
26.0761142313901));
#31460=CARTESIAN_POINT('Ctrl Pts',(-12.4444274066281,-38.2729191333923,
26.0702902335582));
#31461=CARTESIAN_POINT('Ctrl Pts',(-12.4697154987112,-38.254032352867,26.0687450950883));
#31462=CARTESIAN_POINT('Ctrl Pts',(-12.4947744094188,-38.2348601493782,
26.0671999566183));
#31463=CARTESIAN_POINT('Ctrl Pts',(-12.5195974652232,-38.21540877856,26.0656548181484));
#31464=CARTESIAN_POINT('Ctrl Pts',(-12.6121091278228,-38.1429165492224,
26.0598963277381));
#31465=CARTESIAN_POINT('Ctrl Pts',(-12.7016553977147,-38.066298478211,26.0541378373279));
#31466=CARTESIAN_POINT('Ctrl Pts',(-12.7878402403067,-37.9858284938232,
26.0483793469177));
#31467=CARTESIAN_POINT('Ctrl Pts',(-12.8739158144014,-37.9054605324131,
26.0426281573457));
#31468=CARTESIAN_POINT('Ctrl Pts',(-12.9566381307634,-37.8212506493314,
26.0368769677737));
#31469=CARTESIAN_POINT('Ctrl Pts',(-13.0356421573583,-37.7335145312342,
26.0311257782017));
#31470=CARTESIAN_POINT('Ctrl Pts',(-13.1145677909286,-37.645865470721,26.0253802953407));
#31471=CARTESIAN_POINT('Ctrl Pts',(-13.1897821930235,-37.5546974420572,
26.0196348124797));
#31472=CARTESIAN_POINT('Ctrl Pts',(-13.2609558687923,-37.4603641644661,
26.0138893296186));
#31473=CARTESIAN_POINT('Ctrl Pts',(-13.3320794864131,-37.3660972337247,
26.0081478876931));
#31474=CARTESIAN_POINT('Ctrl Pts',(-13.3991677787653,-37.2686698146862,
26.0024064457676));
#31475=CARTESIAN_POINT('Ctrl Pts',(-13.4619308537099,-37.168469451971,25.996665003842));
#31476=CARTESIAN_POINT('Ctrl Pts',(-13.5246713353126,-37.068305159207,25.9909256287107));
#31477=CARTESIAN_POINT('Ctrl Pts',(-13.5830894723226,-36.9653702610003,
25.9851862535794));
#31478=CARTESIAN_POINT('Ctrl Pts',(-13.6369384953953,-36.8600815521669,
25.979446878448));
#31479=CARTESIAN_POINT('Ctrl Pts',(-13.6907815551996,-36.754804503059,25.973708138898));
#31480=CARTESIAN_POINT('Ctrl Pts',(-13.7400563170544,-36.6471745343663,
25.9679693993481));
#31481=CARTESIAN_POINT('Ctrl Pts',(-13.7845621812999,-36.5376326270843,
25.9622306597981));
#31482=CARTESIAN_POINT('Ctrl Pts',(-13.8290742097712,-36.4280755478458,
25.9564911254116));
#31483=CARTESIAN_POINT('Ctrl Pts',(-13.8688158713989,-36.3166063917855,
25.9507515910251));
#31484=CARTESIAN_POINT('Ctrl Pts',(-13.9036351727091,-36.2036849414976,
25.9450120566386));
#31485=CARTESIAN_POINT('Ctrl Pts',(-13.9384862376508,-36.0906604795121,
25.9392672864074));
#31486=CARTESIAN_POINT('Ctrl Pts',(-13.9684058548621,-35.9761814789232,
25.9335225161761));
#31487=CARTESIAN_POINT('Ctrl Pts',(-13.993292283104,-35.8607216400799,25.9277777459449));
#31488=CARTESIAN_POINT('Ctrl Pts',(-14.0181915929177,-35.74520203757,25.9220300021383));
#31489=CARTESIAN_POINT('Ctrl Pts',(-14.0380524566317,-35.6287009980468,
25.9162822583318));
#31490=CARTESIAN_POINT('Ctrl Pts',(-14.0528247789729,-35.5116994341827,
25.9105345145252));
#31491=CARTESIAN_POINT('Ctrl Pts',(-14.0676173085854,-35.3945378222046,
25.9047789082976));
#31492=CARTESIAN_POINT('Ctrl Pts',(-14.0773073680108,-35.2768747353253,
25.8990233020699));
#31493=CARTESIAN_POINT('Ctrl Pts',(-14.0818969247299,-35.1591932658148,
25.8932676958423));
#31494=CARTESIAN_POINT('Ctrl Pts',(-14.0839921694523,-35.1054688011184,
25.8906401210434));
#31495=CARTESIAN_POINT('Ctrl Pts',(-14.0850251129975,-35.0517404692523,
25.8880125462446));
#31496=CARTESIAN_POINT('Ctrl Pts',(-14.0849995364304,-34.9980538850391,
25.8853849714457));
#31497=CARTESIAN_POINT('Ctrl Pts',(-14.08499953643,-34.9980538841979,25.8853849714045));
#31498=CARTESIAN_POINT('Ctrl Pts',(-14.0849449953633,-34.883569313474,25.879781769463));
#31499=CARTESIAN_POINT('Ctrl Pts',(-14.080078085778,-34.7692049070056,25.8741785675215));
#31500=CARTESIAN_POINT('Ctrl Pts',(-14.0704266820107,-34.6552513576889,
25.8685753655799));
#31501=CARTESIAN_POINT('Ctrl Pts',(-14.0603956578551,-34.5368156530634,
25.8627517718956));
#31502=CARTESIAN_POINT('Ctrl Pts',(-14.0451750474139,-34.4186271289466,
25.8569281782113));
#31503=CARTESIAN_POINT('Ctrl Pts',(-14.0247820306556,-34.3011762699278,
25.851104584527));
#31504=CARTESIAN_POINT('Ctrl Pts',(-14.0044147427164,-34.18387359261,25.845288338171));
#31505=CARTESIAN_POINT('Ctrl Pts',(-13.9788880972798,-34.0673071280727,
25.839472091815));
#31506=CARTESIAN_POINT('Ctrl Pts',(-13.9482711523948,-33.9519637853742,
25.8336558454589));
#31507=CARTESIAN_POINT('Ctrl Pts',(-13.9176848552396,-33.8367359019949,
25.8278454211974));
#31508=CARTESIAN_POINT('Ctrl Pts',(-13.8820184994982,-33.7227290971593,
25.8220349969359));
#31509=CARTESIAN_POINT('Ctrl Pts',(-13.8413923561576,-33.6104210112218,
25.8162245726744));
#31510=CARTESIAN_POINT('Ctrl Pts',(-13.7992284293919,-33.4938618322967,
25.8101942118551));
#31511=CARTESIAN_POINT('Ctrl Pts',(-13.7517218964776,-33.3791329548536,
25.8041638510358));
#31512=CARTESIAN_POINT('Ctrl Pts',(-13.6990644946249,-33.2667525091306,
25.7981334902165));
#31513=CARTESIAN_POINT('Ctrl Pts',(-13.6483846971398,-33.1585926297946,
25.7923296059699));
#31514=CARTESIAN_POINT('Ctrl Pts',(-13.5929341350944,-33.0526083705815,
25.7865257217232));
#31515=CARTESIAN_POINT('Ctrl Pts',(-13.5329328695643,-32.9492415210093,
25.7807218374765));
#31516=CARTESIAN_POINT('Ctrl Pts',(-13.4729404668619,-32.8458899398248,
25.7749188105255));
#31517=CARTESIAN_POINT('Ctrl Pts',(-13.4083989023823,-32.7451553524743,
25.7691157835745));
#31518=CARTESIAN_POINT('Ctrl Pts',(-13.3395736832622,-32.6474540144638,
25.7633127566235));
#31519=CARTESIAN_POINT('Ctrl Pts',(-13.2707423875942,-32.5497440504456,
25.7575092173258));
#31520=CARTESIAN_POINT('Ctrl Pts',(-13.1976269205012,-32.4550682020675,
25.7517056780282));
#31521=CARTESIAN_POINT('Ctrl Pts',(-13.1205351353065,-32.3638123228196,
25.7459021387305));
#31522=CARTESIAN_POINT('Ctrl Pts',(-13.0434183501445,-32.2725268503538,
25.7400967174127));
#31523=CARTESIAN_POINT('Ctrl Pts',(-12.9623229457867,-32.184663864449,25.7342912960949));
#31524=CARTESIAN_POINT('Ctrl Pts',(-12.8775954891559,-32.100574332598,25.7284858747771));
#31525=CARTESIAN_POINT('Ctrl Pts',(-12.792774204709,-32.0163916793736,25.7226740244925));
#31526=CARTESIAN_POINT('Ctrl Pts',(-12.7043131294084,-31.9359911091633,
25.7168621742079));
#31527=CARTESIAN_POINT('Ctrl Pts',(-12.6125940604785,-31.8596851630525,
25.7110503239233));
#31528=CARTESIAN_POINT('Ctrl Pts',(-12.5208147499716,-31.7833290987866,
25.7052346563843));
#31529=CARTESIAN_POINT('Ctrl Pts',(-12.4257735085496,-31.7110732611334,
25.6994189888452));
#31530=CARTESIAN_POINT('Ctrl Pts',(-12.3278820701145,-31.6431875137805,
25.6936033213061));
#31531=CARTESIAN_POINT('Ctrl Pts',(-12.2298504127658,-31.5752045274259,
25.6877793234514));
#31532=CARTESIAN_POINT('Ctrl Pts',(-12.1289607539607,-31.5116043423405,
25.6819553255967));
#31533=CARTESIAN_POINT('Ctrl Pts',(-12.0256505210766,-31.4526115286789,
25.6761313277419));
#31534=CARTESIAN_POINT('Ctrl Pts',(-11.9982417555253,-31.4369604150019,
25.6745861894984));
#31535=CARTESIAN_POINT('Ctrl Pts',(-11.9706627263405,-31.4216333392667,
25.673041051255));
#31536=CARTESIAN_POINT('Ctrl Pts',(-11.9429218324976,-31.4066339244652,
25.6714959130115));
#31537=CARTESIAN_POINT('Ctrl Pts',(-11.8383669847753,-31.3501014443163,
25.6656723193424));
#31538=CARTESIAN_POINT('Ctrl Pts',(-11.7311741295239,-31.2980448797148,
25.6598487256734));
#31539=CARTESIAN_POINT('Ctrl Pts',(-11.6217629113311,-31.2507187276185,
25.6540251320044));
#31540=CARTESIAN_POINT('Ctrl Pts',(-11.5124897316419,-31.2034522844928,
25.6482088856638));
#31541=CARTESIAN_POINT('Ctrl Pts',(-11.4010041272226,-31.1609045441083,
25.6423926393232));
#31542=CARTESIAN_POINT('Ctrl Pts',(-11.287751189864,-31.1232846541171,25.6365763929826));
#31543=CARTESIAN_POINT('Ctrl Pts',(-11.1746116193209,-31.0857024218435,
25.6307659687367));
#31544=CARTESIAN_POINT('Ctrl Pts',(-11.0597086205532,-31.0530383547416,
25.6249555444908));
#31545=CARTESIAN_POINT('Ctrl Pts',(-10.943507606343,-31.0254536866741,25.6191451202449));
#31546=CARTESIAN_POINT('Ctrl Pts',(-10.8229081433312,-30.996824881849,25.6131147594198));
#31547=CARTESIAN_POINT('Ctrl Pts',(-10.7009108695577,-30.9736677832646,
25.6070843985947));
#31548=CARTESIAN_POINT('Ctrl Pts',(-10.5780542375612,-30.9561060475777,
25.6010540377696));
#31549=CARTESIAN_POINT('Ctrl Pts',(-10.4598116166339,-30.9392038614938,
25.5952501535388));
#31550=CARTESIAN_POINT('Ctrl Pts',(-10.3407734622321,-30.9274844009111,
25.589446269308));
#31551=CARTESIAN_POINT('Ctrl Pts',(-10.2214299038253,-30.9210057860188,
25.5836423850772));
#31552=CARTESIAN_POINT('Ctrl Pts',(-10.1021039737383,-30.9145281280872,
25.5778393581421));
#31553=CARTESIAN_POINT('Ctrl Pts',(-9.98247313698508,-30.9132897984763,
25.5720363312071));
#31554=CARTESIAN_POINT('Ctrl Pts',(-9.86303107899964,-30.9172969107857,
25.5662333042721));
#31555=CARTESIAN_POINT('Ctrl Pts',(-9.74357847552941,-30.9213043768812,
25.5604297649904));
#31556=CARTESIAN_POINT('Ctrl Pts',(-9.62431509209281,-30.9305581919947,
25.5546262257088));
#31557=CARTESIAN_POINT('Ctrl Pts',(-9.50573239939212,-30.9450123873199,
25.5488226864271));
#31558=CARTESIAN_POINT('Ctrl Pts',(-9.38711125170683,-30.959471269972,25.5430172651253));
#31559=CARTESIAN_POINT('Ctrl Pts',(-9.26917163888798,-30.9791338373683,
25.5372118438236));
#31560=CARTESIAN_POINT('Ctrl Pts',(-9.15239707538142,-31.0039026185317,
25.5314064225218));
#31561=CARTESIAN_POINT('Ctrl Pts',(-9.03549319485371,-31.0286988288278,
25.5255945722533));
#31562=CARTESIAN_POINT('Ctrl Pts',(-8.91975733864368,-31.0586124552982,
25.5197827219847));
#31563=CARTESIAN_POINT('Ctrl Pts',(-8.80566019442701,-31.0934954974013,
25.5139708717162));
#31564=CARTESIAN_POINT('Ctrl Pts',(-8.69148811059312,-31.1284014508739,
25.5081552041931));
#31565=CARTESIAN_POINT('Ctrl Pts',(-8.57895726625642,-31.1682831841049,
25.5023395366701));
#31566=CARTESIAN_POINT('Ctrl Pts',(-8.46851906514466,-31.2129442641843,
25.4965238691471));
#31567=CARTESIAN_POINT('Ctrl Pts',(-8.35792267323427,-31.2576693164387,
25.4906998713083));
#31568=CARTESIAN_POINT('Ctrl Pts',(-8.24942527752503,-31.307187210643,25.4848758734695));
#31569=CARTESIAN_POINT('Ctrl Pts',(-8.14345448376809,-31.3612551963405,
25.4790518756307));
#31570=CARTESIAN_POINT('Ctrl Pts',(-8.11533985412562,-31.3755997278808,
25.4775067372348));
#31571=CARTESIAN_POINT('Ctrl Pts',(-8.08740290818025,-31.3902642888718,
25.4759615988389));
#31572=CARTESIAN_POINT('Ctrl Pts',(-8.05965128011236,-31.4052438406437,
25.474416460443));
#31573=CARTESIAN_POINT('Ctrl Pts',(-7.95507361046443,-31.4616919384936,
25.4685938480784));
#31574=CARTESIAN_POINT('Ctrl Pts',(-7.852792633018,-31.5227983519528,25.4627712357138));
#31575=CARTESIAN_POINT('Ctrl Pts',(-7.75325101340967,-31.5883517192924,
25.4569486233492));
#31576=CARTESIAN_POINT('Ctrl Pts',(-7.67116836825394,-31.6424074380085,
25.4521472605978));
#31577=CARTESIAN_POINT('Ctrl Pts',(-7.59094821434825,-31.699486039335,25.4473458978464));
#31578=CARTESIAN_POINT('Ctrl Pts',(-7.5128274573098,-31.7594448403263,25.442544535095));
#31579=CARTESIAN_POINT('',(-14.0849990113761,-35.0028420162714,25.9896150286377));
#31580=CARTESIAN_POINT('Ctrl Pts',(-14.0849990113767,-35.0028420154021,
25.9896150285955));
#31581=CARTESIAN_POINT('Ctrl Pts',(-14.0850823687409,-34.8830274816084,
25.9837992556086));
#31582=CARTESIAN_POINT('Ctrl Pts',(-14.079890102243,-34.7631670279784,25.9779834826216));
#31583=CARTESIAN_POINT('Ctrl Pts',(-14.0694367788947,-34.6437566806534,
25.9721677096347));
#31584=CARTESIAN_POINT('Ctrl Pts',(-14.0589841763813,-34.5243545675665,
25.9663523376888));
#31585=CARTESIAN_POINT('Ctrl Pts',(-14.0432712736033,-34.4054029029652,
25.960536965743));
#31586=CARTESIAN_POINT('Ctrl Pts',(-14.0223646062431,-34.2873935346609,
25.9547215937972));
#31587=CARTESIAN_POINT('Ctrl Pts',(-14.0014545368584,-34.1693649633554,
25.9489052755486));
#31588=CARTESIAN_POINT('Ctrl Pts',(-13.9753490922789,-34.0522793926447,
25.9430889573));
#31589=CARTESIAN_POINT('Ctrl Pts',(-13.9441660016668,-33.9366188118573,
25.9372726390513));
#31590=CARTESIAN_POINT('Ctrl Pts',(-13.9129706122758,-33.8209126139139,
25.9314540268155));
#31591=CARTESIAN_POINT('Ctrl Pts',(-13.8766936982193,-33.7066329152009,
25.9256354145796));
#31592=CARTESIAN_POINT('Ctrl Pts',(-13.8355027712762,-33.5942462905856,
25.9198168023438));
#31593=CARTESIAN_POINT('Ctrl Pts',(-13.7942616422543,-33.4817226930344,
25.9139910985843));
#31594=CARTESIAN_POINT('Ctrl Pts',(-13.7480946838732,-33.3710971564586,
25.9081653948248));
#31595=CARTESIAN_POINT('Ctrl Pts',(-13.6972175587036,-33.2628162665931,
25.9023396910654));
#31596=CARTESIAN_POINT('Ctrl Pts',(-13.6463043684081,-33.1544586199548,
25.8965098576555));
#31597=CARTESIAN_POINT('Ctrl Pts',(-13.5906745492271,-33.0484492884319,
25.8906800242457));
#31598=CARTESIAN_POINT('Ctrl Pts',(-13.5305888844623,-32.9452087383602,
25.8848501908358));
#31599=CARTESIAN_POINT('Ctrl Pts',(-13.4704104788133,-32.8418088388009,
25.8790113592081));
#31600=CARTESIAN_POINT('Ctrl Pts',(-13.405762716197,-32.741186592108,25.8731725275803));
#31601=CARTESIAN_POINT('Ctrl Pts',(-13.3369488314327,-32.6437322952601,
25.8673336959526));
#31602=CARTESIAN_POINT('Ctrl Pts',(-13.3133690745061,-32.6103386184028,
25.865332962656));
#31603=CARTESIAN_POINT('Ctrl Pts',(-13.2893004869779,-32.5773166103989,
25.8633322293594));
#31604=CARTESIAN_POINT('Ctrl Pts',(-13.2647562933768,-32.5446810095516,
25.8613314960627));
#31605=CARTESIAN_POINT('Ctrl Pts',(-13.1933147821542,-32.4496875996201,
25.855507902402));
#31606=CARTESIAN_POINT('Ctrl Pts',(-13.1176086426052,-32.3576616547356,
25.8496843087413));
#31607=CARTESIAN_POINT('Ctrl Pts',(-13.0379131029185,-32.2690095241623,
25.8438607150805));
#31608=CARTESIAN_POINT('Ctrl Pts',(-12.9583181109923,-32.1804692414192,
25.8380444687481));
#31609=CARTESIAN_POINT('Ctrl Pts',(-12.8747440004701,-32.0952946077671,
25.8322282224158));
#31610=CARTESIAN_POINT('Ctrl Pts',(-12.7875080441697,-32.0138613723256,
25.8264119760834));
#31611=CARTESIAN_POINT('Ctrl Pts',(-12.7003594115419,-31.9325096520013,
25.8206015518457));
#31612=CARTESIAN_POINT('Ctrl Pts',(-12.6095565220285,-31.8548921563931,
25.8147911276079));
#31613=CARTESIAN_POINT('Ctrl Pts',(-12.5154551039248,-31.7813495654019,
25.8089807033701));
#31614=CARTESIAN_POINT('Ctrl Pts',(-12.4177917522681,-31.7050232350398,
25.802950342542));
#31615=CARTESIAN_POINT('Ctrl Pts',(-12.3165755254786,-31.633086725002,25.7969199817138));
#31616=CARTESIAN_POINT('Ctrl Pts',(-12.2122442084415,-31.5658770315818,
25.7908896208857));
#31617=CARTESIAN_POINT('Ctrl Pts',(-12.1118311648171,-31.5011914695758,
25.7850857366627));
#31618=CARTESIAN_POINT('Ctrl Pts',(-12.0085331665854,-31.4408843266798,
25.7792818524398));
#31619=CARTESIAN_POINT('Ctrl Pts',(-11.9027714187935,-31.3852128793216,
25.7734779682169));
#31620=CARTESIAN_POINT('Ctrl Pts',(-11.7970252931406,-31.3295496552303,
25.7676749412896));
#31621=CARTESIAN_POINT('Ctrl Pts',(-11.6888165028904,-31.2785209550916,
25.7618719143624));
#31622=CARTESIAN_POINT('Ctrl Pts',(-11.5785911791187,-31.2323382729857,
25.7560688874351));
#31623=CARTESIAN_POINT('Ctrl Pts',(-11.4683561236013,-31.1861515134309,
25.7502653481611));
#31624=CARTESIAN_POINT('Ctrl Pts',(-11.3561045572124,-31.1448117803874,
25.7444618088871));
#31625=CARTESIAN_POINT('Ctrl Pts',(-11.2423023240401,-31.108482309473,25.7386582696131));
#31626=CARTESIAN_POINT('Ctrl Pts',(-11.1284631861273,-31.0721410573337,
25.7328528483189));
#31627=CARTESIAN_POINT('Ctrl Pts',(-11.0130727701459,-31.0408134227405,
25.7270474270246));
#31628=CARTESIAN_POINT('Ctrl Pts',(-10.8966111730242,-31.0146125151489,
25.7212420057303));
#31629=CARTESIAN_POINT('Ctrl Pts',(-10.7800206054583,-30.988382592476,25.7154301554691));
#31630=CARTESIAN_POINT('Ctrl Pts',(-10.6623568875434,-30.9672908190116,
25.7096183052078));
#31631=CARTESIAN_POINT('Ctrl Pts',(-10.5441095368113,-30.9513990302882,
25.7038064549466));
#31632=CARTESIAN_POINT('Ctrl Pts',(-10.4257845205817,-30.9354968037523,
25.6979907874307));
#31633=CARTESIAN_POINT('Ctrl Pts',(-10.3068755138776,-30.9248014002655,
25.6921751199149));
#31634=CARTESIAN_POINT('Ctrl Pts',(-10.1878747114574,-30.9193225938829,
25.6863594523991));
#31635=CARTESIAN_POINT('Ctrl Pts',(-10.0687034532317,-30.9138359397015,
25.6805354545672));
#31636=CARTESIAN_POINT('Ctrl Pts',(-9.94944054373476,-30.9135807976243,
25.6747114567353));
#31637=CARTESIAN_POINT('Ctrl Pts',(-9.83057587023469,-30.9185149192661,
25.6688874589035));
#31638=CARTESIAN_POINT('Ctrl Pts',(-9.79904042241721,-30.9198239687169,
25.6673423204337));
#31639=CARTESIAN_POINT('Ctrl Pts',(-9.76753296246046,-30.9214979935786,
25.665797181964));
#31640=CARTESIAN_POINT('Ctrl Pts',(-9.73606253046786,-30.9235355990544,
25.6642520434943));
#31641=CARTESIAN_POINT('Ctrl Pts',(-9.61746471748103,-30.9312144117639,
25.6584291160139));
#31642=CARTESIAN_POINT('Ctrl Pts',(-9.49901105975285,-30.9440855036799,
25.6526061885334));
#31643=CARTESIAN_POINT('Ctrl Pts',(-9.38119211766201,-30.9621414332896,
25.646783261053));
#31644=CARTESIAN_POINT('Ctrl Pts',(-9.26351389261787,-30.9801757978009,
25.6409672881857));
#31645=CARTESIAN_POINT('Ctrl Pts',(-9.14646927572767,-31.0033826255236,
25.6351513153183));
#31646=CARTESIAN_POINT('Ctrl Pts',(-9.03054638179244,-31.0317025461611,
25.629335342451));
#31647=CARTESIAN_POINT('Ctrl Pts',(-8.91473456843547,-31.0599953298539,
25.6235249426125));
#31648=CARTESIAN_POINT('Ctrl Pts',(-8.80004273454173,-31.093391365418,25.617714542774));
#31649=CARTESIAN_POINT('Ctrl Pts',(-8.68695080781059,-31.1317798900669,
25.6119041429355));
#31650=CARTESIAN_POINT('Ctrl Pts',(-8.57394311493053,-31.1701398219297,
25.6060980708361));
#31651=CARTESIAN_POINT('Ctrl Pts',(-8.46253334325251,-31.2134847125031,
25.6002919987367));
#31652=CARTESIAN_POINT('Ctrl Pts',(-8.35318755702693,-31.2616536038418,
25.5944859266373));
#31653=CARTESIAN_POINT('Ctrl Pts',(-8.2438906130624,-31.3098009792388,25.5886824479775));
#31654=CARTESIAN_POINT('Ctrl Pts',(-8.13665619309796,-31.3627679035355,
25.5828789693176));
#31655=CARTESIAN_POINT('Ctrl Pts',(-8.03193110999552,-31.4203450104519,
25.5770754906578));
#31656=CARTESIAN_POINT('Ctrl Pts',(-7.92720867010922,-31.4779206641469,
25.5712721584753));
#31657=CARTESIAN_POINT('Ctrl Pts',(-7.82499580308749,-31.5401060801663,
25.5654688262928));
#31658=CARTESIAN_POINT('Ctrl Pts',(-7.72571506550866,-31.6066457543095,
25.5596654941103));
#31659=CARTESIAN_POINT('Ctrl Pts',(-7.65313415233258,-31.6552907425472,
25.5554228669951));
#31660=CARTESIAN_POINT('Ctrl Pts',(-7.5821198585115,-31.7062619290058,25.5511802398798));
#31661=CARTESIAN_POINT('Ctrl Pts',(-7.5128274573098,-31.7594448403263,25.5469376127646));
#31662=CARTESIAN_POINT('Ctrl Pts',(-7.5128274573098,-31.7594448403263,26.796772721093));
#31663=CARTESIAN_POINT('Ctrl Pts',(-7.41816755880118,-31.8320976695064,
26.7909660993717));
#31664=CARTESIAN_POINT('Ctrl Pts',(-7.32661924854595,-31.9089587491885,
26.7851594776504));
#31665=CARTESIAN_POINT('Ctrl Pts',(-7.23857278924136,-31.9897267965047,
26.7793528559291));
#31666=CARTESIAN_POINT('Ctrl Pts',(-7.15056342287312,-32.0704608171938,
26.7735486804691));
#31667=CARTESIAN_POINT('Ctrl Pts',(-7.0660532747713,-32.1550982576077,26.7677445050092));
#31668=CARTESIAN_POINT('Ctrl Pts',(-6.98539899898841,-32.243298020333,26.7619403295492));
#31669=CARTESIAN_POINT('Ctrl Pts',(-6.90475998799386,-32.3314810901961,
26.756137252599));
#31670=CARTESIAN_POINT('Ctrl Pts',(-6.8279756735518,-32.4232248404266,26.7503341756489));
#31671=CARTESIAN_POINT('Ctrl Pts',(-6.75536488494574,-32.5181523072201,
26.7445310986987));
#31672=CARTESIAN_POINT('Ctrl Pts',(-6.68275070259049,-32.6130842108201,
26.738727750519));
#31673=CARTESIAN_POINT('Ctrl Pts',(-6.61431068192869,-32.7111998024259,
26.7329244023393));
#31674=CARTESIAN_POINT('Ctrl Pts',(-6.55032209091048,-32.8120906500635,
26.7271210541596));
#31675=CARTESIAN_POINT('Ctrl Pts',(-6.48631540787171,-32.9130100234001,
26.7213160651516));
#31676=CARTESIAN_POINT('Ctrl Pts',(-6.42676287608266,-33.0167058685485,
26.7155110761436));
#31677=CARTESIAN_POINT('Ctrl Pts',(-6.37189698958961,-33.1227430794238,
26.7097060871355));
#31678=CARTESIAN_POINT('Ctrl Pts',(-6.31697141161673,-33.2288956537506,
26.703894782575));
#31679=CARTESIAN_POINT('Ctrl Pts',(-6.26674284636288,-33.3373943163327,
26.6980834780146));
#31680=CARTESIAN_POINT('Ctrl Pts',(-6.22139666957394,-33.4477816289925,
26.6922721734541));
#31681=CARTESIAN_POINT('Ctrl Pts',(-6.17602239898176,-33.5582373310881,
26.6864572685537));
#31682=CARTESIAN_POINT('Ctrl Pts',(-6.13553667971406,-33.6705836302412,
26.6806423636534));
#31683=CARTESIAN_POINT('Ctrl Pts',(-6.10007525591783,-33.7843470929185,
26.6748274587531));
#31684=CARTESIAN_POINT('Ctrl Pts',(-6.06456135891672,-33.8982788943946,
26.6690039493845));
#31685=CARTESIAN_POINT('Ctrl Pts',(-6.0340867052915,-34.0136316523845,26.6631804400158));
#31686=CARTESIAN_POINT('Ctrl Pts',(-6.00873617634326,-34.1299206415683,
26.6573569306472));
#31687=CARTESIAN_POINT('Ctrl Pts',(-5.99755206376073,-34.1812248628646,
26.6547877225436));
#31688=CARTESIAN_POINT('Ctrl Pts',(-5.98736462608227,-34.2327112275932,
26.6522185144401));
#31689=CARTESIAN_POINT('Ctrl Pts',(-5.97817793786512,-34.2843378586755,
26.6496493063365));
#31690=CARTESIAN_POINT('Ctrl Pts',(-5.95735457765622,-34.4013593478113,
26.6438257119652));
#31691=CARTESIAN_POINT('Ctrl Pts',(-5.94160927488649,-34.5194791313175,
26.6380021175938));
#31692=CARTESIAN_POINT('Ctrl Pts',(-5.93105180598832,-34.6382188583562,
26.6321785232225));
#31693=CARTESIAN_POINT('Ctrl Pts',(-5.92050765688948,-34.7568087777705,
26.6263622761718));
#31694=CARTESIAN_POINT('Ctrl Pts',(-5.9151383592276,-34.8760166818923,26.620546029121));
#31695=CARTESIAN_POINT('Ctrl Pts',(-5.91500264167212,-34.9953543079937,
26.6147297820702));
#31696=CARTESIAN_POINT('Ctrl Pts',(-5.91486705997048,-35.1145724766296,
26.6089193571072));
#31697=CARTESIAN_POINT('Ctrl Pts',(-5.91995463682205,-35.2339197029306,
26.6031089321442));
#31698=CARTESIAN_POINT('Ctrl Pts',(-5.9302722289381,-35.3529034846067,26.5972985071812));
#31699=CARTESIAN_POINT('Ctrl Pts',(-5.94098036146807,-35.4763910278991,
26.5912681466223));
#31700=CARTESIAN_POINT('Ctrl Pts',(-5.95732230389187,-35.5994866223381,
26.5852377860635));
#31701=CARTESIAN_POINT('Ctrl Pts',(-5.97924629213039,-35.7216402293753,
26.5792074255046));
#31702=CARTESIAN_POINT('Ctrl Pts',(-6.00034690533139,-35.8392062481651,
26.5734035405439));
#31703=CARTESIAN_POINT('Ctrl Pts',(-6.02661776934589,-35.9558993199064,
26.5675996555832));
#31704=CARTESIAN_POINT('Ctrl Pts',(-6.05796008286243,-36.0712358711759,
26.5617957706225));
#31705=CARTESIAN_POINT('Ctrl Pts',(-6.0892977668033,-36.1865553860741,26.5559927429542));
#31706=CARTESIAN_POINT('Ctrl Pts',(-6.12570530346265,-36.3005183850366,
26.5501897152858));
#31707=CARTESIAN_POINT('Ctrl Pts',(-6.1670334008828,-36.412654257082,26.5443866876175));
#31708=CARTESIAN_POINT('Ctrl Pts',(-6.20836514716021,-36.5248000296023,
26.5385831475999));
#31709=CARTESIAN_POINT('Ctrl Pts',(-6.25461817674669,-36.6351179713057,
26.5327796075822));
#31710=CARTESIAN_POINT('Ctrl Pts',(-6.30559444797943,-36.7431559359964,
26.5269760675646));
#31711=CARTESIAN_POINT('Ctrl Pts',(-6.35658725023713,-36.8512289361702,
26.521170645525));
#31712=CARTESIAN_POINT('Ctrl Pts',(-6.41230616617751,-36.957020119787,26.5153652234854));
#31713=CARTESIAN_POINT('Ctrl Pts',(-6.47250675904511,-37.060101073981,26.5095598014457));
#31714=CARTESIAN_POINT('Ctrl Pts',(-6.53277401847907,-37.1632961807596,
26.5037479504403));
#31715=CARTESIAN_POINT('Ctrl Pts',(-6.59753265544521,-37.2637747143913,
26.4979360994349));
#31716=CARTESIAN_POINT('Ctrl Pts',(-6.66649429157606,-37.3611363137068,
26.4921242484294));
#31717=CARTESIAN_POINT('Ctrl Pts',(-6.73550122207792,-37.4585618606409,
26.4863085801692));
#31718=CARTESIAN_POINT('Ctrl Pts',(-6.80871639961766,-37.5528660743705,
26.480492911909));
#31719=CARTESIAN_POINT('Ctrl Pts',(-6.88581152381396,-37.6436821168193,
26.4746772436487));
#31720=CARTESIAN_POINT('Ctrl Pts',(-6.96301707836893,-37.734628243346,26.4688532450779));
#31721=CARTESIAN_POINT('Ctrl Pts',(-7.04411339557444,-37.8220759276561,
26.463029246507));
#31722=CARTESIAN_POINT('Ctrl Pts',(-7.12873567890862,-37.905695475859,26.4572052479362));
#31723=CARTESIAN_POINT('Ctrl Pts',(-7.15118632765622,-37.9278800947463,
26.4556601165468));
#31724=CARTESIAN_POINT('Ctrl Pts',(-7.17388497955515,-37.9497954881707,
26.4541149851574));
#31725=CARTESIAN_POINT('Ctrl Pts',(-7.19682445279163,-37.9714359914918,
26.452569853768));
#31726=CARTESIAN_POINT('Ctrl Pts',(-7.28328323016378,-38.0529989567602,
26.4467462601123));
#31727=CARTESIAN_POINT('Ctrl Pts',(-7.37344419473058,-38.1309168275642,
26.4409226664566));
#31728=CARTESIAN_POINT('Ctrl Pts',(-7.46696744324481,-38.2048355755667,
26.4350990728009));
#31729=CARTESIAN_POINT('Ctrl Pts',(-7.56037269831285,-38.2786610641076,
26.4292828264721));
#31730=CARTESIAN_POINT('Ctrl Pts',(-7.65713148251871,-38.3484972142308,
26.4234665801434));
#31731=CARTESIAN_POINT('Ctrl Pts',(-7.75686762006312,-38.4140272591294,
26.4176503338146));
#31732=CARTESIAN_POINT('Ctrl Pts',(-7.85650392120851,-38.4794917081079,
26.4118399095791));
#31733=CARTESIAN_POINT('Ctrl Pts',(-7.95911130735749,-38.5406584040014,
26.4060294853436));
#31734=CARTESIAN_POINT('Ctrl Pts',(-8.0642816225373,-38.5972516402322,26.400219061108));
#31735=CARTESIAN_POINT('Ctrl Pts',(-8.1734328520136,-38.6559870476907,26.3941887002785));
#31736=CARTESIAN_POINT('Ctrl Pts',(-8.28534451683555,-38.7097956467526,
26.388158339449));
#31737=CARTESIAN_POINT('Ctrl Pts',(-8.39952820533579,-38.7584192201622,
26.3821279786195));
#31738=CARTESIAN_POINT('Ctrl Pts',(-8.50942360415092,-38.8052166836339,
26.3763240943952));
#31739=CARTESIAN_POINT('Ctrl Pts',(-8.6214230382177,-38.8472113819989,26.3705202101709));
#31740=CARTESIAN_POINT('Ctrl Pts',(-8.73506790151208,-38.8842208724807,
26.3647163259466));
#31741=CARTESIAN_POINT('Ctrl Pts',(-8.84869597827336,-38.9212248962743,
26.3589132990166));
#31742=CARTESIAN_POINT('Ctrl Pts',(-8.96396861275618,-38.953245050178,26.3531102720866));
#31743=CARTESIAN_POINT('Ctrl Pts',(-9.08041036321069,-38.9801482258717,
26.3473072451566));
#31744=CARTESIAN_POINT('Ctrl Pts',(-9.19686239428267,-39.0070537768411,
26.3415037058786));
#31745=CARTESIAN_POINT('Ctrl Pts',(-9.31448334867906,-39.028841359432,26.3357001666006));
#31746=CARTESIAN_POINT('Ctrl Pts',(-9.43278650524778,-39.0454287598932,
26.3298966273226));
#31747=CARTESIAN_POINT('Ctrl Pts',(-9.5511280261813,-39.0620215394592,26.3240912060229));
#31748=CARTESIAN_POINT('Ctrl Pts',(-9.67015178509111,-39.0734107264371,
26.3182857847233));
#31749=CARTESIAN_POINT('Ctrl Pts',(-9.78936547859593,-39.0795659203392,
26.3124803634237));
#31750=CARTESIAN_POINT('Ctrl Pts',(-9.9087111902775,-39.0857279305512,26.3066685131551));
#31751=CARTESIAN_POINT('Ctrl Pts',(-10.0282468483653,-39.0866443569785,
26.3008566628865));
#31752=CARTESIAN_POINT('Ctrl Pts',(-10.1474795239155,-39.0823369275484,
26.2950448126179));
#31753=CARTESIAN_POINT('Ctrl Pts',(-10.266790512154,-39.0780266689746,26.2892291450936));
#31754=CARTESIAN_POINT('Ctrl Pts',(-10.3857977154447,-39.0684857540623,
26.2834134775692));
#31755=CARTESIAN_POINT('Ctrl Pts',(-10.5040143587992,-39.0537876764977,
26.2775978100449));
#31756=CARTESIAN_POINT('Ctrl Pts',(-10.6224003347691,-39.0390685455192,
26.2717738122029));
#31757=CARTESIAN_POINT('Ctrl Pts',(-10.7399930894212,-39.0191775755394,
26.2659498143608));
#31758=CARTESIAN_POINT('Ctrl Pts',(-10.8563169082389,-38.9942391456527,
26.2601258165188));
#31759=CARTESIAN_POINT('Ctrl Pts',(-10.8871782527635,-38.9876228439833,
26.2585806780791));
#31760=CARTESIAN_POINT('Ctrl Pts',(-10.9179503703753,-38.9806515367974,
26.2570355396394));
#31761=CARTESIAN_POINT('Ctrl Pts',(-10.9486245864041,-38.9733281256485,
26.2554904011996));
#31762=CARTESIAN_POINT('Ctrl Pts',(-11.064235046025,-38.9457263467434,26.2496668076959));
#31763=CARTESIAN_POINT('Ctrl Pts',(-11.1788262582109,-38.9130300575665,
26.2438432141922));
#31764=CARTESIAN_POINT('Ctrl Pts',(-11.2919158013149,-38.8753294779041,
26.2380196206885));
#31765=CARTESIAN_POINT('Ctrl Pts',(-11.4048626651036,-38.8376764631426,
26.232203374516));
#31766=CARTESIAN_POINT('Ctrl Pts',(-11.5163112441204,-38.7950318436155,
26.2263871283435));
#31767=CARTESIAN_POINT('Ctrl Pts',(-11.6257903978905,-38.7475366018395,
26.2205708821711));
#31768=CARTESIAN_POINT('Ctrl Pts',(-11.7351599623722,-38.700088903085,26.2147604580959));
#31769=CARTESIAN_POINT('Ctrl Pts',(-11.8425636510252,-38.6478004030813,
26.2089500340206));
#31770=CARTESIAN_POINT('Ctrl Pts',(-11.9475471345948,-38.5908613393629,
26.2031396099454));
#31771=CARTESIAN_POINT('Ctrl Pts',(-12.056504464562,-38.5317670119255,26.1971092490573));
#31772=CARTESIAN_POINT('Ctrl Pts',(-12.1628543243545,-38.4676632389247,
26.1910788881692));
#31773=CARTESIAN_POINT('Ctrl Pts',(-12.2661130189758,-38.3988169684801,
26.1850485272811));
#31774=CARTESIAN_POINT('Ctrl Pts',(-12.3654937197915,-38.3325562954159,
26.1792446432263));
#31775=CARTESIAN_POINT('Ctrl Pts',(-12.4620108822091,-38.261903167245,26.1734407591716));
#31776=CARTESIAN_POINT('Ctrl Pts',(-12.5552605252404,-38.187141140293,26.1676368751168));
#31777=CARTESIAN_POINT('Ctrl Pts',(-12.6484963942748,-38.1123901565138,
26.1618338483594));
#31778=CARTESIAN_POINT('Ctrl Pts',(-12.7384653852574,-38.0335317362996,
26.1560308216021));
#31779=CARTESIAN_POINT('Ctrl Pts',(-12.8247955503814,-37.9508905602454,
26.1502277948447));
#31780=CARTESIAN_POINT('Ctrl Pts',(-12.9111333375348,-37.8682420878601,
26.1444242557423));
#31781=CARTESIAN_POINT('Ctrl Pts',(-12.9938313650825,-37.7818104779888,
26.1386207166398));
#31782=CARTESIAN_POINT('Ctrl Pts',(-13.0725540690073,-37.6919577435441,
26.1328171775373));
#31783=CARTESIAN_POINT('Ctrl Pts',(-13.1513023017699,-37.6020758709247,
26.127011756416));
#31784=CARTESIAN_POINT('Ctrl Pts',(-13.2260723781308,-37.5087709743006,
26.1212063352947));
#31785=CARTESIAN_POINT('Ctrl Pts',(-13.2965690092148,-37.4124381375456,
26.1154009141734));
#31786=CARTESIAN_POINT('Ctrl Pts',(-13.3671437087831,-37.3159986211034,
26.1095890640864));
#31787=CARTESIAN_POINT('Ctrl Pts',(-13.4334352754196,-37.2165248010505,
26.1037772139993));
#31788=CARTESIAN_POINT('Ctrl Pts',(-13.4951916760395,-37.114440859363,26.0979653639123));
#31789=CARTESIAN_POINT('Ctrl Pts',(-13.5569886385876,-37.0122898684067,
26.0921496965716));
#31790=CARTESIAN_POINT('Ctrl Pts',(-13.6142443075444,-36.9075256991544,
26.0863340292309));
#31791=CARTESIAN_POINT('Ctrl Pts',(-13.6667533185855,-36.8005957626969,
26.0805183618902));
#31792=CARTESIAN_POINT('Ctrl Pts',(-13.7193375431195,-36.6935126606428,
26.0746943642335));
#31793=CARTESIAN_POINT('Ctrl Pts',(-13.7671613759936,-36.5842579722473,
26.0688703665769));
#31794=CARTESIAN_POINT('Ctrl Pts',(-13.8100680749183,-36.4732977514706,
26.0630463689202));
#31795=CARTESIAN_POINT('Ctrl Pts',(-13.8214514690779,-36.4438593663049,
26.0615012288239));
#31796=CARTESIAN_POINT('Ctrl Pts',(-13.8324890351795,-36.4143010065942,
26.0599560887275));
#31797=CARTESIAN_POINT('Ctrl Pts',(-13.8431784448527,-36.3846315181374,
26.0584109486312));
#31798=CARTESIAN_POINT('Ctrl Pts',(-13.8896767283399,-36.2555710435782,
26.0516896829651));
#31799=CARTESIAN_POINT('Ctrl Pts',(-13.9297065577542,-36.1240650714574,
26.044968417299));
#31800=CARTESIAN_POINT('Ctrl Pts',(-13.963040544028,-35.9907243039264,26.0382471516329));
#31801=CARTESIAN_POINT('Ctrl Pts',(-13.9962417189144,-35.8579148011589,
26.0315526652608));
#31802=CARTESIAN_POINT('Ctrl Pts',(-14.0228002009898,-35.7232852282394,
26.0248581788888));
#31803=CARTESIAN_POINT('Ctrl Pts',(-14.0425382248911,-35.5874603818931,
26.0181636925167));
#31804=CARTESIAN_POINT('Ctrl Pts',(-14.0621325522581,-35.4526243660297,
26.0115179432672));
#31805=CARTESIAN_POINT('Ctrl Pts',(-14.0750052824874,-35.3166105657448,
26.0048721940178));
#31806=CARTESIAN_POINT('Ctrl Pts',(-14.0810301740175,-35.1800492120466,
25.9982264447683));
#31807=CARTESIAN_POINT('Ctrl Pts',(-14.0836324814554,-35.1210648096409,
25.9953559727248));
#31808=CARTESIAN_POINT('Ctrl Pts',(-14.084957868942,-35.0619784836735,25.9924855006812));
#31809=CARTESIAN_POINT('Ctrl Pts',(-14.0849990113761,-35.0028420162714,
25.9896150286377));
#31810=CARTESIAN_POINT('Origin',(-10.,-35.,32.7603849714045));
#31811=CARTESIAN_POINT('',(-7.5128274573098,-31.7594448403263,28.0469627561459));
#31812=CARTESIAN_POINT('',(-7.5128274573098,-31.7594448403263,27.9426390119128));
#31813=CARTESIAN_POINT('',(-7.5128274573098,-31.7594448403263,32.7603849714045));
#31814=CARTESIAN_POINT('',(-14.0849997205636,-34.9984890415501,27.1353849713726));
#31815=CARTESIAN_POINT('Ctrl Pts',(-7.5128274573098,-31.7594448403263,27.9426390119128));
#31816=CARTESIAN_POINT('Ctrl Pts',(-7.41802049582305,-31.8322105424504,
27.9368359551733));
#31817=CARTESIAN_POINT('Ctrl Pts',(-7.32640238267038,-31.9091456963177,
27.9310328984338));
#31818=CARTESIAN_POINT('Ctrl Pts',(-7.23834991095762,-31.98993126562,27.9252298416944));
#31819=CARTESIAN_POINT('Ctrl Pts',(-7.15028255297934,-32.0707304926358,
27.9194258038826));
#31820=CARTESIAN_POINT('Ctrl Pts',(-7.06578233601788,-32.1553811534852,
27.9136217660707));
#31821=CARTESIAN_POINT('Ctrl Pts',(-6.98519017205803,-32.243526401116,27.9078177282589));
#31822=CARTESIAN_POINT('Ctrl Pts',(-6.90451492792515,-32.3317625151792,
27.9020077072294));
#31823=CARTESIAN_POINT('Ctrl Pts',(-6.82775606013463,-32.4235001100291,
27.8961976861998));
#31824=CARTESIAN_POINT('Ctrl Pts',(-6.75521520865047,-32.5183479982425,
27.8903876651703));
#31825=CARTESIAN_POINT('Ctrl Pts',(-6.68263681144322,-32.6132449778641,
27.8845746369877));
#31826=CARTESIAN_POINT('Ctrl Pts',(-6.6142810139752,-32.7112551234008,27.8787616088051));
#31827=CARTESIAN_POINT('Ctrl Pts',(-6.55040599104204,-32.811958370286,27.8729485806225));
#31828=CARTESIAN_POINT('Ctrl Pts',(-6.48642767990506,-32.9128244579346,
27.8671261525648));
#31829=CARTESIAN_POINT('Ctrl Pts',(-6.42694482512305,-33.0163919944017,
27.8613037245071));
#31830=CARTESIAN_POINT('Ctrl Pts',(-6.37216980895975,-33.1222159056545,
27.8554812964494));
#31831=CARTESIAN_POINT('Ctrl Pts',(-6.32164664401443,-33.2198253505782,
27.8501108280544));
#31832=CARTESIAN_POINT('Ctrl Pts',(-6.2751283719363,-33.319353988852,27.8447403596593));
#31833=CARTESIAN_POINT('Ctrl Pts',(-6.23274456499622,-33.4204394638272,
27.8393698912643));
#31834=CARTESIAN_POINT('Ctrl Pts',(-6.18678478500024,-33.5300536425917,
27.8335463099551));
#31835=CARTESIAN_POINT('Ctrl Pts',(-6.14553895250771,-33.641852162612,27.8277227286458));
#31836=CARTESIAN_POINT('Ctrl Pts',(-6.10921899689708,-33.7553923566467,
27.8218991473366));
#31837=CARTESIAN_POINT('Ctrl Pts',(-6.07294486555298,-33.8687892989613,
27.8160829135402));
#31838=CARTESIAN_POINT('Ctrl Pts',(-6.04158437312784,-33.9839231591374,
27.8102666797439));
#31839=CARTESIAN_POINT('Ctrl Pts',(-6.01530181397272,-34.1003304127231,
27.8044504459475));
#31840=CARTESIAN_POINT('Ctrl Pts',(-5.98904556462065,-34.2166211383903,
27.798640034414));
#31841=CARTESIAN_POINT('Ctrl Pts',(-5.96785722556352,-34.3341823255599,
27.7928296228804));
#31842=CARTESIAN_POINT('Ctrl Pts',(-5.95185140895948,-34.4525349464517,
27.7870192113468));
#31843=CARTESIAN_POINT('Ctrl Pts',(-5.93523968978527,-34.5753678234253,
27.7809888458197));
#31844=CARTESIAN_POINT('Ctrl Pts',(-5.9242107531769,-34.6990528109013,27.7749584802926));
#31845=CARTESIAN_POINT('Ctrl Pts',(-5.91883462375985,-34.8230418925887,
27.7689281147654));
#31846=CARTESIAN_POINT('Ctrl Pts',(-5.91366041625262,-34.9423740714693,
27.7631242435858));
#31847=CARTESIAN_POINT('Ctrl Pts',(-5.9137220661502,-35.0619874689632,27.7573203724061));
#31848=CARTESIAN_POINT('Ctrl Pts',(-5.91902913880518,-35.1813886161775,
27.7515165012264));
#31849=CARTESIAN_POINT('Ctrl Pts',(-5.92433542745309,-35.3007721244129,
27.7457134874453));
#31850=CARTESIAN_POINT('Ctrl Pts',(-5.93488557970118,-35.4199430368987,
27.7399104736641));
#31851=CARTESIAN_POINT('Ctrl Pts',(-5.95063705693842,-35.5384094681185,
27.7341074598829));
#31852=CARTESIAN_POINT('Ctrl Pts',(-5.96638992462875,-35.6568863568982,
27.7283039338438));
#31853=CARTESIAN_POINT('Ctrl Pts',(-5.98734497637511,-35.7746582359709,
27.7225004078047));
#31854=CARTESIAN_POINT('Ctrl Pts',(-6.0134080625052,-35.8912405533309,27.7166968817657));
#31855=CARTESIAN_POINT('Ctrl Pts',(-6.0394796002739,-36.007860675562,27.7108914737812));
#31856=CARTESIAN_POINT('Ctrl Pts',(-6.07066237761633,-36.1232900706205,
27.7050860657967));
#31857=CARTESIAN_POINT('Ctrl Pts',(-6.10681177669693,-36.2370571765017,
27.6992806578123));
#31858=CARTESIAN_POINT('Ctrl Pts',(-6.14300120770635,-36.3509502683411,
27.6934688209055));
#31859=CARTESIAN_POINT('Ctrl Pts',(-6.18416811529114,-36.4631770071668,
27.6876569839987));
#31860=CARTESIAN_POINT('Ctrl Pts',(-6.23011886103203,-36.5732835720408,
27.6818451470919));
#31861=CARTESIAN_POINT('Ctrl Pts',(-6.27609978720983,-36.6834624548757,
27.6760294929722));
#31862=CARTESIAN_POINT('Ctrl Pts',(-6.32687063571257,-36.7915180217742,
27.6702138388526));
#31863=CARTESIAN_POINT('Ctrl Pts',(-6.38219147051755,-36.8970204121211,
27.6643981847329));
#31864=CARTESIAN_POINT('Ctrl Pts',(-6.43759154701612,-37.0026739243394,
27.6585742002567));
#31865=CARTESIAN_POINT('Ctrl Pts',(-6.49755441363915,-37.1057666087602,
27.6527502157804));
#31866=CARTESIAN_POINT('Ctrl Pts',(-6.5617963858949,-37.2058968488927,27.6469262313042));
#31867=CARTESIAN_POINT('Ctrl Pts',(-6.5788415583959,-37.2324641717144,27.6453809671014));
#31868=CARTESIAN_POINT('Ctrl Pts',(-6.59618775340684,-37.2588231209837,
27.6438357028987));
#31869=CARTESIAN_POINT('Ctrl Pts',(-6.61382920342114,-37.2849665941533,
27.6422904386959));
#31870=CARTESIAN_POINT('Ctrl Pts',(-6.68031409498706,-37.3834928478019,
27.6364668401324));
#31871=CARTESIAN_POINT('Ctrl Pts',(-6.75120994305795,-37.4792738392738,
27.630643241569));
#31872=CARTESIAN_POINT('Ctrl Pts',(-6.82626268160111,-37.5718896620583,
27.6248196430055));
#31873=CARTESIAN_POINT('Ctrl Pts',(-6.90122073068663,-37.6643886371141,
27.6190033917208));
#31874=CARTESIAN_POINT('Ctrl Pts',(-6.98032498424699,-37.753730071613,27.6131871404361));
#31875=CARTESIAN_POINT('Ctrl Pts',(-7.06327782028086,-37.8395224667443,
27.6073708891513));
#31876=CARTESIAN_POINT('Ctrl Pts',(-7.14614762075709,-37.9252289839273,
27.6015604599179));
#31877=CARTESIAN_POINT('Ctrl Pts',(-7.23285805758641,-38.0073932372909,
27.5957500306845));
#31878=CARTESIAN_POINT('Ctrl Pts',(-7.32307130845913,-38.0856567826648,
27.5899396014511));
#31879=CARTESIAN_POINT('Ctrl Pts',(-7.41669920838254,-38.1668826704699,
27.5839092424793));
#31880=CARTESIAN_POINT('Ctrl Pts',(-7.51410004835411,-38.2439063774664,
27.5778788835075));
#31881=CARTESIAN_POINT('Ctrl Pts',(-7.61485386994085,-38.316368938804,27.5718485245357));
#31882=CARTESIAN_POINT('Ctrl Pts',(-7.71182388933896,-38.3861101741029,
27.5660446352413));
#31883=CARTESIAN_POINT('Ctrl Pts',(-7.81189922859877,-38.4516264129335,
27.5602407459469));
#31884=CARTESIAN_POINT('Ctrl Pts',(-7.91467240495817,-38.5126391533087,
27.5544368566526));
#31885=CARTESIAN_POINT('Ctrl Pts',(-8.01743040097529,-38.5736428816603,
27.5486338246347));
#31886=CARTESIAN_POINT('Ctrl Pts',(-8.12288509059288,-38.630144226035,27.5428307926168));
#31887=CARTESIAN_POINT('Ctrl Pts',(-8.23060175399589,-38.6819091307415,
27.5370277605988));
#31888=CARTESIAN_POINT('Ctrl Pts',(-8.33832792790142,-38.7336786058667,
27.5312242162206));
#31889=CARTESIAN_POINT('Ctrl Pts',(-8.44831610461033,-38.7807106329853,
27.5254206718423));
#31890=CARTESIAN_POINT('Ctrl Pts',(-8.56010940666761,-38.8228183424318,
27.519617127464));
#31891=CARTESIAN_POINT('Ctrl Pts',(-8.67193896211582,-38.8649397069652,
27.5138117010574));
#31892=CARTESIAN_POINT('Ctrl Pts',(-8.7855744251755,-38.9021334340867,27.5080062746507));
#31893=CARTESIAN_POINT('Ctrl Pts',(-8.90054211814158,-38.9342619849242,
27.5022008482441));
#31894=CARTESIAN_POINT('Ctrl Pts',(-9.01563712681007,-38.9664261150528,
27.4963889928841));
#31895=CARTESIAN_POINT('Ctrl Pts',(-9.13206691674238,-38.9935137624922,
27.490577137524));
#31896=CARTESIAN_POINT('Ctrl Pts',(-9.24934577711996,-39.0154381127932,
27.484765282164));
#31897=CARTESIAN_POINT('Ctrl Pts',(-9.36670166677805,-39.0373768631057,
27.4789496095514));
#31898=CARTESIAN_POINT('Ctrl Pts',(-9.48490733414273,-39.0541455052459,
27.4731339369387));
#31899=CARTESIAN_POINT('Ctrl Pts',(-9.6034717294852,-39.0657090809209,27.4673182643261));
#31900=CARTESIAN_POINT('Ctrl Pts',(-9.72220595452643,-39.0772892200724,
27.4614942614392));
#31901=CARTESIAN_POINT('Ctrl Pts',(-9.84129952682653,-39.0836493899837,
27.4556702585523));
#31902=CARTESIAN_POINT('Ctrl Pts',(-9.96026103792287,-39.084806704716,27.4498462556654));
#31903=CARTESIAN_POINT('Ctrl Pts',(-9.99182115669804,-39.0851137367138,
27.4483011658194));
#31904=CARTESIAN_POINT('Ctrl Pts',(-10.0233720090006,-39.0850548621266,
27.4467560759735));
#31905=CARTESIAN_POINT('Ctrl Pts',(-10.0549044960451,-39.0846310110356,
27.4452109861275));
#31906=CARTESIAN_POINT('Ctrl Pts',(-10.1737535104524,-39.0830334749978,
27.4393873920321));
#31907=CARTESIAN_POINT('Ctrl Pts',(-10.2927243949168,-39.0762418979449,
27.4335637979367));
#31908=CARTESIAN_POINT('Ctrl Pts',(-10.4113266827035,-39.0642385953701,
27.4277402038413));
#31909=CARTESIAN_POINT('Ctrl Pts',(-10.5297793364882,-39.0522504367039,
27.4219239570552));
#31910=CARTESIAN_POINT('Ctrl Pts',(-10.647863915865,-39.035063671483,27.4161077102691));
#31911=CARTESIAN_POINT('Ctrl Pts',(-10.7650898376149,-39.0127126162209,
27.410291463483));
#31912=CARTESIAN_POINT('Ctrl Pts',(-10.8821984159523,-38.9903839344157,
27.4044810387731));
#31913=CARTESIAN_POINT('Ctrl Pts',(-10.9984496477625,-38.9629013226206,
27.3986706140632));
#31914=CARTESIAN_POINT('Ctrl Pts',(-11.1133585593696,-38.9303508390827,
27.3928601893533));
#31915=CARTESIAN_POINT('Ctrl Pts',(-11.2326169981954,-38.896568256031,27.3868298286952));
#31916=CARTESIAN_POINT('Ctrl Pts',(-11.3504290441579,-38.8573266081899,
27.3807994680371));
#31917=CARTESIAN_POINT('Ctrl Pts',(-11.4662642624002,-38.8127803651414,
27.374769107379));
#31918=CARTESIAN_POINT('Ctrl Pts',(-11.5777491790476,-38.7699070985428,
27.3689652226406));
#31919=CARTESIAN_POINT('Ctrl Pts',(-11.6874026581689,-38.7221206494065,
27.3631613379023));
#31920=CARTESIAN_POINT('Ctrl Pts',(-11.7947684020336,-38.6696091594422,
27.3573574531639));
#31921=CARTESIAN_POINT('Ctrl Pts',(-11.9021182871135,-38.6171054258477,
27.351554425706));
#31922=CARTESIAN_POINT('Ctrl Pts',(-12.0071807422314,-38.5598782187373,
27.3457513982482));
#31923=CARTESIAN_POINT('Ctrl Pts',(-12.1095217128741,-38.4981628239567,
27.3399483707903));
#31924=CARTESIAN_POINT('Ctrl Pts',(-12.2118717194142,-38.4364419801953,
27.3341448309711));
#31925=CARTESIAN_POINT('Ctrl Pts',(-12.3114994140395,-38.3702323717587,
27.3283412911518));
#31926=CARTESIAN_POINT('Ctrl Pts',(-12.4079980612437,-38.2998136821715,
27.3225377513326));
#31927=CARTESIAN_POINT('Ctrl Pts',(-12.5045280020695,-38.2293721564526,
27.3167323294789));
#31928=CARTESIAN_POINT('Ctrl Pts',(-12.5979265477428,-38.1547190755532,
27.3109269076252));
#31929=CARTESIAN_POINT('Ctrl Pts',(-12.6878190123209,-38.0761752155893,
27.3051214857715));
#31930=CARTESIAN_POINT('Ctrl Pts',(-12.7778110247604,-37.9975443753284,
27.2993096349326));
#31931=CARTESIAN_POINT('Ctrl Pts',(-12.8642888982836,-37.9150144243233,
27.2934977840937));
#31932=CARTESIAN_POINT('Ctrl Pts',(-12.9469137752778,-37.82894400812,27.2876859332547));
#31933=CARTESIAN_POINT('Ctrl Pts',(-13.0295929208927,-37.7428170602407,
27.2818702651498));
#31934=CARTESIAN_POINT('Ctrl Pts',(-13.1084137611082,-37.6531453220559,
27.2760545970449));
#31935=CARTESIAN_POINT('Ctrl Pts',(-13.1830778827183,-37.5603203300661,
27.27023892894));
#31936=CARTESIAN_POINT('Ctrl Pts',(-13.2578489527708,-37.4673623761114,
27.2644149305068));
#31937=CARTESIAN_POINT('Ctrl Pts',(-13.3284511793682,-37.3712424811903,
27.2585909320737));
#31938=CARTESIAN_POINT('Ctrl Pts',(-13.394629504484,-37.2723810259916,27.2527669336405));
#31939=CARTESIAN_POINT('Ctrl Pts',(-13.4121869161231,-37.2461526308014,
27.25122180028));
#31940=CARTESIAN_POINT('Ctrl Pts',(-13.4294331970442,-37.2197313982307,
27.2496766669195));
#31941=CARTESIAN_POINT('Ctrl Pts',(-13.446364137165,-37.1931254487746,27.248131533559));
#31942=CARTESIAN_POINT('Ctrl Pts',(-13.5116281814714,-37.0905669463098,
27.2421754761057));
#31943=CARTESIAN_POINT('Ctrl Pts',(-13.5724057739584,-36.9849433669533,
27.2362194186525));
#31944=CARTESIAN_POINT('Ctrl Pts',(-13.6284046856138,-36.8766737695763,
27.2302633611992));
#31945=CARTESIAN_POINT('Ctrl Pts',(-13.6843233506168,-36.7685593229424,
27.2243158387988));
#31946=CARTESIAN_POINT('Ctrl Pts',(-13.7354767897766,-36.6578067427523,
27.2183683163984));
#31947=CARTESIAN_POINT('Ctrl Pts',(-13.7816163114275,-36.5448634480579,
27.212420793998));
#31948=CARTESIAN_POINT('Ctrl Pts',(-13.8276986056336,-36.4320602383912,
27.2064806483865));
#31949=CARTESIAN_POINT('Ctrl Pts',(-13.8687792179631,-36.3170720760405,
27.200540502775));
#31950=CARTESIAN_POINT('Ctrl Pts',(-13.9046557782775,-36.2003700484284,
27.1946003571635));
#31951=CARTESIAN_POINT('Ctrl Pts',(-13.9404859563607,-36.0838188964964,
27.1886678911401));
#31952=CARTESIAN_POINT('Ctrl Pts',(-13.9711253765799,-35.9655586593393,
27.1827354251167));
#31953=CARTESIAN_POINT('Ctrl Pts',(-13.9964203633776,-35.8460787665346,
27.1768029590934));
#31954=CARTESIAN_POINT('Ctrl Pts',(-14.0216960800848,-35.7266898952583,
27.1708750125093));
#31955=CARTESIAN_POINT('Ctrl Pts',(-14.0416353885848,-35.6060835916905,
27.1649470659253));
#31956=CARTESIAN_POINT('Ctrl Pts',(-14.0561348461714,-35.4847629417297,
27.1590191193412));
#31957=CARTESIAN_POINT('Ctrl Pts',(-14.0706246910155,-35.3635227240301,
27.153095102823));
#31958=CARTESIAN_POINT('Ctrl Pts',(-14.0796818242725,-35.2415694834072,
27.1471710863049));
#31959=CARTESIAN_POINT('Ctrl Pts',(-14.0832542386772,-35.1194144979658,
27.1412470697867));
#31960=CARTESIAN_POINT('Ctrl Pts',(-14.0844325971236,-35.0791217596222,
27.1392930369926));
#31961=CARTESIAN_POINT('Ctrl Pts',(-14.0850146333961,-35.0388071211363,
27.1373390041986));
#31962=CARTESIAN_POINT('Ctrl Pts',(-14.0849997205638,-34.9984890422085,
27.1353849714045));
#31963=CARTESIAN_POINT('Ctrl Pts',(-14.0849997205636,-34.9984890415501,
27.1353849713726));
#31964=CARTESIAN_POINT('Ctrl Pts',(-14.0849517284631,-34.868738473512,27.1290965550657));
#31965=CARTESIAN_POINT('Ctrl Pts',(-14.0787177200191,-34.7391739922796,
27.1228081387587));
#31966=CARTESIAN_POINT('Ctrl Pts',(-14.0663757191564,-34.6103674671502,
27.1165197224518));
#31967=CARTESIAN_POINT('Ctrl Pts',(-14.0539812320581,-34.481013172683,27.1102045636981));
#31968=CARTESIAN_POINT('Ctrl Pts',(-14.0354267799426,-34.3524235763946,
27.1038894049444));
#31969=CARTESIAN_POINT('Ctrl Pts',(-14.0108419948859,-34.2251635707713,
27.0975742461907));
#31970=CARTESIAN_POINT('Ctrl Pts',(-13.9862032613468,-34.0976243077068,
27.0912452295477));
#31971=CARTESIAN_POINT('Ctrl Pts',(-13.9555078254915,-33.9714207437558,
27.0849162129047));
#31972=CARTESIAN_POINT('Ctrl Pts',(-13.9189352633586,-33.8471030394676,
27.0785871962617));
#31973=CARTESIAN_POINT('Ctrl Pts',(-13.8822472544181,-33.7223929075987,
27.0722382011232));
#31974=CARTESIAN_POINT('Ctrl Pts',(-13.8396450934937,-33.5995808195232,
27.0658892059847));
#31975=CARTESIAN_POINT('Ctrl Pts',(-13.7913574442726,-33.4791996417153,
27.0595402108463));
#31976=CARTESIAN_POINT('Ctrl Pts',(-13.7698384569852,-33.4255527759707,
27.0567108342277));
#31977=CARTESIAN_POINT('Ctrl Pts',(-13.7471909664105,-33.3723883587508,
27.0538814576091));
#31978=CARTESIAN_POINT('Ctrl Pts',(-13.7234381112611,-33.3197519136723,
27.0510520809905));
#31979=CARTESIAN_POINT('Ctrl Pts',(-13.6745485457436,-33.2114123934716,
27.0452284866185));
#31980=CARTESIAN_POINT('Ctrl Pts',(-13.6208477443864,-33.1050337219617,
27.0394048922465));
#31981=CARTESIAN_POINT('Ctrl Pts',(-13.5625152041965,-33.0010726826948,
27.0335812978744));
#31982=CARTESIAN_POINT('Ctrl Pts',(-13.5042562590829,-32.8972428055648,
27.0277650508229));
#31983=CARTESIAN_POINT('Ctrl Pts',(-13.4413773960105,-32.7958248468748,
27.0219488037714));
#31984=CARTESIAN_POINT('Ctrl Pts',(-13.3741058400978,-32.6972549468476,
27.01613255672));
#31985=CARTESIAN_POINT('Ctrl Pts',(-13.306901623295,-32.5987837157041,27.0103221317562));
#31986=CARTESIAN_POINT('Ctrl Pts',(-13.2353136900053,-32.5031552070109,
27.0045117067924));
#31987=CARTESIAN_POINT('Ctrl Pts',(-13.1596144708337,-32.4107797707228,
26.9987012818287));
#31988=CARTESIAN_POINT('Ctrl Pts',(-13.0810498927768,-32.3149077491324,
26.9926709212701));
#31989=CARTESIAN_POINT('Ctrl Pts',(-12.9980568586636,-32.2225403266311,
26.9866405607115));
#31990=CARTESIAN_POINT('Ctrl Pts',(-12.9109886684102,-32.1341022397184,
26.9806102001529));
#31991=CARTESIAN_POINT('Ctrl Pts',(-12.827190402101,-32.048985524447,26.9748063151914));
#31992=CARTESIAN_POINT('Ctrl Pts',(-12.7396178642165,-31.967508644902,26.96900243023));
#31993=CARTESIAN_POINT('Ctrl Pts',(-12.6486256467501,-31.8900149223223,
26.9631985452686));
#31994=CARTESIAN_POINT('Ctrl Pts',(-12.5576468697513,-31.8125326463466,
26.9573955175994));
#31995=CARTESIAN_POINT('Ctrl Pts',(-12.4632497284872,-31.7390326219744,
26.9515924899303));
#31996=CARTESIAN_POINT('Ctrl Pts',(-12.3658231673449,-31.6698189627508,
26.9457894622612));
#31997=CARTESIAN_POINT('Ctrl Pts',(-12.2683880044126,-31.600599192654,26.9399859222428));
#31998=CARTESIAN_POINT('Ctrl Pts',(-12.1679232227137,-31.5356667766415,
26.9341823822244));
#31999=CARTESIAN_POINT('Ctrl Pts',(-12.0648475752946,-31.4752830623155,
26.9283788422061));
#32000=CARTESIAN_POINT('Ctrl Pts',(-11.9617385016158,-31.414879766238,26.9225734201657));
#32001=CARTESIAN_POINT('Ctrl Pts',(-11.8560172305229,-31.3590283117683,
26.9167679981253));
#32002=CARTESIAN_POINT('Ctrl Pts',(-11.748127405517,-31.3079442617858,26.910962576085));
#32003=CARTESIAN_POINT('Ctrl Pts',(-11.6401181025483,-31.2568036409615,
26.9051507250788));
#32004=CARTESIAN_POINT('Ctrl Pts',(-11.5299358213997,-31.2104411377206,
26.8993388740726));
#32005=CARTESIAN_POINT('Ctrl Pts',(-11.4180446327388,-31.169024351479,26.8935270230664));
#32006=CARTESIAN_POINT('Ctrl Pts',(-11.3060799533475,-31.127580362471,26.8877113548054));
#32007=CARTESIAN_POINT('Ctrl Pts',(-11.1924045190183,-31.0910886842026,
26.8818956865444));
#32008=CARTESIAN_POINT('Ctrl Pts',(-11.0774964206742,-31.0596667065546,
26.8760800182834));
#32009=CARTESIAN_POINT('Ctrl Pts',(-10.9624237290091,-31.02819972035,26.8702560197118));
#32010=CARTESIAN_POINT('Ctrl Pts',(-10.8461152459811,-31.0018170189197,
26.8644320211401));
#32011=CARTESIAN_POINT('Ctrl Pts',(-10.7290582106451,-30.98058472841,26.8586080225685));
#32012=CARTESIAN_POINT('Ctrl Pts',(-10.698002485515,-30.9749517121965,26.8570628911864));
#32013=CARTESIAN_POINT('Ctrl Pts',(-10.6668940924327,-30.9696809307097,
26.8555177598042));
#32014=CARTESIAN_POINT('Ctrl Pts',(-10.6357421573044,-30.9647730039779,
26.8539726284221));
#32015=CARTESIAN_POINT('Ctrl Pts',(-10.5183157488948,-30.9462727019427,
26.8481482959054));
#32016=CARTESIAN_POINT('Ctrl Pts',(-10.3998917399521,-30.9328725381076,
26.8423239633887));
#32017=CARTESIAN_POINT('Ctrl Pts',(-10.2809507483721,-30.9246728135045,
26.836499630872));
#32018=CARTESIAN_POINT('Ctrl Pts',(-10.1586484735487,-30.9162413639382,
26.8305107021885));
#32019=CARTESIAN_POINT('Ctrl Pts',(-10.0357999672896,-30.913308807926,26.8245217735049));
#32020=CARTESIAN_POINT('Ctrl Pts',(-9.91293956784619,-30.9159278310547,
26.8185328448214));
#32021=CARTESIAN_POINT('Ctrl Pts',(-9.79375532453327,-30.9184684893241,
26.8127231133161));
#32022=CARTESIAN_POINT('Ctrl Pts',(-9.67456033602679,-30.9262332574045,
26.8069133818107));
#32023=CARTESIAN_POINT('Ctrl Pts',(-9.5558470133928,-30.9392176708807,26.8011036503054));
#32024=CARTESIAN_POINT('Ctrl Pts',(-9.43721248743642,-30.9521934658747,
26.7952977750441));
#32025=CARTESIAN_POINT('Ctrl Pts',(-9.31905939593694,-30.9703819717122,
26.7894918997828));
#32026=CARTESIAN_POINT('Ctrl Pts',(-9.20187755966171,-30.993726722972,26.7836860245215));
#32027=CARTESIAN_POINT('Ctrl Pts',(-9.08474584711726,-31.0170614886739,
26.7778826326838));
#32028=CARTESIAN_POINT('Ctrl Pts',(-8.96858496299047,-31.0455480321735,
26.772079240846));
#32029=CARTESIAN_POINT('Ctrl Pts',(-8.85387639939024,-31.0790784639163,
26.7662758490082));
#32030=CARTESIAN_POINT('Ctrl Pts',(-8.73918983038655,-31.1126024664239,
26.7604735699318));
#32031=CARTESIAN_POINT('Ctrl Pts',(-8.6259554189508,-31.1511683167176,26.7546712908555));
#32032=CARTESIAN_POINT('Ctrl Pts',(-8.51464069226473,-31.1946179262886,
26.7488690117791));
#32033=CARTESIAN_POINT('Ctrl Pts',(-8.40328786556716,-31.2380824074823,
26.74306474674));
#32034=CARTESIAN_POINT('Ctrl Pts',(-8.29385641732616,-31.2864338402305,
26.7372604817009));
#32035=CARTESIAN_POINT('Ctrl Pts',(-8.18679484698842,-31.3394656027989,
26.7314562166618));
#32036=CARTESIAN_POINT('Ctrl Pts',(-8.07971027020371,-31.3925087613559,
26.7256507043449));
#32037=CARTESIAN_POINT('Ctrl Pts',(-7.97499694650878,-31.4502340620241,
26.719845192028));
#32038=CARTESIAN_POINT('Ctrl Pts',(-7.87307862470323,-31.5123890034429,
26.7140396797111));
#32039=CARTESIAN_POINT('Ctrl Pts',(-7.77108031664891,-31.5745927245171,
26.7082296111855));
#32040=CARTESIAN_POINT('Ctrl Pts',(-7.67188173069061,-31.6412328026179,
26.7024195426598));
#32041=CARTESIAN_POINT('Ctrl Pts',(-7.57587736468658,-31.7120136178869,
26.6966094741342));
#32042=CARTESIAN_POINT('Ctrl Pts',(-7.55470415351006,-31.7276239199108,
26.6953280969118));
#32043=CARTESIAN_POINT('Ctrl Pts',(-7.5336861810716,-31.7434354708017,26.6940467196895));
#32044=CARTESIAN_POINT('Ctrl Pts',(-7.51282745730979,-31.7594448403263,
26.6927653424671));
#32045=CARTESIAN_POINT('',(-14.0849999969885,-35.0001568555874,27.2396150285597));
#32046=CARTESIAN_POINT('Ctrl Pts',(-14.0849999969885,-35.0001568555874,
27.2396150285597));
#32047=CARTESIAN_POINT('Ctrl Pts',(-14.0850045558159,-34.8814310263966,
27.2337980380925));
#32048=CARTESIAN_POINT('Ctrl Pts',(-14.0798288721944,-34.7625114247042,
27.2279810476253));
#32049=CARTESIAN_POINT('Ctrl Pts',(-14.0694482081679,-34.6438872635826,
27.222164057158));
#32050=CARTESIAN_POINT('Ctrl Pts',(-14.0590806442284,-34.525412802598,27.2163544075585));
#32051=CARTESIAN_POINT('Ctrl Pts',(-14.0435211992775,-34.4072334448657,
27.2105447579589));
#32052=CARTESIAN_POINT('Ctrl Pts',(-14.0227971296609,-34.2898392762253,
27.2047351083594));
#32053=CARTESIAN_POINT('Ctrl Pts',(-14.0020937767413,-34.1725624599908,
27.1989312663427));
#32054=CARTESIAN_POINT('Ctrl Pts',(-13.9762361401773,-34.056069672273,27.1931274243259));
#32055=CARTESIAN_POINT('Ctrl Pts',(-13.9453032933436,-33.9408461284912,
27.1873235823092));
#32056=CARTESIAN_POINT('Ctrl Pts',(-13.9134326019726,-33.8221291535458,
27.181343775191));
#32057=CARTESIAN_POINT('Ctrl Pts',(-13.8761740797712,-33.7047600549076,
27.1753639680729));
#32058=CARTESIAN_POINT('Ctrl Pts',(-13.8336711624622,-33.5892589117398,
27.1693841609547));
#32059=CARTESIAN_POINT('Ctrl Pts',(-13.7924649395073,-33.4772815191688,
27.1635867879521));
#32060=CARTESIAN_POINT('Ctrl Pts',(-13.7463298222171,-33.3670601722282,
27.1577894149496));
#32061=CARTESIAN_POINT('Ctrl Pts',(-13.6954469887969,-33.2590529723762,
27.151992041947));
#32062=CARTESIAN_POINT('Ctrl Pts',(-13.6445714584235,-33.1510612744448,
27.1461955010224));
#32063=CARTESIAN_POINT('Ctrl Pts',(-13.5889497414525,-33.0452834618998,
27.1403989600978));
#32064=CARTESIAN_POINT('Ctrl Pts',(-13.5288104726773,-32.9421560681327,
27.1346024191732));
#32065=CARTESIAN_POINT('Ctrl Pts',(-13.4686655518633,-32.8390189821953,
27.1288053334753));
#32066=CARTESIAN_POINT('Ctrl Pts',(-13.4040024414123,-32.7385331639236,
27.1230082477773));
#32067=CARTESIAN_POINT('Ctrl Pts',(-13.3350945511629,-32.6411084520895,
27.1172111620793));
#32068=CARTESIAN_POINT('Ctrl Pts',(-13.2661638185421,-32.5436514448037,
27.1114121546974));
#32069=CARTESIAN_POINT('Ctrl Pts',(-13.1929857441635,-32.4492578959464,
27.1056131473155));
#32070=CARTESIAN_POINT('Ctrl Pts',(-13.1158752651503,-32.3583061623222,
27.0998141399336));
#32071=CARTESIAN_POINT('Ctrl Pts',(-13.0386792579379,-32.2672535482718,
27.0940087004991));
#32072=CARTESIAN_POINT('Ctrl Pts',(-12.9575424053558,-32.1796506814067,
27.0882032610646));
#32073=CARTESIAN_POINT('Ctrl Pts',(-12.8728179817518,-32.0958405960204,
27.0823978216301));
#32074=CARTESIAN_POINT('Ctrl Pts',(-12.788037129969,-32.0119746914229,27.0765885156556));
#32075=CARTESIAN_POINT('Ctrl Pts',(-12.6996642516753,-31.9319068727521,
27.0707792096811));
#32076=CARTESIAN_POINT('Ctrl Pts',(-12.6080860379959,-31.8559401693971,
27.0649699037065));
#32077=CARTESIAN_POINT('Ctrl Pts',(-12.5163779129181,-31.7798657008841,
27.0591523567429));
#32078=CARTESIAN_POINT('Ctrl Pts',(-12.4214557029949,-31.7079042043729,
27.0533348097792));
#32079=CARTESIAN_POINT('Ctrl Pts',(-12.3237354633827,-31.6403157148003,
27.0475172628155));
#32080=CARTESIAN_POINT('Ctrl Pts',(-12.3029678679135,-31.6259517466461,
27.0462809123682));
#32081=CARTESIAN_POINT('Ctrl Pts',(-12.2820739874267,-31.6117851206942,
27.0450445619208));
#32082=CARTESIAN_POINT('Ctrl Pts',(-12.2610579524706,-31.5978180625414,
27.0438082114734));
#32083=CARTESIAN_POINT('Ctrl Pts',(-12.162065909123,-31.5320288863724,27.0379846173779));
#32084=CARTESIAN_POINT('Ctrl Pts',(-12.0600404855395,-31.4704577095777,
27.0321610232824));
#32085=CARTESIAN_POINT('Ctrl Pts',(-11.9553764945523,-31.4133960680677,
27.0263374291869));
#32086=CARTESIAN_POINT('Ctrl Pts',(-11.8508445523827,-31.3564064181015,
27.0205211824007));
#32087=CARTESIAN_POINT('Ctrl Pts',(-11.7436810193416,-31.3039151810071,
27.0147049356145));
#32088=CARTESIAN_POINT('Ctrl Pts',(-11.6343101665915,-31.2561710403151,
27.0088886888283));
#32089=CARTESIAN_POINT('Ctrl Pts',(-11.5250487943121,-31.2084746916157,
27.0030782641183));
#32090=CARTESIAN_POINT('Ctrl Pts',(-11.4135848699965,-31.1655161485198,
26.9972678394083));
#32091=CARTESIAN_POINT('Ctrl Pts',(-11.3003672508535,-31.1274982229949,
26.9914574146983));
#32092=CARTESIAN_POINT('Ctrl Pts',(-11.1828641232246,-31.0880412445762,
26.9854270540403));
#32093=CARTESIAN_POINT('Ctrl Pts',(-11.0634723095887,-31.0539065124743,
26.9793966933822));
#32094=CARTESIAN_POINT('Ctrl Pts',(-10.942716815981,-31.0252660460269,26.9733663327241));
#32095=CARTESIAN_POINT('Ctrl Pts',(-10.8264964095787,-30.9977011994877,
26.9675624479857));
#32096=CARTESIAN_POINT('Ctrl Pts',(-10.7090133376739,-30.9752254787958,
26.9617585632473));
#32097=CARTESIAN_POINT('Ctrl Pts',(-10.5907504313402,-30.9579412513088,
26.9559546785088));
#32098=CARTESIAN_POINT('Ctrl Pts',(-10.4725049933901,-30.9406595768414,
26.9501516510509));
#32099=CARTESIAN_POINT('Ctrl Pts',(-10.3534803540188,-30.9285679296409,
26.944348623593));
#32100=CARTESIAN_POINT('Ctrl Pts',(-10.2341676060109,-30.9217172079054,
26.9385455961351));
#32101=CARTESIAN_POINT('Ctrl Pts',(-10.1148443236319,-30.9148658813053,
26.9327420563158));
#32102=CARTESIAN_POINT('Ctrl Pts',(-9.9952332897256,-30.9132564236021,26.9269385164965));
#32103=CARTESIAN_POINT('Ctrl Pts',(-9.87582811879394,-30.9168876645483,
26.9211349766772));
#32104=CARTESIAN_POINT('Ctrl Pts',(-9.75638422586779,-30.9205200830724,
26.9153295548235));
#32105=CARTESIAN_POINT('Ctrl Pts',(-9.63714673662399,-30.9293965677822,
26.9095241329698));
#32106=CARTESIAN_POINT('Ctrl Pts',(-9.5186060167919,-30.9434639366904,26.9037187111162));
#32107=CARTESIAN_POINT('Ctrl Pts',(-9.39993402371848,-30.9575468839512,
26.8979068602772));
#32108=CARTESIAN_POINT('Ctrl Pts',(-9.28196074598802,-30.9768321416398,
26.8920950094382));
#32109=CARTESIAN_POINT('Ctrl Pts',(-9.16516836187053,-31.0012150425438,
26.8862831585993));
#32110=CARTESIAN_POINT('Ctrl Pts',(-9.04829926766458,-31.0256139583146,
26.8804674904943));
#32111=CARTESIAN_POINT('Ctrl Pts',(-8.93261300650044,-31.0551170845889,
26.8746518223894));
#32112=CARTESIAN_POINT('Ctrl Pts',(-8.81857694830981,-31.0895697713762,
26.8688361542845));
#32113=CARTESIAN_POINT('Ctrl Pts',(-8.70437754555023,-31.1240718079863,
26.8630121558513));
#32114=CARTESIAN_POINT('Ctrl Pts',(-8.59183344762659,-31.163537421163,26.8571881574181));
#32115=CARTESIAN_POINT('Ctrl Pts',(-8.48139252878395,-31.2077636745099,
26.8513641589849));
#32116=CARTESIAN_POINT('Ctrl Pts',(-8.45209204905866,-31.219497101333,26.8498190256249));
#32117=CARTESIAN_POINT('Ctrl Pts',(-8.42293947080304,-31.2315653620464,
26.8482738922649));
#32118=CARTESIAN_POINT('Ctrl Pts',(-8.39394285394541,-31.2439641317465,
26.8467287589049));
#32119=CARTESIAN_POINT('Ctrl Pts',(-8.28465587810226,-31.2906945503794,
26.84090521911));
#32120=CARTESIAN_POINT('Ctrl Pts',(-8.17723389000758,-31.3422740639199,
26.8350816793151));
#32121=CARTESIAN_POINT('Ctrl Pts',(-8.07213713139233,-31.3985322769954,
26.8292581395202));
#32122=CARTESIAN_POINT('Ctrl Pts',(-7.96718840949689,-31.45471124613,26.8234428026208));
#32123=CARTESIAN_POINT('Ctrl Pts',(-7.86455875598442,-31.5155556089732,
26.8176274657214));
#32124=CARTESIAN_POINT('Ctrl Pts',(-7.76468852804543,-31.5808469435622,
26.811812128822));
#32125=CARTESIAN_POINT('Ctrl Pts',(-7.67859497325255,-31.6371316162613,
26.8067989929123));
#32126=CARTESIAN_POINT('Ctrl Pts',(-7.59455190212405,-31.6967201573034,
26.8017858570026));
#32127=CARTESIAN_POINT('Ctrl Pts',(-7.5128274573098,-31.7594448403263,26.796772721093));
#32128=CARTESIAN_POINT('Ctrl Pts',(-7.5128274573098,-31.7594448403263,28.0469627561459));
#32129=CARTESIAN_POINT('Ctrl Pts',(-7.41670716853337,-31.8332185399736,
28.0410436622024));
#32130=CARTESIAN_POINT('Ctrl Pts',(-7.32400111322147,-31.9111734129659,
28.035124568259));
#32131=CARTESIAN_POINT('Ctrl Pts',(-7.23507124736889,-31.9929426355864,
28.0292054743155));
#32132=CARTESIAN_POINT('Ctrl Pts',(-7.14757771632443,-32.0733911772461,
28.0233819815583));
#32133=CARTESIAN_POINT('Ctrl Pts',(-7.0634570630503,-32.157791240188,28.017558488801));
#32134=CARTESIAN_POINT('Ctrl Pts',(-6.9830865523076,-32.2458289361166,28.0117349960438));
#32135=CARTESIAN_POINT('Ctrl Pts',(-6.90281746241604,-32.3337555358487,
28.0059188520465));
#32136=CARTESIAN_POINT('Ctrl Pts',(-6.82628937539092,-32.4253103394787,
28.0001027080492));
#32137=CARTESIAN_POINT('Ctrl Pts',(-6.75384496521342,-32.5201406309773,
27.994286564052));
#32138=CARTESIAN_POINT('Ctrl Pts',(-6.68147308973758,-32.6148759739921,
27.9884762434477));
#32139=CARTESIAN_POINT('Ctrl Pts',(-6.6131770034937,-32.7128799579496,27.9826659228433));
#32140=CARTESIAN_POINT('Ctrl Pts',(-6.54926069551753,-32.8137650509381,
27.9768556022391));
#32141=CARTESIAN_POINT('Ctrl Pts',(-6.48292341778096,-32.9184713871606,
27.9708252030519));
#32142=CARTESIAN_POINT('Ctrl Pts',(-6.42130456768723,-33.0262810731424,
27.9647948038647));
#32143=CARTESIAN_POINT('Ctrl Pts',(-6.36469640883172,-33.1367252483761,
27.9587644046776));
#32144=CARTESIAN_POINT('Ctrl Pts',(-6.31021557311453,-33.2430189538857,
27.9529606266698));
#32145=CARTESIAN_POINT('Ctrl Pts',(-6.26037582611707,-33.3517523185486,
27.9471568486621));
#32146=CARTESIAN_POINT('Ctrl Pts',(-6.2153917105462,-33.4624808634044,27.9413530706543));
#32147=CARTESIAN_POINT('Ctrl Pts',(-6.17041424570425,-33.5731930374697,
27.9355501507129));
#32148=CARTESIAN_POINT('Ctrl Pts',(-6.13029113829591,-33.6858994268841,
27.9297472307714));
#32149=CARTESIAN_POINT('Ctrl Pts',(-6.0951889167183,-33.8001352560057,27.92394431083));
#32150=CARTESIAN_POINT('Ctrl Pts',(-6.06008359989467,-33.9143811582219,
27.9181408791983));
#32151=CARTESIAN_POINT('Ctrl Pts',(-6.03000016910789,-34.0301563779248,
27.9123374475666));
#32152=CARTESIAN_POINT('Ctrl Pts',(-6.00505518761999,-34.1469812745092,
27.9065340159349));
#32153=CARTESIAN_POINT('Ctrl Pts',(-5.98010211894736,-34.2638440458268,
27.9007287028256));
#32154=CARTESIAN_POINT('Ctrl Pts',(-5.96029089787606,-34.3817567716713,
27.8949233897163));
#32155=CARTESIAN_POINT('Ctrl Pts',(-5.94568680155446,-34.5002305642496,
27.8891180766071));
#32156=CARTESIAN_POINT('Ctrl Pts',(-5.93106653291073,-34.618835552644,27.8833063347951));
#32157=CARTESIAN_POINT('Ctrl Pts',(-5.92166494899037,-34.7380024424444,
27.8774945929831));
#32158=CARTESIAN_POINT('Ctrl Pts',(-5.91749537449755,-34.8572380206389,
27.8716828511711));
#32159=CARTESIAN_POINT('Ctrl Pts',(-5.91332306155652,-34.9765519090919,
27.8658672923859));
#32160=CARTESIAN_POINT('Ctrl Pts',(-5.91438959772116,-35.0959341683828,
27.8600517336007));
#32161=CARTESIAN_POINT('Ctrl Pts',(-5.92065623563793,-35.2148940486851,
27.8542361748155));
#32162=CARTESIAN_POINT('Ctrl Pts',(-5.92693185045036,-35.3340243378172,
27.848412285301));
#32163=CARTESIAN_POINT('Ctrl Pts',(-5.93842239579202,-35.4527306352959,
27.8425883957865));
#32164=CARTESIAN_POINT('Ctrl Pts',(-5.9550375820364,-35.5705296112053,27.836764506272));
#32165=CARTESIAN_POINT('Ctrl Pts',(-5.9594486824461,-35.6018035977411,27.8352183447637));
#32166=CARTESIAN_POINT('Ctrl Pts',(-5.96422070613784,-35.6330137040189,
27.8336721832554));
#32167=CARTESIAN_POINT('Ctrl Pts',(-5.96935137004129,-35.6641510534599,
27.8321260217472));
#32168=CARTESIAN_POINT('Ctrl Pts',(-5.98867604478963,-35.7814300570737,
27.8263023956399));
#32169=CARTESIAN_POINT('Ctrl Pts',(-6.01315479434023,-35.8980540344452,
27.8204787695327));
#32170=CARTESIAN_POINT('Ctrl Pts',(-6.04273187030218,-36.0135353716955,
27.8146551434255));
#32171=CARTESIAN_POINT('Ctrl Pts',(-6.07227163203181,-36.1288710184978,
27.8088388643642));
#32172=CARTESIAN_POINT('Ctrl Pts',(-6.10689682662744,-36.243066500305,27.803022585303));
#32173=CARTESIAN_POINT('Ctrl Pts',(-6.14650027023396,-36.3556418526636,
27.7972063062418));
#32174=CARTESIAN_POINT('Ctrl Pts',(-6.18606407243592,-36.4681045217632,
27.7913958490347));
#32175=CARTESIAN_POINT('Ctrl Pts',(-6.23059607581365,-36.5789499045739,
27.7855853918275));
#32176=CARTESIAN_POINT('Ctrl Pts',(-6.27993877240317,-36.6877113091198,
27.7797749346204));
#32177=CARTESIAN_POINT('Ctrl Pts',(-6.33114879748764,-36.8005886879414,
27.7737445860604));
#32178=CARTESIAN_POINT('Ctrl Pts',(-6.38754070981686,-36.9112208059573,
27.7677142375003));
#32179=CARTESIAN_POINT('Ctrl Pts',(-6.44888257438587,-37.0191062452233,
27.7616838889402));
#32180=CARTESIAN_POINT('Ctrl Pts',(-6.507921139498,-37.1229407402376,27.755879971361));
#32181=CARTESIAN_POINT('Ctrl Pts',(-6.57154441183006,-37.2242307183596,
27.7500760537818));
#32182=CARTESIAN_POINT('Ctrl Pts',(-6.63949822635043,-37.3225530842799,
27.7442721362026));
#32183=CARTESIAN_POINT('Ctrl Pts',(-6.70744200441555,-37.4208609284544,
27.7384690758345));
#32184=CARTESIAN_POINT('Ctrl Pts',(-6.77971482060832,-37.5162016962512,
27.7326660154663));
#32185=CARTESIAN_POINT('Ctrl Pts',(-6.8560192153665,-37.6081813253406,27.7268629550981));
#32186=CARTESIAN_POINT('Ctrl Pts',(-6.93233034760052,-37.7001690759875,
27.7210593823351));
#32187=CARTESIAN_POINT('Ctrl Pts',(-7.01267350544634,-37.7887947835733,
27.7152558095721));
#32188=CARTESIAN_POINT('Ctrl Pts',(-7.09671140830339,-37.8736980275117,
27.7094522368091));
#32189=CARTESIAN_POINT('Ctrl Pts',(-7.18077656368583,-37.9586288045955,
27.7036467820141));
#32190=CARTESIAN_POINT('Ctrl Pts',(-7.268538559853,-38.0398344272183,27.6978413272192));
#32191=CARTESIAN_POINT('Ctrl Pts',(-7.35962426946815,-38.1169923005388,
27.6920358724243));
#32192=CARTESIAN_POINT('Ctrl Pts',(-7.45081084511643,-38.1942356165555,
27.6862239888142));
#32193=CARTESIAN_POINT('Ctrl Pts',(-7.54532816924453,-38.2674219719774,
27.680412105204));
#32194=CARTESIAN_POINT('Ctrl Pts',(-7.64277101897887,-38.3362698528497,
27.6746002215939));
#32195=CARTESIAN_POINT('Ctrl Pts',(-7.74027786850679,-38.4051629525368,
27.6687845207786));
#32196=CARTESIAN_POINT('Ctrl Pts',(-7.84071372757151,-38.4697116826011,
27.6629688199633));
#32197=CARTESIAN_POINT('Ctrl Pts',(-7.9436468895561,-38.5296794309353,27.6571531191479));
#32198=CARTESIAN_POINT('Ctrl Pts',(-8.04672748556019,-38.5897330727368,
27.6513290883432));
#32199=CARTESIAN_POINT('Ctrl Pts',(-8.15231216368047,-38.6451924472694,
27.6455050575385));
#32200=CARTESIAN_POINT('Ctrl Pts',(-8.2599471695437,-38.6958681182127,27.6396810267338));
#32201=CARTESIAN_POINT('Ctrl Pts',(-8.28849726270323,-38.7093097965473,
27.6381362075488));
#32202=CARTESIAN_POINT('Ctrl Pts',(-8.31719151868609,-38.7224151763029,
27.6365913883637));
#32203=CARTESIAN_POINT('Ctrl Pts',(-8.34602128478285,-38.7351813088,27.6350465691787));
#32204=CARTESIAN_POINT('Ctrl Pts',(-8.45470265264603,-38.7833065949174,
27.62922296792));
#32205=CARTESIAN_POINT('Ctrl Pts',(-8.56566144290904,-38.826762146425,27.6233993666612));
#32206=CARTESIAN_POINT('Ctrl Pts',(-8.67845927465491,-38.8653272967828,
27.6175757654025));
#32207=CARTESIAN_POINT('Ctrl Pts',(-8.79111479934749,-38.9038437928995,
27.6117595112666));
#32208=CARTESIAN_POINT('Ctrl Pts',(-8.90560436781489,-38.9374820284921,
27.6059432571308));
#32209=CARTESIAN_POINT('Ctrl Pts',(-9.0214678015652,-38.9660685491588,27.600127002995));
#32210=CARTESIAN_POINT('Ctrl Pts',(-9.1372152594184,-38.9946264555571,27.5943165707588));
#32211=CARTESIAN_POINT('Ctrl Pts',(-9.25433345259775,-39.0181426092948,
27.5885061385227));
#32212=CARTESIAN_POINT('Ctrl Pts',(-9.37234571723612,-39.0364929210056,
27.5826957062866));
#32213=CARTESIAN_POINT('Ctrl Pts',(-9.49482476247991,-39.055537794563,27.5766653483834));
#32214=CARTESIAN_POINT('Ctrl Pts',(-9.61826647373684,-39.0690178991552,
27.5706349904802));
#32215=CARTESIAN_POINT('Ctrl Pts',(-9.742124335769,-39.0768523571252,27.5646046325771));
#32216=CARTESIAN_POINT('Ctrl Pts',(-9.86133081533922,-39.0843925983228,
27.5588007399182));
#32217=CARTESIAN_POINT('Ctrl Pts',(-9.98092230874842,-39.0867035537119,
27.5529968472594));
#32218=CARTESIAN_POINT('Ctrl Pts',(-10.1004056308461,-39.0837658734671,
27.5471929546006));
#32219=CARTESIAN_POINT('Ctrl Pts',(-10.2198713070446,-39.0808286270737,
27.5413899190899));
#32220=CARTESIAN_POINT('Ctrl Pts',(-10.3392284355992,-39.0726442965989,
27.5355868835792));
#32221=CARTESIAN_POINT('Ctrl Pts',(-10.4579843811548,-39.0592456573381,
27.5297838480685));
#32222=CARTESIAN_POINT('Ctrl Pts',(-10.5767508144459,-39.0458458347985,
27.5239803000722));
#32223=CARTESIAN_POINT('Ctrl Pts',(-10.694915553396,-39.0272308336835,27.518176752076));
#32224=CARTESIAN_POINT('Ctrl Pts',(-10.8119922711789,-39.0034851756371,
27.5123732040798));
#32225=CARTESIAN_POINT('Ctrl Pts',(-10.9291069581476,-38.9797318166291,
27.5065677739331));
#32226=CARTESIAN_POINT('Ctrl Pts',(-11.0451325222156,-38.950844572643,27.5007623437865));
#32227=CARTESIAN_POINT('Ctrl Pts',(-11.1595946230855,-38.9169586811851,
27.4949569136399));
#32228=CARTESIAN_POINT('Ctrl Pts',(-11.2741834829013,-38.8830352634207,
27.4891450543765));
#32229=CARTESIAN_POINT('Ctrl Pts',(-11.3872050316689,-38.8441022645142,
27.4833331951132));
#32230=CARTESIAN_POINT('Ctrl Pts',(-11.4982016944126,-38.8003442847799,
27.4775213358498));
#32231=CARTESIAN_POINT('Ctrl Pts',(-11.6092712621196,-38.756557563876,27.471705659234));
#32232=CARTESIAN_POINT('Ctrl Pts',(-11.7183129230101,-38.7079397166031,
27.4658899826181));
#32233=CARTESIAN_POINT('Ctrl Pts',(-11.8248921394382,-38.654722107003,27.4600743060023));
#32234=CARTESIAN_POINT('Ctrl Pts',(-11.9316240202275,-38.6014282683534,
27.4542502989954));
#32235=CARTESIAN_POINT('Ctrl Pts',(-12.0358860607236,-38.5435217142231,
27.4484262919884));
#32236=CARTESIAN_POINT('Ctrl Pts',(-12.1372710941066,-38.4812781087262,
27.4426022849815));
#32237=CARTESIAN_POINT('Ctrl Pts',(-12.1641676219605,-38.4647654459286,
27.4410572288578));
#32238=CARTESIAN_POINT('Ctrl Pts',(-12.1908618425745,-38.4479477693427,
27.439512172734));
#32239=CARTESIAN_POINT('Ctrl Pts',(-12.2173465433403,-38.4308307021386,
27.4379671166103));
#32240=CARTESIAN_POINT('Ctrl Pts',(-12.3171719194025,-38.3663135423699,
27.4321435352924));
#32241=CARTESIAN_POINT('Ctrl Pts',(-12.4143401001004,-38.2973318601452,
27.4263199539746));
#32242=CARTESIAN_POINT('Ctrl Pts',(-12.5084262226572,-38.2241313381259,
27.4204963726567));
#32243=CARTESIAN_POINT('Ctrl Pts',(-12.6023936383654,-38.1510231719509,
27.4146801388516));
#32244=CARTESIAN_POINT('Ctrl Pts',(-12.6932864107806,-38.0737070015131,
27.4088639050465));
#32245=CARTESIAN_POINT('Ctrl Pts',(-12.7807072149309,-37.9924726205651,
27.4030476712414));
#32246=CARTESIAN_POINT('Ctrl Pts',(-12.8680405076606,-37.9113195582017,
27.397237259699));
#32247=CARTESIAN_POINT('Ctrl Pts',(-12.9519084489252,-37.8262563645648,
27.3914268481565));
#32248=CARTESIAN_POINT('Ctrl Pts',(-13.0319459642009,-37.737613681688,27.385616436614));
#32249=CARTESIAN_POINT('Ctrl Pts',(-13.1150133113598,-37.6456154170462,
27.3795860710902));
#32250=CARTESIAN_POINT('Ctrl Pts',(-13.19395414564,-37.5497615791823,27.3735557055663));
#32251=CARTESIAN_POINT('Ctrl Pts',(-13.268401237959,-37.4504649248068,27.3675253400425));
#32252=CARTESIAN_POINT('Ctrl Pts',(-13.3400521739576,-37.3548977507787,
27.3617214688537));
#32253=CARTESIAN_POINT('Ctrl Pts',(-13.4075405737231,-37.2561420694291,
27.355917597665));
#32254=CARTESIAN_POINT('Ctrl Pts',(-13.4705799071922,-37.1545997558234,
27.3501137264762));
#32255=CARTESIAN_POINT('Ctrl Pts',(-13.5336099279418,-37.0530724429327,
27.3443107126859));
#32256=CARTESIAN_POINT('Ctrl Pts',(-13.5921919741503,-36.9487596632861,
27.3385076988955));
#32257=CARTESIAN_POINT('Ctrl Pts',(-13.646083412917,-36.8420914054551,27.3327046851052));
#32258=CARTESIAN_POINT('Ctrl Pts',(-13.6999796089217,-36.7354137315404,
27.3269011590569));
#32259=CARTESIAN_POINT('Ctrl Pts',(-13.7491841900861,-36.6263805305119,
27.3210976330085));
#32260=CARTESIAN_POINT('Ctrl Pts',(-13.7935012606565,-36.5154448803562,
27.3152941069602));
#32261=CARTESIAN_POINT('Ctrl Pts',(-13.8378327021985,-36.4044732564084,
27.3094886989665));
#32262=CARTESIAN_POINT('Ctrl Pts',(-13.8772733297251,-36.2915983354265,
27.3036832909728));
#32263=CARTESIAN_POINT('Ctrl Pts',(-13.9116762352757,-36.1772909709921,
27.297877882979));
#32264=CARTESIAN_POINT('Ctrl Pts',(-13.9461172386843,-36.062857022315,27.2920660460629));
#32265=CARTESIAN_POINT('Ctrl Pts',(-13.9755092666319,-35.9469878550576,
27.2862542091468));
#32266=CARTESIAN_POINT('Ctrl Pts',(-13.9997558868884,-35.8301673598144,
27.2804423722307));
#32267=CARTESIAN_POINT('Ctrl Pts',(-14.0240184323186,-35.7132701369014,
27.2746267181016));
#32268=CARTESIAN_POINT('Ctrl Pts',(-14.0431287744825,-35.5954207437815,
27.2688110639726));
#32269=CARTESIAN_POINT('Ctrl Pts',(-14.0570422211961,-35.4771094375846,
27.2629954098435));
#32270=CARTESIAN_POINT('Ctrl Pts',(-14.0709755975632,-35.3586286619967,
27.2571714253579));
#32271=CARTESIAN_POINT('Ctrl Pts',(-14.0796971908158,-35.2396850585239,
27.2513474408724));
#32272=CARTESIAN_POINT('Ctrl Pts',(-14.083214363765,-35.1207702759093,27.2455234563868));
#32273=CARTESIAN_POINT('Ctrl Pts',(-14.0841475669969,-35.0892188961329,
27.2439781922718));
#32274=CARTESIAN_POINT('Ctrl Pts',(-14.0847146691044,-35.0576695226078,
27.2424329281568));
#32275=CARTESIAN_POINT('Ctrl Pts',(-14.0849164197722,-35.0261312739004,
27.2408876640418));
#32276=CARTESIAN_POINT('Ctrl Pts',(-14.0849718051372,-35.0174732732323,
27.2404634522263));
#32277=CARTESIAN_POINT('Ctrl Pts',(-14.0849996645284,-35.0088150963167,
27.2400392404109));
#32278=CARTESIAN_POINT('Ctrl Pts',(-14.0849999969885,-35.0001568563172,
27.2396150285955));
#32279=CARTESIAN_POINT('Origin',(-10.,-35.,32.7603849714045));
#32280=CARTESIAN_POINT('',(-7.51282745730978,-31.7594448403263,29.2969304815276));
#32281=CARTESIAN_POINT('',(-7.5128274573098,-31.7594448403263,29.1925543292906));
#32282=CARTESIAN_POINT('',(-7.5128274573098,-31.7594448403263,32.7603849714045));
#32283=CARTESIAN_POINT('',(-14.0823965473396,-35.0044045793917,29.7396160305011));
#32284=CARTESIAN_POINT('Ctrl Pts',(-14.0849976445926,-35.0043867611016,
29.7396150285955));
#32285=CARTESIAN_POINT('Ctrl Pts',(-14.0851248049252,-34.8859737344617,
29.7338650871352));
#32286=CARTESIAN_POINT('Ctrl Pts',(-14.0800989948151,-34.7674775508307,
29.7281151456748));
#32287=CARTESIAN_POINT('Ctrl Pts',(-14.0699255136412,-34.649384379395,29.7223652042145));
#32288=CARTESIAN_POINT('Ctrl Pts',(-14.0597547176425,-34.5313223773153,
29.7166167803862));
#32289=CARTESIAN_POINT('Ctrl Pts',(-14.0444389866147,-34.4136635905276,
29.7108683565578));
#32290=CARTESIAN_POINT('Ctrl Pts',(-14.0240356521059,-34.2968911388837,
29.7051199327294));
#32291=CARTESIAN_POINT('Ctrl Pts',(-14.0036326709799,-34.1801207097214,
29.6993716084629));
#32292=CARTESIAN_POINT('Ctrl Pts',(-13.9781423333174,-34.0642369953368,
29.6936232841964));
#32293=CARTESIAN_POINT('Ctrl Pts',(-13.9476733383978,-33.9497142230312,
29.6878749599299));
#32294=CARTESIAN_POINT('Ctrl Pts',(-13.9171973565982,-33.8351651893778,
29.6821253175086));
#32295=CARTESIAN_POINT('Ctrl Pts',(-13.8817405552409,-33.7219781204337,
29.6763756750873));
#32296=CARTESIAN_POINT('Ctrl Pts',(-13.8414616644281,-33.6106126239492,
29.670626032666));
#32297=CARTESIAN_POINT('Ctrl Pts',(-13.8011379470234,-33.4991231882111,
29.664869991437));
#32298=CARTESIAN_POINT('Ctrl Pts',(-13.7559815663988,-33.3894597649086,
29.6591139502081));
#32299=CARTESIAN_POINT('Ctrl Pts',(-13.7061997024199,-33.2820626420667,
29.6533579089791));
#32300=CARTESIAN_POINT('Ctrl Pts',(-13.6563885438708,-33.1746023204554,
29.6475984805577));
#32301=CARTESIAN_POINT('Ctrl Pts',(-13.6019466741219,-33.0694113236932,
29.6418390521363));
#32302=CARTESIAN_POINT('Ctrl Pts',(-13.5431267044342,-32.9669042923844,
29.6360796237149));
#32303=CARTESIAN_POINT('Ctrl Pts',(-13.4842097594284,-32.8642282597649,
29.630310699838));
#32304=CARTESIAN_POINT('Ctrl Pts',(-13.4209005215424,-32.7642453812295,
29.6245417759611));
#32305=CARTESIAN_POINT('Ctrl Pts',(-13.3534945117023,-32.6673406678251,
29.6187728520842));
#32306=CARTESIAN_POINT('Ctrl Pts',(-13.3031282057788,-32.5949326963054,
29.6144622663439));
#32307=CARTESIAN_POINT('Ctrl Pts',(-13.2504754795845,-32.5242426933336,
29.6101516806035));
#32308=CARTESIAN_POINT('Ctrl Pts',(-13.1956733769003,-32.4554181742041,
29.6058410948631));
#32309=CARTESIAN_POINT('Ctrl Pts',(-13.1215713269672,-32.3623553590318,
29.6000124272732));
#32310=CARTESIAN_POINT('Ctrl Pts',(-13.0432819943138,-32.2723830731251,
29.5941837596833));
#32311=CARTESIAN_POINT('Ctrl Pts',(-12.961092379355,-32.1859003356445,29.5883550920934));
#32312=CARTESIAN_POINT('Ctrl Pts',(-12.8790067593268,-32.0995270252039,
29.5825337995458));
#32313=CARTESIAN_POINT('Ctrl Pts',(-12.7930309513319,-32.0166347736365,
29.5767125069981));
#32314=CARTESIAN_POINT('Ctrl Pts',(-12.7034931198539,-31.9375908256892,
29.5708912144504));
#32315=CARTESIAN_POINT('Ctrl Pts',(-12.6140453627667,-31.8586263953642,
29.5650757780796));
#32316=CARTESIAN_POINT('Ctrl Pts',(-12.521043014877,-31.7835028349162,29.5592603417089));
#32317=CARTESIAN_POINT('Ctrl Pts',(-12.4248516983507,-31.7125512565204,
29.5534449053381));
#32318=CARTESIAN_POINT('Ctrl Pts',(-12.3251366707921,-31.6390005572414,
29.5474164360446));
#32319=CARTESIAN_POINT('Ctrl Pts',(-12.2219948707104,-31.5699336732242,
29.5413879667511));
#32320=CARTESIAN_POINT('Ctrl Pts',(-12.1158723210058,-31.5056746972839,
29.5353594974577));
#32321=CARTESIAN_POINT('Ctrl Pts',(-12.0136171483038,-31.4437574826985,
29.5295507209964));
#32322=CARTESIAN_POINT('Ctrl Pts',(-11.9085950596014,-31.3863041064149,
29.5237419445352));
#32323=CARTESIAN_POINT('Ctrl Pts',(-11.801234779685,-31.3335605461902,29.5179331680739));
#32324=CARTESIAN_POINT('Ctrl Pts',(-11.6938913330252,-31.2808252557454,
29.5121253023836));
#32325=CARTESIAN_POINT('Ctrl Pts',(-11.5842107899159,-31.2327984923111,
29.5063174366933));
#32326=CARTESIAN_POINT('Ctrl Pts',(-11.4726455446039,-31.1896797903643,
29.500509571003));
#32327=CARTESIAN_POINT('Ctrl Pts',(-11.3610715960219,-31.1465577247023,
29.4947012522377));
#32328=CARTESIAN_POINT('Ctrl Pts',(-11.2476130330501,-31.1083446286469,
29.4888929334724));
#32329=CARTESIAN_POINT('Ctrl Pts',(-11.1327406516267,-31.075191263749,29.4830846147071));
#32330=CARTESIAN_POINT('Ctrl Pts',(-11.0178323368642,-31.0420275281154,
29.4772744790361));
#32331=CARTESIAN_POINT('Ctrl Pts',(-10.901509715417,-31.0139267843516,29.4714643433651));
#32332=CARTESIAN_POINT('Ctrl Pts',(-10.7842564873658,-30.9909893038276,
29.4656542076941));
#32333=CARTESIAN_POINT('Ctrl Pts',(-10.6668759668052,-30.9680269219043,
29.4598377644206));
#32334=CARTESIAN_POINT('Ctrl Pts',(-10.5485632231643,-30.950239070429,29.4540213211471));
#32335=CARTESIAN_POINT('Ctrl Pts',(-10.4298099984691,-30.9376745126448,
29.4482048778736));
#32336=CARTESIAN_POINT('Ctrl Pts',(-10.310980176034,-30.9251018505186,29.4423846829007));
#32337=CARTESIAN_POINT('Ctrl Pts',(-10.1917097125356,-30.9177592172505,
29.4365644879278));
#32338=CARTESIAN_POINT('Ctrl Pts',(-10.0724916561893,-30.9156432624239,
29.4307442929548));
#32339=CARTESIAN_POINT('Ctrl Pts',(-9.95310565333495,-30.9135243267803,
29.4249158988764));
#32340=CARTESIAN_POINT('Ctrl Pts',(-9.83377261098454,-30.9166467554624,
29.419087504798));
#32341=CARTESIAN_POINT('Ctrl Pts',(-9.7149818984416,-30.9249552540145,29.4132591107195));
#32342=CARTESIAN_POINT('Ctrl Pts',(-9.68442702794396,-30.9270923326788,
29.4117599545779));
#32343=CARTESIAN_POINT('Ctrl Pts',(-9.65390799075907,-30.9295722576534,
29.4102607984363));
#32344=CARTESIAN_POINT('Ctrl Pts',(-9.62343300298483,-30.9323935420497,
29.4087616422947));
#32345=CARTESIAN_POINT('Ctrl Pts',(-9.50487393027754,-30.943369390977,29.4029293655663));
#32346=CARTESIAN_POINT('Ctrl Pts',(-9.38661087693688,-30.9595500719646,
29.3970970888379));
#32347=CARTESIAN_POINT('Ctrl Pts',(-9.26913546796359,-30.9809127857421,
29.3912648121095));
#32348=CARTESIAN_POINT('Ctrl Pts',(-9.15179778034071,-31.002250455114,29.3854393728038));
#32349=CARTESIAN_POINT('Ctrl Pts',(-9.03524629757056,-31.0287580038616,
29.3796139334981));
#32350=CARTESIAN_POINT('Ctrl Pts',(-8.91996853885142,-31.0603607978738,
29.3737884941924));
#32351=CARTESIAN_POINT('Ctrl Pts',(-8.8047989632097,-31.0919339340618,29.3679685218038));
#32352=CARTESIAN_POINT('Ctrl Pts',(-8.69090112407866,-31.1285926969889,
29.3621485494153));
#32353=CARTESIAN_POINT('Ctrl Pts',(-8.57875273316241,-31.170211336574,29.3563285770267));
#32354=CARTESIAN_POINT('Ctrl Pts',(-8.46668768181303,-31.2117990485695,
29.3505129295684));
#32355=CARTESIAN_POINT('Ctrl Pts',(-8.35636987120471,-31.2583391599235,
29.3446972821102));
#32356=CARTESIAN_POINT('Ctrl Pts',(-8.24826156776168,-31.3096561860689,
29.3388816346519));
#32357=CARTESIAN_POINT('Ctrl Pts',(-8.14019980301785,-31.3609511211486,
29.3330684907263));
#32358=CARTESIAN_POINT('Ctrl Pts',(-8.03434601938491,-31.4170187044427,
29.3272553468007));
#32359=CARTESIAN_POINT('Ctrl Pts',(-7.93114175266072,-31.4776356587632,
29.3214422028751));
#32360=CARTESIAN_POINT('Ctrl Pts',(-7.82794668659896,-31.5382472090811,
29.3156295771914));
#32361=CARTESIAN_POINT('Ctrl Pts',(-7.72740101990802,-31.6034071207539,
29.3098169515077));
#32362=CARTESIAN_POINT('Ctrl Pts',(-7.62992054908888,-31.6728468029908,
29.304004325824));
#32363=CARTESIAN_POINT('Ctrl Pts',(-7.59037664873343,-31.7010156849423,
29.3016463777252));
#32364=CARTESIAN_POINT('Ctrl Pts',(-7.55133683318268,-31.729888342261,29.2992884296264));
#32365=CARTESIAN_POINT('Ctrl Pts',(-7.51282745730978,-31.7594448403263,
29.2969304815276));
#32366=CARTESIAN_POINT('',(-11.0579044229731,-38.9456385074984,30.));
#32367=CARTESIAN_POINT('Ctrl Pts',(-11.057904422973,-38.9456385074984,30.));
#32368=CARTESIAN_POINT('Ctrl Pts',(-12.3607928946041,-38.596308107828,29.9343068491439));
#32369=CARTESIAN_POINT('Ctrl Pts',(-13.821306101938,-37.2193037646235,29.8475124055022));
#32370=CARTESIAN_POINT('Ctrl Pts',(-14.083832240564,-35.4385219893524,29.7607179618605));
#32371=CARTESIAN_POINT('Ctrl Pts',(-14.0807387137482,-35.0044159360451,
29.739616669075));
#32372=CARTESIAN_POINT('',(-8.94137284034965,-38.9454446564172,29.9999998970666));
#32373=CARTESIAN_POINT('Origin',(-10.,-35.,30.));
#32374=CARTESIAN_POINT('',(-14.084999315681,-34.9976354946767,29.6353849714467));
#32375=CARTESIAN_POINT('Ctrl Pts',(-8.94137284034965,-38.9454446564172,
29.9999998970666));
#32376=CARTESIAN_POINT('Ctrl Pts',(-9.05557825458975,-38.9760878319834,
29.9942072407224));
#32377=CARTESIAN_POINT('Ctrl Pts',(-9.17130798408894,-39.0018198448346,
29.9884145843782));
#32378=CARTESIAN_POINT('Ctrl Pts',(-9.28809962572047,-39.0224896341819,
29.982621928034));
#32379=CARTESIAN_POINT('Ctrl Pts',(-9.40474452355768,-39.0431334528067,
29.9768365499193));
#32380=CARTESIAN_POINT('Ctrl Pts',(-9.52244827714246,-39.0587276246669,
29.9710511718046));
#32381=CARTESIAN_POINT('Ctrl Pts',(-9.64073400885775,-39.0691710393652,
29.9652657936899));
#32382=CARTESIAN_POINT('Ctrl Pts',(-9.75890283044874,-39.0796041321009,
29.9594861336721));
#32383=CARTESIAN_POINT('Ctrl Pts',(-9.87765207688717,-39.0848965571337,
29.9537064736543));
#32384=CARTESIAN_POINT('Ctrl Pts',(-9.9964960350032,-39.0849984972126,29.9479268136365));
#32385=CARTESIAN_POINT('Ctrl Pts',(-10.1152571170041,-39.0851003662034,
29.9421511840783));
#32386=CARTESIAN_POINT('Ctrl Pts',(-10.2341123674742,-39.080018949806,29.93637555452));
#32387=CARTESIAN_POINT('Ctrl Pts',(-10.3525729593925,-39.0697564187928,
29.9305999249618));
#32388=CARTESIAN_POINT('Ctrl Pts',(-10.4709899614492,-39.059497664076,29.9248264206579));
#32389=CARTESIAN_POINT('Ctrl Pts',(-10.5890121825612,-39.0440616202775,
29.9190529163541));
#32390=CARTESIAN_POINT('Ctrl Pts',(-10.7061533900576,-39.0235025027593,
29.9132794120503));
#32391=CARTESIAN_POINT('Ctrl Pts',(-10.8232799176483,-39.0029459616692,
29.9075066312706));
#32392=CARTESIAN_POINT('Ctrl Pts',(-10.9395252442958,-38.9772676949977,
29.901733850491));
#32393=CARTESIAN_POINT('Ctrl Pts',(-11.0544115373312,-38.9465733630509,
29.8959610697114));
#32394=CARTESIAN_POINT('Ctrl Pts',(-11.1693113107022,-38.915875429544,29.8901876115748));
#32395=CARTESIAN_POINT('Ctrl Pts',(-11.2828513343666,-38.8801603677232,
29.8844141534383));
#32396=CARTESIAN_POINT('Ctrl Pts',(-11.3945678743728,-38.839584019626,29.8786406953018));
#32397=CARTESIAN_POINT('Ctrl Pts',(-11.5063934549401,-38.7989680671178,
29.8728616020004));
#32398=CARTESIAN_POINT('Ctrl Pts',(-11.6163916076045,-38.7534814918166,
29.8670825086991));
#32399=CARTESIAN_POINT('Ctrl Pts',(-11.7241173983454,-38.7033287994347,
29.8613034153977));
#32400=CARTESIAN_POINT('Ctrl Pts',(-11.8318953367984,-38.6531518292254,
29.855521524563));
#32401=CARTESIAN_POINT('Ctrl Pts',(-11.9373983553712,-38.5983044328783,
29.8497396337283));
#32402=CARTESIAN_POINT('Ctrl Pts',(-12.0402066034073,-38.5390368768089,
29.8439577428936));
#32403=CARTESIAN_POINT('Ctrl Pts',(-12.1431790206705,-38.4796746794139,
29.8381666192535));
#32404=CARTESIAN_POINT('Ctrl Pts',(-12.243447720281,-38.415878441,29.8323754956134));
#32405=CARTESIAN_POINT('Ctrl Pts',(-12.3406218494647,-38.3479418092029,
29.8265843719733));
#32406=CARTESIAN_POINT('Ctrl Pts',(-12.4324632565271,-38.2837334040672,
29.8211110536318));
#32407=CARTESIAN_POINT('Ctrl Pts',(-12.5215404659313,-38.2158271156631,
29.8156377352903));
#32408=CARTESIAN_POINT('Ctrl Pts',(-12.6075527252282,-38.1445021521944,
29.8101644169488));
#32409=CARTESIAN_POINT('Ctrl Pts',(-12.6979864758416,-38.0695107031664,
29.8044097406971));
#32410=CARTESIAN_POINT('Ctrl Pts',(-12.78534229383,-37.9904821524985,29.7986550644455));
#32411=CARTESIAN_POINT('Ctrl Pts',(-12.8692326440361,-37.907701675619,29.7929003881939));
#32412=CARTESIAN_POINT('Ctrl Pts',(-12.9530187460856,-37.8250240676881,
29.7871528631151));
#32413=CARTESIAN_POINT('Ctrl Pts',(-13.0333476462293,-37.7386040943328,
29.7814053380363));
#32414=CARTESIAN_POINT('Ctrl Pts',(-13.1098640485527,-37.6487677511476,
29.7756578129575));
#32415=CARTESIAN_POINT('Ctrl Pts',(-13.1876741568812,-37.5574124941984,
29.7698131112279));
#32416=CARTESIAN_POINT('Ctrl Pts',(-13.2615413177147,-37.462524548608,29.7639684094983));
#32417=CARTESIAN_POINT('Ctrl Pts',(-13.3311298526084,-37.3644870278903,
29.7581237077686));
#32418=CARTESIAN_POINT('Ctrl Pts',(-13.3994484814726,-37.2682385725532,
29.752385664729));
#32419=CARTESIAN_POINT('Ctrl Pts',(-13.463643061243,-37.1689548732471,29.7466476216893));
#32420=CARTESIAN_POINT('Ctrl Pts',(-13.5234363250196,-37.0670320422123,
29.7409095786496));
#32421=CARTESIAN_POINT('Ctrl Pts',(-13.583209723368,-36.9651430735317,29.73517344199));
#32422=CARTESIAN_POINT('Ctrl Pts',(-13.6385845006397,-36.860617077093,29.7294373053303));
#32423=CARTESIAN_POINT('Ctrl Pts',(-13.6893274390699,-36.7538780024066,
29.7237011686706));
#32424=CARTESIAN_POINT('Ctrl Pts',(-13.7400661989603,-36.6471477173861,
29.7179655043658));
#32425=CARTESIAN_POINT('Ctrl Pts',(-13.7861736993804,-36.5382050952904,
29.712229840061));
#32426=CARTESIAN_POINT('Ctrl Pts',(-13.8274636531967,-36.4274967542725,
29.7064941757563));
#32427=CARTESIAN_POINT('Ctrl Pts',(-13.8701221202582,-36.3131190986384,
29.7005684087305));
#32428=CARTESIAN_POINT('Ctrl Pts',(-13.907637959032,-36.1968570825576,29.6946426417047));
#32429=CARTESIAN_POINT('Ctrl Pts',(-13.9398609751301,-36.0792221720512,
29.6887168746789));
#32430=CARTESIAN_POINT('Ctrl Pts',(-13.9710834565762,-35.9652398620303,
29.6829751045586));
#32431=CARTESIAN_POINT('Ctrl Pts',(-13.9973368939361,-35.8499690830318,
29.6772333344383));
#32432=CARTESIAN_POINT('Ctrl Pts',(-14.0185365737413,-35.7338860984535,
29.6714915643181));
#32433=CARTESIAN_POINT('Ctrl Pts',(-14.0407552795788,-35.61222323794,29.6654737988395));
#32434=CARTESIAN_POINT('Ctrl Pts',(-14.0574222078387,-35.4896686666685,
29.659456033361));
#32435=CARTESIAN_POINT('Ctrl Pts',(-14.0685010078323,-35.3667758842506,
29.6534382678824));
#32436=CARTESIAN_POINT('Ctrl Pts',(-14.0795798078258,-35.2438831018327,
29.6474205024038));
#32437=CARTESIAN_POINT('Ctrl Pts',(-14.0850705212451,-35.1206526339226,
29.6414027369253));
#32438=CARTESIAN_POINT('Ctrl Pts',(-14.084999315681,-34.9976354946767,29.6353849714467));
#32439=CARTESIAN_POINT('Ctrl Pts',(-14.0849993156805,-34.9976354938135,
29.6353849714045));
#32440=CARTESIAN_POINT('Ctrl Pts',(-14.0849113602667,-34.8456808034869,
29.6279516357298));
#32441=CARTESIAN_POINT('Ctrl Pts',(-14.076345106143,-34.6939815686482,29.6205183000551));
#32442=CARTESIAN_POINT('Ctrl Pts',(-14.0593832455855,-34.543236751194,29.6130849643803));
#32443=CARTESIAN_POINT('Ctrl Pts',(-14.0461086539941,-34.4252617283806,
29.6072675309148));
#32444=CARTESIAN_POINT('Ctrl Pts',(-14.0276649934632,-34.3076716578208,
29.6014500974494));
#32445=CARTESIAN_POINT('Ctrl Pts',(-14.0040819085924,-34.1909554590241,
29.5956326639839));
#32446=CARTESIAN_POINT('Ctrl Pts',(-13.9805289239898,-34.0743882309371,
29.589822655599));
#32447=CARTESIAN_POINT('Ctrl Pts',(-13.9518496417305,-33.9586930538953,
29.5840126472142));
#32448=CARTESIAN_POINT('Ctrl Pts',(-13.9181254752496,-33.8443539641396,
29.5782026388294));
#32449=CARTESIAN_POINT('Ctrl Pts',(-13.8844355082274,-33.7301308249135,
29.5723985223364));
#32450=CARTESIAN_POINT('Ctrl Pts',(-13.8457109491444,-33.6172614276375,
29.5665944058434));
#32451=CARTESIAN_POINT('Ctrl Pts',(-13.8020841697217,-33.5062192375213,
29.5607902893504));
#32452=CARTESIAN_POINT('Ctrl Pts',(-13.7567392439761,-33.3908038909825,
29.5547575902863));
#32453=CARTESIAN_POINT('Ctrl Pts',(-13.7060981315312,-33.2773630695008,
29.5487248912222));
#32454=CARTESIAN_POINT('Ctrl Pts',(-13.650366626008,-33.166411034139,29.5426921921581));
#32455=CARTESIAN_POINT('Ctrl Pts',(-13.596808482337,-33.05978579596,29.5368947502953));
#32456=CARTESIAN_POINT('Ctrl Pts',(-13.53854972168,-32.955459273906,29.5310973084325));
#32457=CARTESIAN_POINT('Ctrl Pts',(-13.4758216114673,-32.8538664707767,
29.5252998665696));
#32458=CARTESIAN_POINT('Ctrl Pts',(-13.4131031963228,-32.7522893695255,
29.519503320742));
#32459=CARTESIAN_POINT('Ctrl Pts',(-13.3459170202657,-32.6534454952016,
29.5137067749143));
#32460=CARTESIAN_POINT('Ctrl Pts',(-13.2745391055131,-32.5577431243897,
29.5079102290867));
#32461=CARTESIAN_POINT('Ctrl Pts',(-13.2031552746485,-32.4620328213492,
29.5021132028161));
#32462=CARTESIAN_POINT('Ctrl Pts',(-13.127579259126,-32.3694648676279,29.4963161765455));
#32463=CARTESIAN_POINT('Ctrl Pts',(-13.048128600517,-32.280416018081,29.490519150275));
#32464=CARTESIAN_POINT('Ctrl Pts',(-12.9686524918513,-32.191338643934,29.4847202670702));
#32465=CARTESIAN_POINT('Ctrl Pts',(-12.885299544286,-32.1057829209723,29.4789213838654));
#32466=CARTESIAN_POINT('Ctrl Pts',(-12.7984250584702,-32.0240896868141,
29.4731225006606));
#32467=CARTESIAN_POINT('Ctrl Pts',(-12.7114543284358,-31.9423059485061,
29.4673171931417));
#32468=CARTESIAN_POINT('Ctrl Pts',(-12.620954571213,-31.864393520882,29.4615118856228));
#32469=CARTESIAN_POINT('Ctrl Pts',(-12.5273152611175,-31.7906538717485,
29.4557065781039));
#32470=CARTESIAN_POINT('Ctrl Pts',(-12.4336145483529,-31.7168658688707,
29.4498974638358));
#32471=CARTESIAN_POINT('Ctrl Pts',(-12.3367705145969,-31.6472563318031,
29.4440883495676));
#32472=CARTESIAN_POINT('Ctrl Pts',(-12.237201387277,-31.5820832437337,29.4382792352994));
#32473=CARTESIAN_POINT('Ctrl Pts',(-12.1374888867239,-31.5168163105478,
29.4324617562749));
#32474=CARTESIAN_POINT('Ctrl Pts',(-12.0350438114514,-31.4559987848715,
29.4266442772504));
#32475=CARTESIAN_POINT('Ctrl Pts',(-11.9303088245547,-31.3998426642928,
29.4208267982258));
#32476=CARTESIAN_POINT('Ctrl Pts',(-11.9013754803315,-31.3843293729363,
29.4192197027545));
#32477=CARTESIAN_POINT('Ctrl Pts',(-11.8722674942299,-31.3691715354047,
29.4176126072832));
#32478=CARTESIAN_POINT('Ctrl Pts',(-11.8429944425675,-31.3543729641301,
29.4160055118119));
#32479=CARTESIAN_POINT('Ctrl Pts',(-11.7368984678678,-31.3007376663264,
29.4101808249146));
#32480=CARTESIAN_POINT('Ctrl Pts',(-11.6282885062496,-31.2516513740434,
29.4043561380172));
#32481=CARTESIAN_POINT('Ctrl Pts',(-11.5175912617084,-31.2073568896631,
29.3985314511199));
#32482=CARTESIAN_POINT('Ctrl Pts',(-11.4070336019806,-31.1631182588621,
29.3927141089206));
#32483=CARTESIAN_POINT('Ctrl Pts',(-11.2943942699428,-31.1236595682043,
29.3868967667213));
#32484=CARTESIAN_POINT('Ctrl Pts',(-11.180124143974,-31.0891775794841,29.381079424522));
#32485=CARTESIAN_POINT('Ctrl Pts',(-11.0659683568885,-31.0547300935008,
29.3752679031652));
#32486=CARTESIAN_POINT('Ctrl Pts',(-10.9501854106313,-31.0252495201162,
29.3694563818085));
#32487=CARTESIAN_POINT('Ctrl Pts',(-10.8332451644592,-31.0008841607294,
29.3636448604517));
#32488=CARTESIAN_POINT('Ctrl Pts',(-10.7119096655413,-30.9756030181433,
29.3576149104014));
#32489=CARTESIAN_POINT('Ctrl Pts',(-10.5893285799952,-30.9558293168082,
29.351584960351));
#32490=CARTESIAN_POINT('Ctrl Pts',(-10.466043334308,-30.9416716975401,29.3455550103007));
#32491=CARTESIAN_POINT('Ctrl Pts',(-10.3473577671624,-30.9280422882552,
29.3397500330904));
#32492=CARTESIAN_POINT('Ctrl Pts',(-10.2280200838256,-30.9196174540592,
29.33394505588));
#32493=CARTESIAN_POINT('Ctrl Pts',(-10.1085219886427,-30.9164417503872,
29.3281400786697));
#32494=CARTESIAN_POINT('Ctrl Pts',(-9.98904161281289,-30.9132665176131,
29.3223359622299));
#32495=CARTESIAN_POINT('Ctrl Pts',(-9.86940128034394,-30.9153388782924,
29.3165318457901));
#32496=CARTESIAN_POINT('Ctrl Pts',(-9.75009481274481,-30.9226513029442,
29.3107277293503));
#32497=CARTESIAN_POINT('Ctrl Pts',(-9.6307779101942,-30.9299643671656,29.3049231052627));
#32498=CARTESIAN_POINT('Ctrl Pts',(-9.51179533798562,-30.9425183816275,
29.299118481175));
#32499=CARTESIAN_POINT('Ctrl Pts',(-9.3936372666126,-30.9602538154534,29.2933138570874));
#32500=CARTESIAN_POINT('Ctrl Pts',(-9.27544100576304,-30.9779949814898,
29.2875073569065));
#32501=CARTESIAN_POINT('Ctrl Pts',(-9.15807017916034,-31.0009208368988,
29.2817008567256));
#32502=CARTESIAN_POINT('Ctrl Pts',(-9.04200558532037,-31.0289205873664,
29.2758943565448));
#32503=CARTESIAN_POINT('Ctrl Pts',(-8.92581277050846,-31.0569512702234,
29.2700814417023));
#32504=CARTESIAN_POINT('Ctrl Pts',(-8.81092946592161,-31.0900669411032,
29.2642685268598));
#32505=CARTESIAN_POINT('Ctrl Pts',(-8.69782225691509,-31.1281066484968,
29.2584556120173));
#32506=CARTESIAN_POINT('Ctrl Pts',(-8.58464091024233,-31.1661712895367,
29.2526388870203));
#32507=CARTESIAN_POINT('Ctrl Pts',(-8.47323835756487,-31.2091662482557,
29.2468221620233));
#32508=CARTESIAN_POINT('Ctrl Pts',(-8.36406057817883,-31.2568826884358,
29.2410054370263));
#32509=CARTESIAN_POINT('Ctrl Pts',(-8.25472678958248,-31.3046673128582,
29.2351804002403));
#32510=CARTESIAN_POINT('Ctrl Pts',(-8.14762448475744,-31.3571867058625,
29.2293553634542));
#32511=CARTESIAN_POINT('Ctrl Pts',(-8.04317458259696,-31.4141863844024,
29.2235303266682));
#32512=CARTESIAN_POINT('Ctrl Pts',(-8.01565456857819,-31.4292044162055,
29.2219955708599));
#32513=CARTESIAN_POINT('Ctrl Pts',(-7.98831852233574,-31.4445332365823,
29.2204608150517));
#32514=CARTESIAN_POINT('Ctrl Pts',(-7.96117378602652,-31.4601677060608,
29.2189260592434));
#32515=CARTESIAN_POINT('Ctrl Pts',(-7.85816142420679,-31.5194994162102,
29.2131017690818));
#32516=CARTESIAN_POINT('Ctrl Pts',(-7.75757567177424,-31.583426782036,29.2072774789202));
#32517=CARTESIAN_POINT('Ctrl Pts',(-7.65985340609903,-31.651725979097,29.2014531887587));
#32518=CARTESIAN_POINT('Ctrl Pts',(-7.61008386709288,-31.686510472976,29.1984869022693));
#32519=CARTESIAN_POINT('Ctrl Pts',(-7.56105674097248,-31.7224281736847,
29.19552061578));
#32520=CARTESIAN_POINT('Ctrl Pts',(-7.5128274573098,-31.7594448403263,29.1925543292906));
#32521=CARTESIAN_POINT('Origin',(-10.,-35.,23.));
#32522=CARTESIAN_POINT('',(-13.1787500647504,-33.8227349116068,17.9149431671188));
#32523=CARTESIAN_POINT('',(-13.1787501240207,-33.8227350716434,17.5703580349972));
#32524=CARTESIAN_POINT('',(-13.1787501240207,-33.8227350716434,23.));
#32525=CARTESIAN_POINT('',(-6.62123117139838,-35.2726284383003,17.));
#32526=CARTESIAN_POINT('Ctrl Pts',(-13.1787501240207,-33.8227350716434,
17.5703580349972));
#32527=CARTESIAN_POINT('Ctrl Pts',(-13.1427561410128,-33.7255471955804,
17.5642606734842));
#32528=CARTESIAN_POINT('Ctrl Pts',(-13.1022543457953,-33.6298857670595,
17.5581633119711));
#32529=CARTESIAN_POINT('Ctrl Pts',(-13.0573978208791,-33.5361954955036,
17.5520659504581));
#32530=CARTESIAN_POINT('Ctrl Pts',(-13.01258486052,-33.4425962157308,17.545974510689));
#32531=CARTESIAN_POINT('Ctrl Pts',(-12.9634257646823,-33.3509646690272,
17.5398830709199));
#32532=CARTESIAN_POINT('Ctrl Pts',(-12.9101220782721,-33.2617265600448,
17.5337916311508));
#32533=CARTESIAN_POINT('Ctrl Pts',(-12.8568522287991,-33.1725450990076,
17.5277040581999));
#32534=CARTESIAN_POINT('Ctrl Pts',(-12.7994432384854,-33.085754420227,17.521616485249));
#32535=CARTESIAN_POINT('Ctrl Pts',(-12.7381426726736,-33.001755829088,17.5155289122981));
#32536=CARTESIAN_POINT('Ctrl Pts',(-12.6768617435676,-32.9177841456227,
17.5094432894088));
#32537=CARTESIAN_POINT('Ctrl Pts',(-12.6116919681767,-32.8366031166276,
17.5033576665195));
#32538=CARTESIAN_POINT('Ctrl Pts',(-12.5429238704387,-32.7585845428272,
17.4972720436302));
#32539=CARTESIAN_POINT('Ctrl Pts',(-12.4741600755362,-32.6805708506667,
17.4911868015197));
#32540=CARTESIAN_POINT('Ctrl Pts',(-12.4017986884822,-32.6057195403265,
17.4851015594092));
#32541=CARTESIAN_POINT('Ctrl Pts',(-12.3261695030696,-32.53436813261,17.4790163172987));
#32542=CARTESIAN_POINT('Ctrl Pts',(-12.2505255555982,-32.4630027978142,
17.47292988741));
#32543=CARTESIAN_POINT('Ctrl Pts',(-12.171612852793,-32.3951390161126,17.4668434575212));
#32544=CARTESIAN_POINT('Ctrl Pts',(-12.0897962284543,-32.3310757249337,
17.4607570276325));
#32545=CARTESIAN_POINT('Ctrl Pts',(-12.0078921757233,-32.2669439763894,
17.4546640938482));
#32546=CARTESIAN_POINT('Ctrl Pts',(-11.9230783421455,-32.2066210909662,
17.4485711600638));
#32547=CARTESIAN_POINT('Ctrl Pts',(-11.8357506295315,-32.1503641129655,
17.4424782262795));
#32548=CARTESIAN_POINT('Ctrl Pts',(-11.7483725193403,-32.094074668577,17.4363817762105));
#32549=CARTESIAN_POINT('Ctrl Pts',(-11.6584780096167,-32.0418560193866,
17.4302853261415));
#32550=CARTESIAN_POINT('Ctrl Pts',(-11.5664880974162,-31.9939194782652,
17.4241888760725));
#32551=CARTESIAN_POINT('Ctrl Pts',(-11.4743515815419,-31.9459065410165,
17.418082710134));
#32552=CARTESIAN_POINT('Ctrl Pts',(-11.3801133808725,-31.9021895209563,
17.4119765441955));
#32553=CARTESIAN_POINT('Ctrl Pts',(-11.284215100619,-31.8629318404213,17.405870378257));
#32554=CARTESIAN_POINT('Ctrl Pts',(-11.2229049351904,-31.8378334248755,
17.4019665538836));
#32555=CARTESIAN_POINT('Ctrl Pts',(-11.1609165924618,-31.8145567073918,
17.3980627295102));
#32556=CARTESIAN_POINT('Ctrl Pts',(-11.0983682718265,-31.7931335852666,
17.3941589051368));
#32557=CARTESIAN_POINT('Ctrl Pts',(-11.0015147354448,-31.7599607499757,
17.3881139915062));
#32558=CARTESIAN_POINT('Ctrl Pts',(-10.9029758716802,-31.7311176974456,
17.3820690778757));
#32559=CARTESIAN_POINT('Ctrl Pts',(-10.8031787497248,-31.706778331407,17.3760241642451));
#32560=CARTESIAN_POINT('Ctrl Pts',(-10.7035144749785,-31.6824713652691,
17.3699872974388));
#32561=CARTESIAN_POINT('Ctrl Pts',(-10.6025956903531,-31.6626562751579,
17.3639504306325));
#32562=CARTESIAN_POINT('Ctrl Pts',(-10.5008673376754,-31.6474581326179,
17.3579135638262));
#32563=CARTESIAN_POINT('Ctrl Pts',(-10.3992439061861,-31.6322756652278,
17.3518829233592));
#32564=CARTESIAN_POINT('Ctrl Pts',(-10.2968129954217,-31.6217007449999,
17.3458522828922));
#32565=CARTESIAN_POINT('Ctrl Pts',(-10.1940315703266,-31.6158078050713,
17.3398216424252));
#32566=CARTESIAN_POINT('Ctrl Pts',(-10.0913190575091,-31.6099188162059,
17.3337950453461));
#32567=CARTESIAN_POINT('Ctrl Pts',(-9.98825693183714,-31.6087055948162,
17.327768448267));
#32568=CARTESIAN_POINT('Ctrl Pts',(-9.88530824168519,-31.6121908461257,
17.3217418511879));
#32569=CARTESIAN_POINT('Ctrl Pts',(-9.782394873529,-31.6156749016352,17.3157173218519));
#32570=CARTESIAN_POINT('Ctrl Pts',(-9.67959529947481,-31.6238542132337,
17.3096927925158));
#32571=CARTESIAN_POINT('Ctrl Pts',(-9.57737257670802,-31.6366993706209,
17.3036682631798));
#32572=CARTESIAN_POINT('Ctrl Pts',(-9.47515720184965,-31.6495436046807,
17.2976441668951));
#32573=CARTESIAN_POINT('Ctrl Pts',(-9.37351902910539,-31.6670529636749,
17.2916200706104));
#32574=CARTESIAN_POINT('Ctrl Pts',(-9.2729149678679,-31.6891462704388,17.2855959743257));
#32575=CARTESIAN_POINT('Ctrl Pts',(-9.17229085089137,-31.7112439815735,
17.2795706771182));
#32576=CARTESIAN_POINT('Ctrl Pts',(-9.07270168135648,-31.7379273619785,
17.2735453799108));
#32577=CARTESIAN_POINT('Ctrl Pts',(-8.97459215180163,-31.7690645615622,
17.2675200827034));
#32578=CARTESIAN_POINT('Ctrl Pts',(-8.87636670556745,-31.8002385498329,
17.2614876665907));
#32579=CARTESIAN_POINT('Ctrl Pts',(-8.77962480708826,-31.8358767325254,
17.2554552504781));
#32580=CARTESIAN_POINT('Ctrl Pts',(-8.68479394402274,-31.8757980070391,
17.2494228343654));
#32581=CARTESIAN_POINT('Ctrl Pts',(-8.58990614490615,-31.915743250118,17.2433867964155));
#32582=CARTESIAN_POINT('Ctrl Pts',(-8.49693205876363,-31.9599765155484,
17.2373507584656));
#32583=CARTESIAN_POINT('Ctrl Pts',(-8.40627520250295,-32.0082703443755,
17.2313147205157));
#32584=CARTESIAN_POINT('Ctrl Pts',(-8.31545155112396,-32.0566530266576,
17.2252675771546));
#32585=CARTESIAN_POINT('Ctrl Pts',(-8.22695402074023,-32.109110971783,17.2192204337935));
#32586=CARTESIAN_POINT('Ctrl Pts',(-8.14115796984813,-32.1653727988603,
17.2131732904325));
#32587=CARTESIAN_POINT('Ctrl Pts',(-8.0650455726394,-32.2152844496377,17.2078086778111));
#32588=CARTESIAN_POINT('Ctrl Pts',(-7.99105895925869,-32.2681890221868,
17.2024440651898));
#32589=CARTESIAN_POINT('Ctrl Pts',(-7.91943702063162,-32.3238716863009,
17.1970794525685));
#32590=CARTESIAN_POINT('Ctrl Pts',(-7.83581776040074,-32.3888816995757,
17.1908162188803));
#32591=CARTESIAN_POINT('Ctrl Pts',(-7.75513118295744,-32.4579052413955,
17.1845529851921));
#32592=CARTESIAN_POINT('Ctrl Pts',(-7.67777316876516,-32.5306544173014,
17.178289751504));
#32593=CARTESIAN_POINT('Ctrl Pts',(-7.60052793358127,-32.6032975333504,
17.1720356488837));
#32594=CARTESIAN_POINT('Ctrl Pts',(-7.52660189303604,-32.6796552011327,
17.1657815462635));
#32595=CARTESIAN_POINT('Ctrl Pts',(-7.45635876139179,-32.7593986718401,
17.1595274436433));
#32596=CARTESIAN_POINT('Ctrl Pts',(-7.3862020003943,-32.8390440903256,17.1532810310403));
#32597=CARTESIAN_POINT('Ctrl Pts',(-7.3197193970536,-32.9220667257876,17.1470346184372));
#32598=CARTESIAN_POINT('Ctrl Pts',(-7.25723821870783,-33.0081006868863,
17.1407882058342));
#32599=CARTESIAN_POINT('Ctrl Pts',(-7.19483021640349,-33.0940338876461,
17.1345491088381));
#32600=CARTESIAN_POINT('Ctrl Pts',(-7.13641453710058,-33.1829710653652,
17.1283100118421));
#32601=CARTESIAN_POINT('Ctrl Pts',(-7.08227801460293,-33.2745135531014,
17.1220709148461));
#32602=CARTESIAN_POINT('Ctrl Pts',(-7.02817855180624,-33.3659933745071,
17.1158360888867));
#32603=CARTESIAN_POINT('Ctrl Pts',(-6.97835261871944,-33.4600746128199,
17.1096012629272));
#32604=CARTESIAN_POINT('Ctrl Pts',(-6.93304349073857,-33.5563300817711,
17.1033664369678));
#32605=CARTESIAN_POINT('Ctrl Pts',(-6.88775601855788,-33.6525395447784,
17.0971345909851));
#32606=CARTESIAN_POINT('Ctrl Pts',(-6.84698122377164,-33.7509208080942,
17.0909027450024));
#32607=CARTESIAN_POINT('Ctrl Pts',(-6.81091594762553,-33.8510230770852,
17.0846708990196));
#32608=CARTESIAN_POINT('Ctrl Pts',(-6.77486046283198,-33.9510981693368,
17.0784407449191));
#32609=CARTESIAN_POINT('Ctrl Pts',(-6.74351208542603,-34.0528929604214,
17.0722105908187));
#32610=CARTESIAN_POINT('Ctrl Pts',(-6.71701891222609,-34.1559382488118,
17.0659804367182));
#32611=CARTESIAN_POINT('Ctrl Pts',(-6.6905202480665,-34.2590048943087,17.0597489913596));
#32612=CARTESIAN_POINT('Ctrl Pts',(-6.6688789034052,-34.3633221685375,17.053517546001));
#32613=CARTESIAN_POINT('Ctrl Pts',(-6.65219258767227,-34.4684074939735,
17.0472861006425));
#32614=CARTESIAN_POINT('Ctrl Pts',(-6.63550481518413,-34.5735019936094,
17.0410541112638));
#32615=CARTESIAN_POINT('Ctrl Pts',(-6.62377298967071,-34.6793642816695,
17.0348221218852));
#32616=CARTESIAN_POINT('Ctrl Pts',(-6.61704319803061,-34.7855044557361,
17.0285901325065));
#32617=CARTESIAN_POINT('Ctrl Pts',(-6.61030887275071,-34.8917161329553,
17.0223539448411));
#32618=CARTESIAN_POINT('Ctrl Pts',(-6.60858333145876,-34.9982056700471,
17.0161177571757));
#32619=CARTESIAN_POINT('Ctrl Pts',(-6.61186057071778,-35.1044809563661,
17.0098815695103));
#32620=CARTESIAN_POINT('Ctrl Pts',(-6.61359155708732,-35.1606138955556,
17.0065877130069));
#32621=CARTESIAN_POINT('Ctrl Pts',(-6.61671733632887,-35.2166870797046,
17.0032938565034));
#32622=CARTESIAN_POINT('Ctrl Pts',(-6.62123117139838,-35.2726284383002,
17.));
#32623=CARTESIAN_POINT('',(-13.1787501240207,-33.8227350716434,17.));
#32624=CARTESIAN_POINT('Origin',(-10.,-35.,17.));
#32625=CARTESIAN_POINT('',(-13.1787501240207,-33.8227350716434,16.));
#32626=CARTESIAN_POINT('',(-13.1787501240207,-33.8227350716434,23.));
#32627=CARTESIAN_POINT('Origin',(-10.,-35.,16.));
#32628=CARTESIAN_POINT('',(-10.7859688154841,-38.3003672135327,16.9983147074305));
#32629=CARTESIAN_POINT('Origin',(-10.,-35.,17.));
#32630=CARTESIAN_POINT('Ctrl Pts',(-10.7851704499296,-38.2975615880613,
16.9966427327388));
#32631=CARTESIAN_POINT('Ctrl Pts',(-10.743310784149,-38.3075286415149,16.9992508007924));
#32632=CARTESIAN_POINT('Ctrl Pts',(-10.7012668042908,-38.3166973331851,
17.0018967864938));
#32633=CARTESIAN_POINT('Ctrl Pts',(-10.4536050921614,-38.3657864213433,
17.0175939914567));
#32634=CARTESIAN_POINT('Ctrl Pts',(-10.2448259397233,-38.3873780071541,
17.0312412363625));
#32635=CARTESIAN_POINT('Ctrl Pts',(-9.87026006962071,-38.3912897903155,
17.0553063052265));
#32636=CARTESIAN_POINT('Ctrl Pts',(-9.70520066741884,-38.3809441326568,
17.0657713163129));
#32637=CARTESIAN_POINT('Ctrl Pts',(-9.47799215449731,-38.3499292672403,
17.0798307027395));
#32638=CARTESIAN_POINT('Ctrl Pts',(-9.41470309195617,-38.3394530452039,
17.0837111912157));
#32639=CARTESIAN_POINT('Ctrl Pts',(-9.31979469515452,-38.3209615248075,
17.0894789550261));
#32640=CARTESIAN_POINT('Ctrl Pts',(-9.28793387478838,-38.3142761877813,
17.0914064393494));
#32641=CARTESIAN_POINT('Ctrl Pts',(-9.23261394171108,-38.3018338584622,
17.0947390357368));
#32642=CARTESIAN_POINT('Ctrl Pts',(-9.2091112994877,-38.2962832552482,17.0961504272415));
#32643=CARTESIAN_POINT('Ctrl Pts',(-9.155972702891,-38.2831324826891,17.0993322820044));
#32644=CARTESIAN_POINT('Ctrl Pts',(-9.1263760784018,-38.2753812461509,17.1010979086763));
#32645=CARTESIAN_POINT('Ctrl Pts',(-9.04609325646344,-38.2531898497246,
17.1058720754798));
#32646=CARTESIAN_POINT('Ctrl Pts',(-8.99563138749464,-38.2379663945757,
17.1088561314373));
#32647=CARTESIAN_POINT('Ctrl Pts',(-8.76968187411001,-38.164010562092,17.1221720717703));
#32648=CARTESIAN_POINT('Ctrl Pts',(-8.59882344241059,-38.0921445722062,
17.1320944660758));
#32649=CARTESIAN_POINT('Ctrl Pts',(-8.29718144020483,-37.9351050419574,
17.1502153077104));
#32650=CARTESIAN_POINT('Ctrl Pts',(-8.16476885351069,-37.854181934104,17.1584174494901));
#32651=CARTESIAN_POINT('Ctrl Pts',(-7.9757713259831,-37.7200724455312,17.1711242245388));
#32652=CARTESIAN_POINT('Ctrl Pts',(-7.91470806847342,-37.6735466616793,
17.1754029777835));
#32653=CARTESIAN_POINT('Ctrl Pts',(-7.83652006488241,-37.6096640687498,
17.1811898260787));
#32654=CARTESIAN_POINT('Ctrl Pts',(-7.81792477349181,-37.5941356203807,
17.1825901036778));
#32655=CARTESIAN_POINT('Ctrl Pts',(-7.7874099083126,-37.5680932035323,17.184931071396));
#32656=CARTESIAN_POINT('Ctrl Pts',(-7.77539469403909,-37.5576920898364,
17.185864133032));
#32657=CARTESIAN_POINT('Ctrl Pts',(-7.75262087849325,-37.5376957961096,
17.1876553464526));
#32658=CARTESIAN_POINT('Ctrl Pts',(-7.74184944242308,-37.528115683896,17.188512393171));
#32659=CARTESIAN_POINT('Ctrl Pts',(-7.71229652554076,-37.5014917769243,
17.1908903428796));
#32660=CARTESIAN_POINT('Ctrl Pts',(-7.69364509275221,-37.4843057895331,
17.1924210383931));
#32661=CARTESIAN_POINT('Ctrl Pts',(-7.61451756643669,-37.4097362461635,
17.1990378438738));
#32662=CARTESIAN_POINT('Ctrl Pts',(-7.55598058899076,-37.3503451320522,
17.2042454098228));
#32663=CARTESIAN_POINT('Ctrl Pts',(-7.36537999728428,-37.1421371666012,
17.2221251233073));
#32664=CARTESIAN_POINT('Ctrl Pts',(-7.24423963964011,-36.9838752006094,
17.2350787935645));
#32665=CARTESIAN_POINT('Ctrl Pts',(-7.08015664818693,-36.7252385742279,
17.2546065819693));
#32666=CARTESIAN_POINT('Ctrl Pts',(-7.02697486690723,-36.6318878458345,
17.2613681618698));
#32667=CARTESIAN_POINT('Ctrl Pts',(-6.94433807822268,-36.4693383033307,
17.272621959888));
#32668=CARTESIAN_POINT('Ctrl Pts',(-6.91258980521957,-36.4014008782826,
17.2771806671139));
#32669=CARTESIAN_POINT('Ctrl Pts',(-6.86963337246016,-36.3009176606076,
17.2837169481035));
#32670=CARTESIAN_POINT('Ctrl Pts',(-6.85662736934266,-36.2691692622874,
17.2857530480205));
#32671=CARTESIAN_POINT('Ctrl Pts',(-6.83436650218949,-36.2123867170112,
17.2893444951596));
#32672=CARTESIAN_POINT('Ctrl Pts',(-6.82492124245694,-36.1874308137927,
17.2909059816516));
#32673=CARTESIAN_POINT('Ctrl Pts',(-6.80551948703197,-36.1342808994909,
17.2941967983839));
#32674=CARTESIAN_POINT('Ctrl Pts',(-6.79563932667782,-36.1060613293273,
17.2959235384772));
#32675=CARTESIAN_POINT('Ctrl Pts',(-6.76978587126011,-36.0289633729162,
17.3005880348398));
#32676=CARTESIAN_POINT('Ctrl Pts',(-6.754548971306,-35.9798453703461,17.3035021502739));
#32677=CARTESIAN_POINT('Ctrl Pts',(-6.67131670554485,-35.6882486125514,
17.3205003365769));
#32678=CARTESIAN_POINT('Ctrl Pts',(-6.6293955554992,-35.4391531640892,17.333727087924));
#32679=CARTESIAN_POINT('Ctrl Pts',(-6.60889389514483,-35.0694671655412,
17.3533940834857));
#32680=CARTESIAN_POINT('Ctrl Pts',(-6.60853713860263,-34.9509815624263,
17.3597169713223));
#32681=CARTESIAN_POINT('Ctrl Pts',(-6.61764102105995,-34.7667172823524,
17.3698807385786));
#32682=CARTESIAN_POINT('Ctrl Pts',(-6.6228320213891,-34.7008204603456,17.3735823273943));
#32683=CARTESIAN_POINT('Ctrl Pts',(-6.63239785953204,-34.6124692984434,
17.378684005663));
#32684=CARTESIAN_POINT('Ctrl Pts',(-6.63507874324607,-34.5898425955063,
17.3800028587966));
#32685=CARTESIAN_POINT('Ctrl Pts',(-6.63995072011255,-34.5519928678066,
17.3822321999947));
#32686=CARTESIAN_POINT('Ctrl Pts',(-6.64201774271023,-34.5367541650539,
17.3831360751198));
#32687=CARTESIAN_POINT('Ctrl Pts',(-6.64650987282731,-34.5052480139126,
17.3850188527511));
#32688=CARTESIAN_POINT('Ctrl Pts',(-6.64894979124846,-34.4889833327116,
17.3859984918382));
#32689=CARTESIAN_POINT('Ctrl Pts',(-6.65589118590911,-34.444900542759,17.3886733059703));
#32690=CARTESIAN_POINT('Ctrl Pts',(-6.66062125647275,-34.4171203706953,
17.3903802186767));
#32691=CARTESIAN_POINT('Ctrl Pts',(-6.69129122312531,-34.2496399665877,
17.4007866703774));
#32692=CARTESIAN_POINT('Ctrl Pts',(-6.72564565888985,-34.1116362216724,
17.4098446557825));
#32693=CARTESIAN_POINT('Ctrl Pts',(-6.8285199248545,-33.7869285076647,17.4317545759383));
#32694=CARTESIAN_POINT('Ctrl Pts',(-6.90500801021866,-33.6032665645102,
17.4446235142211));
#32695=CARTESIAN_POINT('Ctrl Pts',(-7.04728568991387,-33.331597609153,17.4638622851735));
#32696=CARTESIAN_POINT('Ctrl Pts',(-7.10198759315005,-33.2382916739901,
17.4705173604536));
#32697=CARTESIAN_POINT('Ctrl Pts',(-7.18221228691058,-33.1153313416155,
17.4793444461009));
#32698=CARTESIAN_POINT('Ctrl Pts',(-7.20391901803817,-33.0832749603318,
17.4816515973875));
#32699=CARTESIAN_POINT('Ctrl Pts',(-7.2417591886613,-33.029404104059,17.4855403539966));
#32700=CARTESIAN_POINT('Ctrl Pts',(-7.25761367514143,-33.0073992201757,
17.4871322078223));
#32701=CARTESIAN_POINT('Ctrl Pts',(-7.28829108222011,-32.9658809982845,
17.4901430954114));
#32702=CARTESIAN_POINT('Ctrl Pts',(-7.30306476304412,-32.9463335855415,
17.49156387896));
#32703=CARTESIAN_POINT('Ctrl Pts',(-7.34205426499023,-32.8958920610367,
17.4952397728289));
#32704=CARTESIAN_POINT('Ctrl Pts',(-7.36659742194331,-32.8652548647136,
17.4974819577439));
#32705=CARTESIAN_POINT('Ctrl Pts',(-7.45796147147842,-32.755179448133,17.5055816764898));
#32706=CARTESIAN_POINT('Ctrl Pts',(-7.52789198927584,-32.6783919661395,
17.5113151602841));
#32707=CARTESIAN_POINT('Ctrl Pts',(-7.78132600292532,-32.424567658594,17.5307906942772));
#32708=CARTESIAN_POINT('Ctrl Pts',(-7.98116525377509,-32.2651027509197,
17.5439231045514));
#32709=CARTESIAN_POINT('Ctrl Pts',(-8.25195591528014,-32.0950108486595,
17.5612419288636));
#32710=CARTESIAN_POINT('Ctrl Pts',(-8.30791132282685,-32.0620661754796,
17.564801953498));
#32711=CARTESIAN_POINT('Ctrl Pts',(-8.40358858683736,-32.009374805817,17.5709153478751));
#32712=CARTESIAN_POINT('Ctrl Pts',(-8.4428155412199,-31.9887636050222,17.5734289693904));
#32713=CARTESIAN_POINT('Ctrl Pts',(-8.49991066293199,-31.9601777889932,
17.577113822043));
#32714=CARTESIAN_POINT('Ctrl Pts',(-8.51746301095371,-31.9515789119634,
17.5782501433891));
#32715=CARTESIAN_POINT('Ctrl Pts',(-8.54837976707107,-31.9367629871929,
17.5802594855762));
#32716=CARTESIAN_POINT('Ctrl Pts',(-8.56171186708872,-31.9304805704015,
17.5811285728894));
#32717=CARTESIAN_POINT('Ctrl Pts',(-8.59145379517805,-31.9167017493821,
17.5830733786653));
#32718=CARTESIAN_POINT('Ctrl Pts',(-8.60788263331463,-31.9092493276539,
17.584151532289));
#32719=CARTESIAN_POINT('Ctrl Pts',(-8.65695942033241,-31.8874578635176,
17.5873820370072));
#32720=CARTESIAN_POINT('Ctrl Pts',(-8.68977401939683,-31.8735028845947,
17.5895548905233));
#32721=CARTESIAN_POINT('Ctrl Pts',(-8.88703087619828,-31.7932666623742,
17.6026667935407));
#32722=CARTESIAN_POINT('Ctrl Pts',(-9.05623637117996,-31.7394571049311,
17.6141062712943));
#32723=CARTESIAN_POINT('Ctrl Pts',(-9.38864232342969,-31.6618012127062,
17.6361100763141));
#32724=CARTESIAN_POINT('Ctrl Pts',(-9.55093775625886,-31.6361212093345,
17.6466475337112));
#32725=CARTESIAN_POINT('Ctrl Pts',(-9.81202945562476,-31.6140497751506,
17.6630089955334));
#32726=CARTESIAN_POINT('Ctrl Pts',(-9.90991152828183,-31.6100326312856,
17.669015680292));
#32727=CARTESIAN_POINT('Ctrl Pts',(-10.0454778836812,-31.6103460946026,
17.677155675251));
#32728=CARTESIAN_POINT('Ctrl Pts',(-10.0831148528553,-31.6110600582777,
17.6793967067006));
#32729=CARTESIAN_POINT('Ctrl Pts',(-10.1478084975021,-31.613365725654,17.6832177877439));
#32730=CARTESIAN_POINT('Ctrl Pts',(-10.1748717170049,-31.6146552603872,
17.6848069267013));
#32731=CARTESIAN_POINT('Ctrl Pts',(-10.2302215503355,-31.6179581476324,
17.6880389357425));
#32732=CARTESIAN_POINT('Ctrl Pts',(-10.2585042251357,-31.620002264818,17.6896807312807));
#32733=CARTESIAN_POINT('Ctrl Pts',(-10.3308235983518,-31.6261421884174,
17.6938558611301));
#32734=CARTESIAN_POINT('Ctrl Pts',(-10.3748125349363,-31.6307453935645,
17.6963735194634));
#32735=CARTESIAN_POINT('Ctrl Pts',(-10.5787240470861,-31.6561268122918,
17.7079589752589));
#32736=CARTESIAN_POINT('Ctrl Pts',(-10.7371303936744,-31.6874396847406,
17.7167017768494));
#32737=CARTESIAN_POINT('Ctrl Pts',(-11.080734111676,-31.7812420173593,17.7357197583529));
#32738=CARTESIAN_POINT('Ctrl Pts',(-11.2639619996605,-31.8486856309957,
17.7458951436701));
#32739=CARTESIAN_POINT('Ctrl Pts',(-11.5182586887286,-31.9680536253725,
17.7611965963785));
#32740=CARTESIAN_POINT('Ctrl Pts',(-11.5947203668731,-32.007564046601,17.7659666375772));
#32741=CARTESIAN_POINT('Ctrl Pts',(-11.6912088833232,-32.0621717811038,
17.7723107866141));
#32742=CARTESIAN_POINT('Ctrl Pts',(-11.7126918010815,-32.0746438082891,
17.7737447764485));
#32743=CARTESIAN_POINT('Ctrl Pts',(-11.7476204917344,-32.0954384735782,
17.7761148612058));
#32744=CARTESIAN_POINT('Ctrl Pts',(-11.7611489165214,-32.1036213098265,
17.7770424477029));
#32745=CARTESIAN_POINT('Ctrl Pts',(-11.7882289210827,-32.1202608552763,
17.7789196386815));
#32746=CARTESIAN_POINT('Ctrl Pts',(-11.8017789396394,-32.128719302198,17.7798693394958));
#32747=CARTESIAN_POINT('Ctrl Pts',(-11.8369774714619,-32.1510388532362,
17.7823625913552));
#32748=CARTESIAN_POINT('Ctrl Pts',(-11.8585285872754,-32.1650507500312,
17.7839153010184));
#32749=CARTESIAN_POINT('Ctrl Pts',(-11.9529827620085,-32.2280019438361,
17.7908296431376));
#32750=CARTESIAN_POINT('Ctrl Pts',(-12.024122872019,-32.2795149174791,17.7963271991821));
#32751=CARTESIAN_POINT('Ctrl Pts',(-12.264603946402,-32.4683063331739,17.8157385601154));
#32752=CARTESIAN_POINT('Ctrl Pts',(-12.4226538947103,-32.619105570469,17.8299665660269));
#32753=CARTESIAN_POINT('Ctrl Pts',(-12.6570594593548,-32.8904474021813,
17.8527151022909));
#32754=CARTESIAN_POINT('Ctrl Pts',(-12.7422797865341,-33.0024798730737,
17.8614577830914));
#32755=CARTESIAN_POINT('Ctrl Pts',(-12.8435903142834,-33.1544211308715,
17.8724712358748));
#32756=CARTESIAN_POINT('Ctrl Pts',(-12.8662282162011,-33.1897781109792,
17.874979389166));
#32757=CARTESIAN_POINT('Ctrl Pts',(-12.9027949185996,-33.2492962550207,
17.8791132148106));
#32758=CARTESIAN_POINT('Ctrl Pts',(-12.9170923761371,-33.2732243688142,
17.8807520415042));
#32759=CARTESIAN_POINT('Ctrl Pts',(-12.9446665028586,-33.3206922763181,
17.8839589219604));
#32760=CARTESIAN_POINT('Ctrl Pts',(-12.9579599999856,-33.3442198382113,
17.8855274906737));
#32761=CARTESIAN_POINT('Ctrl Pts',(-12.9867520348804,-33.3966311670291,
17.8889770496842));
#32762=CARTESIAN_POINT('Ctrl Pts',(-13.0021159329327,-33.4255860253796,
17.8908532632633));
#32763=CARTESIAN_POINT('Ctrl Pts',(-13.054485713031,-33.5278372263349,17.8973810303638));
#32764=CARTESIAN_POINT('Ctrl Pts',(-13.0892479075963,-33.6022536010355,
17.9019570521331));
#32765=CARTESIAN_POINT('Ctrl Pts',(-13.1415533580126,-33.7257353107587,
17.9093181297542));
#32766=CARTESIAN_POINT('Ctrl Pts',(-13.1607152904065,-33.7740389631084,
17.9121418218122));
#32767=CARTESIAN_POINT('Ctrl Pts',(-13.1787500647504,-33.822734911607,17.9149431671188));
#32768=CARTESIAN_POINT('Origin',(-10.,-35.,23.));
#32769=CARTESIAN_POINT('',(-13.1787501240201,-33.8227350716418,19.1603160842799));
#32770=CARTESIAN_POINT('',(-13.1787501466517,-33.8227351327498,18.8205587414464));
#32771=CARTESIAN_POINT('',(-13.1787501240207,-33.8227350716434,23.));
#32772=CARTESIAN_POINT('',(-13.3897489495918,-34.9973314346088,17.6410178032058));
#32773=CARTESIAN_POINT('Ctrl Pts',(-13.1787501466517,-33.8227351327498,
18.8205587414464));
#32774=CARTESIAN_POINT('Ctrl Pts',(-13.1278271796848,-33.6852372822515,
18.8127838077241));
#32775=CARTESIAN_POINT('Ctrl Pts',(-13.0680253938338,-33.5511580716046,
18.8050413658075));
#32776=CARTESIAN_POINT('Ctrl Pts',(-12.9630852026426,-33.351753700127,18.7927313675143));
#32777=CARTESIAN_POINT('Ctrl Pts',(-12.9240518693691,-33.2834602661968,
18.7883601853884));
#32778=CARTESIAN_POINT('Ctrl Pts',(-12.8696313405074,-33.1954955301696,
18.7824417043482));
#32779=CARTESIAN_POINT('Ctrl Pts',(-12.856349561064,-33.1745445718325,18.7810097829634));
#32780=CARTESIAN_POINT('Ctrl Pts',(-12.8350989407793,-33.1418231972354,
18.778735021485));
#32781=CARTESIAN_POINT('Ctrl Pts',(-12.8272836961893,-33.129953498025,18.777901784375));
#32782=CARTESIAN_POINT('Ctrl Pts',(-12.8107581297681,-33.1051950537516,
18.7761460391324));
#32783=CARTESIAN_POINT('Ctrl Pts',(-12.8020333898203,-33.0923166144302,
18.7752225204624));
#32784=CARTESIAN_POINT('Ctrl Pts',(-12.7797669685693,-33.0599318206986,
18.7728750921918));
#32785=CARTESIAN_POINT('Ctrl Pts',(-12.7661085176199,-33.0405070709123,
18.7714438298795));
#32786=CARTESIAN_POINT('Ctrl Pts',(-12.7084889622472,-32.9603647996441,
18.7654467896085));
#32787=CARTESIAN_POINT('Ctrl Pts',(-12.6627265461189,-32.9009740531532,
18.7607807708712));
#32788=CARTESIAN_POINT('Ctrl Pts',(-12.5210053560613,-32.7291462777544,
18.7467189387252));
#32789=CARTESIAN_POINT('Ctrl Pts',(-12.4196220096114,-32.6214139919694,
18.7371537613859));
#32790=CARTESIAN_POINT('Ctrl Pts',(-12.161386459057,-32.3806575304665,18.7144213291779));
#32791=CARTESIAN_POINT('Ctrl Pts',(-11.9988122774959,-32.2545824963507,
18.7013678505348));
#32792=CARTESIAN_POINT('Ctrl Pts',(-11.7811823494712,-32.1154550106523,
18.6856404447628));
#32793=CARTESIAN_POINT('Ctrl Pts',(-11.7358926817733,-32.0879753730936,
18.6824518638282));
#32794=CARTESIAN_POINT('Ctrl Pts',(-11.663607711314,-32.0464022467577,18.6774915253318));
#32795=CARTESIAN_POINT('Ctrl Pts',(-11.637036245979,-32.0315925608539,18.675694715312));
#32796=CARTESIAN_POINT('Ctrl Pts',(-11.5869891390892,-32.0045750904019,
18.6723586935983));
#32797=CARTESIAN_POINT('Ctrl Pts',(-11.5635631207946,-31.9922807075084,
18.6708165433615));
#32798=CARTESIAN_POINT('Ctrl Pts',(-11.5105247638211,-31.9652324017662,
18.6673671587087));
#32799=CARTESIAN_POINT('Ctrl Pts',(-11.4808353161526,-31.9506350965688,
18.6654654149995));
#32800=CARTESIAN_POINT('Ctrl Pts',(-11.3890990613947,-31.9071872962696,
18.6596740261626));
#32801=CARTESIAN_POINT('Ctrl Pts',(-11.3263868349768,-31.8797779793758,
18.6558326136647));
#32802=CARTESIAN_POINT('Ctrl Pts',(-11.1754896755044,-31.8191985269537,
18.6468276740873));
#32803=CARTESIAN_POINT('Ctrl Pts',(-11.0866668015975,-31.7877685571224,
18.6417153030131));
#32804=CARTESIAN_POINT('Ctrl Pts',(-10.7881320092118,-31.6959350202277,
18.6249532813954));
#32805=CARTESIAN_POINT('Ctrl Pts',(-10.5739249964252,-31.6520753753334,
18.613625428358));
#32806=CARTESIAN_POINT('Ctrl Pts',(-10.26961590203,-31.6198470445316,18.5969872147209));
#32807=CARTESIAN_POINT('Ctrl Pts',(-10.1819112909128,-31.6139945922539,
18.5921246758359));
#32808=CARTESIAN_POINT('Ctrl Pts',(-10.0684446739674,-31.6108440048291,
18.5856377460135));
#32809=CARTESIAN_POINT('Ctrl Pts',(-10.0427971848497,-31.6104231311858,
18.5841585211107));
#32810=CARTESIAN_POINT('Ctrl Pts',(-10.001196762476,-31.6102126783775,18.5817347061495));
#32811=CARTESIAN_POINT('Ctrl Pts',(-9.98524528787591,-31.6102445820032,
18.5807994637303));
#32812=CARTESIAN_POINT('Ctrl Pts',(-9.95354951481549,-31.6105317002119,
18.5789284808173));
#32813=CARTESIAN_POINT('Ctrl Pts',(-9.93780564695028,-31.6107840377502,
18.5779929044681));
#32814=CARTESIAN_POINT('Ctrl Pts',(-9.8973398152633,-31.6117146543137,18.575573209462));
#32815=CARTESIAN_POINT('Ctrl Pts',(-9.87262284234043,-31.6125538116422,
18.5740808191472));
#32816=CARTESIAN_POINT('Ctrl Pts',(-9.7625826134207,-31.6174957686995,18.56737896883));
#32817=CARTESIAN_POINT('Ctrl Pts',(-9.67742886540143,-31.6245522551736,
18.5620387286689));
#32818=CARTESIAN_POINT('Ctrl Pts',(-9.40238391878068,-31.6578468389858,
18.5444696605795));
#32819=CARTESIAN_POINT('Ctrl Pts',(-9.21442544796143,-31.696970124836,18.5319858923283));
#32820=CARTESIAN_POINT('Ctrl Pts',(-8.87115991819229,-31.7993950796104,
18.5090954006666));
#32821=CARTESIAN_POINT('Ctrl Pts',(-8.71525221256635,-31.8587283404383,
18.4986581401984));
#32822=CARTESIAN_POINT('Ctrl Pts',(-8.52413059969507,-31.9480853491866,
18.4859064923559));
#32823=CARTESIAN_POINT('Ctrl Pts',(-8.48431059322875,-31.9676643614449,
18.4832510396663));
#32824=CARTESIAN_POINT('Ctrl Pts',(-8.41970955662775,-32.0010185171241,
18.4789434730602));
#32825=CARTESIAN_POINT('Ctrl Pts',(-8.39469755452233,-32.0143322436214,
18.4772757746419));
#32826=CARTESIAN_POINT('Ctrl Pts',(-8.34619330226916,-32.0409365044549,
18.4740408938562));
#32827=CARTESIAN_POINT('Ctrl Pts',(-8.32268711817533,-32.0541970666111,
18.4724728198936));
#32828=CARTESIAN_POINT('Ctrl Pts',(-8.26703283162491,-32.0864755335199,
18.4687578621645));
#32829=CARTESIAN_POINT('Ctrl Pts',(-8.23503541868252,-32.1057470382195,
18.4666201622408));
#32830=CARTESIAN_POINT('Ctrl Pts',(-8.12182354356072,-32.1765085121722,
18.4590427891796));
#32831=CARTESIAN_POINT('Ctrl Pts',(-8.04248633201922,-32.2309219177966,
18.4537082799207));
#32832=CARTESIAN_POINT('Ctrl Pts',(-7.83825290124936,-32.3841658422554,
18.4397773625463));
#32833=CARTESIAN_POINT('Ctrl Pts',(-7.71782266634565,-32.4885445099542,
18.4313585204422));
#32834=CARTESIAN_POINT('Ctrl Pts',(-7.4742422944954,-32.7317015465711,18.4131103908508));
#32835=CARTESIAN_POINT('Ctrl Pts',(-7.35424700723463,-32.87288774716,18.4033037390942));
#32836=CARTESIAN_POINT('Ctrl Pts',(-7.22611945710972,-33.0513597652028,
18.3908923618807));
#32837=CARTESIAN_POINT('Ctrl Pts',(-7.20629453394378,-33.0798902103678,
18.388907466408));
#32838=CARTESIAN_POINT('Ctrl Pts',(-7.17683217255581,-33.1237124707789,
18.3858493179413));
#32839=CARTESIAN_POINT('Ctrl Pts',(-7.166872199568,-33.1387857971824,18.3847957682614));
#32840=CARTESIAN_POINT('Ctrl Pts',(-7.14890008985113,-33.1664631434829,
18.3828568725705));
#32841=CARTESIAN_POINT('Ctrl Pts',(-7.14085007775999,-33.1790415167915,
18.3819739705732));
#32842=CARTESIAN_POINT('Ctrl Pts',(-7.12235598055536,-33.2083640464982,
18.3799118918268));
#32843=CARTESIAN_POINT('Ctrl Pts',(-7.11197474349381,-33.225146606345,18.3787289008106));
#32844=CARTESIAN_POINT('Ctrl Pts',(-7.07842552556662,-33.2804568130526,
18.3748235298702));
#32845=CARTESIAN_POINT('Ctrl Pts',(-7.05587829782229,-33.3193533471446,
18.372066755563));
#32846=CARTESIAN_POINT('Ctrl Pts',(-7.00207386331143,-33.4165789693409,
18.3651716934198));
#32847=CARTESIAN_POINT('Ctrl Pts',(-6.97173886628657,-33.4753961479894,
18.3609969811496));
#32848=CARTESIAN_POINT('Ctrl Pts',(-6.82654717612096,-33.7783640672862,
18.3396011187023));
#32849=CARTESIAN_POINT('Ctrl Pts',(-6.73939664834711,-34.0347579820041,
18.3219444666333));
#32850=CARTESIAN_POINT('Ctrl Pts',(-6.66497278660186,-34.3867439103519,
18.2995451818813));
#32851=CARTESIAN_POINT('Ctrl Pts',(-6.64987894258677,-34.4754233464817,
18.2940398668148));
#32852=CARTESIAN_POINT('Ctrl Pts',(-6.63352859880435,-34.601663725078,18.286398292647));
#32853=CARTESIAN_POINT('Ctrl Pts',(-6.62934178848976,-34.6388007865018,
18.2841738239773));
#32854=CARTESIAN_POINT('Ctrl Pts',(-6.62318771767488,-34.7028911956753,
18.2803738919918));
#32855=CARTESIAN_POINT('Ctrl Pts',(-6.62092713086152,-34.7298122142041,
18.2787895410305));
#32856=CARTESIAN_POINT('Ctrl Pts',(-6.61695247586294,-34.785059057254,18.2755613450546));
#32857=CARTESIAN_POINT('Ctrl Pts',(-6.61527177715232,-34.8133851881557,
18.273918648314));
#32858=CARTESIAN_POINT('Ctrl Pts',(-6.61187090757798,-34.8861437963664,
18.2697293008994));
#32859=CARTESIAN_POINT('Ctrl Pts',(-6.61066890199132,-34.9305957643352,
18.2671986266567));
#32860=CARTESIAN_POINT('Ctrl Pts',(-6.6089920360372,-35.1585030551804,18.2543525370803));
#32861=CARTESIAN_POINT('Ctrl Pts',(-6.62253531671405,-35.3417609369562,
18.2444724383207));
#32862=CARTESIAN_POINT('Ctrl Pts',(-6.6795570276113,-35.7068858323845,18.2248183471407));
#32863=CARTESIAN_POINT('Ctrl Pts',(-6.72335585861298,-35.8880452831363,
18.215077091432));
#32864=CARTESIAN_POINT('Ctrl Pts',(-6.8051404964262,-36.1352546474058,18.2008170043095));
#32865=CARTESIAN_POINT('Ctrl Pts',(-6.83080086226466,-36.2050334632,18.1966764071039));
#32866=CARTESIAN_POINT('Ctrl Pts',(-6.86789828736187,-36.296510253193,18.191024706514));
#32867=CARTESIAN_POINT('Ctrl Pts',(-6.87730805220173,-36.3190128509112,
18.1896160472342));
#32868=CARTESIAN_POINT('Ctrl Pts',(-6.89255644117843,-36.354400098528,18.1873687046291));
#32869=CARTESIAN_POINT('Ctrl Pts',(-6.89823447317542,-36.3673535383788,
18.1865392029941));
#32870=CARTESIAN_POINT('Ctrl Pts',(-6.9103819001591,-36.394600738888,18.1847790829892));
#32871=CARTESIAN_POINT('Ctrl Pts',(-6.91686974382693,-36.4088857369226,
18.1838473230294));
#32872=CARTESIAN_POINT('Ctrl Pts',(-6.93364271801762,-36.4451459355761,
18.1814602314316));
#32873=CARTESIAN_POINT('Ctrl Pts',(-6.94406492355331,-36.4670564034257,
18.1799971218698));
#32874=CARTESIAN_POINT('Ctrl Pts',(-6.98974975120966,-36.560499542065,18.1736740466874));
#32875=CARTESIAN_POINT('Ctrl Pts',(-7.0272934993271,-36.6308830568857,18.1687008904929));
#32876=CARTESIAN_POINT('Ctrl Pts',(-7.15070409073578,-36.8437983042673,
18.1531361019726));
#32877=CARTESIAN_POINT('Ctrl Pts',(-7.24460716391243,-36.9813853731174,
18.1423405209087));
#32878=CARTESIAN_POINT('Ctrl Pts',(-7.45995554359306,-37.2518324796645,
18.120148132963));
#32879=CARTESIAN_POINT('Ctrl Pts',(-7.58265348968885,-37.3830706828012,
18.1088100265218));
#32880=CARTESIAN_POINT('Ctrl Pts',(-7.75439721099543,-37.5397819128541,
18.0946538037738));
#32881=CARTESIAN_POINT('Ctrl Pts',(-7.79445456941998,-37.5746444180604,
18.0914574223302));
#32882=CARTESIAN_POINT('Ctrl Pts',(-7.85876832258284,-37.6280145971421,
18.0864859461972));
#32883=CARTESIAN_POINT('Ctrl Pts',(-7.88248242294936,-37.6471594626543,
18.0846857165856));
#32884=CARTESIAN_POINT('Ctrl Pts',(-7.92729346366907,-37.6823487651706,
18.0813436725575));
#32885=CARTESIAN_POINT('Ctrl Pts',(-7.94832646812252,-37.6984705040206,
18.0797989098084));
#32886=CARTESIAN_POINT('Ctrl Pts',(-7.99607813897189,-37.7341909293101,
18.0763439285654));
#32887=CARTESIAN_POINT('Ctrl Pts',(-8.02289966232174,-37.7536479855994,
18.0744392084099));
#32888=CARTESIAN_POINT('Ctrl Pts',(-8.10605431856967,-37.8121291796384,
18.0686389853354));
#32889=CARTESIAN_POINT('Ctrl Pts',(-8.16329055996146,-37.8498421139435,
18.0647918084539));
#32890=CARTESIAN_POINT('Ctrl Pts',(-8.301926517572,-37.9352762695603,18.0557735704154));
#32891=CARTESIAN_POINT('Ctrl Pts',(-8.38425282610886,-37.9813860867071,
18.0506537823879));
#32892=CARTESIAN_POINT('Ctrl Pts',(-8.6635497587908,-38.1228447160072,18.0338528189895));
#32893=CARTESIAN_POINT('Ctrl Pts',(-8.86779853617199,-38.2025567598758,
18.022495284381));
#32894=CARTESIAN_POINT('Ctrl Pts',(-9.16245346482691,-38.2858133747848,
18.0058434992633));
#32895=CARTESIAN_POINT('Ctrl Pts',(-9.24749747447466,-38.3063259537656,
18.0010028974775));
#32896=CARTESIAN_POINT('Ctrl Pts',(-9.35832415173827,-38.32856006576,17.9945425827067));
#32897=CARTESIAN_POINT('Ctrl Pts',(-9.38347143557366,-38.3333095342386,
17.9930666638767));
#32898=CARTESIAN_POINT('Ctrl Pts',(-9.4243652360559,-38.3405544116143,17.9906468381062));
#32899=CARTESIAN_POINT('Ctrl Pts',(-9.44008027195994,-38.3432243469305,
17.9897122181947));
#32900=CARTESIAN_POINT('Ctrl Pts',(-9.47126875699553,-38.3482971087787,
17.9878469954287));
#32901=CARTESIAN_POINT('Ctrl Pts',(-9.48674103188765,-38.350703725545,17.9869165919148));
#32902=CARTESIAN_POINT('Ctrl Pts',(-9.52655937792873,-38.3566149698747,
17.984510053648));
#32903=CARTESIAN_POINT('Ctrl Pts',(-9.5509276317461,-38.3599619059399,17.9830256788122));
#32904=CARTESIAN_POINT('Ctrl Pts',(-9.65953938558319,-38.3736769313171,
17.976364511486));
#32905=CARTESIAN_POINT('Ctrl Pts',(-9.74411280584278,-38.3811431427272,
17.9710575386435));
#32906=CARTESIAN_POINT('Ctrl Pts',(-10.0176372067226,-38.3949695261054,
17.9536853377977));
#32907=CARTESIAN_POINT('Ctrl Pts',(-10.2068697736873,-38.3887069160527,
17.9413671592005));
#32908=CARTESIAN_POINT('Ctrl Pts',(-10.564789248577,-38.3467569961094,17.9183047714037));
#32909=CARTESIAN_POINT('Ctrl Pts',(-10.7332443929623,-38.3139305723157,
17.9075520350472));
#32910=CARTESIAN_POINT('Ctrl Pts',(-10.941327119456,-38.2567283914272,17.8945066813705));
#32911=CARTESIAN_POINT('Ctrl Pts',(-10.9839064843871,-38.2441185048608,
17.8918488944142));
#32912=CARTESIAN_POINT('Ctrl Pts',(-11.0531433294776,-38.2221253479804,
17.8875445302911));
#32913=CARTESIAN_POINT('Ctrl Pts',(-11.0799519537448,-38.2132392504568,
17.8858821730731));
#32914=CARTESIAN_POINT('Ctrl Pts',(-11.1319910531298,-38.1952652886215,
17.8826627483972));
#32915=CARTESIAN_POINT('Ctrl Pts',(-11.1572308448781,-38.1862110478725,
17.8811047254976));
#32916=CARTESIAN_POINT('Ctrl Pts',(-11.2169974784316,-38.1639671388135,
17.8774222671109));
#32917=CARTESIAN_POINT('Ctrl Pts',(-11.2514216383299,-38.1505102687802,
17.8753067864029));
#32918=CARTESIAN_POINT('Ctrl Pts',(-11.37266383406,-38.1008141957698,17.8678688735315));
#32919=CARTESIAN_POINT('Ctrl Pts',(-11.4581892171857,-38.0615259219255,
17.862647119791));
#32920=CARTESIAN_POINT('Ctrl Pts',(-11.6786908915289,-37.948893036407,17.8491294299995));
#32921=CARTESIAN_POINT('Ctrl Pts',(-11.8105097499169,-37.8698485908608,
17.8409977537255));
#32922=CARTESIAN_POINT('Ctrl Pts',(-12.0954276728645,-37.6715302788106,
17.8226034464986));
#32923=CARTESIAN_POINT('Ctrl Pts',(-12.2445504355825,-37.5475219854541,
17.8123746483425));
#32924=CARTESIAN_POINT('Ctrl Pts',(-12.4071665466224,-37.3868766637562,
17.7994609296924));
#32925=CARTESIAN_POINT('Ctrl Pts',(-12.4316913777557,-37.3618864987385,
17.7974601089233));
#32926=CARTESIAN_POINT('Ctrl Pts',(-12.468134756586,-37.3235823382524,17.7943969570222));
#32927=CARTESIAN_POINT('Ctrl Pts',(-12.4803430552487,-37.3105459001232,
17.7933550618218));
#32928=CARTESIAN_POINT('Ctrl Pts',(-12.5025788884134,-37.2864224081972,
17.7914268454443));
#32929=CARTESIAN_POINT('Ctrl Pts',(-12.5126369302576,-37.2753646186839,
17.7905427873545));
#32930=CARTESIAN_POINT('Ctrl Pts',(-12.5359491360268,-37.2493921740165,
17.7884661795447));
#32931=CARTESIAN_POINT('Ctrl Pts',(-12.5491451686072,-37.2344265572653,
17.7872696071724));
#32932=CARTESIAN_POINT('Ctrl Pts',(-12.5923860692065,-37.1845054573929,
17.7832806932646));
#32933=CARTESIAN_POINT('Ctrl Pts',(-12.6218488895095,-37.1490550445159,
17.7804521145876));
#32934=CARTESIAN_POINT('Ctrl Pts',(-12.693263742535,-37.0594719215604,17.7733368634722));
#32935=CARTESIAN_POINT('Ctrl Pts',(-12.7343149033388,-37.0046484076015,
17.7690110799991));
#32936=CARTESIAN_POINT('Ctrl Pts',(-12.924817613039,-36.7334862321096,17.7478820424465));
#32937=CARTESIAN_POINT('Ctrl Pts',(-13.0504372340232,-36.5014631297012,
17.7306880273113));
#32938=CARTESIAN_POINT('Ctrl Pts',(-13.1824802009045,-36.1708462768496,
17.7084873475608));
#32939=CARTESIAN_POINT('Ctrl Pts',(-13.2134182675029,-36.0830543445701,
17.7027833940108));
#32940=CARTESIAN_POINT('Ctrl Pts',(-13.2518542173537,-35.9577546765959,
17.6949101000677));
#32941=CARTESIAN_POINT('Ctrl Pts',(-13.2623896988519,-35.9212293417552,
17.6926460526183));
#32942=CARTESIAN_POINT('Ctrl Pts',(-13.2793418861227,-35.8585151524786,
17.6888099965516));
#32943=CARTESIAN_POINT('Ctrl Pts',(-13.2860644253252,-35.8324134357044,
17.6872284409606));
#32944=CARTESIAN_POINT('Ctrl Pts',(-13.2992080677314,-35.7787377920279,
17.6840058317488));
#32945=CARTESIAN_POINT('Ctrl Pts',(-13.305596490129,-35.7511579978445,17.6823659162278));
#32946=CARTESIAN_POINT('Ctrl Pts',(-13.3177838770018,-35.6953733685506,
17.6790795065311));
#32947=CARTESIAN_POINT('Ctrl Pts',(-13.3235704614071,-35.6671682210812,
17.6774335128797));
#32948=CARTESIAN_POINT('Ctrl Pts',(-13.3368339124911,-35.5980579803883,
17.6734362028842));
#32949=CARTESIAN_POINT('Ctrl Pts',(-13.3439189242645,-35.5570819803451,
17.6710966870807));
#32950=CARTESIAN_POINT('Ctrl Pts',(-13.3766779417949,-35.344380267151,17.6590918149364));
#32951=CARTESIAN_POINT('Ctrl Pts',(-13.3898844254065,-35.1709939538293,
17.6497907008939));
#32952=CARTESIAN_POINT('Ctrl Pts',(-13.3897489685498,-34.9973556256544,
17.6405626171251));
#32953=CARTESIAN_POINT('Ctrl Pts',(-13.3897489495918,-34.9973314346088,
17.6410178032058));
#32954=CARTESIAN_POINT('Ctrl Pts',(-13.3896451068354,-34.8654250268716,
17.6332792606915));
#32955=CARTESIAN_POINT('Ctrl Pts',(-13.381838229504,-34.7338444491851,17.6255407181773));
#32956=CARTESIAN_POINT('Ctrl Pts',(-13.3664638492093,-34.6033563129622,
17.617802175663));
#32957=CARTESIAN_POINT('Ctrl Pts',(-13.3507856217542,-34.4702893118427,
17.6099106946808));
#32958=CARTESIAN_POINT('Ctrl Pts',(-13.3272378167578,-34.338358106954,17.6020192136986));
#32959=CARTESIAN_POINT('Ctrl Pts',(-13.2960126784577,-34.2083526757789,
17.5941277327164));
#32960=CARTESIAN_POINT('Ctrl Pts',(-13.2922017700226,-34.1924860112503,
17.5931646077127));
#32961=CARTESIAN_POINT('Ctrl Pts',(-13.2882765642279,-34.1766480068593,
17.5922014827091));
#32962=CARTESIAN_POINT('Ctrl Pts',(-13.2842374593052,-34.1608400787715,
17.5912383577054));
#32963=CARTESIAN_POINT('Ctrl Pts',(-13.258626776551,-34.0606070224349,17.5851314876452));
#32964=CARTESIAN_POINT('Ctrl Pts',(-13.2283809689128,-33.9613816652927,
17.579024617585));
#32965=CARTESIAN_POINT('Ctrl Pts',(-13.1935957197208,-33.8636235476387,
17.5729177475248));
#32966=CARTESIAN_POINT('Ctrl Pts',(-13.1887356065883,-33.8499650135632,
17.5720645100156));
#32967=CARTESIAN_POINT('Ctrl Pts',(-13.1837869610759,-33.8363351084987,
17.5712112725064));
#32968=CARTESIAN_POINT('Ctrl Pts',(-13.1787501240207,-33.8227350716434,
17.5703580349972));
#32969=CARTESIAN_POINT('Ctrl Pts',(-13.1787500647504,-33.822734911607,17.9149431671188));
#32970=CARTESIAN_POINT('Ctrl Pts',(-13.2574736629433,-34.0352976090998,
17.9271713202471));
#32971=CARTESIAN_POINT('Ctrl Pts',(-13.3147214038581,-34.2553371507137,
17.9389318292027));
#32972=CARTESIAN_POINT('Ctrl Pts',(-13.3598256104917,-34.54563607905,17.9548343611894));
#32973=CARTESIAN_POINT('Ctrl Pts',(-13.3681327220865,-34.6119848253376,
17.9584977817604));
#32974=CARTESIAN_POINT('Ctrl Pts',(-13.3787671453846,-34.7236151964397,
17.9647713098526));
#32975=CARTESIAN_POINT('Ctrl Pts',(-13.3821578507305,-34.7687774939372,
17.9673394228452));
#32976=CARTESIAN_POINT('Ctrl Pts',(-13.3857286033999,-34.8337516451611,
17.9710941787719));
#32977=CARTESIAN_POINT('Ctrl Pts',(-13.3866414449915,-34.8535200578378,
17.9722445405624));
#32978=CARTESIAN_POINT('Ctrl Pts',(-13.3879395062227,-34.8882228830459,
17.9742796982406));
#32979=CARTESIAN_POINT('Ctrl Pts',(-13.3883991777765,-34.9031536159209,
17.9751604929724));
#32980=CARTESIAN_POINT('Ctrl Pts',(-13.3891957335569,-34.9361074688981,
17.9771163142488));
#32981=CARTESIAN_POINT('Ctrl Pts',(-13.389487559345,-34.9541303058339,17.9781936029256));
#32982=CARTESIAN_POINT('Ctrl Pts',(-13.3899283133611,-35.0077826861086,
17.9814215909546));
#32983=CARTESIAN_POINT('Ctrl Pts',(-13.3896592322845,-35.043412119444,17.9835927777448));
#32984=CARTESIAN_POINT('Ctrl Pts',(-13.384777880587,-35.252728184127,17.9964846924534));
#32985=CARTESIAN_POINT('Ctrl Pts',(-13.3673786748111,-35.4258458803741,
18.0076865605367));
#32986=CARTESIAN_POINT('Ctrl Pts',(-13.307491412664,-35.7606544881738,18.0296124871599));
#32987=CARTESIAN_POINT('Ctrl Pts',(-13.2661681023012,-35.9220894308829,
18.0403063602688));
#32988=CARTESIAN_POINT('Ctrl Pts',(-13.1817368252688,-36.173320122958,18.0568624955752));
#32989=CARTESIAN_POINT('Ctrl Pts',(-13.1462568947524,-36.2653852359981,
18.0629138888606));
#32990=CARTESIAN_POINT('Ctrl Pts',(-13.0917431188089,-36.3903052130589,
18.0710985399781));
#32991=CARTESIAN_POINT('Ctrl Pts',(-13.0761015147676,-36.4245784432275,
18.0733415370835));
#32992=CARTESIAN_POINT('Ctrl Pts',(-13.0482555855393,-36.4829950076799,
18.0771615828884));
#32993=CARTESIAN_POINT('Ctrl Pts',(-13.0363278852742,-36.5072655186889,
18.0787478132954));
#32994=CARTESIAN_POINT('Ctrl Pts',(-13.0113552853821,-36.5565800938483,
18.0819699714671));
#32995=CARTESIAN_POINT('Ctrl Pts',(-12.9982853213871,-36.581609131581,18.0836048782435));
#32996=CARTESIAN_POINT('Ctrl Pts',(-12.9641062008404,-36.6451155957622,
18.0877537861169));
#32997=CARTESIAN_POINT('Ctrl Pts',(-12.9425594472246,-36.6833523224569,
18.0902523715505));
#32998=CARTESIAN_POINT('Ctrl Pts',(-12.8419742782966,-36.8540140932111,
18.1014226665075));
#32999=CARTESIAN_POINT('Ctrl Pts',(-12.7546946868513,-36.9813758409625,
18.1097989087319));
#33000=CARTESIAN_POINT('Ctrl Pts',(-12.6379670212617,-37.1290113202829,
18.1198578482986));
#33001=CARTESIAN_POINT('Ctrl Pts',(-12.6164971619536,-37.1553426282019,
18.1216670540787));
#33002=CARTESIAN_POINT('Ctrl Pts',(-12.4712559637912,-37.3281018902216,
18.1336623432424));
#33003=CARTESIAN_POINT('Ctrl Pts',(-12.335657144121,-37.4641145648641,18.143694985248));
#33004=CARTESIAN_POINT('Ctrl Pts',(-12.1380088740832,-37.6313184438488,
18.1579324884406));
#33005=CARTESIAN_POINT('Ctrl Pts',(-12.0854417220138,-37.6731723370791,
18.1616886154957));
#33006=CARTESIAN_POINT('Ctrl Pts',(-12.0128229667522,-37.7275452489114,
18.1668889927681));
#33007=CARTESIAN_POINT('Ctrl Pts',(-11.9938305113286,-37.7414593204963,
18.1682501142065));
#33008=CARTESIAN_POINT('Ctrl Pts',(-11.9633409847396,-37.7633118506042,
18.1704394914702));
#33009=CARTESIAN_POINT('Ctrl Pts',(-11.9519367615474,-37.7713792720609,
18.171259344059));
#33010=CARTESIAN_POINT('Ctrl Pts',(-11.9275144520872,-37.7884302522046,
18.1730178204206));
#33011=CARTESIAN_POINT('Ctrl Pts',(-11.9144827582823,-37.7973936047479,
18.1739577879707));
#33012=CARTESIAN_POINT('Ctrl Pts',(-11.8806732143477,-37.8203013107773,
18.176399679444));
#33013=CARTESIAN_POINT('Ctrl Pts',(-11.8598031859927,-37.8341071348051,
18.1779101307904));
#33014=CARTESIAN_POINT('Ctrl Pts',(-11.7642922454333,-37.8957797503511,
18.1848298470815));
#33015=CARTESIAN_POINT('Ctrl Pts',(-11.6879485776571,-37.9409343059859,
18.1903799206523));
#33016=CARTESIAN_POINT('Ctrl Pts',(-11.4265037944314,-38.0820345128476,
18.2092412651861));
#33017=CARTESIAN_POINT('Ctrl Pts',(-11.2343381561607,-38.1639000220664,
18.2228388566312));
#33018=CARTESIAN_POINT('Ctrl Pts',(-10.895315268362,-38.2727060105552,18.2454863242625));
#33019=CARTESIAN_POINT('Ctrl Pts',(-10.751956360791,-38.3085895427248,18.2546898537724));
#33020=CARTESIAN_POINT('Ctrl Pts',(-10.5638877520947,-38.3428025811365,
18.2662342924794));
#33021=CARTESIAN_POINT('Ctrl Pts',(-10.5209294173895,-38.3497658574244,
18.2688370541273));
#33022=CARTESIAN_POINT('Ctrl Pts',(-10.4499501385651,-38.3598726121073,
18.2730831189388));
#33023=CARTESIAN_POINT('Ctrl Pts',(-10.4220038630253,-38.3634969760628,
18.2747411051786));
#33024=CARTESIAN_POINT('Ctrl Pts',(-10.3670785386468,-38.3699249129996,
18.2779736614267));
#33025=CARTESIAN_POINT('Ctrl Pts',(-10.3401046693868,-38.3727539858738,
18.2795489050284));
#33026=CARTESIAN_POINT('Ctrl Pts',(-10.275258016893,-38.3787693559963,18.2833078970419));
#33027=CARTESIAN_POINT('Ctrl Pts',(-10.2373594976023,-38.3816430873576,
18.285481901486));
#33028=CARTESIAN_POINT('Ctrl Pts',(-10.0985283019247,-38.3898247199358,
18.2933699948383));
#33029=CARTESIAN_POINT('Ctrl Pts',(-9.99741648630631,-38.3912557102519,
18.2989667259291));
#33030=CARTESIAN_POINT('Ctrl Pts',(-9.63032288922031,-38.3800294606252,
18.3189619407942));
#33031=CARTESIAN_POINT('Ctrl Pts',(-9.36616538847495,-38.3405840724596,
18.332661166564));
#33032=CARTESIAN_POINT('Ctrl Pts',(-9.02426850672867,-38.2474804654496,
18.3519248469663));
#33033=CARTESIAN_POINT('Ctrl Pts',(-8.94012669182979,-38.2210010048482,
18.3568037818863));
#33034=CARTESIAN_POINT('Ctrl Pts',(-8.832912255196,-38.1826046598288,18.3633115135663));
#33035=CARTESIAN_POINT('Ctrl Pts',(-8.80880492608107,-38.1736604159552,
18.3647942356018));
#33036=CARTESIAN_POINT('Ctrl Pts',(-8.76989507419001,-38.1587184009094,
18.3672225731859));
#33037=CARTESIAN_POINT('Ctrl Pts',(-8.75502865536089,-38.1528885792252,
18.3681587857228));
#33038=CARTESIAN_POINT('Ctrl Pts',(-8.72558067395743,-38.1410998975053,
18.3700310598773));
#33039=CARTESIAN_POINT('Ctrl Pts',(-8.71099840431787,-38.1351440229613,
18.3709669474307));
#33040=CARTESIAN_POINT('Ctrl Pts',(-8.67364480995784,-38.1195829472141,
18.3733858808067));
#33041=CARTESIAN_POINT('Ctrl Pts',(-8.6509363965119,-38.1098300871039,18.3748771684393));
#33042=CARTESIAN_POINT('Ctrl Pts',(-8.5505332316712,-38.0654020824224,18.381556861461));
#33043=CARTESIAN_POINT('Ctrl Pts',(-8.47405861599768,-38.0280595242528,
18.3868748474453));
#33044=CARTESIAN_POINT('Ctrl Pts',(-8.23161809754652,-37.898158582785,18.4043133548527));
#33045=CARTESIAN_POINT('Ctrl Pts',(-8.07200105003478,-37.7945157955768,
18.4166851830328));
#33046=CARTESIAN_POINT('Ctrl Pts',(-7.7889267376143,-37.5748576077641,18.4395875901524));
#33047=CARTESIAN_POINT('Ctrl Pts',(-7.6638036435863,-37.4618969002117,18.4501384093483));
#33048=CARTESIAN_POINT('Ctrl Pts',(-7.51690801857805,-37.3079499707143,
18.4629997505395));
#33049=CARTESIAN_POINT('Ctrl Pts',(-7.48687169763568,-37.2752066438739,
18.4656588844473));
#33050=CARTESIAN_POINT('Ctrl Pts',(-7.43873051083282,-37.2206098095412,
18.4699716966451));
#33051=CARTESIAN_POINT('Ctrl Pts',(-7.42024165763747,-37.1991035197149,
18.4716409983953));
#33052=CARTESIAN_POINT('Ctrl Pts',(-7.3846780533992,-37.1566699912887,18.4748785611568));
#33053=CARTESIAN_POINT('Ctrl Pts',(-7.36757926060233,-37.1357657756271,
18.4764477199936));
#33054=CARTESIAN_POINT('Ctrl Pts',(-7.32742284928981,-37.0854573778795,
18.4801646435222));
#33055=CARTESIAN_POINT('Ctrl Pts',(-7.30459775569439,-37.055871591215,18.4823032285057));
#33056=CARTESIAN_POINT('Ctrl Pts',(-7.22480663496711,-36.9488329423689,
18.4898807817139));
#33057=CARTESIAN_POINT('Ctrl Pts',(-7.17064980608984,-36.8693388486506,
18.495214702772));
#33058=CARTESIAN_POINT('Ctrl Pts',(-7.03604808777771,-36.652483273502,18.5091409839819));
#33059=CARTESIAN_POINT('Ctrl Pts',(-6.96176965723963,-36.5115791388387,
18.5175561156818));
#33060=CARTESIAN_POINT('Ctrl Pts',(-6.82305328459711,-36.1965333013897,
18.5358082816679));
#33061=CARTESIAN_POINT('Ctrl Pts',(-6.7624614118829,-36.0212795028723,18.5456225529541));
#33062=CARTESIAN_POINT('Ctrl Pts',(-6.70785374268399,-35.8083225048791,
18.5580422966834));
#33063=CARTESIAN_POINT('Ctrl Pts',(-6.69974185301445,-35.774537422732,18.5600273869828));
#33064=CARTESIAN_POINT('Ctrl Pts',(-6.68820203150838,-35.7229978848826,
18.5630861173421));
#33065=CARTESIAN_POINT('Ctrl Pts',(-6.68439425470741,-35.7053298771089,
18.5641400686341));
#33066=CARTESIAN_POINT('Ctrl Pts',(-6.6776977075306,-35.6730049726649,18.566079585272));
#33067=CARTESIAN_POINT('Ctrl Pts',(-6.67476427489355,-35.6583582323194,
18.5669627045738));
#33068=CARTESIAN_POINT('Ctrl Pts',(-6.66817914558223,-35.6243112561122,
18.569025384291));
#33069=CARTESIAN_POINT('Ctrl Pts',(-6.66460001719369,-35.60489806064,18.5702087600021));
#33070=CARTESIAN_POINT('Ctrl Pts',(-6.65341850820725,-35.5411307161891,
18.5741171559401));
#33071=CARTESIAN_POINT('Ctrl Pts',(-6.64653007681595,-35.4966580252875,
18.5768766383884));
#33072=CARTESIAN_POINT('Ctrl Pts',(-6.63169189566488,-35.3863894336289,
18.5837805623838));
#33073=CARTESIAN_POINT('Ctrl Pts',(-6.62478263028336,-35.3204732486462,
18.587961534498));
#33074=CARTESIAN_POINT('Ctrl Pts',(-6.59944757504377,-34.983849319207,18.6094602550772));
#33075=CARTESIAN_POINT('Ctrl Pts',(-6.61164025555888,-34.7117881422173,
18.6272151811768));
#33076=CARTESIAN_POINT('Ctrl Pts',(-6.67065558785496,-34.3568047009002,
18.6496033405606));
#33077=CARTESIAN_POINT('Ctrl Pts',(-6.68857958873701,-34.2701154978643,
18.655017960122));
#33078=CARTESIAN_POINT('Ctrl Pts',(-6.71880925266393,-34.1481960826065,
18.6625563139971));
#33079=CARTESIAN_POINT('Ctrl Pts',(-6.7283328481143,-34.1123194010776,18.6647651953944));
#33080=CARTESIAN_POINT('Ctrl Pts',(-6.74578859275448,-34.0506633339324,
18.6685463835757));
#33081=CARTESIAN_POINT('Ctrl Pts',(-6.75344253429222,-34.0248094171066,
18.6701273667004));
#33082=CARTESIAN_POINT('Ctrl Pts',(-6.76980080030374,-33.9718819409708,
18.673355494956));
#33083=CARTESIAN_POINT('Ctrl Pts',(-6.77853899142676,-33.9448210318468,
18.6750014057077));
#33084=CARTESIAN_POINT('Ctrl Pts',(-6.80192063656046,-33.8754107135872,
18.6792131744246));
#33085=CARTESIAN_POINT('Ctrl Pts',(-6.81706535669886,-33.833235242997,18.681762680768));
#33086=CARTESIAN_POINT('Ctrl Pts',(-6.9019704603064,-33.6107593076599,18.695179582384));
#33087=CARTESIAN_POINT('Ctrl Pts',(-6.98622468615936,-33.4363676811077,
18.7055577256501));
#33088=CARTESIAN_POINT('Ctrl Pts',(-7.1886866603987,-33.095194185605,18.7266282824366));
#33089=CARTESIAN_POINT('Ctrl Pts',(-7.30799856086935,-32.9300042637491,
18.7372713487305));
#33090=CARTESIAN_POINT('Ctrl Pts',(-7.47612085504177,-32.7365415700979,
18.7515098503233));
#33091=CARTESIAN_POINT('Ctrl Pts',(-7.51179091238259,-32.6973873712854,
18.7544956269074));
#33092=CARTESIAN_POINT('Ctrl Pts',(-7.56323019788442,-32.6435149984917,
18.7587797369064));
#33093=CARTESIAN_POINT('Ctrl Pts',(-7.57824655962961,-32.6280854034999,
18.7600278961994));
#33094=CARTESIAN_POINT('Ctrl Pts',(-7.60407813739368,-32.6020439887711,
18.7621730236245));
#33095=CARTESIAN_POINT('Ctrl Pts',(-7.61481960187461,-32.5913594983349,
18.7630644850142));
#33096=CARTESIAN_POINT('Ctrl Pts',(-7.63777718931109,-32.5688278497078,
18.7649693705438));
#33097=CARTESIAN_POINT('Ctrl Pts',(-7.65001126983398,-32.5570002921701,
18.7659840955195));
#33098=CARTESIAN_POINT('Ctrl Pts',(-7.68451809053389,-32.5241391253324,
18.7688437503801));
#33099=CARTESIAN_POINT('Ctrl Pts',(-7.70698713908062,-32.503315113735,18.7707030147454));
#33100=CARTESIAN_POINT('Ctrl Pts',(-7.75895290914514,-32.45644713967,18.7749904932201));
#33101=CARTESIAN_POINT('Ctrl Pts',(-7.78862684921236,-32.4306067331975,
18.7774297813377));
#33102=CARTESIAN_POINT('Ctrl Pts',(-7.89086491244491,-32.344659745318,18.7857851952846));
#33103=CARTESIAN_POINT('Ctrl Pts',(-7.9654802216647,-32.2870661386771,18.7918007486963));
#33104=CARTESIAN_POINT('Ctrl Pts',(-8.27333827740561,-32.0692885299454,
18.8160346946936));
#33105=CARTESIAN_POINT('Ctrl Pts',(-8.52387278761695,-31.9354396280636,
18.8343522476638));
#33106=CARTESIAN_POINT('Ctrl Pts',(-8.83698466013862,-31.8155793734949,
18.8547560357336));
#33107=CARTESIAN_POINT('Ctrl Pts',(-8.88624770630459,-31.7980169127796,
18.8579028433028));
#33108=CARTESIAN_POINT('Ctrl Pts',(-8.96463871014907,-31.7720984692396,
18.8628130766327));
#33109=CARTESIAN_POINT('Ctrl Pts',(-8.99350455856831,-31.7629815712283,
18.8646007410966));
#33110=CARTESIAN_POINT('Ctrl Pts',(-9.0475873805674,-31.7466936343888,18.8679131964173));
#33111=CARTESIAN_POINT('Ctrl Pts',(-9.07277271641578,-31.7394261658924,
18.8694409808716));
#33112=CARTESIAN_POINT('Ctrl Pts',(-9.12999083630758,-31.7236319293576,
18.872879752454));
#33113=CARTESIAN_POINT('Ctrl Pts',(-9.16206972925407,-31.7152813436048,
18.8747850187413));
#33114=CARTESIAN_POINT('Ctrl Pts',(-9.26110465546569,-31.6910464568305,
18.8806016352486));
#33115=CARTESIAN_POINT('Ctrl Pts',(-9.32842784161424,-31.6767287799142,
18.8844640931337));
#33116=CARTESIAN_POINT('Ctrl Pts',(-9.48956637990019,-31.6475566437947,
18.8935307373691));
#33117=CARTESIAN_POINT('Ctrl Pts',(-9.58366231910807,-31.634575287889,18.8986827212484));
#33118=CARTESIAN_POINT('Ctrl Pts',(-9.81192811106071,-31.6128058270445,
18.9109842334276));
#33119=CARTESIAN_POINT('Ctrl Pts',(-9.94631440408638,-31.6080133025493,
18.9180618170391));
#33120=CARTESIAN_POINT('Ctrl Pts',(-10.2452954378598,-31.6151269838291,
18.9339608201663));
#33121=CARTESIAN_POINT('Ctrl Pts',(-10.4094393189859,-31.6310412971696,
18.94279341346));
#33122=CARTESIAN_POINT('Ctrl Pts',(-10.5998792455353,-31.6636301120385,
18.9537924781046));
#33123=CARTESIAN_POINT('Ctrl Pts',(-10.6279396037921,-31.6687973824746,
18.9554327660765));
#33124=CARTESIAN_POINT('Ctrl Pts',(-10.6721884930077,-31.6775246727265,
18.9580551671047));
#33125=CARTESIAN_POINT('Ctrl Pts',(-10.6884224815881,-31.6808503902108,
18.9590249308205));
#33126=CARTESIAN_POINT('Ctrl Pts',(-10.7196327192991,-31.6874829773589,
18.9609052200413));
#33127=CARTESIAN_POINT('Ctrl Pts',(-10.7346119324671,-31.6907726656868,
18.9618148278932));
#33128=CARTESIAN_POINT('Ctrl Pts',(-10.7716311645891,-31.6991664348316,
18.9640798298665));
#33129=CARTESIAN_POINT('Ctrl Pts',(-10.7936432026019,-31.7043896945485,
18.9654415773468));
#33130=CARTESIAN_POINT('Ctrl Pts',(-10.8787282346104,-31.7254814510871,
18.970758983208));
#33131=CARTESIAN_POINT('Ctrl Pts',(-10.9413883522577,-31.7429427563722,
18.9747896425663));
#33132=CARTESIAN_POINT('Ctrl Pts',(-11.1138394929039,-31.796391066361,18.9861335968407));
#33133=CARTESIAN_POINT('Ctrl Pts',(-11.2223508278271,-31.8362040814966,
18.9935569811521));
#33134=CARTESIAN_POINT('Ctrl Pts',(-11.563625161657,-31.9816002236887,19.0174613192039));
#33135=CARTESIAN_POINT('Ctrl Pts',(-11.7866056809594,-32.1079867292141,
19.0338700050418));
#33136=CARTESIAN_POINT('Ctrl Pts',(-12.0342478586321,-32.2880255862164,
19.0524707901725));
#33137=CARTESIAN_POINT('Ctrl Pts',(-12.0745372071784,-32.3187194548577,
19.0555138727141));
#33138=CARTESIAN_POINT('Ctrl Pts',(-12.1372938188597,-32.3687914018689,
19.0602831952697));
#33139=CARTESIAN_POINT('Ctrl Pts',(-12.1602193550271,-32.3875804363166,
19.0620319406714));
#33140=CARTESIAN_POINT('Ctrl Pts',(-12.2032181771113,-32.4237740154303,
19.0653252976279));
#33141=CARTESIAN_POINT('Ctrl Pts',(-12.2233389244651,-32.4411184580734,
19.0668721369762));
#33142=CARTESIAN_POINT('Ctrl Pts',(-12.2689709539587,-32.4813986920384,
19.0703947754584));
#33143=CARTESIAN_POINT('Ctrl Pts',(-12.294342333644,-32.5044890068333,19.0723640439074));
#33144=CARTESIAN_POINT('Ctrl Pts',(-12.3744593674015,-32.5796578095867,
19.0786219805554));
#33145=CARTESIAN_POINT('Ctrl Pts',(-12.4278178244577,-32.6331845522344,
19.0828498272079));
#33146=CARTESIAN_POINT('Ctrl Pts',(-12.5534346986981,-32.7679201282267,
19.0930080478961));
#33147=CARTESIAN_POINT('Ctrl Pts',(-12.6236634372342,-32.8509067920648,
19.0988658796263));
#33148=CARTESIAN_POINT('Ctrl Pts',(-12.81405373795,-33.0991574364479,19.1155633335551));
#33149=CARTESIAN_POINT('Ctrl Pts',(-12.923416834321,-33.2720746587202,19.1262019620166));
#33150=CARTESIAN_POINT('Ctrl Pts',(-13.0523092494715,-33.5235316630535,
19.1416406721746));
#33151=CARTESIAN_POINT('Ctrl Pts',(-13.0856347582639,-33.5945083183905,
19.1459984642093));
#33152=CARTESIAN_POINT('Ctrl Pts',(-13.1262158566297,-33.6893537579689,
19.1519013883363));
#33153=CARTESIAN_POINT('Ctrl Pts',(-13.1357135010849,-33.7122422912396,
19.153331886331));
#33154=CARTESIAN_POINT('Ctrl Pts',(-13.1502593583121,-33.7484118745938,
19.1556048590737));
#33155=CARTESIAN_POINT('Ctrl Pts',(-13.155476662514,-33.761624500976,19.156437753559));
#33156=CARTESIAN_POINT('Ctrl Pts',(-13.1662316670458,-33.7893704231475,
19.1581929677179));
#33157=CARTESIAN_POINT('Ctrl Pts',(-13.1717526174749,-33.803909600387,19.1591163004037));
#33158=CARTESIAN_POINT('Ctrl Pts',(-13.1776997615675,-33.8199018810217,
19.1601354427775));
#33159=CARTESIAN_POINT('Ctrl Pts',(-13.1782254172952,-33.8213183033965,
19.1602257375613));
#33160=CARTESIAN_POINT('Ctrl Pts',(-13.1787501240201,-33.8227350716418,
19.1603160842799));
#33161=CARTESIAN_POINT('Origin',(-10.,-35.,23.));
#33162=CARTESIAN_POINT('',(-13.1787501237351,-33.8227350708723,20.4156322019944));
#33163=CARTESIAN_POINT('',(-13.1787501240278,-33.8227350716626,20.0676097122989));
#33164=CARTESIAN_POINT('',(-13.1787501240207,-33.8227350716434,23.));
#33165=CARTESIAN_POINT('Ctrl Pts',(-13.1787501240278,-33.8227350716626,
20.0676097122989));
#33166=CARTESIAN_POINT('Ctrl Pts',(-13.1611853468585,-33.7753081618307,
20.0645358172842));
#33167=CARTESIAN_POINT('Ctrl Pts',(-13.1425606400635,-33.7282783450763,
20.0614952758765));
#33168=CARTESIAN_POINT('Ctrl Pts',(-13.1112568932655,-33.6541247221329,
20.0567113797675));
#33169=CARTESIAN_POINT('Ctrl Pts',(-13.099259690771,-33.6267231981489,20.0549458528331));
#33170=CARTESIAN_POINT('Ctrl Pts',(-13.0759469510001,-33.5753392155133,
20.0516382942934));
#33171=CARTESIAN_POINT('Ctrl Pts',(-13.0647097156829,-33.5513239100277,
20.0500937795061));
#33172=CARTESIAN_POINT('Ctrl Pts',(-13.0384948140615,-33.4969700983274,
20.046599939044));
#33173=CARTESIAN_POINT('Ctrl Pts',(-13.0233422630176,-33.4667187802419,
20.0446567445545));
#33174=CARTESIAN_POINT('Ctrl Pts',(-12.9741865859815,-33.3721449234778,
20.0385816191994));
#33175=CARTESIAN_POINT('Ctrl Pts',(-12.9385632426113,-33.308685392804,20.0345054032097));
#33176=CARTESIAN_POINT('Ctrl Pts',(-12.7492455449724,-32.9955000486554,
20.0142917830798));
#33177=CARTESIAN_POINT('Ctrl Pts',(-12.5656684892498,-32.765339734078,19.9992411396829));
#33178=CARTESIAN_POINT('Ctrl Pts',(-12.3059904598391,-32.5145598716652,
19.9797116865118));
#33179=CARTESIAN_POINT('Ctrl Pts',(-12.2558052955851,-32.4689239099351,
19.9759977495463));
#33180=CARTESIAN_POINT('Ctrl Pts',(-12.1695355872243,-32.3950790764823,
19.9696472301789));
#33181=CARTESIAN_POINT('Ctrl Pts',(-12.1341863687468,-32.3660399003952,
19.9670539915919));
#33182=CARTESIAN_POINT('Ctrl Pts',(-12.082659346815,-32.3254290472168,19.9632690030034));
#33183=CARTESIAN_POINT('Ctrl Pts',(-12.0669490907539,-32.3132694308581,
19.9621143428392));
#33184=CARTESIAN_POINT('Ctrl Pts',(-12.0392317543396,-32.2922034082524,
19.9600743146627));
#33185=CARTESIAN_POINT('Ctrl Pts',(-12.0272712214014,-32.2832372364144,
19.9591930115543));
#33186=CARTESIAN_POINT('Ctrl Pts',(-12.0007909774868,-32.2636586581814,
19.9572392635049));
#33187=CARTESIAN_POINT('Ctrl Pts',(-11.986246071251,-32.2530826391922,19.9561646006955));
#33188=CARTESIAN_POINT('Ctrl Pts',(-11.9428365403902,-32.2220433511747,
19.9529544518074));
#33189=CARTESIAN_POINT('Ctrl Pts',(-11.9137357601464,-32.2019163355518,
19.9507988211438));
#33190=CARTESIAN_POINT('Ctrl Pts',(-11.72870768896,-32.0781817134344,19.9370968595503));
#33191=CARTESIAN_POINT('Ctrl Pts',(-11.5647463020549,-31.9871920798866,
19.9249909928736));
#33192=CARTESIAN_POINT('Ctrl Pts',(-11.2506782001936,-31.8454832450127,
19.9027863463488));
#33193=CARTESIAN_POINT('Ctrl Pts',(-11.1028855288573,-31.7908220921335,
19.8926988712996));
#33194=CARTESIAN_POINT('Ctrl Pts',(-10.860121843555,-31.7197982307892,19.876920978072));
#33195=CARTESIAN_POINT('Ctrl Pts',(-10.7673250960579,-31.6968578472047,
19.8710644115977));
#33196=CARTESIAN_POINT('Ctrl Pts',(-10.6371360758448,-31.6704575776151,
19.8630908578149));
#33197=CARTESIAN_POINT('Ctrl Pts',(-10.6004754981986,-31.6636510278115,
19.8608716578841));
#33198=CARTESIAN_POINT('Ctrl Pts',(-10.5370934559862,-31.6529618743906,
19.8570783816861));
#33199=CARTESIAN_POINT('Ctrl Pts',(-10.5104247471574,-31.6487912277859,
19.8554954837629));
#33200=CARTESIAN_POINT('Ctrl Pts',(-10.4556145866066,-31.6408890933222,
19.8522682473569));
#33201=CARTESIAN_POINT('Ctrl Pts',(-10.4274703327131,-31.6371916616105,
19.8506250820894));
#33202=CARTESIAN_POINT('Ctrl Pts',(-10.3550419318484,-31.6286004332206,
19.8464304174761));
#33203=CARTESIAN_POINT('Ctrl Pts',(-10.3107010440653,-31.6242252840418,
19.8438949997539));
#33204=CARTESIAN_POINT('Ctrl Pts',(-10.0931031414894,-31.6070786695997,
19.8315938814629));
#33205=CARTESIAN_POINT('Ctrl Pts',(-9.91912016172872,-31.6067639673029,
19.8222131202546));
#33206=CARTESIAN_POINT('Ctrl Pts',(-9.56089029654409,-31.6336969049995,
19.8030834940875));
#33207=CARTESIAN_POINT('Ctrl Pts',(-9.377379939208,-31.6627628969024,19.7933834722086));
#33208=CARTESIAN_POINT('Ctrl Pts',(-9.11543702474463,-31.72661762402,19.7786880680003));
#33209=CARTESIAN_POINT('Ctrl Pts',(-9.03447156840141,-31.749579023568,19.7740203113382));
#33210=CARTESIAN_POINT('Ctrl Pts',(-8.93102322441993,-31.7831225913699,
19.7677962255488));
#33211=CARTESIAN_POINT('Ctrl Pts',(-8.90768008125241,-31.7909738660044,
19.7663742831878));
#33212=CARTESIAN_POINT('Ctrl Pts',(-8.86956932772088,-31.8042561015582,
19.7640208972209));
#33213=CARTESIAN_POINT('Ctrl Pts',(-8.8547498525729,-31.8095369220686,19.7630978068953));
#33214=CARTESIAN_POINT('Ctrl Pts',(-8.82677319264438,-31.8197262513598,
19.7613391071707));
#33215=CARTESIAN_POINT('Ctrl Pts',(-8.81360870219809,-31.8246137352099,
19.7605047871282));
#33216=CARTESIAN_POINT('Ctrl Pts',(-8.77811132179096,-31.8380441401931,
19.7582375120424));
#33217=CARTESIAN_POINT('Ctrl Pts',(-8.7558382593947,-31.846741638616,19.7567960001449));
#33218=CARTESIAN_POINT('Ctrl Pts',(-8.66859845564776,-31.8818764383098,
19.751080418585));
#33219=CARTESIAN_POINT('Ctrl Pts',(-8.60437037262096,-31.9100904206449,
19.7467201914259));
#33220=CARTESIAN_POINT('Ctrl Pts',(-8.37017146646221,-32.0217606199007,
19.7303664474104));
#33221=CARTESIAN_POINT('Ctrl Pts',(-8.20640599282022,-32.1174196323892,
19.7180428013634));
#33222=CARTESIAN_POINT('Ctrl Pts',(-7.89977225548018,-32.3328247178107,
19.6940168808215));
#33223=CARTESIAN_POINT('Ctrl Pts',(-7.75704118188679,-32.4516802642273,
19.6823490353678));
#33224=CARTESIAN_POINT('Ctrl Pts',(-7.59296174265422,-32.6128353619107,
19.6684468833062));
#33225=CARTESIAN_POINT('Ctrl Pts',(-7.56180779388541,-32.6446640938806,
19.6657812837434));
#33226=CARTESIAN_POINT('Ctrl Pts',(-7.51184066651742,-32.6977676839168,
19.6614608145589));
#33227=CARTESIAN_POINT('Ctrl Pts',(-7.49265232859032,-32.7186805936257,
19.6597902119846));
#33228=CARTESIAN_POINT('Ctrl Pts',(-7.45573060093968,-32.7599493538083,
19.6565520219705));
#33229=CARTESIAN_POINT('Ctrl Pts',(-7.43797331849109,-32.7802808696794,
19.6549835115507));
#33230=CARTESIAN_POINT('Ctrl Pts',(-7.39626501728809,-32.8292028996488,
19.6512711479091));
#33231=CARTESIAN_POINT('Ctrl Pts',(-7.37253899993583,-32.8579811485152,
19.6491364132991));
#33232=CARTESIAN_POINT('Ctrl Pts',(-7.29345492890884,-32.9571970752566,
19.6419345124926));
#33233=CARTESIAN_POINT('Ctrl Pts',(-7.24041394565002,-33.0294374841514,
19.6369559349648));
#33234=CARTESIAN_POINT('Ctrl Pts',(-7.04295711140645,-33.3220047531251,
19.6176508908766));
#33235=CARTESIAN_POINT('Ctrl Pts',(-6.92157235358177,-33.5567235724241,
19.6040656428064));
#33236=CARTESIAN_POINT('Ctrl Pts',(-6.80383465870549,-33.8686976563005,
19.5860516642116));
#33237=CARTESIAN_POINT('Ctrl Pts',(-6.78112733445468,-33.9350231730128,
19.5822189121504));
#33238=CARTESIAN_POINT('Ctrl Pts',(-6.74670955580571,-34.0467433695319,
19.5756874641138));
#33239=CARTESIAN_POINT('Ctrl Pts',(-6.73385488040754,-34.091764056572,19.5730353796341));
#33240=CARTESIAN_POINT('Ctrl Pts',(-6.71683463237456,-34.1564171818552,
19.5691796650591));
#33241=CARTESIAN_POINT('Ctrl Pts',(-6.71190410388051,-34.1758445912841,
19.5680150557355));
#33242=CARTESIAN_POINT('Ctrl Pts',(-6.70359403968709,-34.2098501885008,
19.5659642405519));
#33243=CARTESIAN_POINT('Ctrl Pts',(-6.70013828832138,-34.2244088363186,
19.5650822560961));
#33244=CARTESIAN_POINT('Ctrl Pts',(-6.69276971516678,-34.2563926978317,
19.5631354784728));
#33245=CARTESIAN_POINT('Ctrl Pts',(-6.68889817987596,-34.2738259972481,
19.5620685859996));
#33246=CARTESIAN_POINT('Ctrl Pts',(-6.67811567128542,-34.3242587156416,
19.558967148552));
#33247=CARTESIAN_POINT('Ctrl Pts',(-6.67155923932524,-34.3573308049227,
19.5569148203269));
#33248=CARTESIAN_POINT('Ctrl Pts',(-6.62035128375505,-34.6374806322714,
19.5394047114061));
#33249=CARTESIAN_POINT('Ctrl Pts',(-6.60278758370256,-34.888706792209,19.522948874795));
#33250=CARTESIAN_POINT('Ctrl Pts',(-6.61796212383946,-35.2569707242624,
19.4993579350556));
#33251=CARTESIAN_POINT('Ctrl Pts',(-6.62890263878737,-35.3740595957055,
19.4919248274958));
#33252=CARTESIAN_POINT('Ctrl Pts',(-6.65742461145622,-35.5691550810337,
19.4797226243928));
#33253=CARTESIAN_POINT('Ctrl Pts',(-6.67171945646803,-35.6475321798334,
19.4748699296963));
#33254=CARTESIAN_POINT('Ctrl Pts',(-6.69624504014244,-35.759493793627,19.4680083786439));
#33255=CARTESIAN_POINT('Ctrl Pts',(-6.70425520842962,-35.7935326481029,
19.4659316826203));
#33256=CARTESIAN_POINT('Ctrl Pts',(-6.71929456906651,-35.8532800341837,
19.4623018077232));
#33257=CARTESIAN_POINT('Ctrl Pts',(-6.72610282747604,-35.8790405594974,
19.4607418086034));
#33258=CARTESIAN_POINT('Ctrl Pts',(-6.74103385251855,-35.9329539583043,
19.457486558318));
#33259=CARTESIAN_POINT('Ctrl Pts',(-6.74921935847811,-35.961087268357,19.4557934525214));
#33260=CARTESIAN_POINT('Ctrl Pts',(-6.77206196209059,-36.0359635560181,
19.4512999845432));
#33261=CARTESIAN_POINT('Ctrl Pts',(-6.78736949485529,-36.0825017521497,
19.4485205595353));
#33262=CARTESIAN_POINT('Ctrl Pts',(-6.89296663141016,-36.3815396500134,
19.4307154226582));
#33263=CARTESIAN_POINT('Ctrl Pts',(-7.01193493440893,-36.6228942557022,
19.4166951656437));
#33264=CARTESIAN_POINT('Ctrl Pts',(-7.24502229282914,-36.9813949015625,
19.3939448329222));
#33265=CARTESIAN_POINT('Ctrl Pts',(-7.34124890867364,-37.1087578283937,
19.3853772865324));
#33266=CARTESIAN_POINT('Ctrl Pts',(-7.46475761880317,-37.2502798016761,
19.3746825590842));
#33267=CARTESIAN_POINT('Ctrl Pts',(-7.48371678793185,-37.2714602795498,
19.3730481757949));
#33268=CARTESIAN_POINT('Ctrl Pts',(-7.51413051543064,-37.3045892932183,
19.3704330879398));
#33269=CARTESIAN_POINT('Ctrl Pts',(-7.52541047499721,-37.3166971235827,
19.3694646179305));
#33270=CARTESIAN_POINT('Ctrl Pts',(-7.54720055073982,-37.3397457292179,
19.3675953660787));
#33271=CARTESIAN_POINT('Ctrl Pts',(-7.55769618130358,-37.350699308632,19.3666956103486));
#33272=CARTESIAN_POINT('Ctrl Pts',(-7.58143745514546,-37.3751458453699,
19.3646623692457));
#33273=CARTESIAN_POINT('Ctrl Pts',(-7.59472318478407,-37.3885991661621,
19.3635259687682));
#33274=CARTESIAN_POINT('Ctrl Pts',(-7.64232656506652,-37.4360031557601,
19.3594614917787));
#33275=CARTESIAN_POINT('Ctrl Pts',(-7.67725466493795,-37.46932966877,19.3564925850621));
#33276=CARTESIAN_POINT('Ctrl Pts',(-7.86577981016146,-37.6416706991776,
19.3405923055625));
#33277=CARTESIAN_POINT('Ctrl Pts',(-8.03116332555608,-37.7671278048527,
19.3270986645285));
#33278=CARTESIAN_POINT('Ctrl Pts',(-8.37276183680249,-37.9800458057855,
19.3012508776266));
#33279=CARTESIAN_POINT('Ctrl Pts',(-8.54721145733076,-38.0688763949976,
19.2889244251002));
#33280=CARTESIAN_POINT('Ctrl Pts',(-8.76996210152708,-38.1590228584702,
19.2743944193604));
#33281=CARTESIAN_POINT('Ctrl Pts',(-8.81188952445043,-38.1750295178659,
19.2717077962796));
#33282=CARTESIAN_POINT('Ctrl Pts',(-8.88090021395099,-38.199817213159,19.267362247924));
#33283=CARTESIAN_POINT('Ctrl Pts',(-8.90779706059852,-38.2090975899293,
19.2656872375211));
#33284=CARTESIAN_POINT('Ctrl Pts',(-8.96040147925873,-38.2265099971639,
19.2624464713426));
#33285=CARTESIAN_POINT('Ctrl Pts',(-8.98609544144652,-38.2346760972051,
19.2608797131301));
#33286=CARTESIAN_POINT('Ctrl Pts',(-9.04735744456869,-38.253344801224,19.2571809411306));
#33287=CARTESIAN_POINT('Ctrl Pts',(-9.08300617360643,-38.2635720782276,
19.2550578583474));
#33288=CARTESIAN_POINT('Ctrl Pts',(-9.20398881013651,-38.2961418823728,
19.2479444240423));
#33289=CARTESIAN_POINT('Ctrl Pts',(-9.29002760445747,-38.3157391417449,
19.2430396121035));
#33290=CARTESIAN_POINT('Ctrl Pts',(-9.64378970841421,-38.3819123559373,
19.223341819376));
#33291=CARTESIAN_POINT('Ctrl Pts',(-9.91585905934855,-38.3995775941096,
19.2093577381375));
#33292=CARTESIAN_POINT('Ctrl Pts',(-10.2533021625765,-38.3809226174505,
19.1910572017665));
#33293=CARTESIAN_POINT('Ctrl Pts',(-10.3193685896116,-38.3753225855994,
19.1874233018042));
#33294=CARTESIAN_POINT('Ctrl Pts',(-10.4299473272693,-38.362674029551,19.1811951147816));
#33295=CARTESIAN_POINT('Ctrl Pts',(-10.4745612976508,-38.3566683641654,
19.1786420343931));
#33296=CARTESIAN_POINT('Ctrl Pts',(-10.5385513147805,-38.3467532576821,
19.174905375416));
#33297=CARTESIAN_POINT('Ctrl Pts',(-10.5580351500368,-38.343559722372,19.1737575957409));
#33298=CARTESIAN_POINT('Ctrl Pts',(-10.5922100331009,-38.3376511968254,
19.1717249940317));
#33299=CARTESIAN_POINT('Ctrl Pts',(-10.6069127576297,-38.3350090145937,
19.1708441291067));
#33300=CARTESIAN_POINT('Ctrl Pts',(-10.6393637676653,-38.3289556381055,
19.1688854154355));
#33301=CARTESIAN_POINT('Ctrl Pts',(-10.6571023192061,-38.3254996884165,
19.1678052649529));
#33302=CARTESIAN_POINT('Ctrl Pts',(-10.7099331864079,-38.3147676142774,
19.1645616809863));
#33303=CARTESIAN_POINT('Ctrl Pts',(-10.744937598293,-38.3070768391787,19.1623774978116));
#33304=CARTESIAN_POINT('Ctrl Pts',(-10.9244070868059,-38.2646520009408,
19.151020528956));
#33305=CARTESIAN_POINT('Ctrl Pts',(-11.0665874787242,-38.2210037792346,
19.141498603022));
#33306=CARTESIAN_POINT('Ctrl Pts',(-11.3243046032701,-38.1229470467411,
19.1237370464006));
#33307=CARTESIAN_POINT('Ctrl Pts',(-11.4405398140531,-38.0710630035466,
19.1155228035228));
#33308=CARTESIAN_POINT('Ctrl Pts',(-11.6434641435263,-37.9664215234145,
19.1009929985612));
#33309=CARTESIAN_POINT('Ctrl Pts',(-11.7312278867476,-37.9160733361442,
19.0946392723619));
#33310=CARTESIAN_POINT('Ctrl Pts',(-11.8773329560114,-37.8233310446316,
19.0839755566213));
#33311=CARTESIAN_POINT('Ctrl Pts',(-11.93681223353,-37.7828648459176,19.0796075647189));
#33312=CARTESIAN_POINT('Ctrl Pts',(-12.022197371093,-37.7207090326118,19.0732951080739));
#33313=CARTESIAN_POINT('Ctrl Pts',(-12.0491358446431,-37.7004781541207,
19.071297043557));
#33314=CARTESIAN_POINT('Ctrl Pts',(-12.0967167044531,-37.6636227593792,
19.0677549023571));
#33315=CARTESIAN_POINT('Ctrl Pts',(-12.1174738447297,-37.6471516237341,
19.0662050832352));
#33316=CARTESIAN_POINT('Ctrl Pts',(-12.1613122314387,-37.6115195196296,
19.0629210718914));
#33317=CARTESIAN_POINT('Ctrl Pts',(-12.1843366701767,-37.5922920664684,
19.061189694256));
#33318=CARTESIAN_POINT('Ctrl Pts',(-12.2458296142369,-37.5395389026308,
19.056545175639));
#33319=CARTESIAN_POINT('Ctrl Pts',(-12.2838020755113,-37.5054454603878,
19.0536551283866));
#33320=CARTESIAN_POINT('Ctrl Pts',(-12.5009175032319,-37.3014698201752,
19.0369651388992));
#33321=CARTESIAN_POINT('Ctrl Pts',(-12.6618394362214,-37.1132850329462,
19.0239862285052));
#33322=CARTESIAN_POINT('Ctrl Pts',(-12.899684260763,-36.7643675571192,19.0015660251271));
#33323=CARTESIAN_POINT('Ctrl Pts',(-12.9870591560932,-36.6120252524541,
18.992199849269));
#33324=CARTESIAN_POINT('Ctrl Pts',(-13.074544533561,-36.4277265536526,18.9805880349539));
#33325=CARTESIAN_POINT('Ctrl Pts',(-13.0865108010922,-36.4016697758418,
18.9789398844224));
#33326=CARTESIAN_POINT('Ctrl Pts',(-13.1048804590286,-36.3602933345371,
18.9763078668655));
#33327=CARTESIAN_POINT('Ctrl Pts',(-13.1115045591466,-36.3450724790802,
18.9753365072467));
#33328=CARTESIAN_POINT('Ctrl Pts',(-13.1239572817365,-36.3158743448492,
18.9734660452761));
#33329=CARTESIAN_POINT('Ctrl Pts',(-13.1298044531037,-36.301905696061,18.9725680284185));
#33330=CARTESIAN_POINT('Ctrl Pts',(-13.14406548639,-36.2671853488605,18.9703288036037));
#33331=CARTESIAN_POINT('Ctrl Pts',(-13.1523676076886,-36.2463887427764,
18.9689813365523));
#33332=CARTESIAN_POINT('Ctrl Pts',(-13.1816270525135,-36.1709318029151,
18.9640737920417));
#33333=CARTESIAN_POINT('Ctrl Pts',(-13.2013725906665,-36.1158157043508,
18.9604544513983));
#33334=CARTESIAN_POINT('Ctrl Pts',(-13.2818106808362,-35.8715409242023,
18.9443435420874));
#33335=CARTESIAN_POINT('Ctrl Pts',(-13.3272339491523,-35.6777724713108,
18.9314074419919));
#33336=CARTESIAN_POINT('Ctrl Pts',(-13.3781944289231,-35.3223842453021,
18.9083686215589));
#33337=CARTESIAN_POINT('Ctrl Pts',(-13.3896657123435,-35.1621907236818,
18.8982236322739));
#33338=CARTESIAN_POINT('Ctrl Pts',(-13.389778607959,-34.9461372905748,18.8849939288848));
#33339=CARTESIAN_POINT('Ctrl Pts',(-13.388438049834,-34.8905087781159,18.8816264220252));
#33340=CARTESIAN_POINT('Ctrl Pts',(-13.3840803320592,-34.8011250038821,
18.8762764696107));
#33341=CARTESIAN_POINT('Ctrl Pts',(-13.381925533382,-34.7673397987074,18.8742682890804));
#33342=CARTESIAN_POINT('Ctrl Pts',(-13.377181046961,-34.7071582269766,18.8707148637787));
#33343=CARTESIAN_POINT('Ctrl Pts',(-13.3747870192056,-34.6807496871589,
18.8691637405984));
#33344=CARTESIAN_POINT('Ctrl Pts',(-13.3690346306615,-34.6246272115056,
18.8658837243108));
#33345=CARTESIAN_POINT('Ctrl Pts',(-13.3655924598424,-34.5949240197089,
18.8641575546559));
#33346=CARTESIAN_POINT('Ctrl Pts',(-13.3551001403706,-34.5137872241645,
18.859466777882));
#33347=CARTESIAN_POINT('Ctrl Pts',(-13.3472606761465,-34.4624628550752,
18.8565265836641));
#33348=CARTESIAN_POINT('Ctrl Pts',(-13.3091777776031,-34.2464988705079,
18.8442430615774));
#33349=CARTESIAN_POINT('Ctrl Pts',(-13.2679403249764,-34.0840332654547,
18.8352348849132));
#33350=CARTESIAN_POINT('Ctrl Pts',(-13.2033719792797,-33.8908891407193,
18.8244023837771));
#33351=CARTESIAN_POINT('Ctrl Pts',(-13.1913320735613,-33.856707778262,18.8224797537842));
#33352=CARTESIAN_POINT('Ctrl Pts',(-13.1787501466517,-33.8227351327498,
18.8205587414464));
#33353=CARTESIAN_POINT('',(-13.3897492734215,-34.9977805770088,19.2362441100456));
#33354=CARTESIAN_POINT('Ctrl Pts',(-13.1787501240201,-33.8227350716418,
19.1603160842799));
#33355=CARTESIAN_POINT('Ctrl Pts',(-13.1864743779049,-33.8435914416932,
19.161646086278));
#33356=CARTESIAN_POINT('Ctrl Pts',(-13.1939929729178,-33.8645227656139,
19.1629873410737));
#33357=CARTESIAN_POINT('Ctrl Pts',(-13.2259874889372,-33.9564263874323,
19.1688999912539));
#33358=CARTESIAN_POINT('Ctrl Pts',(-13.248306214562,-34.0281222976731,19.1735734052367));
#33359=CARTESIAN_POINT('Ctrl Pts',(-13.3486745287529,-34.3927961905211,
19.1974547585279));
#33360=CARTESIAN_POINT('Ctrl Pts',(-13.3895507473258,-34.6945694760009,
19.217413212814));
#33361=CARTESIAN_POINT('Ctrl Pts',(-13.3897492734215,-34.9977805770088,
19.2362441100456));
#33362=CARTESIAN_POINT('Ctrl Pts',(-13.3897492760003,-34.9977845192167,
19.236244354876));
#33363=CARTESIAN_POINT('Ctrl Pts',(-13.3897845749226,-35.0517928847712,
19.2395985377884));
#33364=CARTESIAN_POINT('Ctrl Pts',(-13.3885291145359,-35.1057969828223,
19.2429192167761));
#33365=CARTESIAN_POINT('Ctrl Pts',(-13.3840382928665,-35.2009817582665,
19.2487120744362));
#33366=CARTESIAN_POINT('Ctrl Pts',(-13.3813400213536,-35.2421749746294,
19.2511992241826));
#33367=CARTESIAN_POINT('Ctrl Pts',(-13.3756795764973,-35.3096641480058,
19.2552424422283));
#33368=CARTESIAN_POINT('Ctrl Pts',(-13.3731608174323,-35.3359920340823,
19.2568118173895));
#33369=CARTESIAN_POINT('Ctrl Pts',(-13.3676455837124,-35.3872997343317,
19.2598554009154));
#33370=CARTESIAN_POINT('Ctrl Pts',(-13.3646786396044,-35.4122809293162,
19.2613304166859));
#33371=CARTESIAN_POINT('Ctrl Pts',(-13.3577914067957,-35.4652304537003,
19.2644430440054));
#33372=CARTESIAN_POINT('Ctrl Pts',(-13.353799125562,-35.4931875932648,19.2660783040404));
#33373=CARTESIAN_POINT('Ctrl Pts',(-13.3427185322349,-35.5644110344104,
19.2702251560015));
#33374=CARTESIAN_POINT('Ctrl Pts',(-13.3351392672814,-35.6075963439119,
19.2727213995748));
#33375=CARTESIAN_POINT('Ctrl Pts',(-13.296058462672,-35.8074215452538,19.2842035962231));
#33376=CARTESIAN_POINT('Ctrl Pts',(-13.2543445292222,-35.9618628763027,
19.2928694811663));
#33377=CARTESIAN_POINT('Ctrl Pts',(-13.1383490953228,-36.2956197712006,
19.3117355404843));
#33378=CARTESIAN_POINT('Ctrl Pts',(-13.059272919385,-36.4726535645523,19.3218343031454));
#33379=CARTESIAN_POINT('Ctrl Pts',(-12.9217425693223,-36.7210451343814,
19.3372616502941));
#33380=CARTESIAN_POINT('Ctrl Pts',(-12.8748145766163,-36.798336603414,19.3422616321036));
#33381=CARTESIAN_POINT('Ctrl Pts',(-12.8109493466584,-36.8946245164247,
19.3488692801207));
#33382=CARTESIAN_POINT('Ctrl Pts',(-12.7968075449926,-36.9154387915058,
19.3503212366677));
#33383=CARTESIAN_POINT('Ctrl Pts',(-12.7733851514048,-36.9491000386322,
19.3527114435025));
#33384=CARTESIAN_POINT('Ctrl Pts',(-12.7642436310545,-36.9620431403915,
19.3536408211248));
#33385=CARTESIAN_POINT('Ctrl Pts',(-12.7457723506806,-36.9878105443928,
19.3555128129378));
#33386=CARTESIAN_POINT('Ctrl Pts',(-12.7364426676058,-37.0006344160155,
19.3564554125316));
#33387=CARTESIAN_POINT('Ctrl Pts',(-12.7120421745917,-37.0336834781207,
19.358912127531));
#33388=CARTESIAN_POINT('Ctrl Pts',(-12.6968352596872,-37.0538064041418,
19.3604349584379));
#33389=CARTESIAN_POINT('Ctrl Pts',(-12.6304483155188,-37.1396459325888,
19.367041392582));
#33390=CARTESIAN_POINT('Ctrl Pts',(-12.5770833450086,-37.2036293652792,
19.3722474779447));
#33391=CARTESIAN_POINT('Ctrl Pts',(-12.3879346911847,-37.4141378826565,
19.3901860990655));
#33392=CARTESIAN_POINT('Ctrl Pts',(-12.2415811064057,-37.5506096986927,
19.4032060297474));
#33393=CARTESIAN_POINT('Ctrl Pts',(-11.9566924007405,-37.7726957725488,
19.4262534029351));
#33394=CARTESIAN_POINT('Ctrl Pts',(-11.8223770407936,-37.8627680028019,
19.4363531739312));
#33395=CARTESIAN_POINT('Ctrl Pts',(-11.6444657816674,-37.9644594575813,
19.4487277933124));
#33396=CARTESIAN_POINT('Ctrl Pts',(-11.6063858318561,-37.9852658849396,
19.4513228272647));
#33397=CARTESIAN_POINT('Ctrl Pts',(-11.5429600089168,-38.0183558042834,
19.4555593685868));
#33398=CARTESIAN_POINT('Ctrl Pts',(-11.5178427355597,-38.0310643100842,
19.4572154406488));
#33399=CARTESIAN_POINT('Ctrl Pts',(-11.4684901122207,-38.0552677659962,
19.4604284252984));
#33400=CARTESIAN_POINT('Ctrl Pts',(-11.4442709384102,-38.0667908061405,
19.4619862113479));
#33401=CARTESIAN_POINT('Ctrl Pts',(-11.3855472598943,-38.0938804949821,
19.465719312078));
#33402=CARTESIAN_POINT('Ctrl Pts',(-11.3509134130815,-38.1091591853157,
19.4678848198425));
#33403=CARTESIAN_POINT('Ctrl Pts',(-11.2305431202365,-38.1598692547302,
19.4752943690897));
#33404=CARTESIAN_POINT('Ctrl Pts',(-11.143609868394,-38.1923609649953,19.4804426927704));
#33405=CARTESIAN_POINT('Ctrl Pts',(-10.8026758494185,-38.3040686270126,
19.5000333692691));
#33406=CARTESIAN_POINT('Ctrl Pts',(-10.5410520818374,-38.35684544356,19.5137354224122));
#33407=CARTESIAN_POINT('Ctrl Pts',(-10.210333311462,-38.3838587911433,19.5317087893995));
#33408=CARTESIAN_POINT('Ctrl Pts',(-10.144569352785,-38.3873056045895,19.5353191552091));
#33409=CARTESIAN_POINT('Ctrl Pts',(-10.0339647138807,-38.3898758513815,
19.5415112926484));
#33410=CARTESIAN_POINT('Ctrl Pts',(-9.9891651350432,-38.3900286281257,19.54405247508));
#33411=CARTESIAN_POINT('Ctrl Pts',(-9.92467337934728,-38.3889702474023,
19.5477747948146));
#33412=CARTESIAN_POINT('Ctrl Pts',(-9.90497250681671,-38.3884750511983,
19.548920510633));
#33413=CARTESIAN_POINT('Ctrl Pts',(-9.87034934580922,-38.3873025962247,
19.5509509327028));
#33414=CARTESIAN_POINT('Ctrl Pts',(-9.85542548127593,-38.3866984463618,
19.5518317148028));
#33415=CARTESIAN_POINT('Ctrl Pts',(-9.82242407454618,-38.3851439440076,
19.5537921348201));
#33416=CARTESIAN_POINT('Ctrl Pts',(-9.80435006495777,-38.3841474260754,
19.5548741014684));
#33417=CARTESIAN_POINT('Ctrl Pts',(-9.75037289045416,-38.3807375261865,
19.5581284079223));
#33418=CARTESIAN_POINT('Ctrl Pts',(-9.7145003391815,-38.3778972210151,19.5603216883914));
#33419=CARTESIAN_POINT('Ctrl Pts',(-9.52846418521909,-38.3601828585759,
19.571831760279));
#33420=CARTESIAN_POINT('Ctrl Pts',(-9.37938107206355,-38.3358656870698,
19.5815081576014));
#33421=CARTESIAN_POINT('Ctrl Pts',(-9.10374894855583,-38.2717872840282,
19.5997387997388));
#33422=CARTESIAN_POINT('Ctrl Pts',(-8.97692488673516,-38.2343743998584,
19.6082684906967));
#33423=CARTESIAN_POINT('Ctrl Pts',(-8.71638000743087,-38.1406501500173,
19.625857486038));
#33424=CARTESIAN_POINT('Ctrl Pts',(-8.58342192362891,-38.0829659163685,
19.6348694913263));
#33425=CARTESIAN_POINT('Ctrl Pts',(-8.41691090705096,-37.9976694432793,
19.646155627523));
#33426=CARTESIAN_POINT('Ctrl Pts',(-8.37963833479819,-37.9776872709997,
19.6486827369162));
#33427=CARTESIAN_POINT('Ctrl Pts',(-8.31838738648109,-37.9433592929094,
19.652838558637));
#33428=CARTESIAN_POINT('Ctrl Pts',(-8.29419579396036,-37.9294055692992,
19.6544807398343));
#33429=CARTESIAN_POINT('Ctrl Pts',(-8.24699091918078,-37.9013947038992,
19.6576876853369));
#33430=CARTESIAN_POINT('Ctrl Pts',(-8.22396751888269,-37.8873587848961,
19.6592530486379));
#33431=CARTESIAN_POINT('Ctrl Pts',(-8.17350936039638,-37.8557656979162,
19.6626877478857));
#33432=CARTESIAN_POINT('Ctrl Pts',(-8.14615506089277,-37.8380847104437,
19.6645524460385));
#33433=CARTESIAN_POINT('Ctrl Pts',(-8.05181835175569,-37.7751623597298,
19.6709972658533));
#33434=CARTESIAN_POINT('Ctrl Pts',(-7.98620010269377,-37.72792030648,19.6755044206689));
#33435=CARTESIAN_POINT('Ctrl Pts',(-7.70086023007183,-37.5065763306376,
19.695340422984));
#33436=CARTESIAN_POINT('Ctrl Pts',(-7.50156901498557,-37.3079864808002,
19.7097511677582));
#33437=CARTESIAN_POINT('Ctrl Pts',(-7.28778513431875,-37.0343981394582,
19.7285448794397));
#33438=CARTESIAN_POINT('Ctrl Pts',(-7.24814548197941,-36.9804497167778,
19.7322124223347));
#33439=CARTESIAN_POINT('Ctrl Pts',(-7.18438797133657,-36.8880646357383,
19.7384920718721));
#33440=CARTESIAN_POINT('Ctrl Pts',(-7.15939707648405,-36.8502523576473,
19.74106207898));
#33441=CARTESIAN_POINT('Ctrl Pts',(-7.12459150827332,-36.795222251874,19.7448191079696));
#33442=CARTESIAN_POINT('Ctrl Pts',(-7.11415703127194,-36.778400193081,19.7459697888211));
#33443=CARTESIAN_POINT('Ctrl Pts',(-7.09610551330263,-36.7487210102446,
19.7480055257937));
#33444=CARTESIAN_POINT('Ctrl Pts',(-7.08842521861717,-36.7359034080442,
19.7488865795069));
#33445=CARTESIAN_POINT('Ctrl Pts',(-7.07166225659191,-36.7075035553839,
19.750843221709));
#33446=CARTESIAN_POINT('Ctrl Pts',(-7.06261915196061,-36.6918995397369,
19.7519210767044));
#33447=CARTESIAN_POINT('Ctrl Pts',(-7.03607488908259,-36.6452427049893,
19.7551505023003));
#33448=CARTESIAN_POINT('Ctrl Pts',(-7.01893907605644,-36.6139861127826,
19.7573225634741));
#33449=CARTESIAN_POINT('Ctrl Pts',(-6.93476612076658,-36.4545354950783,
19.7684243122262));
#33450=CARTESIAN_POINT('Ctrl Pts',(-6.87549603906129,-36.322422248421,19.7776853448444));
#33451=CARTESIAN_POINT('Ctrl Pts',(-6.78140600123141,-36.0707245556632,
19.7949886816328));
#33452=CARTESIAN_POINT('Ctrl Pts',(-6.74437420746595,-35.9522083421974,
19.8030051329824));
#33453=CARTESIAN_POINT('Ctrl Pts',(-6.68806199929361,-35.7297773673681,
19.8176313335132));
#33454=CARTESIAN_POINT('Ctrl Pts',(-6.66697666990258,-35.6264716675134,
19.8242640758911));
#33455=CARTESIAN_POINT('Ctrl Pts',(-6.63933547000476,-35.4492367986342,
19.8353305846701));
#33456=CARTESIAN_POINT('Ctrl Pts',(-6.63032988216214,-35.3757716663386,
19.839828523691));
#33457=CARTESIAN_POINT('Ctrl Pts',(-6.62070214116034,-35.26816014551,19.8462890806219));
#33458=CARTESIAN_POINT('Ctrl Pts',(-6.61817949469435,-35.2342094769752,
19.8483089608516));
#33459=CARTESIAN_POINT('Ctrl Pts',(-6.6146012889051,-35.173737467794,19.8518752833638));
#33460=CARTESIAN_POINT('Ctrl Pts',(-6.61334499168027,-35.1472312970535,
19.8534277647332));
#33461=CARTESIAN_POINT('Ctrl Pts',(-6.61133929925244,-35.0909448175668,
19.8567027921618));
#33462=CARTESIAN_POINT('Ctrl Pts',(-6.61067095413299,-35.0611637572551,
19.8584227206753));
#33463=CARTESIAN_POINT('Ctrl Pts',(-6.60991982337146,-34.9800204922067,
19.8630762675357));
#33464=CARTESIAN_POINT('Ctrl Pts',(-6.61061163404398,-34.9286580179134,
19.8659861444027));
#33465=CARTESIAN_POINT('Ctrl Pts',(-6.62149561329613,-34.6280993142513,
19.8828396673708));
#33466=CARTESIAN_POINT('Ctrl Pts',(-6.65799596034638,-34.380627654014,19.895942516164));
#33467=CARTESIAN_POINT('Ctrl Pts',(-6.75149621644082,-34.0244203445412,
19.9154999551234));
#33468=CARTESIAN_POINT('Ctrl Pts',(-6.7876972036621,-33.9111289956048,19.9218440965742));
#33469=CARTESIAN_POINT('Ctrl Pts',(-6.85319494731223,-33.7380961440355,
19.9320338326522));
#33470=CARTESIAN_POINT('Ctrl Pts',(-6.87842514284344,-33.676915478525,19.9357387863629));
#33471=CARTESIAN_POINT('Ctrl Pts',(-6.91471662730229,-33.595738781596,19.9408425588553));
#33472=CARTESIAN_POINT('Ctrl Pts',(-6.92421440008435,-33.5750558108276,
19.9421597161659));
#33473=CARTESIAN_POINT('Ctrl Pts',(-6.94046996523299,-33.5405764884283,
19.9443862149576));
#33474=CARTESIAN_POINT('Ctrl Pts',(-6.94711477082101,-33.5267271840455,
19.9452889490864));
#33475=CARTESIAN_POINT('Ctrl Pts',(-6.96110150128007,-33.4980765853706,
19.9471748687212));
#33476=CARTESIAN_POINT('Ctrl Pts',(-6.96845781942039,-33.4832831473512,
19.9481588321655));
#33477=CARTESIAN_POINT('Ctrl Pts',(-6.98870892790336,-33.4432944357736,
19.9508451615955));
#33478=CARTESIAN_POINT('Ctrl Pts',(-7.00181133561802,-33.4182064757061,
19.9525593123731));
#33479=CARTESIAN_POINT('Ctrl Pts',(-7.08580668873753,-33.2621692315521,
19.9633885815555));
#33480=CARTESIAN_POINT('Ctrl Pts',(-7.16494440344835,-33.1358567381559,
19.972895562966));
#33481=CARTESIAN_POINT('Ctrl Pts',(-7.40016299556947,-32.8102107509234,
19.9987446931162));
#33482=CARTESIAN_POINT('Ctrl Pts',(-7.57069647243771,-32.6224281179145,
20.0150842408273));
#33483=CARTESIAN_POINT('Ctrl Pts',(-7.8087481616659,-32.4129276439528,20.0345333576256));
#33484=CARTESIAN_POINT('Ctrl Pts',(-7.85814783147684,-32.3718831614362,
20.038419588502));
#33485=CARTESIAN_POINT('Ctrl Pts',(-7.9341130578812,-32.3123318583815,20.0441781602691));
#33486=CARTESIAN_POINT('Ctrl Pts',(-7.95982411599474,-32.2927631489304,
20.0460914598109));
#33487=CARTESIAN_POINT('Ctrl Pts',(-8.00498997773149,-32.2593963042025,
20.0493921633121));
#33488=CARTESIAN_POINT('Ctrl Pts',(-8.02431756212809,-32.2454306045935,
20.0507859168318));
#33489=CARTESIAN_POINT('Ctrl Pts',(-8.06831482215952,-32.2143404470535,
20.0539175367482));
#33490=CARTESIAN_POINT('Ctrl Pts',(-8.09306810379204,-32.1973374091629,
20.0556507651515));
#33491=CARTESIAN_POINT('Ctrl Pts',(-8.16060552678165,-32.1522549975581,
20.0603054444828));
#33492=CARTESIAN_POINT('Ctrl Pts',(-8.20380571031646,-32.1248112957943,
20.0632036280528));
#33493=CARTESIAN_POINT('Ctrl Pts',(-8.45768393087942,-31.971486859662,20.0798180113542));
#33494=CARTESIAN_POINT('Ctrl Pts',(-8.68091048194822,-31.8678051342531,
20.0927250252142));
#33495=CARTESIAN_POINT('Ctrl Pts',(-9.08061482754219,-31.7325388330612,
20.1151269772694));
#33496=CARTESIAN_POINT('Ctrl Pts',(-9.25198638662764,-31.689103881127,20.1245512738168));
#33497=CARTESIAN_POINT('Ctrl Pts',(-9.45420982645986,-31.6543549080649,
20.1362299670203));
#33498=CARTESIAN_POINT('Ctrl Pts',(-9.4825418027632,-31.6498559891247,20.1378788917572));
#33499=CARTESIAN_POINT('Ctrl Pts',(-9.52735651853127,-31.6433217479596,
20.1405119133108));
#33500=CARTESIAN_POINT('Ctrl Pts',(-9.54380358260815,-31.6410469560046,
20.1414834893378));
#33501=CARTESIAN_POINT('Ctrl Pts',(-9.57528171350542,-31.6369286714489,
20.1433541519405));
#33502=CARTESIAN_POINT('Ctrl Pts',(-9.5903094631734,-31.6350649316252,20.1442521500799));
#33503=CARTESIAN_POINT('Ctrl Pts',(-9.6275844368058,-31.6306954826203,20.1464910671147));
#33504=CARTESIAN_POINT('Ctrl Pts',(-9.64984476244935,-31.6283093953852,
20.1478382400458));
#33505=CARTESIAN_POINT('Ctrl Pts',(-9.73035663857398,-31.6204851974397,
20.152743295928));
#33506=CARTESIAN_POINT('Ctrl Pts',(-9.78872015733889,-31.6163351474166,
20.1563603616714));
#33507=CARTESIAN_POINT('Ctrl Pts',(-10.0705548380071,-31.603614440014,20.1740333755053));
#33508=CARTESIAN_POINT('Ctrl Pts',(-10.2943960671935,-31.6156621029647,
20.1886517875108));
#33509=CARTESIAN_POINT('Ctrl Pts',(-10.6811901815642,-31.6751668178118,
20.2136564721994));
#33510=CARTESIAN_POINT('Ctrl Pts',(-10.8448576272418,-31.7129398609659,
20.2241628828816));
#33511=CARTESIAN_POINT('Ctrl Pts',(-11.0468404665663,-31.7756484944184,
20.2369381997889));
#33512=CARTESIAN_POINT('Ctrl Pts',(-11.0883529119116,-31.7894228242865,
20.2395544742172));
#33513=CARTESIAN_POINT('Ctrl Pts',(-11.156193277019,-31.8134001835384,20.2438162690791));
#33514=CARTESIAN_POINT('Ctrl Pts',(-11.1826799885321,-31.8231352876215,
20.2454767027279));
#33515=CARTESIAN_POINT('Ctrl Pts',(-11.2340599647061,-31.8427514893372,
20.2486918369664));
#33516=CARTESIAN_POINT('Ctrl Pts',(-11.258963708446,-31.8525990729377,20.2502474941414));
#33517=CARTESIAN_POINT('Ctrl Pts',(-11.3185582253842,-31.8769848125534,
20.2539650084044));
#33518=CARTESIAN_POINT('Ctrl Pts',(-11.353129221953,-31.8918074185857,20.2561172732135));
#33519=CARTESIAN_POINT('Ctrl Pts',(-11.4706727424195,-31.9445381461186,
20.263427379208));
#33520=CARTESIAN_POINT('Ctrl Pts',(-11.5523612280448,-31.9852194157938,
20.2684930426778));
#33521=CARTESIAN_POINT('Ctrl Pts',(-11.867082872848,-32.1581411203871,20.2881165580502));
#33522=CARTESIAN_POINT('Ctrl Pts',(-12.0857183711477,-32.3144963491286,
20.3019116597494));
#33523=CARTESIAN_POINT('Ctrl Pts',(-12.3324345241596,-32.5394087269167,
20.3199930828976));
#33524=CARTESIAN_POINT('Ctrl Pts',(-12.3798932094113,-32.5852810378745,
20.3236113222095));
#33525=CARTESIAN_POINT('Ctrl Pts',(-12.4573188271259,-32.6646193956947,
20.329815520593));
#33526=CARTESIAN_POINT('Ctrl Pts',(-12.4880150635659,-32.6973495638589,
20.3323606836019));
#33527=CARTESIAN_POINT('Ctrl Pts',(-12.5312525497046,-32.7453260885405,
20.336087794199));
#33528=CARTESIAN_POINT('Ctrl Pts',(-12.5443256021088,-32.7600890403227,
20.3372341936409));
#33529=CARTESIAN_POINT('Ctrl Pts',(-12.5670738128593,-32.7862339252988,
20.3392653421095));
#33530=CARTESIAN_POINT('Ctrl Pts',(-12.5768036963897,-32.7975670516342,
20.3401461561398));
#33531=CARTESIAN_POINT('Ctrl Pts',(-12.5981529378784,-32.8227692583367,
20.3421060354534));
#33532=CARTESIAN_POINT('Ctrl Pts',(-12.6097362277962,-32.8366671130018,
20.3431874207463));
#33533=CARTESIAN_POINT('Ctrl Pts',(-12.6432926523992,-32.8775904723364,
20.346371705913));
#33534=CARTESIAN_POINT('Ctrl Pts',(-12.664960536664,-32.9048619652437,20.348493789315));
#33535=CARTESIAN_POINT('Ctrl Pts',(-12.7979277733539,-33.0776166751844,
20.3619116875571));
#33536=CARTESIAN_POINT('Ctrl Pts',(-12.8976944995374,-33.2315785541648,
20.3737450059443));
#33537=CARTESIAN_POINT('Ctrl Pts',(-13.0591705866021,-33.5314413754368,
20.3956960454426));
#33538=CARTESIAN_POINT('Ctrl Pts',(-13.1240689965493,-33.6750897656337,
20.4057968251401));
#33539=CARTESIAN_POINT('Ctrl Pts',(-13.1787501237351,-33.8227350708723,
20.4156322019944));
#33540=CARTESIAN_POINT('Origin',(-10.,-35.,23.));
#33541=CARTESIAN_POINT('',(-13.1787500936073,-33.8227349895238,21.6644775413951));
#33542=CARTESIAN_POINT('',(-13.1787501333198,-33.8227350967521,21.3230163149173));
#33543=CARTESIAN_POINT('',(-13.1787501240207,-33.8227350716434,23.));
#33544=CARTESIAN_POINT('',(-13.3897498409715,-35.0010383320299,20.1438256239882));
#33545=CARTESIAN_POINT('Ctrl Pts',(-13.1787501333198,-33.8227350967521,
21.3230163149173));
#33546=CARTESIAN_POINT('Ctrl Pts',(-13.1402669858312,-33.7188261890181,
21.3160962228213));
#33547=CARTESIAN_POINT('Ctrl Pts',(-13.0967084745643,-33.6168571994136,
21.3090034474752));
#33548=CARTESIAN_POINT('Ctrl Pts',(-12.9319060910036,-33.2780694004307,
21.2847566361131));
#33549=CARTESIAN_POINT('Ctrl Pts',(-12.7878270355097,-33.0534180346275,
21.2675898966232));
#33550=CARTESIAN_POINT('Ctrl Pts',(-12.5843253798839,-32.8057708926119,
21.2480502979645));
#33551=CARTESIAN_POINT('Ctrl Pts',(-12.5486894025159,-32.7644772669941,
21.2447643123992));
#33552=CARTESIAN_POINT('Ctrl Pts',(-12.4914279145765,-32.7012748556937,
21.2396883190259));
#33553=CARTESIAN_POINT('Ctrl Pts',(-12.470475362046,-32.6787714628998,21.2378712795906));
#33554=CARTESIAN_POINT('Ctrl Pts',(-12.4309554134957,-32.6374677252693,
21.2345168297461));
#33555=CARTESIAN_POINT('Ctrl Pts',(-12.4124689287212,-32.6185935462785,
21.2329761820125));
#33556=CARTESIAN_POINT('Ctrl Pts',(-12.3706673022276,-32.5769016409987,
21.2295542213116));
#33557=CARTESIAN_POINT('Ctrl Pts',(-12.3472394637039,-32.554200310458,21.2276780149003));
#33558=CARTESIAN_POINT('Ctrl Pts',(-12.275504143539,-32.4866698058873,21.2220533878851));
#33559=CARTESIAN_POINT('Ctrl Pts',(-12.2262123506855,-32.442906508084,21.2183491001455));
#33560=CARTESIAN_POINT('Ctrl Pts',(-12.107161973885,-32.3432622192004,21.2097379492105));
#33561=CARTESIAN_POINT('Ctrl Pts',(-12.0364072414175,-32.2886471672074,
21.2048759668668));
#33562=CARTESIAN_POINT('Ctrl Pts',(-11.8490594979172,-32.1555105769936,
21.1925141486322));
#33563=CARTESIAN_POINT('Ctrl Pts',(-11.7295949226222,-32.0813284984821,
21.1851131518274));
#33564=CARTESIAN_POINT('Ctrl Pts',(-11.4575776911211,-31.9349995939614,
21.1687009623497));
#33565=CARTESIAN_POINT('Ctrl Pts',(-11.3035604610276,-31.8663953974293,
21.1596846456035));
#33566=CARTESIAN_POINT('Ctrl Pts',(-11.1180925343261,-31.7998284730845,
21.1484691655834));
#33567=CARTESIAN_POINT('Ctrl Pts',(-11.0909592120591,-31.7904772006969,
21.1468195383833));
#33568=CARTESIAN_POINT('Ctrl Pts',(-11.0479437416215,-31.7762607500315,
21.144185650614));
#33569=CARTESIAN_POINT('Ctrl Pts',(-11.0321383707925,-31.7711656599278,
21.1432139247373));
#33570=CARTESIAN_POINT('Ctrl Pts',(-11.0016828610239,-31.7615943488389,
21.141332802366));
#33571=CARTESIAN_POINT('Ctrl Pts',(-10.9870388245504,-31.7571009821792,
21.1404243639876));
#33572=CARTESIAN_POINT('Ctrl Pts',(-10.9507883214316,-31.7462461771116,
21.1381666232616));
#33573=CARTESIAN_POINT('Ctrl Pts',(-10.9291481272544,-31.7400006027872,
21.1368110558194));
#33574=CARTESIAN_POINT('Ctrl Pts',(-10.8455676430775,-31.7167782287938,
21.1315498580947));
#33575=CARTESIAN_POINT('Ctrl Pts',(-10.7832151156938,-31.7013483303259,
21.1275711494764));
#33576=CARTESIAN_POINT('Ctrl Pts',(-10.6098975805984,-31.6636496193188,
21.1164313952084));
#33577=CARTESIAN_POINT('Ctrl Pts',(-10.4981989458723,-31.6451521146798,
21.109164354599));
#33578=CARTESIAN_POINT('Ctrl Pts',(-10.1276219202218,-31.602700570786,21.0851320572966));
#33579=CARTESIAN_POINT('Ctrl Pts',(-9.86686416085046,-31.6029060269525,
21.0684276299297));
#33580=CARTESIAN_POINT('Ctrl Pts',(-9.55890117551041,-31.6386986539795,
21.049599996885));
#33581=CARTESIAN_POINT('Ctrl Pts',(-9.50927023819553,-31.6455850563841,
21.0465904952647));
#33582=CARTESIAN_POINT('Ctrl Pts',(-9.430657627776,-31.6582749635263,21.0418610150642));
#33583=CARTESIAN_POINT('Ctrl Pts',(-9.40156920191443,-31.6633613293175,
21.040119170246));
#33584=CARTESIAN_POINT('Ctrl Pts',(-9.34642253506713,-31.6737485909019,
21.0368314608407));
#33585=CARTESIAN_POINT('Ctrl Pts',(-9.32035310494966,-31.6789772514309,
21.0352834753672));
#33586=CARTESIAN_POINT('Ctrl Pts',(-9.26059311701581,-31.6916962833092,
21.0317480336775));
#33587=CARTESIAN_POINT('Ctrl Pts',(-9.22694974368161,-31.6993955937712,
21.0297672844043));
#33588=CARTESIAN_POINT('Ctrl Pts',(-9.11881987240803,-31.7258852755978,
21.0234273879753));
#33589=CARTESIAN_POINT('Ctrl Pts',(-9.04485035878773,-31.746694602652,21.0191314290186));
#33590=CARTESIAN_POINT('Ctrl Pts',(-8.86556078921875,-31.8037759822806,
21.008762965669));
#33591=CARTESIAN_POINT('Ctrl Pts',(-8.76119783629265,-31.8427588424619,
21.0027673901583));
#33592=CARTESIAN_POINT('Ctrl Pts',(-8.45706527544295,-31.9737693017101,
20.9851079822851));
#33593=CARTESIAN_POINT('Ctrl Pts',(-8.26414575489642,-32.0801514292994,
20.9736783224813));
#33594=CARTESIAN_POINT('Ctrl Pts',(-8.03157299617445,-32.2396425856585,
20.9581176603113));
#33595=CARTESIAN_POINT('Ctrl Pts',(-7.98123160821174,-32.2762431927009,
20.9546286238107));
#33596=CARTESIAN_POINT('Ctrl Pts',(-7.91377655284419,-32.3281838219972,
20.9497432595533));
#33597=CARTESIAN_POINT('Ctrl Pts',(-7.89576650758314,-32.3423447724907,
20.9484176227441));
#33598=CARTESIAN_POINT('Ctrl Pts',(-7.8660203626061,-32.3662254978074,20.9461898727932));
#33599=CARTESIAN_POINT('Ctrl Pts',(-7.85420339910283,-32.3758441050319,
20.9452946150572));
#33600=CARTESIAN_POINT('Ctrl Pts',(-7.82978833270833,-32.3959923286371,
20.943422612116));
#33601=CARTESIAN_POINT('Ctrl Pts',(-7.81720131000704,-32.4065342709862,
20.9424450650092));
#33602=CARTESIAN_POINT('Ctrl Pts',(-7.78349194359313,-32.4351859310051,
20.9397945169206));
#33603=CARTESIAN_POINT('Ctrl Pts',(-7.76251561109412,-32.4534645744628,
20.9381102320255));
#33604=CARTESIAN_POINT('Ctrl Pts',(-7.63914115920134,-32.5636734607895,
20.9280063637996));
#33605=CARTESIAN_POINT('Ctrl Pts',(-7.5422015101325,-32.6615045183677,20.9192503672406));
#33606=CARTESIAN_POINT('Ctrl Pts',(-7.26386237778455,-32.9788799457678,
20.8921258805095));
#33607=CARTESIAN_POINT('Ctrl Pts',(-7.10388848068874,-33.2156329374354,
20.8736960217714));
#33608=CARTESIAN_POINT('Ctrl Pts',(-6.95192399279683,-33.5159728107689,
20.8532167153632));
#33609=CARTESIAN_POINT('Ctrl Pts',(-6.92953703226849,-33.5628633835,20.8500909368474));
#33610=CARTESIAN_POINT('Ctrl Pts',(-6.89585595133953,-33.6377934887922,
20.845205852921));
#33611=CARTESIAN_POINT('Ctrl Pts',(-6.88384435354187,-33.665499745435,20.8434227181669));
#33612=CARTESIAN_POINT('Ctrl Pts',(-6.86302113163335,-33.715345884085,20.8402549143128));
#33613=CARTESIAN_POINT('Ctrl Pts',(-6.85406981794108,-33.7374248733243,
20.8388656687195));
#33614=CARTESIAN_POINT('Ctrl Pts',(-6.8336126228141,-33.7894525156608,20.835623627216));
#33615=CARTESIAN_POINT('Ctrl Pts',(-6.82229755519256,-33.8194740546552,
20.8337772126321));
#33616=CARTESIAN_POINT('Ctrl Pts',(-6.79003306443656,-33.9089063573563,
20.8283451548976));
#33617=CARTESIAN_POINT('Ctrl Pts',(-6.77031102225478,-33.9687469450605,
20.8247991167207));
#33618=CARTESIAN_POINT('Ctrl Pts',(-6.70769152097348,-34.1782149534663,
20.8126495899334));
#33619=CARTESIAN_POINT('Ctrl Pts',(-6.67343517303043,-34.3302255491785,
20.8043011876052));
#33620=CARTESIAN_POINT('Ctrl Pts',(-6.62018744111716,-34.6759896355574,
20.7857092651865));
#33621=CARTESIAN_POINT('Ctrl Pts',(-6.60717982923769,-34.8700901801265,
20.7755465852486));
#33622=CARTESIAN_POINT('Ctrl Pts',(-6.61207055170485,-35.1281897981063,
20.7613192373044));
#33623=CARTESIAN_POINT('Ctrl Pts',(-6.61509347986115,-35.192107749702,20.7577357147022));
#33624=CARTESIAN_POINT('Ctrl Pts',(-6.62167006993555,-35.2789760005041,
20.7527384990922));
#33625=CARTESIAN_POINT('Ctrl Pts',(-6.62365353953989,-35.3020351648611,
20.7513997481108));
#33626=CARTESIAN_POINT('Ctrl Pts',(-6.62733828003341,-35.3402814640963,
20.7491562971281));
#33627=CARTESIAN_POINT('Ctrl Pts',(-6.62890645244173,-35.3554811346509,
20.7482586673095));
#33628=CARTESIAN_POINT('Ctrl Pts',(-6.63236437584895,-35.3869139952379,
20.7463889541675));
#33629=CARTESIAN_POINT('Ctrl Pts',(-6.63426883061069,-35.403144896676,20.7454161534632));
#33630=CARTESIAN_POINT('Ctrl Pts',(-6.63968877441915,-35.4466184566698,
20.7427920121682));
#33631=CARTESIAN_POINT('Ctrl Pts',(-6.64341809397308,-35.4738326519488,
20.7411297518359));
#33632=CARTESIAN_POINT('Ctrl Pts',(-6.6664677706267,-35.6280740387228,20.7316086516929));
#33633=CARTESIAN_POINT('Ctrl Pts',(-6.69266619964882,-35.7539570652183,
20.7234557804387));
#33634=CARTESIAN_POINT('Ctrl Pts',(-6.8018451310795,-36.1610677375388,20.6964123240988));
#33635=CARTESIAN_POINT('Ctrl Pts',(-6.91414650493017,-36.4331215507197,
20.6773850848167));
#33636=CARTESIAN_POINT('Ctrl Pts',(-7.08628851226897,-36.7330512816328,
20.6563329025517));
#33637=CARTESIAN_POINT('Ctrl Pts',(-7.113579933122,-36.7781341461501,20.6531613022237));
#33638=CARTESIAN_POINT('Ctrl Pts',(-7.15823289906459,-36.8481575065837,
20.6482215381644));
#33639=CARTESIAN_POINT('Ctrl Pts',(-7.17489669645336,-36.8735308482042,
20.6464286460806));
#33640=CARTESIAN_POINT('Ctrl Pts',(-7.20657499486972,-36.9203823239639,
20.6431115129367));
#33641=CARTESIAN_POINT('Ctrl Pts',(-7.22150195426622,-36.9419166295661,
20.6415842007553));
#33642=CARTESIAN_POINT('Ctrl Pts',(-7.25580218730712,-36.9901944067439,
20.6381529187887));
#33643=CARTESIAN_POINT('Ctrl Pts',(-7.27531973466054,-37.0168324108284,
20.6362545656993));
#33644=CARTESIAN_POINT('Ctrl Pts',(-7.33627964198508,-37.0975315003419,
20.630483837977));
#33645=CARTESIAN_POINT('Ctrl Pts',(-7.37896590193656,-37.1506337805261,
20.6266591987111));
#33646=CARTESIAN_POINT('Ctrl Pts',(-7.58601327742642,-37.3928742705515,
20.6090082627623));
#33647=CARTESIAN_POINT('Ctrl Pts',(-7.76941000004373,-37.5646933635845,
20.5959518322867));
#33648=CARTESIAN_POINT('Ctrl Pts',(-8.08633919688312,-37.8016751161388,
20.5748438226631));
#33649=CARTESIAN_POINT('Ctrl Pts',(-8.20805936123526,-37.8810451562144,
20.5670006748164));
#33650=CARTESIAN_POINT('Ctrl Pts',(-8.35911326130663,-37.9662595784076,
20.5571243457608));
#33651=CARTESIAN_POINT('Ctrl Pts',(-8.383921828391,-37.9798483867735,20.5554977813112));
#33652=CARTESIAN_POINT('Ctrl Pts',(-8.42348200470763,-38.0008780247653,
20.5528923465613));
#33653=CARTESIAN_POINT('Ctrl Pts',(-8.43812348158442,-38.0085244930506,
20.5519255584112));
#33654=CARTESIAN_POINT('Ctrl Pts',(-8.46648955797091,-38.0230757213934,
20.5500466006328));
#33655=CARTESIAN_POINT('Ctrl Pts',(-8.48020614165381,-38.0299946678135,
20.5491352887193));
#33656=CARTESIAN_POINT('Ctrl Pts',(-8.51436810221523,-38.0469363956527,
20.5468596335747));
#33657=CARTESIAN_POINT('Ctrl Pts',(-8.53486816575161,-38.0568467709969,
20.5454888063523));
#33658=CARTESIAN_POINT('Ctrl Pts',(-8.61540468158909,-38.0947844405223,
20.5400874502244));
#33659=CARTESIAN_POINT('Ctrl Pts',(-8.67615454567597,-38.1212540694852,
20.5359789978298));
#33660=CARTESIAN_POINT('Ctrl Pts',(-8.84818660320149,-38.1902852711145,
20.5243247150522));
#33661=CARTESIAN_POINT('Ctrl Pts',(-8.96099324102022,-38.2287856282417,
20.5166624581554));
#33662=CARTESIAN_POINT('Ctrl Pts',(-9.31505042551913,-38.3291439555038,
20.4929438817597));
#33663=CARTESIAN_POINT('Ctrl Pts',(-9.56130054585836,-38.3704502663933,
20.4769745507221));
#33664=CARTESIAN_POINT('Ctrl Pts',(-9.86061079356185,-38.3872639936425,
20.4587511193313));
#33665=CARTESIAN_POINT('Ctrl Pts',(-9.91140033374375,-38.3889728872996,
20.455696094601));
#33666=CARTESIAN_POINT('Ctrl Pts',(-9.99215996494449,-38.3898732474655,
20.4508955534453));
#33667=CARTESIAN_POINT('Ctrl Pts',(-10.0221124866583,-38.389810204744,20.4491275693709));
#33668=CARTESIAN_POINT('Ctrl Pts',(-10.0785643457313,-38.3889430948752,
20.4458178786924));
#33669=CARTESIAN_POINT('Ctrl Pts',(-10.1050625594161,-38.3882251362819,
20.4442736520243));
#33670=CARTESIAN_POINT('Ctrl Pts',(-10.1652907692601,-38.3858860240237,
20.4407837667086));
#33671=CARTESIAN_POINT('Ctrl Pts',(-10.1990107043103,-38.384071521527,20.4388441839593));
#33672=CARTESIAN_POINT('Ctrl Pts',(-10.3048986162235,-38.3767853637381,
20.4327940403518));
#33673=CARTESIAN_POINT('Ctrl Pts',(-10.3769239266166,-38.3695061849631,
20.4287385149376));
#33674=CARTESIAN_POINT('Ctrl Pts',(-10.5498090115357,-38.3464201319128,
20.4191023404541));
#33675=CARTESIAN_POINT('Ctrl Pts',(-10.6502960138072,-38.3283531406261,
20.4135840059501));
#33676=CARTESIAN_POINT('Ctrl Pts',(-10.7967287142194,-38.295139165467,20.4055517842023));
#33677=CARTESIAN_POINT('Ctrl Pts',(-10.843406787834,-38.2835017663891,20.4029923955733));
#33678=CARTESIAN_POINT('Ctrl Pts',(-11.0919051537793,-38.2158992789203,
20.3893191280384));
#33679=CARTESIAN_POINT('Ctrl Pts',(-11.2884395632971,-38.142319548116,20.3783583074076));
#33680=CARTESIAN_POINT('Ctrl Pts',(-11.5181487604185,-38.0311266306934,
20.3641016456152));
#33681=CARTESIAN_POINT('Ctrl Pts',(-11.5589778005654,-38.0103308972074,
20.3615073647234));
#33682=CARTESIAN_POINT('Ctrl Pts',(-11.6156935357303,-37.9799802336969,
20.3578010037077));
#33683=CARTESIAN_POINT('Ctrl Pts',(-11.6319440950488,-37.9711119521423,
20.3567269650976));
#33684=CARTESIAN_POINT('Ctrl Pts',(-11.661296218146,-37.9547804098513,20.354763543297));
#33685=CARTESIAN_POINT('Ctrl Pts',(-11.6744223805344,-37.9473618849605,
20.3538768664203));
#33686=CARTESIAN_POINT('Ctrl Pts',(-11.702029753591,-37.9315150528478,20.3519928890465));
#33687=CARTESIAN_POINT('Ctrl Pts',(-11.7164984827113,-37.9230666635997,
20.3509944281097));
#33688=CARTESIAN_POINT('Ctrl Pts',(-11.7561780687489,-37.8995012946895,
20.3482268092283));
#33689=CARTESIAN_POINT('Ctrl Pts',(-11.7812552597969,-37.8841634384853,
20.346444696278));
#33690=CARTESIAN_POINT('Ctrl Pts',(-11.8376694057658,-37.8486427316393,
20.3423657172438));
#33691=CARTESIAN_POINT('Ctrl Pts',(-11.8688790736459,-37.8282653787377,
20.3400591758521));
#33692=CARTESIAN_POINT('Ctrl Pts',(-11.9712615007684,-37.7589834744033,
20.3323409508029));
#33693=CARTESIAN_POINT('Ctrl Pts',(-12.0408989220013,-37.7078758753492,
20.3268437335704));
#33694=CARTESIAN_POINT('Ctrl Pts',(-12.3326375227201,-37.4761150116692,
20.3029432463605));
#33695=CARTESIAN_POINT('Ctrl Pts',(-12.533357563899,-37.2703509316107,20.2843462311002));
#33696=CARTESIAN_POINT('Ctrl Pts',(-12.737328507536,-37.0000430749118,20.2636622936412));
#33697=CARTESIAN_POINT('Ctrl Pts',(-12.7678580124946,-36.9575755757717,
20.2605031129089));
#33698=CARTESIAN_POINT('Ctrl Pts',(-12.8159836261468,-36.8872532201749,
20.2554151089511));
#33699=CARTESIAN_POINT('Ctrl Pts',(-12.8341770862056,-36.8598195768509,
20.2534644572795));
#33700=CARTESIAN_POINT('Ctrl Pts',(-12.8662568969194,-36.8098826812721,
20.2499736942696));
#33701=CARTESIAN_POINT('Ctrl Pts',(-12.8802848339037,-36.7874739867632,
20.2484284903702));
#33702=CARTESIAN_POINT('Ctrl Pts',(-12.9099403627754,-36.7388454965389,
20.2451196653981));
#33703=CARTESIAN_POINT('Ctrl Pts',(-12.925478940079,-36.7125739792878,20.2433593357253));
#33704=CARTESIAN_POINT('Ctrl Pts',(-12.9680067176365,-36.6384027527018,
20.238462512425));
#33705=CARTESIAN_POINT('Ctrl Pts',(-12.9941891622714,-36.5900500584078,
20.2353543111342));
#33706=CARTESIAN_POINT('Ctrl Pts',(-13.0509083310789,-36.4789294992827,
20.2283823441658));
#33707=CARTESIAN_POINT('Ctrl Pts',(-13.0807062230327,-36.4158121555035,
20.2245422924027));
#33708=CARTESIAN_POINT('Ctrl Pts',(-13.2089862089231,-36.1208292940687,
20.2070443581614));
#33709=CARTESIAN_POINT('Ctrl Pts',(-13.2833725401939,-35.8793792505666,
20.1940356182472));
#33710=CARTESIAN_POINT('Ctrl Pts',(-13.3487487639202,-35.534838357255,20.1750619076463));
#33711=CARTESIAN_POINT('Ctrl Pts',(-13.3629151346599,-35.4369998758927,
20.1696206628712));
#33712=CARTESIAN_POINT('Ctrl Pts',(-13.3754286172593,-35.3123869531831,
20.1624712441341));
#33713=CARTESIAN_POINT('Ctrl Pts',(-13.3777621711456,-35.2860534602704,
20.1609480529267));
#33714=CARTESIAN_POINT('Ctrl Pts',(-13.381022401637,-35.2436235590546,20.1584701245838));
#33715=CARTESIAN_POINT('Ctrl Pts',(-13.3821427005456,-35.2275426304932,
20.1575255239153));
#33716=CARTESIAN_POINT('Ctrl Pts',(-13.3840196643209,-35.1975123351502,
20.1557503303104));
#33717=CARTESIAN_POINT('Ctrl Pts',(-13.3848048732879,-35.1835651354541,
20.154921322793));
#33718=CARTESIAN_POINT('Ctrl Pts',(-13.3862870557921,-35.1539806745553,
20.1531537799897));
#33719=CARTESIAN_POINT('Ctrl Pts',(-13.3869619695638,-35.1383425771513,
20.1522141047543));
#33720=CARTESIAN_POINT('Ctrl Pts',(-13.3889969388095,-35.0821610184463,
20.1488202887959));
#33721=CARTESIAN_POINT('Ctrl Pts',(-13.3897374162124,-35.0416003335705,
20.1463365969691));
#33722=CARTESIAN_POINT('Ctrl Pts',(-13.3897498409715,-35.0010383320299,
20.1438256239882));
#33723=CARTESIAN_POINT('Ctrl Pts',(-13.3897498397764,-35.0010422262792,
20.1438258650599));
#33724=CARTESIAN_POINT('Ctrl Pts',(-13.389821234382,-34.7688375145137,20.1294513438218));
#33725=CARTESIAN_POINT('Ctrl Pts',(-13.3660333076597,-34.5372390899468,
20.1142711274129));
#33726=CARTESIAN_POINT('Ctrl Pts',(-13.2845988396862,-34.1456188175152,
20.0886397868102));
#33727=CARTESIAN_POINT('Ctrl Pts',(-13.2382874513302,-33.9840947286066,
20.0780693460874));
#33728=CARTESIAN_POINT('Ctrl Pts',(-13.17971517951,-33.8253432955754,20.0677787655689));
#33729=CARTESIAN_POINT('Ctrl Pts',(-13.1792330523841,-33.8240390335285,
20.0676942263837));
#33730=CARTESIAN_POINT('Ctrl Pts',(-13.1787501240278,-33.8227350716626,
20.0676097122989));
#33731=CARTESIAN_POINT('Ctrl Pts',(-13.1787501237351,-33.8227350708723,
20.4156322019944));
#33732=CARTESIAN_POINT('Ctrl Pts',(-13.1797424235209,-33.8254143939277,
20.4158106848247));
#33733=CARTESIAN_POINT('Ctrl Pts',(-13.1807313585004,-33.8280950329722,
20.4159890846477));
#33734=CARTESIAN_POINT('Ctrl Pts',(-13.2150215335141,-33.921406256347,20.4221931120437));
#33735=CARTESIAN_POINT('Ctrl Pts',(-13.244440856324,-34.0134229941018,20.4281139314852));
#33736=CARTESIAN_POINT('Ctrl Pts',(-13.2797552385806,-34.1426723325319,
20.4361575738012));
#33737=CARTESIAN_POINT('Ctrl Pts',(-13.2890192513423,-34.1789289390912,
20.4383850332551));
#33738=CARTESIAN_POINT('Ctrl Pts',(-13.3039345352182,-34.2416126379442,
20.4421878980678));
#33739=CARTESIAN_POINT('Ctrl Pts',(-13.3098734955927,-34.2679670021105,
20.4437722436665));
#33740=CARTESIAN_POINT('Ctrl Pts',(-13.32139648777,-34.3221108660603,20.4469985481911));
#33741=CARTESIAN_POINT('Ctrl Pts',(-13.3269482992382,-34.3499050900237,
20.4486393834504));
#33742=CARTESIAN_POINT('Ctrl Pts',(-13.3402905217088,-34.4213546115755,
20.4528199944899));
#33743=CARTESIAN_POINT('Ctrl Pts',(-13.3475742324,-34.4650997574206,20.4553439052827));
#33744=CARTESIAN_POINT('Ctrl Pts',(-13.3779360975941,-34.6724903830181,
20.4671585580073));
#33745=CARTESIAN_POINT('Ctrl Pts',(-13.3898865545848,-34.8375436181589,
20.4761050069103));
#33746=CARTESIAN_POINT('Ctrl Pts',(-13.3895661459623,-35.2220415882748,
20.4966099349805));
#33747=CARTESIAN_POINT('Ctrl Pts',(-13.3681189732072,-35.4407059894748,
20.5080097651198));
#33748=CARTESIAN_POINT('Ctrl Pts',(-13.3135660392957,-35.7173776565305,
20.5235638768887));
#33749=CARTESIAN_POINT('Ctrl Pts',(-13.299704827826,-35.7786511828263,20.5270843393847));
#33750=CARTESIAN_POINT('Ctrl Pts',(-13.2784570121082,-35.8617732784254,
20.5320069342596));
#33751=CARTESIAN_POINT('Ctrl Pts',(-13.272537286335,-35.8839871102126,20.5333369757181));
#33752=CARTESIAN_POINT('Ctrl Pts',(-13.2623153201382,-35.9208346303501,
20.5355699921975));
#33753=CARTESIAN_POINT('Ctrl Pts',(-13.2581393019259,-35.9355030442002,
20.5364660398317));
#33754=CARTESIAN_POINT('Ctrl Pts',(-13.2492696351486,-35.9658781587236,
20.5383372406426));
#33755=CARTESIAN_POINT('Ctrl Pts',(-13.2445608352887,-35.9815797170145,
20.5393131670107));
#33756=CARTESIAN_POINT('Ctrl Pts',(-13.2315887423729,-36.0237219589988,
20.5419546928587));
#33757=CARTESIAN_POINT('Ctrl Pts',(-13.2231150762426,-36.0500959705038,
20.5436314513064));
#33758=CARTESIAN_POINT('Ctrl Pts',(-13.1716747087254,-36.2037113325952,
20.5535243483592));
#33759=CARTESIAN_POINT('Ctrl Pts',(-13.1215031014286,-36.3284025082254,
20.5620612116359));
#33760=CARTESIAN_POINT('Ctrl Pts',(-12.9399339258703,-36.7121453464489,
20.5893258653224));
#33761=CARTESIAN_POINT('Ctrl Pts',(-12.7825810609813,-36.9575371546396,
20.6081403924394));
#33762=CARTESIAN_POINT('Ctrl Pts',(-12.5628266413932,-37.2192258679611,
20.6289125791546));
#33763=CARTESIAN_POINT('Ctrl Pts',(-12.5289008953034,-37.257809677729,20.6320007408338));
#33764=CARTESIAN_POINT('Ctrl Pts',(-12.4739362530422,-37.3175270977966,
20.6368235108994));
#33765=CARTESIAN_POINT('Ctrl Pts',(-12.4534741776545,-37.3391786972222,
20.6385814941019));
#33766=CARTESIAN_POINT('Ctrl Pts',(-12.4142509870333,-37.3796010786396,
20.6418825939049));
#33767=CARTESIAN_POINT('Ctrl Pts',(-12.3955497982724,-37.3984266394473,
20.6434280795951));
#33768=CARTESIAN_POINT('Ctrl Pts',(-12.3523587219765,-37.4408957534412,
20.6469344879373));
#33769=CARTESIAN_POINT('Ctrl Pts',(-12.3277296834012,-37.4643940993537,
20.6488891045618));
#33770=CARTESIAN_POINT('Ctrl Pts',(-12.2484683858948,-37.5377680256003,
20.6550437536267));
#33771=CARTESIAN_POINT('Ctrl Pts',(-12.1925539232534,-37.5862298832706,
20.6591858792891));
#33772=CARTESIAN_POINT('Ctrl Pts',(-12.0532865343691,-37.6991690574091,
20.6690827226406));
#33773=CARTESIAN_POINT('Ctrl Pts',(-11.9684264437239,-37.7616658990211,
20.6747701365353));
#33774=CARTESIAN_POINT('Ctrl Pts',(-11.7775230978549,-37.8889832016795,
20.6870305484804));
#33775=CARTESIAN_POINT('Ctrl Pts',(-11.6705517284192,-37.9521296165816,
20.6935702853099));
#33776=CARTESIAN_POINT('Ctrl Pts',(-11.4319126876795,-38.0758681851275,
20.7078772969879));
#33777=CARTESIAN_POINT('Ctrl Pts',(-11.2993461803352,-38.1341714628078,
20.7156537544188));
#33778=CARTESIAN_POINT('Ctrl Pts',(-11.1299937593077,-38.1960584916601,
20.725834478796));
#33779=CARTESIAN_POINT('Ctrl Pts',(-11.0963226753759,-38.2077643552676,
20.7278705781836));
#33780=CARTESIAN_POINT('Ctrl Pts',(-11.04534786445,-38.2245896156921,20.7309796358504));
#33781=CARTESIAN_POINT('Ctrl Pts',(-11.0281766202933,-38.2301057495256,
20.7320314441309));
#33782=CARTESIAN_POINT('Ctrl Pts',(-10.9966993173681,-38.2399411779736,
20.7339691389511));
#33783=CARTESIAN_POINT('Ctrl Pts',(-10.9824075572206,-38.2443032735718,
20.7348526163829));
#33784=CARTESIAN_POINT('Ctrl Pts',(-10.9491168111755,-38.2542240528466,
20.736918975448));
#33785=CARTESIAN_POINT('Ctrl Pts',(-10.9300975247785,-38.2597109473222,
20.7381057197938));
#33786=CARTESIAN_POINT('Ctrl Pts',(-10.8673802098969,-38.2772107722701,
20.7420369952975));
#33787=CARTESIAN_POINT('Ctrl Pts',(-10.8234909448036,-38.2885135117182,
20.7448165165827));
#33788=CARTESIAN_POINT('Ctrl Pts',(-10.7142562356151,-38.314320803047,20.7517828237837));
#33789=CARTESIAN_POINT('Ctrl Pts',(-10.6486835175387,-38.327776005892,20.7560069176683));
#33790=CARTESIAN_POINT('Ctrl Pts',(-10.3067826126751,-38.3874433044256,
20.7781167557791));
#33791=CARTESIAN_POINT('Ctrl Pts',(-10.0258504827591,-38.4012138276423,
20.7964513705028));
#33792=CARTESIAN_POINT('Ctrl Pts',(-9.66575347564894,-38.3742004447113,
20.8188363146694));
#33793=CARTESIAN_POINT('Ctrl Pts',(-9.58532116182324,-38.3652626159723,
20.8237735646167));
#33794=CARTESIAN_POINT('Ctrl Pts',(-9.47304950182729,-38.3486996992343,
20.8305771750314));
#33795=CARTESIAN_POINT('Ctrl Pts',(-9.44088800875054,-38.3434802819212,
20.8325160494675));
#33796=CARTESIAN_POINT('Ctrl Pts',(-9.38225346324154,-38.33309487243,20.8360333705681));
#33797=CARTESIAN_POINT('Ctrl Pts',(-9.35575754640354,-38.3280751097144,
20.8376162176144));
#33798=CARTESIAN_POINT('Ctrl Pts',(-9.30195380167332,-38.3172151275187,
20.8408179705861));
#33799=CARTESIAN_POINT('Ctrl Pts',(-9.2746525696217,-38.3113525741656,20.8424360414151));
#33800=CARTESIAN_POINT('Ctrl Pts',(-9.20621416126245,-38.2957693488341,
20.8464773583752));
#33801=CARTESIAN_POINT('Ctrl Pts',(-9.16517995368286,-38.2856152044868,
20.8488868384231));
#33802=CARTESIAN_POINT('Ctrl Pts',(-8.98473369464489,-38.2373638059727,
20.8594356288459));
#33803=CARTESIAN_POINT('Ctrl Pts',(-8.84764516355096,-38.1911400024787,
20.8673170334236));
#33804=CARTESIAN_POINT('Ctrl Pts',(-8.59149612605775,-38.0861024177645,
20.8821582104425));
#33805=CARTESIAN_POINT('Ctrl Pts',(-8.47212062560268,-38.0287780253845,
20.8891284860037));
#33806=CARTESIAN_POINT('Ctrl Pts',(-8.224351938089,-37.8914141523077,20.9041912290463));
#33807=CARTESIAN_POINT('Ctrl Pts',(-8.09735267827896,-37.8094708373664,
20.912286788813));
#33808=CARTESIAN_POINT('Ctrl Pts',(-7.94737564428935,-37.6978572712773,
20.9228388833352));
#33809=CARTESIAN_POINT('Ctrl Pts',(-7.91884593000181,-37.6759107089597,
20.9248941885139));
#33810=CARTESIAN_POINT('Ctrl Pts',(-7.8765007992569,-37.6422497880646,20.9280267388225));
#33811=CARTESIAN_POINT('Ctrl Pts',(-7.862420122644,-37.6308715350572,20.9290823542122));
#33812=CARTESIAN_POINT('Ctrl Pts',(-7.83699970722492,-37.6099911226178,
20.9310150389804));
#33813=CARTESIAN_POINT('Ctrl Pts',(-7.82563006605457,-37.6005267335806,
20.9318895306533));
#33814=CARTESIAN_POINT('Ctrl Pts',(-7.799327871552,-37.5783390183394,20.9339359794902));
#33815=CARTESIAN_POINT('Ctrl Pts',(-7.78444349625642,-37.5655602211776,
20.9351117428707));
#33816=CARTESIAN_POINT('Ctrl Pts',(-7.73633303353773,-37.5235246861547,
20.9389677481076));
#33817=CARTESIAN_POINT('Ctrl Pts',(-7.70357027040226,-37.4937471961838,
20.9416812438432));
#33818=CARTESIAN_POINT('Ctrl Pts',(-7.62434280108415,-37.4188533207945,
20.9484424817542));
#33819=CARTESIAN_POINT('Ctrl Pts',(-7.57857052049581,-37.3730311736921,
20.9525249925178));
#33820=CARTESIAN_POINT('Ctrl Pts',(-7.3604677212843,-37.1418070952463,20.9727533046572));
#33821=CARTESIAN_POINT('Ctrl Pts',(-7.20794170573196,-36.9387879661309,
20.9893089686952));
#33822=CARTESIAN_POINT('Ctrl Pts',(-7.02672877305157,-36.6312102281304,
21.0116773367356));
#33823=CARTESIAN_POINT('Ctrl Pts',(-6.97815184977662,-36.5393588630552,
21.018067453703));
#33824=CARTESIAN_POINT('Ctrl Pts',(-6.91707256867729,-36.4097923364397,
21.0266843595967));
#33825=CARTESIAN_POINT('Ctrl Pts',(-6.90090148345945,-36.3738793832178,
21.0290326290667));
#33826=CARTESIAN_POINT('Ctrl Pts',(-6.87466876944409,-36.3127999263316,
21.0329607685183));
#33827=CARTESIAN_POINT('Ctrl Pts',(-6.8642767216079,-36.287780467368,21.0345515520571));
#33828=CARTESIAN_POINT('Ctrl Pts',(-6.8438458292439,-36.2368776995388,21.0377521993739));
#33829=CARTESIAN_POINT('Ctrl Pts',(-6.83382277271924,-36.2109902664664,
21.0393614437692));
#33830=CARTESIAN_POINT('Ctrl Pts',(-6.8096313074882,-36.1461544965799,21.043347608061));
#33831=CARTESIAN_POINT('Ctrl Pts',(-6.79585684569702,-36.1070634046308,
21.0457115686704));
#33832=CARTESIAN_POINT('Ctrl Pts',(-6.74055254072495,-35.9404246774226,
21.0556351117259));
#33833=CARTESIAN_POINT('Ctrl Pts',(-6.70589367841861,-35.8107188038258,
21.0629756613967));
#33834=CARTESIAN_POINT('Ctrl Pts',(-6.65116097682716,-35.5431351969952,
21.0776617444635));
#33835=CARTESIAN_POINT('Ctrl Pts',(-6.63171047904686,-35.4053950531635,
21.0849841031622));
#33836=CARTESIAN_POINT('Ctrl Pts',(-6.60843292257013,-35.1106220637268,
21.1006946879956));
#33837=CARTESIAN_POINT('Ctrl Pts',(-6.60694605196937,-34.9537408978524,
21.1090814540416));
#33838=CARTESIAN_POINT('Ctrl Pts',(-6.6184568825366,-34.7615546718182,21.1199501502817));
#33839=CARTESIAN_POINT('Ctrl Pts',(-6.62116740510742,-34.7258100813717,
21.1219972994564));
#33840=CARTESIAN_POINT('Ctrl Pts',(-6.62609648201241,-34.6721176903392,
21.125119874907));
#33841=CARTESIAN_POINT('Ctrl Pts',(-6.62789272521778,-34.6541326075708,
21.1261738757734));
#33842=CARTESIAN_POINT('Ctrl Pts',(-6.63143618344756,-34.6213100703901,
21.1281135060378));
#33843=CARTESIAN_POINT('Ctrl Pts',(-6.63313777459847,-34.6064685807681,
21.1289966895752));
#33844=CARTESIAN_POINT('Ctrl Pts',(-6.63731579869345,-34.5720399584068,
21.1310595589739));
#33845=CARTESIAN_POINT('Ctrl Pts',(-6.6398652989797,-34.5524627562589,21.1322430611186));
#33846=CARTESIAN_POINT('Ctrl Pts',(-6.6487874216445,-34.4883311560712,21.1361519951363));
#33847=CARTESIAN_POINT('Ctrl Pts',(-6.65587616557099,-34.4438830000727,
21.1389118971841));
#33848=CARTESIAN_POINT('Ctrl Pts',(-6.67558698498592,-34.3343603925951,
21.1458170409067));
#33849=CARTESIAN_POINT('Ctrl Pts',(-6.68923674053706,-34.2694907689832,
21.1499988242277));
#33850=CARTESIAN_POINT('Ctrl Pts',(-6.76844148015486,-33.9411649947635,
21.1715082441051));
#33851=CARTESIAN_POINT('Ctrl Pts',(-6.86358870626935,-33.6858247758495,
21.1892732232653));
#33852=CARTESIAN_POINT('Ctrl Pts',(-7.02872066587874,-33.3660755931273,
21.2116608912612));
#33853=CARTESIAN_POINT('Ctrl Pts',(-7.07231429488231,-33.2891907265559,
21.2170667399001));
#33854=CARTESIAN_POINT('Ctrl Pts',(-7.13841167655764,-33.1825584685678,
21.2245956565906));
#33855=CARTESIAN_POINT('Ctrl Pts',(-7.15847479032698,-33.1513474907533,
21.2268035569805));
#33856=CARTESIAN_POINT('Ctrl Pts',(-7.19399589927461,-33.098034455884,21.2305837155766));
#33857=CARTESIAN_POINT('Ctrl Pts',(-7.20921239205201,-33.0757763814661,
21.2321646340288));
#33858=CARTESIAN_POINT('Ctrl Pts',(-7.24102482853563,-33.03041371838,21.2353931999895));
#33859=CARTESIAN_POINT('Ctrl Pts',(-7.25764932291308,-33.007331700204,21.2370396057097));
#33860=CARTESIAN_POINT('Ctrl Pts',(-7.30122555589158,-32.9484073644773,
21.2412538616494));
#33861=CARTESIAN_POINT('Ctrl Pts',(-7.32860195801543,-32.9128850994988,
21.2438053259418));
#33862=CARTESIAN_POINT('Ctrl Pts',(-7.47836403436166,-32.7263375614643,
21.2572837640717));
#33863=CARTESIAN_POINT('Ctrl Pts',(-7.61286865388196,-32.5855013357581,
21.2677155456504));
#33864=CARTESIAN_POINT('Ctrl Pts',(-7.91274481328573,-32.3212085415871,
21.2889430882737));
#33865=CARTESIAN_POINT('Ctrl Pts',(-8.07877354977005,-32.1997442559754,
21.2996877185417));
#33866=CARTESIAN_POINT('Ctrl Pts',(-8.29808102172875,-32.0680328262602,
21.3139243093506));
#33867=CARTESIAN_POINT('Ctrl Pts',(-8.34198504788414,-32.0429836677071,
21.3167776545881));
#33868=CARTESIAN_POINT('Ctrl Pts',(-8.40512137217996,-32.0088097791362,
21.3209087969181));
#33869=CARTESIAN_POINT('Ctrl Pts',(-8.42390673970332,-31.998869086536,21.3221413959815));
#33870=CARTESIAN_POINT('Ctrl Pts',(-8.4562049603431,-31.9821646421291,21.3242685907873));
#33871=CARTESIAN_POINT('Ctrl Pts',(-8.46967166931177,-31.9753134764087,
21.3251578984764));
#33872=CARTESIAN_POINT('Ctrl Pts',(-8.49852202645079,-31.9608779061521,
21.3270688328802));
#33873=CARTESIAN_POINT('Ctrl Pts',(-8.5139174609892,-31.9533201898323,21.3280918680074));
#33874=CARTESIAN_POINT('Ctrl Pts',(-8.55754828394438,-31.9323109212226,
21.3309990539693));
#33875=CARTESIAN_POINT('Ctrl Pts',(-8.58591273040245,-31.9191331933119,
21.3328982757617));
#33876=CARTESIAN_POINT('Ctrl Pts',(-8.76875066305002,-31.8372459939738,
21.3451809033527));
#33877=CARTESIAN_POINT('Ctrl Pts',(-8.9279881005379,-31.7797874663349,21.3560484720248));
#33878=CARTESIAN_POINT('Ctrl Pts',(-9.33064306543395,-31.667683375062,21.3829872596265));
#33879=CARTESIAN_POINT('Ctrl Pts',(-9.57711889399226,-31.6275259536363,
21.3989589344847));
#33880=CARTESIAN_POINT('Ctrl Pts',(-9.8765360968515,-31.6121182134518,21.4171842130132));
#33881=CARTESIAN_POINT('Ctrl Pts',(-9.92732938377889,-31.6106481836983,
21.4202390070607));
#33882=CARTESIAN_POINT('Ctrl Pts',(-10.008087806878,-31.610127341894,21.4250392711657));
#33883=CARTESIAN_POINT('Ctrl Pts',(-10.0380388796514,-31.6103311104707,
21.4268072045195));
#33884=CARTESIAN_POINT('Ctrl Pts',(-10.0944853168803,-31.6114634151667,
21.4301168491632));
#33885=CARTESIAN_POINT('Ctrl Pts',(-10.1209799618856,-31.6123058624658,
21.4316610797822));
#33886=CARTESIAN_POINT('Ctrl Pts',(-10.1811978643435,-31.6149279735065,
21.4351510392527));
#33887=CARTESIAN_POINT('Ctrl Pts',(-10.214910150706,-31.6169009717589,21.4370906911254));
#33888=CARTESIAN_POINT('Ctrl Pts',(-10.3207713096603,-31.624685288591,21.4431413193169));
#33889=CARTESIAN_POINT('Ctrl Pts',(-10.3927689855877,-31.6323038770644,
21.4471972469665));
#33890=CARTESIAN_POINT('Ctrl Pts',(-10.5655658827432,-31.6562063501155,
21.4568346261945));
#33891=CARTESIAN_POINT('Ctrl Pts',(-10.6659815489268,-31.6747494525009,
21.4623537406012));
#33892=CARTESIAN_POINT('Ctrl Pts',(-10.8123115190576,-31.7086670178691,
21.4703889722032));
#33893=CARTESIAN_POINT('Ctrl Pts',(-10.8589746217431,-31.720535790954,21.4729505707608));
#33894=CARTESIAN_POINT('Ctrl Pts',(-11.1073057613315,-31.7893630352085,
21.486632408585));
#33895=CARTESIAN_POINT('Ctrl Pts',(-11.3035978550968,-31.863930491877,21.4975995931196));
#33896=CARTESIAN_POINT('Ctrl Pts',(-11.5327556708386,-31.9762353780533,
21.5118573801948));
#33897=CARTESIAN_POINT('Ctrl Pts',(-11.5733689209364,-31.9971676269638,
21.5144445463399));
#33898=CARTESIAN_POINT('Ctrl Pts',(-11.6298068361418,-32.0277152434651,
21.5181423536427));
#33899=CARTESIAN_POINT('Ctrl Pts',(-11.6459963162013,-32.0366500221665,
21.5192151827082));
#33900=CARTESIAN_POINT('Ctrl Pts',(-11.675378410593,-32.0531807032142,21.5211858768225));
#33901=CARTESIAN_POINT('Ctrl Pts',(-11.6885946907965,-32.060733977467,21.5220811588593));
#33902=CARTESIAN_POINT('Ctrl Pts',(-11.7163085137288,-32.0768213978027,
21.5239779974719));
#33903=CARTESIAN_POINT('Ctrl Pts',(-11.7307939268888,-32.0853747392143,
21.5249806542448));
#33904=CARTESIAN_POINT('Ctrl Pts',(-11.7706878609703,-32.1093335582906,
21.5277719296868));
#33905=CARTESIAN_POINT('Ctrl Pts',(-11.7959578097172,-32.1249654970002,
21.5295738524112));
#33906=CARTESIAN_POINT('Ctrl Pts',(-11.9731265290204,-32.2378088681751,
21.5424306498272));
#33907=CARTESIAN_POINT('Ctrl Pts',(-12.1172483973595,-32.3466669134747,
21.5540478761972));
#33908=CARTESIAN_POINT('Ctrl Pts',(-12.4303626577193,-32.6249880504184,
21.5810525332624));
#33909=CARTESIAN_POINT('Ctrl Pts',(-12.5914987687936,-32.8019301407458,
21.5963332882119));
#33910=CARTESIAN_POINT('Ctrl Pts',(-12.7633592544891,-33.036092859493,21.6140032734572));
#33911=CARTESIAN_POINT('Ctrl Pts',(-12.7930338605456,-33.0785297499357,
21.6171180454524));
#33912=CARTESIAN_POINT('Ctrl Pts',(-12.8384373410203,-33.1467358479106,
21.6219899861644));
#33913=CARTESIAN_POINT('Ctrl Pts',(-12.8548133696525,-33.1720625643064,
21.6237707702938));
#33914=CARTESIAN_POINT('Ctrl Pts',(-12.8835193579078,-33.2177853828403,
21.6269364457863));
#33915=CARTESIAN_POINT('Ctrl Pts',(-12.8959761784949,-33.2380990818352,
21.628325879629));
#33916=CARTESIAN_POINT('Ctrl Pts',(-12.9247252436309,-33.2861097653666,
21.6315709493723));
#33917=CARTESIAN_POINT('Ctrl Pts',(-12.9408400705193,-33.3139106582638,
21.6334201626978));
#33918=CARTESIAN_POINT('Ctrl Pts',(-12.9875015230559,-33.3971145452151,
21.6388701299844));
#33919=CARTESIAN_POINT('Ctrl Pts',(-13.0168959875074,-33.4531495120161,
21.6424308683072));
#33920=CARTESIAN_POINT('Ctrl Pts',(-13.09460618968,-33.611942182526,21.6522535415147));
#33921=CARTESIAN_POINT('Ctrl Pts',(-13.1393414202323,-33.7163270668683,
21.6584041337633));
#33922=CARTESIAN_POINT('Ctrl Pts',(-13.1787500936073,-33.8227349895238,
21.6644775413951));
#33923=CARTESIAN_POINT('Origin',(-10.,-35.,23.));
#33924=CARTESIAN_POINT('',(-13.1787501240204,-33.8227350716428,22.9104831197053));
#33925=CARTESIAN_POINT('',(-13.1787501379842,-33.8227351093465,22.5700367124769));
#33926=CARTESIAN_POINT('',(-13.1787501240207,-33.8227350716434,23.));
#33927=CARTESIAN_POINT('Ctrl Pts',(-13.1787501379842,-33.8227351093465,
22.5700367124769));
#33928=CARTESIAN_POINT('Ctrl Pts',(-13.1376176986524,-33.711672808721,22.563741246396));
#33929=CARTESIAN_POINT('Ctrl Pts',(-13.0906853862704,-33.6028221111455,
22.5574976443462));
#33930=CARTESIAN_POINT('Ctrl Pts',(-12.9793754110903,-33.3778768480948,
22.5440690148351));
#33931=CARTESIAN_POINT('Ctrl Pts',(-12.9137041264173,-33.2626794508871,
22.5368727854472));
#33932=CARTESIAN_POINT('Ctrl Pts',(-12.8264011327451,-33.128469811955,22.5277475901435));
#33933=CARTESIAN_POINT('Ctrl Pts',(-12.8110515889448,-33.1054928164769,
22.5261575527729));
#33934=CARTESIAN_POINT('Ctrl Pts',(-12.7861599442011,-33.0692006692235,
22.5235971835025));
#33935=CARTESIAN_POINT('Ctrl Pts',(-12.7767989417492,-33.0557621279459,
22.5226382308669));
#33936=CARTESIAN_POINT('Ctrl Pts',(-12.7585282543424,-33.0299340604824,
22.5207729722818));
#33937=CARTESIAN_POINT('Ctrl Pts',(-12.749631677789,-33.0175359926719,22.5198674993266));
#33938=CARTESIAN_POINT('Ctrl Pts',(-12.7270964442602,-32.9865748962383,
22.5175816295615));
#33939=CARTESIAN_POINT('Ctrl Pts',(-12.7133518333218,-32.968090201426,22.5161944028187));
#33940=CARTESIAN_POINT('Ctrl Pts',(-12.6612222251301,-32.8994548846264,
22.5109631377593));
#33941=CARTESIAN_POINT('Ctrl Pts',(-12.6216284478103,-32.8502426255418,
22.5070497055591));
#33942=CARTESIAN_POINT('Ctrl Pts',(-12.3878900997955,-32.575787906325,22.484408035944));
#33943=CARTESIAN_POINT('Ctrl Pts',(-12.1661413279739,-32.3757504411427,
22.4648031407634));
#33944=CARTESIAN_POINT('Ctrl Pts',(-11.8647312001848,-32.1684164322998,
22.4419289575259));
#33945=CARTESIAN_POINT('Ctrl Pts',(-11.8071866185858,-32.1313478058999,
22.4377009266429));
#33946=CARTESIAN_POINT('Ctrl Pts',(-11.7021411727101,-32.0680968746584,
22.4302316393656));
#33947=CARTESIAN_POINT('Ctrl Pts',(-11.6550608448305,-32.0412646934652,
22.4269692887427));
#33948=CARTESIAN_POINT('Ctrl Pts',(-11.5806252426908,-32.0011751200555,
22.4219405041543));
#33949=CARTESIAN_POINT('Ctrl Pts',(-11.5537022595429,-31.9871382048065,
22.4201472123033));
#33950=CARTESIAN_POINT('Ctrl Pts',(-11.5029760807918,-31.9615517666286,
22.4168149269598));
#33951=CARTESIAN_POINT('Ctrl Pts',(-11.4792194034459,-31.9499156107942,
22.4152730391401));
#33952=CARTESIAN_POINT('Ctrl Pts',(-11.4253987337083,-31.9243306858185,
22.4118206763353));
#33953=CARTESIAN_POINT('Ctrl Pts',(-11.3952612695439,-31.9105422189353,
22.4099157474859));
#33954=CARTESIAN_POINT('Ctrl Pts',(-11.3019674795773,-31.8695021943585,
22.4041011236112));
#33955=CARTESIAN_POINT('Ctrl Pts',(-11.2381783226978,-31.843728282554,22.4002402748824));
#33956=CARTESIAN_POINT('Ctrl Pts',(-10.893496879008,-31.7165198661492,22.3798981167027));
#33957=CARTESIAN_POINT('Ctrl Pts',(-10.6009377597614,-31.6506056722566,
22.3645787437914));
#33958=CARTESIAN_POINT('Ctrl Pts',(-10.2356426849547,-31.6177634356753,
22.344741667329));
#33959=CARTESIAN_POINT('Ctrl Pts',(-10.1675852748959,-31.6137091251308,
22.3410096298109));
#33960=CARTESIAN_POINT('Ctrl Pts',(-10.053565861396,-31.6103623432665,22.3346314948549));
#33961=CARTESIAN_POINT('Ctrl Pts',(-10.0076557669188,-31.6099478305808,
22.3320292315965));
#33962=CARTESIAN_POINT('Ctrl Pts',(-9.94186130276043,-31.6106902301714,
22.3282333881118));
#33963=CARTESIAN_POINT('Ctrl Pts',(-9.92197169764219,-31.6110897966416,
22.3270771907272));
#33964=CARTESIAN_POINT('Ctrl Pts',(-9.88714251583776,-31.6120962552786,
22.3250355048485));
#33965=CARTESIAN_POINT('Ctrl Pts',(-9.87220163151213,-31.612626952792,22.3241541054779));
#33966=CARTESIAN_POINT('Ctrl Pts',(-9.83931643290485,-31.6140129134367,
22.3222014745032));
#33967=CARTESIAN_POINT('Ctrl Pts',(-9.82137534201628,-31.6149119717656,
22.3211280437448));
#33968=CARTESIAN_POINT('Ctrl Pts',(-9.76928420541067,-31.6179376080129,
22.317989383098));
#33969=CARTESIAN_POINT('Ctrl Pts',(-9.73515909739502,-31.6204386520451,
22.3159057471138));
#33970=CARTESIAN_POINT('Ctrl Pts',(-9.45373903072422,-31.6453523862283,
22.2985268603149));
#33971=CARTESIAN_POINT('Ctrl Pts',(-9.20956567706115,-31.6943582004883,
22.2822605001604));
#33972=CARTESIAN_POINT('Ctrl Pts',(-8.85983550571905,-31.8055490534237,
22.258763718696));
#33973=CARTESIAN_POINT('Ctrl Pts',(-8.74868598711848,-31.8474281753225,
22.251252866723));
#33974=CARTESIAN_POINT('Ctrl Pts',(-8.56652355707648,-31.9272199770638,
22.2389418655143));
#33975=CARTESIAN_POINT('Ctrl Pts',(-8.49425235966925,-31.9619813328979,
22.2340560959784));
#33976=CARTESIAN_POINT('Ctrl Pts',(-8.39225059753278,-32.0155778876293,
22.227157380898));
#33977=CARTESIAN_POINT('Ctrl Pts',(-8.36147799758298,-32.032361330629,22.2250755680216));
#33978=CARTESIAN_POINT('Ctrl Pts',(-8.30777079576461,-32.0627434840589,
22.221439913661));
#33979=CARTESIAN_POINT('Ctrl Pts',(-8.284726381506,-32.0761409072782,22.2198791812572));
#33980=CARTESIAN_POINT('Ctrl Pts',(-8.23672289347574,-32.1048117585278,
22.2166254201802));
#33981=CARTESIAN_POINT('Ctrl Pts',(-8.21179864953554,-32.1201393929929,
22.2149344972395));
#33982=CARTESIAN_POINT('Ctrl Pts',(-8.14584906974524,-32.1618826795923,
22.2104540432144));
#33983=CARTESIAN_POINT('Ctrl Pts',(-8.10518958857028,-32.1888650979512,
22.2076852277565));
#33984=CARTESIAN_POINT('Ctrl Pts',(-7.84382399588872,-32.3705604753737,
22.1898109435594));
#33985=CARTESIAN_POINT('Ctrl Pts',(-7.64166368014102,-32.5502434123526,
22.175723802859));
#33986=CARTESIAN_POINT('Ctrl Pts',(-7.3578104031017,-32.8705977040419,22.1529484125132));
#33987=CARTESIAN_POINT('Ctrl Pts',(-7.26116989790374,-32.9964234827058,
22.1444297194764));
#33988=CARTESIAN_POINT('Ctrl Pts',(-7.15801121976463,-33.1522143681483,
22.1337909986669));
#33989=CARTESIAN_POINT('Ctrl Pts',(-7.14262718598728,-33.1760941751605,
22.1321577443594));
#33990=CARTESIAN_POINT('Ctrl Pts',(-7.11876148391041,-33.2141827162502,
22.1295440559974));
#33991=CARTESIAN_POINT('Ctrl Pts',(-7.11008030176965,-33.2282655756924,
22.1285758346648));
#33992=CARTESIAN_POINT('Ctrl Pts',(-7.09363604649763,-33.2553843339179,
22.1267067536304));
#33993=CARTESIAN_POINT('Ctrl Pts',(-7.08585685595849,-33.268409703383,22.1258069157041));
#33994=CARTESIAN_POINT('Ctrl Pts',(-7.06857617134252,-33.2977905010256,
22.1237731504447));
#33995=CARTESIAN_POINT('Ctrl Pts',(-7.05912361379391,-33.3141741231999,
22.1226363025139));
#33996=CARTESIAN_POINT('Ctrl Pts',(-7.02601084463858,-33.3726927998073,
22.1185683067489));
#33997=CARTESIAN_POINT('Ctrl Pts',(-7.00311607546772,-33.4152519236794,
22.115596236862));
#33998=CARTESIAN_POINT('Ctrl Pts',(-6.88693653507092,-33.642744952137,22.0996944143998));
#33999=CARTESIAN_POINT('Ctrl Pts',(-6.80984180491637,-33.8354441446983,
22.0862029319513));
#34000=CARTESIAN_POINT('Ctrl Pts',(-6.70449611617657,-34.1897662310774,
22.0624657948694));
#34001=CARTESIAN_POINT('Ctrl Pts',(-6.6694358220799,-34.3487109761724,22.0521706120813));
#34002=CARTESIAN_POINT('Ctrl Pts',(-6.63673133105342,-34.5723810005353,
22.0383130559082));
#34003=CARTESIAN_POINT('Ctrl Pts',(-6.62931334434065,-34.6354366661849,
22.0344726589624));
#34004=CARTESIAN_POINT('Ctrl Pts',(-6.62081025148256,-34.7307107481719,
22.0287672340598));
#34005=CARTESIAN_POINT('Ctrl Pts',(-6.61840662364092,-34.7627946004006,
22.0268623701878));
#34006=CARTESIAN_POINT('Ctrl Pts',(-6.61501816603948,-34.8186964332337,
22.0235709215679));
#34007=CARTESIAN_POINT('Ctrl Pts',(-6.61382715518108,-34.8424991823737,
22.0221780984308));
#34008=CARTESIAN_POINT('Ctrl Pts',(-6.61169902960354,-34.8964176622354,
22.0190418353438));
#34009=CARTESIAN_POINT('Ctrl Pts',(-6.6109122000578,-34.9265375237965,22.0173031230613));
#34010=CARTESIAN_POINT('Ctrl Pts',(-6.60986689105551,-35.0082962245054,
22.012616958412));
#34011=CARTESIAN_POINT('Ctrl Pts',(-6.61038657672287,-35.0599379549259,
22.0096933305404));
#34012=CARTESIAN_POINT('Ctrl Pts',(-6.61999523229314,-35.3517658402121,
21.9933425233035));
#34013=CARTESIAN_POINT('Ctrl Pts',(-6.6534287301087,-35.5904602623956,21.9806847615013));
#34014=CARTESIAN_POINT('Ctrl Pts',(-6.75573419163348,-35.9988947511982,
21.95833983974));
#34015=CARTESIAN_POINT('Ctrl Pts',(-6.81357409613821,-36.1703531082455,
21.9487094528061));
#34016=CARTESIAN_POINT('Ctrl Pts',(-6.89611400993883,-36.362762611134,21.9367934717562));
#34017=CARTESIAN_POINT('Ctrl Pts',(-6.90777305965901,-36.3890149773763,
21.9351424287581));
#34018=CARTESIAN_POINT('Ctrl Pts',(-6.92669885405144,-36.4302101536988,
21.9325067943769));
#34019=CARTESIAN_POINT('Ctrl Pts',(-6.93374451162188,-36.4452537050986,
21.9315347656889));
#34020=CARTESIAN_POINT('Ctrl Pts',(-6.94742216941084,-36.4739073439134,
21.9296638825868));
#34021=CARTESIAN_POINT('Ctrl Pts',(-6.95403522431336,-36.487525738278,21.9287661255488));
#34022=CARTESIAN_POINT('Ctrl Pts',(-6.97064368655332,-36.5211527350863,
21.9265287657307));
#34023=CARTESIAN_POINT('Ctrl Pts',(-6.98074624347804,-36.5411073980275,
21.9251829280307));
#34024=CARTESIAN_POINT('Ctrl Pts',(-7.0179176497323,-36.6127601490116,21.9202883697684));
#34025=CARTESIAN_POINT('Ctrl Pts',(-7.04612164722486,-36.6638546475441,
21.9166807809232));
#34026=CARTESIAN_POINT('Ctrl Pts',(-7.17614792112779,-36.8856763746233,
21.9005752241649));
#34027=CARTESIAN_POINT('Ctrl Pts',(-7.29155253324919,-37.04798061258,21.8876309094508));
#34028=CARTESIAN_POINT('Ctrl Pts',(-7.44847768085481,-37.2320388334943,
21.872109708858));
#34029=CARTESIAN_POINT('Ctrl Pts',(-7.47707043848378,-37.2643078529894,
21.8693523126196));
#34030=CARTESIAN_POINT('Ctrl Pts',(-7.57490351605026,-37.3705651144733,
21.8601598026941));
#34031=CARTESIAN_POINT('Ctrl Pts',(-7.64684738181105,-37.4419965886759,
21.8537928539741));
#34032=CARTESIAN_POINT('Ctrl Pts',(-7.77521767097204,-37.5585025426337,
21.8431099084415));
#34033=CARTESIAN_POINT('Ctrl Pts',(-7.83007854770229,-37.6051936072031,
21.8387356304577));
#34034=CARTESIAN_POINT('Ctrl Pts',(-7.91273957331627,-37.6711205583938,
21.8324158928297));
#34035=CARTESIAN_POINT('Ctrl Pts',(-7.93940321835026,-37.6917433296695,
21.8304166645453));
#34036=CARTESIAN_POINT('Ctrl Pts',(-7.98757256395356,-37.727864212312,21.8268731254822));
#34037=CARTESIAN_POINT('Ctrl Pts',(-8.00896050673847,-37.7435140133772,
21.8253230582709));
#34038=CARTESIAN_POINT('Ctrl Pts',(-8.05493723459717,-37.7763348443081,
21.8220391954535));
#34039=CARTESIAN_POINT('Ctrl Pts',(-8.07957490053254,-37.7934337024044,
21.8203082055762));
#34040=CARTESIAN_POINT('Ctrl Pts',(-8.14670308686897,-37.8387135928312,
21.8156663631566));
#34041=CARTESIAN_POINT('Ctrl Pts',(-8.18960859901228,-37.8662672006653,
21.812778552512));
#34042=CARTESIAN_POINT('Ctrl Pts',(-8.44415559762776,-38.0217383655734,
21.796067227445));
#34043=CARTESIAN_POINT('Ctrl Pts',(-8.66865943771152,-38.1271549339003,
21.7830680071628));
#34044=CARTESIAN_POINT('Ctrl Pts',(-9.0162365776545,-38.2460787385525,21.7635625263914));
#34045=CARTESIAN_POINT('Ctrl Pts',(-9.13180257655126,-38.2788790223566,
21.757157668853));
#34046=CARTESIAN_POINT('Ctrl Pts',(-9.31376882354845,-38.3202293482322,
21.746882945748));
#34047=CARTESIAN_POINT('Ctrl Pts',(-9.37909662960953,-38.3330637553211,
21.7431565387111));
#34048=CARTESIAN_POINT('Ctrl Pts',(-9.46725425752513,-38.3477017776507,
21.7380276239211));
#34049=CARTESIAN_POINT('Ctrl Pts',(-9.48978960961286,-38.351210305986,21.73670780782));
#34050=CARTESIAN_POINT('Ctrl Pts',(-9.5275677849971,-38.3567021153977,21.7344781314196));
#34051=CARTESIAN_POINT('Ctrl Pts',(-9.54279225449063,-38.3588096640907,
21.733574921589));
#34052=CARTESIAN_POINT('Ctrl Pts',(-9.57439480773207,-38.3629656115988,
21.7316895338593));
#34053=CARTESIAN_POINT('Ctrl Pts',(-9.59077424765902,-38.3649980301599,
21.7307065962187));
#34054=CARTESIAN_POINT('Ctrl Pts',(-9.63520362093801,-38.3701818035246,
21.7280259940869));
#34055=CARTESIAN_POINT('Ctrl Pts',(-9.66327853207224,-38.3731024779914,
21.7263166255495));
#34056=CARTESIAN_POINT('Ctrl Pts',(-9.83078526454199,-38.3884164612281,
21.7160384550533));
#34057=CARTESIAN_POINT('Ctrl Pts',(-9.97082841551456,-38.3925125819555,
21.7071234683187));
#34058=CARTESIAN_POINT('Ctrl Pts',(-10.3105953595599,-38.3814098703585,
21.6852711138366));
#34059=CARTESIAN_POINT('Ctrl Pts',(-10.5095286513717,-38.3572003441564,
21.6723096346984));
#34060=CARTESIAN_POINT('Ctrl Pts',(-10.8113704460571,-38.293003325,21.6529509665439));
#34061=CARTESIAN_POINT('Ctrl Pts',(-10.916428042639,-38.2653263801649,21.6462660008175));
#34062=CARTESIAN_POINT('Ctrl Pts',(-11.0570823376647,-38.2209463248077,
21.6373978945339));
#34063=CARTESIAN_POINT('Ctrl Pts',(-11.0939766533955,-38.2086030553521,
21.6350792451096));
#34064=CARTESIAN_POINT('Ctrl Pts',(-11.1563640427418,-38.1865296420804,
21.6311698040555));
#34065=CARTESIAN_POINT('Ctrl Pts',(-11.1819663706516,-38.1771220503234,
21.6295687435354));
#34066=CARTESIAN_POINT('Ctrl Pts',(-11.2304956242356,-38.1586221217308,
21.626539285772));
#34067=CARTESIAN_POINT('Ctrl Pts',(-11.2534421970858,-38.149586622816,21.6251091443025));
#34068=CARTESIAN_POINT('Ctrl Pts',(-11.3070591443628,-38.1277954983539,
21.6217718261546));
#34069=CARTESIAN_POINT('Ctrl Pts',(-11.3376449672406,-38.1148377707331,
21.6198714395194));
#34070=CARTESIAN_POINT('Ctrl Pts',(-11.4468684890122,-38.0666594719413,
21.6130922200153));
#34071=CARTESIAN_POINT('Ctrl Pts',(-11.5243500729054,-38.0288920786886,
21.6082976337194));
#34072=CARTESIAN_POINT('Ctrl Pts',(-11.8417914851368,-37.8588888231763,
21.5885707029542));
#34073=CARTESIAN_POINT('Ctrl Pts',(-12.0666877467752,-37.7007838589456,
21.5744754338813));
#34074=CARTESIAN_POINT('Ctrl Pts',(-12.3194609763066,-37.4728370824409,
21.5560461746748));
#34075=CARTESIAN_POINT('Ctrl Pts',(-12.3674969355891,-37.4268868604747,
21.5524033050401));
#34076=CARTESIAN_POINT('Ctrl Pts',(-12.4458056605234,-37.347439756066,21.5461613960323));
#34077=CARTESIAN_POINT('Ctrl Pts',(-12.4768169988418,-37.3146956362789,
21.5436038013213));
#34078=CARTESIAN_POINT('Ctrl Pts',(-12.520461477466,-37.2667309867488,21.5398617162945));
#34079=CARTESIAN_POINT('Ctrl Pts',(-12.5336302327839,-37.2520020489353,
21.5387131697554));
#34080=CARTESIAN_POINT('Ctrl Pts',(-12.5565294444878,-37.2259347422351,
21.536679722016));
#34081=CARTESIAN_POINT('Ctrl Pts',(-12.5663148680068,-37.2146458550585,
21.5357987896089));
#34082=CARTESIAN_POINT('Ctrl Pts',(-12.5877666903053,-37.1895650046557,
21.533840542503));
#34083=CARTESIAN_POINT('Ctrl Pts',(-12.5993975323103,-37.1757444219897,
21.5327609347309));
#34084=CARTESIAN_POINT('Ctrl Pts',(-12.6330427024561,-37.135110018607,21.529586875146));
#34085=CARTESIAN_POINT('Ctrl Pts',(-12.6547558930936,-37.1080511407784,
21.5274734153496));
#34086=CARTESIAN_POINT('Ctrl Pts',(-12.7903099733162,-36.9337081422798,
21.5138825438768));
#34087=CARTESIAN_POINT('Ctrl Pts',(-12.8922632108645,-36.7775996746517,
21.501849193541));
#34088=CARTESIAN_POINT('Ctrl Pts',(-13.0562987579485,-36.4746302106539,
21.4796454067493));
#34089=CARTESIAN_POINT('Ctrl Pts',(-13.1218661346566,-36.3302088964952,
21.4694890464365));
#34090=CARTESIAN_POINT('Ctrl Pts',(-13.2105287638497,-36.0918366105283,
21.4536219736481));
#34091=CARTESIAN_POINT('Ctrl Pts',(-13.2401341735268,-36.000567512039,21.4477425953186));
#34092=CARTESIAN_POINT('Ctrl Pts',(-13.275832687443,-35.8721920037655,21.4397441484479));
#34093=CARTESIAN_POINT('Ctrl Pts',(-13.2852396834973,-35.8360616464855,
21.4375220092756));
#34094=CARTESIAN_POINT('Ctrl Pts',(-13.30041843446,-35.7735452004135,21.4337253265084));
#34095=CARTESIAN_POINT('Ctrl Pts',(-13.3064751037301,-35.7472325413186,
21.4321419190067));
#34096=CARTESIAN_POINT('Ctrl Pts',(-13.3182496912756,-35.6931297441005,
21.4289150345263));
#34097=CARTESIAN_POINT('Ctrl Pts',(-13.3239344023829,-35.6653345140264,
21.4272727130019));
#34098=CARTESIAN_POINT('Ctrl Pts',(-13.3376335982534,-35.5937887527209,
21.4230831144521));
#34099=CARTESIAN_POINT('Ctrl Pts',(-13.3451373092684,-35.5499452330688,
21.4205518410088));
#34100=CARTESIAN_POINT('Ctrl Pts',(-13.3771969771401,-35.3375653629982,
21.4084463936505));
#34101=CARTESIAN_POINT('Ctrl Pts',(-13.3898921009111,-35.1674812302973,
21.3992404617354));
#34102=CARTESIAN_POINT('Ctrl Pts',(-13.3895475950888,-34.7579871130917,
21.3774224061149));
#34103=CARTESIAN_POINT('Ctrl Pts',(-13.3640366909492,-34.5195447800139,
21.365014017526));
#34104=CARTESIAN_POINT('Ctrl Pts',(-13.3041286563306,-34.2415911078333,
21.3491058622142));
#34105=CARTESIAN_POINT('Ctrl Pts',(-13.293717064086,-34.1975800844463,21.3465412789965));
#34106=CARTESIAN_POINT('Ctrl Pts',(-13.2775434534815,-34.1348428241764,
21.3428028679112));
#34107=CARTESIAN_POINT('Ctrl Pts',(-13.272494294406,-34.1159360420124,21.3416653853085));
#34108=CARTESIAN_POINT('Ctrl Pts',(-13.2632990015683,-34.0826624060655,
21.3396426608231));
#34109=CARTESIAN_POINT('Ctrl Pts',(-13.259221079058,-34.0682776263751,21.3387612019157));
#34110=CARTESIAN_POINT('Ctrl Pts',(-13.2500374926068,-34.0366809231078,
21.3368092106831));
#34111=CARTESIAN_POINT('Ctrl Pts',(-13.2448902572386,-34.0194825172306,
21.3357364900349));
#34112=CARTESIAN_POINT('Ctrl Pts',(-13.2292397424989,-33.9686627847612,
21.3325379953537));
#34113=CARTESIAN_POINT('Ctrl Pts',(-13.2183490524295,-33.9351643634232,
21.3303922840306));
#34114=CARTESIAN_POINT('Ctrl Pts',(-13.1978680991166,-33.8753539939704,
21.3265012087214));
#34115=CARTESIAN_POINT('Ctrl Pts',(-13.1884710371189,-33.84898265086,21.3247643411037));
#34116=CARTESIAN_POINT('Ctrl Pts',(-13.1787501333198,-33.8227350967521,
21.3230163149173));
#34117=CARTESIAN_POINT('',(-13.389749867084,-34.9990507350945,21.7311301749608));
#34118=CARTESIAN_POINT('Ctrl Pts',(-13.1787500936073,-33.8227349895238,
21.6644775413951));
#34119=CARTESIAN_POINT('Ctrl Pts',(-13.1948737496338,-33.8662707037832,
21.6669624140685));
#34120=CARTESIAN_POINT('Ctrl Pts',(-13.2101057520662,-33.9101450433166,
21.6694348331333));
#34121=CARTESIAN_POINT('Ctrl Pts',(-13.2712235710965,-34.0986084927412,
21.6799584931992));
#34122=CARTESIAN_POINT('Ctrl Pts',(-13.3082740429438,-34.2458582370596,
21.6879338889851));
#34123=CARTESIAN_POINT('Ctrl Pts',(-13.3523689409156,-34.4889866704007,
21.70132228591));
#34124=CARTESIAN_POINT('Ctrl Pts',(-13.3654246881183,-34.5835557279141,
21.7065849537685));
#34125=CARTESIAN_POINT('Ctrl Pts',(-13.376957464737,-34.7046195661836,21.7135295727455));
#34126=CARTESIAN_POINT('Ctrl Pts',(-13.3791392763981,-34.7307250836849,
21.715039329318));
#34127=CARTESIAN_POINT('Ctrl Pts',(-13.3821708185903,-34.7728793126426,
21.717500700615));
#34128=CARTESIAN_POINT('Ctrl Pts',(-13.3832094036412,-34.7889138547634,
21.7184424219694));
#34129=CARTESIAN_POINT('Ctrl Pts',(-13.3849363291718,-34.8188768975796,
21.7202133817078));
#34130=CARTESIAN_POINT('Ctrl Pts',(-13.3856527898447,-34.8328034192798,
21.7210410532929));
#34131=CARTESIAN_POINT('Ctrl Pts',(-13.3869928569964,-34.8624109981548,
21.7228097754308));
#34132=CARTESIAN_POINT('Ctrl Pts',(-13.3875935356735,-34.8780928088416,
21.7237520103063));
#34133=CARTESIAN_POINT('Ctrl Pts',(-13.3891851625189,-34.9288597128656,
21.7268186450154));
#34134=CARTESIAN_POINT('Ctrl Pts',(-13.3897400388564,-34.9639549119412,
21.7289638292364));
#34135=CARTESIAN_POINT('Ctrl Pts',(-13.389749867084,-34.9990507350945,21.7311301749608));
#34136=CARTESIAN_POINT('Ctrl Pts',(-13.3897498660442,-34.9990470292048,
21.7311299462089));
#34137=CARTESIAN_POINT('Ctrl Pts',(-13.3898014297935,-35.1824610573557,
21.7424514621912));
#34138=CARTESIAN_POINT('Ctrl Pts',(-13.374966596757,-35.3655710725717,21.75431371688));
#34139=CARTESIAN_POINT('Ctrl Pts',(-13.3201353354254,-35.7011744871535,
21.7762271822552));
#34140=CARTESIAN_POINT('Ctrl Pts',(-13.2841883531142,-35.8538492343368,
21.7862660856627));
#34141=CARTESIAN_POINT('Ctrl Pts',(-13.2095983064274,-36.0945150714575,
21.8019809951908));
#34142=CARTESIAN_POINT('Ctrl Pts',(-13.1775629265222,-36.1843061302093,
21.8078213884003));
#34143=CARTESIAN_POINT('Ctrl Pts',(-13.127799109752,-36.3071592484198,21.8157772703349));
#34144=CARTESIAN_POINT('Ctrl Pts',(-13.1132458624233,-36.3414518023022,
21.8179943667585));
#34145=CARTESIAN_POINT('Ctrl Pts',(-13.0871796535606,-36.4001625144136,
21.8217851933286));
#34146=CARTESIAN_POINT('Ctrl Pts',(-13.0759350710889,-36.4246953292758,
21.8233677151569));
#34147=CARTESIAN_POINT('Ctrl Pts',(-13.0522597927309,-36.4747615068826,
21.8265951718281));
#34148=CARTESIAN_POINT('Ctrl Pts',(-13.0397987851075,-36.5002782281438,
21.8282389208609));
#34149=CARTESIAN_POINT('Ctrl Pts',(-13.0069434719252,-36.5654665427469,
21.8324371465003));
#34150=CARTESIAN_POINT('Ctrl Pts',(-12.9860837897947,-36.6048982523692,
21.8349754860888));
#34151=CARTESIAN_POINT('Ctrl Pts',(-12.8789622783248,-36.7980699339472,
21.8474232633832));
#34152=CARTESIAN_POINT('Ctrl Pts',(-12.7815747146027,-36.9453356086829,
21.856934959789));
#34153=CARTESIAN_POINT('Ctrl Pts',(-12.5604090539148,-37.2289762607998,
21.8760799413469));
#34154=CARTESIAN_POINT('Ctrl Pts',(-12.4361123461674,-37.3641869203607,
21.8856737265604));
#34155=CARTESIAN_POINT('Ctrl Pts',(-12.2400646918167,-37.545489596148,21.9002317856925));
#34156=CARTESIAN_POINT('Ctrl Pts',(-12.1765519452948,-37.600005116813,21.9048752055764));
#34157=CARTESIAN_POINT('Ctrl Pts',(-12.0918562634241,-37.667423278751,21.9110711413184));
#34158=CARTESIAN_POINT('Ctrl Pts',(-12.0724543058802,-37.6825254239083,
21.9124907678182));
#34159=CARTESIAN_POINT('Ctrl Pts',(-12.0403782051454,-37.7069372130646,
21.9148413176081));
#34160=CARTESIAN_POINT('Ctrl Pts',(-12.0278001317851,-37.7163723794699,
21.9157639272681));
#34161=CARTESIAN_POINT('Ctrl Pts',(-12.003859659853,-37.7340718570004,21.917522580629));
#34162=CARTESIAN_POINT('Ctrl Pts',(-11.9925106385795,-37.7423536962041,
21.9183573447529));
#34163=CARTESIAN_POINT('Ctrl Pts',(-11.9616775860849,-37.7645613877999,
21.9206273817551));
#34164=CARTESIAN_POINT('Ctrl Pts',(-11.9420972906718,-37.7783514286413,
21.9220712465145));
#34165=CARTESIAN_POINT('Ctrl Pts',(-11.8643354689945,-37.8318939990843,
21.9278092094343));
#34166=CARTESIAN_POINT('Ctrl Pts',(-11.8050696840158,-37.8700335241079,
21.9321902869708));
#34167=CARTESIAN_POINT('Ctrl Pts',(-11.5825515252263,-38.0036122115057,
21.9485512081874));
#34168=CARTESIAN_POINT('Ctrl Pts',(-11.4125858551877,-38.0871921023347,
21.9608582823783));
#34169=CARTESIAN_POINT('Ctrl Pts',(-11.0778030109755,-38.2183553781346,
21.9839109068227));
#34170=CARTESIAN_POINT('Ctrl Pts',(-10.9145832554482,-38.2684891111561,
21.9946603017103));
#34171=CARTESIAN_POINT('Ctrl Pts',(-10.6972330757303,-38.3176812395879,
22.0082163571504));
#34172=CARTESIAN_POINT('Ctrl Pts',(-10.6459381339013,-38.3280485502794,
22.0113636114434));
#34173=CARTESIAN_POINT('Ctrl Pts',(-10.5649023637633,-38.3424825215882,
22.0162563644988));
#34174=CARTESIAN_POINT('Ctrl Pts',(-10.535314081407,-38.3473486535563,22.0180263976449));
#34175=CARTESIAN_POINT('Ctrl Pts',(-10.4794596757818,-38.355774992147,22.0213378715053));
#34176=CARTESIAN_POINT('Ctrl Pts',(-10.453208967522,-38.3594209425359,22.0228818630104));
#34177=CARTESIAN_POINT('Ctrl Pts',(-10.3934740504008,-38.3670045641113,
22.0263684815111));
#34178=CARTESIAN_POINT('Ctrl Pts',(-10.3599681695719,-38.3707513400725,
22.0283050782568));
#34179=CARTESIAN_POINT('Ctrl Pts',(-10.2715337675651,-38.3793067604117,
22.0333699483863));
#34180=CARTESIAN_POINT('Ctrl Pts',(-10.2165331813105,-38.3832763134464,
22.0364727101992));
#34181=CARTESIAN_POINT('Ctrl Pts',(-9.90312068228571,-38.3982215058787,
22.0539308080207));
#34182=CARTESIAN_POINT('Ctrl Pts',(-9.64422867801832,-38.3809359490208,
22.0674124687924));
#34183=CARTESIAN_POINT('Ctrl Pts',(-9.25546531681056,-38.3097924925162,
22.0884811352638));
#34184=CARTESIAN_POINT('Ctrl Pts',(-9.12273998932656,-38.2771124984082,
22.0958458289397));
#34185=CARTESIAN_POINT('Ctrl Pts',(-8.95896723938749,-38.2261244666974,
22.1055377358029));
#34186=CARTESIAN_POINT('Ctrl Pts',(-8.92573790191977,-38.2152121280007,
22.107536540246));
#34187=CARTESIAN_POINT('Ctrl Pts',(-8.87576387900573,-38.1979397625401,
22.1105999404111));
#34188=CARTESIAN_POINT('Ctrl Pts',(-8.85889002823405,-38.1919576409867,
22.1116443036231));
#34189=CARTESIAN_POINT('Ctrl Pts',(-8.82800610899173,-38.1807324844832,
22.1135755383714));
#34190=CARTESIAN_POINT('Ctrl Pts',(-8.81398223913815,-38.1755299812052,
22.1144601263776));
#34191=CARTESIAN_POINT('Ctrl Pts',(-8.78162832270628,-38.1632832810413,
22.1165184405307));
#34192=CARTESIAN_POINT('Ctrl Pts',(-8.76332455319008,-38.1561724380565,
22.1176958732035));
#34193=CARTESIAN_POINT('Ctrl Pts',(-8.70269691962236,-38.1320108242399,
22.1216366890609));
#34194=CARTESIAN_POINT('Ctrl Pts',(-8.6606572828943,-38.1142652010072,22.1244357608061));
#34195=CARTESIAN_POINT('Ctrl Pts',(-8.42660583762881,-38.0098527789951,
22.140345773963));
#34196=CARTESIAN_POINT('Ctrl Pts',(-8.24264930127822,-37.9062853810792,
22.1540685466479));
#34197=CARTESIAN_POINT('Ctrl Pts',(-7.90736028029149,-37.673981032209,22.1802689251291));
#34198=CARTESIAN_POINT('Ctrl Pts',(-7.75531358766897,-37.5476889197956,
22.1927199908908));
#34199=CARTESIAN_POINT('Ctrl Pts',(-7.58317184072951,-37.3772600271542,
22.207367828932));
#34200=CARTESIAN_POINT('Ctrl Pts',(-7.55187501122673,-37.3450176796722,
22.2100578466236));
#34201=CARTESIAN_POINT('Ctrl Pts',(-7.501813478758,-37.29134877964,22.2144073871783));
#34202=CARTESIAN_POINT('Ctrl Pts',(-7.48266218809584,-37.2702919502743,
22.2160830538561));
#34203=CARTESIAN_POINT('Ctrl Pts',(-7.44589610966172,-37.2288303634244,
22.2193240945206));
#34204=CARTESIAN_POINT('Ctrl Pts',(-7.42825507096532,-37.2084518453126,
22.2208904842015));
#34205=CARTESIAN_POINT('Ctrl Pts',(-7.38694751422866,-37.1595680598413,
22.2245868114883));
#34206=CARTESIAN_POINT('Ctrl Pts',(-7.36350130915709,-37.1308806406257,
22.2267078497248));
#34207=CARTESIAN_POINT('Ctrl Pts',(-7.28602816096082,-37.0328521861737,
22.2338020674531));
#34208=CARTESIAN_POINT('Ctrl Pts',(-7.23422722925325,-36.9617935298267,
22.2386903889364));
#34209=CARTESIAN_POINT('Ctrl Pts',(-7.03366624091163,-36.6629100794874,
22.2583932251581));
#34210=CARTESIAN_POINT('Ctrl Pts',(-6.90983989402039,-36.4196150802825,
22.272394499527));
#34211=CARTESIAN_POINT('Ctrl Pts',(-6.79364603208641,-36.1018609088283,
22.2907149503242));
#34212=CARTESIAN_POINT('Ctrl Pts',(-6.77270400059847,-36.0389239064928,
22.2943502301844));
#34213=CARTESIAN_POINT('Ctrl Pts',(-6.74066576285426,-35.9322943698348,
22.3005805224513));
#34214=CARTESIAN_POINT('Ctrl Pts',(-6.72857025323899,-35.888920396955,22.3031342905904));
#34215=CARTESIAN_POINT('Ctrl Pts',(-6.71241868753829,-35.8261985690928,
22.3068717668717));
#34216=CARTESIAN_POINT('Ctrl Pts',(-6.70766185898986,-35.8070343772999,
22.3080196532421));
#34217=CARTESIAN_POINT('Ctrl Pts',(-6.69960068354594,-35.7732998146078,
22.3100523932856));
#34218=CARTESIAN_POINT('Ctrl Pts',(-6.69622480620727,-35.7587474599528,
22.310933288554));
#34219=CARTESIAN_POINT('Ctrl Pts',(-6.68897760945146,-35.726541395849,22.3128920343417));
#34220=CARTESIAN_POINT('Ctrl Pts',(-6.68515124754349,-35.7088789647203,
22.3139721861852));
#34221=CARTESIAN_POINT('Ctrl Pts',(-6.67438372353001,-35.6571818427568,
22.3171493743282));
#34222=CARTESIAN_POINT('Ctrl Pts',(-6.66782444519026,-35.6230709939965,
22.319265472243));
#34223=CARTESIAN_POINT('Ctrl Pts',(-6.62960161763157,-35.4063907765405,
22.3328067584454));
#34224=CARTESIAN_POINT('Ctrl Pts',(-6.61243092858146,-35.2215958436088,
22.3447825320378));
#34225=CARTESIAN_POINT('Ctrl Pts',(-6.60874088432275,-34.8774078561114,
22.3669663739473));
#34226=CARTESIAN_POINT('Ctrl Pts',(-6.61821705820595,-34.7185414332373,
22.3771588389397));
#34227=CARTESIAN_POINT('Ctrl Pts',(-6.65125485446441,-34.4656367369562,
22.3930725831109));
#34228=CARTESIAN_POINT('Ctrl Pts',(-6.66774796781935,-34.3709235048089,
22.3989638545905));
#34229=CARTESIAN_POINT('Ctrl Pts',(-6.69621222701085,-34.2405351241062,
22.4069752770926));
#34230=CARTESIAN_POINT('Ctrl Pts',(-6.70478256745449,-34.204171635057,22.4091989470177));
#34231=CARTESIAN_POINT('Ctrl Pts',(-6.72058073435574,-34.1417788602738,
22.4129974078084));
#34232=CARTESIAN_POINT('Ctrl Pts',(-6.72752164809753,-34.1156811979278,
22.4145810845332));
#34233=CARTESIAN_POINT('Ctrl Pts',(-6.7423902829352,-34.0623495648298,22.4178077987725));
#34234=CARTESIAN_POINT('Ctrl Pts',(-6.75034945539181,-34.0351265283714,
22.4194496900079));
#34235=CARTESIAN_POINT('Ctrl Pts',(-6.77165371380438,-33.9655146496115,
22.4236366885944));
#34236=CARTESIAN_POINT('Ctrl Pts',(-6.78549257598768,-33.923281855694,22.4261658324929));
#34237=CARTESIAN_POINT('Ctrl Pts',(-6.85583670590559,-33.7220692811147,
22.4381797374926));
#34238=CARTESIAN_POINT('Ctrl Pts',(-6.92332986983456,-33.5671779217981,
22.4473039103074));
#34239=CARTESIAN_POINT('Ctrl Pts',(-7.07971194799279,-33.2708419029367,
22.465161458087));
#34240=CARTESIAN_POINT('Ctrl Pts',(-7.16805894470149,-33.129658681684,22.4738770472087));
#34241=CARTESIAN_POINT('Ctrl Pts',(-7.30855850616282,-32.9380522139871,
22.4867038150892));
#34242=CARTESIAN_POINT('Ctrl Pts',(-7.35250952116893,-32.8819161706727,
22.4905986910988));
#34243=CARTESIAN_POINT('Ctrl Pts',(-7.42855954470036,-32.7908501354757,
22.4972244262691));
#34244=CARTESIAN_POINT('Ctrl Pts',(-7.45968155666443,-32.7551323236651,
22.4999069213872));
#34245=CARTESIAN_POINT('Ctrl Pts',(-7.50508206894105,-32.7051808444429,
22.503799149493));
#34246=CARTESIAN_POINT('Ctrl Pts',(-7.51875614414188,-32.6904027787917,
22.5049688462187));
#34247=CARTESIAN_POINT('Ctrl Pts',(-7.54273544682032,-32.6649462151685,
22.5070174223472));
#34248=CARTESIAN_POINT('Ctrl Pts',(-7.55298044535729,-32.6542121681171,
22.5078919043169));
#34249=CARTESIAN_POINT('Ctrl Pts',(-7.57562548140609,-32.6307959520671,
22.5098236188996));
#34250=CARTESIAN_POINT('Ctrl Pts',(-7.58805458115482,-32.6181438135356,
22.5108829411165));
#34251=CARTESIAN_POINT('Ctrl Pts',(-7.62399014855268,-32.5821330852437,
22.5139414881966));
#34252=CARTESIAN_POINT('Ctrl Pts',(-7.64774000680703,-32.5590215118438,
22.5159577899144));
#34253=CARTESIAN_POINT('Ctrl Pts',(-7.85656091948985,-32.3616904577138,
22.5336126020715));
#34254=CARTESIAN_POINT('Ctrl Pts',(-8.0603371460303,-32.2084575586157,22.5502799925132));
#34255=CARTESIAN_POINT('Ctrl Pts',(-8.42181563377445,-31.9954877196059,
22.5771231250587));
#34256=CARTESIAN_POINT('Ctrl Pts',(-8.57028324371348,-31.9220652871872,
22.5875139429465));
#34257=CARTESIAN_POINT('Ctrl Pts',(-8.76847037169948,-31.841504697235,22.6004891765195));
#34258=CARTESIAN_POINT('Ctrl Pts',(-8.81379345509957,-31.8242052647429,
22.6034001258894));
#34259=CARTESIAN_POINT('Ctrl Pts',(-8.88697090826083,-31.7980593538467,
22.6080125397807));
#34260=CARTESIAN_POINT('Ctrl Pts',(-8.91459418364839,-31.7885903478059,
22.6097340364942));
#34261=CARTESIAN_POINT('Ctrl Pts',(-8.96767651560219,-31.7711573855649,
22.6130058119521));
#34262=CARTESIAN_POINT('Ctrl Pts',(-8.9931138511195,-31.7631347343151,22.6145578890372));
#34263=CARTESIAN_POINT('Ctrl Pts',(-9.05173785083539,-31.7454033476397,
22.6181000459552));
#34264=CARTESIAN_POINT('Ctrl Pts',(-9.08498395861011,-31.7359003933252,
22.6200834231012));
#34265=CARTESIAN_POINT('Ctrl Pts',(-9.1920558845101,-31.707059850489,22.6263948678563));
#34266=CARTESIAN_POINT('Ctrl Pts',(-9.26639369848994,-31.6897052261789,
22.6306609566973));
#34267=CARTESIAN_POINT('Ctrl Pts',(-9.57747557085968,-31.6280766783013,
22.6481317161137));
#34268=CARTESIAN_POINT('Ctrl Pts',(-9.81800128341718,-31.6065838420149,
22.6606773170699));
#34269=CARTESIAN_POINT('Ctrl Pts',(-10.2005904220841,-31.6132190992123,
22.6811039488407));
#34270=CARTESIAN_POINT('Ctrl Pts',(-10.3420931772,-31.6245762595113,22.6887780304506));
#34271=CARTESIAN_POINT('Ctrl Pts',(-10.510133267236,-31.648738868499,22.6984497112034));
#34272=CARTESIAN_POINT('Ctrl Pts',(-10.5377626351861,-31.6530613446452,
22.7000583515354));
#34273=CARTESIAN_POINT('Ctrl Pts',(-10.5815532377616,-31.6604683755219,
22.7026416717853));
#34274=CARTESIAN_POINT('Ctrl Pts',(-10.5977515228169,-31.6633296939084,
22.7036046165762));
#34275=CARTESIAN_POINT('Ctrl Pts',(-10.6288967639686,-31.669065358405,22.7054714176766));
#34276=CARTESIAN_POINT('Ctrl Pts',(-10.6438462278285,-31.6719226678952,
22.7063743588041));
#34277=CARTESIAN_POINT('Ctrl Pts',(-10.6811603653796,-31.6793153761943,
22.7086445849749));
#34278=CARTESIAN_POINT('Ctrl Pts',(-10.7034992376547,-31.6839760895616,
22.7100185081185));
#34279=CARTESIAN_POINT('Ctrl Pts',(-10.7859292328761,-31.7020444255662,
22.7151388644035));
#34280=CARTESIAN_POINT('Ctrl Pts',(-10.8456958063665,-31.7168622669218,
22.7189511238833));
#34281=CARTESIAN_POINT('Ctrl Pts',(-11.1174858838226,-31.7921602125352,
22.7366490045419));
#34282=CARTESIAN_POINT('Ctrl Pts',(-11.3236965972872,-31.8716077971768,
22.7510560753466));
#34283=CARTESIAN_POINT('Ctrl Pts',(-11.6203312529385,-32.0205115446803,
22.7722595594451));
#34284=CARTESIAN_POINT('Ctrl Pts',(-11.7174108754945,-32.0753926600818,
22.7792920733027));
#34285=CARTESIAN_POINT('Ctrl Pts',(-11.8765853574774,-32.1760416102348,
22.7909294053451));
#34286=CARTESIAN_POINT('Ctrl Pts',(-11.940141184754,-32.2193225309812,22.7956077829984));
#34287=CARTESIAN_POINT('Ctrl Pts',(-12.030028391597,-32.2851185409094,22.8022728460976));
#34288=CARTESIAN_POINT('Ctrl Pts',(-12.0575700804559,-32.3059320528537,
22.8043220708423));
#34289=CARTESIAN_POINT('Ctrl Pts',(-12.1057547361529,-32.3435156722515,
22.8079210725417));
#34290=CARTESIAN_POINT('Ctrl Pts',(-12.1265269486587,-32.3601145500539,
22.8094772911971));
#34291=CARTESIAN_POINT('Ctrl Pts',(-12.1699478058771,-32.3956568563033,
22.8127413424798));
#34292=CARTESIAN_POINT('Ctrl Pts',(-12.1925486637182,-32.4146553175153,
22.8144468090642));
#34293=CARTESIAN_POINT('Ctrl Pts',(-12.2528071535975,-32.4666676766893,
22.819013963924));
#34294=CARTESIAN_POINT('Ctrl Pts',(-12.2899868851227,-32.5002253782329,
22.8218534424652));
#34295=CARTESIAN_POINT('Ctrl Pts',(-12.5155548551991,-32.7130763878839,
22.8392504509205));
#34296=CARTESIAN_POINT('Ctrl Pts',(-12.6835305718693,-32.9127265797917,
22.852876034994));
#34297=CARTESIAN_POINT('Ctrl Pts',(-12.8894232342055,-33.223930495808,22.8727117155986));
#34298=CARTESIAN_POINT('Ctrl Pts',(-12.9470505615618,-33.3212863198408,
22.878760878303));
#34299=CARTESIAN_POINT('Ctrl Pts',(-13.0295989251202,-33.4781405116842,
22.888535624039));
#34300=CARTESIAN_POINT('Ctrl Pts',(-13.0578736639977,-33.5357822730399,
22.8921339168106));
#34301=CARTESIAN_POINT('Ctrl Pts',(-13.0938326434641,-33.6146799005638,
22.8971125471099));
#34302=CARTESIAN_POINT('Ctrl Pts',(-13.1029674435577,-33.6352636924332,
22.8984162489877));
#34303=CARTESIAN_POINT('Ctrl Pts',(-13.1179696269838,-33.669998087967,22.9006267133852));
#34304=CARTESIAN_POINT('Ctrl Pts',(-13.1239475829133,-33.6841006217632,
22.9015270859914));
#34305=CARTESIAN_POINT('Ctrl Pts',(-13.1362076135993,-33.7135775626803,
22.9034159088437));
#34306=CARTESIAN_POINT('Ctrl Pts',(-13.1424725514251,-33.728958253706,22.9044052311375));
#34307=CARTESIAN_POINT('Ctrl Pts',(-13.1589894645888,-33.7703766095457,
22.9070782124231));
#34308=CARTESIAN_POINT('Ctrl Pts',(-13.1690322333133,-33.7964956538649,
22.9087731676124));
#34309=CARTESIAN_POINT('Ctrl Pts',(-13.1787501240202,-33.8227350716421,
22.9104831197053));
#34310=CARTESIAN_POINT('Origin',(-10.,-35.,23.));
#34311=CARTESIAN_POINT('',(-13.1787501240175,-33.8227350716349,24.1659533822777));
#34312=CARTESIAN_POINT('',(-13.1787501550516,-33.8227351554304,23.8178420415151));
#34313=CARTESIAN_POINT('',(-13.1787501240207,-33.8227350716434,23.));
#34314=CARTESIAN_POINT('',(-13.3897493118742,-35.0021598954043,22.6386988750799));
#34315=CARTESIAN_POINT('Ctrl Pts',(-13.1787501550516,-33.8227351554304,
23.8178420415151));
#34316=CARTESIAN_POINT('Ctrl Pts',(-13.1694440940813,-33.79760772307,23.8161925519317));
#34317=CARTESIAN_POINT('Ctrl Pts',(-13.1598381340822,-33.7725853491873,
23.8145514041043));
#34318=CARTESIAN_POINT('Ctrl Pts',(-13.130346019916,-33.698404848225,23.8096905622592));
#34319=CARTESIAN_POINT('Ctrl Pts',(-13.10960418551,-33.6496006415447,23.8064985649223));
#34320=CARTESIAN_POINT('Ctrl Pts',(-13.0751712864305,-33.5735876306355,
23.8015344797837));
#34321=CARTESIAN_POINT('Ctrl Pts',(-13.062244683633,-33.5460439221437,23.7997372591049));
#34322=CARTESIAN_POINT('Ctrl Pts',(-13.0373921036912,-33.4948908274866,
23.7964013663375));
#34323=CARTESIAN_POINT('Ctrl Pts',(-13.0255573302067,-33.4712399426843,
23.7948597426906));
#34324=CARTESIAN_POINT('Ctrl Pts',(-12.9983125042682,-33.4183491415447,
23.7914127065048));
#34325=CARTESIAN_POINT('Ctrl Pts',(-12.9827490387604,-33.3891910128053,
23.7895127638632));
#34326=CARTESIAN_POINT('Ctrl Pts',(-12.9337345732362,-33.3005095107186,
23.7837314481919));
#34327=CARTESIAN_POINT('Ctrl Pts',(-12.8989087696405,-33.2417635878976,
23.7798980772683));
#34328=CARTESIAN_POINT('Ctrl Pts',(-12.7279484206883,-32.9722846198199,
23.7622230869209));
#34329=CARTESIAN_POINT('Ctrl Pts',(-12.5704730652143,-32.7760384464127,
23.7491527600519));
#34330=CARTESIAN_POINT('Ctrl Pts',(-12.2903356675787,-32.4968648057453,
23.7280551933204));
#34331=CARTESIAN_POINT('Ctrl Pts',(-12.1814707797683,-32.4014427254085,
23.7202398678366));
#34332=CARTESIAN_POINT('Ctrl Pts',(-12.044442129159,-32.2960285951779,23.7103947022976));
#34333=CARTESIAN_POINT('Ctrl Pts',(-12.0218109396094,-32.2790653460101,
23.7087683334301));
#34334=CARTESIAN_POINT('Ctrl Pts',(-11.9856313116043,-32.2526474236907,
23.7061631400269));
#34335=CARTESIAN_POINT('Ctrl Pts',(-11.9722209738447,-32.2430048441155,
23.7051963938343));
#34336=CARTESIAN_POINT('Ctrl Pts',(-11.9462019749968,-32.2245830984589,
23.7033174543664));
#34337=CARTESIAN_POINT('Ctrl Pts',(-11.9336032485929,-32.2157910373626,
23.7024061179539));
#34338=CARTESIAN_POINT('Ctrl Pts',(-11.9021829762087,-32.1941804127002,
23.7001303088349));
#34339=CARTESIAN_POINT('Ctrl Pts',(-11.8832913539988,-32.1814654081235,
23.6987593502386));
#34340=CARTESIAN_POINT('Ctrl Pts',(-11.8089228310228,-32.1324931578094,
23.6933567634038));
#34341=CARTESIAN_POINT('Ctrl Pts',(-11.7525185632101,-32.097677687176,23.6892471682913));
#34342=CARTESIAN_POINT('Ctrl Pts',(-11.5919337201054,-32.0049450740948,
23.677588285181));
#34343=CARTESIAN_POINT('Ctrl Pts',(-11.485666761563,-31.9508363905632,23.6699224755694));
#34344=CARTESIAN_POINT('Ctrl Pts',(-11.1494196489394,-31.8013842420114,
23.6462064915628));
#34345=CARTESIAN_POINT('Ctrl Pts',(-10.9115910377708,-31.7256532180256,
23.6302435018371));
#34346=CARTESIAN_POINT('Ctrl Pts',(-10.6177630574535,-31.6666298512308,
23.6120250663025));
#34347=CARTESIAN_POINT('Ctrl Pts',(-10.5677176320278,-31.6577425514174,
23.6089694134727));
#34348=CARTESIAN_POINT('Ctrl Pts',(-10.4878875144455,-31.6454109039628,
23.6041681220882));
#34349=CARTESIAN_POINT('Ctrl Pts',(-10.4582258686399,-31.641230676341,23.6024000039088));
#34350=CARTESIAN_POINT('Ctrl Pts',(-10.4022184996779,-31.634093299625,23.5990901980501));
#34351=CARTESIAN_POINT('Ctrl Pts',(-10.375886093528,-31.6310510035616,23.597545988276));
#34352=CARTESIAN_POINT('Ctrl Pts',(-10.3159377033617,-31.6248365476773,
23.594056322629));
#34353=CARTESIAN_POINT('Ctrl Pts',(-10.2823043038806,-31.6218571138223,
23.5921169396167));
#34354=CARTESIAN_POINT('Ctrl Pts',(-10.176476420174,-31.6140738938347,23.5860681692523));
#34355=CARTESIAN_POINT('Ctrl Pts',(-10.1041672257485,-31.6110783824963,
23.5820137802031));
#34356=CARTESIAN_POINT('Ctrl Pts',(-9.92981888811991,-31.6094419995471,
23.5723810027352));
#34357=CARTESIAN_POINT('Ctrl Pts',(-9.82782854056136,-31.6130887499518,
23.5668648654558));
#34358=CARTESIAN_POINT('Ctrl Pts',(-9.67834119998528,-31.6252049403332,
23.5588418623242));
#34359=CARTESIAN_POINT('Ctrl Pts',(-9.63061625344907,-31.6300946865812,
23.5562894306932));
#34360=CARTESIAN_POINT('Ctrl Pts',(-9.37553546434112,-31.6617135406022,
23.5426422736755));
#34361=CARTESIAN_POINT('Ctrl Pts',(-9.17090401804028,-31.7065677367936,
23.5317006181288));
#34362=CARTESIAN_POINT('Ctrl Pts',(-8.92769650464525,-31.7839922848569,
23.5174472563382));
#34363=CARTESIAN_POINT('Ctrl Pts',(-8.88395749993603,-31.7989081360397,
23.5148314732064));
#34364=CARTESIAN_POINT('Ctrl Pts',(-8.82308213222965,-31.8210670772726,
23.5110992809424));
#34365=CARTESIAN_POINT('Ctrl Pts',(-8.80567792500265,-31.8275648245501,
23.5100216110964));
#34366=CARTESIAN_POINT('Ctrl Pts',(-8.77423336622413,-31.8395998677479,
23.5080537301525));
#34367=CARTESIAN_POINT('Ctrl Pts',(-8.76017468979705,-31.8450885858741,
23.5071662710338));
#34368=CARTESIAN_POINT('Ctrl Pts',(-8.73061981882877,-31.8568553092986,
23.5052836951311));
#34369=CARTESIAN_POINT('Ctrl Pts',(-8.71513285466987,-31.8631542939036,
23.5042874550362));
#34370=CARTESIAN_POINT('Ctrl Pts',(-8.67270184314376,-31.8807791171718,
23.5015323352365));
#34371=CARTESIAN_POINT('Ctrl Pts',(-8.64585730445979,-31.8923390229004,
23.4997606834218));
#34372=CARTESIAN_POINT('Ctrl Pts',(-8.58538190791726,-31.9193135169226,
23.495709802704));
#34373=CARTESIAN_POINT('Ctrl Pts',(-8.55184741881983,-31.9349343487788,
23.4934210799052));
#34374=CARTESIAN_POINT('Ctrl Pts',(-8.44183160161243,-31.9883896988216,
23.4857864734567));
#34375=CARTESIAN_POINT('Ctrl Pts',(-8.36652570751825,-32.0285616975968,
23.4803568245721));
#34376=CARTESIAN_POINT('Ctrl Pts',(-8.05252377068077,-32.2116121589933,
23.4570484137369));
#34377=CARTESIAN_POINT('Ctrl Pts',(-7.83033880105019,-32.3807663672527,
23.4389671628804));
#34378=CARTESIAN_POINT('Ctrl Pts',(-7.58611001355821,-32.619341809599,23.4180304098819));
#34379=CARTESIAN_POINT('Ctrl Pts',(-7.54214797958754,-32.6647564308409,
23.4142055918965));
#34380=CARTESIAN_POINT('Ctrl Pts',(-7.47752579955761,-32.7353617871283,
23.4084937506741));
#34381=CARTESIAN_POINT('Ctrl Pts',(-7.4559182686312,-32.7596628419597,23.4065677043994));
#34382=CARTESIAN_POINT('Ctrl Pts',(-7.41739843860323,-32.8042605205775,
23.4031031527287));
#34383=CARTESIAN_POINT('Ctrl Pts',(-7.40036758741181,-32.8244508591349,
23.4015598915683));
#34384=CARTESIAN_POINT('Ctrl Pts',(-7.36397387653125,-32.8686338372851,
23.3982357845438));
#34385=CARTESIAN_POINT('Ctrl Pts',(-7.34469873556579,-32.892695862372,23.3964585036294));
#34386=CARTESIAN_POINT('Ctrl Pts',(-7.29102497250578,-32.9616051704085,
23.3914583848634));
#34387=CARTESIAN_POINT('Ctrl Pts',(-7.25741513543777,-33.0070554569765,
23.3882658807429));
#34388=CARTESIAN_POINT('Ctrl Pts',(-7.18337160049578,-33.1126068471707,
23.381068797031));
#34389=CARTESIAN_POINT('Ctrl Pts',(-7.14369575630167,-33.1732062564826,
23.3770903832142));
#34390=CARTESIAN_POINT('Ctrl Pts',(-7.00485319900036,-33.4008658753611,
23.3626102640712));
#34391=CARTESIAN_POINT('Ctrl Pts',(-6.91815847123986,-33.5750830210797,
23.3524430407306));
#34392=CARTESIAN_POINT('Ctrl Pts',(-6.79268960287007,-33.893046966402,23.3342191521376));
#34393=CARTESIAN_POINT('Ctrl Pts',(-6.74754754833187,-34.0337034603451,
23.3262533069705));
#34394=CARTESIAN_POINT('Ctrl Pts',(-6.70484501038276,-34.2042868580791,
23.3162396105382));
#34395=CARTESIAN_POINT('Ctrl Pts',(-6.69831751718405,-34.2318213218514,
23.3146124203341));
#34396=CARTESIAN_POINT('Ctrl Pts',(-6.68852646295664,-34.2755546937307,
23.3120062135951));
#34397=CARTESIAN_POINT('Ctrl Pts',(-6.68503518335092,-34.2917018793287,
23.311039291401));
#34398=CARTESIAN_POINT('Ctrl Pts',(-6.67852550614222,-34.3229119404873,
23.3091602787077));
#34399=CARTESIAN_POINT('Ctrl Pts',(-6.67549125330258,-34.3379708370795,
23.3082490486839));
#34400=CARTESIAN_POINT('Ctrl Pts',(-6.6682151032405,-34.3753940263804,23.3059738966956));
#34401=CARTESIAN_POINT('Ctrl Pts',(-6.66409596913806,-34.3977812227259,
23.3046034968694));
#34402=CARTESIAN_POINT('Ctrl Pts',(-6.64887998274017,-34.4854303592358,
23.2992061160042));
#34403=CARTESIAN_POINT('Ctrl Pts',(-6.63947099576578,-34.5509666784846,
23.2951013509861));
#34404=CARTESIAN_POINT('Ctrl Pts',(-6.61853837241558,-34.7349144495417,
23.2834619016546));
#34405=CARTESIAN_POINT('Ctrl Pts',(-6.61132000297716,-34.8537179595692,
23.275811096451));
#34406=CARTESIAN_POINT('Ctrl Pts',(-6.6083495691758,-35.2218460701567,23.2520840295923));
#34407=CARTESIAN_POINT('Ctrl Pts',(-6.63382522673741,-35.4705450740019,
23.2360941190474));
#34408=CARTESIAN_POINT('Ctrl Pts',(-6.69717401394581,-35.7644508238692,
23.2178180705981));
#34409=CARTESIAN_POINT('Ctrl Pts',(-6.70913984768951,-35.8144227689762,
23.214729481356));
#34410=CARTESIAN_POINT('Ctrl Pts',(-6.72983157683658,-35.8929115307665,
23.2099062043782));
#34411=CARTESIAN_POINT('Ctrl Pts',(-6.73780518433496,-35.9216168331301,
23.208148133519));
#34412=CARTESIAN_POINT('Ctrl Pts',(-6.75359432906417,-35.9756840309177,
23.2048469589763));
#34413=CARTESIAN_POINT('Ctrl Pts',(-6.76133124597041,-36.0010663659831,
23.2033014848752));
#34414=CARTESIAN_POINT('Ctrl Pts',(-6.77967087247175,-36.0587935497158,
23.1997952246571));
#34415=CARTESIAN_POINT('Ctrl Pts',(-6.79046439546347,-36.0910750632311,
23.197840742505));
#34416=CARTESIAN_POINT('Ctrl Pts',(-6.82624766654928,-36.1929671506637,
23.1916870361398));
#34417=CARTESIAN_POINT('Ctrl Pts',(-6.85303081167555,-36.2619272978937,
23.1875456924529));
#34418=CARTESIAN_POINT('Ctrl Pts',(-6.92336364909026,-36.4268152097634,
23.177651218374));
#34419=CARTESIAN_POINT('Ctrl Pts',(-6.96916961968725,-36.5216971093717,
23.1719653453803));
#34420=CARTESIAN_POINT('Ctrl Pts',(-7.07844932709289,-36.7234739894091,
23.1597045524583));
#34421=CARTESIAN_POINT('Ctrl Pts',(-7.14353171380071,-36.8293195196082,
23.1531629979742));
#34422=CARTESIAN_POINT('Ctrl Pts',(-7.2967195397611,-37.050272731669,23.1388533510533));
#34423=CARTESIAN_POINT('Ctrl Pts',(-7.3866876373612,-37.1637777684862,23.1310761063742));
#34424=CARTESIAN_POINT('Ctrl Pts',(-7.50750583466518,-37.2976398027246,
23.1208944759729));
#34425=CARTESIAN_POINT('Ctrl Pts',(-7.53180529102275,-37.3237234119275,
23.1188583384088));
#34426=CARTESIAN_POINT('Ctrl Pts',(-7.56901104871671,-37.3624189025289,
23.1157492339123));
#34427=CARTESIAN_POINT('Ctrl Pts',(-7.58161481919966,-37.3753196496195,
23.114697417928));
#34428=CARTESIAN_POINT('Ctrl Pts',(-7.60484838214149,-37.3987240552316,
23.1127597160731));
#34429=CARTESIAN_POINT('Ctrl Pts',(-7.61544553135115,-37.409258874664,23.1118762394365));
#34430=CARTESIAN_POINT('Ctrl Pts',(-7.64024227225387,-37.4335859070175,
23.1098098917815));
#34431=CARTESIAN_POINT('Ctrl Pts',(-7.65449335541902,-37.4473241385295,
23.108623158207));
#34432=CARTESIAN_POINT('Ctrl Pts',(-7.70176408991363,-37.4921016191482,
23.1046919583316));
#34433=CARTESIAN_POINT('Ctrl Pts',(-7.73528464685746,-37.5226023718299,
23.101912503679));
#34434=CARTESIAN_POINT('Ctrl Pts',(-7.81979828322199,-37.5964600003939,
23.0949464048634));
#34435=CARTESIAN_POINT('Ctrl Pts',(-7.87148258168086,-37.63899540643,23.0907224553632));
#34436=CARTESIAN_POINT('Ctrl Pts',(-8.1458523419351,-37.8514920644522,23.0686147340667));
#34437=CARTESIAN_POINT('Ctrl Pts',(-8.38776326914076,-37.9949289257836,
23.0502821308231));
#34438=CARTESIAN_POINT('Ctrl Pts',(-8.71874056877548,-38.1393195935546,
23.0278973259944));
#34439=CARTESIAN_POINT('Ctrl Pts',(-8.79404962947304,-38.1690122402669,
23.0229585723145));
#34440=CARTESIAN_POINT('Ctrl Pts',(-8.90107521646151,-38.2068412908393,
23.0161532775115));
#34441=CARTESIAN_POINT('Ctrl Pts',(-8.93195185394021,-38.2172565973856,
23.0142141750579));
#34442=CARTESIAN_POINT('Ctrl Pts',(-8.98864838219097,-38.2354752612977,
23.0106965705255));
#34443=CARTESIAN_POINT('Ctrl Pts',(-9.01442012981425,-38.2434186660722,
23.0091136654869));
#34444=CARTESIAN_POINT('Ctrl Pts',(-9.0670627654046,-38.2589588434761,23.0059119239557));
#34445=CARTESIAN_POINT('Ctrl Pts',(-9.09393824325474,-38.2665328389706,
23.0042939209376));
#34446=CARTESIAN_POINT('Ctrl Pts',(-9.16171958338777,-38.2847339264534,
23.0002530266599));
#34447=CARTESIAN_POINT('Ctrl Pts',(-9.20273691397202,-38.2949298656002,
22.9978438952389));
#34448=CARTESIAN_POINT('Ctrl Pts',(-9.38472826244784,-38.3365710134546,
22.9873002152675));
#34449=CARTESIAN_POINT('Ctrl Pts',(-9.52744338117719,-38.3597562075392,
22.9794232391571));
#34450=CARTESIAN_POINT('Ctrl Pts',(-9.80296663439148,-38.3866069115911,
22.9645827992421));
#34451=CARTESIAN_POINT('Ctrl Pts',(-9.93535907813262,-38.3917179258534,
22.9576091044348));
#34452=CARTESIAN_POINT('Ctrl Pts',(-10.2186965811993,-38.3860571144902,
22.942541361258));
#34453=CARTESIAN_POINT('Ctrl Pts',(-10.3692987441442,-38.3729543115252,
22.9344442747116));
#34454=CARTESIAN_POINT('Ctrl Pts',(-10.5540816896695,-38.3443525882184,
22.9238903774055));
#34455=CARTESIAN_POINT('Ctrl Pts',(-10.5895623520611,-38.3382805109371,
22.9218349557408));
#34456=CARTESIAN_POINT('Ctrl Pts',(-10.6427316386463,-38.3283072054364,
22.9187022627679));
#34457=CARTESIAN_POINT('Ctrl Pts',(-10.6604977367765,-38.324827141485,22.9176466241199));
#34458=CARTESIAN_POINT('Ctrl Pts',(-10.6927295424391,-38.3182449738906,
22.9157139182871));
#34459=CARTESIAN_POINT('Ctrl Pts',(-10.707204038937,-38.3151902431169,22.9148394291914));
#34460=CARTESIAN_POINT('Ctrl Pts',(-10.7408253945437,-38.3078645112366,
22.9127930148259));
#34461=CARTESIAN_POINT('Ctrl Pts',(-10.7599555812798,-38.3035219635617,
22.9116172838046));
#34462=CARTESIAN_POINT('Ctrl Pts',(-10.8221293671421,-38.2888399181798,
22.9077615000137));
#34463=CARTESIAN_POINT('Ctrl Pts',(-10.8650067016278,-38.2778236247112,
22.9050481984178));
#34464=CARTESIAN_POINT('Ctrl Pts',(-10.9700398998716,-38.2486336029008,
22.8982875606185));
#34465=CARTESIAN_POINT('Ctrl Pts',(-11.0319134454529,-38.2295125786671,
22.8942054631409));
#34466=CARTESIAN_POINT('Ctrl Pts',(-11.3327138817197,-38.1270282713596,
22.8739821659142));
#34467=CARTESIAN_POINT('Ctrl Pts',(-11.5623694805042,-38.0188497286454,
22.8574312179954));
#34468=CARTESIAN_POINT('Ctrl Pts',(-11.866314326056,-37.8316201889597,22.8350626703784));
#34469=CARTESIAN_POINT('Ctrl Pts',(-11.9522381613845,-37.7730798005677,
22.8286684304963));
#34470=CARTESIAN_POINT('Ctrl Pts',(-12.0668419958852,-37.6870282359272,
22.8200471030434));
#34471=CARTESIAN_POINT('Ctrl Pts',(-12.0979266917168,-37.6628293916601,
22.8176983664549));
#34472=CARTESIAN_POINT('Ctrl Pts',(-12.1496678465436,-37.6210812983317,
22.813769678177));
#34473=CARTESIAN_POINT('Ctrl Pts',(-12.170547861932,-37.6038166343889,22.812178805928));
#34474=CARTESIAN_POINT('Ctrl Pts',(-12.212396890734,-37.5683604687079,22.8089781632739));
#34475=CARTESIAN_POINT('Ctrl Pts',(-12.2333539214903,-37.5501580005037,
22.8073690099432));
#34476=CARTESIAN_POINT('Ctrl Pts',(-12.285030989637,-37.504147596669,22.8033834211524));
#34477=CARTESIAN_POINT('Ctrl Pts',(-12.3154696284277,-37.4760295677066,
22.8010199366185));
#34478=CARTESIAN_POINT('Ctrl Pts',(-12.4421539997109,-37.3546237252692,
22.791102545365));
#34479=CARTESIAN_POINT('Ctrl Pts',(-12.5333419419097,-37.2562253356138,
22.7837673076984));
#34480=CARTESIAN_POINT('Ctrl Pts',(-12.706761857214,-37.045281055661,22.7690831906271));
#34481=CARTESIAN_POINT('Ctrl Pts',(-12.7883638456398,-36.9325532897672,
22.7617578250463));
#34482=CARTESIAN_POINT('Ctrl Pts',(-12.9467634478842,-36.6827267903299,
22.7460410038403));
#34483=CARTESIAN_POINT('Ctrl Pts',(-13.0214195153088,-36.5446678894903,
22.7376510464476));
#34484=CARTESIAN_POINT('Ctrl Pts',(-13.10107390006,-36.3693176155241,22.7267787654395));
#34485=CARTESIAN_POINT('Ctrl Pts',(-13.1153804520665,-36.3364484616631,
22.7247315884129));
#34486=CARTESIAN_POINT('Ctrl Pts',(-13.1361122373471,-36.2866747048548,
22.7216089787021));
#34487=CARTESIAN_POINT('Ctrl Pts',(-13.1429282742043,-36.2699344836114,
22.7205549721204));
#34488=CARTESIAN_POINT('Ctrl Pts',(-13.1551328274853,-36.2392598959705,
22.7186153364739));
#34489=CARTESIAN_POINT('Ctrl Pts',(-13.1605635675376,-36.2253432817686,
22.7177321533613));
#34490=CARTESIAN_POINT('Ctrl Pts',(-13.1729575065669,-36.1929524264085,
22.7156692917471));
#34491=CARTESIAN_POINT('Ctrl Pts',(-13.1798514675643,-36.1744528228081,
22.7144857970722));
#34492=CARTESIAN_POINT('Ctrl Pts',(-13.2019304779914,-36.1135851557525,
22.7105769156143));
#34493=CARTESIAN_POINT('Ctrl Pts',(-13.2164327785833,-36.0709764013763,
22.7078170598837));
#34494=CARTESIAN_POINT('Ctrl Pts',(-13.2501833991684,-35.9649381586313,
22.7009120606399));
#34495=CARTESIAN_POINT('Ctrl Pts',(-13.2684274840359,-35.9012095623811,
22.6967303772893));
#34496=CARTESIAN_POINT('Ctrl Pts',(-13.3543056274298,-35.564178620736,22.6745805635256));
#34497=CARTESIAN_POINT('Ctrl Pts',(-13.3895698991912,-35.2837309463288,
22.6561515965784));
#34498=CARTESIAN_POINT('Ctrl Pts',(-13.3897493118742,-35.0021598954043,
22.6386988750799));
#34499=CARTESIAN_POINT('Ctrl Pts',(-13.3897493143655,-35.0021559820986,
22.6386986325201));
#34500=CARTESIAN_POINT('Ctrl Pts',(-13.3897813530779,-34.9517830205386,
22.6355763483221));
#34501=CARTESIAN_POINT('Ctrl Pts',(-13.3886905509555,-34.9014133179565,
22.6324836405767));
#34502=CARTESIAN_POINT('Ctrl Pts',(-13.3847480855858,-34.8117581780564,
22.6270320201307));
#34503=CARTESIAN_POINT('Ctrl Pts',(-13.3823338406184,-34.7724641323813,
22.6246609047137));
#34504=CARTESIAN_POINT('Ctrl Pts',(-13.3771513033993,-34.70681828144,22.6207292907024));
#34505=CARTESIAN_POINT('Ctrl Pts',(-13.3747576087104,-34.6804415728901,
22.6191575733152));
#34506=CARTESIAN_POINT('Ctrl Pts',(-13.3694901319793,-34.6290915669839,
22.616112774202));
#34507=CARTESIAN_POINT('Ctrl Pts',(-13.3666472101612,-34.6041169008927,
22.6146388442416));
#34508=CARTESIAN_POINT('Ctrl Pts',(-13.360026987176,-34.5512033824149,22.6115299700426));
#34509=CARTESIAN_POINT('Ctrl Pts',(-13.3561783860098,-34.5232752685115,
22.6098973538604));
#34510=CARTESIAN_POINT('Ctrl Pts',(-13.3454914997547,-34.4522842053785,
22.605766655022));
#34511=CARTESIAN_POINT('Ctrl Pts',(-13.3381698616087,-34.4092985647781,
22.6032836747446));
#34512=CARTESIAN_POINT('Ctrl Pts',(-13.3010067134662,-34.2139597188259,
22.5920679108909));
#34513=CARTESIAN_POINT('Ctrl Pts',(-13.261549413046,-34.0636201719023,22.5836355080249));
#34514=CARTESIAN_POINT('Ctrl Pts',(-13.201321222039,-33.8850797250537,22.5735646774699));
#34515=CARTESIAN_POINT('Ctrl Pts',(-13.1902628614254,-33.8538207821783,
22.5717987757316));
#34516=CARTESIAN_POINT('Ctrl Pts',(-13.1787501379842,-33.8227351093465,
22.5700367124769));
#34517=CARTESIAN_POINT('Ctrl Pts',(-13.1787501240202,-33.8227350716421,
22.9104831197053));
#34518=CARTESIAN_POINT('Ctrl Pts',(-13.1790010828795,-33.8234126893014,
22.9105272782207));
#34519=CARTESIAN_POINT('Ctrl Pts',(-13.1792518250776,-33.8240903872375,
22.9105714467413));
#34520=CARTESIAN_POINT('Ctrl Pts',(-13.2379593845312,-33.9829193244527,
22.9209241292555));
#34521=CARTESIAN_POINT('Ctrl Pts',(-13.2845300383789,-34.1451980259089,
22.931747794009));
#34522=CARTESIAN_POINT('Ctrl Pts',(-13.3479888900709,-34.4505396763261,
22.9518445278896));
#34523=CARTESIAN_POINT('Ctrl Pts',(-13.3682219700549,-34.5925434889456,
22.9610882235064));
#34524=CARTESIAN_POINT('Ctrl Pts',(-13.3862516589892,-34.8228200820771,
22.9756971533644));
#34525=CARTESIAN_POINT('Ctrl Pts',(-13.3897019623642,-34.9104709072447,
22.9811718835349));
#34526=CARTESIAN_POINT('Ctrl Pts',(-13.3897847493606,-35.0631798689789,
22.9905426671675));
#34527=CARTESIAN_POINT('Ctrl Pts',(-13.3879493868013,-35.1281879909346,
22.994479274308));
#34528=CARTESIAN_POINT('Ctrl Pts',(-13.3823960453813,-35.2255117986716,
23.0002961702296));
#34529=CARTESIAN_POINT('Ctrl Pts',(-13.3800816042195,-35.2578895846344,
23.0022186676488));
#34530=CARTESIAN_POINT('Ctrl Pts',(-13.3750412122609,-35.3165428174658,
23.0056794712165));
#34531=CARTESIAN_POINT('Ctrl Pts',(-13.3724725330889,-35.3428288374107,
23.0072224844828));
#34532=CARTESIAN_POINT('Ctrl Pts',(-13.366235136149,-35.399774102426,23.0105489599472));
#34533=CARTESIAN_POINT('Ctrl Pts',(-13.3624541712792,-35.4304188209739,
23.0123288159882));
#34534=CARTESIAN_POINT('Ctrl Pts',(-13.3505366499884,-35.5172330286673,
23.0173447067182));
#34535=CARTESIAN_POINT('Ctrl Pts',(-13.3414072947925,-35.5732570585567,
23.0205500901092));
#34536=CARTESIAN_POINT('Ctrl Pts',(-13.3173626238281,-35.7005802010372,
23.0277817467983));
#34537=CARTESIAN_POINT('Ctrl Pts',(-13.3015475742769,-35.771681205236,23.0317814653936));
#34538=CARTESIAN_POINT('Ctrl Pts',(-13.2346130159345,-36.03263006282,23.0464064850513));
#34539=CARTESIAN_POINT('Ctrl Pts',(-13.1693029993633,-36.2184275686629,
23.056689182484));
#34540=CARTESIAN_POINT('Ctrl Pts',(-13.0286963490147,-36.5291421174995,
23.0748829678814));
#34541=CARTESIAN_POINT('Ctrl Pts',(-12.9607857935857,-36.656809011298,23.0826901502761));
#34542=CARTESIAN_POINT('Ctrl Pts',(-12.8700995577321,-36.803810810818,23.0925261908049));
#34543=CARTESIAN_POINT('Ctrl Pts',(-12.8549505486745,-36.827693126973,23.0941524954441));
#34544=CARTESIAN_POINT('Ctrl Pts',(-12.8304838875117,-36.8652181744952,
23.0967576094203));
#34545=CARTESIAN_POINT('Ctrl Pts',(-12.8213619502363,-36.8789876521033,
23.0977243416623));
#34546=CARTESIAN_POINT('Ctrl Pts',(-12.803561480858,-36.9054354178798,23.0996032748626));
#34547=CARTESIAN_POINT('Ctrl Pts',(-12.7948968044657,-36.9181222397981,
23.1005146192387));
#34548=CARTESIAN_POINT('Ctrl Pts',(-12.7731754228395,-36.9494670392508,
23.1027904785544));
#34549=CARTESIAN_POINT('Ctrl Pts',(-12.7600164756916,-36.9680530112449,
23.104161480002));
#34550=CARTESIAN_POINT('Ctrl Pts',(-12.7078295433343,-37.040210096098,23.1095644683791));
#34551=CARTESIAN_POINT('Ctrl Pts',(-12.6674231164322,-37.0927615279647,
23.1136744363155));
#34552=CARTESIAN_POINT('Ctrl Pts',(-12.550115483698,-37.2364083187136,23.1253348210549));
#34553=CARTESIAN_POINT('Ctrl Pts',(-12.4699123664173,-37.3246809491208,
23.1330017904794));
#34554=CARTESIAN_POINT('Ctrl Pts',(-12.208469436395,-37.5835935496903,23.1567169218281));
#34555=CARTESIAN_POINT('Ctrl Pts',(-12.0129456059501,-37.738682096861,23.1726778351449));
#34556=CARTESIAN_POINT('Ctrl Pts',(-11.7591371750142,-37.8980035332952,
23.1908946337718));
#34557=CARTESIAN_POINT('Ctrl Pts',(-11.7154879285399,-37.9240536358084,
23.1939504911727));
#34558=CARTESIAN_POINT('Ctrl Pts',(-11.6452077499257,-37.9638815313459,
23.198752026844));
#34559=CARTESIAN_POINT('Ctrl Pts',(-11.6189527653518,-37.9783039304401,
23.2005201886356));
#34560=CARTESIAN_POINT('Ctrl Pts',(-11.5691106555619,-38.0048293431154,
23.2038300318621));
#34561=CARTESIAN_POINT('Ctrl Pts',(-11.5455661723416,-38.0170072748266,
23.2053742360527));
#34562=CARTESIAN_POINT('Ctrl Pts',(-11.4917134558521,-38.0440656774081,
23.208863829948));
#34563=CARTESIAN_POINT('Ctrl Pts',(-11.4613206427465,-38.0587721358313,
23.2108031477835));
#34564=CARTESIAN_POINT('Ctrl Pts',(-11.3651291295619,-38.1035561850087,
23.2168514704541));
#34565=CARTESIAN_POINT('Ctrl Pts',(-11.2985824090147,-38.1319839204299,
23.2209054890995));
#34566=CARTESIAN_POINT('Ctrl Pts',(-11.1361526102051,-38.1953033271573,
23.2305371594068));
#34567=CARTESIAN_POINT('Ctrl Pts',(-11.0395045968132,-38.228039371375,23.2360525806019));
#34568=CARTESIAN_POINT('Ctrl Pts',(-10.8954870939265,-38.2696795590069,
23.2440723574039));
#34569=CARTESIAN_POINT('Ctrl Pts',(-10.8491734664789,-38.2820125034578,
23.2466223021425));
#34570=CARTESIAN_POINT('Ctrl Pts',(-10.5996175873226,-38.3428309209478,
23.2602603601131));
#34571=CARTESIAN_POINT('Ctrl Pts',(-10.3925017358387,-38.3734234894795,
23.2711953993331));
#34572=CARTESIAN_POINT('Ctrl Pts',(-10.1376333653962,-38.3872717712888,
23.2854476542762));
#34573=CARTESIAN_POINT('Ctrl Pts',(-10.0913114128663,-38.3888367903651,
23.2880708896157));
#34574=CARTESIAN_POINT('Ctrl Pts',(-10.0263759546072,-38.3896984131283,
23.291812027625));
#34575=CARTESIAN_POINT('Ctrl Pts',(-10.0077763137609,-38.3897921054777,
23.2928909476672));
#34576=CARTESIAN_POINT('Ctrl Pts',(-9.97408011176945,-38.3896845206079,
23.2948603665365));
#34577=CARTESIAN_POINT('Ctrl Pts',(-9.95898363218618,-38.3895354610581,
23.2957480976578));
#34578=CARTESIAN_POINT('Ctrl Pts',(-9.92718395915454,-38.3890090010259,
23.2976302029118));
#34579=CARTESIAN_POINT('Ctrl Pts',(-9.91048195208024,-38.388608959139,23.2986256876876));
#34580=CARTESIAN_POINT('Ctrl Pts',(-9.86462781526631,-38.387171438149,23.3013765621024));
#34581=CARTESIAN_POINT('Ctrl Pts',(-9.83548571069105,-38.3858811119874,
23.303144661988));
#34582=CARTESIAN_POINT('Ctrl Pts',(-9.6252057363491,-38.3738494978915,23.3160286331056));
#34583=CARTESIAN_POINT('Ctrl Pts',(-9.44518642037493,-38.3489553476491,
23.3277180509822));
#34584=CARTESIAN_POINT('Ctrl Pts',(-9.03521032534632,-38.2582890758964,
23.3547840198888));
#34585=CARTESIAN_POINT('Ctrl Pts',(-8.80842727543235,-38.1823660636285,
23.3700538834943));
#34586=CARTESIAN_POINT('Ctrl Pts',(-8.54436482382719,-38.0617336899138,
23.387714922686));
#34587=CARTESIAN_POINT('Ctrl Pts',(-8.49775787613767,-38.0391373772526,
23.390830489602));
#34588=CARTESIAN_POINT('Ctrl Pts',(-8.42485451841121,-38.0017047546445,
23.3957033796484));
#34589=CARTESIAN_POINT('Ctrl Pts',(-8.39820847715695,-37.9875707067175,
23.3974843336162));
#34590=CARTESIAN_POINT('Ctrl Pts',(-8.35085531054139,-37.9616371497472,
23.4006501625686));
#34591=CARTESIAN_POINT('Ctrl Pts',(-8.33007753945989,-37.9499714968297,
23.4020395824929));
#34592=CARTESIAN_POINT('Ctrl Pts',(-8.28157722534894,-37.9220644103186,
23.4052844318827));
#34593=CARTESIAN_POINT('Ctrl Pts',(-8.25395890360866,-37.9056458562175,
23.4071334417713));
#34594=CARTESIAN_POINT('Ctrl Pts',(-8.17268069860289,-37.8557501323348,
23.4125821060863));
#34595=CARTESIAN_POINT('Ctrl Pts',(-8.11971828912701,-37.8211604057424,
23.416141774823));
#34596=CARTESIAN_POINT('Ctrl Pts',(-7.93654824841711,-37.6940809644331,
23.4285286780925));
#34597=CARTESIAN_POINT('Ctrl Pts',(-7.81193341496044,-37.5938920255088,
23.4370847052617));
#34598=CARTESIAN_POINT('Ctrl Pts',(-7.54701195905143,-37.3481712643646,
23.4562779408289));
#34599=CARTESIAN_POINT('Ctrl Pts',(-7.41172423186079,-37.1981524233418,
23.4668293920215));
#34600=CARTESIAN_POINT('Ctrl Pts',(-7.25753326725108,-36.9930642822274,
23.4810612625621));
#34601=CARTESIAN_POINT('Ctrl Pts',(-7.22556390326457,-36.9483153418577,
23.4841575152034));
#34602=CARTESIAN_POINT('Ctrl Pts',(-7.18243226498748,-36.8847266767542,
23.4885743706552));
#34603=CARTESIAN_POINT('Ctrl Pts',(-7.17034112097579,-36.8665243533994,
23.4898406012223));
#34604=CARTESIAN_POINT('Ctrl Pts',(-7.15013825211101,-36.8354629376268,
23.4920068378794));
#34605=CARTESIAN_POINT('Ctrl Pts',(-7.14193531276381,-36.822663549731,23.492901052687));
#34606=CARTESIAN_POINT('Ctrl Pts',(-7.12480973069822,-36.7955418959299,
23.4947999599309));
#34607=CARTESIAN_POINT('Ctrl Pts',(-7.11590761350785,-36.7812076982218,
23.4958058059921));
#34608=CARTESIAN_POINT('Ctrl Pts',(-7.09149913517007,-36.7412424228365,
23.4986151084747));
#34609=CARTESIAN_POINT('Ctrl Pts',(-7.07622533069247,-36.715471948305,23.5004321375612));
#34610=CARTESIAN_POINT('Ctrl Pts',(-6.97673175715375,-36.5424138805786,
23.5126535679864));
#34611=CARTESIAN_POINT('Ctrl Pts',(-6.90333759894026,-36.3891952764166,
23.5235547410299));
#34612=CARTESIAN_POINT('Ctrl Pts',(-6.75053742216397,-35.9972141772379,
23.5506687645879));
#34613=CARTESIAN_POINT('Ctrl Pts',(-6.68560622531708,-35.7538400602735,
23.5667839378455));
#34614=CARTESIAN_POINT('Ctrl Pts',(-6.64052294392229,-35.4549034333119,
23.5851580632396));
#34615=CARTESIAN_POINT('Ctrl Pts',(-6.63403877164963,-35.4041394072019,
23.5882337708725));
#34616=CARTESIAN_POINT('Ctrl Pts',(-6.62560612918472,-35.3236602908664,
23.5930417801839));
#34617=CARTESIAN_POINT('Ctrl Pts',(-6.6228956525964,-35.2940345056107,23.5947972151775));
#34618=CARTESIAN_POINT('Ctrl Pts',(-6.61850537903817,-35.2379152297356,
23.5980961604659));
#34619=CARTESIAN_POINT('Ctrl Pts',(-6.61674612479648,-35.2114303740201,
23.5996420010538));
#34620=CARTESIAN_POINT('Ctrl Pts',(-6.61343724596228,-35.1508682745644,
23.6031527918713));
#34621=CARTESIAN_POINT('Ctrl Pts',(-6.61209054415758,-35.1167825455154,
23.6051113752996));
#34622=CARTESIAN_POINT('Ctrl Pts',(-6.60944386494779,-35.0083069601176,
23.6112938448838));
#34623=CARTESIAN_POINT('Ctrl Pts',(-6.6100781074341,-34.9338897022159,23.6154590467951));
#34624=CARTESIAN_POINT('Ctrl Pts',(-6.61756186888467,-34.753425244386,23.6254259231571));
#34625=CARTESIAN_POINT('Ctrl Pts',(-6.62694851964493,-34.6475619564078,
23.6311589136535));
#34626=CARTESIAN_POINT('Ctrl Pts',(-6.65796802398009,-34.4199289329964,
23.6434301671122));
#34627=CARTESIAN_POINT('Ctrl Pts',(-6.68132093506506,-34.2985518921759,
23.6499375610396));
#34628=CARTESIAN_POINT('Ctrl Pts',(-6.74609655649723,-34.0391626945003,
23.6641690918936));
#34629=CARTESIAN_POINT('Ctrl Pts',(-6.78979213682082,-33.901977345488,23.6719027159648));
#34630=CARTESIAN_POINT('Ctrl Pts',(-6.85500491518204,-33.7348205297763,
23.6820342088643));
#34631=CARTESIAN_POINT('Ctrl Pts',(-6.86846901528448,-33.7018526058065,
23.6840682832975));
#34632=CARTESIAN_POINT('Ctrl Pts',(-6.88952781414028,-33.6525235179322,
23.6871748631689));
#34633=CARTESIAN_POINT('Ctrl Pts',(-6.89673821474192,-33.6359998719865,
23.6882262688977));
#34634=CARTESIAN_POINT('Ctrl Pts',(-6.91016583274607,-33.6058862287929,
23.6901636098934));
#34635=CARTESIAN_POINT('Ctrl Pts',(-6.91634159756907,-33.5922787141369,
23.6910471428099));
#34636=CARTESIAN_POINT('Ctrl Pts',(-6.93091106840179,-33.5607326788209,
23.6931141493239));
#34637=CARTESIAN_POINT('Ctrl Pts',(-6.93937220442957,-33.5428264526464,
23.694301494231));
#34638=CARTESIAN_POINT('Ctrl Pts',(-6.96773465624343,-33.4841401759713,
23.6982369190404));
#34639=CARTESIAN_POINT('Ctrl Pts',(-6.9882971767302,-33.443687112948,23.7010200860654));
#34640=CARTESIAN_POINT('Ctrl Pts',(-7.04123950430119,-33.3445131015472,
23.707997780355));
#34641=CARTESIAN_POINT('Ctrl Pts',(-7.07456107777427,-33.2863177814506,
23.7122297590936));
#34642=CARTESIAN_POINT('Ctrl Pts',(-7.25681623951452,-32.9888370647024,
23.7344557312121));
#34643=CARTESIAN_POINT('Ctrl Pts',(-7.43347240524709,-32.7677798443104,
23.7529007125881));
#34644=CARTESIAN_POINT('Ctrl Pts',(-7.69267842377447,-32.5154378570647,
23.7753098168571));
#34645=CARTESIAN_POINT('Ctrl Pts',(-7.75185067938511,-32.4617706754214,
23.7801806313066));
#34646=CARTESIAN_POINT('Ctrl Pts',(-7.83753258748941,-32.3894096367838,
23.7869015435543));
#34647=CARTESIAN_POINT('Ctrl Pts',(-7.86249483829816,-32.3689319380587,
23.7888222420256));
#34648=CARTESIAN_POINT('Ctrl Pts',(-7.90878120517758,-32.3320546613213,
23.7923170393959));
#34649=CARTESIAN_POINT('Ctrl Pts',(-7.93001505060156,-32.3155464709985,
23.7938953333241));
#34650=CARTESIAN_POINT('Ctrl Pts',(-7.97377293734329,-32.282354984855,23.7970983145203));
#34651=CARTESIAN_POINT('Ctrl Pts',(-7.99631195689883,-32.2656948172535,
23.7987220349153));
#34652=CARTESIAN_POINT('Ctrl Pts',(-8.05377661773693,-32.224310822668,23.80279825973));
#34653=CARTESIAN_POINT('Ctrl Pts',(-8.08896908041864,-32.1999648362236,
23.8052364805353));
#34654=CARTESIAN_POINT('Ctrl Pts',(-8.25115199474961,-32.0922499406877,
23.8162264931445));
#34655=CARTESIAN_POINT('Ctrl Pts',(-8.38320221879958,-32.0168051495611,
23.8244906097043));
#34656=CARTESIAN_POINT('Ctrl Pts',(-8.56042531927445,-31.9307882131128,
23.8350306602775));
#34657=CARTESIAN_POINT('Ctrl Pts',(-8.60135950282255,-31.911919512682,23.837429898961));
#34658=CARTESIAN_POINT('Ctrl Pts',(-8.82835529851998,-31.8127249721091,
23.8505875494917));
#34659=CARTESIAN_POINT('Ctrl Pts',(-9.02093949721846,-31.7484003248942,
23.8611927633129));
#34660=CARTESIAN_POINT('Ctrl Pts',(-9.270449647207,-31.6892513907292,23.8754287775475));
#34661=CARTESIAN_POINT('Ctrl Pts',(-9.32308914197298,-31.6780892375746,
23.8784605562108));
#34662=CARTESIAN_POINT('Ctrl Pts',(-9.39725792566655,-31.6641978213119,
23.8827996267804));
#34663=CARTESIAN_POINT('Ctrl Pts',(-9.41858407477265,-31.6604147483941,
23.8840550111149));
#34664=CARTESIAN_POINT('Ctrl Pts',(-9.45490728261951,-31.6543297887092,
23.8862085799005));
#34665=CARTESIAN_POINT('Ctrl Pts',(-9.46988654740198,-31.6519236933609,
23.8871011446386));
#34666=CARTESIAN_POINT('Ctrl Pts',(-9.50164327201351,-31.6470411229716,
23.889003590587));
#34667=CARTESIAN_POINT('Ctrl Pts',(-9.51842370899059,-31.6445899046113,
23.8900147129457));
#34668=CARTESIAN_POINT('Ctrl Pts',(-9.56529403486736,-31.6381021021548,
23.8928539274645));
#34669=CARTESIAN_POINT('Ctrl Pts',(-9.59542009108317,-31.634343792011,23.8946960429954));
#34670=CARTESIAN_POINT('Ctrl Pts',(-9.79981789317652,-31.611628420839,23.9072925210599));
#34671=CARTESIAN_POINT('Ctrl Pts',(-9.97526950691085,-31.6058118904308,
23.9185738642919));
#34672=CARTESIAN_POINT('Ctrl Pts',(-10.3933747781349,-31.6243769869812,
23.9455507285583));
#34673=CARTESIAN_POINT('Ctrl Pts',(-10.6345530369694,-31.6612949652629,
23.961141443297));
#34674=CARTESIAN_POINT('Ctrl Pts',(-10.9193819838988,-31.7369061772017,
23.9790634071563));
#34675=CARTESIAN_POINT('Ctrl Pts',(-10.9687336709589,-31.7512156064774,
23.9821534868314));
#34676=CARTESIAN_POINT('Ctrl Pts',(-11.0464279570525,-31.7756709325043,
23.9869959303421));
#34677=CARTESIAN_POINT('Ctrl Pts',(-11.0749920456646,-31.7850814016771,
23.9887714324808));
#34678=CARTESIAN_POINT('Ctrl Pts',(-11.125967887394,-31.8026308238658,23.9919323590753));
#34679=CARTESIAN_POINT('Ctrl Pts',(-11.1484258698202,-31.8106283696777,
23.9933222493374));
#34680=CARTESIAN_POINT('Ctrl Pts',(-11.2010610211555,-31.8300004115753,
23.9965742897645));
#34681=CARTESIAN_POINT('Ctrl Pts',(-11.2311642225951,-31.8415700535238,
23.998429922751));
#34682=CARTESIAN_POINT('Ctrl Pts',(-11.3203962394804,-31.8773344864136,
24.0039211067087));
#34683=CARTESIAN_POINT('Ctrl Pts',(-11.3790126147566,-31.9027736493883,
24.0075156888564));
#34684=CARTESIAN_POINT('Ctrl Pts',(-11.5858996660041,-31.9996001644871,
24.0202021968438));
#34685=CARTESIAN_POINT('Ctrl Pts',(-11.7296538869797,-32.0801060843263,
24.0290039686395));
#34686=CARTESIAN_POINT('Ctrl Pts',(-12.0438125389283,-32.2874160022344,
24.048985853139));
#34687=CARTESIAN_POINT('Ctrl Pts',(-12.2092816530836,-32.4203995041232,
24.0600735199346));
#34688=CARTESIAN_POINT('Ctrl Pts',(-12.393087090061,-32.5988525326871,24.0744171755984));
#34689=CARTESIAN_POINT('Ctrl Pts',(-12.4243195403229,-32.6303904623322,
24.0769356056674));
#34690=CARTESIAN_POINT('Ctrl Pts',(-12.4683199746456,-32.6766018300751,
24.0806185107391));
#34691=CARTESIAN_POINT('Ctrl Pts',(-12.4815961412126,-32.6907873405985,
24.0817481056172));
#34692=CARTESIAN_POINT('Ctrl Pts',(-12.5048644784994,-32.7160818237243,
24.0837623146084));
#34693=CARTESIAN_POINT('Ctrl Pts',(-12.5149062735316,-32.7271439300249,
24.084643267543));
#34694=CARTESIAN_POINT('Ctrl Pts',(-12.5369240889633,-32.7517234727664,
24.0866012363964));
#34695=CARTESIAN_POINT('Ctrl Pts',(-12.548865280149,-32.7652702786513,24.0876805407923));
#34696=CARTESIAN_POINT('Ctrl Pts',(-12.584131396493,-32.805928654695,24.0909187230498));
#34697=CARTESIAN_POINT('Ctrl Pts',(-12.6071354052805,-32.8333138431699,
24.093098249348));
#34698=CARTESIAN_POINT('Ctrl Pts',(-12.7204882791658,-32.9726743106362,
24.104160264052));
#34699=CARTESIAN_POINT('Ctrl Pts',(-12.8040703056619,-33.0899504987808,
24.1133698032258));
#34700=CARTESIAN_POINT('Ctrl Pts',(-12.9994144334242,-33.4046224791904,
24.1372187559737));
#34701=CARTESIAN_POINT('Ctrl Pts',(-13.0993092042049,-33.6085900380416,
24.1518424645592));
#34702=CARTESIAN_POINT('Ctrl Pts',(-13.1783251486862,-33.8215880661724,
24.1658778257468));
#34703=CARTESIAN_POINT('Ctrl Pts',(-13.1785377141563,-33.822161540685,24.1659156062566));
#34704=CARTESIAN_POINT('Ctrl Pts',(-13.1787501240175,-33.8227350716349,
24.1659533822777));
#34705=CARTESIAN_POINT('Origin',(-10.,-35.,23.));
#34706=CARTESIAN_POINT('',(-13.1787501041971,-33.8227350181174,25.4139789249709));
#34707=CARTESIAN_POINT('',(-13.1787501240264,-33.8227350716589,25.0733224007726));
#34708=CARTESIAN_POINT('',(-13.1787501240207,-33.8227350716434,23.));
#34709=CARTESIAN_POINT('Ctrl Pts',(-13.1787501240264,-33.8227350716589,
25.0733224007726));
#34710=CARTESIAN_POINT('Ctrl Pts',(-13.1777037596094,-33.8199097679058,
25.0731373103509));
#34711=CARTESIAN_POINT('Ctrl Pts',(-13.1766536278777,-33.8170858576181,
25.0729520551845));
#34712=CARTESIAN_POINT('Ctrl Pts',(-13.1105312555146,-33.6399991599586,
25.061318838559));
#34713=CARTESIAN_POINT('Ctrl Pts',(-13.03123358399,-33.4713992994131,25.0492945094602));
#34714=CARTESIAN_POINT('Ctrl Pts',(-12.859508122886,-33.1727790714007,25.0270938575118));
#34715=CARTESIAN_POINT('Ctrl Pts',(-12.7709567695585,-33.0410898103502,
25.0169318539089));
#34716=CARTESIAN_POINT('Ctrl Pts',(-12.6145332893973,-32.8404112798225,
25.0010574830173));
#34717=CARTESIAN_POINT('Ctrl Pts',(-12.552368643226,-32.7672831003161,24.9951762428979));
#34718=CARTESIAN_POINT('Ctrl Pts',(-12.4618136261793,-32.6694909035106,
24.9871757644255));
#34719=CARTESIAN_POINT('Ctrl Pts',(-12.4359952175913,-32.642516925621,24.9849533853306));
#34720=CARTESIAN_POINT('Ctrl Pts',(-12.3907465244094,-32.5967802616235,
24.9811564238413));
#34721=CARTESIAN_POINT('Ctrl Pts',(-12.3715283686053,-32.5778135260492,
24.9795729741009));
#34722=CARTESIAN_POINT('Ctrl Pts',(-12.3316579991339,-32.5393942289379,
24.976346116251));
#34723=CARTESIAN_POINT('Ctrl Pts',(-12.3109840539793,-32.5199672262558,
24.9747038621571));
#34724=CARTESIAN_POINT('Ctrl Pts',(-12.2572818440721,-32.4707587587375,
24.9705146713141));
#34725=CARTESIAN_POINT('Ctrl Pts',(-12.2239064735533,-32.441363090422,24.9679837318499));
#34726=CARTESIAN_POINT('Ctrl Pts',(-12.051759736685,-32.2956572505476,24.9552725652429));
#34727=CARTESIAN_POINT('Ctrl Pts',(-11.9044025749955,-32.1899380234172,
24.9455152308359));
#34728=CARTESIAN_POINT('Ctrl Pts',(-11.5952888492264,-32.0037049552123,
24.9263185053184));
#34729=CARTESIAN_POINT('Ctrl Pts',(-11.4341568436961,-31.9233267497013,
24.9169035832575));
#34730=CARTESIAN_POINT('Ctrl Pts',(-11.190539411228,-31.8251153799393,24.9025774546773));
#34731=CARTESIAN_POINT('Ctrl Pts',(-11.112552554242,-31.7969543904365,24.8979758074541));
#34732=CARTESIAN_POINT('Ctrl Pts',(-11.0102705949371,-31.7642065287768,
24.8918282026853));
#34733=CARTESIAN_POINT('Ctrl Pts',(-10.9868430939097,-31.7569849372781,
24.890412583451));
#34734=CARTESIAN_POINT('Ctrl Pts',(-10.9482790901677,-31.7455540268332,
24.8880669355799));
#34735=CARTESIAN_POINT('Ctrl Pts',(-10.9331875284635,-31.7411945677443,
24.8871451520212));
#34736=CARTESIAN_POINT('Ctrl Pts',(-10.9045301716943,-31.7331317800673,
24.8853865735951));
#34737=CARTESIAN_POINT('Ctrl Pts',(-10.8909705841274,-31.7294076682649,
24.8845510413255));
#34738=CARTESIAN_POINT('Ctrl Pts',(-10.8541917129508,-31.7195521176187,
24.8822761980079));
#34739=CARTESIAN_POINT('Ctrl Pts',(-10.830930246086,-31.713583007912,24.8808282337519));
#34740=CARTESIAN_POINT('Ctrl Pts',(-10.7386138374729,-31.6909364876734,
24.8750507733567));
#34741=CARTESIAN_POINT('Ctrl Pts',(-10.6691091929677,-31.6761854416009,
24.8706328341077));
#34742=CARTESIAN_POINT('Ctrl Pts',(-10.3914354597829,-31.6263164408925,
24.8528434475071));
#34743=CARTESIAN_POINT('Ctrl Pts',(-10.1806449343159,-31.6084913805317,
24.8390639713098));
#34744=CARTESIAN_POINT('Ctrl Pts',(-9.8050428765181,-31.6118638516153,24.8150813786961));
#34745=CARTESIAN_POINT('Ctrl Pts',(-9.64082993207185,-31.6253171939246,
24.8047837523791));
#34746=CARTESIAN_POINT('Ctrl Pts',(-9.43518396737897,-31.6573535366117,
24.7922137639916));
#34747=CARTESIAN_POINT('Ctrl Pts',(-9.39227501204829,-31.6648878378857,
24.7896081305403));
#34748=CARTESIAN_POINT('Ctrl Pts',(-9.32186304665412,-31.6786554559428,
24.7853589910096));
#34749=CARTESIAN_POINT('Ctrl Pts',(-9.2942723693428,-31.6844083648889,24.7837007465797));
#34750=CARTESIAN_POINT('Ctrl Pts',(-9.2405918998506,-31.6963016838651,24.7804867126448));
#34751=CARTESIAN_POINT('Ctrl Pts',(-9.2144969265699,-31.7024087262599,24.7789300080147));
#34752=CARTESIAN_POINT('Ctrl Pts',(-9.15184397193125,-31.7178574146537,
24.7752047757453));
#34753=CARTESIAN_POINT('Ctrl Pts',(-9.11536377024632,-31.7275013367975,
24.7730459467168));
#34754=CARTESIAN_POINT('Ctrl Pts',(-8.99053105994283,-31.7627422400702,
24.7656867285968));
#34755=CARTESIAN_POINT('Ctrl Pts',(-8.90306050369842,-31.7913256589993,
24.7605802564749));
#34756=CARTESIAN_POINT('Ctrl Pts',(-8.56669974555132,-31.916606648316,24.7409730465801));
#34757=CARTESIAN_POINT('Ctrl Pts',(-8.32844245781738,-32.0389950659119,
24.7272239332942));
#34758=CARTESIAN_POINT('Ctrl Pts',(-8.05233236780887,-32.2248709460987,
24.7091958965059));
#34759=CARTESIAN_POINT('Ctrl Pts',(-7.99873727330996,-32.263268901778,24.7055815331206));
#34760=CARTESIAN_POINT('Ctrl Pts',(-7.91062939412495,-32.3303660067952,
24.6993832720935));
#34761=CARTESIAN_POINT('Ctrl Pts',(-7.87550446549777,-32.3582328805144,
24.6968400688663));
#34762=CARTESIAN_POINT('Ctrl Pts',(-7.82574694359087,-32.3993429048742,
24.6931153189437));
#34763=CARTESIAN_POINT('Ctrl Pts',(-7.81065979865678,-32.4120310817214,
24.6919692581946));
#34764=CARTESIAN_POINT('Ctrl Pts',(-7.7843369962257,-32.4345632661665,24.6899384713474));
#34765=CARTESIAN_POINT('Ctrl Pts',(-7.77305440585038,-32.4443510628681,
24.6890576749047));
#34766=CARTESIAN_POINT('Ctrl Pts',(-7.74824537923675,-32.4661622615566,
24.6870975337613));
#34767=CARTESIAN_POINT('Ctrl Pts',(-7.73475046598716,-32.4782194637301,
24.6860158647647));
#34768=CARTESIAN_POINT('Ctrl Pts',(-7.6947303294352,-32.5145563993446,24.682763361456));
#34769=CARTESIAN_POINT('Ctrl Pts',(-7.66849503062537,-32.5391500448926,
24.6805716192283));
#34770=CARTESIAN_POINT('Ctrl Pts',(-7.53448594092292,-32.6688403226377,
24.6690857645331));
#34771=CARTESIAN_POINT('Ctrl Pts',(-7.43341640947634,-32.7806067077771,
24.6594336963436));
#34772=CARTESIAN_POINT('Ctrl Pts',(-7.25870959952693,-33.0017562762593,
24.6412775559854));
#34773=CARTESIAN_POINT('Ctrl Pts',(-7.18335653062317,-33.1094516690399,
24.6327981474552));
#34774=CARTESIAN_POINT('Ctrl Pts',(-7.03793256607087,-33.3453642949642,
24.6151884792975));
#34775=CARTESIAN_POINT('Ctrl Pts',(-6.969505030181,-33.4742962776749,24.606109752659));
#34776=CARTESIAN_POINT('Ctrl Pts',(-6.89218229929252,-33.6458697615538,
24.5947561331348));
#34777=CARTESIAN_POINT('Ctrl Pts',(-6.87550208800552,-33.6848146118189,
24.5922243676755));
#34778=CARTESIAN_POINT('Ctrl Pts',(-6.84903845778761,-33.7499491557499,
24.5880630162852));
#34779=CARTESIAN_POINT('Ctrl Pts',(-6.83884146638376,-33.7759646455863,
24.5864198872428));
#34780=CARTESIAN_POINT('Ctrl Pts',(-6.81944242775695,-33.8273171685963,
24.5832125741429));
#34781=CARTESIAN_POINT('Ctrl Pts',(-6.81021864308454,-33.8526437127554,
24.5816477718171));
#34782=CARTESIAN_POINT('Ctrl Pts',(-6.79053277593163,-33.9087699276644,
24.5782160781016));
#34783=CARTESIAN_POINT('Ctrl Pts',(-6.78020988729705,-33.939615792822,24.5763537937888));
#34784=CARTESIAN_POINT('Ctrl Pts',(-6.74587268238143,-34.0473469306297,
24.5699270820992));
#34785=CARTESIAN_POINT('Ctrl Pts',(-6.72415488617519,-34.1249385080632,
24.5654350586408));
#34786=CARTESIAN_POINT('Ctrl Pts',(-6.63925294291248,-34.4760244381511,
24.5455916288613));
#34787=CARTESIAN_POINT('Ctrl Pts',(-6.60742110607607,-34.7559303116643,
24.5311629748319));
#34788=CARTESIAN_POINT('Ctrl Pts',(-6.61116905249123,-35.103506303396,24.5123486145624));
#34789=CARTESIAN_POINT('Ctrl Pts',(-6.61387482203468,-35.1704233714469,
24.5086797101106));
#34790=CARTESIAN_POINT('Ctrl Pts',(-6.62173269143315,-35.2824363383509,
24.5023979788015));
#34791=CARTESIAN_POINT('Ctrl Pts',(-6.62581194236091,-35.3275894322445,
24.4998272876006));
#34792=CARTESIAN_POINT('Ctrl Pts',(-6.63297163165144,-35.3923225438618,
24.4960694337222));
#34793=CARTESIAN_POINT('Ctrl Pts',(-6.63532034145911,-35.4119802981523,
24.4949186339168));
#34794=CARTESIAN_POINT('Ctrl Pts',(-6.63974378192479,-35.4464375836497,
24.4928827674385));
#34795=CARTESIAN_POINT('Ctrl Pts',(-6.64174439099302,-35.461245726155,24.4920017050168));
#34796=CARTESIAN_POINT('Ctrl Pts',(-6.64637548459245,-35.4938956236464,
24.4900451449926));
#34797=CARTESIAN_POINT('Ctrl Pts',(-6.64905043774846,-35.5117296908787,
24.4889673823148));
#34798=CARTESIAN_POINT('Ctrl Pts',(-6.65743468330857,-35.5647408057601,
24.485738519422));
#34799=CARTESIAN_POINT('Ctrl Pts',(-6.66355638595195,-35.5998490372737,
24.4835669388163));
#34800=CARTESIAN_POINT('Ctrl Pts',(-6.69729039371144,-35.7767821809214,
24.4724765897741));
#34801=CARTESIAN_POINT('Ctrl Pts',(-6.73339539780418,-35.9168255296127,
24.4632272721264));
#34802=CARTESIAN_POINT('Ctrl Pts',(-6.81678009774279,-36.1716706251502,
24.4459608456862));
#34803=CARTESIAN_POINT('Ctrl Pts',(-6.86164576670486,-36.2870257574511,
24.4379696851665));
#34804=CARTESIAN_POINT('Ctrl Pts',(-6.9563661274185,-36.4959521922733,24.4233450031194));
#34805=CARTESIAN_POINT('Ctrl Pts',(-7.00449857195458,-36.5901428467637,
24.4166898999895));
#34806=CARTESIAN_POINT('Ctrl Pts',(-7.09375258837058,-36.7463189936019,
24.4055912703018));
#34807=CARTESIAN_POINT('Ctrl Pts',(-7.13265177899439,-36.8094804493413,
24.4010830628702));
#34808=CARTESIAN_POINT('Ctrl Pts',(-7.19240189958801,-36.8997259456667,
24.3946108353764));
#34809=CARTESIAN_POINT('Ctrl Pts',(-7.21163747058635,-36.9278486179572,
24.3925892584952));
#34810=CARTESIAN_POINT('Ctrl Pts',(-7.24660475850377,-36.9773527611934,
24.3890210540228));
#34811=CARTESIAN_POINT('Ctrl Pts',(-7.26216954724209,-36.9988481106571,
24.3874683641327));
#34812=CARTESIAN_POINT('Ctrl Pts',(-7.295727707954,-37.0440652463354,24.3841940140367));
#34813=CARTESIAN_POINT('Ctrl Pts',(-7.31378448124538,-37.0677373211333,
24.3824749563784));
#34814=CARTESIAN_POINT('Ctrl Pts',(-7.36378710284971,-37.1315291208781,
24.3778266265635));
#34815=CARTESIAN_POINT('Ctrl Pts',(-7.39633588030019,-37.1711675134272,
24.3749210020832));
#34816=CARTESIAN_POINT('Ctrl Pts',(-7.59283026622022,-37.3996846906618,
24.3580314469152));
#34817=CARTESIAN_POINT('Ctrl Pts',(-7.77637103877369,-37.5706882477391,
24.3448941107025));
#34818=CARTESIAN_POINT('Ctrl Pts',(-8.11353617574474,-37.8214508688737,
24.3225781722141));
#34819=CARTESIAN_POINT('Ctrl Pts',(-8.25743678234348,-37.9125232396933,
24.3134867302454));
#34820=CARTESIAN_POINT('Ctrl Pts',(-8.43418665700761,-38.0065835303801,
24.3021118298687));
#34821=CARTESIAN_POINT('Ctrl Pts',(-8.46101698582948,-38.0204051217703,
24.3003795694543));
#34822=CARTESIAN_POINT('Ctrl Pts',(-8.50317187264601,-38.0414136422275,
24.2976437774197));
#34823=CARTESIAN_POINT('Ctrl Pts',(-8.51837240181083,-38.0488474903851,
24.2966544580675));
#34824=CARTESIAN_POINT('Ctrl Pts',(-8.54731852613893,-38.0627360629923,
24.2947639889825));
#34825=CARTESIAN_POINT('Ctrl Pts',(-8.56105277922902,-38.0692126868888,
24.2938641411524));
#34826=CARTESIAN_POINT('Ctrl Pts',(-8.59455814967905,-38.0847384087863,
24.2916625817283));
#34827=CARTESIAN_POINT('Ctrl Pts',(-8.61437352309773,-38.0936898773976,
24.2903552937946));
#34828=CARTESIAN_POINT('Ctrl Pts',(-8.68398513447013,-38.1243335486597,
24.2857479243447));
#34829=CARTESIAN_POINT('Ctrl Pts',(-8.7342132110815,-38.1450180236902,24.282397184276));
#34830=CARTESIAN_POINT('Ctrl Pts',(-8.97367527450129,-38.236965710208,24.2663695794947));
#34831=CARTESIAN_POINT('Ctrl Pts',(-9.16853643458028,-38.2924084356933,
24.2532006209466));
#34832=CARTESIAN_POINT('Ctrl Pts',(-9.55643201873365,-38.3661203646877,
24.2278562357609));
#34833=CARTESIAN_POINT('Ctrl Pts',(-9.74843809505455,-38.3858905111979,
24.2157101759797));
#34834=CARTESIAN_POINT('Ctrl Pts',(-9.98588834605419,-38.3900164914881,
24.2013513859106));
#34835=CARTESIAN_POINT('Ctrl Pts',(-10.0306812641088,-38.3899070634982,
24.1986700591061));
#34836=CARTESIAN_POINT('Ctrl Pts',(-10.1038862041232,-38.3882770162454,
24.1943308617843));
#34837=CARTESIAN_POINT('Ctrl Pts',(-10.1323034122903,-38.3872864306022,
24.1926569942099));
#34838=CARTESIAN_POINT('Ctrl Pts',(-10.1876414829368,-38.3846599416066,
24.1894169729571));
#34839=CARTESIAN_POINT('Ctrl Pts',(-10.2145618418345,-38.383060082835,24.1878498364535));
#34840=CARTESIAN_POINT('Ctrl Pts',(-10.2785001973706,-38.3784939861124,
24.1841478573401));
#34841=CARTESIAN_POINT('Ctrl Pts',(-10.3154945775324,-38.3752403321314,
24.1820219911742));
#34842=CARTESIAN_POINT('Ctrl Pts',(-10.440554876662,-38.3621670813373,24.1748833247072));
#34843=CARTESIAN_POINT('Ctrl Pts',(-10.5282897841573,-38.3495026112845,
24.1699569627529));
#34844=CARTESIAN_POINT('Ctrl Pts',(-10.8821379423599,-38.2841732464141,
24.1502667923338));
#34845=CARTESIAN_POINT('Ctrl Pts',(-11.1419510929791,-38.2031077929201,
24.1363060898995));
#34846=CARTESIAN_POINT('Ctrl Pts',(-11.4497562110455,-38.064800448062,24.1180326370402));
#34847=CARTESIAN_POINT('Ctrl Pts',(-11.5093790202929,-38.0358802602029,
24.1144006674799));
#34848=CARTESIAN_POINT('Ctrl Pts',(-11.6080050806346,-37.9844177633764,
24.1081754427482));
#34849=CARTESIAN_POINT('Ctrl Pts',(-11.6474768113919,-37.9628110775127,
24.1056233445802));
#34850=CARTESIAN_POINT('Ctrl Pts',(-11.7036288203203,-37.9306046478162,
24.1018878794908));
#34851=CARTESIAN_POINT('Ctrl Pts',(-11.7206662814277,-37.9206338809392,
24.100740281153));
#34852=CARTESIAN_POINT('Ctrl Pts',(-11.7504423115027,-37.9028572053049,
24.0987078493396));
#34853=CARTESIAN_POINT('Ctrl Pts',(-11.7632178752809,-37.8951150153885,
24.0978269697308));
#34854=CARTESIAN_POINT('Ctrl Pts',(-11.7913389761971,-37.8778180071843,
24.0958680042558));
#34855=CARTESIAN_POINT('Ctrl Pts',(-11.80665933728,-37.8682248546455,24.0947876134484));
#34856=CARTESIAN_POINT('Ctrl Pts',(-11.8512089351539,-37.8398306917014,
24.091609051988));
#34857=CARTESIAN_POINT('Ctrl Pts',(-11.8802258171739,-37.8207026702786,
24.0894917961642));
#34858=CARTESIAN_POINT('Ctrl Pts',(-12.0617385625394,-37.6970036602281,
24.0759730861485));
#34859=CARTESIAN_POINT('Ctrl Pts',(-12.2057476118327,-37.5805546601346,
24.0640234658594));
#34860=CARTESIAN_POINT('Ctrl Pts',(-12.4547259282142,-37.3430889791939,
24.0418486337316));
#34861=CARTESIAN_POINT('Ctrl Pts',(-12.5620456576854,-37.225235939274,24.0316396997669));
#34862=CARTESIAN_POINT('Ctrl Pts',(-12.720280298216,-37.0247789155064,24.0157046819958));
#34863=CARTESIAN_POINT('Ctrl Pts',(-12.7766335035764,-36.9467828968309,
24.0098079991194));
#34864=CARTESIAN_POINT('Ctrl Pts',(-12.8501730243033,-36.8352970124455,
24.0017906735044));
#34865=CARTESIAN_POINT('Ctrl Pts',(-12.8702319900878,-36.803765473424,23.9995663076097));
#34866=CARTESIAN_POINT('Ctrl Pts',(-12.903882433553,-36.7488856908229,23.9957670377681));
#34867=CARTESIAN_POINT('Ctrl Pts',(-12.9177234441872,-36.725695313065,23.9941832379845));
#34868=CARTESIAN_POINT('Ctrl Pts',(-12.9455273160126,-36.6778194288057,
23.9909565988483));
#34869=CARTESIAN_POINT('Ctrl Pts',(-12.959460508519,-36.6531191047775,23.9893149016175));
#34870=CARTESIAN_POINT('Ctrl Pts',(-12.994418941029,-36.5892870530843,23.9851290780429));
#34871=CARTESIAN_POINT('Ctrl Pts',(-13.0149882672211,-36.5499110094683,
23.9826008970126));
#34872=CARTESIAN_POINT('Ctrl Pts',(-13.1096368043195,-36.3597053322764,
23.9706263010761));
#34873=CARTESIAN_POINT('Ctrl Pts',(-13.1732098537437,-36.2039050022012,
23.9615372197958));
#34874=CARTESIAN_POINT('Ctrl Pts',(-13.2835703195063,-35.8630016912642,
23.9424380108322));
#34875=CARTESIAN_POINT('Ctrl Pts',(-13.3268230420832,-35.6773828705033,
23.9324998099822));
#34876=CARTESIAN_POINT('Ctrl Pts',(-13.3665598520118,-35.4048804225185,
23.9174975833685));
#34877=CARTESIAN_POINT('Ctrl Pts',(-13.3756655976754,-35.3202076480346,
23.9127765415568));
#34878=CARTESIAN_POINT('Ctrl Pts',(-13.383289906604,-35.2106310184132,23.9064908535421));
#34879=CARTESIAN_POINT('Ctrl Pts',(-13.3847357889658,-35.1859558572627,
23.9050639048499));
#34880=CARTESIAN_POINT('Ctrl Pts',(-13.3866610174315,-35.1455345782663,
23.9027043891909));
#34881=CARTESIAN_POINT('Ctrl Pts',(-13.3873006950602,-35.1297965467947,
23.9017802615147));
#34882=CARTESIAN_POINT('Ctrl Pts',(-13.3883026527301,-35.1000348929821,
23.9000214294544));
#34883=CARTESIAN_POINT('Ctrl Pts',(-13.3886876081946,-35.0860123523354,
23.8991880353236));
#34884=CARTESIAN_POINT('Ctrl Pts',(-13.3894915958565,-35.0481630098936,
23.8969266057667));
#34885=CARTESIAN_POINT('Ctrl Pts',(-13.3897464126101,-35.0243339654891,
23.8954900880576));
#34886=CARTESIAN_POINT('Ctrl Pts',(-13.3897612595208,-34.9246694112491,
23.8894339278107));
#34887=CARTESIAN_POINT('Ctrl Pts',(-13.3872276505839,-34.8488601237088,
23.8847115859043));
#34888=CARTESIAN_POINT('Ctrl Pts',(-13.3720525628155,-34.6225561572871,
23.8703860111663));
#34889=CARTESIAN_POINT('Ctrl Pts',(-13.3518968174119,-34.4727547277818,
23.8606071038608));
#34890=CARTESIAN_POINT('Ctrl Pts',(-13.2871052863501,-34.1539954505898,
23.8396687482438));
#34891=CARTESIAN_POINT('Ctrl Pts',(-13.2392695055602,-33.9861443455545,
23.8285690331584));
#34892=CARTESIAN_POINT('Ctrl Pts',(-13.1787501550516,-33.8227351554304,
23.8178420415151));
#34893=CARTESIAN_POINT('',(-13.3897487153538,-35.0029511451049,24.2344127503854));
#34894=CARTESIAN_POINT('Ctrl Pts',(-13.1787501240175,-33.8227350716349,
24.1659533822777));
#34895=CARTESIAN_POINT('Ctrl Pts',(-13.2050987685498,-33.8938794292528,
24.1706393556419));
#34896=CARTESIAN_POINT('Ctrl Pts',(-13.2290530202204,-33.965892250316,24.1752555057));
#34897=CARTESIAN_POINT('Ctrl Pts',(-13.2602388283821,-34.0713398226487,
24.1818343453727));
#34898=CARTESIAN_POINT('Ctrl Pts',(-13.2694125310574,-34.1041714605046,
24.1838579400893));
#34899=CARTESIAN_POINT('Ctrl Pts',(-13.28486230881,-34.1628664636576,24.1874329555466));
#34900=CARTESIAN_POINT('Ctrl Pts',(-13.2913318785798,-34.1886754838599,
24.1889904038047));
#34901=CARTESIAN_POINT('Ctrl Pts',(-13.3043200618768,-34.243203414143,24.1922513776549));
#34902=CARTESIAN_POINT('Ctrl Pts',(-13.3107696814499,-34.2719365830112,
24.1939526121165));
#34903=CARTESIAN_POINT('Ctrl Pts',(-13.3231506591771,-34.3306649670845,
24.1973967439237));
#34904=CARTESIAN_POINT('Ctrl Pts',(-13.3290522492268,-34.3606637065046,
24.1991385882913));
#34905=CARTESIAN_POINT('Ctrl Pts',(-13.3467253257844,-34.4573902297874,
24.2047027675562));
#34906=CARTESIAN_POINT('Ctrl Pts',(-13.356902710259,-34.5243943175358,24.2084773853082));
#34907=CARTESIAN_POINT('Ctrl Pts',(-13.3816250256084,-34.7281277796348,
24.2197649678847));
#34908=CARTESIAN_POINT('Ctrl Pts',(-13.3898684009191,-34.8654777316019,
24.2271128972712));
#34909=CARTESIAN_POINT('Ctrl Pts',(-13.3897487153538,-35.0029511451049,
24.2344127503854));
#34910=CARTESIAN_POINT('Ctrl Pts',(-13.3897487163515,-35.002949998855,24.2344126895194));
#34911=CARTESIAN_POINT('Ctrl Pts',(-13.389557470868,-35.2227040272623,24.2460816526017));
#34912=CARTESIAN_POINT('Ctrl Pts',(-13.3679972012171,-35.4419036878591,
24.2575682627097));
#34913=CARTESIAN_POINT('Ctrl Pts',(-13.3198065562547,-35.6856496526208,
24.2715260273842));
#34914=CARTESIAN_POINT('Ctrl Pts',(-13.3138742712255,-35.7137704312125,
24.2731550001771));
#34915=CARTESIAN_POINT('Ctrl Pts',(-13.302317964461,-35.765297633892,24.2761798111977));
#34916=CARTESIAN_POINT('Ctrl Pts',(-13.2968007467721,-35.7887262974359,
24.2775704471149));
#34917=CARTESIAN_POINT('Ctrl Pts',(-13.2872933619645,-35.8272552760768,
24.2798856118402));
#34918=CARTESIAN_POINT('Ctrl Pts',(-13.2834473764778,-35.8423907952853,
24.280802319444));
#34919=CARTESIAN_POINT('Ctrl Pts',(-13.2754188054373,-35.8730959907211,
24.2826777256283));
#34920=CARTESIAN_POINT('Ctrl Pts',(-13.2712294963358,-35.8886633326383,
24.2836367407879));
#34921=CARTESIAN_POINT('Ctrl Pts',(-13.2598759827137,-35.929684272583,24.286184399295));
#34922=CARTESIAN_POINT('Ctrl Pts',(-13.2525248446699,-35.9550844518139,
24.287782933385));
#34923=CARTESIAN_POINT('Ctrl Pts',(-13.2165368732437,-36.0741961793681,
24.2953699858009));
#34924=CARTESIAN_POINT('Ctrl Pts',(-13.1841443911628,-36.166716855223,24.3015283282721));
#34925=CARTESIAN_POINT('Ctrl Pts',(-13.0713591454305,-36.4489985478191,
24.3208951226771));
#34926=CARTESIAN_POINT('Ctrl Pts',(-12.977644349327,-36.6329371806667,24.3343226006404));
#34927=CARTESIAN_POINT('Ctrl Pts',(-12.817473713754,-36.8871033407532,24.3533856702217));
#34928=CARTESIAN_POINT('Ctrl Pts',(-12.7638252912858,-36.964838193712,24.3592992059404));
#34929=CARTESIAN_POINT('Ctrl Pts',(-12.6657480381098,-37.0949676548479,
24.3693201602546));
#34930=CARTESIAN_POINT('Ctrl Pts',(-12.6228456871337,-37.148437476239,24.3734764560856));
#34931=CARTESIAN_POINT('Ctrl Pts',(-12.5568640109711,-37.2257463500624,
24.3795466231905));
#34932=CARTESIAN_POINT('Ctrl Pts',(-12.5350107605126,-37.2506045734466,
24.3815083486727));
#34933=CARTESIAN_POINT('Ctrl Pts',(-12.4950445170227,-37.2947456178366,
24.3850110316012));
#34934=CARTESIAN_POINT('Ctrl Pts',(-12.4770634542439,-37.3141437498389,
24.3865572329557));
#34935=CARTESIAN_POINT('Ctrl Pts',(-12.4379371296702,-37.3553749667458,
24.3898598001322));
#34936=CARTESIAN_POINT('Ctrl Pts',(-12.4167214558623,-37.3771382318965,
24.3916129911705));
#34937=CARTESIAN_POINT('Ctrl Pts',(-12.3578077616813,-37.4359684584709,
24.3963825126837));
#34938=CARTESIAN_POINT('Ctrl Pts',(-12.3195300432494,-37.4724442503966,
24.3993735159308));
#34939=CARTESIAN_POINT('Ctrl Pts',(-12.1154255111954,-37.6580266281995,
24.4148066693152));
#34940=CARTESIAN_POINT('Ctrl Pts',(-11.9360338293216,-37.79140053632,24.4266058166952));
#34941=CARTESIAN_POINT('Ctrl Pts',(-11.577078147921,-38.0069111006793,24.4488059708313));
#34942=CARTESIAN_POINT('Ctrl Pts',(-11.4009444952813,-38.0928989344067,
24.4591763062561));
#34943=CARTESIAN_POINT('Ctrl Pts',(-11.1915248128081,-38.1735632068501,
24.4719476335477));
#34944=CARTESIAN_POINT('Ctrl Pts',(-11.1645146641302,-38.1835735091049,
24.473603172001));
#34945=CARTESIAN_POINT('Ctrl Pts',(-11.1217161260763,-38.198817675594,24.4762443519741));
#34946=CARTESIAN_POINT('Ctrl Pts',(-11.1060105763349,-38.2042818491567,
24.4772173417119));
#34947=CARTESIAN_POINT('Ctrl Pts',(-11.0759381263507,-38.2144970338249,
24.4790886989367));
#34948=CARTESIAN_POINT('Ctrl Pts',(-11.061578624952,-38.2192677462002,24.479985950123));
#34949=CARTESIAN_POINT('Ctrl Pts',(-11.025958939709,-38.2308375914742,24.4822200337298));
#34950=CARTESIAN_POINT('Ctrl Pts',(-11.0046628076571,-38.2375231077081,
24.4835630608457));
#34951=CARTESIAN_POINT('Ctrl Pts',(-10.9277882803292,-38.2608248945439,
24.4884335003926));
#34952=CARTESIAN_POINT('Ctrl Pts',(-10.8718541780812,-38.2762233685315,
24.4920190430788));
#34953=CARTESIAN_POINT('Ctrl Pts',(-10.6223486242638,-38.3380698021468,
24.5081173038665));
#34954=CARTESIAN_POINT('Ctrl Pts',(-10.4253048259013,-38.368848449039,24.5210800690393));
#34955=CARTESIAN_POINT('Ctrl Pts',(-10.0687596977649,-38.3927475661615,
24.5440117078395));
#34956=CARTESIAN_POINT('Ctrl Pts',(-9.91025244986144,-38.3922587063558,
24.5540277623386));
#34957=CARTESIAN_POINT('Ctrl Pts',(-9.68936331675368,-38.3760772867058,
24.5676024860253));
#34958=CARTESIAN_POINT('Ctrl Pts',(-9.62652036301723,-38.3697042526392,
24.5714226215228));
#34959=CARTESIAN_POINT('Ctrl Pts',(-9.53204530914583,-38.3574476241247,
24.5771045277702));
#34960=CARTESIAN_POINT('Ctrl Pts',(-9.50026127651868,-38.3528640676407,
24.5790056425006));
#34961=CARTESIAN_POINT('Ctrl Pts',(-9.44501497096434,-38.3440939518448,
24.5822929907971));
#34962=CARTESIAN_POINT('Ctrl Pts',(-9.42152322346232,-38.3401103878718,
24.5836854133492));
#34963=CARTESIAN_POINT('Ctrl Pts',(-9.36838100463392,-38.3305214226798,
24.5868238132335));
#34964=CARTESIAN_POINT('Ctrl Pts',(-9.33875923745743,-38.3247670957518,
24.5885650222385));
#34965=CARTESIAN_POINT('Ctrl Pts',(-9.25845816925667,-38.3080521345346,
24.5932655370562));
#34966=CARTESIAN_POINT('Ctrl Pts',(-9.20794615505068,-38.2963228477853,
24.5962007625502));
#34967=CARTESIAN_POINT('Ctrl Pts',(-8.92746188475293,-38.2243720739452,
24.6124133615817));
#34968=CARTESIAN_POINT('Ctrl Pts',(-8.70405324593885,-38.141249183347,24.624941401881));
#34969=CARTESIAN_POINT('Ctrl Pts',(-8.32790229774715,-37.9542740463019,
24.6472297425558));
#34970=CARTESIAN_POINT('Ctrl Pts',(-8.17147062457748,-37.8600893357387,
24.6569393433433));
#34971=CARTESIAN_POINT('Ctrl Pts',(-7.99978149385415,-37.736855025669,24.6689624963716));
#34972=CARTESIAN_POINT('Ctrl Pts',(-7.97639372514418,-37.7196078814374,
24.6706322077397));
#34973=CARTESIAN_POINT('Ctrl Pts',(-7.93993272728111,-37.6919892692622,
24.673290870923));
#34974=CARTESIAN_POINT('Ctrl Pts',(-7.92670889104122,-37.6818179181006,
24.674266888401));
#34975=CARTESIAN_POINT('Ctrl Pts',(-7.90165412414407,-37.6622505317391,
24.6761397904135));
#34976=CARTESIAN_POINT('Ctrl Pts',(-7.8898100958466,-37.6528723759848,24.6770354994564));
#34977=CARTESIAN_POINT('Ctrl Pts',(-7.8634904877021,-37.6317446232106,24.6790485325802));
#34978=CARTESIAN_POINT('Ctrl Pts',(-7.84904836924341,-37.6199541419106,
24.6801685879334));
#34979=CARTESIAN_POINT('Ctrl Pts',(-7.79883931084995,-37.5782687319091,
24.6841148188025));
#34980=CARTESIAN_POINT('Ctrl Pts',(-7.76359386597663,-37.547756893067,24.6869789411453));
#34981=CARTESIAN_POINT('Ctrl Pts',(-7.57406914437529,-37.3767227843365,
24.7028519654682));
#34982=CARTESIAN_POINT('Ctrl Pts',(-7.43239553345001,-37.2229153903095,
24.7164451304174));
#34983=CARTESIAN_POINT('Ctrl Pts',(-7.18670198487238,-36.9011195230579,
24.7424468042141));
#34984=CARTESIAN_POINT('Ctrl Pts',(-7.08138567914864,-36.7351114304078,
24.7548281053633));
#34985=CARTESIAN_POINT('Ctrl Pts',(-6.97034051022602,-36.5210470738262,
24.7694099776128));
#34986=CARTESIAN_POINT('Ctrl Pts',(-6.95045951579454,-36.4807849100586,
24.7720980970854));
#34987=CARTESIAN_POINT('Ctrl Pts',(-6.9192942610958,-36.4143786324943,24.7764453784158));
#34988=CARTESIAN_POINT('Ctrl Pts',(-6.90752958165394,-36.388467338913,24.7781206519957));
#34989=CARTESIAN_POINT('Ctrl Pts',(-6.88525848933116,-36.3377282837044,
24.7813614683322));
#34990=CARTESIAN_POINT('Ctrl Pts',(-6.87471925435066,-36.3129173476333,
24.7829280196204));
#34991=CARTESIAN_POINT('Ctrl Pts',(-6.85039335736396,-36.2536972920977,
24.7866255737663));
#34992=CARTESIAN_POINT('Ctrl Pts',(-6.8368727761614,-36.2191821941423,24.7887476605256));
#34993=CARTESIAN_POINT('Ctrl Pts',(-6.79314956497395,-36.1019393907378,
24.7958521552615));
#34994=CARTESIAN_POINT('Ctrl Pts',(-6.76560407892482,-36.0182558063276,
24.8007493369715));
#34995=CARTESIAN_POINT('Ctrl Pts',(-6.6664776636023,-35.672259401858,24.8204494026849));
#34996=CARTESIAN_POINT('Ctrl Pts',(-6.62331920405078,-35.4028910901985,
24.8344413777944));
#34997=CARTESIAN_POINT('Ctrl Pts',(-6.61022501780199,-35.0650144979142,
24.8527510581505));
#34998=CARTESIAN_POINT('Ctrl Pts',(-6.60960197732753,-34.9987021291413,
24.856385581082));
#34999=CARTESIAN_POINT('Ctrl Pts',(-6.61182133907472,-34.8874069387649,
24.8626147146398));
#35000=CARTESIAN_POINT('Ctrl Pts',(-6.61361546613743,-34.8424207392027,
24.8651681009589));
#35001=CARTESIAN_POINT('Ctrl Pts',(-6.61748442389753,-34.7777764802262,
24.8689051173671));
#35002=CARTESIAN_POINT('Ctrl Pts',(-6.61883618504558,-34.758078254302,24.8700529378478));
#35003=CARTESIAN_POINT('Ctrl Pts',(-6.62151287794324,-34.7234986168888,
24.8720856073144));
#35004=CARTESIAN_POINT('Ctrl Pts',(-6.62276422071056,-34.7086124099631,
24.872966498933));
#35005=CARTESIAN_POINT('Ctrl Pts',(-6.62574688776563,-34.6757352363023,
24.8749252947229));
#35006=CARTESIAN_POINT('Ctrl Pts',(-6.62752369249953,-34.6577497619699,
24.876005501044));
#35007=CARTESIAN_POINT('Ctrl Pts',(-6.63325267066989,-34.6041441034158,
24.8792491418261));
#35008=CARTESIAN_POINT('Ctrl Pts',(-6.63762589911724,-34.5685725369179,
24.8814333234479));
#35009=CARTESIAN_POINT('Ctrl Pts',(-6.66302676493493,-34.3859254697169,
24.8927895837874));
#35010=CARTESIAN_POINT('Ctrl Pts',(-6.69314215077066,-34.240288137942,24.9023107148573));
#35011=CARTESIAN_POINT('Ctrl Pts',(-6.76658094138884,-33.9745353272757,
24.9200703050858));
#35012=CARTESIAN_POINT('Ctrl Pts',(-6.80732503891533,-33.8539610898808,
24.9282833771205));
#35013=CARTESIAN_POINT('Ctrl Pts',(-6.91116848139234,-33.5955725659471,
24.9460051862209));
#35014=CARTESIAN_POINT('Ctrl Pts',(-6.97692902598639,-33.4591079773554,
24.9554407948336));
#35015=CARTESIAN_POINT('Ctrl Pts',(-7.07268868593591,-33.29029801448,24.9671537458906));
#35016=CARTESIAN_POINT('Ctrl Pts',(-7.09448263704099,-33.25351738835,24.9697092945455));
#35017=CARTESIAN_POINT('Ctrl Pts',(-7.13170346490561,-33.1933276251907,
24.9738988956297));
#35018=CARTESIAN_POINT('Ctrl Pts',(-7.14673487782694,-33.1696808212458,
24.9755468724839));
#35019=CARTESIAN_POINT('Ctrl Pts',(-7.17676900970466,-33.1237016656158,
24.9787561612413));
#35020=CARTESIAN_POINT('Ctrl Pts',(-7.19174777841637,-33.1013562247761,
24.9803181888145));
#35021=CARTESIAN_POINT('Ctrl Pts',(-7.22529801605274,-33.0525715174157,
24.9837349091707));
#35022=CARTESIAN_POINT('Ctrl Pts',(-7.24398479870379,-33.0262145237367,
24.9855851477254));
#35023=CARTESIAN_POINT('Ctrl Pts',(-7.31024396435616,-32.9355345737865,
24.991970307384));
#35024=CARTESIAN_POINT('Ctrl Pts',(-7.35971591371658,-32.8726292512907,
24.9964337567691));
#35025=CARTESIAN_POINT('Ctrl Pts',(-7.59323727156486,-32.5964087329697,
25.0163133572538));
#35026=CARTESIAN_POINT('Ctrl Pts',(-7.80119511333199,-32.4048111331099,
25.0307937211409));
#35027=CARTESIAN_POINT('Ctrl Pts',(-8.08500697919784,-32.2021972025712,
25.0496676982648));
#35028=CARTESIAN_POINT('Ctrl Pts',(-8.14070628208018,-32.1648765931853,
25.0533405193687));
#35029=CARTESIAN_POINT('Ctrl Pts',(-8.23589638556857,-32.1051076052235,
25.0596282379565));
#35030=CARTESIAN_POINT('Ctrl Pts',(-8.27479905542806,-32.0817565504525,
25.0622008953476));
#35031=CARTESIAN_POINT('Ctrl Pts',(-8.33133751215488,-32.0493453690614,
25.0659611158944));
#35032=CARTESIAN_POINT('Ctrl Pts',(-8.34860391579449,-32.0396472876639,
25.0671122530522));
#35033=CARTESIAN_POINT('Ctrl Pts',(-8.37904675691685,-32.0228975555821,
25.0691484819474));
#35034=CARTESIAN_POINT('Ctrl Pts',(-8.39218639271998,-32.0157808771441,
25.070029564123));
#35035=CARTESIAN_POINT('Ctrl Pts',(-8.42128281592764,-32.000269650466,25.0719858730274));
#35036=CARTESIAN_POINT('Ctrl Pts',(-8.43725958041177,-31.991915482223,25.073063360658));
#35037=CARTESIAN_POINT('Ctrl Pts',(-8.48402679719789,-31.9679342755029,
25.0762252483454));
#35038=CARTESIAN_POINT('Ctrl Pts',(-8.51498945259423,-31.952650202956,25.0783284484239));
#35039=CARTESIAN_POINT('Ctrl Pts',(-8.71712084217275,-31.8566842438053,
25.0920965934837));
#35040=CARTESIAN_POINT('Ctrl Pts',(-8.89454619189799,-31.7899883613176,
25.1043370156309));
#35041=CARTESIAN_POINT('Ctrl Pts',(-9.22716259565232,-31.6958184650572,
25.1266135216758));
#35042=CARTESIAN_POINT('Ctrl Pts',(-9.38051372151334,-31.6636640829672,
25.136641502814));
#35043=CARTESIAN_POINT('Ctrl Pts',(-9.62987868787729,-31.6291716481908,
25.1523422370958));
#35044=CARTESIAN_POINT('Ctrl Pts',(-9.72472321203555,-31.6201037175278,
25.1581789822731));
#35045=CARTESIAN_POINT('Ctrl Pts',(-9.85701999312256,-31.6130620443345,
25.1661308788803));
#35046=CARTESIAN_POINT('Ctrl Pts',(-9.89424008132489,-31.6116955562562,
25.1683475016195));
#35047=CARTESIAN_POINT('Ctrl Pts',(-9.95845499241266,-31.6103971879772,
25.1721377783345));
#35048=CARTESIAN_POINT('Ctrl Pts',(-9.98543981315512,-31.6101738577671,
25.1737202172129));
#35049=CARTESIAN_POINT('Ctrl Pts',(-10.0408224162439,-31.6103768622678,
25.1769477289714));
#35050=CARTESIAN_POINT('Ctrl Pts',(-10.0692179855594,-31.6108377986161,
25.1785916131774));
#35051=CARTESIAN_POINT('Ctrl Pts',(-10.1422022420484,-31.6129401917839,
25.1827906551621));
#35052=CARTESIAN_POINT('Ctrl Pts',(-10.1867710803497,-31.6151052533139,
25.1853296632776));
#35053=CARTESIAN_POINT('Ctrl Pts',(-10.4077268521521,-31.6302164811966,
25.1978103623513));
#35054=CARTESIAN_POINT('Ctrl Pts',(-10.5829611608843,-31.6560730077891,
25.2073514090393));
#35055=CARTESIAN_POINT('Ctrl Pts',(-10.9107081500622,-31.7309941693607,
25.2252453198962));
#35056=CARTESIAN_POINT('Ctrl Pts',(-11.063321650142,-31.777402845856,25.2336047440714));
#35057=CARTESIAN_POINT('Ctrl Pts',(-11.2778284180127,-31.8595361580688,
25.2460112859812));
#35058=CARTESIAN_POINT('Ctrl Pts',(-11.3427534508646,-31.8867427401561,
25.2498591920003));
#35059=CARTESIAN_POINT('Ctrl Pts',(-11.4494996777622,-31.9354347249306,
25.2564136621465));
#35060=CARTESIAN_POINT('Ctrl Pts',(-11.4918066171576,-31.9558051626408,
25.2590731907785));
#35061=CARTESIAN_POINT('Ctrl Pts',(-11.5515691203872,-31.986125257689,25.2629378511485));
#35062=CARTESIAN_POINT('Ctrl Pts',(-11.569382185958,-31.9953623829993,25.2641037151851));
#35063=CARTESIAN_POINT('Ctrl Pts',(-11.6003359971998,-32.0117641087771,
25.2661559086322));
#35064=CARTESIAN_POINT('Ctrl Pts',(-11.6135129667573,-32.018858449966,25.2670379971065));
#35065=CARTESIAN_POINT('Ctrl Pts',(-11.642297569464,-32.0346025328819,25.2689839691578));
#35066=CARTESIAN_POINT('Ctrl Pts',(-11.6578839313121,-32.0432882650192,
25.2700499376898));
#35067=CARTESIAN_POINT('Ctrl Pts',(-11.7026593526718,-32.0687053844993,
25.2731461002313));
#35068=CARTESIAN_POINT('Ctrl Pts',(-11.7316680360506,-32.0857483597004,
25.2751939895415));
#35069=CARTESIAN_POINT('Ctrl Pts',(-11.9753072010917,-32.2338115438166,
25.2927219189394));
#35070=CARTESIAN_POINT('Ctrl Pts',(-12.1749888619193,-32.3879025223372,
25.3092037589841));
#35071=CARTESIAN_POINT('Ctrl Pts',(-12.4401638581022,-32.6442037764079,
25.332807356536));
#35072=CARTESIAN_POINT('Ctrl Pts',(-12.5202544506499,-32.7300888027633,
25.3402295786459));
#35073=CARTESIAN_POINT('Ctrl Pts',(-12.6469057588669,-32.8808903219142,
25.3524165107193));
#35074=CARTESIAN_POINT('Ctrl Pts',(-12.6959189647463,-32.9436054801293,
25.3572645381508));
#35075=CARTESIAN_POINT('Ctrl Pts',(-12.7632234716228,-33.0362732166188,
25.3641208420278));
#35076=CARTESIAN_POINT('Ctrl Pts',(-12.783326200648,-33.0648715205522,25.366196813312));
#35077=CARTESIAN_POINT('Ctrl Pts',(-12.8179657177998,-33.1158067840632,
25.3698258716006));
#35078=CARTESIAN_POINT('Ctrl Pts',(-12.8326879204357,-33.1380134084014,
25.3713857688134));
#35079=CARTESIAN_POINT('Ctrl Pts',(-12.8630502057364,-33.1850048773397,
25.374641237903));
#35080=CARTESIAN_POINT('Ctrl Pts',(-12.8786338183571,-33.2098236976073,
25.3763346587354));
#35081=CARTESIAN_POINT('Ctrl Pts',(-12.919415939758,-33.2766840806945,25.3808299991001));
#35082=CARTESIAN_POINT('Ctrl Pts',(-12.944028242768,-33.3190760774526,25.3836109494865));
#35083=CARTESIAN_POINT('Ctrl Pts',(-13.0495237701613,-33.5102105692971,
25.3958677269295));
#35084=CARTESIAN_POINT('Ctrl Pts',(-13.1200463218647,-33.6642280914039,
25.4049836951215));
#35085=CARTESIAN_POINT('Ctrl Pts',(-13.1787501041971,-33.8227350181174,
25.4139789249709));
#35086=CARTESIAN_POINT('Origin',(-10.,-35.,23.));
#35087=CARTESIAN_POINT('',(-13.1787501100144,-33.8227350338248,26.6607619345813));
#35088=CARTESIAN_POINT('',(-13.1787501930238,-33.8227352579598,26.3195306104224));
#35089=CARTESIAN_POINT('',(-13.1787501240207,-33.8227350716434,23.));
#35090=CARTESIAN_POINT('',(-13.3897489515553,-34.9973339299542,25.1396837753564));
#35091=CARTESIAN_POINT('Ctrl Pts',(-13.1787501930238,-33.8227352579598,
26.3195306104224));
#35092=CARTESIAN_POINT('Ctrl Pts',(-13.1275287934103,-33.6844315883653,
26.3116511514972));
#35093=CARTESIAN_POINT('Ctrl Pts',(-13.0673147987542,-33.5495611216508,
26.3039018275174));
#35094=CARTESIAN_POINT('Ctrl Pts',(-12.9360680687594,-33.3006443959325,
26.2888533570821));
#35095=CARTESIAN_POINT('Ctrl Pts',(-12.8667205839725,-33.1861060663972,
26.2815933404214));
#35096=CARTESIAN_POINT('Ctrl Pts',(-12.7748581417378,-33.0528595926025,
26.2723744883258));
#35097=CARTESIAN_POINT('Ctrl Pts',(-12.7586346206402,-33.0299420327976,
26.2707595185889));
#35098=CARTESIAN_POINT('Ctrl Pts',(-12.7324443584637,-32.9939032256492,
26.2681683890439));
#35099=CARTESIAN_POINT('Ctrl Pts',(-12.7226630753473,-32.9806480758556,
26.2672040864343));
#35100=CARTESIAN_POINT('Ctrl Pts',(-12.703559380756,-32.9551507375422,26.2653261325253));
#35101=CARTESIAN_POINT('Ctrl Pts',(-12.6942496035125,-32.9428998878466,
26.264413287662));
#35102=CARTESIAN_POINT('Ctrl Pts',(-12.6708780749975,-32.9125758101539,
26.2621282078519));
#35103=CARTESIAN_POINT('Ctrl Pts',(-12.6567160940558,-32.8945810458098,
26.2607493737556));
#35104=CARTESIAN_POINT('Ctrl Pts',(-12.6001872699501,-32.8242318317679,
26.2552728093567));
#35105=CARTESIAN_POINT('Ctrl Pts',(-12.5564486954784,-32.7730043106772,
26.2510944892195));
#35106=CARTESIAN_POINT('Ctrl Pts',(-12.4289817699211,-32.6324186583855,
26.2391567064824));
#35107=CARTESIAN_POINT('Ctrl Pts',(-12.3418970711533,-32.5462458637701,
26.2312749164038));
#35108=CARTESIAN_POINT('Ctrl Pts',(-12.0685078467215,-32.3035575717819,
26.2077110947291));
#35109=CARTESIAN_POINT('Ctrl Pts',(-11.8698006332764,-32.1621475627646,
26.1921269852289));
#35110=CARTESIAN_POINT('Ctrl Pts',(-11.612824737059,-32.0180808469371,26.1742103397903));
#35111=CARTESIAN_POINT('Ctrl Pts',(-11.5674357647263,-31.9939742143985,
26.1711196937653));
#35112=CARTESIAN_POINT('Ctrl Pts',(-11.4946398504755,-31.9574087950245,
26.1662765732097));
#35113=CARTESIAN_POINT('Ctrl Pts',(-11.4675863175996,-31.9442676800934,
26.1645009494808));
#35114=CARTESIAN_POINT('Ctrl Pts',(-11.41878173469,-31.9213587884274,26.1613399136456));
#35115=CARTESIAN_POINT('Ctrl Pts',(-11.3970960169682,-31.9114572882191,
26.1599500339689));
#35116=CARTESIAN_POINT('Ctrl Pts',(-11.3458355913086,-31.8887026251433,
26.1566981549842));
#35117=CARTESIAN_POINT('Ctrl Pts',(-11.3161780838081,-31.8760409497009,
26.15484267066));
#35118=CARTESIAN_POINT('Ctrl Pts',(-11.2272522331854,-31.8395670790632,
26.1493524451096));
#35119=CARTESIAN_POINT('Ctrl Pts',(-11.1674852575761,-31.8170040552819,
26.1457586504029));
#35120=CARTESIAN_POINT('Ctrl Pts',(-10.9515867180849,-31.7423989277845,
26.1330719643843));
#35121=CARTESIAN_POINT('Ctrl Pts',(-10.7923445334855,-31.7000487436451,
26.1242693340018));
#35122=CARTESIAN_POINT('Ctrl Pts',(-10.4225491747609,-31.630027421544,26.1042889504311));
#35123=CARTESIAN_POINT('Ctrl Pts',(-10.2112356651129,-31.6102175589044,
26.0932035591212));
#35124=CARTESIAN_POINT('Ctrl Pts',(-9.95506088281142,-31.610256853287,26.0788608354605));
#35125=CARTESIAN_POINT('Ctrl Pts',(-9.91064829397407,-31.6111367671557,
26.0763404584383));
#35126=CARTESIAN_POINT('Ctrl Pts',(-9.84684810430115,-31.6136557644243,
26.0726552101951));
#35127=CARTESIAN_POINT('Ctrl Pts',(-9.82743560367628,-31.6145894967909,
26.0715252803161));
#35128=CARTESIAN_POINT('Ctrl Pts',(-9.79311537120632,-31.6165362340046,
26.0695107111265));
#35129=CARTESIAN_POINT('Ctrl Pts',(-9.77820466278739,-31.6174809502731,
26.0686297381704));
#35130=CARTESIAN_POINT('Ctrl Pts',(-9.74529027420171,-31.6197849231823,
26.0666720297836));
#35131=CARTESIAN_POINT('Ctrl Pts',(-9.72729112865333,-31.6211894327692,
26.0655930101992));
#35132=CARTESIAN_POINT('Ctrl Pts',(-9.67369544307343,-31.625802643764,26.0623565514663));
#35133=CARTESIAN_POINT('Ctrl Pts',(-9.63813856958889,-31.629430530412,26.0601784950129));
#35134=CARTESIAN_POINT('Ctrl Pts',(-9.45998187875568,-31.6504593630266,
26.0491318455236));
#35135=CARTESIAN_POINT('Ctrl Pts',(-9.31854207937637,-31.6763498051946,
26.039937130674));
#35136=CARTESIAN_POINT('Ctrl Pts',(-8.914660216476,-31.7771482142732,26.0131334800925));
#35137=CARTESIAN_POINT('Ctrl Pts',(-8.65901798882663,-31.8748517235715,
25.9955698331783));
#35138=CARTESIAN_POINT('Ctrl Pts',(-8.37507263254275,-32.0247096409041,
25.9760997762504));
#35139=CARTESIAN_POINT('Ctrl Pts',(-8.33280865278018,-32.048184449669,25.9731991254146));
#35140=CARTESIAN_POINT('Ctrl Pts',(-8.26587225564731,-32.0872596031988,
25.9685989542391));
#35141=CARTESIAN_POINT('Ctrl Pts',(-8.24087522746037,-32.1022878391613,
25.9668795897919));
#35142=CARTESIAN_POINT('Ctrl Pts',(-8.19338731153039,-32.1316786207549,
25.9636094140972));
#35143=CARTESIAN_POINT('Ctrl Pts',(-8.17086607256977,-32.1459877231989,
25.9620568390419));
#35144=CARTESIAN_POINT('Ctrl Pts',(-8.11898913144285,-32.1798146036373,
25.9584753084798));
#35145=CARTESIAN_POINT('Ctrl Pts',(-8.08976398221491,-32.1995275315742,
25.9564536905079));
#35146=CARTESIAN_POINT('Ctrl Pts',(-7.99404942229286,-32.2662844860209,
25.9498141380747));
#35147=CARTESIAN_POINT('Ctrl Pts',(-7.92894577255225,-32.3152702134998,
25.9452684634052));
#35148=CARTESIAN_POINT('Ctrl Pts',(-7.77121350786264,-32.4431078872044,
25.934108786597));
#35149=CARTESIAN_POINT('Ctrl Pts',(-7.68094372798789,-32.5246884829679,
25.927589658665));
#35150=CARTESIAN_POINT('Ctrl Pts',(-7.46575488408208,-32.741291247819,25.9113503186686));
#35151=CARTESIAN_POINT('Ctrl Pts',(-7.34708032452994,-32.8819410982023,
25.9017322140363));
#35152=CARTESIAN_POINT('Ctrl Pts',(-7.19533725223829,-33.0946675905303,
25.8874490695594));
#35153=CARTESIAN_POINT('Ctrl Pts',(-7.15246625819151,-33.1593548466305,
25.8831343939313));
#35154=CARTESIAN_POINT('Ctrl Pts',(-7.09892266121463,-33.2464990398643,
25.8772813469308));
#35155=CARTESIAN_POINT('Ctrl Pts',(-7.08622096590751,-33.2676873817578,
25.8758551637343));
#35156=CARTESIAN_POINT('Ctrl Pts',(-7.06658944382127,-33.3012625408345,
25.8735873867013));
#35157=CARTESIAN_POINT('Ctrl Pts',(-7.05950364228452,-33.3135577090986,
25.8727552975367));
#35158=CARTESIAN_POINT('Ctrl Pts',(-7.04480723162945,-33.3394328983479,
25.8709999839324));
#35159=CARTESIAN_POINT('Ctrl Pts',(-7.03721266316546,-33.3530213835385,
25.8700757267377));
#35160=CARTESIAN_POINT('Ctrl Pts',(-7.01823261251563,-33.3875373185417,
25.8677227740536));
#35161=CARTESIAN_POINT('Ctrl Pts',(-7.00697379096015,-33.4085331627742,
25.8662866487066));
#35162=CARTESIAN_POINT('Ctrl Pts',(-6.96083415653091,-33.4967975148889,
25.8602346779064));
#35163=CARTESIAN_POINT('Ctrl Pts',(-6.92799473476246,-33.5651032391929,
25.8555163028674));
#35164=CARTESIAN_POINT('Ctrl Pts',(-6.83674094832738,-33.7724310680922,
25.8412094669498));
#35165=CARTESIAN_POINT('Ctrl Pts',(-6.78528281092349,-33.9143093400934,
25.8314457715305));
#35166=CARTESIAN_POINT('Ctrl Pts',(-6.68753696179293,-34.2526317979794,
25.80877642403));
#35167=CARTESIAN_POINT('Ctrl Pts',(-6.64898337271048,-34.4507473405117,
25.7959797191622));
#35168=CARTESIAN_POINT('Ctrl Pts',(-6.62279343430231,-34.7038722220211,
25.7804843580662));
#35169=CARTESIAN_POINT('Ctrl Pts',(-6.61857482675904,-34.756730354728,25.7772925334374));
#35170=CARTESIAN_POINT('Ctrl Pts',(-6.61388946112314,-34.8400435347316,
25.7723286541669));
#35171=CARTESIAN_POINT('Ctrl Pts',(-6.61259017752397,-34.8704413751505,
25.7705314700851));
#35172=CARTESIAN_POINT('Ctrl Pts',(-6.61092678106691,-34.9272873280363,
25.7671956110137));
#35173=CARTESIAN_POINT('Ctrl Pts',(-6.61046263334993,-34.9537299827227,
25.7656539849983));
#35174=CARTESIAN_POINT('Ctrl Pts',(-6.61011468400408,-35.0132253827938,
25.7622068996898));
#35175=CARTESIAN_POINT('Ctrl Pts',(-6.61040475210597,-35.0462766892399,
25.7603069109981));
#35176=CARTESIAN_POINT('Ctrl Pts',(-6.61277586923587,-35.1475797878267,
25.754525288429));
#35177=CARTESIAN_POINT('Ctrl Pts',(-6.61643571069143,-35.2157792211217,
25.7506916644));
#35178=CARTESIAN_POINT('Ctrl Pts',(-6.64315802820328,-35.5338058696532,
25.7330159722488));
#35179=CARTESIAN_POINT('Ctrl Pts',(-6.6918456095314,-35.7806764872546,25.7199452386104));
#35180=CARTESIAN_POINT('Ctrl Pts',(-6.81084117792656,-36.1578362115865,
25.6988479729883));
#35181=CARTESIAN_POINT('Ctrl Pts',(-6.86313051908764,-36.2928108712379,
25.6910334574032));
#35182=CARTESIAN_POINT('Ctrl Pts',(-6.93575178011109,-36.4496854204239,
25.6811891993183));
#35183=CARTESIAN_POINT('Ctrl Pts',(-6.94795354802824,-36.4752007712583,
25.679562836663));
#35184=CARTESIAN_POINT('Ctrl Pts',(-6.96778452493482,-36.5153703165132,
25.6769576509158));
#35185=CARTESIAN_POINT('Ctrl Pts',(-6.97520431449757,-36.5301270925732,
25.6759909060457));
#35186=CARTESIAN_POINT('Ctrl Pts',(-6.98973325513308,-36.5585041642485,
25.6741119671164));
#35187=CARTESIAN_POINT('Ctrl Pts',(-6.9968276296409,-36.5721312874253,25.6732006298927));
#35188=CARTESIAN_POINT('Ctrl Pts',(-7.01466688631889,-36.6058361793591,
25.6709248157731));
#35189=CARTESIAN_POINT('Ctrl Pts',(-7.0255218382554,-36.6258546177568,25.6695538529262));
#35190=CARTESIAN_POINT('Ctrl Pts',(-7.06875434913484,-36.7037007686679,
25.6641512264641));
#35191=CARTESIAN_POINT('Ctrl Pts',(-7.10262157527926,-36.7606801135123,
25.6600415945817));
#35192=CARTESIAN_POINT('Ctrl Pts',(-7.20200166040816,-36.917240903225,25.648382563442));
#35193=CARTESIAN_POINT('Ctrl Pts',(-7.27112757513383,-37.014413101441,25.6407166395166));
#35194=CARTESIAN_POINT('Ctrl Pts',(-7.49992639763282,-37.3025939195883,
25.6170007397345));
#35195=CARTESIAN_POINT('Ctrl Pts',(-7.67563763592788,-37.479855468991,25.6010379548524));
#35196=CARTESIAN_POINT('Ctrl Pts',(-7.90871828068696,-37.6682444692122,
25.5828196807745));
#35197=CARTESIAN_POINT('Ctrl Pts',(-7.94895756980383,-37.6992986394652,
25.5797640077375));
#35198=CARTESIAN_POINT('Ctrl Pts',(-8.01399975508353,-37.7471995306856,
25.574962692194));
#35199=CARTESIAN_POINT('Ctrl Pts',(-8.03835278508185,-37.7646414821188,
25.5731945696784));
#35200=CARTESIAN_POINT('Ctrl Pts',(-8.08468633467785,-37.796905647308,25.5698847600573));
#35201=CARTESIAN_POINT('Ctrl Pts',(-8.10661561672311,-37.8117971606208,
25.568340550792));
#35202=CARTESIAN_POINT('Ctrl Pts',(-8.15686934140836,-37.8450684227092,
25.5648508921096));
#35203=CARTESIAN_POINT('Ctrl Pts',(-8.185298473421,-37.8632854278068,25.562911515456));
#35204=CARTESIAN_POINT('Ctrl Pts',(-8.27548781193689,-37.9191946045994,
25.5568627889473));
#35205=CARTESIAN_POINT('Ctrl Pts',(-8.33818711939478,-37.9553372723505,
25.5528084362073));
#35206=CARTESIAN_POINT('Ctrl Pts',(-8.49195128019705,-38.037531518084,25.5431757673161));
#35207=CARTESIAN_POINT('Ctrl Pts',(-8.58403230329462,-38.0815330650078,
25.5376597002759));
#35208=CARTESIAN_POINT('Ctrl Pts',(-8.72212775165444,-38.1400235921513,
25.5296370091679));
#35209=CARTESIAN_POINT('Ctrl Pts',(-8.7666863409551,-38.1577908664127,25.5270848170772));
#35210=CARTESIAN_POINT('Ctrl Pts',(-9.00739007930714,-38.2478966858258,
25.5134385408668));
#35211=CARTESIAN_POINT('Ctrl Pts',(-9.20951422219543,-38.3029113453702,
25.502497526991));
#35212=CARTESIAN_POINT('Ctrl Pts',(-9.46092488778908,-38.3469298844386,
25.4882442732159));
#35213=CARTESIAN_POINT('Ctrl Pts',(-9.5066113265404,-38.353969114046,25.4856277679349));
#35214=CARTESIAN_POINT('Ctrl Pts',(-9.57084227228276,-38.3625249322152,
25.4818947086259));
#35215=CARTESIAN_POINT('Ctrl Pts',(-9.58927890880338,-38.3648266562847,
25.4808169174309));
#35216=CARTESIAN_POINT('Ctrl Pts',(-9.62272436181845,-38.3687231919704,
25.4788488872577));
#35217=CARTESIAN_POINT('Ctrl Pts',(-9.63772691868671,-38.3703695732399,
25.4779614017852));
#35218=CARTESIAN_POINT('Ctrl Pts',(-9.66936996797806,-38.3736283632646,
25.4760788717889));
#35219=CARTESIAN_POINT('Ctrl Pts',(-9.68601199357414,-38.375217927378,25.4750827051862));
#35220=CARTESIAN_POINT('Ctrl Pts',(-9.73177407710077,-38.37924752609,25.4723279986244));
#35221=CARTESIAN_POINT('Ctrl Pts',(-9.76091433394061,-38.3814341495968,
25.4705566925829));
#35222=CARTESIAN_POINT('Ctrl Pts',(-9.82699105636127,-38.3855340462016,
25.4665067398777));
#35223=CARTESIAN_POINT('Ctrl Pts',(-9.8639376220256,-38.3872200538519,25.4642186052806));
#35224=CARTESIAN_POINT('Ctrl Pts',(-9.98615734372112,-38.3907945940137,
25.4565867515744));
#35225=CARTESIAN_POINT('Ctrl Pts',(-10.07147127874,-38.3900693120792,25.4511593252153));
#35226=CARTESIAN_POINT('Ctrl Pts',(-10.4342491945548,-38.3732850748911,
25.4278701189639));
#35227=CARTESIAN_POINT('Ctrl Pts',(-10.7092555860482,-38.3263531081236,
25.4098055995211));
#35228=CARTESIAN_POINT('Ctrl Pts',(-11.0361673540544,-38.2281233395888,
25.3888702850396));
#35229=CARTESIAN_POINT('Ctrl Pts',(-11.0963530811589,-38.2081823210776,
25.385033244961));
#35230=CARTESIAN_POINT('Ctrl Pts',(-11.1865501928067,-38.1754627188258,
25.3793071009394));
#35231=CARTESIAN_POINT('Ctrl Pts',(-11.2169923098703,-38.1639207744977,
25.3773786800668));
#35232=CARTESIAN_POINT('Ctrl Pts',(-11.2718256535501,-38.1422225089752,
25.3739116159283));
#35233=CARTESIAN_POINT('Ctrl Pts',(-11.2962731030927,-38.132216290365,25.3723681843576));
#35234=CARTESIAN_POINT('Ctrl Pts',(-11.3489656455862,-38.1099268842096,
25.3690456386899));
#35235=CARTESIAN_POINT('Ctrl Pts',(-11.3771654836561,-38.0975423901317,
25.3672700622237));
#35236=CARTESIAN_POINT('Ctrl Pts',(-11.4564834654865,-38.0614110360573,
25.3622803699208));
#35237=CARTESIAN_POINT('Ctrl Pts',(-11.5071848006246,-38.0367706696,25.3590963787428));
#35238=CARTESIAN_POINT('Ctrl Pts',(-11.6213302696875,-37.9777336868732,
25.3519221203194));
#35239=CARTESIAN_POINT('Ctrl Pts',(-11.6843382284646,-37.9425525207368,
25.347957763896));
#35240=CARTESIAN_POINT('Ctrl Pts',(-11.9113616681144,-37.8061082065748,
25.3335721351127));
#35241=CARTESIAN_POINT('Ctrl Pts',(-12.0677762878915,-37.6929258019597,
25.3234801161834));
#35242=CARTESIAN_POINT('Ctrl Pts',(-12.3270309109062,-37.4693555238239,
25.3052357620447));
#35243=CARTESIAN_POINT('Ctrl Pts',(-12.4337297570218,-37.3642630279971,
25.2971662790281));
#35244=CARTESIAN_POINT('Ctrl Pts',(-12.5519368459782,-37.2313279986519,
25.2870363961496));
#35245=CARTESIAN_POINT('Ctrl Pts',(-12.5704799050936,-37.2099410059806,
25.285408719021));
#35246=CARTESIAN_POINT('Ctrl Pts',(-12.5994186509405,-37.1757069488328,
25.2828019115322));
#35247=CARTESIAN_POINT('Ctrl Pts',(-12.6099923539027,-37.1630113124236,
25.2818348850014));
#35248=CARTESIAN_POINT('Ctrl Pts',(-12.6302166226172,-37.1383642209727,
25.2799558287584));
#35249=CARTESIAN_POINT('Ctrl Pts',(-12.6398794290999,-37.1264236616857,
25.2790446616619));
#35250=CARTESIAN_POINT('Ctrl Pts',(-12.6636560058445,-37.0966305492294,
25.2767698985695));
#35251=CARTESIAN_POINT('Ctrl Pts',(-12.6776716534895,-37.078700900043,25.2753998294631));
#35252=CARTESIAN_POINT('Ctrl Pts',(-12.7317201533232,-37.0081051699611,
25.27000552723));
#35253=CARTESIAN_POINT('Ctrl Pts',(-12.7703861561577,-36.9544157040958,
25.265903618178));
#35254=CARTESIAN_POINT('Ctrl Pts',(-12.8788188305548,-36.7941638573607,
25.253739180942));
#35255=CARTESIAN_POINT('Ctrl Pts',(-12.9441804497685,-36.6847612420923,
25.2455361145666));
#35256=CARTESIAN_POINT('Ctrl Pts',(-13.1084485628498,-36.3709243740313,
25.2227023152081));
#35257=CARTESIAN_POINT('Ctrl Pts',(-13.1932326572253,-36.15981814523,25.2081578691538));
#35258=CARTESIAN_POINT('Ctrl Pts',(-13.2711802378338,-35.8903131964984,
25.1910045978432));
#35259=CARTESIAN_POINT('Ctrl Pts',(-13.2848489513258,-35.838478139077,25.1877641573827));
#35260=CARTESIAN_POINT('Ctrl Pts',(-13.3050041925644,-35.7539629530655,
25.1825737660494));
#35261=CARTESIAN_POINT('Ctrl Pts',(-13.312248065908,-35.7214746813781,25.1806004950809));
#35262=CARTESIAN_POINT('Ctrl Pts',(-13.324390475741,-35.6629730989752,25.1770853115999));
#35263=CARTESIAN_POINT('Ctrl Pts',(-13.3294649830156,-35.6369994905114,
25.1755379974232));
#35264=CARTESIAN_POINT('Ctrl Pts',(-13.3387175443593,-35.5865055452396,
25.1725548612563));
#35265=CARTESIAN_POINT('Ctrl Pts',(-13.3429308949007,-35.5619934832242,
25.1711180294128));
#35266=CARTESIAN_POINT('Ctrl Pts',(-13.3516007611882,-35.5080021073847,
25.1679769160015));
#35267=CARTESIAN_POINT('Ctrl Pts',(-13.355938936534,-35.4785057328764,25.1662763497801));
#35268=CARTESIAN_POINT('Ctrl Pts',(-13.3674688356676,-35.3922183796251,
25.161343561259));
#35269=CARTESIAN_POINT('Ctrl Pts',(-13.3736120590693,-35.3352965699076,
25.158142570588));
#35270=CARTESIAN_POINT('Ctrl Pts',(-13.3860065529804,-35.1848084218353,
25.1497937535001));
#35271=CARTESIAN_POINT('Ctrl Pts',(-13.3898226926569,-35.0910913397411,
25.1447109691293));
#35272=CARTESIAN_POINT('Ctrl Pts',(-13.3897489515553,-34.9973339299542,
25.1396837753564));
#35273=CARTESIAN_POINT('Ctrl Pts',(-13.389748954038,-34.9973370883974,25.1396839447095));
#35274=CARTESIAN_POINT('Ctrl Pts',(-13.3895886446596,-34.7932715281918,
25.1287421175687));
#35275=CARTESIAN_POINT('Ctrl Pts',(-13.371001697134,-34.5896392054684,25.1181177862061));
#35276=CARTESIAN_POINT('Ctrl Pts',(-13.3222361968378,-34.3235637280122,
25.1034711517141));
#35277=CARTESIAN_POINT('Ctrl Pts',(-13.3083405108317,-34.258581387182,25.0998294964393));
#35278=CARTESIAN_POINT('Ctrl Pts',(-13.2818257879657,-34.1502604925755,
25.0935894458589));
#35279=CARTESIAN_POINT('Ctrl Pts',(-13.2702342466418,-34.1066885748227,
25.0910324631202));
#35280=CARTESIAN_POINT('Ctrl Pts',(-13.2523190069828,-34.0443764191298,
25.0872911150932));
#35281=CARTESIAN_POINT('Ctrl Pts',(-13.2466944756061,-34.0254384099583,
25.086142674056));
#35282=CARTESIAN_POINT('Ctrl Pts',(-13.2365262793365,-33.992266941969,25.0841093394122));
#35283=CARTESIAN_POINT('Ctrl Pts',(-13.2320535534741,-33.9780126769839,
25.0832284129384));
#35284=CARTESIAN_POINT('Ctrl Pts',(-13.2219643393755,-33.9465878301534,
25.0812700861574));
#35285=CARTESIAN_POINT('Ctrl Pts',(-13.2163048048448,-33.9294324991637,
25.0801903914591));
#35286=CARTESIAN_POINT('Ctrl Pts',(-13.2003412141904,-33.8823125588762,
25.0771971170973));
#35287=CARTESIAN_POINT('Ctrl Pts',(-13.1897539871707,-33.8524467622835,
25.0752688638173));
#35288=CARTESIAN_POINT('Ctrl Pts',(-13.1787501240264,-33.8227350716589,
25.0733224007726));
#35289=CARTESIAN_POINT('Ctrl Pts',(-13.1787501041971,-33.8227350181174,
25.4139789249709));
#35290=CARTESIAN_POINT('Ctrl Pts',(-13.2129572634916,-33.9150982607561,
25.419220516707));
#35291=CARTESIAN_POINT('Ctrl Pts',(-13.2431511806743,-34.0089857317186,
25.4244249055303));
#35292=CARTESIAN_POINT('Ctrl Pts',(-13.3114018017695,-34.2580493560975,
25.4381640698729));
#35293=CARTESIAN_POINT('Ctrl Pts',(-13.3426519766591,-34.4147313341876,
25.4467386760083));
#35294=CARTESIAN_POINT('Ctrl Pts',(-13.3663308146369,-34.6012141985136,
25.4574414958164));
#35295=CARTESIAN_POINT('Ctrl Pts',(-13.3695568005663,-34.6294596858261,
25.459076027929));
#35296=CARTESIAN_POINT('Ctrl Pts',(-13.3740979302152,-34.6742054682466,
25.4616912925964));
#35297=CARTESIAN_POINT('Ctrl Pts',(-13.3756481974522,-34.6906811651713,
25.4626597874223));
#35298=CARTESIAN_POINT('Ctrl Pts',(-13.3783881988411,-34.7222800736297,
25.4645289931918));
#35299=CARTESIAN_POINT('Ctrl Pts',(-13.3795971498082,-34.7374009685751,
25.4654286768883));
#35300=CARTESIAN_POINT('Ctrl Pts',(-13.3823498932698,-34.7750062334487,
25.4676783979022));
#35301=CARTESIAN_POINT('Ctrl Pts',(-13.3837709941551,-34.7974986553637,
25.4690348218451));
#35302=CARTESIAN_POINT('Ctrl Pts',(-13.3881296072056,-34.8794653319769,
25.4740132425915));
#35303=CARTESIAN_POINT('Ctrl Pts',(-13.3897239753482,-34.9389972047508,
25.4776966446478));
#35304=CARTESIAN_POINT('Ctrl Pts',(-13.389794204562,-35.1016409861366,25.4878913106812));
#35305=CARTESIAN_POINT('Ctrl Pts',(-13.3851345470166,-35.204689100525,25.4944934049557));
#35306=CARTESIAN_POINT('Ctrl Pts',(-13.3515711786711,-35.5733225716754,
25.5183172007609));
#35307=CARTESIAN_POINT('Ctrl Pts',(-13.2960042769614,-35.8355401828051,
25.5355547403311));
#35308=CARTESIAN_POINT('Ctrl Pts',(-13.1929877658504,-36.1393475372853,
25.5550977597033));
#35309=CARTESIAN_POINT('Ctrl Pts',(-13.1745538687943,-36.1897444721278,
25.5583290371695));
#35310=CARTESIAN_POINT('Ctrl Pts',(-13.1437547084232,-36.2681266632395,
25.5633399240688));
#35311=CARTESIAN_POINT('Ctrl Pts',(-13.1321945298213,-36.2964167615916,
25.565145452981));
#35312=CARTESIAN_POINT('Ctrl Pts',(-13.1099245549794,-36.3488784241009,
25.5684890536845));
#35313=CARTESIAN_POINT('Ctrl Pts',(-13.0993115814652,-36.3730883147344,
25.5700301974044));
#35314=CARTESIAN_POINT('Ctrl Pts',(-13.0748704925588,-36.427114770452,25.5734663663822));
#35315=CARTESIAN_POINT('Ctrl Pts',(-13.0608896441662,-36.4568595706773,
25.5753560782388));
#35316=CARTESIAN_POINT('Ctrl Pts',(-13.0169917442215,-36.5468314821119,
25.5810694871647));
#35317=CARTESIAN_POINT('Ctrl Pts',(-12.9857124468639,-36.6063775501698,
25.5848468795753));
#35318=CARTESIAN_POINT('Ctrl Pts',(-12.8303869168392,-36.8818362195399,
25.6023724886231));
#35319=CARTESIAN_POINT('Ctrl Pts',(-12.6845741895147,-37.0845777120648,
25.6153579235765));
#35320=CARTESIAN_POINT('Ctrl Pts',(-12.4187419946939,-37.3794981642517,
25.6365239427438));
#35321=CARTESIAN_POINT('Ctrl Pts',(-12.3125290895914,-37.4828460358857,
25.6445138166512));
#35322=CARTESIAN_POINT('Ctrl Pts',(-12.1783851838074,-37.5972762493921,
25.6545544356736));
#35323=CARTESIAN_POINT('Ctrl Pts',(-12.1566266061187,-37.6153713876843,
25.6561817391956));
#35324=CARTESIAN_POINT('Ctrl Pts',(-12.1218111934531,-37.6435951395608,
25.6587880855468));
#35325=CARTESIAN_POINT('Ctrl Pts',(-12.1089020023421,-37.6539047311729,
25.6597550318242));
#35326=CARTESIAN_POINT('Ctrl Pts',(-12.0838449286878,-37.6736176539674,
25.6616340540304));
#35327=CARTESIAN_POINT('Ctrl Pts',(-12.0717076683729,-37.6830334230064,
25.6625452689832));
#35328=CARTESIAN_POINT('Ctrl Pts',(-12.0414282470533,-37.7061954614059,
25.6648203290142));
#35329=CARTESIAN_POINT('Ctrl Pts',(-12.0232109799637,-37.7198419865925,
25.6661906508364));
#35330=CARTESIAN_POINT('Ctrl Pts',(-11.9514880592596,-37.7724502247904,
25.6715873077567));
#35331=CARTESIAN_POINT('Ctrl Pts',(-11.8969862249369,-37.8100227728828,
25.675691401441));
#35332=CARTESIAN_POINT('Ctrl Pts',(-11.7415854188545,-37.9105713946347,
25.6873281520633));
#35333=CARTESIAN_POINT('Ctrl Pts',(-11.6384216439193,-37.9698682801586,
25.6949768743176));
#35334=CARTESIAN_POINT('Ctrl Pts',(-11.3100229291648,-38.1362997480817,
25.7187054880072));
#35335=CARTESIAN_POINT('Ctrl Pts',(-11.0758985346293,-38.2241301926879,
25.7346991449924));
#35336=CARTESIAN_POINT('Ctrl Pts',(-10.7844420210448,-38.2981350251136,
25.7529781359782));
#35337=CARTESIAN_POINT('Ctrl Pts',(-10.7343692539989,-38.309644415842,25.7560663467279));
#35338=CARTESIAN_POINT('Ctrl Pts',(-10.6548760180456,-38.3260231273484,
25.7608891748018));
#35339=CARTESIAN_POINT('Ctrl Pts',(-10.6256213060734,-38.331649817864,25.7626471679003));
#35340=CARTESIAN_POINT('Ctrl Pts',(-10.5701751945687,-38.3415579252178,
25.765948275864));
#35341=CARTESIAN_POINT('Ctrl Pts',(-10.5440004526708,-38.3459188105124,
25.7674937599726));
#35342=CARTESIAN_POINT('Ctrl Pts',(-10.4841385288724,-38.3551711582749,
25.7710001505805));
#35343=CARTESIAN_POINT('Ctrl Pts',(-10.4504231877382,-38.3598634925088,
25.772954751293));
#35344=CARTESIAN_POINT('Ctrl Pts',(-10.3432344720431,-38.3731389655881,
25.7791092898475));
#35345=CARTESIAN_POINT('Ctrl Pts',(-10.2695458403651,-38.3798258098917,
25.7832513239744));
#35346=CARTESIAN_POINT('Ctrl Pts',(-10.0905440204856,-38.3901770211333,
25.7931478901322));
#35347=CARTESIAN_POINT('Ctrl Pts',(-9.9851639209605,-38.3913537642606,25.7988351237834));
#35348=CARTESIAN_POINT('Ctrl Pts',(-9.75584331201983,-38.3832234372192,
25.8110955807886));
#35349=CARTESIAN_POINT('Ctrl Pts',(-9.63212701842956,-38.3720146546837,
25.8176355307134));
#35350=CARTESIAN_POINT('Ctrl Pts',(-9.36614070135747,-38.3331009518414,
25.8319428517003));
#35351=CARTESIAN_POINT('Ctrl Pts',(-9.2244776685438,-38.3030133054572,25.8397194017971));
#35352=CARTESIAN_POINT('Ctrl Pts',(-9.05086013906078,-38.254352363876,25.849900232811));
#35353=CARTESIAN_POINT('Ctrl Pts',(-9.01669095744491,-38.2441915633943,
25.8519363366232));
#35354=CARTESIAN_POINT('Ctrl Pts',(-8.96548552225046,-38.2280814957475,
25.8550453996338));
#35355=CARTESIAN_POINT('Ctrl Pts',(-8.94832512701744,-38.2225316565853,
25.8560972087198));
#35356=CARTESIAN_POINT('Ctrl Pts',(-8.91702914806747,-38.2121336366651,
25.8580349042542));
#35357=CARTESIAN_POINT('Ctrl Pts',(-8.9028801765355,-38.2073285507279,25.8589183815811));
#35358=CARTESIAN_POINT('Ctrl Pts',(-8.87006229146392,-38.1959408131902,
25.8609847393125));
#35359=CARTESIAN_POINT('Ctrl Pts',(-8.85141882194449,-38.189288030629,25.8621714824119));
#35360=CARTESIAN_POINT('Ctrl Pts',(-8.79028749083757,-38.1668682492365,
25.8661027488397));
#35361=CARTESIAN_POINT('Ctrl Pts',(-8.74805912484931,-38.150413066012,25.868882262076));
#35362=CARTESIAN_POINT('Ctrl Pts',(-8.64431527820294,-38.1075719227212,
25.8758485440499));
#35363=CARTESIAN_POINT('Ctrl Pts',(-8.58322809779685,-38.0802014207884,
25.8800726204313));
#35364=CARTESIAN_POINT('Ctrl Pts',(-8.27084281022892,-37.9289761100363,
25.9021822029667));
#35365=CARTESIAN_POINT('Ctrl Pts',(-8.03475214678143,-37.7760984401869,
25.9205165747857));
#35366=CARTESIAN_POINT('Ctrl Pts',(-7.75821188526995,-37.5438820513353,
25.9429015005832));
#35367=CARTESIAN_POINT('Ctrl Pts',(-7.69813674202134,-37.4896539955077,
25.947838930622));
#35368=CARTESIAN_POINT('Ctrl Pts',(-7.61666811687911,-37.410642169025,25.9546427428696));
#35369=CARTESIAN_POINT('Ctrl Pts',(-7.59360813427828,-37.3876232600545,
25.9565816447087));
#35370=CARTESIAN_POINT('Ctrl Pts',(-7.55207491946181,-37.3449509628874,
25.9600989999674));
#35371=CARTESIAN_POINT('Ctrl Pts',(-7.53349772445642,-37.3254029340383,
25.961681854077));
#35372=CARTESIAN_POINT('Ctrl Pts',(-7.49616355970659,-37.2851669018394,
25.9648836059633));
#35373=CARTESIAN_POINT('Ctrl Pts',(-7.4774249821693,-37.2644646246677,25.9665016688372));
#35374=CARTESIAN_POINT('Ctrl Pts',(-7.43096969455841,-37.2118487255616,
25.9705429356919));
#35375=CARTESIAN_POINT('Ctrl Pts',(-7.40358969162847,-37.1796433719326,
25.9729523743342));
#35376=CARTESIAN_POINT('Ctrl Pts',(-7.28529368550675,-37.0351060836231,
25.9835005559506));
#35377=CARTESIAN_POINT('Ctrl Pts',(-7.20100857082505,-36.9175349346139,
25.991381432895));
#35378=CARTESIAN_POINT('Ctrl Pts',(-7.05441355906147,-36.6826865021368,
26.0062225217367));
#35379=CARTESIAN_POINT('Ctrl Pts',(-6.99098006290977,-36.5664331386744,
26.0131932043671));
#35380=CARTESIAN_POINT('Ctrl Pts',(-6.87006125878939,-36.3102237985343,
26.0282565425033));
#35381=CARTESIAN_POINT('Ctrl Pts',(-6.81481892294492,-36.1695365786471,
26.0363522838461));
#35382=CARTESIAN_POINT('Ctrl Pts',(-6.75825114706546,-35.9913450430184,
26.0469045926988));
#35383=CARTESIAN_POINT('Ctrl Pts',(-6.74790789526704,-35.9568685101434,
26.0489599117236));
#35384=CARTESIAN_POINT('Ctrl Pts',(-6.73319066519045,-35.9048146605224,
26.0520924790329));
#35385=CARTESIAN_POINT('Ctrl Pts',(-6.72840507145545,-35.887355279121,26.0531480972335));
#35386=CARTESIAN_POINT('Ctrl Pts',(-6.71996330565019,-35.8555601733856,
26.055080784534));
#35387=CARTESIAN_POINT('Ctrl Pts',(-6.71626080182107,-35.8412376477149,
26.0559552758819));
#35388=CARTESIAN_POINT('Ctrl Pts',(-6.70786670185911,-35.8078664835325,
26.058001720546));
#35389=CARTESIAN_POINT('Ctrl Pts',(-6.7032466080321,-35.7888009507106,26.0591774800221));
#35390=CARTESIAN_POINT('Ctrl Pts',(-6.68874004512308,-35.7265827244959,
26.0630334589216));
#35391=CARTESIAN_POINT('Ctrl Pts',(-6.67953378370474,-35.6832778757785,
26.0657469316272));
#35392=CARTESIAN_POINT('Ctrl Pts',(-6.65895609562506,-35.5762152776175,
26.072508098465));
#35393=CARTESIAN_POINT('Ctrl Pts',(-6.64855888022745,-35.5122889800574,
26.0765905603229));
#35394=CARTESIAN_POINT('Ctrl Pts',(-6.60654095726604,-35.1972301629496,
26.0968182803444));
#35395=CARTESIAN_POINT('Ctrl Pts',(-6.60128315806256,-34.9433621271681,
26.1133733876838));
#35396=CARTESIAN_POINT('Ctrl Pts',(-6.63379626043595,-34.58785613312,26.1357417760478));
#35397=CARTESIAN_POINT('Ctrl Pts',(-6.64800289240874,-34.4849185214098,
26.1421323788901));
#35398=CARTESIAN_POINT('Ctrl Pts',(-6.67408617961277,-34.3440630302138,
26.1507498057135));
#35399=CARTESIAN_POINT('Ctrl Pts',(-6.68193156180881,-34.3054655626707,
26.1530981300991));
#35400=CARTESIAN_POINT('Ctrl Pts',(-6.6963059968704,-34.240562780938,26.1570263339079));
#35401=CARTESIAN_POINT('Ctrl Pts',(-6.70248092819276,-34.2141838697252,
26.1586171277142));
#35402=CARTESIAN_POINT('Ctrl Pts',(-6.71562190038833,-34.1609314207618,
26.1618177740163));
#35403=CARTESIAN_POINT('Ctrl Pts',(-6.7226031572945,-34.134063752851,26.1634270074025));
#35404=CARTESIAN_POINT('Ctrl Pts',(-6.74082766727707,-34.0673059747721,
26.1674131029878));
#35405=CARTESIAN_POINT('Ctrl Pts',(-6.75247404875212,-34.027530028233,26.1697770068922));
#35406=CARTESIAN_POINT('Ctrl Pts',(-6.80488914833904,-33.859973807664,26.1796998190131));
#35407=CARTESIAN_POINT('Ctrl Pts',(-6.85249455974218,-33.7344535966079,
26.1870397376459));
#35408=CARTESIAN_POINT('Ctrl Pts',(-6.96432232106842,-33.4852783937836,
26.2017255878084));
#35409=CARTESIAN_POINT('Ctrl Pts',(-7.02897240599284,-33.3621000178203,
26.2090483043451));
#35410=CARTESIAN_POINT('Ctrl Pts',(-7.18222353086735,-33.109205826839,26.2247596311003));
#35411=CARTESIAN_POINT('Ctrl Pts',(-7.27263585152958,-32.9809799028101,
26.233146776698));
#35412=CARTESIAN_POINT('Ctrl Pts',(-7.39421758924553,-32.8316854329314,
26.2440158992788));
#35413=CARTESIAN_POINT('Ctrl Pts',(-7.4172920549161,-32.8042519519879,26.246063051668));
#35414=CARTESIAN_POINT('Ctrl Pts',(-7.45264863034253,-32.7635445997001,
26.2491856309586));
#35415=CARTESIAN_POINT('Ctrl Pts',(-7.46460969206261,-32.7499938416638,
26.2502396323647));
#35416=CARTESIAN_POINT('Ctrl Pts',(-7.48665385528628,-32.725418850499,26.2521792628443));
#35417=CARTESIAN_POINT('Ctrl Pts',(-7.49670227708665,-32.714364698152,26.2530624460443));
#35418=CARTESIAN_POINT('Ctrl Pts',(-7.52019945817633,-32.6888565369721,
26.2551253135916));
#35419=CARTESIAN_POINT('Ctrl Pts',(-7.53370173168165,-32.6744532590733,
26.2563088142036));
#35420=CARTESIAN_POINT('Ctrl Pts',(-7.57839587030927,-32.6276037053638,
26.2602177389312));
#35421=CARTESIAN_POINT('Ctrl Pts',(-7.61010701372241,-32.5956618706364,
26.2629776330275));
#35422=CARTESIAN_POINT('Ctrl Pts',(-7.69006631473472,-32.5182658650929,
26.2698827521669));
#35423=CARTESIAN_POINT('Ctrl Pts',(-7.73902908824637,-32.473578103648,26.2740645185709));
#35424=CARTESIAN_POINT('Ctrl Pts',(-7.99505764738329,-32.2533099340334,
26.2955736995837));
#35425=CARTESIAN_POINT('Ctrl Pts',(-8.22140544168132,-32.1015983993868,
26.3133384524663));
#35426=CARTESIAN_POINT('Ctrl Pts',(-8.5421804687877,-31.9384689103824,26.3357261314496));
#35427=CARTESIAN_POINT('Ctrl Pts',(-8.62247034456128,-31.9015125373524,
26.341132176333));
#35428=CARTESIAN_POINT('Ctrl Pts',(-8.73840037337257,-31.853549958443,26.3486613063678));
#35429=CARTESIAN_POINT('Ctrl Pts',(-8.77291390409971,-31.8399301654411,
26.3508692307131));
#35430=CARTESIAN_POINT('Ctrl Pts',(-8.83288295510866,-31.8173957595879,
26.3546494168831));
#35431=CARTESIAN_POINT('Ctrl Pts',(-8.85823353818087,-31.8082134537633,
26.3562303392996));
#35432=CARTESIAN_POINT('Ctrl Pts',(-8.91054866164516,-31.7899673068413,
26.3594589016785));
#35433=CARTESIAN_POINT('Ctrl Pts',(-8.93752319627041,-31.7809384561716,
26.3611053000019));
#35434=CARTESIAN_POINT('Ctrl Pts',(-9.00730686013322,-31.7585533917055,
26.3653195122652));
#35435=CARTESIAN_POINT('Ctrl Pts',(-9.05027380715635,-31.7457049600124,
26.3678709409509));
#35436=CARTESIAN_POINT('Ctrl Pts',(-9.28076529627067,-31.6817350555673,
26.3813481869752));
#35437=CARTESIAN_POINT('Ctrl Pts',(-9.47217660170899,-31.645958513302,26.3917789287601));
#35438=CARTESIAN_POINT('Ctrl Pts',(-9.86988956466424,-31.6065336636191,
26.4130034303189));
#35439=CARTESIAN_POINT('Ctrl Pts',(-10.0755613419869,-31.6048831516737,
26.4237460936282));
#35440=CARTESIAN_POINT('Ctrl Pts',(-10.3305179848077,-31.6260227368063,
26.4379828610382));
#35441=CARTESIAN_POINT('Ctrl Pts',(-10.3808353652946,-31.631331332962,26.4408389212348));
#35442=CARTESIAN_POINT('Ctrl Pts',(-10.4520974594067,-31.6404665742537,
26.4449731134135));
#35443=CARTESIAN_POINT('Ctrl Pts',(-10.473156123429,-31.6433677317321,26.446205945882));
#35444=CARTESIAN_POINT('Ctrl Pts',(-10.5091345892581,-31.6486696134076,
26.4483334095148));
#35445=CARTESIAN_POINT('Ctrl Pts',(-10.5240679906151,-31.6509723612199,
26.4492227489572));
#35446=CARTESIAN_POINT('Ctrl Pts',(-10.5559164797611,-31.6561016756259,
26.4511335902493));
#35447=CARTESIAN_POINT('Ctrl Pts',(-10.5728255565746,-31.6589567512475,
26.4521564984432));
#35448=CARTESIAN_POINT('Ctrl Pts',(-10.6205009856308,-31.6673792374303,
26.4550629539747));
#35449=CARTESIAN_POINT('Ctrl Pts',(-10.6512122412304,-31.6732440596472,
26.4569615608066));
#35450=CARTESIAN_POINT('Ctrl Pts',(-10.836672362302,-31.7113271106378,26.4685691744811));
#35451=CARTESIAN_POINT('Ctrl Pts',(-10.9890816830527,-31.7539102136194,
26.4787014293021));
#35452=CARTESIAN_POINT('Ctrl Pts',(-11.3858389876231,-31.8953085214995,
26.5058354895143));
#35453=CARTESIAN_POINT('Ctrl Pts',(-11.6226409072967,-32.0122351439981,
26.5227618272676));
#35454=CARTESIAN_POINT('Ctrl Pts',(-11.8852248964148,-32.1824126316501,
26.5417572993969));
#35455=CARTESIAN_POINT('Ctrl Pts',(-11.9263039295433,-32.2103360326956,
26.5447398694716));
#35456=CARTESIAN_POINT('Ctrl Pts',(-11.9907327384722,-32.2562334583408,
26.5494373778344));
#35457=CARTESIAN_POINT('Ctrl Pts',(-12.0144862833857,-32.2736257103926,
26.5511736749775));
#35458=CARTESIAN_POINT('Ctrl Pts',(-12.0592727073015,-32.3073230854144,
26.5544569288129));
#35459=CARTESIAN_POINT('Ctrl Pts',(-12.0803459229166,-32.3235706716264,
26.5560059195984));
#35460=CARTESIAN_POINT('Ctrl Pts',(-12.1284420332533,-32.3615643835789,
26.5595520838058));
#35461=CARTESIAN_POINT('Ctrl Pts',(-12.1553270775538,-32.3834806887348,
26.5615424030793));
#35462=CARTESIAN_POINT('Ctrl Pts',(-12.2414728540983,-32.4559344303847,
26.5679513397322));
#35463=CARTESIAN_POINT('Ctrl Pts',(-12.2993314179036,-32.5081038435288,
26.5723047372074));
#35464=CARTESIAN_POINT('Ctrl Pts',(-12.4370656755033,-32.641180676283,26.5828522676746));
#35465=CARTESIAN_POINT('Ctrl Pts',(-12.5147680926914,-32.7242009170442,
26.5889656108552));
#35466=CARTESIAN_POINT('Ctrl Pts',(-12.7392859507738,-32.9896553456035,
26.6074936889142));
#35467=CARTESIAN_POINT('Ctrl Pts',(-12.871489288313,-33.1834918118743,26.6196426154485));
#35468=CARTESIAN_POINT('Ctrl Pts',(-13.0057340614978,-33.4320953232967,
26.6353892693375));
#35469=CARTESIAN_POINT('Ctrl Pts',(-13.0278814834501,-33.475304765655,26.6381332859469));
#35470=CARTESIAN_POINT('Ctrl Pts',(-13.0573717272145,-33.5360183428181,
26.6420189060492));
#35471=CARTESIAN_POINT('Ctrl Pts',(-13.0655080173236,-33.553132787245,26.6431174733388));
#35472=CARTESIAN_POINT('Ctrl Pts',(-13.0799026601356,-33.5840780026437,
26.6451112449979));
#35473=CARTESIAN_POINT('Ctrl Pts',(-13.0862125285197,-33.5978845551625,
26.6460034342897));
#35474=CARTESIAN_POINT('Ctrl Pts',(-13.0991978172164,-33.6268098908368,
26.6478789637757));
#35475=CARTESIAN_POINT('Ctrl Pts',(-13.1058556962028,-33.6419357322663,
26.6488632232741));
#35476=CARTESIAN_POINT('Ctrl Pts',(-13.1236240344906,-33.6831172084403,
26.6515512100539));
#35477=CARTESIAN_POINT('Ctrl Pts',(-13.1345186940054,-33.7092638385882,
26.6532667455711));
#35478=CARTESIAN_POINT('Ctrl Pts',(-13.1567086308783,-33.7644568695072,
26.6569020894987));
#35479=CARTESIAN_POINT('Ctrl Pts',(-13.1679315584425,-33.793523706734,26.6588246380766));
#35480=CARTESIAN_POINT('Ctrl Pts',(-13.1787501100144,-33.8227350338248,
26.6607619345813));
#35481=CARTESIAN_POINT('Origin',(-10.,-35.,23.));
#35482=CARTESIAN_POINT('',(-13.1787501240207,-33.8227350716434,27.9134187994658));
#35483=CARTESIAN_POINT('',(-13.1787501609633,-33.8227351713926,27.5681448070208));
#35484=CARTESIAN_POINT('',(-13.1787501240207,-33.8227350716434,23.));
#35485=CARTESIAN_POINT('Ctrl Pts',(-13.1787501609633,-33.8227351713926,
27.5681448070208));
#35486=CARTESIAN_POINT('Ctrl Pts',(-13.1643813608665,-33.7839377619137,
27.5655680901549));
#35487=CARTESIAN_POINT('Ctrl Pts',(-13.1492995268026,-33.7453960250088,
27.5630098028168));
#35488=CARTESIAN_POINT('Ctrl Pts',(-13.1092449476349,-33.6483163142835,
27.5565712050213));
#35489=CARTESIAN_POINT('Ctrl Pts',(-13.0833267073364,-33.5901949926469,
27.5527215942986));
#35490=CARTESIAN_POINT('Ctrl Pts',(-13.0418498987587,-33.5038078207362,
27.5470054725543));
#35491=CARTESIAN_POINT('Ctrl Pts',(-13.0275001359323,-33.4749803679706,
27.5450989013236));
#35492=CARTESIAN_POINT('Ctrl Pts',(-13.0018174493583,-33.4251777478082,
27.541805575749));
#35493=CARTESIAN_POINT('Ctrl Pts',(-12.9906701651826,-33.4041099250419,
27.5404125606289));
#35494=CARTESIAN_POINT('Ctrl Pts',(-12.964940509539,-33.3566986492947,27.5372772306927));
#35495=CARTESIAN_POINT('Ctrl Pts',(-12.950227387756,-33.3304281988641,27.5355396253448));
#35496=CARTESIAN_POINT('Ctrl Pts',(-12.9093833772063,-33.2597270433301,
27.5308598489441));
#35497=CARTESIAN_POINT('Ctrl Pts',(-12.8825854768214,-33.2156897803185,
27.5279413885189));
#35498=CARTESIAN_POINT('Ctrl Pts',(-12.7246105800999,-32.9689422747003,
27.5115334046535));
#35499=CARTESIAN_POINT('Ctrl Pts',(-12.573077890682,-32.7800946832824,27.4988217574958));
#35500=CARTESIAN_POINT('Ctrl Pts',(-12.2771947268719,-32.4827645222447,
27.4765592928455));
#35501=CARTESIAN_POINT('Ctrl Pts',(-12.141904666696,-32.3666902011078,27.4670685685695));
#35502=CARTESIAN_POINT('Ctrl Pts',(-11.9741568379915,-32.2442801585959,
27.455263900406));
#35503=CARTESIAN_POINT('Ctrl Pts',(-11.949938424716,-32.227090503062,27.4535585315313));
#35504=CARTESIAN_POINT('Ctrl Pts',(-11.9116558996629,-32.2006679958829,
27.4508558875668));
#35505=CARTESIAN_POINT('Ctrl Pts',(-11.897743034697,-32.1912174708495,27.4498722689473));
#35506=CARTESIAN_POINT('Ctrl Pts',(-11.8711037197195,-32.173410586427,27.4479850771965));
#35507=CARTESIAN_POINT('Ctrl Pts',(-11.8583904396998,-32.1650358411843,
27.447082696634));
#35508=CARTESIAN_POINT('Ctrl Pts',(-11.8301063356236,-32.14667597092,27.4450718566857));
#35509=CARTESIAN_POINT('Ctrl Pts',(-11.8145093358306,-32.1367321027922,
27.4439608775482));
#35510=CARTESIAN_POINT('Ctrl Pts',(-11.760078219655,-32.1026528827749,27.4400785412877));
#35511=CARTESIAN_POINT('Ctrl Pts',(-11.7208392858743,-32.0791769342427,
27.4372707474602));
#35512=CARTESIAN_POINT('Ctrl Pts',(-11.4992150140852,-31.9525991408178,
27.4214120803381));
#35513=CARTESIAN_POINT('Ctrl Pts',(-11.3080580221233,-31.8657895011142,
27.4077648192133));
#35514=CARTESIAN_POINT('Ctrl Pts',(-11.0645877792841,-31.7814008929861,
27.3912148823381));
#35515=CARTESIAN_POINT('Ctrl Pts',(-11.0187229994492,-31.7665914313692,
27.3881300362067));
#35516=CARTESIAN_POINT('Ctrl Pts',(-10.8748300020872,-31.7234950250931,
27.3785675276167));
#35517=CARTESIAN_POINT('Ctrl Pts',(-10.775825532725,-31.6986503006313,27.3721552421899));
#35518=CARTESIAN_POINT('Ctrl Pts',(-10.6049390277344,-31.6638810653378,
27.3614066409619));
#35519=CARTESIAN_POINT('Ctrl Pts',(-10.53358621181,-31.6517276526281,27.357011058869));
#35520=CARTESIAN_POINT('Ctrl Pts',(-10.4284457954929,-31.637266102549,27.3506670227089));
#35521=CARTESIAN_POINT('Ctrl Pts',(-10.3949290634287,-31.6331652515554,
27.3486642052471));
#35522=CARTESIAN_POINT('Ctrl Pts',(-10.335000502167,-31.6267401067101,27.3451167207868));
#35523=CARTESIAN_POINT('Ctrl Pts',(-10.3086125162228,-31.6242236421584,
27.3435662482546));
#35524=CARTESIAN_POINT('Ctrl Pts',(-10.2523493454763,-31.6195234093727,
27.3402839930804));
#35525=CARTESIAN_POINT('Ctrl Pts',(-10.2224691350522,-31.6174255752575,
27.3385549827382));
#35526=CARTESIAN_POINT('Ctrl Pts',(-10.1418306684677,-31.6128372696264,
27.3339244854419));
#35527=CARTESIAN_POINT('Ctrl Pts',(-10.0910368006633,-31.6110916244331,
27.3310458419315));
#35528=CARTESIAN_POINT('Ctrl Pts',(-9.79136223960751,-31.6075355972096,
27.314252463339));
#35529=CARTESIAN_POINT('Ctrl Pts',(-9.54293614804405,-31.6319964111137,
27.3011750101278));
#35530=CARTESIAN_POINT('Ctrl Pts',(-9.18283369375264,-31.7080642270481,
27.2816303785854));
#35531=CARTESIAN_POINT('Ctrl Pts',(-9.06764156705829,-31.7388182408458,
27.2752714006471));
#35532=CARTESIAN_POINT('Ctrl Pts',(-8.89128037632563,-31.7960123153208,
27.2650608821389));
#35533=CARTESIAN_POINT('Ctrl Pts',(-8.82886292459748,-31.8182971395685,
27.2613506692065));
#35534=CARTESIAN_POINT('Ctrl Pts',(-8.74593117112914,-31.8506770630332,
27.2562407327734));
#35535=CARTESIAN_POINT('Ctrl Pts',(-8.72480407748053,-31.8591722607726,
27.2549229228342));
#35536=CARTESIAN_POINT('Ctrl Pts',(-8.68956939028939,-31.8737542159128,
27.2526956450542));
#35537=CARTESIAN_POINT('Ctrl Pts',(-8.67541426678867,-31.8797253784759,
27.2517927951618));
#35538=CARTESIAN_POINT('Ctrl Pts',(-8.64612532627924,-31.8923157719466,
27.2499070103446));
#35539=CARTESIAN_POINT('Ctrl Pts',(-8.63099862683602,-31.8989496765556,
27.2489233019772));
#35540=CARTESIAN_POINT('Ctrl Pts',(-8.59010240544302,-31.9172424959816,
27.2462383929969));
#35541=CARTESIAN_POINT('Ctrl Pts',(-8.56442990275235,-31.9291135745576,
27.2445254276006));
#35542=CARTESIAN_POINT('Ctrl Pts',(-8.40824763206342,-32.0037193468699,
27.2339482870017));
#35543=CARTESIAN_POINT('Ctrl Pts',(-8.28173042756514,-32.074437597072,27.2247136372165));
#35544=CARTESIAN_POINT('Ctrl Pts',(-7.94955891696659,-32.2891039192817,
27.1992754665067));
#35545=CARTESIAN_POINT('Ctrl Pts',(-7.75469953489457,-32.4481527733674,
27.1830534737424));
#35546=CARTESIAN_POINT('Ctrl Pts',(-7.53140141296439,-32.6759775391306,
27.1634391483731));
#35547=CARTESIAN_POINT('Ctrl Pts',(-7.48512666091504,-32.7261327066511,
27.159302369321));
#35548=CARTESIAN_POINT('Ctrl Pts',(-7.41873337237048,-32.80260169821,27.1532546321753));
#35549=CARTESIAN_POINT('Ctrl Pts',(-7.39743750208104,-32.8278661965755,
27.1512963341591));
#35550=CARTESIAN_POINT('Ctrl Pts',(-7.35976781351184,-32.8739053695781,
27.1477973489305));
#35551=CARTESIAN_POINT('Ctrl Pts',(-7.3432615293839,-32.8945677086267,27.1462514646324));
#35552=CARTESIAN_POINT('Ctrl Pts',(-7.3082845860345,-32.9394177481084,27.1429470015176));
#35553=CARTESIAN_POINT('Ctrl Pts',(-7.28989435650107,-32.9636654070215,
27.1411916331636));
#35554=CARTESIAN_POINT('Ctrl Pts',(-7.2403468065514,-33.0308545829959,27.1364095396556));
#35555=CARTESIAN_POINT('Ctrl Pts',(-7.20986648157781,-33.0742858996902,
27.1334083719637));
#35556=CARTESIAN_POINT('Ctrl Pts',(-7.07285580709606,-33.2795985920008,
27.119601327904));
#35557=CARTESIAN_POINT('Ctrl Pts',(-6.97930978398156,-33.4497115805019,
27.1092606810493));
#35558=CARTESIAN_POINT('Ctrl Pts',(-6.83741220874823,-33.7699854450732,
27.0906803702884));
#35559=CARTESIAN_POINT('Ctrl Pts',(-6.78400664131824,-33.9172817198232,
27.0824332969634));
#35560=CARTESIAN_POINT('Ctrl Pts',(-6.71971189664959,-34.1420435312312,
27.0696441038781));
#35561=CARTESIAN_POINT('Ctrl Pts',(-6.70100364014649,-34.217056430038,27.0653414095174));
#35562=CARTESIAN_POINT('Ctrl Pts',(-6.67987290411002,-34.3160876629172,
27.0595403772934));
#35563=CARTESIAN_POINT('Ctrl Pts',(-6.67511831688643,-34.3395897176305,
27.05815486262));
#35564=CARTESIAN_POINT('Ctrl Pts',(-6.66768308675801,-34.3784596970306,
27.0558459286593));
#35565=CARTESIAN_POINT('Ctrl Pts',(-6.66485839126151,-34.3937997068489,
27.0549302444276));
#35566=CARTESIAN_POINT('Ctrl Pts',(-6.6596715321306,-34.4231019996741,27.0531716989397));
#35567=CARTESIAN_POINT('Ctrl Pts',(-6.65729080581259,-34.43706056888,27.0523299681995));
#35568=CARTESIAN_POINT('Ctrl Pts',(-6.65102308935945,-34.4752514621302,
27.0500167595333));
#35569=CARTESIAN_POINT('Ctrl Pts',(-6.64731177780774,-34.4995112543806,
27.0485361352145));
#35570=CARTESIAN_POINT('Ctrl Pts',(-6.63319544764557,-34.5990012943337,
27.0424240480923));
#35571=CARTESIAN_POINT('Ctrl Pts',(-6.6250573262537,-34.6745262833766,27.0376911637111));
#35572=CARTESIAN_POINT('Ctrl Pts',(-6.60425265632037,-34.9561373062805,
27.0198457310312));
#35573=CARTESIAN_POINT('Ctrl Pts',(-6.60788209419339,-35.162976625266,27.0063766598641));
#35574=CARTESIAN_POINT('Ctrl Pts',(-6.648045311981,-35.5305406980391,26.9827752344443));
#35575=CARTESIAN_POINT('Ctrl Pts',(-6.67749351563748,-35.6914017720423,
26.97255754757));
#35576=CARTESIAN_POINT('Ctrl Pts',(-6.72932968277317,-35.8916345909871,
26.9600664028032));
#35577=CARTESIAN_POINT('Ctrl Pts',(-6.74103904799746,-35.9335257601553,
26.9574649922675));
#35578=CARTESIAN_POINT('Ctrl Pts',(-6.76165543098856,-36.0021591580661,
26.9532208738375));
#35579=CARTESIAN_POINT('Ctrl Pts',(-6.77009522292039,-36.0290353386993,
26.9515634968187));
#35580=CARTESIAN_POINT('Ctrl Pts',(-6.78721870717594,-36.0812770345316,
26.9483498890499));
#35581=CARTESIAN_POINT('Ctrl Pts',(-6.7958702169174,-36.1066508277452,26.9467927597209));
#35582=CARTESIAN_POINT('Ctrl Pts',(-6.81743683136609,-36.1675289639846,
26.9430644194347));
#35583=CARTESIAN_POINT('Ctrl Pts',(-6.83064639531074,-36.2029256395468,
26.9409029499154));
#35584=CARTESIAN_POINT('Ctrl Pts',(-6.87815348722067,-36.3240077944213,
26.9335238726485));
#35585=CARTESIAN_POINT('Ctrl Pts',(-6.9153577825169,-36.40851220673,26.9284008903459));
#35586=CARTESIAN_POINT('Ctrl Pts',(-7.07325039934854,-36.7307805053421,
26.9088002061576));
#35587=CARTESIAN_POINT('Ctrl Pts',(-7.21835204256103,-36.9554768439312,
26.8950696547273));
#35588=CARTESIAN_POINT('Ctrl Pts',(-7.43027226994807,-37.2116161311006,
26.8770631742104));
#35589=CARTESIAN_POINT('Ctrl Pts',(-7.47374395077426,-37.261144848647,26.8734503832279));
#35590=CARTESIAN_POINT('Ctrl Pts',(-7.54916387998048,-37.3421819318584,
26.8672545310238));
#35591=CARTESIAN_POINT('Ctrl Pts',(-7.58034507818804,-37.3743806670719,
26.8647121229581));
#35592=CARTESIAN_POINT('Ctrl Pts',(-7.62614415678353,-37.4198351223223,
26.8609883304553));
#35593=CARTESIAN_POINT('Ctrl Pts',(-7.6402549104934,-37.4335974719789,26.8598424066997));
#35594=CARTESIAN_POINT('Ctrl Pts',(-7.66526830996823,-37.4575711815212,
26.8578117657721));
#35595=CARTESIAN_POINT('Ctrl Pts',(-7.67611966867757,-37.4678347533675,
26.8569309760888));
#35596=CARTESIAN_POINT('Ctrl Pts',(-7.7002696094403,-37.49037602687,26.8549707278462));
#35597=CARTESIAN_POINT('Ctrl Pts',(-7.71359874458483,-37.5026190064143,
26.8538889432502));
#35598=CARTESIAN_POINT('Ctrl Pts',(-7.75370929357483,-37.5388731547109,
26.8506357390741));
#35599=CARTESIAN_POINT('Ctrl Pts',(-7.7807747187098,-37.562564684434,26.8484433988428));
#35600=CARTESIAN_POINT('Ctrl Pts',(-7.92315109332242,-37.6832455514444,
26.8369480518014));
#35601=CARTESIAN_POINT('Ctrl Pts',(-8.04445070891223,-37.7728916180789,
26.8272864418007));
#35602=CARTESIAN_POINT('Ctrl Pts',(-8.28213386071937,-37.9251783213993,
26.8091010239399));
#35603=CARTESIAN_POINT('Ctrl Pts',(-8.39701516869686,-37.989677964705,26.8006018354876));
#35604=CARTESIAN_POINT('Ctrl Pts',(-8.64606803263779,-38.1110148204502,
26.7830002692553));
#35605=CARTESIAN_POINT('Ctrl Pts',(-8.78075004027341,-38.166225396847,26.7739477666337));
#35606=CARTESIAN_POINT('Ctrl Pts',(-8.9586966417522,-38.2261252883098,26.762620658718));
#35607=CARTESIAN_POINT('Ctrl Pts',(-8.99906733322436,-38.2388780618731,
26.7600907149053));
#35608=CARTESIAN_POINT('Ctrl Pts',(-9.06645817759303,-38.2587858305177,
26.7559315267622));
#35609=CARTESIAN_POINT('Ctrl Pts',(-9.09334600186111,-38.26636862904,26.7542887683861));
#35610=CARTESIAN_POINT('Ctrl Pts',(-9.14635811110742,-38.2806138514496,
26.7510815992656));
#35611=CARTESIAN_POINT('Ctrl Pts',(-9.17247416380091,-38.2872987038947,
26.7495165777871));
#35612=CARTESIAN_POINT('Ctrl Pts',(-9.23028737403051,-38.3013643417998,
26.7460837100557));
#35613=CARTESIAN_POINT('Ctrl Pts',(-9.26201687841528,-38.3086016774235,
26.7442204828709));
#35614=CARTESIAN_POINT('Ctrl Pts',(-9.37273114119309,-38.3321830583544,
26.73778670631));
#35615=CARTESIAN_POINT('Ctrl Pts',(-9.45219391236756,-38.3461649698683,
26.7332887801457));
#35616=CARTESIAN_POINT('Ctrl Pts',(-9.8099106929276,-38.3960209019083,26.7134482685919));
#35617=CARTESIAN_POINT('Ctrl Pts',(-10.0914482915887,-38.4001058095978,
26.6990266168772));
#35618=CARTESIAN_POINT('Ctrl Pts',(-10.4368141211214,-38.3621541916367,
26.6802203311006));
#35619=CARTESIAN_POINT('Ctrl Pts',(-10.5031291686947,-38.3528715342877,
26.676551959183));
#35620=CARTESIAN_POINT('Ctrl Pts',(-10.6138086552864,-38.3340214136477,
26.6702710420488));
#35621=CARTESIAN_POINT('Ctrl Pts',(-10.6583356234607,-38.3255155465053,
26.6677006183227));
#35622=CARTESIAN_POINT('Ctrl Pts',(-10.7220432405637,-38.3120160835871,
26.6639430866258));
#35623=CARTESIAN_POINT('Ctrl Pts',(-10.7413732819027,-38.3077428248048,
26.6627923329609));
#35624=CARTESIAN_POINT('Ctrl Pts',(-10.7752264897846,-38.2999473109075,
26.6607565162829));
#35625=CARTESIAN_POINT('Ctrl Pts',(-10.7897655231144,-38.2964979556856,
26.6598754567988));
#35626=CARTESIAN_POINT('Ctrl Pts',(-10.8218010594089,-38.2886734890689,
26.6579188632706));
#35627=CARTESIAN_POINT('Ctrl Pts',(-10.8392855297969,-38.2842548723115,
26.6568410635853));
#35628=CARTESIAN_POINT('Ctrl Pts',(-10.8912166359325,-38.2706892545022,
26.6536119766901));
#35629=CARTESIAN_POINT('Ctrl Pts',(-10.925554147983,-38.2611385425921,26.6514402050523));
#35630=CARTESIAN_POINT('Ctrl Pts',(-11.0983744421087,-38.210120736119,26.6403453218782));
#35631=CARTESIAN_POINT('Ctrl Pts',(-11.2342451086578,-38.1603692727695,
26.631091344763));
#35632=CARTESIAN_POINT('Ctrl Pts',(-11.4798383103547,-38.0521825339116,
26.6138102530762));
#35633=CARTESIAN_POINT('Ctrl Pts',(-11.5903456795482,-37.996087760883,26.6058090486547));
#35634=CARTESIAN_POINT('Ctrl Pts',(-11.7889218549526,-37.8811994277568,
26.591183772273));
#35635=CARTESIAN_POINT('Ctrl Pts',(-11.8777917220539,-37.8240844093866,
26.5845375592733));
#35636=CARTESIAN_POINT('Ctrl Pts',(-12.0242457051605,-37.7199859788669,
26.5734516970385));
#35637=CARTESIAN_POINT('Ctrl Pts',(-12.0832145070974,-37.6750912108364,
26.5689475692721));
#35638=CARTESIAN_POINT('Ctrl Pts',(-12.1670755527956,-37.6067889374803,
26.5624799775202));
#35639=CARTESIAN_POINT('Ctrl Pts',(-12.1931580784501,-37.5848835149813,
26.5604590738322));
#35640=CARTESIAN_POINT('Ctrl Pts',(-12.2389677001923,-37.5452176475842,
26.5568916156273));
#35641=CARTESIAN_POINT('Ctrl Pts',(-12.2588243685801,-37.5276118704048,
26.5553390080314));
#35642=CARTESIAN_POINT('Ctrl Pts',(-12.3005196453697,-37.4897592448251,
26.5520643880616));
#35643=CARTESIAN_POINT('Ctrl Pts',(-12.3223024083116,-37.4694540574639,
26.5503449841888));
#35644=CARTESIAN_POINT('Ctrl Pts',(-12.3808847611805,-37.4133847064915,
26.5456945828851));
#35645=CARTESIAN_POINT('Ctrl Pts',(-12.4171451048612,-37.3770670831036,
26.5427872703335));
#35646=CARTESIAN_POINT('Ctrl Pts',(-12.6250171846187,-37.1591893865509,
26.5259119482922));
#35647=CARTESIAN_POINT('Ctrl Pts',(-12.7769569875033,-36.959932397515,26.5127882387389));
#35648=CARTESIAN_POINT('Ctrl Pts',(-12.9667199856531,-36.6440950197546,
26.4932202044339));
#35649=CARTESIAN_POINT('Ctrl Pts',(-13.022428787916,-36.5392845628019,26.4868881874643));
#35650=CARTESIAN_POINT('Ctrl Pts',(-13.1004416261757,-36.3718726463021,
26.4767154394661));
#35651=CARTESIAN_POINT('Ctrl Pts',(-13.1265969675572,-36.3111686007616,
26.4730147892819));
#35652=CARTESIAN_POINT('Ctrl Pts',(-13.159347275358,-36.2285957104624,26.4679160605329));
#35653=CARTESIAN_POINT('Ctrl Pts',(-13.1675214715775,-36.2073650205264,
26.4665994374467));
#35654=CARTESIAN_POINT('Ctrl Pts',(-13.1808551926849,-36.1716659973395,
26.4643735760864));
#35655=CARTESIAN_POINT('Ctrl Pts',(-13.186131352381,-36.1572415325053,26.4634709364931));
#35656=CARTESIAN_POINT('Ctrl Pts',(-13.1968803503905,-36.1272240969356,
26.4615849070096));
#35657=CARTESIAN_POINT('Ctrl Pts',(-13.2023374466621,-36.1116262824911,
26.4606007355055));
#35658=CARTESIAN_POINT('Ctrl Pts',(-13.2168363248903,-36.0691917869529,
26.4579132437476));
#35659=CARTESIAN_POINT('Ctrl Pts',(-13.2256560046555,-36.042281269149,26.456198122282));
#35660=CARTESIAN_POINT('Ctrl Pts',(-13.2797922504546,-35.8698295941028,
26.4451522720509));
#35661=CARTESIAN_POINT('Ctrl Pts',(-13.3155812996538,-35.7214935176125,
26.4354108845216));
#35662=CARTESIAN_POINT('Ctrl Pts',(-13.3733890042827,-35.3833848395515,
26.4133313788544));
#35663=CARTESIAN_POINT('Ctrl Pts',(-13.3896100394668,-35.1931105210115,
26.4010055067278));
#35664=CARTESIAN_POINT('Ctrl Pts',(-13.3898250629205,-34.8983315803273,
26.3825329145607));
#35665=CARTESIAN_POINT('Ctrl Pts',(-13.3851018685923,-34.7942352126983,
26.3761238809521));
#35666=CARTESIAN_POINT('Ctrl Pts',(-13.3719934748467,-34.6512612540976,
26.3674867017218));
#35667=CARTESIAN_POINT('Ctrl Pts',(-13.3677102680831,-34.6120741640032,
26.365136301304));
#35668=CARTESIAN_POINT('Ctrl Pts',(-13.3596408897165,-34.5485301049426,
26.3613510938373));
#35669=CARTESIAN_POINT('Ctrl Pts',(-13.3562709821072,-34.5241248940409,
26.3599035917135));
#35670=CARTESIAN_POINT('Ctrl Pts',(-13.3486063365844,-34.4727562249109,
26.3568693632134));
#35671=CARTESIAN_POINT('Ctrl Pts',(-13.3442512838865,-34.445803455646,26.3552846252909));
#35672=CARTESIAN_POINT('Ctrl Pts',(-13.3328777702249,-34.3804394466201,
26.3514576980142));
#35673=CARTESIAN_POINT('Ctrl Pts',(-13.3255202663303,-34.3420907003197,
26.3492262057105));
#35674=CARTESIAN_POINT('Ctrl Pts',(-13.2949464803174,-34.1963858352286,
26.3407913880578));
#35675=CARTESIAN_POINT('Ctrl Pts',(-13.2671793421232,-34.0900492891848,
26.3347292253266));
#35676=CARTESIAN_POINT('Ctrl Pts',(-13.2171487806147,-33.9305891135584,
26.325664421708));
#35677=CARTESIAN_POINT('Ctrl Pts',(-13.1986265369331,-33.8764036723632,
26.3225882159661));
#35678=CARTESIAN_POINT('Ctrl Pts',(-13.1787501930238,-33.8227352579598,
26.3195306104224));
#35679=CARTESIAN_POINT('',(-13.3897497681227,-34.9987462009367,26.7339821967504));
#35680=CARTESIAN_POINT('Ctrl Pts',(-13.1787501100144,-33.8227350338248,
26.6607619345813));
#35681=CARTESIAN_POINT('Ctrl Pts',(-13.2216841843832,-33.9386619470895,
26.6684502125966));
#35682=CARTESIAN_POINT('Ctrl Pts',(-13.258249581665,-34.0568647109076,26.6763673997128));
#35683=CARTESIAN_POINT('Ctrl Pts',(-13.3167604124846,-34.2905904905764,
26.6918795664257));
#35684=CARTESIAN_POINT('Ctrl Pts',(-13.3393195908669,-34.4057716545837,
26.6994587083872));
#35685=CARTESIAN_POINT('Ctrl Pts',(-13.3783572706517,-34.6797789408598,
26.7171358122187));
#35686=CARTESIAN_POINT('Ctrl Pts',(-13.3896826954089,-34.8390678269662,
26.7271303610769));
#35687=CARTESIAN_POINT('Ctrl Pts',(-13.3897497009165,-34.9985760489549,
26.7367914542175));
#35688=CARTESIAN_POINT('Ctrl Pts',(-13.3897497681227,-34.9987462009367,
26.7339821967504));
#35689=CARTESIAN_POINT('Ctrl Pts',(-13.3897890807776,-35.1050312244497,
26.7401898647502));
#35690=CARTESIAN_POINT('Ctrl Pts',(-13.384825222301,-35.2112871201384,26.7463975327499));
#35691=CARTESIAN_POINT('Ctrl Pts',(-13.3748927040034,-35.3170241299407,
26.7526052007497));
#35692=CARTESIAN_POINT('Ctrl Pts',(-13.3649548482649,-35.4228179596774,
26.7588162045662));
#35693=CARTESIAN_POINT('Ctrl Pts',(-13.3500430540965,-35.5280919481609,
26.7650272083827));
#35694=CARTESIAN_POINT('Ctrl Pts',(-13.3302435188097,-35.6323631614237,
26.7712382121992));
#35695=CARTESIAN_POINT('Ctrl Pts',(-13.3101893565053,-35.7379753287885,
26.7775290910914));
#35696=CARTESIAN_POINT('Ctrl Pts',(-13.2851209398701,-35.8425583312712,
26.7838199699835));
#35697=CARTESIAN_POINT('Ctrl Pts',(-13.2551803933349,-35.9456244864363,
26.7901108488757));
#35698=CARTESIAN_POINT('Ctrl Pts',(-13.2255498660117,-36.0476234437076,
26.7963365888995));
#35699=CARTESIAN_POINT('Ctrl Pts',(-13.1911478356904,-36.1481364617781,
26.8025623289234));
#35700=CARTESIAN_POINT('Ctrl Pts',(-13.1521609226748,-36.2467103031827,
26.8087880689473));
#35701=CARTESIAN_POINT('Ctrl Pts',(-13.1125621394122,-36.3468311868132,
26.8151115172736));
#35702=CARTESIAN_POINT('Ctrl Pts',(-13.0682335273692,-36.4449511173892,
26.8214349655998));
#35703=CARTESIAN_POINT('Ctrl Pts',(-13.0194189846595,-36.5406213219276,
26.8277584139261));
#35704=CARTESIAN_POINT('Ctrl Pts',(-12.9706044419497,-36.6362915264661,
26.8340818622524));
#35705=CARTESIAN_POINT('Ctrl Pts',(-12.9173042373172,-36.7295116662979,
26.8404053105786));
#35706=CARTESIAN_POINT('Ctrl Pts',(-12.8598073032938,-36.819864624231,26.8467287589049));
#35707=CARTESIAN_POINT('Ctrl Pts',(-12.8043271157924,-36.9070483868538,
26.8528304077103));
#35708=CARTESIAN_POINT('Ctrl Pts',(-12.7447627250912,-36.9918401274393,
26.8589320565157));
#35709=CARTESIAN_POINT('Ctrl Pts',(-12.6813468174827,-37.0738332398906,
26.8650337053211));
#35710=CARTESIAN_POINT('Ctrl Pts',(-12.6180143251107,-37.1557185012503,
26.8711273282147));
#35711=CARTESIAN_POINT('Ctrl Pts',(-12.5508406470472,-37.2348121173873,
26.8772209511084));
#35712=CARTESIAN_POINT('Ctrl Pts',(-12.4801026278758,-37.3107349518505,
26.883314574002));
#35713=CARTESIAN_POINT('Ctrl Pts',(-12.4094374149536,-37.3865796436562,
26.8894019251081));
#35714=CARTESIAN_POINT('Ctrl Pts',(-12.3352154459125,-37.4592597319462,
26.8954892762142));
#35715=CARTESIAN_POINT('Ctrl Pts',(-12.257754298081,-37.5284284826739,26.9015766273203));
#35716=CARTESIAN_POINT('Ctrl Pts',(-12.1803482539649,-37.5975480286678,
26.9076596480534));
#35717=CARTESIAN_POINT('Ctrl Pts',(-12.0997079314097,-37.6631609202428,
26.9137426687865));
#35718=CARTESIAN_POINT('Ctrl Pts',(-12.0161876933331,-37.7249572928309,
26.9198256895197));
#35719=CARTESIAN_POINT('Ctrl Pts',(-11.9326983778213,-37.7867307859064,
26.9259064580729));
#35720=CARTESIAN_POINT('Ctrl Pts',(-11.8463316094067,-37.8446903141597,
26.931987226626));
#35721=CARTESIAN_POINT('Ctrl Pts',(-11.7574741265705,-37.8985668453453,
26.9380679951792));
#35722=CARTESIAN_POINT('Ctrl Pts',(-11.6686265213079,-37.9524373875091,
26.9441480877822));
#35723=CARTESIAN_POINT('Ctrl Pts',(-11.5772891179516,-38.0022256133608,
26.9502281803851));
#35724=CARTESIAN_POINT('Ctrl Pts',(-11.4838760925702,-38.0477068107675,
26.956308272988));
#35725=CARTESIAN_POINT('Ctrl Pts',(-11.390449250198,-38.0931947354296,26.9623892649151));
#35726=CARTESIAN_POINT('Ctrl Pts',(-11.2949465604751,-38.1343741786936,
26.9684702568421));
#35727=CARTESIAN_POINT('Ctrl Pts',(-11.1978043188133,-38.1710676240554,
26.9745512487691));
#35728=CARTESIAN_POINT('Ctrl Pts',(-11.100561247805,-38.207799155589,26.9806385524965));
#35729=CARTESIAN_POINT('Ctrl Pts',(-11.0016756271896,-38.2400352388196,
26.986725856224));
#35730=CARTESIAN_POINT('Ctrl Pts',(-10.9016011110949,-38.2676475481564,
26.9928131599514));
#35731=CARTESIAN_POINT('Ctrl Pts',(-10.8014728281809,-38.295274692699,26.9989037341914));
#35732=CARTESIAN_POINT('Ctrl Pts',(-10.700154794652,-38.3182730203065,27.0049943084314));
#35733=CARTESIAN_POINT('Ctrl Pts',(-10.5981111607529,-38.3365653150932,
27.0110848826714));
#35734=CARTESIAN_POINT('Ctrl Pts',(-10.4959009340921,-38.3548874732216,
27.0171854001635));
#35735=CARTESIAN_POINT('Ctrl Pts',(-10.3929631649858,-38.3684881943241,
27.0232859176557));
#35736=CARTESIAN_POINT('Ctrl Pts',(-10.2897676712297,-38.3773421146236,
27.0293864351478));
#35737=CARTESIAN_POINT('Ctrl Pts',(-10.2084487595871,-38.3843190778254,
27.034193693923));
#35738=CARTESIAN_POINT('Ctrl Pts',(-10.1269699497257,-38.3883495208024,
27.0390009526982));
#35739=CARTESIAN_POINT('Ctrl Pts',(-10.045559979307,-38.3894438114218,27.0438082114734));
#35740=CARTESIAN_POINT('Ctrl Pts',(-9.94222969266637,-38.3908327489535,
27.0499098649274));
#35741=CARTESIAN_POINT('Ctrl Pts',(-9.8386612147156,-38.3874945496007,27.0560115183814));
#35742=CARTESIAN_POINT('Ctrl Pts',(-9.73532216989635,-38.3794009393311,
27.0621131718354));
#35743=CARTESIAN_POINT('Ctrl Pts',(-9.63211905313828,-38.3713179750738,
27.0682067994176));
#35744=CARTESIAN_POINT('Ctrl Pts',(-9.52914519239832,-38.3584920683563,
27.0743004269998));
#35745=CARTESIAN_POINT('Ctrl Pts',(-9.42686944319496,-38.3409469357289,
27.0803940545821));
#35746=CARTESIAN_POINT('Ctrl Pts',(-9.32469895942654,-38.3234198611067,
27.0864814104101));
#35747=CARTESIAN_POINT('Ctrl Pts',(-9.22322557777763,-38.3011832910373,
27.0925687662381));
#35748=CARTESIAN_POINT('Ctrl Pts',(-9.12291338147732,-38.2743127715764,
27.0986561220662));
#35749=CARTESIAN_POINT('Ctrl Pts',(-9.0226725439398,-38.2474613669101,27.1047391475516));
#35750=CARTESIAN_POINT('Ctrl Pts',(-8.92359166110563,-38.2159826784515,
27.110822173037));
#35751=CARTESIAN_POINT('Ctrl Pts',(-8.82612414410728,-38.1800032291575,
27.1169051985224));
#35752=CARTESIAN_POINT('Ctrl Pts',(-8.72869271321997,-38.1440371007979,
27.1229859718448));
#35753=CARTESIAN_POINT('Ctrl Pts',(-8.63287386186256,-38.1035736713432,
27.1290667451673));
#35754=CARTESIAN_POINT('Ctrl Pts',(-8.53910459725674,-38.0587889245163,
27.1351475184897));
#35755=CARTESIAN_POINT('Ctrl Pts',(-8.44534575604772,-38.0140091559645,
27.141227615873));
#35756=CARTESIAN_POINT('Ctrl Pts',(-8.35363643452957,-37.9649092095808,
27.1473077132563));
#35757=CARTESIAN_POINT('Ctrl Pts',(-8.26439161211884,-37.9117123117534,
27.1533878106396));
#35758=CARTESIAN_POINT('Ctrl Pts',(-8.17513358917933,-37.8585075453779,
27.1594688073524));
#35759=CARTESIAN_POINT('Ctrl Pts',(-8.08834115704462,-37.8012048426389,
27.1655498040653));
#35760=CARTESIAN_POINT('Ctrl Pts',(-8.0044019470703,-37.7400718008189,27.1716308007781));
#35761=CARTESIAN_POINT('Ctrl Pts',(-7.92037561227555,-37.6788753058727,
27.1777181092699));
#35762=CARTESIAN_POINT('Ctrl Pts',(-7.83920876045743,-37.6138407843401,
27.1838054177618));
#35763=CARTESIAN_POINT('Ctrl Pts',(-7.76125739651567,-37.5452773164911,
27.1898927262536));
#35764=CARTESIAN_POINT('Ctrl Pts',(-7.68326415190567,-37.4766770117773,
27.1959833052533));
#35765=CARTESIAN_POINT('Ctrl Pts',(-7.60849014427039,-37.4045442811282,
27.202073884253));
#35766=CARTESIAN_POINT('Ctrl Pts',(-7.53725438541685,-37.3292249999413,
27.2081644632527));
#35767=CARTESIAN_POINT('Ctrl Pts',(-7.46590233038794,-37.2537827560111,
27.2142649854474));
#35768=CARTESIAN_POINT('Ctrl Pts',(-7.39810034314356,-37.1751438932789,
27.2203655076422));
#35769=CARTESIAN_POINT('Ctrl Pts',(-7.33412717462984,-37.0936874507559,
27.2264660298369));
#35770=CARTESIAN_POINT('Ctrl Pts',(-7.28371631876174,-37.0294997752202,
27.2312732412386));
#35771=CARTESIAN_POINT('Ctrl Pts',(-7.23568215067551,-36.9635632256665,
27.2360804526402));
#35772=CARTESIAN_POINT('Ctrl Pts',(-7.19014138122318,-36.8960747888693,
27.2408876640418));
#35773=CARTESIAN_POINT('Ctrl Pts',(-7.13233799060928,-36.8104139508768,
27.2469892982864));
#35774=CARTESIAN_POINT('Ctrl Pts',(-7.0783576454435,-36.7219626636669,27.2530909325309));
#35775=CARTESIAN_POINT('Ctrl Pts',(-7.02848032780385,-36.6310965330879,
27.2591925667755));
#35776=CARTESIAN_POINT('Ctrl Pts',(-6.97866861725399,-36.5403499250227,
27.265286175118));
#35777=CARTESIAN_POINT('Ctrl Pts',(-6.93294940888755,-36.4471951602325,
27.2713797834605));
#35778=CARTESIAN_POINT('Ctrl Pts',(-6.89155987630513,-36.3520373737082,
27.2774733918029));
#35779=CARTESIAN_POINT('Ctrl Pts',(-6.85021294330727,-36.256977526975,27.2835607283862));
#35780=CARTESIAN_POINT('Ctrl Pts',(-6.81318699451426,-36.1599191481521,
27.2896480649694));
#35781=CARTESIAN_POINT('Ctrl Pts',(-6.78067323890418,-36.0612917920121,
27.2957354015527));
#35782=CARTESIAN_POINT('Ctrl Pts',(-6.7481826121946,-35.9627345951713,27.301818407864));
#35783=CARTESIAN_POINT('Ctrl Pts',(-6.72019792928452,-35.8626110455444,
27.3079014141754));
#35784=CARTESIAN_POINT('Ctrl Pts',(-6.69686191353556,-35.7613697158727,
27.3139844204867));
#35785=CARTESIAN_POINT('Ctrl Pts',(-6.6735345374864,-35.6601658688075,27.3200651746849));
#35786=CARTESIAN_POINT('Ctrl Pts',(-6.65485250403436,-35.5578454805441,
27.326145928883));
#35787=CARTESIAN_POINT('Ctrl Pts',(-6.64090817697617,-35.4548705167346,
27.3322266830812));
#35788=CARTESIAN_POINT('Ctrl Pts',(-6.62696539980954,-35.3519069984418,
27.3383067614124));
#35789=CARTESIAN_POINT('Ctrl Pts',(-6.61775933931373,-35.248289473158,27.3443868397437));
#35790=CARTESIAN_POINT('Ctrl Pts',(-6.61333077204748,-35.1444873798624,
27.3504669180749));
#35791=CARTESIAN_POINT('Ctrl Pts',(-6.60890154966468,-35.0406699311559,
27.3565478958302));
#35792=CARTESIAN_POINT('Ctrl Pts',(-6.60925124284346,-34.9366682876005,
27.3626288735855));
#35793=CARTESIAN_POINT('Ctrl Pts',(-6.61436852639487,-34.832953337554,27.3687098513408));
#35794=CARTESIAN_POINT('Ctrl Pts',(-6.6194911216758,-34.7291307316084,27.3747971411382));
#35795=CARTESIAN_POINT('Ctrl Pts',(-6.62939116927492,-34.6255958415428,
27.3808844309356));
#35796=CARTESIAN_POINT('Ctrl Pts',(-6.64400531235691,-34.522815843713,27.386971720733));
#35797=CARTESIAN_POINT('Ctrl Pts',(-6.65862730743689,-34.4199806234639,
27.3930622811557));
#35798=CARTESIAN_POINT('Ctrl Pts',(-6.6779683635389,-34.3179015237124,27.3991528415785));
#35799=CARTESIAN_POINT('Ctrl Pts',(-6.70191407119283,-34.2170349505219,
27.4052434020012));
#35800=CARTESIAN_POINT('Ctrl Pts',(-6.72589887312402,-34.116003700395,27.4113439060039));
#35801=CARTESIAN_POINT('Ctrl Pts',(-6.75450322669983,-34.0161893429761,
27.4174444100066));
#35802=CARTESIAN_POINT('Ctrl Pts',(-6.78756291584155,-33.9180327903196,
27.4235449140092));
#35803=CARTESIAN_POINT('Ctrl Pts',(-6.81361505484069,-33.8406821491045,
27.4283523148762));
#35804=CARTESIAN_POINT('Ctrl Pts',(-6.84243293384911,-33.7643607104903,
27.4331597157432));
#35805=CARTESIAN_POINT('Ctrl Pts',(-6.87391576234909,-33.6892740936372,
27.4379671166102));
#35806=CARTESIAN_POINT('Ctrl Pts',(-6.9138744530809,-33.5939725262786,27.4440687743589));
#35807=CARTESIAN_POINT('Ctrl Pts',(-6.95826267774881,-33.500338838719,27.4501704321076));
#35808=CARTESIAN_POINT('Ctrl Pts',(-7.00691976425638,-33.4088130955476,
27.4562720898564));
#35809=CARTESIAN_POINT('Ctrl Pts',(-7.05551284823835,-33.3174077434464,
27.4623657216106));
#35810=CARTESIAN_POINT('Ctrl Pts',(-7.10836343177939,-33.2281051979174,
27.4684593533649));
#35811=CARTESIAN_POINT('Ctrl Pts',(-7.16526267946933,-33.1413259064347,
27.4745529851191));
#35812=CARTESIAN_POINT('Ctrl Pts',(-7.22210336351543,-33.0546359326799,
27.4806403449929));
#35813=CARTESIAN_POINT('Ctrl Pts',(-7.28298419211704,-32.9704644045166,
27.4867277048667));
#35814=CARTESIAN_POINT('Ctrl Pts',(-7.34765070978279,-32.8892067118772,
27.4928150647405));
#35815=CARTESIAN_POINT('Ctrl Pts',(-7.41227122369864,-32.8080068259468,
27.4988980940675));
#35816=CARTESIAN_POINT('Ctrl Pts',(-7.48067180556188,-32.7297169871251,
27.5049811233945));
#35817=CARTESIAN_POINT('Ctrl Pts',(-7.5525555158057,-32.654702458261,27.5110641527215));
#35818=CARTESIAN_POINT('Ctrl Pts',(-7.62441261054486,-32.5797157041116,
27.5171449297594));
#35819=CARTESIAN_POINT('Ctrl Pts',(-7.69974997492076,-32.5080021582398,
27.5232257067974));
#35820=CARTESIAN_POINT('Ctrl Pts',(-7.77823186265473,-32.4398923057072,
27.5293064838353));
#35821=CARTESIAN_POINT('Ctrl Pts',(-7.85670502466954,-32.3717900257172,
27.5353865848045));
#35822=CARTESIAN_POINT('Ctrl Pts',(-7.93832169178252,-32.3072909227079,
27.5414666857736));
#35823=CARTESIAN_POINT('Ctrl Pts',(-8.02271158897098,-32.2466864322947,
27.5475467867428));
#35824=CARTESIAN_POINT('Ctrl Pts',(-8.10711396672057,-32.1860729789833,
27.5536277869081));
#35825=CARTESIAN_POINT('Ctrl Pts',(-8.19429004191073,-32.129355532131,27.5597087870734));
#35826=CARTESIAN_POINT('Ctrl Pts',(-8.28383976695354,-32.0767827454994,
27.5657897872387));
#35827=CARTESIAN_POINT('Ctrl Pts',(-8.37348243687032,-32.0241553928596,
27.5718770989566));
#35828=CARTESIAN_POINT('Ctrl Pts',(-8.46550330714674,-31.9756815084767,
27.5779644106745));
#35829=CARTESIAN_POINT('Ctrl Pts',(-8.55947691288674,-31.9315641936006,
27.5840517223923));
#35830=CARTESIAN_POINT('Ctrl Pts',(-8.65350100562476,-31.8874231768482,
27.5901423044976));
#35831=CARTESIAN_POINT('Ctrl Pts',(-8.74947952832602,-31.8476435556022,
27.5962328866028));
#35832=CARTESIAN_POINT('Ctrl Pts',(-8.84696803868841,-31.8123798283525,
27.602323468708));
#35833=CARTESIAN_POINT('Ctrl Pts',(-8.94461570049785,-31.7770585325422,
27.6084239937794));
#35834=CARTESIAN_POINT('Ctrl Pts',(-9.04377786564368,-31.7462679852451,
27.6145245188508));
#35835=CARTESIAN_POINT('Ctrl Pts',(-9.14399574824647,-31.7201125349366,
27.6206250439221));
#35836=CARTESIAN_POINT('Ctrl Pts',(-9.22296680446462,-31.6995022058908,
27.6254322190076));
#35837=CARTESIAN_POINT('Ctrl Pts',(-9.30259308017987,-31.6817689645993,
27.6302393940932));
#35838=CARTESIAN_POINT('Ctrl Pts',(-9.38264738479791,-31.66694122299,27.6350465691787));
#35839=CARTESIAN_POINT('Ctrl Pts',(-9.4842592359165,-31.6481205701842,27.641148251798));
#35840=CARTESIAN_POINT('Ctrl Pts',(-9.58690422524929,-31.6339189683107,
27.6472499344173));
#35841=CARTESIAN_POINT('Ctrl Pts',(-9.69012621650684,-31.6244432606156,
27.6533516170366));
#35842=CARTESIAN_POINT('Ctrl Pts',(-9.7932124376878,-31.61498001652,27.6594452739833));
#35843=CARTESIAN_POINT('Ctrl Pts',(-9.89687372961916,-31.6102303475855,
27.6655389309299));
#35844=CARTESIAN_POINT('Ctrl Pts',(-10.0006439622708,-31.6102500611678,
27.6716325878765));
#35845=CARTESIAN_POINT('Ctrl Pts',(-10.1043073945313,-31.610269754461,27.6777199732275));
#35846=CARTESIAN_POINT('Ctrl Pts',(-10.208079119075,-31.6150490693068,27.6838073585784));
#35847=CARTESIAN_POINT('Ctrl Pts',(-10.3114889564063,-31.6245919220727,
27.6898947439293));
#35848=CARTESIAN_POINT('Ctrl Pts',(-10.4148252337353,-31.6341279865843,
27.6959777990532));
#35849=CARTESIAN_POINT('Ctrl Pts',(-10.5177997110688,-31.6484208114754,
27.702060854177));
#35850=CARTESIAN_POINT('Ctrl Pts',(-10.6199441184374,-31.6674222660957,
27.7081439093008));
#35851=CARTESIAN_POINT('Ctrl Pts',(-10.7220507093345,-31.6864166858916,
27.7142247123221));
#35852=CARTESIAN_POINT('Ctrl Pts',(-10.8233274209573,-31.7101161926559,
27.7203055153434));
#35853=CARTESIAN_POINT('Ctrl Pts',(-10.9233137983367,-31.7384211350481,
27.7263863183646));
#35854=CARTESIAN_POINT('Ctrl Pts',(-11.0232890616861,-31.7667229311919,
27.7324664454716));
#35855=CARTESIAN_POINT('Ctrl Pts',(-11.1219738644293,-31.7996290285011,
27.7385465725785));
#35856=CARTESIAN_POINT('Ctrl Pts',(-11.2189214842533,-31.8369894913665,
27.7446266996854));
#35857=CARTESIAN_POINT('Ctrl Pts',(-11.3158834437109,-31.8743554802609,
27.7507077261109));
#35858=CARTESIAN_POINT('Ctrl Pts',(-11.4111073105846,-31.9161769898498,
27.7567887525364));
#35859=CARTESIAN_POINT('Ctrl Pts',(-11.5041658239971,-31.9622557322218,
27.7628697789619));
#35860=CARTESIAN_POINT('Ctrl Pts',(-11.597320924078,-32.0083823003332,27.7689571169656));
#35861=CARTESIAN_POINT('Ctrl Pts',(-11.6883057982808,-32.0587747354434,
27.7750444549693));
#35862=CARTESIAN_POINT('Ctrl Pts',(-11.7767173518078,-32.1131885211734,
27.781131792973));
#35863=CARTESIAN_POINT('Ctrl Pts',(-11.8651764047115,-32.1676315408756,
27.7872224014176));
#35864=CARTESIAN_POINT('Ctrl Pts',(-11.9510590294139,-32.2260999739477,
27.7933130098621));
#35865=CARTESIAN_POINT('Ctrl Pts',(-12.0339923783905,-32.2883067896332,
27.7994036183067));
#35866=CARTESIAN_POINT('Ctrl Pts',(-12.1170611141713,-32.3506151565291,
27.8055041695309));
#35867=CARTESIAN_POINT('Ctrl Pts',(-12.1971706257857,-32.4166738253225,
27.8116047207551));
#35868=CARTESIAN_POINT('Ctrl Pts',(-12.273982147142,-32.48615627833,27.8177052719793));
#35869=CARTESIAN_POINT('Ctrl Pts',(-12.3345056248876,-32.5409048319852,
27.8225121885686));
#35870=CARTESIAN_POINT('Ctrl Pts',(-12.3929821732118,-32.5977782733554,
27.8273191051579));
#35871=CARTESIAN_POINT('Ctrl Pts',(-12.4492635157942,-32.6566021906857,
27.8321260217471));
#35872=CARTESIAN_POINT('Ctrl Pts',(-12.5197884220859,-32.7303131411903,
27.8381494626683));
#35873=CARTESIAN_POINT('Ctrl Pts',(-12.5871173119216,-32.8073514381577,
27.8441729035895));
#35874=CARTESIAN_POINT('Ctrl Pts',(-12.6509144243622,-32.887404966112,27.8501963445107));
#35875=CARTESIAN_POINT('Ctrl Pts',(-12.7146125210988,-32.9673342477465,
27.8562104368074));
#35876=CARTESIAN_POINT('Ctrl Pts',(-12.7747894695597,-33.0502691130629,
27.8622245291042));
#35877=CARTESIAN_POINT('Ctrl Pts',(-12.8311464980834,-33.1358609040927,
27.8682386214009));
#35878=CARTESIAN_POINT('Ctrl Pts',(-12.8874529871053,-33.221375938654,27.8742473204178));
#35879=CARTESIAN_POINT('Ctrl Pts',(-12.9399461180647,-33.309542802434,27.8802560194346));
#35880=CARTESIAN_POINT('Ctrl Pts',(-12.9883679065639,-33.3999805258939,
27.8862647184515));
#35881=CARTESIAN_POINT('Ctrl Pts',(-13.0367575515633,-33.4903582147073,
27.8922694287554));
#35882=CARTESIAN_POINT('Ctrl Pts',(-13.0810810178945,-33.5830033808398,
27.8982741390593));
#35883=CARTESIAN_POINT('Ctrl Pts',(-13.1211247321806,-33.6775078568586,
27.9042788493632));
#35884=CARTESIAN_POINT('Ctrl Pts',(-13.1414419793625,-33.7254572250255,
27.9073254993974));
#35885=CARTESIAN_POINT('Ctrl Pts',(-13.1606582077987,-33.7738848260026,
27.9103721494316));
#35886=CARTESIAN_POINT('Ctrl Pts',(-13.1787501240207,-33.8227350716434,
27.9134187994658));
#35887=CARTESIAN_POINT('Origin',(-10.,-35.,23.));
#35888=CARTESIAN_POINT('',(-13.1787501097524,-33.8227350331175,29.1634929519179));
#35889=CARTESIAN_POINT('',(-13.1787501240208,-33.8227350716437,28.823527842849));
#35890=CARTESIAN_POINT('',(-13.1787501240207,-33.8227350716434,23.));
#35891=CARTESIAN_POINT('',(-7.42676557298528,-32.7934484719078,30.));
#35892=CARTESIAN_POINT('Ctrl Pts',(-7.42676557298526,-32.7934484719078,
30.));
#35893=CARTESIAN_POINT('Ctrl Pts',(-7.42045295623278,-32.8008101140653,
29.9994308516325));
#35894=CARTESIAN_POINT('Ctrl Pts',(-7.41417188875379,-32.8081988938986,
29.9988635376667));
#35895=CARTESIAN_POINT('Ctrl Pts',(-7.40029705405223,-32.82466331742,29.9976078642351));
#35896=CARTESIAN_POINT('Ctrl Pts',(-7.3927189018354,-32.8337520059171,29.9969203688605));
#35897=CARTESIAN_POINT('Ctrl Pts',(-7.36365296757774,-32.8689850725241,
29.9942762747548));
#35898=CARTESIAN_POINT('Ctrl Pts',(-7.34250898726559,-32.8954116895691,
29.9923374526965));
#35899=CARTESIAN_POINT('Ctrl Pts',(-7.23066464143884,-33.0395730979113,
29.981973894332));
#35900=CARTESIAN_POINT('Ctrl Pts',(-7.14737974006372,-33.1628674953582,
29.97386011666));
#35901=CARTESIAN_POINT('Ctrl Pts',(-6.99559951859121,-33.4229059648852,
29.9574884969299));
#35902=CARTESIAN_POINT('Ctrl Pts',(-6.92771857518107,-33.559606692338,29.9492480664531));
#35903=CARTESIAN_POINT('Ctrl Pts',(-6.8342281892156,-33.784825790337,29.9357546417517));
#35904=CARTESIAN_POINT('Ctrl Pts',(-6.8026160581166,-33.8706223604427,29.9306341923334));
#35905=CARTESIAN_POINT('Ctrl Pts',(-6.76258063009137,-33.9945021639557,
29.923203264082));
#35906=CARTESIAN_POINT('Ctrl Pts',(-6.7512855014978,-34.0316178299341,29.920972378891));
#35907=CARTESIAN_POINT('Ctrl Pts',(-6.73249217375053,-34.0974062589309,
29.9170055373366));
#35908=CARTESIAN_POINT('Ctrl Pts',(-6.72472821916191,-34.1259991168292,
29.9152773583261));
#35909=CARTESIAN_POINT('Ctrl Pts',(-6.70914932295406,-34.1864978506844,
29.9116100895573));
#35910=CARTESIAN_POINT('Ctrl Pts',(-6.70142138553885,-34.2184227836219,
29.909668684328));
#35911=CARTESIAN_POINT('Ctrl Pts',(-6.68178351044353,-34.3050348342957,
29.9043821702176));
#35912=CARTESIAN_POINT('Ctrl Pts',(-6.67076241279652,-34.3599110889422,
29.9010116993012));
#35913=CARTESIAN_POINT('Ctrl Pts',(-6.60789009691365,-34.7187757307886,
29.8788139171087));
#35914=CARTESIAN_POINT('Ctrl Pts',(-6.59638019761221,-35.0283172761005,
29.8587607128677));
#35915=CARTESIAN_POINT('Ctrl Pts',(-6.64201860350012,-35.4877615589473,
29.8288687764698));
#35916=CARTESIAN_POINT('Ctrl Pts',(-6.66753844244158,-35.6392650389571,
29.8190273788908));
#35917=CARTESIAN_POINT('Ctrl Pts',(-6.70994576996796,-35.8165654634065,
29.8078585840293));
#35918=CARTESIAN_POINT('Ctrl Pts',(-6.71700888275631,-35.844514913058,29.8061086866409));
#35919=CARTESIAN_POINT('Ctrl Pts',(-6.72873079523429,-35.8885282184635,
29.8033734263145));
#35920=CARTESIAN_POINT('Ctrl Pts',(-6.73315323901014,-35.9046529011187,
29.8023756938387));
#35921=CARTESIAN_POINT('Ctrl Pts',(-6.74175642433794,-35.9351349870315,
29.8004986507799));
#35922=CARTESIAN_POINT('Ctrl Pts',(-6.74591303029129,-35.9494981069945,
29.7996181225295));
#35923=CARTESIAN_POINT('Ctrl Pts',(-6.75628299928376,-35.9844633455038,
29.7974840067185));
#35924=CARTESIAN_POINT('Ctrl Pts',(-6.76259766332361,-36.0050344390657,
29.7962362630186));
#35925=CARTESIAN_POINT('Ctrl Pts',(-6.78590624680633,-36.0784661715619,
29.791805548616));
#35926=CARTESIAN_POINT('Ctrl Pts',(-6.80400329066443,-36.1309702509515,
29.7886809796411));
#35927=CARTESIAN_POINT('Ctrl Pts',(-6.89313402640073,-36.3703041807197,
29.7745352753796));
#35928=CARTESIAN_POINT('Ctrl Pts',(-6.97931842156187,-36.5510789630564,
29.7641071426166));
#35929=CARTESIAN_POINT('Ctrl Pts',(-7.14584504109605,-36.8331685036441,
29.7467579644264));
#35930=CARTESIAN_POINT('Ctrl Pts',(-7.21691002322565,-36.939359338186,29.7399497211604));
#35931=CARTESIAN_POINT('Ctrl Pts',(-7.3439289923636,-37.1077532575538,29.7283971177205));
#35932=CARTESIAN_POINT('Ctrl Pts',(-7.39649518087785,-37.1723485236772,
29.7237639846271));
#35933=CARTESIAN_POINT('Ctrl Pts',(-7.47416806215517,-37.2609228966324,
29.7170722531329));
#35934=CARTESIAN_POINT('Ctrl Pts',(-7.4973483452594,-37.2865550262831,29.715093352464));
#35935=CARTESIAN_POINT('Ctrl Pts',(-7.53836442036808,-37.3305385401572,
29.7116200047846));
#35936=CARTESIAN_POINT('Ctrl Pts',(-7.55602387716367,-37.3490509296667,
29.710133298304));
#35937=CARTESIAN_POINT('Ctrl Pts',(-7.59300842837803,-37.3869532810686,
29.7070364537089));
#35938=CARTESIAN_POINT('Ctrl Pts',(-7.61236218715025,-37.4063125311953,
29.7054250756153));
#35939=CARTESIAN_POINT('Ctrl Pts',(-7.66332897322519,-37.4560735083499,
29.7012039386291));
#35940=CARTESIAN_POINT('Ctrl Pts',(-7.6953005197271,-37.4860990702586,29.6985777143103));
#35941=CARTESIAN_POINT('Ctrl Pts',(-7.85830967512745,-37.6333393469694,
29.6852885042185));
#35942=CARTESIAN_POINT('Ctrl Pts',(-7.99772571991931,-37.7408384349338,
29.6742196531397));
#35943=CARTESIAN_POINT('Ctrl Pts',(-8.31020344983826,-37.9451715705292,
29.6501926681347));
#35944=CARTESIAN_POINT('Ctrl Pts',(-8.48471222671159,-38.0386427793486,
29.6372125479186));
#35945=CARTESIAN_POINT('Ctrl Pts',(-8.72023422058169,-38.1394326880846,
29.6208818902536));
#35946=CARTESIAN_POINT('Ctrl Pts',(-8.77469235248713,-38.1610852485021,
29.6171856118582));
#35947=CARTESIAN_POINT('Ctrl Pts',(-8.86803820943254,-38.1954244499402,
29.6110150118393));
#35948=CARTESIAN_POINT('Ctrl Pts',(-8.90664327070889,-38.208838779557,29.6085099334164));
#35949=CARTESIAN_POINT('Ctrl Pts',(-8.96295821420876,-38.2272724531387,
29.6049329637538));
#35950=CARTESIAN_POINT('Ctrl Pts',(-8.98047978690964,-38.2328504022311,
29.6038307732371));
#35951=CARTESIAN_POINT('Ctrl Pts',(-9.01198313323975,-38.2425978107858,
29.601869389844));
#35952=CARTESIAN_POINT('Ctrl Pts',(-9.02594765867314,-38.2468199725771,
29.6010071538164));
#35953=CARTESIAN_POINT('Ctrl Pts',(-9.05729624435203,-38.2560777376331,
29.5990868037388));
#35954=CARTESIAN_POINT('Ctrl Pts',(-9.07469450810737,-38.2610646088578,
29.598031466103));
#35955=CARTESIAN_POINT('Ctrl Pts',(-9.12576449401288,-38.2752611917336,
29.5949619708963));
#35956=CARTESIAN_POINT('Ctrl Pts',(-9.15954047621683,-38.2840906779917,
29.5929677561252));
#35957=CARTESIAN_POINT('Ctrl Pts',(-9.33012177461731,-38.3258786672071,
29.583048483904));
#35958=CARTESIAN_POINT('Ctrl Pts',(-9.46876093541178,-38.3508205140381,
29.5754730698707));
#35959=CARTESIAN_POINT('Ctrl Pts',(-9.85799846387174,-38.3960713984852,
29.5546071660816));
#35960=CARTESIAN_POINT('Ctrl Pts',(-10.1098689701902,-38.3972618388653,
29.5415030110932));
#35961=CARTESIAN_POINT('Ctrl Pts',(-10.4241018902344,-38.3637413616659,
29.5239587946753));
#35962=CARTESIAN_POINT('Ctrl Pts',(-10.4884313808481,-38.3550040832986,
29.5203077919428));
#35963=CARTESIAN_POINT('Ctrl Pts',(-10.5847276879626,-38.3390968386799,
29.5147335958256));
#35964=CARTESIAN_POINT('Ctrl Pts',(-10.6169080298704,-38.333301448101,29.5128524144307));
#35965=CARTESIAN_POINT('Ctrl Pts',(-10.6727136531311,-38.3224155671968,
29.5095560193829));
#35966=CARTESIAN_POINT('Ctrl Pts',(-10.6963779766777,-38.3175362137878,
29.5081474412235));
#35967=CARTESIAN_POINT('Ctrl Pts',(-10.7497802973275,-38.3059286295644,
29.5049435614938));
#35968=CARTESIAN_POINT('Ctrl Pts',(-10.7794834432576,-38.2990513894333,
29.5031437292096));
#35969=CARTESIAN_POINT('Ctrl Pts',(-10.8597870652118,-38.2793134692414,
29.4982279594976));
#35970=CARTESIAN_POINT('Ctrl Pts',(-10.9101881843626,-38.2656833361335,
29.4950884796461));
#35971=CARTESIAN_POINT('Ctrl Pts',(-11.166831840013,-38.1898756936946,29.4788171915766));
#35972=CARTESIAN_POINT('Ctrl Pts',(-11.3670978527846,-38.1093123705836,
29.4651224033587));
#35973=CARTESIAN_POINT('Ctrl Pts',(-11.6765486482266,-37.9491197511119,
29.4427547224856));
#35974=CARTESIAN_POINT('Ctrl Pts',(-11.7910535477669,-37.8810158421817,
29.4341920092372));
#35975=CARTESIAN_POINT('Ctrl Pts',(-11.9597415219069,-37.7667323860013,
29.4213816558017));
#35976=CARTESIAN_POINT('Ctrl Pts',(-12.0169744152259,-37.7252908972784,
29.4169991055172));
#35977=CARTESIAN_POINT('Ctrl Pts',(-12.0915250879281,-37.6676738027531,
29.41128335649));
#35978=CARTESIAN_POINT('Ctrl Pts',(-12.1100259357576,-37.6530645163738,
29.4098643319993));
#35979=CARTESIAN_POINT('Ctrl Pts',(-12.1406371129868,-37.628369474216,29.4075175666014));
#35980=CARTESIAN_POINT('Ctrl Pts',(-12.1528319999229,-37.6183902973371,
29.4065829678717));
#35981=CARTESIAN_POINT('Ctrl Pts',(-12.1777684613347,-37.5976925902304,
29.4046732883358));
#35982=CARTESIAN_POINT('Ctrl Pts',(-12.1905015132489,-37.5869645166162,
29.4036989108514));
#35983=CARTESIAN_POINT('Ctrl Pts',(-12.2247779792527,-37.5576507778983,
29.4010763884273));
#35984=CARTESIAN_POINT('Ctrl Pts',(-12.2461677389903,-37.5388865981802,
29.3994403068191));
#35985=CARTESIAN_POINT('Ctrl Pts',(-12.3796144082921,-37.4188137116368,
29.3892176200321));
#35986=CARTESIAN_POINT('Ctrl Pts',(-12.485041879298,-37.3103681156634,29.3810672753795));
#35987=CARTESIAN_POINT('Ctrl Pts',(-12.7062679107487,-37.050076439927,29.3628493400805));
#35988=CARTESIAN_POINT('Ctrl Pts',(-12.8171840470334,-36.8947748789666,
29.3528560813828));
#35989=CARTESIAN_POINT('Ctrl Pts',(-12.9511049416009,-36.6692910333153,
29.3385984195455));
#35990=CARTESIAN_POINT('Ctrl Pts',(-12.985773997062,-36.6064575111552,29.3346527340544));
#35991=CARTESIAN_POINT('Ctrl Pts',(-13.0439797208477,-36.4925638035981,
29.3275075439075));
#35992=CARTESIAN_POINT('Ctrl Pts',(-13.068289527896,-36.4419286125954,29.3243333587413));
#35993=CARTESIAN_POINT('Ctrl Pts',(-13.1039883720903,-36.3625759767692,
29.3193500754838));
#35994=CARTESIAN_POINT('Ctrl Pts',(-13.1162622550995,-36.3342663054993,
29.3175705856089));
#35995=CARTESIAN_POINT('Ctrl Pts',(-13.1383795284386,-36.2812823627509,
29.314235155466));
#35996=CARTESIAN_POINT('Ctrl Pts',(-13.1483226999809,-36.2566521695357,
29.3126826805156));
#35997=CARTESIAN_POINT('Ctrl Pts',(-13.1699193630262,-36.2012894991984,
29.3091876036033));
#35998=CARTESIAN_POINT('Ctrl Pts',(-13.1814172712542,-36.1704995777464,
29.3072400680654));
#35999=CARTESIAN_POINT('Ctrl Pts',(-13.2148807886321,-36.0767509084875,
29.301296931113));
#36000=CARTESIAN_POINT('Ctrl Pts',(-13.2354371883807,-36.0133095651879,
29.2972567709006));
#36001=CARTESIAN_POINT('Ctrl Pts',(-13.3389873981864,-35.6583518947158,
29.2745426702211));
#36002=CARTESIAN_POINT('Ctrl Pts',(-13.3844514449687,-35.3573497967771,
29.2547082041147));
#36003=CARTESIAN_POINT('Ctrl Pts',(-13.3904139851082,-34.9858265034264,
29.2310162355354));
#36004=CARTESIAN_POINT('Ctrl Pts',(-13.3894334515727,-34.9172370072722,
29.2266834672566));
#36005=CARTESIAN_POINT('Ctrl Pts',(-13.384313564574,-34.802628385905,29.2195581642237));
#36006=CARTESIAN_POINT('Ctrl Pts',(-13.3813134937036,-34.7565798745864,
29.2167263888309));
#36007=CARTESIAN_POINT('Ctrl Pts',(-13.3756699803911,-34.6907175259261,
29.2127338454318));
#36008=CARTESIAN_POINT('Ctrl Pts',(-13.3737902532577,-34.6708452720184,
29.211536753869));
#36009=CARTESIAN_POINT('Ctrl Pts',(-13.3701959708319,-34.636121404494,29.209459579159));
#36010=CARTESIAN_POINT('Ctrl Pts',(-13.3685585365772,-34.6212627164359,
29.2085754659808));
#36011=CARTESIAN_POINT('Ctrl Pts',(-13.3647497753424,-34.5886816769454,
29.2066475378164));
#36012=CARTESIAN_POINT('Ctrl Pts',(-13.362536670606,-34.5709650557845,29.2056059802193));
#36013=CARTESIAN_POINT('Ctrl Pts',(-13.3555736289156,-34.5185913490761,
29.2025448884499));
#36014=CARTESIAN_POINT('Ctrl Pts',(-13.3504269693134,-34.4839883793366,
29.2005457490284));
#36015=CARTESIAN_POINT('Ctrl Pts',(-13.3143128154574,-34.2645768592071,
29.1879830638303));
#36016=CARTESIAN_POINT('Ctrl Pts',(-13.268598232159,-34.0825049102161,29.1780597520728));
#36017=CARTESIAN_POINT('Ctrl Pts',(-13.1986445260763,-33.8775346613848,
29.166582597997));
#36018=CARTESIAN_POINT('Ctrl Pts',(-13.1888728361093,-33.8500675524935,
29.1650383635687));
#36019=CARTESIAN_POINT('Ctrl Pts',(-13.1787501097524,-33.8227350331175,
29.1634929519179));
#36020=CARTESIAN_POINT('',(-12.5373010662035,-32.7522214606544,30.));
#36021=CARTESIAN_POINT('Origin',(-10.,-35.,30.));
#36022=CARTESIAN_POINT('Ctrl Pts',(-12.5373010662035,-32.7522214606544,
30.));
#36023=CARTESIAN_POINT('Ctrl Pts',(-12.5306561517406,-32.7447206556345,
29.9993854250735));
#36024=CARTESIAN_POINT('Ctrl Pts',(-12.5239780167117,-32.7372493619221,
29.9987689954815));
#36025=CARTESIAN_POINT('Ctrl Pts',(-12.3346109279579,-32.5272726485279,
29.9813261713196));
#36026=CARTESIAN_POINT('Ctrl Pts',(-12.1281855390359,-32.3475265511935,
29.9633698274277));
#36027=CARTESIAN_POINT('Ctrl Pts',(-11.8172905516303,-32.1367067220662,
29.9394502167781));
#36028=CARTESIAN_POINT('Ctrl Pts',(-11.7295349331529,-32.0828601282193,
29.9329812956598));
#36029=CARTESIAN_POINT('Ctrl Pts',(-11.5754986281841,-31.9977426364613,
29.9221327305273));
#36030=CARTESIAN_POINT('Ctrl Pts',(-11.5104084178899,-31.9644748681779,
29.9176933147489));
#36031=CARTESIAN_POINT('Ctrl Pts',(-11.4133909228341,-31.9187830869011,
29.9112827185171));
#36032=CARTESIAN_POINT('Ctrl Pts',(-11.3822731483448,-31.9046982963963,
29.9092566876991));
#36033=CARTESIAN_POINT('Ctrl Pts',(-11.3263160351192,-31.8803827036066,
29.9056655026499));
#36034=CARTESIAN_POINT('Ctrl Pts',(-11.3015582984652,-31.8699724669921,
29.9040945175085));
#36035=CARTESIAN_POINT('Ctrl Pts',(-11.2485040519356,-31.8484023520084,
29.9007648567265));
#36036=CARTESIAN_POINT('Ctrl Pts',(-11.2201756644919,-31.8373268370343,
29.8990090431216));
#36037=CARTESIAN_POINT('Ctrl Pts',(-11.1431474279658,-31.808400249115,29.8942914827256));
#36038=CARTESIAN_POINT('Ctrl Pts',(-11.0941797798121,-31.791282808994,29.8913532204723));
#36039=CARTESIAN_POINT('Ctrl Pts',(-10.8312114803665,-31.7060784396256,
29.8758609008324));
#36040=CARTESIAN_POINT('Ctrl Pts',(-10.611235019576,-31.6582588968864,29.8639495621657));
#36041=CARTESIAN_POINT('Ctrl Pts',(-10.2620345608516,-31.6180102868005,
29.8452229819141));
#36042=CARTESIAN_POINT('Ctrl Pts',(-10.135228081649,-31.6105713624658,29.8384474161599));
#36043=CARTESIAN_POINT('Ctrl Pts',(-9.93956104973214,-31.6100916280698,
29.8276695400054));
#36044=CARTESIAN_POINT('Ctrl Pts',(-9.8708263071449,-31.6120146741786,29.8238212778998));
#36045=CARTESIAN_POINT('Ctrl Pts',(-9.77888496054104,-31.6173887666256,
29.8185357394441));
#36046=CARTESIAN_POINT('Ctrl Pts',(-9.75558304095288,-31.618992620027,29.8171842305274));
#36047=CARTESIAN_POINT('Ctrl Pts',(-9.71663497216785,-31.6220781145327,
29.814902557778));
#36048=CARTESIAN_POINT('Ctrl Pts',(-9.70097876753382,-31.623428026694,29.8139792321263));
#36049=CARTESIAN_POINT('Ctrl Pts',(-9.66868136025601,-31.6264391660914,
29.8120607777874));
#36050=CARTESIAN_POINT('Ctrl Pts',(-9.65204207586059,-31.6281147708921,
29.8110649239935));
#36051=CARTESIAN_POINT('Ctrl Pts',(-9.60678639400856,-31.6330106348878,
29.8083372352713));
#36052=CARTESIAN_POINT('Ctrl Pts',(-9.57819816527388,-31.6364724739644,
29.8065932601901));
#36053=CARTESIAN_POINT('Ctrl Pts',(-9.38983715711678,-31.6617207750094,
29.7949795702531));
#36054=CARTESIAN_POINT('Ctrl Pts',(-9.23176180625438,-31.6945185390058,
29.7846569208221));
#36055=CARTESIAN_POINT('Ctrl Pts',(-8.9521123635773,-31.7736885440693,29.7659520500969));
#36056=CARTESIAN_POINT('Ctrl Pts',(-8.82970498088461,-31.8160455659469,
29.7576020183712));
#36057=CARTESIAN_POINT('Ctrl Pts',(-8.57359015920598,-31.9214412213651,
29.7400043071661));
#36058=CARTESIAN_POINT('Ctrl Pts',(-8.44096175182365,-31.9864343477039,
29.7308156751714));
#36059=CARTESIAN_POINT('Ctrl Pts',(-8.27603078891577,-32.0810704645365,
29.7193422150339));
#36060=CARTESIAN_POINT('Ctrl Pts',(-8.23948655403542,-32.1029649421173,
29.7167960502857));
#36061=CARTESIAN_POINT('Ctrl Pts',(-8.17954572580588,-32.1404300672805,
29.7126114739265));
#36062=CARTESIAN_POINT('Ctrl Pts',(-8.15591347260316,-32.1556127347825,
29.7109594486569));
#36063=CARTESIAN_POINT('Ctrl Pts',(-8.10986093556611,-32.1860146662392,
29.7077347563357));
#36064=CARTESIAN_POINT('Ctrl Pts',(-8.08742907389436,-32.2012124667646,
29.706161469149));
#36065=CARTESIAN_POINT('Ctrl Pts',(-8.03833119757791,-32.235342719613,29.7027109130018));
#36066=CARTESIAN_POINT('Ctrl Pts',(-8.0117519070617,-32.2543955138952,29.7008382837032));
#36067=CARTESIAN_POINT('Ctrl Pts',(-7.92028176962833,-32.3219888878312,
29.6943728225227));
#36068=CARTESIAN_POINT('Ctrl Pts',(-7.85685658006084,-32.3724709153663,
29.689853022791));
#36069=CARTESIAN_POINT('Ctrl Pts',(-7.58150804141698,-32.6082394598178,
29.6699370741624));
#36070=CARTESIAN_POINT('Ctrl Pts',(-7.39136364075251,-32.8171970863654,
29.6554659459212));
#36071=CARTESIAN_POINT('Ctrl Pts',(-7.19054858480866,-33.1021334788801,
29.6365956262216));
#36072=CARTESIAN_POINT('Ctrl Pts',(-7.15350484188685,-33.1581588026217,
29.6329157366886));
#36073=CARTESIAN_POINT('Ctrl Pts',(-7.09421495757469,-33.2538942970608,
29.6266153441988));
#36074=CARTESIAN_POINT('Ctrl Pts',(-7.07105974920675,-33.2930200837212,
29.6240371239073));
#36075=CARTESIAN_POINT('Ctrl Pts',(-7.03893671154437,-33.3498778285416,
29.6202686032285));
#36076=CARTESIAN_POINT('Ctrl Pts',(-7.02932611122453,-33.3672429500064,
29.6191147785978));
#36077=CARTESIAN_POINT('Ctrl Pts',(-7.01275010019831,-33.3978245215162,
29.6170760364678));
#36078=CARTESIAN_POINT('Ctrl Pts',(-7.0057186838236,-33.4110042106843,29.6161951738241));
#36079=CARTESIAN_POINT('Ctrl Pts',(-6.9904364187531,-33.4401109573056,29.6142444460281));
#36080=CARTESIAN_POINT('Ctrl Pts',(-6.98222485247605,-33.4560570275034,
29.6131723923681));
#36081=CARTESIAN_POINT('Ctrl Pts',(-6.95867039359623,-33.5027033727614,
29.6100282889433));
#36082=CARTESIAN_POINT('Ctrl Pts',(-6.94366716234826,-33.533571565035,29.6079375869728));
#36083=CARTESIAN_POINT('Ctrl Pts',(-6.82431268162507,-33.7889268329935,
29.5905918399206));
#36084=CARTESIAN_POINT('Ctrl Pts',(-6.74437654767733,-34.0239894615909,
29.5743687130192));
#36085=CARTESIAN_POINT('Ctrl Pts',(-6.66495266076797,-34.3819025280143,
29.5508843058554));
#36086=CARTESIAN_POINT('Ctrl Pts',(-6.64529730870072,-34.499441216909,29.5433454835769));
#36087=CARTESIAN_POINT('Ctrl Pts',(-6.62281878658863,-34.6975219916843,
29.5310018882551));
#36088=CARTESIAN_POINT('Ctrl Pts',(-6.616603708912,-34.7775656458223,29.5261100967243));
#36089=CARTESIAN_POINT('Ctrl Pts',(-6.61176946195864,-34.8926699005481,
29.5192124964783));
#36090=CARTESIAN_POINT('Ctrl Pts',(-6.61084309435512,-34.9276015467316,
29.5171371173606));
#36091=CARTESIAN_POINT('Ctrl Pts',(-6.6101640395619,-34.9890491212673,29.5135165502415));
#36092=CARTESIAN_POINT('Ctrl Pts',(-6.61018204956866,-35.0155590176464,
29.5119644235955));
#36093=CARTESIAN_POINT('Ctrl Pts',(-6.61087126471377,-35.0710921438624,
29.508732709748));
#36094=CARTESIAN_POINT('Ctrl Pts',(-6.6116043275727,-35.1001125400493,29.507055160839));
#36095=CARTESIAN_POINT('Ctrl Pts',(-6.6145465589619,-35.1772976644314,29.5026212854126));
#36096=CARTESIAN_POINT('Ctrl Pts',(-6.61741069967402,-35.2254316209416,
29.4998852315949));
#36097=CARTESIAN_POINT('Ctrl Pts',(-6.64345057301039,-35.5471287286141,
29.4817611065749));
#36098=CARTESIAN_POINT('Ctrl Pts',(-6.69875750342126,-35.817056970931,29.4674454397777));
#36099=CARTESIAN_POINT('Ctrl Pts',(-6.83574493718743,-36.2257129992017,
29.4445267462644));
#36100=CARTESIAN_POINT('Ctrl Pts',(-6.89567578940038,-36.3704171157163,
29.4361163223826));
#36101=CARTESIAN_POINT('Ctrl Pts',(-6.97796816957431,-36.5357497886958,
29.4256026530395));
#36102=CARTESIAN_POINT('Ctrl Pts',(-6.99087696428638,-36.5608914895648,
29.4239778696222));
#36103=CARTESIAN_POINT('Ctrl Pts',(-7.01179025491488,-36.6003992970988,
29.4213787117641));
#36104=CARTESIAN_POINT('Ctrl Pts',(-7.01958780436487,-36.6148741468381,
29.4204165322531));
#36105=CARTESIAN_POINT('Ctrl Pts',(-7.03477106425126,-36.6425747719546,
29.418555006081));
#36106=CARTESIAN_POINT('Ctrl Pts',(-7.04214065894238,-36.655808748256,29.4176566397267));
#36107=CARTESIAN_POINT('Ctrl Pts',(-7.05888871716779,-36.685415530278,29.4156272194948));
#36108=CARTESIAN_POINT('Ctrl Pts',(-7.06831569410279,-36.701760318824,29.4144932598419));
#36109=CARTESIAN_POINT('Ctrl Pts',(-7.10225250751533,-36.7594821142495,
29.4104425147323));
#36110=CARTESIAN_POINT('Ctrl Pts',(-7.12750484700645,-36.8004135484821,
29.4074852082441));
#36111=CARTESIAN_POINT('Ctrl Pts',(-7.26628139098329,-37.01500114668,29.391579572438));
#36112=CARTESIAN_POINT('Ctrl Pts',(-7.39469513943745,-37.1784920962804,
29.3780656527411));
#36113=CARTESIAN_POINT('Ctrl Pts',(-7.62700505106574,-37.4241215347924,
29.356354825326));
#36114=CARTESIAN_POINT('Ctrl Pts',(-7.72218525187601,-37.5137691142794,
29.3480524135006));
#36115=CARTESIAN_POINT('Ctrl Pts',(-7.86722720113023,-37.6353596936616,
29.3363048842906));
#36116=CARTESIAN_POINT('Ctrl Pts',(-7.91311554080379,-37.6718447534405,
29.3327065933551));
#36117=CARTESIAN_POINT('Ctrl Pts',(-7.99843319002137,-37.7361395963207,
29.3262290696783));
#36118=CARTESIAN_POINT('Ctrl Pts',(-8.03755337391213,-37.7643323213405,
29.3233362606002));
#36119=CARTESIAN_POINT('Ctrl Pts',(-8.10129185662458,-37.8082314194474,
29.3187431584008));
#36120=CARTESIAN_POINT('Ctrl Pts',(-8.12553365844463,-37.8244702747154,
29.317023225757));
#36121=CARTESIAN_POINT('Ctrl Pts',(-8.17239670399396,-37.854993304413,29.3137485609934));
#36122=CARTESIAN_POINT('Ctrl Pts',(-8.19498319840252,-37.869326572894,29.3121921099086));
#36123=CARTESIAN_POINT('Ctrl Pts',(-8.24735732118121,-37.9016997150768,
29.3086315624225));
#36124=CARTESIAN_POINT('Ctrl Pts',(-8.27725825818875,-37.919551098129,29.3066343289466));
#36125=CARTESIAN_POINT('Ctrl Pts',(-8.37461928773071,-37.9756606656903,
29.3002395545177));
#36126=CARTESIAN_POINT('Ctrl Pts',(-8.44312077263089,-38.012066923236,29.295906109762));
#36127=CARTESIAN_POINT('Ctrl Pts',(-8.76828574431323,-38.1708212911649,
29.2759813179573));
#36128=CARTESIAN_POINT('Ctrl Pts',(-9.03841289963471,-38.262907974306,29.2613611154626));
#36129=CARTESIAN_POINT('Ctrl Pts',(-9.3826466085178,-38.3337353546587,29.2423341723327));
#36130=CARTESIAN_POINT('Ctrl Pts',(-9.44882123344469,-38.3453127941734,
29.2386533982827));
#36131=CARTESIAN_POINT('Ctrl Pts',(-9.56027391939214,-38.3614151181076,
29.2323531698479));
#36132=CARTESIAN_POINT('Ctrl Pts',(-9.60537925505668,-38.3670082684365,
29.2297759291608));
#36133=CARTESIAN_POINT('Ctrl Pts',(-9.6703289220231,-38.3737392027223,29.2260082337158));
#36134=CARTESIAN_POINT('Ctrl Pts',(-9.69009383672856,-38.3756121454315,
29.224854178764));
#36135=CARTESIAN_POINT('Ctrl Pts',(-9.72479870431629,-38.3785934519707,
29.222812880647));
#36136=CARTESIAN_POINT('Ctrl Pts',(-9.73973133779197,-38.3797765723892,
29.2219296579063));
#36137=CARTESIAN_POINT('Ctrl Pts',(-9.77269636957026,-38.3821686411594,
29.2199686438619));
#36138=CARTESIAN_POINT('Ctrl Pts',(-9.79073065098603,-38.3833323757695,
29.2188885870589));
#36139=CARTESIAN_POINT('Ctrl Pts',(-9.84339772183443,-38.3863082395444,
29.2157149675137));
#36140=CARTESIAN_POINT('Ctrl Pts',(-9.87804909260263,-38.3877330979374,
29.2136024398239));
#36141=CARTESIAN_POINT('Ctrl Pts',(-10.0992375914457,-38.3934305388155,
29.1999866938263));
#36142=CARTESIAN_POINT('Ctrl Pts',(-10.2858252244566,-38.3828261856222,
29.1879253988217));
#36143=CARTESIAN_POINT('Ctrl Pts',(-10.6270387969918,-38.3349945614687,
29.1657228109617));
#36144=CARTESIAN_POINT('Ctrl Pts',(-10.7817871966751,-38.3021481822025,
29.1555946626709));
#36145=CARTESIAN_POINT('Ctrl Pts',(-11.0257350640444,-38.2322500743586,
29.1397643006186));
#36146=CARTESIAN_POINT('Ctrl Pts',(-11.116627494615,-38.201986675398,29.1338946232812));
#36147=CARTESIAN_POINT('Ctrl Pts',(-11.2410006421076,-38.1546339265408,
29.125906158457));
#36148=CARTESIAN_POINT('Ctrl Pts',(-11.2756571009011,-38.140779669454,29.123684743495));
#36149=CARTESIAN_POINT('Ctrl Pts',(-11.33498627107,-38.1159181695847,29.1198883687044));
#36150=CARTESIAN_POINT('Ctrl Pts',(-11.3597686611631,-38.1051833495652,
29.1183045664951));
#36151=CARTESIAN_POINT('Ctrl Pts',(-11.4072312223114,-38.0839471196215,
29.1152742210495));
#36152=CARTESIAN_POINT('Ctrl Pts',(-11.4299286493282,-38.0734888410702,
29.1138263560431));
#36153=CARTESIAN_POINT('Ctrl Pts',(-11.4899341140477,-38.0450315386373,
29.110000783983));
#36154=CARTESIAN_POINT('Ctrl Pts',(-11.5270320409718,-38.0265977750521,
29.1076379452056));
#36155=CARTESIAN_POINT('Ctrl Pts',(-11.6739241603084,-37.9502192381555,
29.0982798932008));
#36156=CARTESIAN_POINT('Ctrl Pts',(-11.7808411519285,-37.8869403609809,
29.0914679645895));
#36157=CARTESIAN_POINT('Ctrl Pts',(-12.076976694583,-37.6889458770903,29.0722603903397));
#36158=CARTESIAN_POINT('Ctrl Pts',(-12.2561325260305,-37.5404959509894,
29.0602416907974));
#36159=CARTESIAN_POINT('Ctrl Pts',(-12.4836279800624,-37.3088053002554,
29.0426171665116));
#36160=CARTESIAN_POINT('Ctrl Pts',(-12.5458000791666,-37.2400645155497,
29.0374974802518));
#36161=CARTESIAN_POINT('Ctrl Pts',(-12.6212907351034,-37.1493911611895,
29.0307518206718));
#36162=CARTESIAN_POINT('Ctrl Pts',(-12.6372884116417,-37.1297317281637,
29.0292896486945));
#36163=CARTESIAN_POINT('Ctrl Pts',(-12.6629509068905,-37.0974627194914,
29.0268868801914));
#36164=CARTESIAN_POINT('Ctrl Pts',(-12.6727504658101,-37.0849609869787,
29.0259553337933));
#36165=CARTESIAN_POINT('Ctrl Pts',(-12.6909740369686,-37.0613727613137,
29.0241954972243));
#36166=CARTESIAN_POINT('Ctrl Pts',(-12.6994183450146,-37.0503022973416,
29.0233686649165));
#36167=CARTESIAN_POINT('Ctrl Pts',(-12.7217977374099,-37.0205850707344,
29.0211474484368));
#36168=CARTESIAN_POINT('Ctrl Pts',(-12.735609106206,-37.0018465734701,29.0197450777153));
#36169=CARTESIAN_POINT('Ctrl Pts',(-12.7872933816789,-36.9301904704465,
29.014380406756));
#36170=CARTESIAN_POINT('Ctrl Pts',(-12.8238307315121,-36.8763311371606,
29.0103442239218));
#36171=CARTESIAN_POINT('Ctrl Pts',(-12.9626713459625,-36.6584196172848,
28.9940987623408));
#36172=CARTESIAN_POINT('Ctrl Pts',(-13.0524094633405,-36.4867989293626,
28.9815119135545));
#36173=CARTESIAN_POINT('Ctrl Pts',(-13.1994769537249,-36.135331530575,28.9570738544806));
#36174=CARTESIAN_POINT('Ctrl Pts',(-13.2574284162014,-35.956456140612,28.9452554138676));
#36175=CARTESIAN_POINT('Ctrl Pts',(-13.3104556802108,-35.7302583670716,
28.9312104571741));
#36176=CARTESIAN_POINT('Ctrl Pts',(-13.3197773129748,-35.6866388934361,
28.9285407428772));
#36177=CARTESIAN_POINT('Ctrl Pts',(-13.3336179253263,-35.6149813238029,
28.9242162089102));
#36178=CARTESIAN_POINT('Ctrl Pts',(-13.3386500333267,-35.5870490004382,
28.9225455652366));
#36179=CARTESIAN_POINT('Ctrl Pts',(-13.3477776448171,-35.5324630223267,
28.9193090872333));
#36180=CARTESIAN_POINT('Ctrl Pts',(-13.351907065774,-35.5058172726549,28.9177423065832));
#36181=CARTESIAN_POINT('Ctrl Pts',(-13.360976406036,-35.4422969357932,28.9140369723842));
#36182=CARTESIAN_POINT('Ctrl Pts',(-13.3656281265312,-35.4053843239786,
28.9119074725128));
#36183=CARTESIAN_POINT('Ctrl Pts',(-13.3793607531627,-35.2797756250799,
28.904734764804));
#36184=CARTESIAN_POINT('Ctrl Pts',(-13.3855504025031,-35.1907976947157,
28.8997792954819));
#36185=CARTESIAN_POINT('Ctrl Pts',(-13.3963448169338,-34.8310795359271,
28.8800930409592));
#36186=CARTESIAN_POINT('Ctrl Pts',(-13.3720213298232,-34.5605060481494,
28.8661591960902));
#36187=CARTESIAN_POINT('Ctrl Pts',(-13.3020205114909,-34.2309418720216,
28.8479157967827));
#36188=CARTESIAN_POINT('Ctrl Pts',(-13.2863681330099,-34.166589248693,28.8442860523348));
#36189=CARTESIAN_POINT('Ctrl Pts',(-13.2569378835888,-34.0593708183655,
28.8380644260001));
#36190=CARTESIAN_POINT('Ctrl Pts',(-13.2441722875617,-34.0162452525518,
28.8355136982275));
#36191=CARTESIAN_POINT('Ctrl Pts',(-13.2245785486048,-33.9545874371081,
28.8317803780731));
#36192=CARTESIAN_POINT('Ctrl Pts',(-13.2184400212476,-33.9358392829293,
28.8306335529532));
#36193=CARTESIAN_POINT('Ctrl Pts',(-13.2073681900358,-33.9029962009852,
28.8286022971459));
#36194=CARTESIAN_POINT('Ctrl Pts',(-13.202504854457,-33.8888786357704,28.8277218147451));
#36195=CARTESIAN_POINT('Ctrl Pts',(-13.1915487826005,-33.8577442971194,
28.8257634062535));
#36196=CARTESIAN_POINT('Ctrl Pts',(-13.1854132048364,-33.8407440297242,
28.8246831712498));
#36197=CARTESIAN_POINT('Ctrl Pts',(-13.1790115181001,-33.8234410461142,
28.8235731461798));
#36198=CARTESIAN_POINT('Ctrl Pts',(-13.1788808503858,-33.8230880477997,
28.8235504960504));
#36199=CARTESIAN_POINT('Ctrl Pts',(-13.1787501240208,-33.8227350716437,
28.823527842849));
#36200=CARTESIAN_POINT('Origin',(130.,35.,32.7603849714045));
#36201=CARTESIAN_POINT('',(132.487160689988,38.2405642567579,18.0469660621892));
#36202=CARTESIAN_POINT('',(132.487160689988,38.2405642567579,17.9425407177715));
#36203=CARTESIAN_POINT('',(132.487160689988,38.2405642567579,32.7603849714045));
#36204=CARTESIAN_POINT('',(125.917571176467,34.9941421690681,17.135384982874));
#36205=CARTESIAN_POINT('Ctrl Pts',(132.487160689988,38.2405642567579,17.9425407177715));
#36206=CARTESIAN_POINT('Ctrl Pts',(132.581704160612,38.1680013371556,17.9367376591697));
#36207=CARTESIAN_POINT('Ctrl Pts',(132.673155546112,38.0912314422968,17.9309346005679));
#36208=CARTESIAN_POINT('Ctrl Pts',(132.761122989607,38.0105522477221,17.9251315419662));
#36209=CARTESIAN_POINT('Ctrl Pts',(132.849041292519,37.9299181223515,17.9193317250828));
#36210=CARTESIAN_POINT('Ctrl Pts',(132.933479223414,37.8453793164917,17.9135319081995));
#36211=CARTESIAN_POINT('Ctrl Pts',(133.014078181312,37.7572736021182,17.9077320913162));
#36212=CARTESIAN_POINT('Ctrl Pts',(133.094654295706,37.6691928588278,17.9019339182276));
#36213=CARTESIAN_POINT('Ctrl Pts',(133.171393324555,37.5775475187252,17.896135745139));
#36214=CARTESIAN_POINT('Ctrl Pts',(133.243974139683,37.4827115783087,17.8903375720504));
#36215=CARTESIAN_POINT('Ctrl Pts',(133.316551597246,37.3878800249717,17.8845396671834));
#36216=CARTESIAN_POINT('Ctrl Pts',(133.384970975045,37.2898584898196,17.8787417623164));
#36217=CARTESIAN_POINT('Ctrl Pts',(133.448952408548,37.1890528279536,17.8729438574494));
#36218=CARTESIAN_POINT('Ctrl Pts',(133.512946056224,37.0882279221019,17.8671448457517));
#36219=CARTESIAN_POINT('Ctrl Pts',(133.572499855678,36.9846181780772,17.861345834054));
#36220=CARTESIAN_POINT('Ctrl Pts',(133.627378475355,36.8786565403319,17.8555468223563));
#36221=CARTESIAN_POINT('Ctrl Pts',(133.682314831683,36.7725834225588,17.8497417096394));
#36222=CARTESIAN_POINT('Ctrl Pts',(133.732565995698,36.6641538329253,17.8439365969225));
#36223=CARTESIAN_POINT('Ctrl Pts',(133.777943536637,36.5538235530401,17.8381314842057));
#36224=CARTESIAN_POINT('Ctrl Pts',(133.823345530585,36.4434338184715,17.8323232432348));
#36225=CARTESIAN_POINT('Ctrl Pts',(133.863868530571,36.3311417379457,17.8265150022639));
#36226=CARTESIAN_POINT('Ctrl Pts',(133.89937362207,36.217419547857,17.8207067612931));
#36227=CARTESIAN_POINT('Ctrl Pts',(133.934935959653,36.1035139995584,17.8148891554949));
#36228=CARTESIAN_POINT('Ctrl Pts',(133.965464119497,35.9881741305205,17.8090715496968));
#36229=CARTESIAN_POINT('Ctrl Pts',(133.990869940087,35.8718842361849,17.8032539438986));
#36230=CARTESIAN_POINT('Ctrl Pts',(134.012612259543,35.7723632613325,17.7982752326903));
#36231=CARTESIAN_POINT('Ctrl Pts',(134.030603846559,35.6721467966439,17.7932965214821));
#36232=CARTESIAN_POINT('Ctrl Pts',(134.044819683309,35.5715406630487,17.7883178102738));
#36233=CARTESIAN_POINT('Ctrl Pts',(134.061475242332,35.4536685021903,17.7824846525185));
#36234=CARTESIAN_POINT('Ctrl Pts',(134.073000529151,35.3348804874062,17.7766514947632));
#36235=CARTESIAN_POINT('Ctrl Pts',(134.079303343295,35.2156599948512,17.7708183370079));
#36236=CARTESIAN_POINT('Ctrl Pts',(134.085598200645,35.0965900085528,17.7649925431439));
#36237=CARTESIAN_POINT('Ctrl Pts',(134.08668367818,34.9770890332654,17.7591667492798));
#36238=CARTESIAN_POINT('Ctrl Pts',(134.082518957228,34.8576484497061,17.7533409554158));
#36239=CARTESIAN_POINT('Ctrl Pts',(134.078358418247,34.7383278014458,17.7475210114756));
#36240=CARTESIAN_POINT('Ctrl Pts',(134.06895818348,34.6190678285839,17.7417010675355));
#36241=CARTESIAN_POINT('Ctrl Pts',(134.054329427311,34.5003622363787,17.7358811235954));
#36242=CARTESIAN_POINT('Ctrl Pts',(134.039180772276,34.3774379052638,17.7298543416833));
#36243=CARTESIAN_POINT('Ctrl Pts',(134.018425025373,34.2551085359106,17.7238275597712));
#36244=CARTESIAN_POINT('Ctrl Pts',(133.992133504218,34.133919700893,17.7178007778591));
#36245=CARTESIAN_POINT('Ctrl Pts',(133.966773400114,34.0170241643375,17.7119875038458));
#36246=CARTESIAN_POINT('Ctrl Pts',(133.936263183771,33.9011901548335,17.7061742298324));
#36247=CARTESIAN_POINT('Ctrl Pts',(133.900719174936,33.786898636434,17.7003609558191));
#36248=CARTESIAN_POINT('Ctrl Pts',(133.865180801703,33.672625239272,17.6945486035165));
#36249=CARTESIAN_POINT('Ctrl Pts',(133.82461034417,33.5598942351823,17.6887362512138));
#36250=CARTESIAN_POINT('Ctrl Pts',(133.779174119798,33.4491718430957,17.6829238989112));
#36251=CARTESIAN_POINT('Ctrl Pts',(133.733734473169,33.338441111396,17.6771111088221));
#36252=CARTESIAN_POINT('Ctrl Pts',(133.683428485553,33.2297196688949,17.671298318733));
#36253=CARTESIAN_POINT('Ctrl Pts',(133.628470545243,33.1234535704379,17.6654855286438));
#36254=CARTESIAN_POINT('Ctrl Pts',(133.573495612497,33.0171546155841,17.6596709412991));
#36255=CARTESIAN_POINT('Ctrl Pts',(133.513866053221,32.9133128758775,17.6538563539544));
#36256=CARTESIAN_POINT('Ctrl Pts',(133.44984179878,32.8123490764308,17.6480417666097));
#36257=CARTESIAN_POINT('Ctrl Pts',(133.385748640617,32.7112766184512,17.6422209215317));
#36258=CARTESIAN_POINT('Ctrl Pts',(133.317251564341,32.6130886271358,17.6364000764537));
#36259=CARTESIAN_POINT('Ctrl Pts',(133.244653443095,32.5181762685054,17.6305792313757));
#36260=CARTESIAN_POINT('Ctrl Pts',(133.172008829618,32.4232031274841,17.6247546585968));
#36261=CARTESIAN_POINT('Ctrl Pts',(133.095258200717,32.3315101087105,17.618930085818));
#36262=CARTESIAN_POINT('Ctrl Pts',(133.014743192293,32.2434535221544,17.6131055130391));
#36263=CARTESIAN_POINT('Ctrl Pts',(132.934115768986,32.1552739911792,17.6072728080041));
#36264=CARTESIAN_POINT('Ctrl Pts',(132.849713761962,32.070741313553,17.6014401029691));
#36265=CARTESIAN_POINT('Ctrl Pts',(132.761914021121,31.9901734369007,17.5956073979341));
#36266=CARTESIAN_POINT('Ctrl Pts',(132.739991625622,31.9700567390663,17.5941510511912));
#36267=CARTESIAN_POINT('Ctrl Pts',(132.717857555366,31.9501870155264,17.5926947044482));
#36268=CARTESIAN_POINT('Ctrl Pts',(132.695517967664,31.930568800901,17.5912383577053));
#36269=CARTESIAN_POINT('Ctrl Pts',(132.606179064856,31.852113021276,17.5854142385741));
#36270=CARTESIAN_POINT('Ctrl Pts',(132.51326988702,31.7774361102096,17.5795901194429));
#36271=CARTESIAN_POINT('Ctrl Pts',(132.417143370658,31.7068794547295,17.5737660003117));
#36272=CARTESIAN_POINT('Ctrl Pts',(132.3211364942,31.63641061468,17.5679491299301));
#36273=CARTESIAN_POINT('Ctrl Pts',(132.221920570064,31.5700520697725,17.5621322595485));
#36274=CARTESIAN_POINT('Ctrl Pts',(132.119883396255,31.5081066187121,17.5563153891669));
#36275=CARTESIAN_POINT('Ctrl Pts',(132.017946657148,31.4462221402628,17.550504244303));
#36276=CARTESIAN_POINT('Ctrl Pts',(131.913194539782,31.3887423246919,17.5446930994391));
#36277=CARTESIAN_POINT('Ctrl Pts',(131.806045274565,31.3359277482259,17.5388819545752));
#36278=CARTESIAN_POINT('Ctrl Pts',(131.694858288392,31.281122952585,17.5328518275152));
#36279=CARTESIAN_POINT('Ctrl Pts',(131.581090298122,31.2313421790629,17.5268217004553));
#36280=CARTESIAN_POINT('Ctrl Pts',(131.465238829872,31.1868254470279,17.5207915733954));
#36281=CARTESIAN_POINT('Ctrl Pts',(131.353715623188,31.1439718795879,17.514986734522));
#36282=CARTESIAN_POINT('Ctrl Pts',(131.240262240536,31.1059962332136,17.5091818956486));
#36283=CARTESIAN_POINT('Ctrl Pts',(131.125343875498,31.0730640237102,17.5033770567752));
#36284=CARTESIAN_POINT('Ctrl Pts',(131.010440813741,31.0401361996751,17.497572990912));
#36285=CARTESIAN_POINT('Ctrl Pts',(130.894073549817,31.0122505893171,17.4917689250489));
#36286=CARTESIAN_POINT('Ctrl Pts',(130.776722274975,30.9895227830646,17.4859648591858));
#36287=CARTESIAN_POINT('Ctrl Pts',(130.659358966333,30.9667926461867,17.4801601981441));
#36288=CARTESIAN_POINT('Ctrl Pts',(130.541011846842,30.9492214427428,17.4743555371023));
#36289=CARTESIAN_POINT('Ctrl Pts',(130.422170497491,30.9368734857196,17.4685508760606));
#36290=CARTESIAN_POINT('Ctrl Pts',(130.303288949406,30.9245213519327,17.4627442515607));
#36291=CARTESIAN_POINT('Ctrl Pts',(130.183913244704,30.9173960206188,17.4569376270608));
#36292=CARTESIAN_POINT('Ctrl Pts',(130.064536629376,30.9155098208627,17.4511310025609));
#36293=CARTESIAN_POINT('Ctrl Pts',(129.945025504436,30.9136214957993,17.445317835349));
#36294=CARTESIAN_POINT('Ctrl Pts',(129.825513875141,30.9169840921842,17.4395046681372));
#36295=CARTESIAN_POINT('Ctrl Pts',(129.706493698786,30.9255578233152,17.4336915009253));
#36296=CARTESIAN_POINT('Ctrl Pts',(129.587393980228,30.9341372843442,17.427874448724));
#36297=CARTESIAN_POINT('Ctrl Pts',(129.468786773136,30.9479347687692,17.4220573965227));
#36298=CARTESIAN_POINT('Ctrl Pts',(129.35115597566,30.9668589868344,17.4162403443214));
#36299=CARTESIAN_POINT('Ctrl Pts',(129.233354945568,30.9858105915978,17.4104148738144));
#36300=CARTESIAN_POINT('Ctrl Pts',(129.11653354369,31.0099036563026,17.4045894033074));
#36301=CARTESIAN_POINT('Ctrl Pts',(129.001162746281,31.0389964477946,17.3987639328003));
#36302=CARTESIAN_POINT('Ctrl Pts',(128.970762585872,31.0466623870788,17.3972289235792));
#36303=CARTESIAN_POINT('Ctrl Pts',(128.940463045509,31.0546752045074,17.395693914358));
#36304=CARTESIAN_POINT('Ctrl Pts',(128.910272516687,31.0630317486532,17.3941589051369));
#36305=CARTESIAN_POINT('Ctrl Pts',(128.796624973599,31.0944886574235,17.3883806020264));
#36306=CARTESIAN_POINT('Ctrl Pts',(128.684141022598,31.1309259262771,17.3826022989159));
#36307=CARTESIAN_POINT('Ctrl Pts',(128.573294016828,31.1722415126369,17.3768239958053));
#36308=CARTESIAN_POINT('Ctrl Pts',(128.462588204215,31.2135044726036,17.3710530529014));
#36309=CARTESIAN_POINT('Ctrl Pts',(128.353515576709,31.2596332518481,17.3652821099975));
#36310=CARTESIAN_POINT('Ctrl Pts',(128.246536858835,31.310475367669,17.3595111670936));
#36311=CARTESIAN_POINT('Ctrl Pts',(128.139665375776,31.3612665196631,17.3537460089476));
#36312=CARTESIAN_POINT('Ctrl Pts',(128.034884001239,31.4167614353966,17.3479808508016));
#36313=CARTESIAN_POINT('Ctrl Pts',(127.932635253745,31.4767588776894,17.3422156926557));
#36314=CARTESIAN_POINT('Ctrl Pts',(127.825381772362,31.5396929939268,17.3361683493187));
#36315=CARTESIAN_POINT('Ctrl Pts',(127.72091557039,31.6075814196211,17.3301210059818));
#36316=CARTESIAN_POINT('Ctrl Pts',(127.61972050568,31.6801363689273,17.3240736626448));
#36317=CARTESIAN_POINT('Ctrl Pts',(127.523350765193,31.7492316519403,17.3183146771677));
#36318=CARTESIAN_POINT('Ctrl Pts',(127.429947779764,31.8225584266251,17.3125556916906));
#36319=CARTESIAN_POINT('Ctrl Pts',(127.33990051386,31.899823275386,17.3067967062135));
#36320=CARTESIAN_POINT('Ctrl Pts',(127.249863444096,31.977079375373,17.301038372832));
#36321=CARTESIAN_POINT('Ctrl Pts',(127.163181654013,32.0582723926968,17.2952800394504));
#36322=CARTESIAN_POINT('Ctrl Pts',(127.080210638688,32.1430689393043,17.2895217060688));
#36323=CARTESIAN_POINT('Ctrl Pts',(126.997228643662,32.2278767071884,17.2837626106768));
#36324=CARTESIAN_POINT('Ctrl Pts',(126.917958690283,32.3162886553778,17.2780035152848));
#36325=CARTESIAN_POINT('Ctrl Pts',(126.842718523364,32.4079354411411,17.2722444198928));
#36326=CARTESIAN_POINT('Ctrl Pts',(126.767449922388,32.4996168611974,17.2664831480776));
#36327=CARTESIAN_POINT('Ctrl Pts',(126.696214399148,32.5945352284173,17.2607218762623));
#36328=CARTESIAN_POINT('Ctrl Pts',(126.62928816068,32.692289728699,17.2549606044471));
#36329=CARTESIAN_POINT('Ctrl Pts',(126.562279589997,32.7901644859184,17.2491922451535));
#36330=CARTESIAN_POINT('Ctrl Pts',(126.49959111936,32.8908819966749,17.2434238858598));
#36331=CARTESIAN_POINT('Ctrl Pts',(126.441454582281,32.994014080301,17.2376555265662));
#36332=CARTESIAN_POINT('Ctrl Pts',(126.383276299843,33.0972202186628,17.2318830252607));
#36333=CARTESIAN_POINT('Ctrl Pts',(126.329656643999,33.2028440115217,17.2261105239551));
#36334=CARTESIAN_POINT('Ctrl Pts',(126.280779817259,33.3104360822107,17.2203380226495));
#36335=CARTESIAN_POINT('Ctrl Pts',(126.231825524133,33.4181986788858,17.2145563723289));
#36336=CARTESIAN_POINT('Ctrl Pts',(126.187629215659,33.5279353952719,17.2087747220083));
#36337=CARTESIAN_POINT('Ctrl Pts',(126.148325715824,33.6391803173768,17.2029930716876));
#36338=CARTESIAN_POINT('Ctrl Pts',(126.134925509125,33.6771083633948,17.2010218653146));
#36339=CARTESIAN_POINT('Ctrl Pts',(126.122093612364,33.7152116296383,17.1990506589415));
#36340=CARTESIAN_POINT('Ctrl Pts',(126.109834007681,33.7534713993642,17.1970794525685));
#36341=CARTESIAN_POINT('Ctrl Pts',(126.063948535826,33.8966707628269,17.1897015854277));
#36342=CARTESIAN_POINT('Ctrl Pts',(126.025960954389,34.0424458435051,17.182323718287));
#36343=CARTESIAN_POINT('Ctrl Pts',(125.996105954063,34.1900262541832,17.1749458511462));
#36344=CARTESIAN_POINT('Ctrl Pts',(125.966728932655,34.3352439006973,17.1676861037478));
#36345=CARTESIAN_POINT('Ctrl Pts',(125.945226128074,34.482209666858,17.1604263563494));
#36346=CARTESIAN_POINT('Ctrl Pts',(125.931775537335,34.6301693341903,17.153166608951));
#36347=CARTESIAN_POINT('Ctrl Pts',(125.920793836325,34.7509706327901,17.1472394064299));
#36348=CARTESIAN_POINT('Ctrl Pts',(125.915178848841,34.8724341239438,17.1413122039088));
#36349=CARTESIAN_POINT('Ctrl Pts',(125.915004205853,34.9941381057528,17.1353850013877));
#36350=CARTESIAN_POINT('',(126.824949217806,37.5702679880679,17.));
#36351=CARTESIAN_POINT('Ctrl Pts',(125.919161438299,34.9941446863292,17.1353849714045));
#36352=CARTESIAN_POINT('Ctrl Pts',(125.92665550953,35.9198397886616,17.090256647603));
#36353=CARTESIAN_POINT('Ctrl Pts',(126.2419104066,36.8500404311903,17.0451283238015));
#36354=CARTESIAN_POINT('Ctrl Pts',(126.824949217806,37.5702679880679,17.));
#36355=CARTESIAN_POINT('',(128.537425954644,38.8141974466263,17.0000001263023));
#36356=CARTESIAN_POINT('Origin',(130.,35.,17.));
#36357=CARTESIAN_POINT('',(125.915001286801,35.0032424009398,17.239615028553));
#36358=CARTESIAN_POINT('Ctrl Pts',(125.915001286801,35.0032424009399,17.239615028553));
#36359=CARTESIAN_POINT('Ctrl Pts',(125.915121833596,35.1551155066225,17.2322214796527));
#36360=CARTESIAN_POINT('Ctrl Pts',(125.923715576038,35.3066295363267,17.2248279307525));
#36361=CARTESIAN_POINT('Ctrl Pts',(125.94064101634,35.4569788198348,17.2174343818523));
#36362=CARTESIAN_POINT('Ctrl Pts',(125.95789917151,35.610283621261,17.2098954929428));
#36363=CARTESIAN_POINT('Ctrl Pts',(125.983819809633,35.7623776772745,17.2023566040334));
#36364=CARTESIAN_POINT('Ctrl Pts',(126.018204397236,35.9124301495502,17.1948177151239));
#36365=CARTESIAN_POINT('Ctrl Pts',(126.025778835979,35.9454845887252,17.193157004433));
#36366=CARTESIAN_POINT('Ctrl Pts',(126.033763810909,35.9784400380016,17.1914962937421));
#36367=CARTESIAN_POINT('Ctrl Pts',(126.042156888354,36.0112877452039,17.1898355830512));
#36368=CARTESIAN_POINT('Ctrl Pts',(126.071413105751,36.1257868272338,17.1840467513238));
#36369=CARTESIAN_POINT('Ctrl Pts',(126.10569155362,36.2392087379591,17.1782579195964));
#36370=CARTESIAN_POINT('Ctrl Pts',(126.144897365093,36.3510768572991,17.1724690878689));
#36371=CARTESIAN_POINT('Ctrl Pts',(126.1840541934,36.4628052102548,17.1666874886228));
#36372=CARTESIAN_POINT('Ctrl Pts',(126.228126008179,36.5729832451381,17.1609058893767));
#36373=CARTESIAN_POINT('Ctrl Pts',(126.276967308782,36.681146210216,17.1551242901305));
#36374=CARTESIAN_POINT('Ctrl Pts',(126.325760720866,36.7892031223401,17.1493483596979));
#36375=CARTESIAN_POINT('Ctrl Pts',(126.379314148376,36.895248519388,17.1435724292653));
#36376=CARTESIAN_POINT('Ctrl Pts',(126.437433053197,36.9988350981372,17.1377964988327));
#36377=CARTESIAN_POINT('Ctrl Pts',(126.495512284402,37.1023509657452,17.1320245112142));
#36378=CARTESIAN_POINT('Ctrl Pts',(126.558150592357,37.2034109938462,17.1262525235958));
#36379=CARTESIAN_POINT('Ctrl Pts',(126.625106600157,37.3015906542424,17.1204805359774));
#36380=CARTESIAN_POINT('Ctrl Pts',(126.692038577867,37.3997350785762,17.114710619889));
#36381=CARTESIAN_POINT('Ctrl Pts',(126.7632849423,37.4950008487302,17.1089407038006));
#36382=CARTESIAN_POINT('Ctrl Pts',(126.838560236032,37.5869912289767,17.1031707877122));
#36383=CARTESIAN_POINT('Ctrl Pts',(126.913826833735,37.6789709822169,17.0974015381819));
#36384=CARTESIAN_POINT('Ctrl Pts',(126.993121173229,37.7676757778223,17.0916322886517));
#36385=CARTESIAN_POINT('Ctrl Pts',(127.076117092332,37.8527414432873,17.0858630391214));
#36386=CARTESIAN_POINT('Ctrl Pts',(127.159123622615,37.9378179845522,17.0800930519821));
#36387=CARTESIAN_POINT('Ctrl Pts',(127.245832384141,38.0192541748308,17.0743230648428));
#36388=CARTESIAN_POINT('Ctrl Pts',(127.335880412824,38.0967227556284,17.0685530777035));
#36389=CARTESIAN_POINT('Ctrl Pts',(127.426018169077,38.1742685293145,17.0627773411111));
#36390=CARTESIAN_POINT('Ctrl Pts',(127.519501524578,38.2478385262392,17.0570016045186));
#36391=CARTESIAN_POINT('Ctrl Pts',(127.615934339647,38.3171457500579,17.0512258679262));
#36392=CARTESIAN_POINT('Ctrl Pts',(127.712414812686,38.3864872261334,17.0454472769125));
#36393=CARTESIAN_POINT('Ctrl Pts',(127.811847302618,38.4515615061195,17.0396686858988));
#36394=CARTESIAN_POINT('Ctrl Pts',(127.913808126291,38.5121259183109,17.0338900948852));
#36395=CARTESIAN_POINT('Ctrl Pts',(128.015934147913,38.5727884575696,17.0281021413404));
#36396=CARTESIAN_POINT('Ctrl Pts',(128.120596323314,38.6289263334615,17.0223141877957));
#36397=CARTESIAN_POINT('Ctrl Pts',(128.227347413244,38.6803434359674,17.016526234251));
#36398=CARTESIAN_POINT('Ctrl Pts',(128.328948092551,38.7292798219659,17.0110175316014));
#36399=CARTESIAN_POINT('Ctrl Pts',(128.432440532449,38.7739402350394,17.0055088289519));
#36400=CARTESIAN_POINT('Ctrl Pts',(128.537425954644,38.8141974466263,17.0000001263023));
#36401=CARTESIAN_POINT('Ctrl Pts',(132.487160689988,38.2405642567579,18.0469660621892));
#36402=CARTESIAN_POINT('Ctrl Pts',(132.581995851227,38.1677774621218,18.0411567024933));
#36403=CARTESIAN_POINT('Ctrl Pts',(132.673587220315,38.0908594993528,18.0353473427975));
#36404=CARTESIAN_POINT('Ctrl Pts',(132.761569442504,38.0101427232324,18.0295379831017));
#36405=CARTESIAN_POINT('Ctrl Pts',(132.849596883711,37.9293844622157,18.0237256376488));
#36406=CARTESIAN_POINT('Ctrl Pts',(132.934011193521,37.8448237867974,18.0179132921958));
#36407=CARTESIAN_POINT('Ctrl Pts',(133.014484760213,37.756829089814,18.0121009467429));
#36408=CARTESIAN_POINT('Ctrl Pts',(133.095089119703,37.6686913760231,18.0062791545493));
#36409=CARTESIAN_POINT('Ctrl Pts',(133.171739674954,37.5771088012885,18.0004573623556));
#36410=CARTESIAN_POINT('Ctrl Pts',(133.244149517064,37.4824824089878,17.994635570162));
#36411=CARTESIAN_POINT('Ctrl Pts',(133.312483103624,37.3931829355919,17.9891415112163));
#36412=CARTESIAN_POINT('Ctrl Pts',(133.377040210958,37.3011732045948,17.9836474522707));
#36413=CARTESIAN_POINT('Ctrl Pts',(133.437616789531,37.2068112307882,17.978153393325));
#36414=CARTESIAN_POINT('Ctrl Pts',(133.50183711402,37.1067732834495,17.9723288608644));
#36415=CARTESIAN_POINT('Ctrl Pts',(133.561790434345,37.0037686003075,17.9665043284039));
#36416=CARTESIAN_POINT('Ctrl Pts',(133.61719148879,36.8981967056732,17.9606797959433));
#36417=CARTESIAN_POINT('Ctrl Pts',(133.672522632229,36.792758033002,17.9548626135037));
#36418=CARTESIAN_POINT('Ctrl Pts',(133.72331274761,36.6847589506059,17.9490454310642));
#36419=CARTESIAN_POINT('Ctrl Pts',(133.769319891238,36.5746277520473,17.9432282486247));
#36420=CARTESIAN_POINT('Ctrl Pts',(133.815280959147,36.4646068488419,17.9374168920383));
#36421=CARTESIAN_POINT('Ctrl Pts',(133.856468428238,36.3524584518935,17.931605535452));
#36422=CARTESIAN_POINT('Ctrl Pts',(133.892686612845,36.2386347057038,17.9257941788656));
#36423=CARTESIAN_POINT('Ctrl Pts',(133.930267513151,36.1205283206296,17.9197641689444));
#36424=CARTESIAN_POINT('Ctrl Pts',(133.962497634803,36.0006184357189,17.9137341590232));
#36425=CARTESIAN_POINT('Ctrl Pts',(133.989213388344,35.879432511484,17.907704149102));
#36426=CARTESIAN_POINT('Ctrl Pts',(134.014931363188,35.7627726334056,17.9018993477056));
#36427=CARTESIAN_POINT('Ctrl Pts',(134.03553938943,35.6449307561636,17.8960945463092));
#36428=CARTESIAN_POINT('Ctrl Pts',(134.05094274229,35.5263913930623,17.8902897449128));
#36429=CARTESIAN_POINT('Ctrl Pts',(134.06634380127,35.407869682942,17.8844858079723));
#36430=CARTESIAN_POINT('Ctrl Pts',(134.0765416757,35.2886510982102,17.8786818710318));
#36431=CARTESIAN_POINT('Ctrl Pts',(134.081493234088,35.1692275984909,17.8728779340913));
#36432=CARTESIAN_POINT('Ctrl Pts',(134.086445222649,35.0497937237118,17.8670734929268));
#36433=CARTESIAN_POINT('Ctrl Pts',(134.086149972063,34.9301553064141,17.8612690517624));
#36434=CARTESIAN_POINT('Ctrl Pts',(134.080616452514,34.8108060057166,17.8554646105979));
#36435=CARTESIAN_POINT('Ctrl Pts',(134.075081147455,34.691418194388,17.849658296505));
#36436=CARTESIAN_POINT('Ctrl Pts',(134.064304230807,34.5723200927413,17.8438519824122));
#36437=CARTESIAN_POINT('Ctrl Pts',(134.048346626875,34.4540012924314,17.8380456683193));
#36438=CARTESIAN_POINT('Ctrl Pts',(134.032371403262,34.3355518497259,17.8322329431507));
#36439=CARTESIAN_POINT('Ctrl Pts',(134.011204128747,34.2178838307071,17.8264202179822));
#36440=CARTESIAN_POINT('Ctrl Pts',(133.98495707752,34.1014778298091,17.8206074928137));
#36441=CARTESIAN_POINT('Ctrl Pts',(133.958692832105,33.9849955724731,17.8147909597854));
#36442=CARTESIAN_POINT('Ctrl Pts',(133.927342289602,33.8697773727218,17.8089744267572));
#36443=CARTESIAN_POINT('Ctrl Pts',(133.891067468789,33.7562882354296,17.803157893729));
#36444=CARTESIAN_POINT('Ctrl Pts',(133.854740822545,33.642636957475,17.797333050685));
#36445=CARTESIAN_POINT('Ctrl Pts',(133.813475996655,33.5307200542088,17.7915082076411));
#36446=CARTESIAN_POINT('Ctrl Pts',(133.767482984804,33.4209822802718,17.7856833645971));
#36447=CARTESIAN_POINT('Ctrl Pts',(133.755350967756,33.3920356970721,17.7841468899836));
#36448=CARTESIAN_POINT('Ctrl Pts',(133.742890211318,33.3632406005495,17.7826104153701));
#36449=CARTESIAN_POINT('Ctrl Pts',(133.730105090453,33.3346048474387,17.7810739407566));
#36450=CARTESIAN_POINT('Ctrl Pts',(133.681642154084,33.2260589294508,17.7752498212811));
#36451=CARTESIAN_POINT('Ctrl Pts',(133.628359295553,33.1194555429994,17.7694257018056));
#36452=CARTESIAN_POINT('Ctrl Pts',(133.570434327724,33.0152522297759,17.76360158233));
#36453=CARTESIAN_POINT('Ctrl Pts',(133.512582326264,32.9111801783859,17.7577847993257));
#36454=CARTESIAN_POINT('Ctrl Pts',(133.450100042775,32.8095025405984,17.7519680163213));
#36455=CARTESIAN_POINT('Ctrl Pts',(133.383213095,32.7106563923645,17.7461512333169));
#36456=CARTESIAN_POINT('Ctrl Pts',(133.316392979415,32.6119090093582,17.7403402623336));
#36457=CARTESIAN_POINT('Ctrl Pts',(133.245177182433,32.5159878237591,17.7345292913504));
#36458=CARTESIAN_POINT('Ctrl Pts',(133.169836623754,32.4233042906255,17.7287183203671));
#36459=CARTESIAN_POINT('Ctrl Pts',(133.091654233912,32.3271247527196,17.722688160693));
#36460=CARTESIAN_POINT('Ctrl Pts',(133.009030002331,32.2344323156608,17.7166580010188));
#36461=CARTESIAN_POINT('Ctrl Pts',(132.922315528805,32.1456529730768,17.7106278413447));
#36462=CARTESIAN_POINT('Ctrl Pts',(132.838846755965,32.0601966187024,17.7048233890133));
#36463=CARTESIAN_POINT('Ctrl Pts',(132.751588742913,31.9783660088873,17.6990189366818));
#36464=CARTESIAN_POINT('Ctrl Pts',(132.660894819584,31.9005058865823,17.6932144843504));
#36465=CARTESIAN_POINT('Ctrl Pts',(132.570214184431,31.8226571720872,17.6874108824682));
#36466=CARTESIAN_POINT('Ctrl Pts',(132.476098949816,31.748778054045,17.6816072805861));
#36467=CARTESIAN_POINT('Ctrl Pts',(132.378936948102,31.6791741995469,17.675803678704));
#36468=CARTESIAN_POINT('Ctrl Pts',(132.281766265341,31.6095641262146,17.6699995582926));
#36469=CARTESIAN_POINT('Ctrl Pts',(132.18154860613,31.5442303136562,17.6641954378812));
#36470=CARTESIAN_POINT('Ctrl Pts',(132.078701776204,31.4834357782623,17.6583913174697));
#36471=CARTESIAN_POINT('Ctrl Pts',(131.975821499723,31.4226214720326,17.6525853095151));
#36472=CARTESIAN_POINT('Ctrl Pts',(131.870310703314,31.3663495864621,17.6467793015605));
#36473=CARTESIAN_POINT('Ctrl Pts',(131.762612260656,31.3148374501812,17.6409732936059));
#36474=CARTESIAN_POINT('Ctrl Pts',(131.654794468821,31.2632682292214,17.6351608515539));
#36475=CARTESIAN_POINT('Ctrl Pts',(131.544784560114,31.21646946248,17.6293484095019));
#36476=CARTESIAN_POINT('Ctrl Pts',(131.433046022634,31.1746105953755,17.6235359674499));
#36477=CARTESIAN_POINT('Ctrl Pts',(131.321234031561,31.1327242114963,17.6177197044713));
#36478=CARTESIAN_POINT('Ctrl Pts',(131.207691535957,31.0957843204613,17.6119034414927));
#36479=CARTESIAN_POINT('Ctrl Pts',(131.092896241219,31.0639102136854,17.6060871785142));
#36480=CARTESIAN_POINT('Ctrl Pts',(130.97793651638,31.0319904511829,17.6002625844562));
#36481=CARTESIAN_POINT('Ctrl Pts',(130.861720807078,31.0051510472991,17.5944379903983));
#36482=CARTESIAN_POINT('Ctrl Pts',(130.744736168808,30.9834600663171,17.5886133963404));
#36483=CARTESIAN_POINT('Ctrl Pts',(130.71381319552,30.9777264107243,17.5870737602896));
#36484=CARTESIAN_POINT('Ctrl Pts',(130.682836516287,30.9723522053115,17.5855341242389));
#36485=CARTESIAN_POINT('Ctrl Pts',(130.651815156237,30.9673380997039,17.5839944881881));
#36486=CARTESIAN_POINT('Ctrl Pts',(130.534583178963,30.9483894297009,17.5781760915022));
#36487=CARTESIAN_POINT('Ctrl Pts',(130.416333096405,30.9345261234571,17.5723576948162));
#36488=CARTESIAN_POINT('Ctrl Pts',(130.297544102524,30.9258507014282,17.5665392981303));
#36489=CARTESIAN_POINT('Ctrl Pts',(130.178905374958,30.9171862536794,17.5607282616298));
#36490=CARTESIAN_POINT('Ctrl Pts',(130.059729496346,30.9136966673801,17.5549172251293));
#36491=CARTESIAN_POINT('Ctrl Pts',(129.940504821447,30.9154332758873,17.5491061886289));
#36492=CARTESIAN_POINT('Ctrl Pts',(129.821399734198,30.9171681424989,17.5433009808564));
#36493=CARTESIAN_POINT('Ctrl Pts',(129.702246354756,30.9241187699002,17.5374957730839));
#36494=CARTESIAN_POINT('Ctrl Pts',(129.583536504175,30.9362845625406,17.5316905653114));
#36495=CARTESIAN_POINT('Ctrl Pts',(129.460182596709,30.948926294059,17.5256582515742));
#36496=CARTESIAN_POINT('Ctrl Pts',(129.337308077732,30.9671995934947,17.519625937837));
#36497=CARTESIAN_POINT('Ctrl Pts',(129.215463336517,30.9910441230102,17.5135936240999));
#36498=CARTESIAN_POINT('Ctrl Pts',(129.09833760526,31.0139651611128,17.5077949400484));
#36499=CARTESIAN_POINT('Ctrl Pts',(128.982163809782,31.0420338337901,17.501996255997));
#36500=CARTESIAN_POINT('Ctrl Pts',(128.867423224995,31.0751439709566,17.4961975719455));
#36501=CARTESIAN_POINT('Ctrl Pts',(128.75269930978,31.108249297865,17.4903997303299));
#36502=CARTESIAN_POINT('Ctrl Pts',(128.639408584219,31.1463945193783,17.4846018887143));
#36503=CARTESIAN_POINT('Ctrl Pts',(128.5280185711,31.1894231836934,17.4788040470987));
#36504=CARTESIAN_POINT('Ctrl Pts',(128.416618323132,31.2324558016114,17.47300567276));
#36505=CARTESIAN_POINT('Ctrl Pts',(128.30711951653,31.2803726070192,17.4672072984214));
#36506=CARTESIAN_POINT('Ctrl Pts',(128.199970437257,31.3329686975358,17.4614089240827));
#36507=CARTESIAN_POINT('Ctrl Pts',(128.092786100998,31.3855820945907,17.4556086418115));
#36508=CARTESIAN_POINT('Ctrl Pts',(127.987953396773,31.4428776585701,17.4498083595403));
#36509=CARTESIAN_POINT('Ctrl Pts',(127.885896133519,31.5046044799294,17.4440080772692));
#36510=CARTESIAN_POINT('Ctrl Pts',(127.783724623509,31.5664004006247,17.4382013019429));
#36511=CARTESIAN_POINT('Ctrl Pts',(127.684335106399,31.6326372683155,17.4323945266166));
#36512=CARTESIAN_POINT('Ctrl Pts',(127.588122632924,31.7030206906646,17.4265877512904));
#36513=CARTESIAN_POINT('Ctrl Pts',(127.491846393153,31.7734507607088,17.4207771274345));
#36514=CARTESIAN_POINT('Ctrl Pts',(127.398751708728,31.8480326029509,17.4149665035786));
#36515=CARTESIAN_POINT('Ctrl Pts',(127.309199450961,31.9264324628711,17.4091558797227));
#36516=CARTESIAN_POINT('Ctrl Pts',(127.219517508456,32.0049458572306,17.4033368412354));
#36517=CARTESIAN_POINT('Ctrl Pts',(127.133388526181,32.0872880230325,17.3975178027482));
#36518=CARTESIAN_POINT('Ctrl Pts',(127.051135632554,32.1730893288947,17.3916987642609));
#36519=CARTESIAN_POINT('Ctrl Pts',(127.028596082769,32.1966012409975,17.3901041880472));
#36520=CARTESIAN_POINT('Ctrl Pts',(127.006347352703,32.220372719968,17.3885096118334));
#36521=CARTESIAN_POINT('Ctrl Pts',(126.984395538433,32.244395759298,17.3869150356197));
#36522=CARTESIAN_POINT('Ctrl Pts',(126.904949793899,32.3313374681727,17.3811441096744));
#36523=CARTESIAN_POINT('Ctrl Pts',(126.829126556866,32.4218715866098,17.3753731837292));
#36524=CARTESIAN_POINT('Ctrl Pts',(126.757272073936,32.5156609334618,17.3696022577839));
#36525=CARTESIAN_POINT('Ctrl Pts',(126.685531583472,32.609301489613,17.3638404870374));
#36526=CARTESIAN_POINT('Ctrl Pts',(126.617747567003,32.7061866680698,17.358078716291));
#36527=CARTESIAN_POINT('Ctrl Pts',(126.554228459588,32.8059435988822,17.3523169455445));
#36528=CARTESIAN_POINT('Ctrl Pts',(126.490767188589,32.9056096974456,17.3465604210962));
#36529=CARTESIAN_POINT('Ctrl Pts',(126.431563330612,33.0081420020447,17.3408038966478));
#36530=CARTESIAN_POINT('Ctrl Pts',(126.376884074655,33.1131359371927,17.3350473721994));
#36531=CARTESIAN_POINT('Ctrl Pts',(126.322241085739,33.2180602331461,17.3292946658737));
#36532=CARTESIAN_POINT('Ctrl Pts',(126.272116924162,33.325442545264,17.323541959548));
#36533=CARTESIAN_POINT('Ctrl Pts',(126.226734181323,33.4348514250694,17.3177892532224));
#36534=CARTESIAN_POINT('Ctrl Pts',(126.181370319882,33.5442147855327,17.3120389402985));
#36535=CARTESIAN_POINT('Ctrl Pts',(126.140744112726,33.6556026522314,17.3062886273746));
#36536=CARTESIAN_POINT('Ctrl Pts',(126.105030784296,33.7685618940773,17.3005383144507));
#36537=CARTESIAN_POINT('Ctrl Pts',(126.069314310588,33.8815310842595,17.2947874950959));
#36538=CARTESIAN_POINT('Ctrl Pts',(126.038511715076,33.9960715316613,17.2890366757411));
#36539=CARTESIAN_POINT('Ctrl Pts',(126.012748796744,34.1117135359975,17.2832858563864));
#36540=CARTESIAN_POINT('Ctrl Pts',(125.986984894525,34.2273599567015,17.2775348174078));
#36541=CARTESIAN_POINT('Ctrl Pts',(125.966261135726,34.3441076095336,17.2717837784293));
#36542=CARTESIAN_POINT('Ctrl Pts',(125.950652243617,34.4614763256111,17.2660327394508));
#36543=CARTESIAN_POINT('Ctrl Pts',(125.935032726191,34.5789249371669,17.2602777856129));
#36544=CARTESIAN_POINT('Ctrl Pts',(125.924535074559,34.696995041783,17.2545228317751));
#36545=CARTESIAN_POINT('Ctrl Pts',(125.919182137792,34.8152012568155,17.2487678779372));
#36546=CARTESIAN_POINT('Ctrl Pts',(125.916344314637,34.8778674807292,17.2457169281566));
#36547=CARTESIAN_POINT('Ctrl Pts',(125.914951543149,34.9405719254792,17.2426659783761));
#36548=CARTESIAN_POINT('Ctrl Pts',(125.9150012868,35.0032424000665,17.2396150285955));
#36549=CARTESIAN_POINT('Origin',(130.,35.,32.7603849714045));
#36550=CARTESIAN_POINT('',(132.487160689988,38.2405642567579,19.2967873935987));
#36551=CARTESIAN_POINT('',(132.487160689988,38.2405642567579,19.1927515487681));
#36552=CARTESIAN_POINT('',(132.487160689988,38.2405642567579,32.7603849714045));
#36553=CARTESIAN_POINT('',(125.915000065372,35.0007308119611,18.3853849714449));
#36554=CARTESIAN_POINT('Ctrl Pts',(132.487160689988,38.2405642567579,19.1927515487681));
#36555=CARTESIAN_POINT('Ctrl Pts',(132.581827195764,38.1679069066276,19.186927974649));
#36556=CARTESIAN_POINT('Ctrl Pts',(132.673193347444,38.0911853678094,19.1811044005299));
#36557=CARTESIAN_POINT('Ctrl Pts',(132.760910624345,38.0107470043793,19.1752808264108));
#36558=CARTESIAN_POINT('Ctrl Pts',(132.798099043779,37.9766445367301,19.1728118770248));
#36559=CARTESIAN_POINT('Ctrl Pts',(132.834632090439,37.9418744364773,19.1703429276389));
#36560=CARTESIAN_POINT('Ctrl Pts',(132.870485381438,37.9064649791367,19.1678739782529));
#36561=CARTESIAN_POINT('Ctrl Pts',(132.955052702871,37.8229445301852,19.1620504560461));
#36562=CARTESIAN_POINT('Ctrl Pts',(133.03610818715,37.7355954240947,19.1562269338393));
#36563=CARTESIAN_POINT('Ctrl Pts',(133.113286014791,37.6447448251409,19.1504034116324));
#36564=CARTESIAN_POINT('Ctrl Pts',(133.190366468885,37.5540088503632,19.1445872368338));
#36565=CARTESIAN_POINT('Ctrl Pts',(133.263578735065,37.4597804779985,19.1387710620352));
#36566=CARTESIAN_POINT('Ctrl Pts',(133.332592949286,37.3624244399279,19.1329548872366));
#36567=CARTESIAN_POINT('Ctrl Pts',(133.401538079113,37.2651658568956,19.1271445345271));
#36568=CARTESIAN_POINT('Ctrl Pts',(133.466293282176,37.164786167805,19.1213341818177));
#36569=CARTESIAN_POINT('Ctrl Pts',(133.526568598092,37.0616835166802,19.1155238291083));
#36570=CARTESIAN_POINT('Ctrl Pts',(133.589126507816,36.9546764235892,19.1094934414656));
#36571=CARTESIAN_POINT('Ctrl Pts',(133.646858231296,36.8447363991944,19.103463053823));
#36572=CARTESIAN_POINT('Ctrl Pts',(133.699488436065,36.7323424348039,19.0974326661803));
#36573=CARTESIAN_POINT('Ctrl Pts',(133.750141212168,36.6241713505636,19.0916288530198));
#36574=CARTESIAN_POINT('Ctrl Pts',(133.796068714334,36.513727802009,19.0858250398592));
#36575=CARTESIAN_POINT('Ctrl Pts',(133.837072404662,36.4014636496815,19.0800212266986));
#36576=CARTESIAN_POINT('Ctrl Pts',(133.878070040312,36.2892160744815,19.0742182705396));
#36577=CARTESIAN_POINT('Ctrl Pts',(133.914145169957,36.1751488135945,19.0684153143806));
#36578=CARTESIAN_POINT('Ctrl Pts',(133.945147964157,36.0597322968145,19.0626123582216));
#36579=CARTESIAN_POINT('Ctrl Pts',(133.976153497589,35.9443055824762,19.0568088893458));
#36580=CARTESIAN_POINT('Ctrl Pts',(134.00208569858,35.8275297696088,19.05100542047));
#36581=CARTESIAN_POINT('Ctrl Pts',(134.022845201741,35.709888359414,19.0452019515942));
#36582=CARTESIAN_POINT('Ctrl Pts',(134.043611438645,35.5922087899689,19.0393966002519));
#36583=CARTESIAN_POINT('Ctrl Pts',(134.059201569904,35.4736634667302,19.0335912489095));
#36584=CARTESIAN_POINT('Ctrl Pts',(134.06956781371,35.3547433010181,19.0277858975672));
#36585=CARTESIAN_POINT('Ctrl Pts',(134.079945539115,35.2356914199295,19.0219741162469));
#36586=CARTESIAN_POINT('Ctrl Pts',(134.085087792334,35.1162642746923,19.0161623349267));
#36587=CARTESIAN_POINT('Ctrl Pts',(134.084998865295,34.996955244281,19.0103505536064));
#36588=CARTESIAN_POINT('Ctrl Pts',(134.08490987984,34.8775678396986,19.0045349545236));
#36589=CARTESIAN_POINT('Ctrl Pts',(134.079582888704,34.758299111467,18.9987193554409));
#36590=CARTESIAN_POINT('Ctrl Pts',(134.069074134723,34.6396381178254,18.9929037563581));
#36591=CARTESIAN_POINT('Ctrl Pts',(134.058550325626,34.5208071273265,18.9870798256953));
#36592=CARTESIAN_POINT('Ctrl Pts',(134.042829990362,34.4025860125479,18.9812558950325));
#36593=CARTESIAN_POINT('Ctrl Pts',(134.022020616267,34.2854545764428,18.9754319643697));
#36594=CARTESIAN_POINT('Ctrl Pts',(134.016497302086,34.2543650434737,18.9738861514746));
#36595=CARTESIAN_POINT('Ctrl Pts',(134.010615737949,34.22335219832,18.9723403385795));
#36596=CARTESIAN_POINT('Ctrl Pts',(134.004378520531,34.1924248243584,18.9707945256844));
#36597=CARTESIAN_POINT('Ctrl Pts',(133.980880488013,34.0759093351174,18.9649708451492));
#36598=CARTESIAN_POINT('Ctrl Pts',(133.952254965815,33.9602324116435,18.9591471646139));
#36599=CARTESIAN_POINT('Ctrl Pts',(133.918575070159,33.8458793739264,18.9533234840787));
#36600=CARTESIAN_POINT('Ctrl Pts',(133.884937668285,33.7316706149524,18.9475071512565));
#36601=CARTESIAN_POINT('Ctrl Pts',(133.846258691171,33.6187828077004,18.9416908184343));
#36602=CARTESIAN_POINT('Ctrl Pts',(133.802662384732,33.5076917919737,18.9358744856121));
#36603=CARTESIAN_POINT('Ctrl Pts',(133.759109721393,33.3967119864997,18.9300639753656));
#36604=CARTESIAN_POINT('Ctrl Pts',(133.710649669962,33.2875257721358,18.9242534651191));
#36605=CARTESIAN_POINT('Ctrl Pts',(133.657456294753,33.180593928785,18.9184429548725));
#36606=CARTESIAN_POINT('Ctrl Pts',(133.602250554129,33.0696167331239,18.912412626466));
#36607=CARTESIAN_POINT('Ctrl Pts',(133.541946410013,32.9610682776073,18.9063822980595));
#36608=CARTESIAN_POINT('Ctrl Pts',(133.476793536316,32.8554413727221,18.900351969653));
#36609=CARTESIAN_POINT('Ctrl Pts',(133.414086300286,32.7537793756406,18.8945480011515));
#36610=CARTESIAN_POINT('Ctrl Pts',(133.346888019939,32.6548239292565,18.88874403265));
#36611=CARTESIAN_POINT('Ctrl Pts',(133.275467798784,32.5589887957797,18.8829400641485));
#36612=CARTESIAN_POINT('Ctrl Pts',(133.204058136611,32.4631678308599,18.8771369537233));
#36613=CARTESIAN_POINT('Ctrl Pts',(133.128428018869,32.3704665887504,18.8713338432981));
#36614=CARTESIAN_POINT('Ctrl Pts',(133.048888780157,32.281268272478,18.8655307328729));
#36615=CARTESIAN_POINT('Ctrl Pts',(132.96934253096,32.1920620943829,18.8597271109692));
#36616=CARTESIAN_POINT('Ctrl Pts',(132.885886747526,32.106359760753,18.8539234890655));
#36617=CARTESIAN_POINT('Ctrl Pts',(132.798871359905,32.024509433605,18.8481198671618));
#36618=CARTESIAN_POINT('Ctrl Pts',(132.711827768946,31.9426325772144,18.8423143641942));
#36619=CARTESIAN_POINT('Ctrl Pts',(132.621222576549,31.8646104899304,18.8365088612266));
#36620=CARTESIAN_POINT('Ctrl Pts',(132.527440187252,31.7907522532745,18.830703358259));
#36621=CARTESIAN_POINT('Ctrl Pts',(132.433553973492,31.7168122497553,18.824891428144));
#36622=CARTESIAN_POINT('Ctrl Pts',(132.336483862763,31.647045551026,18.8190794980291));
#36623=CARTESIAN_POINT('Ctrl Pts',(132.236644869113,31.581719038834,18.8132675679142));
#36624=CARTESIAN_POINT('Ctrl Pts',(132.136740318165,31.5163496312816,18.8074518215105));
#36625=CARTESIAN_POINT('Ctrl Pts',(132.03406361379,31.4554264245687,18.8016360751068));
#36626=CARTESIAN_POINT('Ctrl Pts',(131.929054635268,31.3991704824928,18.795820328703));
#36627=CARTESIAN_POINT('Ctrl Pts',(131.823895281049,31.3428339803865,18.7899962539932));
#36628=CARTESIAN_POINT('Ctrl Pts',(131.716397353196,31.2911782593473,18.7841721792834));
#36629=CARTESIAN_POINT('Ctrl Pts',(131.607021081889,31.2443764509253,18.7783481045735));
#36630=CARTESIAN_POINT('Ctrl Pts',(131.578018265652,31.2319662248956,18.7768037607543));
#36631=CARTESIAN_POINT('Ctrl Pts',(131.548883460521,31.2198970188987,18.7752594169352));
#36632=CARTESIAN_POINT('Ctrl Pts',(131.519625410735,31.2081714686646,18.773715073116));
#36633=CARTESIAN_POINT('Ctrl Pts',(131.409293645245,31.1639545550928,18.7678913705337));
#36634=CARTESIAN_POINT('Ctrl Pts',(131.296852536977,31.124485886127,18.7620676679513));
#36635=CARTESIAN_POINT('Ctrl Pts',(131.182748083465,31.089970336294,18.756243965369));
#36636=CARTESIAN_POINT('Ctrl Pts',(131.068787563187,31.0554983249433,18.7504276089009));
#36637=CARTESIAN_POINT('Ctrl Pts',(130.953168258269,31.0259671228756,18.7446112524328));
#36638=CARTESIAN_POINT('Ctrl Pts',(130.836356263406,31.0015336439252,18.7387948959647));
#36639=CARTESIAN_POINT('Ctrl Pts',(130.719661174336,30.9771246180736,18.7329843605235));
#36640=CARTESIAN_POINT('Ctrl Pts',(130.60177616731,30.9578032490152,18.7271738250824));
#36641=CARTESIAN_POINT('Ctrl Pts',(130.483182048679,30.9436765282051,18.7213632896412));
#36642=CARTESIAN_POINT('Ctrl Pts',(130.360102095237,30.9290154627183,18.7153329700957));
#36643=CARTESIAN_POINT('Ctrl Pts',(130.236258755539,30.919949910678,18.7093026505501));
#36644=CARTESIAN_POINT('Ctrl Pts',(130.112201061256,30.9165411815652,18.7032723310045));
#36645=CARTESIAN_POINT('Ctrl Pts',(129.99279934068,30.913260384486,18.6974683336506));
#36646=CARTESIAN_POINT('Ctrl Pts',(129.873199510158,30.9152194652718,18.6916643362967));
#36647=CARTESIAN_POINT('Ctrl Pts',(129.753895146443,30.9224201539325,18.6858603389427));
#36648=CARTESIAN_POINT('Ctrl Pts',(129.634608394418,30.9296197796288,18.680057198374));
#36649=CARTESIAN_POINT('Ctrl Pts',(129.515617429928,30.9420594498307,18.6742540578052));
#36650=CARTESIAN_POINT('Ctrl Pts',(129.397413419314,30.959688822284,18.6684509172365));
#36651=CARTESIAN_POINT('Ctrl Pts',(129.27919896491,30.9773197523619,18.6626472639374));
#36652=CARTESIAN_POINT('Ctrl Pts',(129.161772006497,31.0001412361272,18.6568436106384));
#36653=CARTESIAN_POINT('Ctrl Pts',(129.045615558698,31.0280514431579,18.6510399573393));
#36654=CARTESIAN_POINT('Ctrl Pts',(128.929421438311,31.0559707022019,18.645234421763));
#36655=CARTESIAN_POINT('Ctrl Pts',(128.814499044847,31.0889818714539,18.6394288861867));
#36656=CARTESIAN_POINT('Ctrl Pts',(128.701317603836,31.1269328647837,18.6336233506104));
#36657=CARTESIAN_POINT('Ctrl Pts',(128.588010831276,31.1649258831725,18.6278113862703));
#36658=CARTESIAN_POINT('Ctrl Pts',(128.476449246677,31.2078695145774,18.6219994219301));
#36659=CARTESIAN_POINT('Ctrl Pts',(128.367083559166,31.2555629398728,18.6161874575899));
#36660=CARTESIAN_POINT('Ctrl Pts',(128.257646040819,31.3032876899708,18.6103716759807));
#36661=CARTESIAN_POINT('Ctrl Pts',(128.150407657762,31.3557682677385,18.6045558943715));
#36662=CARTESIAN_POINT('Ctrl Pts',(128.045794427749,31.4127579421815,18.5987401127623));
#36663=CARTESIAN_POINT('Ctrl Pts',(127.9410313689,31.4698292381992,18.5929160016924));
#36664=CARTESIAN_POINT('Ctrl Pts',(127.838901315844,31.5314223105997,18.5870918906226));
#36665=CARTESIAN_POINT('Ctrl Pts',(127.739801352189,31.5972471332118,18.5812677795527));
#36666=CARTESIAN_POINT('Ctrl Pts',(127.713528570899,31.6146982109336,18.579723726551));
#36667=CARTESIAN_POINT('Ctrl Pts',(127.687468578554,31.6324465008316,18.5781796735493));
#36668=CARTESIAN_POINT('Ctrl Pts',(127.661628368802,31.6504861376001,18.5766356205475));
#36669=CARTESIAN_POINT('Ctrl Pts',(127.564645396162,31.718192151442,18.5708405108539));
#36670=CARTESIAN_POINT('Ctrl Pts',(127.470441308212,31.7902284102539,18.5650454011603));
#36671=CARTESIAN_POINT('Ctrl Pts',(127.379429631301,31.8663382533056,18.5592502914667));
#36672=CARTESIAN_POINT('Ctrl Pts',(127.288533111891,31.9423517942162,18.5534625143526));
#36673=CARTESIAN_POINT('Ctrl Pts',(127.200821284793,32.0224284072574,18.5476747372384));
#36674=CARTESIAN_POINT('Ctrl Pts',(127.11667878607,32.1062681918846,18.5418869601243));
#36675=CARTESIAN_POINT('Ctrl Pts',(127.032620235032,32.1900243308401,18.5361049573869));
#36676=CARTESIAN_POINT('Ctrl Pts',(126.952124220215,32.2775358841227,18.5303229546495));
#36677=CARTESIAN_POINT('Ctrl Pts',(126.875541831694,32.368463157297,18.5245409519122));
#36678=CARTESIAN_POINT('Ctrl Pts',(126.798745363373,32.4596446102215,18.5187427860594));
#36679=CARTESIAN_POINT('Ctrl Pts',(126.725884750906,32.5542606341769,18.5129446202066));
#36680=CARTESIAN_POINT('Ctrl Pts',(126.657276560392,32.6519316436068,18.5071464543538));
#36681=CARTESIAN_POINT('Ctrl Pts',(126.588934008571,32.7492244882857,18.5013707379664));
#36682=CARTESIAN_POINT('Ctrl Pts',(126.52481124611,32.8495483631417,18.4955950215789));
#36683=CARTESIAN_POINT('Ctrl Pts',(126.465179972521,32.9524960626813,18.4898193051915));
#36684=CARTESIAN_POINT('Ctrl Pts',(126.405556689024,33.055429968092,18.4840443627017));
#36685=CARTESIAN_POINT('Ctrl Pts',(126.350423904548,33.1609866418927,18.4782694202119));
#36686=CARTESIAN_POINT('Ctrl Pts',(126.300008551479,33.268732175292,18.4724944777221));
#36687=CARTESIAN_POINT('Ctrl Pts',(126.249587741316,33.3764893713586,18.4667189101369));
#36688=CARTESIAN_POINT('Ctrl Pts',(126.203885552365,33.4864355239355,18.4609433425517));
#36689=CARTESIAN_POINT('Ctrl Pts',(126.163081447441,33.5981151898151,18.4551677749666));
#36690=CARTESIAN_POINT('Ctrl Pts',(126.121997103856,33.7105618608782,18.4493525413398));
#36691=CARTESIAN_POINT('Ctrl Pts',(126.08587853268,33.8247655513889,18.443537307713));
#36692=CARTESIAN_POINT('Ctrl Pts',(126.054858023747,33.9402454118026,18.4377220740862));
#36693=CARTESIAN_POINT('Ctrl Pts',(126.02400421083,34.0551047139662,18.431938089988));
#36694=CARTESIAN_POINT('Ctrl Pts',(125.998193836137,34.1712260861413,18.4261541058898));
#36695=CARTESIAN_POINT('Ctrl Pts',(125.977505562765,34.2881267652104,18.4203701217916));
#36696=CARTESIAN_POINT('Ctrl Pts',(125.956649628456,34.4059748252858,18.4145392634005));
#36697=CARTESIAN_POINT('Ctrl Pts',(125.940999236854,34.5246144548944,18.4087084050094));
#36698=CARTESIAN_POINT('Ctrl Pts',(125.930581533309,34.6435475586353,18.4028775466183));
#36699=CARTESIAN_POINT('Ctrl Pts',(125.920163829764,34.7624806623761,18.3970466882272));
#36700=CARTESIAN_POINT('Ctrl Pts',(125.914978771819,34.8817068147453,18.3912158298361));
#36701=CARTESIAN_POINT('Ctrl Pts',(125.915000065372,35.0007308119611,18.3853849714449));
#36702=CARTESIAN_POINT('Ctrl Pts',(125.915000065372,35.0007308127869,18.3853849714045));
#36703=CARTESIAN_POINT('Ctrl Pts',(125.915007160729,35.040391496008,18.3834420369294));
#36704=CARTESIAN_POINT('Ctrl Pts',(125.915591831772,35.0800463838246,18.3814991024543));
#36705=CARTESIAN_POINT('Ctrl Pts',(125.916753658372,35.119684224453,18.3795561679791));
#36706=CARTESIAN_POINT('Ctrl Pts',(125.920236583737,35.2385105970872,18.3737316363627));
#36707=CARTESIAN_POINT('Ctrl Pts',(125.928916363599,35.3573761657475,18.3679071047463));
#36708=CARTESIAN_POINT('Ctrl Pts',(125.942802843878,35.4757901179652,18.3620825731299));
#36709=CARTESIAN_POINT('Ctrl Pts',(125.956671800716,35.5940546428387,18.3562653915282));
#36710=CARTESIAN_POINT('Ctrl Pts',(125.975734342444,35.7118682829417,18.3504482099265));
#36711=CARTESIAN_POINT('Ctrl Pts',(125.999948318737,35.8287409409616,18.3446310283248));
#36712=CARTESIAN_POINT('Ctrl Pts',(126.024138044988,35.9454965522483,18.338819672569));
#36713=CARTESIAN_POINT('Ctrl Pts',(126.053468859994,36.061312658808,18.3330083168133));
#36714=CARTESIAN_POINT('Ctrl Pts',(126.087846967805,36.1757055977941,18.3271969610575));
#36715=CARTESIAN_POINT('Ctrl Pts',(126.12351856505,36.2944026147938,18.3211669508223));
#36716=CARTESIAN_POINT('Ctrl Pts',(126.164624676602,36.4115668212268,18.315136940587));
#36717=CARTESIAN_POINT('Ctrl Pts',(126.211002489441,36.5266705161822,18.3091069303517));
#36718=CARTESIAN_POINT('Ctrl Pts',(126.255648177386,36.6374753026025,18.303302129763));
#36719=CARTESIAN_POINT('Ctrl Pts',(126.305178684521,36.7463703179019,18.2974973291744));
#36720=CARTESIAN_POINT('Ctrl Pts',(126.359398611619,36.8529021914066,18.2916925285857));
#36721=CARTESIAN_POINT('Ctrl Pts',(126.413610464331,36.9594182002729,18.2858885924432));
#36722=CARTESIAN_POINT('Ctrl Pts',(126.4725101631,37.0635714035169,18.2800846563006));
#36723=CARTESIAN_POINT('Ctrl Pts',(126.535855522528,37.1649314167436,18.2742807201581));
#36724=CARTESIAN_POINT('Ctrl Pts',(126.599206385276,37.2663002359281,18.268476279781));
#36725=CARTESIAN_POINT('Ctrl Pts',(126.667003460254,37.3648750364461,18.2626718394039));
#36726=CARTESIAN_POINT('Ctrl Pts',(126.738960601225,37.4602534502846,18.2568673990269));
#36727=CARTESIAN_POINT('Ctrl Pts',(126.810940960867,37.5556626402207,18.25106108571));
#36728=CARTESIAN_POINT('Ctrl Pts',(126.887083810414,37.6478730665739,18.2452547723932));
#36729=CARTESIAN_POINT('Ctrl Pts',(126.967062420869,37.7365150540593,18.2394484590764));
#36730=CARTESIAN_POINT('Ctrl Pts',(127.047129340469,37.8252549164404,18.2336357346633));
#36731=CARTESIAN_POINT('Ctrl Pts',(127.131040201393,37.9104181718577,18.2278230102503));
#36732=CARTESIAN_POINT('Ctrl Pts',(127.218430974147,37.991671565265,18.2220102858372));
#36733=CARTESIAN_POINT('Ctrl Pts',(127.305878995919,38.0729781871409,18.2161937535535));
#36734=CARTESIAN_POINT('Ctrl Pts',(127.39681115944,38.1503695820478,18.2103772212697));
#36735=CARTESIAN_POINT('Ctrl Pts',(127.490831181968,38.2235534496289,18.2045606889859));
#36736=CARTESIAN_POINT('Ctrl Pts',(127.58498553022,38.2968418744708,18.1987358466646));
#36737=CARTESIAN_POINT('Ctrl Pts',(127.6822362112,38.365910538259,18.1929110043434));
#36738=CARTESIAN_POINT('Ctrl Pts',(127.782158781132,38.4305109426864,18.1870861620221));
#36739=CARTESIAN_POINT('Ctrl Pts',(127.808516447484,38.4475512961048,18.1855496798183));
#36740=CARTESIAN_POINT('Ctrl Pts',(127.83505989868,38.4642809979911,18.1840131976145));
#36741=CARTESIAN_POINT('Ctrl Pts',(127.861781087519,38.4806960341731,18.1824767154107));
#36742=CARTESIAN_POINT('Ctrl Pts',(127.96306915626,38.5429180903552,18.1766525989758));
#36743=CARTESIAN_POINT('Ctrl Pts',(128.067238419904,38.6008153648951,18.1708284825408));
#36744=CARTESIAN_POINT('Ctrl Pts',(128.173883774923,38.6541106349578,18.1650043661059));
#36745=CARTESIAN_POINT('Ctrl Pts',(128.280394791564,38.7073387703559,18.1591875861589));
#36746=CARTESIAN_POINT('Ctrl Pts',(128.389375333819,38.7559762505954,18.1533708062119));
#36747=CARTESIAN_POINT('Ctrl Pts',(128.500392399092,38.799789736722,18.1475540262648));
#36748=CARTESIAN_POINT('Ctrl Pts',(128.611298537879,38.8435594451104,18.1417430583518));
#36749=CARTESIAN_POINT('Ctrl Pts',(128.724236773994,38.8825145993402,18.1359320904387));
#36750=CARTESIAN_POINT('Ctrl Pts',(128.838751182359,38.9164685857959,18.1301211225256));
#36751=CARTESIAN_POINT('Ctrl Pts',(128.957585137217,38.9517033353034,18.1240909617055));
#36752=CARTESIAN_POINT('Ctrl Pts',(129.07811611319,38.981551993627,18.1180608008853));
#36753=CARTESIAN_POINT('Ctrl Pts',(129.19981338699,39.0058615033922,18.1120306400652));
#36754=CARTESIAN_POINT('Ctrl Pts',(129.316955478314,39.0292610975165,18.1062261908164));
#36755=CARTESIAN_POINT('Ctrl Pts',(129.435177690273,39.0475286695622,18.1004217415676));
#36756=CARTESIAN_POINT('Ctrl Pts',(129.55399375061,39.0605791982801,18.0946172923188));
#36757=CARTESIAN_POINT('Ctrl Pts',(129.672792402414,39.073627814878,18.0888136935185));
#36758=CARTESIAN_POINT('Ctrl Pts',(129.79218432387,39.0814608637114,18.0830100947182));
#36759=CARTESIAN_POINT('Ctrl Pts',(129.911676830767,39.0840450557966,18.0772064959179));
#36760=CARTESIAN_POINT('Ctrl Pts',(130.031180013947,39.0866294787713,18.0714023785842));
#36761=CARTESIAN_POINT('Ctrl Pts',(130.150783392269,39.0839641037346,18.0655982612505));
#36762=CARTESIAN_POINT('Ctrl Pts',(130.269993626076,39.0760677670861,18.0597941439168));
#36763=CARTESIAN_POINT('Ctrl Pts',(130.389242628115,39.0681688624785,18.0539881390323));
#36764=CARTESIAN_POINT('Ctrl Pts',(130.508097824223,39.0550356399889,18.0481821341479));
#36765=CARTESIAN_POINT('Ctrl Pts',(130.62607098278,39.0367387981539,18.0423761292634));
#36766=CARTESIAN_POINT('Ctrl Pts',(130.744174877349,39.0184216800444,18.036563690255));
#36767=CARTESIAN_POINT('Ctrl Pts',(130.861394379612,38.994929583096,18.0307512512465));
#36768=CARTESIAN_POINT('Ctrl Pts',(130.977251281277,38.9663843652933,18.0249388122381));
#36769=CARTESIAN_POINT('Ctrl Pts',(131.093184344101,38.9378203826447,18.0191225522911));
#36770=CARTESIAN_POINT('Ctrl Pts',(131.207752631618,38.9041967783932,18.0133062923442));
#36771=CARTESIAN_POINT('Ctrl Pts',(131.320494520823,38.8656848320156,18.0074900323972));
#36772=CARTESIAN_POINT('Ctrl Pts',(131.433397899752,38.827117721727,18.0016654413302));
#36773=CARTESIAN_POINT('Ctrl Pts',(131.544469279945,38.7836484419674,17.9958408502633));
#36774=CARTESIAN_POINT('Ctrl Pts',(131.653268246692,38.7354958311422,17.9900162591963));
#36775=CARTESIAN_POINT('Ctrl Pts',(131.682028035717,38.7227672274637,17.988476593745));
#36776=CARTESIAN_POINT('Ctrl Pts',(131.710629181738,38.7097116203617,17.9869369282936));
#36777=CARTESIAN_POINT('Ctrl Pts',(131.739063868762,38.6963335699539,17.9853972628422));
#36778=CARTESIAN_POINT('Ctrl Pts',(131.846528305251,38.6457733282606,17.9795783389351));
#36779=CARTESIAN_POINT('Ctrl Pts',(131.951961213614,38.5904402353699,17.9737594150281));
#36780=CARTESIAN_POINT('Ctrl Pts',(132.054909090144,38.5305203060235,17.967940491121));
#36781=CARTESIAN_POINT('Ctrl Pts',(132.157711917597,38.4706848012496,17.9621297658244));
#36782=CARTESIAN_POINT('Ctrl Pts',(132.258036329994,38.4062755242499,17.9563190405279));
#36783=CARTESIAN_POINT('Ctrl Pts',(132.355450358798,38.3375258212094,17.9505083152313));
#36784=CARTESIAN_POINT('Ctrl Pts',(132.399974678273,38.3061028959946,17.9478524494114));
#36785=CARTESIAN_POINT('Ctrl Pts',(132.443891305796,38.2737738779582,17.9451965835914));
#36786=CARTESIAN_POINT('Ctrl Pts',(132.487160689988,38.2405642567579,17.9425407177715));
#36787=CARTESIAN_POINT('',(125.915000466471,34.998047803468,18.4896150286331));
#36788=CARTESIAN_POINT('Ctrl Pts',(125.915000466471,34.9980478042441,18.4896150285955));
#36789=CARTESIAN_POINT('Ctrl Pts',(125.914942432928,35.1194838827728,18.483727517173));
#36790=CARTESIAN_POINT('Ctrl Pts',(125.920303700289,35.2409117170285,18.4778400057506));
#36791=CARTESIAN_POINT('Ctrl Pts',(125.931055605702,35.3618238744374,18.4719524943281));
#36792=CARTESIAN_POINT('Ctrl Pts',(125.941810869906,35.482773803618,18.4660631437048));
#36793=CARTESIAN_POINT('Ctrl Pts',(125.957960090728,35.6032073451722,18.4601737930816));
#36794=CARTESIAN_POINT('Ctrl Pts',(125.979422790103,35.7226229302054,18.4542844424583));
#36795=CARTESIAN_POINT('Ctrl Pts',(126.000896649805,35.8421006098063,18.4483920294485));
#36796=CARTESIAN_POINT('Ctrl Pts',(126.027689420367,35.9605588938576,18.4424996164387));
#36797=CARTESIAN_POINT('Ctrl Pts',(126.059669749903,36.0775075499385,18.4366072034289));
#36798=CARTESIAN_POINT('Ctrl Pts',(126.091695456131,36.1946221437388,18.430706429711));
#36799=CARTESIAN_POINT('Ctrl Pts',(126.128923319468,36.3102224531799,18.424805655993));
#36800=CARTESIAN_POINT('Ctrl Pts',(126.171172255081,36.4238339438785,18.4189048822751));
#36801=CARTESIAN_POINT('Ctrl Pts',(126.213453803262,36.5375331329366,18.4129995536643));
#36802=CARTESIAN_POINT('Ctrl Pts',(126.260763995858,36.6492400836464,18.4070942250534));
#36803=CARTESIAN_POINT('Ctrl Pts',(126.312874497657,36.75850235427,18.4011888964426));
#36804=CARTESIAN_POINT('Ctrl Pts',(126.365076841081,36.8679571930732,18.3952731600453));
#36805=CARTESIAN_POINT('Ctrl Pts',(126.422096212423,36.9749583984458,18.389357423648));
#36806=CARTESIAN_POINT('Ctrl Pts',(126.483659079887,37.0790794918762,18.3834416872507));
#36807=CARTESIAN_POINT('Ctrl Pts',(126.522265549195,37.1443744978332,18.3797318909878));
#36808=CARTESIAN_POINT('Ctrl Pts',(126.562657939128,37.2085374477177,18.3760220947248));
#36809=CARTESIAN_POINT('Ctrl Pts',(126.604760614711,37.2714696820741,18.3723122984619));
#36810=CARTESIAN_POINT('Ctrl Pts',(126.670854131373,37.3702618044849,18.3664885953902));
#36811=CARTESIAN_POINT('Ctrl Pts',(126.741369638143,37.4663260767103,18.3606648923186));
#36812=CARTESIAN_POINT('Ctrl Pts',(126.816054720177,37.5592415781028,18.3548411892469));
#36813=CARTESIAN_POINT('Ctrl Pts',(126.890645593262,37.652039874407,18.3490248322867));
#36814=CARTESIAN_POINT('Ctrl Pts',(126.969395326886,37.7416969844718,18.3432084753265));
#36815=CARTESIAN_POINT('Ctrl Pts',(127.052007838526,37.8278202234029,18.3373921183664));
#36816=CARTESIAN_POINT('Ctrl Pts',(127.134537671353,37.9138572699768,18.3315815824311));
#36817=CARTESIAN_POINT('Ctrl Pts',(127.220922310471,37.9963671882897,18.3257710464958));
#36818=CARTESIAN_POINT('Ctrl Pts',(127.310825342853,38.0749901891484,18.3199605105605));
#36819=CARTESIAN_POINT('Ctrl Pts',(127.40412895595,38.1565871037164,18.3139301911993));
#36820=CARTESIAN_POINT('Ctrl Pts',(127.501222103233,38.2339969004973,18.3078998718382));
#36821=CARTESIAN_POINT('Ctrl Pts',(127.601686269053,38.3068589700728,18.3018695524771));
#36822=CARTESIAN_POINT('Ctrl Pts',(127.698379954332,38.3769864823738,18.2960655546269));
#36823=CARTESIAN_POINT('Ctrl Pts',(127.798195825115,38.4429012124677,18.2902615567767));
#36824=CARTESIAN_POINT('Ctrl Pts',(127.900727493049,38.5043230361313,18.2844575589266));
#36825=CARTESIAN_POINT('Ctrl Pts',(128.003244025274,38.5657357927145,18.2786544178617));
#36826=CARTESIAN_POINT('Ctrl Pts',(128.108475207192,38.6226567520707,18.2728512767968));
#36827=CARTESIAN_POINT('Ctrl Pts',(128.215987237424,38.67485012796,18.2670481357319));
#36828=CARTESIAN_POINT('Ctrl Pts',(128.323508766756,38.7270481153337,18.2612444819373));
#36829=CARTESIAN_POINT('Ctrl Pts',(128.433311177737,38.77451751042,18.2554408281427));
#36830=CARTESIAN_POINT('Ctrl Pts',(128.544938324261,38.8170696246983,18.2496371743481));
#36831=CARTESIAN_POINT('Ctrl Pts',(128.656601674374,38.8596355397352,18.2438316382774));
#36832=CARTESIAN_POINT('Ctrl Pts',(128.770090555666,38.8972808568925,18.2380261022068));
#36833=CARTESIAN_POINT('Ctrl Pts',(128.884931825912,38.9298661513004,18.2322205661361));
#36834=CARTESIAN_POINT('Ctrl Pts',(128.999900265625,38.9624875290299,18.2264086013059));
#36835=CARTESIAN_POINT('Ctrl Pts',(129.116223690522,38.9900375879859,18.2205966364756));
#36836=CARTESIAN_POINT('Ctrl Pts',(129.233416723662,39.0124275794635,18.2147846716453));
#36837=CARTESIAN_POINT('Ctrl Pts',(129.350686728555,39.0348322765668,18.2089688895479));
#36838=CARTESIAN_POINT('Ctrl Pts',(129.468827076049,39.0520700978789,18.2031531074504));
#36839=CARTESIAN_POINT('Ctrl Pts',(129.587346843827,39.0641041291656,18.197337325353));
#36840=CARTESIAN_POINT('Ctrl Pts',(129.706036357474,39.0761553957803,18.1915132138014));
#36841=CARTESIAN_POINT('Ctrl Pts',(129.825105969824,39.0829879733735,18.1856891022498));
#36842=CARTESIAN_POINT('Ctrl Pts',(129.944064192394,39.0846170182071,18.1798649906981));
#36843=CARTESIAN_POINT('Ctrl Pts',(129.97560157555,39.085048899333,18.1783209424299));
#36844=CARTESIAN_POINT('Ctrl Pts',(130.007131156836,39.0851153331897,18.1767768941617));
#36845=CARTESIAN_POINT('Ctrl Pts',(130.038643852423,39.0848172116595,18.1752328458935));
#36846=CARTESIAN_POINT('Ctrl Pts',(130.157465235959,39.0836931182737,18.1694108764283));
#36847=CARTESIAN_POINT('Ctrl Pts',(130.276429348989,39.0773783961636,18.1635889069632));
#36848=CARTESIAN_POINT('Ctrl Pts',(130.395046143852,39.0658533599022,18.157766937498));
#36849=CARTESIAN_POINT('Ctrl Pts',(130.513522752562,39.0543419443973,18.1519518486731));
#36850=CARTESIAN_POINT('Ctrl Pts',(130.631652456621,39.037632497184,18.1461367598482));
#36851=CARTESIAN_POINT('Ctrl Pts',(130.748944759515,39.0157573068096,18.1403216710233));
#36852=CARTESIAN_POINT('Ctrl Pts',(130.866126151197,38.9939028015426,18.1345120809271));
#36853=CARTESIAN_POINT('Ctrl Pts',(130.982471317448,38.9668923420503,18.1287024908309));
#36854=CARTESIAN_POINT('Ctrl Pts',(131.097495075478,38.934809977534,18.1228929007347));
#36855=CARTESIAN_POINT('Ctrl Pts',(131.212437236041,38.9027503721395,18.1170874319422));
#36856=CARTESIAN_POINT('Ctrl Pts',(131.326059461223,38.8656261288792,18.1112819631497));
#36857=CARTESIAN_POINT('Ctrl Pts',(131.437887584763,38.8235721901886,18.1054764943573));
#36858=CARTESIAN_POINT('Ctrl Pts',(131.54967089478,38.7815351040131,18.0996733520235));
#36859=CARTESIAN_POINT('Ctrl Pts',(131.659661151168,38.7345723942665,18.0938702096897));
#36860=CARTESIAN_POINT('Ctrl Pts',(131.767400673247,38.6828684283051,18.0880670673559));
#36861=CARTESIAN_POINT('Ctrl Pts',(131.875115437006,38.6311763438082,18.0822652585723));
#36862=CARTESIAN_POINT('Ctrl Pts',(131.980580129119,38.57474535076,18.0764634497886));
#36863=CARTESIAN_POINT('Ctrl Pts',(132.083359010499,38.513807085395,18.0706616410049));
#36864=CARTESIAN_POINT('Ctrl Pts',(132.186158212569,38.4528567717608,18.0648586851299));
#36865=CARTESIAN_POINT('Ctrl Pts',(132.286270192468,38.3873976150219,18.059055729255));
#36866=CARTESIAN_POINT('Ctrl Pts',(132.383286005582,38.3177059567715,18.05325277338));
#36867=CARTESIAN_POINT('Ctrl Pts',(132.418320472563,38.2925388214203,18.051157202983));
#36868=CARTESIAN_POINT('Ctrl Pts',(132.452951454051,38.2668201369431,18.0490616325861));
#36869=CARTESIAN_POINT('Ctrl Pts',(132.487160689988,38.2405642567579,18.0469660621892));
#36870=CARTESIAN_POINT('Ctrl Pts',(132.487160689988,38.2405642567579,19.2967873935987));
#36871=CARTESIAN_POINT('Ctrl Pts',(132.581876183315,38.1678693082642,19.2909824695503));
#36872=CARTESIAN_POINT('Ctrl Pts',(132.673459504492,38.0909741961783,19.2851775455019));
#36873=CARTESIAN_POINT('Ctrl Pts',(132.761523565565,38.0101848110752,19.2793726214535));
#36874=CARTESIAN_POINT('Ctrl Pts',(132.849563259112,37.9294177805789,19.2735693036408));
#36875=CARTESIAN_POINT('Ctrl Pts',(132.934085328219,37.8447588955322,19.2677659858281));
#36876=CARTESIAN_POINT('Ctrl Pts',(133.014736884083,37.7565533769093,19.2619626680154));
#36877=CARTESIAN_POINT('Ctrl Pts',(133.095385157486,37.6683514481887,19.2561595863937));
#36878=CARTESIAN_POINT('Ctrl Pts',(133.172162955497,37.5766034744098,19.250356504772));
#36879=CARTESIAN_POINT('Ctrl Pts',(133.244755734828,37.4816899929886,19.2445534231502));
#36880=CARTESIAN_POINT('Ctrl Pts',(133.317362691672,37.3867579747784,19.2387492081752));
#36881=CARTESIAN_POINT('Ctrl Pts',(133.385782756442,37.2886595438449,19.2329449932002));
#36882=CARTESIAN_POINT('Ctrl Pts',(133.449743394979,37.1878060948816,19.2271407782253));
#36883=CARTESIAN_POINT('Ctrl Pts',(133.513770844082,37.0868472986892,19.2213305004138));
#36884=CARTESIAN_POINT('Ctrl Pts',(133.573329344478,36.983128082249,19.2155202226024));
#36885=CARTESIAN_POINT('Ctrl Pts',(133.628191099959,36.8770866634695,19.209709944791));
#36886=CARTESIAN_POINT('Ctrl Pts',(133.683082542347,36.7709878633391,19.2038965229101));
#36887=CARTESIAN_POINT('Ctrl Pts',(133.733272005007,36.6625647278601,19.1980831010292));
#36888=CARTESIAN_POINT('Ctrl Pts',(133.778579578207,36.5522761903602,19.1922696791483));
#36889=CARTESIAN_POINT('Ctrl Pts',(133.823958933984,36.4418129183755,19.1864470468335));
#36890=CARTESIAN_POINT('Ctrl Pts',(133.864440809216,36.3294787240977,19.1806244145188));
#36891=CARTESIAN_POINT('Ctrl Pts',(133.899894803097,36.2157489563125,19.1748017822041));
#36892=CARTESIAN_POINT('Ctrl Pts',(133.928658564759,36.1234801996423,19.1700778910479));
#36893=CARTESIAN_POINT('Ctrl Pts',(133.954113891697,36.0302932286143,19.1653539998918));
#36894=CARTESIAN_POINT('Ctrl Pts',(133.976216024986,35.9364460062615,19.1606301087357));
#36895=CARTESIAN_POINT('Ctrl Pts',(134.003463478975,35.8207513880271,19.1548065076723));
#36896=CARTESIAN_POINT('Ctrl Pts',(134.025701189063,35.7036800028105,19.1489829066089));
#36897=CARTESIAN_POINT('Ctrl Pts',(134.042793156527,35.5857034177309,19.1431593055455));
#36898=CARTESIAN_POINT('Ctrl Pts',(134.059863559811,35.4678756784928,19.1373430518622));
#36899=CARTESIAN_POINT('Ctrl Pts',(134.071801075186,35.3491454114585,19.1315267981788));
#36900=CARTESIAN_POINT('Ctrl Pts',(134.078520127143,35.229996896702,19.1257105444954));
#36901=CARTESIAN_POINT('Ctrl Pts',(134.085232453231,35.1109676513335,19.1199001129661));
#36902=CARTESIAN_POINT('Ctrl Pts',(134.086736685061,34.991521396484,19.1140896814369));
#36903=CARTESIAN_POINT('Ctrl Pts',(134.0829988062,34.872149506973,19.1082792499076));
#36904=CARTESIAN_POINT('Ctrl Pts',(134.079119447524,34.7482593563155,19.1022488918351));
#36905=CARTESIAN_POINT('Ctrl Pts',(134.069593242631,34.6244497553083,19.0962185337626));
#36906=CARTESIAN_POINT('Ctrl Pts',(134.054441532323,34.5012727589446,19.0901881756901));
#36907=CARTESIAN_POINT('Ctrl Pts',(134.039858836088,34.3827216063255,19.0843842843686));
#36908=CARTESIAN_POINT('Ctrl Pts',(134.020065594881,34.2647568426569,19.0785803930471));
#36909=CARTESIAN_POINT('Ctrl Pts',(133.995133781885,34.1478667564042,19.0727765017256));
#36910=CARTESIAN_POINT('Ctrl Pts',(133.970205651937,34.0309939377167,19.0669734677828));
#36911=CARTESIAN_POINT('Ctrl Pts',(133.940140544955,33.9151958799733,19.0611704338401));
#36912=CARTESIAN_POINT('Ctrl Pts',(133.905061562992,33.8009507144231,19.0553673998973));
#36913=CARTESIAN_POINT('Ctrl Pts',(133.86997948447,33.6866954640075,19.0495638536981));
#36914=CARTESIAN_POINT('Ctrl Pts',(133.829882770845,33.5739937687013,19.043760307499));
#36915=CARTESIAN_POINT('Ctrl Pts',(133.784944218305,33.4633080125401,19.0379567612998));
#36916=CARTESIAN_POINT('Ctrl Pts',(133.739991093487,33.3525863641815,19.0321513331781));
#36917=CARTESIAN_POINT('Ctrl Pts',(133.690193160771,33.243882333199,19.0263459050563));
#36918=CARTESIAN_POINT('Ctrl Pts',(133.635770850116,33.1376371660055,19.0205404769345));
#36919=CARTESIAN_POINT('Ctrl Pts',(133.581288273529,33.0312743455166,19.0147286200239));
#36920=CARTESIAN_POINT('Ctrl Pts',(133.522171283474,32.927376187576,19.0089167631132));
#36921=CARTESIAN_POINT('Ctrl Pts',(133.458685732184,32.8263583538243,19.0031049062026));
#36922=CARTESIAN_POINT('Ctrl Pts',(133.395158484336,32.7252741727576,18.9972892321333));
#36923=CARTESIAN_POINT('Ctrl Pts',(133.327257192831,32.6270744184652,18.991473558064));
#36924=CARTESIAN_POINT('Ctrl Pts',(133.255289420561,32.5321434830236,18.9856578839946));
#36925=CARTESIAN_POINT('Ctrl Pts',(133.183218564689,32.437076572513,18.979833879799));
#36926=CARTESIAN_POINT('Ctrl Pts',(133.107069862149,32.3452881392585,18.9740098756034));
#36927=CARTESIAN_POINT('Ctrl Pts',(133.027189365608,32.2571275011857,18.9681858714078));
#36928=CARTESIAN_POINT('Ctrl Pts',(133.005997571408,32.2337390374252,18.9666407996609));
#36929=CARTESIAN_POINT('Ctrl Pts',(132.984543319394,32.210605687761,18.9650957279141));
#36930=CARTESIAN_POINT('Ctrl Pts',(132.962833467122,32.1877335037192,18.9635506561672));
#36931=CARTESIAN_POINT('Ctrl Pts',(132.881005719069,32.1015247497516,18.9577270448391));
#36932=CARTESIAN_POINT('Ctrl Pts',(132.795280312383,32.0187513282001,18.9519034335109));
#36933=CARTESIAN_POINT('Ctrl Pts',(132.705977105291,31.9397854804535,18.9460798221827));
#36934=CARTESIAN_POINT('Ctrl Pts',(132.616786565085,31.8609192577542,18.9402635580505));
#36935=CARTESIAN_POINT('Ctrl Pts',(132.524027505579,31.7858513224785,18.9344472939182));
#36936=CARTESIAN_POINT('Ctrl Pts',(132.428058057757,31.7149187120923,18.928631029786));
#36937=CARTESIAN_POINT('Ctrl Pts',(132.332184673777,31.6440571040848,18.9228205876386));
#36938=CARTESIAN_POINT('Ctrl Pts',(132.233107620922,31.5773228274695,18.9170101454913));
#36939=CARTESIAN_POINT('Ctrl Pts',(132.131219226661,31.5150136861229,18.911199703344));
#36940=CARTESIAN_POINT('Ctrl Pts',(132.02547458861,31.4503462856131,18.9051693491879));
#36941=CARTESIAN_POINT('Ctrl Pts',(131.916701934944,31.390445897466,18.8991389950319));
#36942=CARTESIAN_POINT('Ctrl Pts',(131.805374685602,31.335597286789,18.8931086408758));
#36943=CARTESIAN_POINT('Ctrl Pts',(131.698227997263,31.2828083512071,18.8873047385864));
#36944=CARTESIAN_POINT('Ctrl Pts',(131.588715513263,31.2346988224533,18.881500836297));
#36945=CARTESIAN_POINT('Ctrl Pts',(131.477285079027,31.1914761658506,18.8756969340076));
#36946=CARTESIAN_POINT('Ctrl Pts',(131.365871103701,31.1482598934805,18.8698938889876));
#36947=CARTESIAN_POINT('Ctrl Pts',(131.252540122111,31.1099292054201,18.8640908439676));
#36948=CARTESIAN_POINT('Ctrl Pts',(131.137759511339,31.0766432364164,18.8582877989476));
#36949=CARTESIAN_POINT('Ctrl Pts',(131.022968766545,31.0433543285821,18.8524842415746));
#36950=CARTESIAN_POINT('Ctrl Pts',(130.906728530291,31.015111139103,18.8466806842017));
#36951=CARTESIAN_POINT('Ctrl Pts',(130.789520249559,30.9920226079061,18.8408771268287));
#36952=CARTESIAN_POINT('Ctrl Pts',(130.672273959939,30.9689265894446,18.8350716874491));
#36953=CARTESIAN_POINT('Ctrl Pts',(130.554059401948,30.9509886325373,18.8292662480694));
#36954=CARTESIAN_POINT('Ctrl Pts',(130.435366454686,30.9382662507085,18.8234608086898));
#36955=CARTESIAN_POINT('Ctrl Pts',(130.316542068664,30.925529780308,18.8176489404551));
#36956=CARTESIAN_POINT('Ctrl Pts',(130.197238642173,30.9180204572198,18.8118370722204));
#36957=CARTESIAN_POINT('Ctrl Pts',(130.077949554722,30.9157437804517,18.8060252039858));
#36958=CARTESIAN_POINT('Ctrl Pts',(129.958582118705,30.913465608372,18.8002095185407));
#36959=CARTESIAN_POINT('Ctrl Pts',(129.839229447754,30.9164269169426,18.7943938330956));
#36960=CARTESIAN_POINT('Ctrl Pts',(129.72038163265,30.9245811787449,18.7885781476506));
#36961=CARTESIAN_POINT('Ctrl Pts',(129.601363585529,30.932747120328,18.7827541320914));
#36962=CARTESIAN_POINT('Ctrl Pts',(129.482852241905,30.946120815644,18.7769301165323));
#36963=CARTESIAN_POINT('Ctrl Pts',(129.365329456219,30.9646043191706,18.7711061009732));
#36964=CARTESIAN_POINT('Ctrl Pts',(129.334153597955,30.9695075307717,18.7695611351817));
#36965=CARTESIAN_POINT('Ctrl Pts',(129.303047230723,30.9747700493633,18.7680161693902));
#36966=CARTESIAN_POINT('Ctrl Pts',(129.272019173074,30.98038945722,18.7664712035988));
#36967=CARTESIAN_POINT('Ctrl Pts',(129.155063459534,31.0015709911399,18.7606476815923));
#36968=CARTESIAN_POINT('Ctrl Pts',(129.038844342866,31.0278953878007,18.7548241595859));
#36969=CARTESIAN_POINT('Ctrl Pts',(128.923848478047,31.0592991864645,18.7490006375794));
#36970=CARTESIAN_POINT('Ctrl Pts',(128.808997700956,31.0906633636534,18.7431844629813));
#36971=CARTESIAN_POINT('Ctrl Pts',(128.695367496481,31.1270940897332,18.7373682883832));
#36972=CARTESIAN_POINT('Ctrl Pts',(128.583436056807,31.1684765960723,18.731552113785));
#36973=CARTESIAN_POINT('Ctrl Pts',(128.471616662397,31.209817677823,18.725741761276));
#36974=CARTESIAN_POINT('Ctrl Pts',(128.361493030679,31.2561005380775,18.7199314087669));
#36975=CARTESIAN_POINT('Ctrl Pts',(128.253529286087,31.3071603006027,18.7141210562579));
#36976=CARTESIAN_POINT('Ctrl Pts',(128.141477007272,31.3601536713711,18.7080906685401));
#36977=CARTESIAN_POINT('Ctrl Pts',(128.031751869413,31.4182927759754,18.7020602808223));
#36978=CARTESIAN_POINT('Ctrl Pts',(127.924851574246,31.4813377526267,18.6960298931045));
#36979=CARTESIAN_POINT('Ctrl Pts',(127.821967755206,31.5420139926597,18.6902260801428));
#36980=CARTESIAN_POINT('Ctrl Pts',(127.721700721023,31.607233881173,18.6844222671811));
#36981=CARTESIAN_POINT('Ctrl Pts',(127.624469472989,31.6767365865402,18.6786184542194));
#36982=CARTESIAN_POINT('Ctrl Pts',(127.527252582283,31.7462290290226,18.6728154982583));
#36983=CARTESIAN_POINT('Ctrl Pts',(127.433070918374,31.8200027932999,18.6670125422973));
#36984=CARTESIAN_POINT('Ctrl Pts',(127.342313766925,31.8977542188724,18.6612095863362));
#36985=CARTESIAN_POINT('Ctrl Pts',(127.251548596664,31.9755125141414,18.6554061176573));
#36986=CARTESIAN_POINT('Ctrl Pts',(127.164208850573,32.0572489037796,18.6496026489784));
#36987=CARTESIAN_POINT('Ctrl Pts',(127.080649545393,32.1426204446752,18.6437991802994));
#36988=CARTESIAN_POINT('Ctrl Pts',(126.997063136129,32.2280196774902,18.6379938291526));
#36989=CARTESIAN_POINT('Ctrl Pts',(126.917259892013,32.3170561149127,18.6321884780057));
#36990=CARTESIAN_POINT('Ctrl Pts',(126.84155644026,32.40935157153,18.6263831268588));
#36991=CARTESIAN_POINT('Ctrl Pts',(126.765769139704,32.5017492541796,18.6205713457312));
#36992=CARTESIAN_POINT('Ctrl Pts',(126.694090954679,32.5974128453291,18.6147595646035));
#36993=CARTESIAN_POINT('Ctrl Pts',(126.626796927584,32.6959327196799,18.6089477834759));
#36994=CARTESIAN_POINT('Ctrl Pts',(126.559458694985,32.7945173118204,18.6031321845842));
#36995=CARTESIAN_POINT('Ctrl Pts',(126.496510570627,32.8959615776701,18.5973165856926));
#36996=CARTESIAN_POINT('Ctrl Pts',(126.438182280427,32.9998301240808,18.5915009868009));
#36997=CARTESIAN_POINT('Ctrl Pts',(126.379770427547,33.1038474753693,18.5856770563256));
#36998=CARTESIAN_POINT('Ctrl Pts',(126.325991802468,33.2102956761344,18.5798531258504));
#36999=CARTESIAN_POINT('Ctrl Pts',(126.277028611372,33.3187180368966,18.5740291953751));
#37000=CARTESIAN_POINT('Ctrl Pts',(126.264032572894,33.3474960054232,18.5724833805935));
#37001=CARTESIAN_POINT('Ctrl Pts',(126.251375512216,33.3764129658833,18.5709375658119));
#37002=CARTESIAN_POINT('Ctrl Pts',(126.23906024573,33.4054602028317,18.5693917510304));
#37003=CARTESIAN_POINT('Ctrl Pts',(126.186096181761,33.5303831768987,18.5627436908306));
#37004=CARTESIAN_POINT('Ctrl Pts',(126.139308119113,33.6580710664456,18.5560956306308));
#37005=CARTESIAN_POINT('Ctrl Pts',(126.098961571862,33.7879256696925,18.549447570431));
#37006=CARTESIAN_POINT('Ctrl Pts',(126.059996556184,33.913333839565,18.5430271506538));
#37007=CARTESIAN_POINT('Ctrl Pts',(126.027039357914,34.040762517582,18.5366067308765));
#37008=CARTESIAN_POINT('Ctrl Pts',(126.000282123105,34.169649528663,18.5301863110992));
#37009=CARTESIAN_POINT('Ctrl Pts',(125.973599397814,34.298177634609,18.5237837699399));
#37010=CARTESIAN_POINT('Ctrl Pts',(125.953082277172,34.4281557287952,18.5173812287806));
#37011=CARTESIAN_POINT('Ctrl Pts',(125.93887329776,34.5590069066826,18.5109786876212));
#37012=CARTESIAN_POINT('Ctrl Pts',(125.924722847556,34.6893190862678,18.5046025196201));
#37013=CARTESIAN_POINT('Ctrl Pts',(125.916828775928,34.8204969250766,18.4982263516189));
#37014=CARTESIAN_POINT('Ctrl Pts',(125.915282546901,34.9519549342306,18.4918501836178));
#37015=CARTESIAN_POINT('Ctrl Pts',(125.915101870904,34.9673157290102,18.4911051319563));
#37016=CARTESIAN_POINT('Ctrl Pts',(125.915007810492,34.9826803339909,18.4903600802947));
#37017=CARTESIAN_POINT('Ctrl Pts',(125.915000466471,34.998047803468,18.4896150286331));
#37018=CARTESIAN_POINT('Origin',(130.,35.,32.7603849714045));
#37019=CARTESIAN_POINT('',(132.487160689988,38.2405642567579,20.546920386683));
#37020=CARTESIAN_POINT('',(132.487160689988,38.2405642567579,20.4426725202732));
#37021=CARTESIAN_POINT('',(132.487160689988,38.2405642567579,32.7603849714045));
#37022=CARTESIAN_POINT('',(125.915000768169,35.0025051829245,19.6353849713624));
#37023=CARTESIAN_POINT('Ctrl Pts',(132.487160689988,38.2405642567579,20.4426725202732));
#37024=CARTESIAN_POINT('Ctrl Pts',(132.581973835524,38.1677943593616,20.4368690147981));
#37025=CARTESIAN_POINT('Ctrl Pts',(132.673580961777,38.0908673687084,20.431065509323));
#37026=CARTESIAN_POINT('Ctrl Pts',(132.76160895586,38.0101064723553,20.4252620038479));
#37027=CARTESIAN_POINT('Ctrl Pts',(132.849664893768,37.9293199390622,20.4194566560935));
#37028=CARTESIAN_POINT('Ctrl Pts',(132.934139139189,37.8446973555699,20.4136513083391));
#37029=CARTESIAN_POINT('Ctrl Pts',(133.014694994994,37.7565991887033,20.4078459605848));
#37030=CARTESIAN_POINT('Ctrl Pts',(133.09533980489,37.6684037391209,20.4020342022544));
#37031=CARTESIAN_POINT('Ctrl Pts',(133.172057312327,37.5767253466558,20.396222443924));
#37032=CARTESIAN_POINT('Ctrl Pts',(133.244550630625,37.4819581393143,20.3904106855936));
#37033=CARTESIAN_POINT('Ctrl Pts',(133.317091117818,37.3871292702292,20.3845951457531));
#37034=CARTESIAN_POINT('Ctrl Pts',(133.385401708896,37.2892079178341,20.3787796059127));
#37035=CARTESIAN_POINT('Ctrl Pts',(133.449229365947,37.1886164079366,20.3729640660722));
#37036=CARTESIAN_POINT('Ctrl Pts',(133.513148940274,37.0878800376765,20.3671401513578));
#37037=CARTESIAN_POINT('Ctrl Pts',(133.572572491666,36.9844661874427,20.3613162366434));
#37038=CARTESIAN_POINT('Ctrl Pts',(133.627293266933,36.8788210547205,20.355492321929));
#37039=CARTESIAN_POINT('Ctrl Pts',(133.643396632603,36.8477315426449,20.3537784458405));
#37040=CARTESIAN_POINT('Ctrl Pts',(133.659093048241,36.8164489212308,20.352064569752));
#37041=CARTESIAN_POINT('Ctrl Pts',(133.674378053835,36.7849848507742,20.3503506936635));
#37042=CARTESIAN_POINT('Ctrl Pts',(133.726315092397,36.678072842759,20.3445271008653));
#37043=CARTESIAN_POINT('Ctrl Pts',(133.773665842193,36.568719760455,20.3387035080672));
#37044=CARTESIAN_POINT('Ctrl Pts',(133.816194276692,36.4573559079866,20.332879915269));
#37045=CARTESIAN_POINT('Ctrl Pts',(133.858669055247,36.3461325575771,20.3270636697991));
#37046=CARTESIAN_POINT('Ctrl Pts',(133.896333475179,36.2329038609136,20.3212474243291));
#37047=CARTESIAN_POINT('Ctrl Pts',(133.928997921923,36.118123575246,20.3154311788592));
#37048=CARTESIAN_POINT('Ctrl Pts',(133.961629671378,36.0034581852706,20.3096207554827));
#37049=CARTESIAN_POINT('Ctrl Pts',(133.989271293348,35.8872446865745,20.3038103321063));
#37050=CARTESIAN_POINT('Ctrl Pts',(134.011781924604,35.7699550567527,20.2979999087298));
#37051=CARTESIAN_POINT('Ctrl Pts',(134.035144634587,35.6482257469733,20.2919695475783));
#37052=CARTESIAN_POINT('Ctrl Pts',(134.052980079561,35.5253376470726,20.2859391864269));
#37053=CARTESIAN_POINT('Ctrl Pts',(134.065188110961,35.4018340733461,20.2799088252754));
#37054=CARTESIAN_POINT('Ctrl Pts',(134.076937654419,35.2829688313354,20.2741049419055));
#37055=CARTESIAN_POINT('Ctrl Pts',(134.083474806991,35.163533954478,20.2683010585356));
#37056=CARTESIAN_POINT('Ctrl Pts',(134.084762795526,35.0440216342746,20.2624971751656));
#37057=CARTESIAN_POINT('Ctrl Pts',(134.086050593813,34.9245269672265,20.2566941490869));
#37058=CARTESIAN_POINT('Ctrl Pts',(134.082090765599,34.8049552877843,20.2508911230081));
#37059=CARTESIAN_POINT('Ctrl Pts',(134.072898649705,34.685800080789,20.2450880969293));
#37060=CARTESIAN_POINT('Ctrl Pts',(134.063705722235,34.5666343535193,20.2392845584984));
#37061=CARTESIAN_POINT('Ctrl Pts',(134.049279620003,34.4478855789528,20.2334810200674));
#37062=CARTESIAN_POINT('Ctrl Pts',(134.029687618859,34.3300427667274,20.2276774816365));
#37063=CARTESIAN_POINT('Ctrl Pts',(134.010089264234,34.2121617393149,20.2218720611789));
#37064=CARTESIAN_POINT('Ctrl Pts',(133.985321745944,34.0951876611345,20.2160666407214));
#37065=CARTESIAN_POINT('Ctrl Pts',(133.955503447749,33.9795993557207,20.2102612202639));
#37066=CARTESIAN_POINT('Ctrl Pts',(133.925652128473,33.8638830466644,20.2044493708258));
#37067=CARTESIAN_POINT('Ctrl Pts',(133.89073896668,33.749555969232,20.1986375213877));
#37068=CARTESIAN_POINT('Ctrl Pts',(133.850932270771,33.6370819371911,20.1928256719496));
#37069=CARTESIAN_POINT('Ctrl Pts',(133.81109942956,33.5245340314549,20.18701000525));
#37070=CARTESIAN_POINT('Ctrl Pts',(133.766366805904,33.4138419727021,20.1811943385504));
#37071=CARTESIAN_POINT('Ctrl Pts',(133.716950257121,33.3054482049546,20.1753786718509));
#37072=CARTESIAN_POINT('Ctrl Pts',(133.667462924315,33.1968991745076,20.1695546748189));
#37073=CARTESIAN_POINT('Ctrl Pts',(133.613278459981,33.0906553683099,20.1637306777869));
#37074=CARTESIAN_POINT('Ctrl Pts',(133.554657961418,32.9871334427427,20.157906680755));
#37075=CARTESIAN_POINT('Ctrl Pts',(133.53910553912,32.9596683623857,20.1563615342017));
#37076=CARTESIAN_POINT('Ctrl Pts',(133.523241105127,32.9323947026958,20.1548163876484));
#37077=CARTESIAN_POINT('Ctrl Pts',(133.507070025083,32.9053198718738,20.1532712410951));
#37078=CARTESIAN_POINT('Ctrl Pts',(133.446121885334,32.8032759410962,20.1474476468882));
#37079=CARTESIAN_POINT('Ctrl Pts',(133.380618063269,32.7037297433222,20.1416240526814));
#37080=CARTESIAN_POINT('Ctrl Pts',(133.310789071845,32.6071145615065,20.1358004584745));
#37081=CARTESIAN_POINT('Ctrl Pts',(133.241048180136,32.5106212741907,20.1299842116026));
#37082=CARTESIAN_POINT('Ctrl Pts',(133.166993209696,32.4170519757968,20.1241679647307));
#37083=CARTESIAN_POINT('Ctrl Pts',(133.088899730347,32.3268139877923,20.1183517178588));
#37084=CARTESIAN_POINT('Ctrl Pts',(133.010884423089,32.2366663286133,20.1125412930887));
#37085=CARTESIAN_POINT('Ctrl Pts',(132.9288389148,32.149843652915,20.1067308683186));
#37086=CARTESIAN_POINT('Ctrl Pts',(132.843080737974,32.0667224956783,20.1009204435484));
#37087=CARTESIAN_POINT('Ctrl Pts',(132.754076447697,31.9804550412993,20.0948900829225));
#37088=CARTESIAN_POINT('Ctrl Pts',(132.661073134668,31.8981752246436,20.0888597222966));
#37089=CARTESIAN_POINT('Ctrl Pts',(132.564470314927,31.8202646330463,20.0828293616707));
#37090=CARTESIAN_POINT('Ctrl Pts',(132.471495505365,31.7452800473365,20.0770254769364));
#37091=CARTESIAN_POINT('Ctrl Pts',(132.375187025588,31.6743427036232,20.071221592202));
#37092=CARTESIAN_POINT('Ctrl Pts',(132.275936372796,31.6077531594853,20.0654177074677));
#37093=CARTESIAN_POINT('Ctrl Pts',(132.17670038053,31.5411734514312,20.0596146800376));
#37094=CARTESIAN_POINT('Ctrl Pts',(132.074523418519,31.4789404932156,20.0538116526075));
#37095=CARTESIAN_POINT('Ctrl Pts',(131.969826631561,31.4213119664334,20.0480086251774));
#37096=CARTESIAN_POINT('Ctrl Pts',(131.865120601135,31.3636783517444,20.0422050854096));
#37097=CARTESIAN_POINT('Ctrl Pts',(131.757894661182,31.3106501736544,20.0364015456419));
#37098=CARTESIAN_POINT('Ctrl Pts',(131.648594683564,31.2624392219892,20.0305980058741));
#37099=CARTESIAN_POINT('Ctrl Pts',(131.539259261419,31.2142126361546,20.0247925840957));
#37100=CARTESIAN_POINT('Ctrl Pts',(131.427848837409,31.170806548242,20.0189871623173));
#37101=CARTESIAN_POINT('Ctrl Pts',(131.31482877954,31.1323844192456,20.013181740539));
#37102=CARTESIAN_POINT('Ctrl Pts',(131.201683562745,31.093919741409,20.0073698898101));
#37103=CARTESIAN_POINT('Ctrl Pts',(131.086925540872,31.0604501709099,20.0015580390813));
#37104=CARTESIAN_POINT('Ctrl Pts',(130.971034895071,31.0320891854081,19.9957461883525));
#37105=CARTESIAN_POINT('Ctrl Pts',(130.855068131856,31.003709572304,19.9899305203781));
#37106=CARTESIAN_POINT('Ctrl Pts',(130.737967662783,30.9804453058232,19.9841148524038));
#37107=CARTESIAN_POINT('Ctrl Pts',(130.62022186056,30.9623583809749,19.9782991844295));
#37108=CARTESIAN_POINT('Ctrl Pts',(130.502307400535,30.9442455486129,19.9724751861559));
#37109=CARTESIAN_POINT('Ctrl Pts',(130.383746166865,30.9313249038325,19.9666511878823));
#37110=CARTESIAN_POINT('Ctrl Pts',(130.265029763147,30.9236064683784,19.9608271896087));
#37111=CARTESIAN_POINT('Ctrl Pts',(130.233533751851,30.9215587317335,19.9592820559146));
#37112=CARTESIAN_POINT('Ctrl Pts',(130.202026806011,30.9198768764323,19.9577369222206));
#37113=CARTESIAN_POINT('Ctrl Pts',(130.170518062656,30.9185604757257,19.9561917885266));
#37114=CARTESIAN_POINT('Ctrl Pts',(130.051761867873,30.9135989722801,19.9503681923312));
#37115=CARTESIAN_POINT('Ctrl Pts',(129.932597446704,30.913816880325,19.9445445961357));
#37116=CARTESIAN_POINT('Ctrl Pts',(129.813513543656,30.9192589151478,19.9387209999403));
#37117=CARTESIAN_POINT('Ctrl Pts',(129.694579882291,30.9246940840514,19.9329047510593));
#37118=CARTESIAN_POINT('Ctrl Pts',(129.575726941313,30.9353402519184,19.9270885021784));
#37119=CARTESIAN_POINT('Ctrl Pts',(129.457446450288,30.9511902186328,19.9212722532974));
#37120=CARTESIAN_POINT('Ctrl Pts',(129.339284358416,30.9670243194793,19.9154618265004));
#37121=CARTESIAN_POINT('Ctrl Pts',(129.221693978929,30.9880518025519,19.9096513997034));
#37122=CARTESIAN_POINT('Ctrl Pts',(129.105164294844,31.0142134953341,19.9038409729064));
#37123=CARTESIAN_POINT('Ctrl Pts',(128.984223793319,31.0413654461064,19.8978106130335));
#37124=CARTESIAN_POINT('Ctrl Pts',(128.864426319196,31.0740479401577,19.8917802531607));
#37125=CARTESIAN_POINT('Ctrl Pts',(128.746310020765,31.1121360059841,19.8857498932878));
#37126=CARTESIAN_POINT('Ctrl Pts',(128.632629637027,31.1487936560838,19.8799460064956));
#37127=CARTESIAN_POINT('Ctrl Pts',(128.520506854986,31.1904580455362,19.8741421197033));
#37128=CARTESIAN_POINT('Ctrl Pts',(128.410407657071,31.2369664918712,19.868338232911));
#37129=CARTESIAN_POINT('Ctrl Pts',(128.300324721989,31.2834680684093,19.8625352034151));
#37130=CARTESIAN_POINT('Ctrl Pts',(128.192265152654,31.3348121200356,19.8567321739192));
#37131=CARTESIAN_POINT('Ctrl Pts',(128.08667532298,31.3907876648352,19.8509291444233));
#37132=CARTESIAN_POINT('Ctrl Pts',(127.981076170894,31.4467681516547,19.8451256025843));
#37133=CARTESIAN_POINT('Ctrl Pts',(127.877947552801,31.507380753393,19.8393220607452));
#37134=CARTESIAN_POINT('Ctrl Pts',(127.777711014526,31.5723686509429,19.8335185189062));
#37135=CARTESIAN_POINT('Ctrl Pts',(127.677441970831,31.6373776232314,19.8277130950533));
#37136=CARTESIAN_POINT('Ctrl Pts',(127.580067214605,31.7067644910825,19.8219076712003));
#37137=CARTESIAN_POINT('Ctrl Pts',(127.485978557904,31.7802296372751,19.8161022473474));
#37138=CARTESIAN_POINT('Ctrl Pts',(127.391785707129,31.8537761390013,19.8102903945498));
#37139=CARTESIAN_POINT('Ctrl Pts',(127.300886541748,31.9314096825366,19.8044785417523));
#37140=CARTESIAN_POINT('Ctrl Pts',(127.213639189223,32.0127908623322,19.7986666889547));
#37141=CARTESIAN_POINT('Ctrl Pts',(127.126334532342,32.0942254935615,19.7928510189126));
#37142=CARTESIAN_POINT('Ctrl Pts',(127.042686750473,32.1794123724234,19.7870353488705));
#37143=CARTESIAN_POINT('Ctrl Pts',(126.96301540279,32.2679770212694,19.7812196788284));
#37144=CARTESIAN_POINT('Ctrl Pts',(126.883229935017,32.3566685288428,19.7753956785043));
#37145=CARTESIAN_POINT('Ctrl Pts',(126.807432528508,32.4487471491802,19.7695716781802));
#37146=CARTESIAN_POINT('Ctrl Pts',(126.735901044559,32.543807212556,19.7637476778561));
#37147=CARTESIAN_POINT('Ctrl Pts',(126.716923659823,32.5690267564012,19.7622025638901));
#37148=CARTESIAN_POINT('Ctrl Pts',(126.69824628613,32.5944560030195,19.7606574499241));
#37149=CARTESIAN_POINT('Ctrl Pts',(126.679873574968,32.6200870768437,19.7591123359582));
#37150=CARTESIAN_POINT('Ctrl Pts',(126.610112055718,32.7174087314556,19.7532455100591));
#37151=CARTESIAN_POINT('Ctrl Pts',(126.544521954283,32.8179553758546,19.7473786841601));
#37152=CARTESIAN_POINT('Ctrl Pts',(126.483412466926,32.9213376603614,19.7415118582611));
#37153=CARTESIAN_POINT('Ctrl Pts',(126.422382087734,33.0245861132317,19.7356526271537));
#37154=CARTESIAN_POINT('Ctrl Pts',(126.365820987408,33.130662563725,19.7297933960463));
#37155=CARTESIAN_POINT('Ctrl Pts',(126.313996696666,33.2391466137661,19.7239341649389));
#37156=CARTESIAN_POINT('Ctrl Pts',(126.262227894924,33.3475145084027,19.7180812073931));
#37157=CARTESIAN_POINT('Ctrl Pts',(126.215185984125,33.4582845152963,19.7122282498472));
#37158=CARTESIAN_POINT('Ctrl Pts',(126.173093649867,33.5710098715147,19.7063752923013));
#37159=CARTESIAN_POINT('Ctrl Pts',(126.130548943581,33.6849467024306,19.7004594322266));
#37160=CARTESIAN_POINT('Ctrl Pts',(126.093061051587,33.800880808957,19.6945435721518));
#37161=CARTESIAN_POINT('Ctrl Pts',(126.06081105525,33.9183274721267,19.6886277120771));
#37162=CARTESIAN_POINT('Ctrl Pts',(126.028952030982,34.0343503098646,19.682783570958));
#37163=CARTESIAN_POINT('Ctrl Pts',(126.002204712039,34.1518488359259,19.6769394298389));
#37164=CARTESIAN_POINT('Ctrl Pts',(125.980694158516,34.2703387411867,19.6710952887198));
#37165=CARTESIAN_POINT('Ctrl Pts',(125.958787640624,34.3910097981563,19.6651435691673));
#37166=CARTESIAN_POINT('Ctrl Pts',(125.942312718303,34.5127086884001,19.6591918496147));
#37167=CARTESIAN_POINT('Ctrl Pts',(125.931347179938,34.6349120245762,19.6532401300621));
#37168=CARTESIAN_POINT('Ctrl Pts',(125.920381641572,34.7571153607523,19.6472884105096));
#37169=CARTESIAN_POINT('Ctrl Pts',(125.91492553145,34.8798227059536,19.641336690957));
#37170=CARTESIAN_POINT('Ctrl Pts',(125.915000768169,35.002505182056,19.6353849714045));
#37171=CARTESIAN_POINT('Ctrl Pts',(125.915000768169,35.0025051829244,19.6353849713624));
#37172=CARTESIAN_POINT('Ctrl Pts',(125.915083357689,35.137177234539,19.6288515991299));
#37173=CARTESIAN_POINT('Ctrl Pts',(125.921829701157,35.271602954508,19.6223182268974));
#37174=CARTESIAN_POINT('Ctrl Pts',(125.935142558203,35.4051653710125,19.6157848546649));
#37175=CARTESIAN_POINT('Ctrl Pts',(125.948507987173,35.5392552199948,19.6092256824147));
#37176=CARTESIAN_POINT('Ctrl Pts',(125.968491780739,35.6724747379491,19.6026665101645));
#37177=CARTESIAN_POINT('Ctrl Pts',(125.994945663421,35.8042168619514,19.5961073379143));
#37178=CARTESIAN_POINT('Ctrl Pts',(126.021539621793,35.9366565723635,19.5895134342565));
#37179=CARTESIAN_POINT('Ctrl Pts',(126.054672268095,36.0676030087451,19.5829195305986));
#37180=CARTESIAN_POINT('Ctrl Pts',(126.094144257802,36.1964597448879,19.5763256269407));
#37181=CARTESIAN_POINT('Ctrl Pts',(126.122663682996,36.2895617160448,19.5715613790904));
#37182=CARTESIAN_POINT('Ctrl Pts',(126.154491475474,36.3815731981222,19.5667971312401));
#37183=CARTESIAN_POINT('Ctrl Pts',(126.189537223157,36.4722766133754,19.5620328833897));
#37184=CARTESIAN_POINT('Ctrl Pts',(126.23237555976,36.5831483650317,19.5562092823377));
#37185=CARTESIAN_POINT('Ctrl Pts',(126.280125989353,36.6923276736055,19.5503856812857));
#37186=CARTESIAN_POINT('Ctrl Pts',(126.332634487451,36.7993485480485,19.5445620802337));
#37187=CARTESIAN_POINT('Ctrl Pts',(126.385076737899,36.9062343989887,19.5387458265615));
#37188=CARTESIAN_POINT('Ctrl Pts',(126.442264938661,37.0109668688231,19.5329295728893));
#37189=CARTESIAN_POINT('Ctrl Pts',(126.503996270988,37.1130979453719,19.5271133192172));
#37190=CARTESIAN_POINT('Ctrl Pts',(126.56566580936,37.2151267872377,19.5213028876989));
#37191=CARTESIAN_POINT('Ctrl Pts',(126.631869222121,37.3145590687665,19.5154924561807));
#37192=CARTESIAN_POINT('Ctrl Pts',(126.7023571311,37.410970034902,19.5096820246624));
#37193=CARTESIAN_POINT('Ctrl Pts',(126.775513028367,37.5110301847367,19.5036516665857));
#37194=CARTESIAN_POINT('Ctrl Pts',(126.853283971465,37.6078353825645,19.497621308509));
#37195=CARTESIAN_POINT('Ctrl Pts',(126.93534063123,37.7009420492502,19.4915909504323));
#37196=CARTESIAN_POINT('Ctrl Pts',(127.014315698474,37.7905521465116,19.4857870591213));
#37197=CARTESIAN_POINT('Ctrl Pts',(127.097260097391,37.8767361619249,19.4799831678102));
#37198=CARTESIAN_POINT('Ctrl Pts',(127.183838715792,37.9591317343657,19.4741792764992));
#37199=CARTESIAN_POINT('Ctrl Pts',(127.270404544387,38.04151513494,19.4683762425667));
#37200=CARTESIAN_POINT('Ctrl Pts',(127.360603229098,38.1201109240758,19.4625732086341));
#37201=CARTESIAN_POINT('Ctrl Pts',(127.454063194637,38.1945939934676,19.4567701747016));
#37202=CARTESIAN_POINT('Ctrl Pts',(127.547531410255,38.2690836377729,19.4509666285124));
#37203=CARTESIAN_POINT('Ctrl Pts',(127.644261159742,38.3394595860072,19.4451630823233));
#37204=CARTESIAN_POINT('Ctrl Pts',(127.743848745212,38.4054377861764,19.4393595361341));
#37205=CARTESIAN_POINT('Ctrl Pts',(127.843468624067,38.4714373811751,19.4335541080221));
#37206=CARTESIAN_POINT('Ctrl Pts',(127.945947841699,38.5330361665828,19.4277486799101));
#37207=CARTESIAN_POINT('Ctrl Pts',(128.050855321786,38.5899944322228,19.4219432517981));
#37208=CARTESIAN_POINT('Ctrl Pts',(128.155878973854,38.6470157720548,19.4161313948968));
#37209=CARTESIAN_POINT('Ctrl Pts',(128.263335896781,38.6993861396859,19.4103195379955));
#37210=CARTESIAN_POINT('Ctrl Pts',(128.372771972104,38.746912588416,19.4045076810943));
#37211=CARTESIAN_POINT('Ctrl Pts',(128.482279923749,38.7944702519559,19.3986920070341));
#37212=CARTESIAN_POINT('Ctrl Pts',(128.593769236102,38.8371775149667,19.3928763329739));
#37213=CARTESIAN_POINT('Ctrl Pts',(128.70676902177,38.8748907903252,19.3870606589137));
#37214=CARTESIAN_POINT('Ctrl Pts',(128.819930663574,38.9126580845915,19.3812366547268));
#37215=CARTESIAN_POINT('Ctrl Pts',(128.934606705762,38.945417002089,19.37541265054));
#37216=CARTESIAN_POINT('Ctrl Pts',(129.050314298558,38.9730746366606,19.3695886463531));
#37217=CARTESIAN_POINT('Ctrl Pts',(129.081010798426,38.980412033935,19.3680435745092));
#37218=CARTESIAN_POINT('Ctrl Pts',(129.1117798641,38.9873906812343,19.3664985026652));
#37219=CARTESIAN_POINT('Ctrl Pts',(129.142612418835,38.994009456131,19.3649534308213));
#37220=CARTESIAN_POINT('Ctrl Pts',(129.258835029318,39.0189587768508,19.3591293178138));
#37221=CARTESIAN_POINT('Ctrl Pts',(129.376334977682,39.0388711371857,19.3533052048063));
#37222=CARTESIAN_POINT('Ctrl Pts',(129.494637966386,39.0536198902934,19.3474810917988));
#37223=CARTESIAN_POINT('Ctrl Pts',(129.612789294764,39.0683497360112,19.3416644451021));
#37224=CARTESIAN_POINT('Ctrl Pts',(129.731741213936,39.0779290916249,19.3358477984054));
#37225=CARTESIAN_POINT('Ctrl Pts',(129.851007742483,39.0822819975107,19.3300311517087));
#37226=CARTESIAN_POINT('Ctrl Pts',(129.970134823259,39.0866298139298,19.324221305901));
#37227=CARTESIAN_POINT('Ctrl Pts',(130.089575375356,39.0857633314435,19.3184114600933));
#37228=CARTESIAN_POINT('Ctrl Pts',(130.208837595067,39.0796583017315,19.3126016142855));
#37229=CARTESIAN_POINT('Ctrl Pts',(130.328021353255,39.0735572884627,19.3067955907223));
#37230=CARTESIAN_POINT('Ctrl Pts',(130.447026606094,39.0622246020963,19.300989567159));
#37231=CARTESIAN_POINT('Ctrl Pts',(130.565361077398,39.0456880567047,19.2951835435957));
#37232=CARTESIAN_POINT('Ctrl Pts',(130.68364562509,39.0291584878439,19.2893799695103));
#37233=CARTESIAN_POINT('Ctrl Pts',(130.801259550487,39.0074294834135,19.2835763954249));
#37234=CARTESIAN_POINT('Ctrl Pts',(130.917715867536,38.9805806845827,19.2777728213395));
#37235=CARTESIAN_POINT('Ctrl Pts',(131.034150536512,38.9537368766769,19.2719703260808));
#37236=CARTESIAN_POINT('Ctrl Pts',(131.149427627894,38.9217752605688,19.2661678308222));
#37237=CARTESIAN_POINT('Ctrl Pts',(131.263071145331,38.8848264159204,19.2603653355635));
#37238=CARTESIAN_POINT('Ctrl Pts',(131.37676781597,38.847860289605,19.2545601263691));
#37239=CARTESIAN_POINT('Ctrl Pts',(131.488828995976,38.8059023962963,19.2487549171747));
#37240=CARTESIAN_POINT('Ctrl Pts',(131.598794668697,38.7591329595196,19.2429497079803));
#37241=CARTESIAN_POINT('Ctrl Pts',(131.708783845301,38.7123535263197,19.23714325799));
#37242=CARTESIAN_POINT('Ctrl Pts',(131.816676250757,38.6607606708509,19.2313368079997));
#37243=CARTESIAN_POINT('Ctrl Pts',(131.922033903607,38.6045818999415,19.2255303580094));
#37244=CARTESIAN_POINT('Ctrl Pts',(132.027506875214,38.5483416388044,19.2197175525946));
#37245=CARTESIAN_POINT('Ctrl Pts',(132.130439195344,38.4875056352456,19.2139047471799));
#37246=CARTESIAN_POINT('Ctrl Pts',(132.2304191985,38.4223464463672,19.2080919417651));
#37247=CARTESIAN_POINT('Ctrl Pts',(132.318370565114,38.3650265871113,19.2029784774328));
#37248=CARTESIAN_POINT('Ctrl Pts',(132.404037544159,38.304361979733,19.1978650131004));
#37249=CARTESIAN_POINT('Ctrl Pts',(132.487160689988,38.2405642567579,19.1927515487681));
#37250=CARTESIAN_POINT('',(125.915000261184,34.9985392205114,19.7396150285596));
#37251=CARTESIAN_POINT('Ctrl Pts',(125.915000261184,34.9985392205114,19.7396150285596));
#37252=CARTESIAN_POINT('Ctrl Pts',(125.914958122368,35.1163783992937,19.7338448931807));
#37253=CARTESIAN_POINT('Ctrl Pts',(125.920019141926,35.2344196377308,19.7280747578017));
#37254=CARTESIAN_POINT('Ctrl Pts',(125.93020956506,35.3521800898317,19.7223046224228));
#37255=CARTESIAN_POINT('Ctrl Pts',(125.940387587581,35.4697972405372,19.716541508658));
#37256=CARTESIAN_POINT('Ctrl Pts',(125.95568256745,35.5871338729639,19.7107783948932));
#37257=CARTESIAN_POINT('Ctrl Pts',(125.976068747181,35.7037060981617,19.7050152811284));
#37258=CARTESIAN_POINT('Ctrl Pts',(125.996435680781,35.8201682701516,19.6992576081893));
#37259=CARTESIAN_POINT('Ctrl Pts',(126.021884184085,35.9358670620511,19.6934999352502));
#37260=CARTESIAN_POINT('Ctrl Pts',(126.05233666646,36.0503233811675,19.6877422623111));
#37261=CARTESIAN_POINT('Ctrl Pts',(126.082770032881,36.1647078525486,19.6819882036395));
#37262=CARTESIAN_POINT('Ctrl Pts',(126.118201025284,36.2778510007493,19.6762341449679));
#37263=CARTESIAN_POINT('Ctrl Pts',(126.158501038498,36.3892842505328,19.6704800862964));
#37264=CARTESIAN_POINT('Ctrl Pts',(126.198788206548,36.5006819822548,19.6647278616646));
#37265=CARTESIAN_POINT('Ctrl Pts',(126.243941169226,36.6103705075494,19.6589756370328));
#37266=CARTESIAN_POINT('Ctrl Pts',(126.293781763915,36.717897373685,19.6532234124009));
#37267=CARTESIAN_POINT('Ctrl Pts',(126.343618775968,36.8254165105849,19.64747160125));
#37268=CARTESIAN_POINT('Ctrl Pts',(126.398142574683,36.930773919495,19.641719790099));
#37269=CARTESIAN_POINT('Ctrl Pts',(126.457127560654,37.0335387575654,19.6359679789481));
#37270=CARTESIAN_POINT('Ctrl Pts',(126.516122868011,37.1363215777649,19.6302151613263));
#37271=CARTESIAN_POINT('Ctrl Pts',(126.579580706571,37.2365105644042,19.6244623437045));
#37272=CARTESIAN_POINT('Ctrl Pts',(126.647230782592,37.3337016893336,19.6187095260827));
#37273=CARTESIAN_POINT('Ctrl Pts',(126.714949685714,37.4309916963915,19.6129508555515));
#37274=CARTESIAN_POINT('Ctrl Pts',(126.786869104481,37.5252774092623,19.6071921850203));
#37275=CARTESIAN_POINT('Ctrl Pts',(126.86267680895,37.6161858104691,19.6014335144891));
#37276=CARTESIAN_POINT('Ctrl Pts',(126.938525657696,37.7071435517858,19.5956717184663));
#37277=CARTESIAN_POINT('Ctrl Pts',(127.018266713924,37.7947200239878,19.5899099224436));
#37278=CARTESIAN_POINT('Ctrl Pts',(127.101550292612,37.8785785196416,19.5841481264209));
#37279=CARTESIAN_POINT('Ctrl Pts',(127.184962488914,37.9625665207726,19.578377432264));
#37280=CARTESIAN_POINT('Ctrl Pts',(127.271927827361,38.0428247965871,19.5726067381072));
#37281=CARTESIAN_POINT('Ctrl Pts',(127.362062681504,38.1190562200269,19.5668360439503));
#37282=CARTESIAN_POINT('Ctrl Pts',(127.424785193413,38.172103694391,19.5628203672577));
#37283=CARTESIAN_POINT('Ctrl Pts',(127.489041833165,38.2232020634187,19.5588046905651));
#37284=CARTESIAN_POINT('Ctrl Pts',(127.554695457864,38.2722638488067,19.5547890138726));
#37285=CARTESIAN_POINT('Ctrl Pts',(127.649907355902,38.3434140058528,19.548965417665));
#37286=CARTESIAN_POINT('Ctrl Pts',(127.748380712973,38.4105199278196,19.5431418214574));
#37287=CARTESIAN_POINT('Ctrl Pts',(127.849737400486,38.4732687418528,19.5373182252498));
#37288=CARTESIAN_POINT('Ctrl Pts',(127.950966211782,38.5359383891217,19.5315019763567));
#37289=CARTESIAN_POINT('Ctrl Pts',(128.055070774009,38.594261649066,19.5256857274635));
#37290=CARTESIAN_POINT('Ctrl Pts',(128.161641181065,38.6479668108197,19.5198694785704));
#37291=CARTESIAN_POINT('Ctrl Pts',(128.268104910799,38.7016182135334,19.5140590517611));
#37292=CARTESIAN_POINT('Ctrl Pts',(128.377029212391,38.7506605317018,19.5082486249519));
#37293=CARTESIAN_POINT('Ctrl Pts',(128.487977100522,38.7948664998198,19.5024381981426));
#37294=CARTESIAN_POINT('Ctrl Pts',(128.603124526696,38.8407457277713,19.4964078382744));
#37295=CARTESIAN_POINT('Ctrl Pts',(128.720451376436,38.8814150100987,19.4903774784061));
#37296=CARTESIAN_POINT('Ctrl Pts',(128.839442933545,38.9166736263699,19.4843471185378));
#37297=CARTESIAN_POINT('Ctrl Pts',(128.953965705526,38.9506080883576,19.4785432317333));
#37298=CARTESIAN_POINT('Ctrl Pts',(129.070029975251,38.9795308293925,19.4727393449288));
#37299=CARTESIAN_POINT('Ctrl Pts',(129.187159294016,39.0033130013397,19.4669354581243));
#37300=CARTESIAN_POINT('Ctrl Pts',(129.304271311523,39.0270916604047,19.4611324286162));
#37301=CARTESIAN_POINT('Ctrl Pts',(129.422447665148,39.0457311791947,19.4553293991081));
#37302=CARTESIAN_POINT('Ctrl Pts',(129.541200817629,39.0591536445737,19.4495263696));
#37303=CARTESIAN_POINT('Ctrl Pts',(129.659964454696,39.0725772950075,19.4437228277488));
#37304=CARTESIAN_POINT('Ctrl Pts',(129.779304586097,39.0807829303666,19.4379192858975));
#37305=CARTESIAN_POINT('Ctrl Pts',(129.898728284197,39.083744487548,19.4321157440463));
#37306=CARTESIAN_POINT('Ctrl Pts',(130.018190709863,39.0867070051242,19.4263103201812));
#37307=CARTESIAN_POINT('Ctrl Pts',(130.137736348122,39.0844220523211,19.4205048963161));
#37308=CARTESIAN_POINT('Ctrl Pts',(130.256872645791,39.0769156777942,19.4146994724511));
#37309=CARTESIAN_POINT('Ctrl Pts',(130.376140875368,39.0694009906848,19.4088876196415));
#37310=CARTESIAN_POINT('Ctrl Pts',(130.494998451751,39.0566533657399,19.4030757668319));
#37311=CARTESIAN_POINT('Ctrl Pts',(130.612958156422,39.0387507101176,19.3972639140223));
#37312=CARTESIAN_POINT('Ctrl Pts',(130.730995337425,39.0208362959708,19.3914482439682));
#37313=CARTESIAN_POINT('Ctrl Pts',(130.848133072549,38.9977601869015,19.3856325739142));
#37314=CARTESIAN_POINT('Ctrl Pts',(130.963896171616,38.9696510136715,19.3798169038601));
#37315=CARTESIAN_POINT('Ctrl Pts',(131.079825088075,38.9415015772678,19.3739929035243));
#37316=CARTESIAN_POINT('Ctrl Pts',(131.194375047637,38.9083048006121,19.3681689031884));
#37317=CARTESIAN_POINT('Ctrl Pts',(131.307087662258,38.8702386028736,19.3623449028525));
#37318=CARTESIAN_POINT('Ctrl Pts',(131.33699044588,38.8601395977345,19.360799789003));
#37319=CARTESIAN_POINT('Ctrl Pts',(131.366764028469,38.8496981178781,19.3592546751536));
#37320=CARTESIAN_POINT('Ctrl Pts',(131.39640012409,38.8389180368224,19.3577095613041));
#37321=CARTESIAN_POINT('Ctrl Pts',(131.508084011547,38.7982932063865,19.3518867861492));
#37322=CARTESIAN_POINT('Ctrl Pts',(131.618173684637,38.7527250769583,19.3460640109944));
#37323=CARTESIAN_POINT('Ctrl Pts',(131.726200385228,38.7023583335542,19.3402412358395));
#37324=CARTESIAN_POINT('Ctrl Pts',(131.834107404725,38.6520473906786,19.3344249116463));
#37325=CARTESIAN_POINT('Ctrl Pts',(131.939955627691,38.5969485711775,19.3286085874531));
#37326=CARTESIAN_POINT('Ctrl Pts',(132.043293086022,38.5372557674861,19.3227922632599));
#37327=CARTESIAN_POINT('Ctrl Pts',(132.146519157764,38.4776273061725,19.3169822084343));
#37328=CARTESIAN_POINT('Ctrl Pts',(132.247239499223,38.413414918366,19.3111721536086));
#37329=CARTESIAN_POINT('Ctrl Pts',(132.345024570039,38.3448594538358,19.305362098783));
#37330=CARTESIAN_POINT('Ctrl Pts',(132.393129575289,38.3111338456868,19.3025038637216));
#37331=CARTESIAN_POINT('Ctrl Pts',(132.440524568373,38.2763578776289,19.2996456286602));
#37332=CARTESIAN_POINT('Ctrl Pts',(132.487160689988,38.2405642567579,19.2967873935987));
#37333=CARTESIAN_POINT('Ctrl Pts',(132.487160689988,38.2405642567579,20.546920386683));
#37334=CARTESIAN_POINT('Ctrl Pts',(132.523548081502,38.2126366236008,20.5446756833603));
#37335=CARTESIAN_POINT('Ctrl Pts',(132.559444026617,38.1841121588552,20.5424309800375));
#37336=CARTESIAN_POINT('Ctrl Pts',(132.594828390309,38.1550104001174,20.5401862767148));
#37337=CARTESIAN_POINT('Ctrl Pts',(132.68662856323,38.0795096363405,20.5343626831359));
#37338=CARTESIAN_POINT('Ctrl Pts',(132.775278808925,37.9998771827638,20.528539089557));
#37339=CARTESIAN_POINT('Ctrl Pts',(132.860385118191,37.9164056603347,20.5227154959782));
#37340=CARTESIAN_POINT('Ctrl Pts',(132.945384053206,37.8330394496301,20.5168992497277));
#37341=CARTESIAN_POINT('Ctrl Pts',(133.026847655955,37.7458440871956,20.5110830034771));
#37342=CARTESIAN_POINT('Ctrl Pts',(133.104414314992,37.6551528695865,20.5052667572266));
#37343=CARTESIAN_POINT('Ctrl Pts',(133.181903329377,37.5645524343848,20.4994563330706));
#37344=CARTESIAN_POINT('Ctrl Pts',(133.255502896449,37.4704634141061,20.4936459089145));
#37345=CARTESIAN_POINT('Ctrl Pts',(133.324888111454,37.3732560010055,20.4878354847585));
#37346=CARTESIAN_POINT('Ctrl Pts',(133.396899701919,37.2723690840767,20.4818051238996));
#37347=CARTESIAN_POINT('Ctrl Pts',(133.464371272435,37.1681233483222,20.4757747630408));
#37348=CARTESIAN_POINT('Ctrl Pts',(133.526985163058,37.0609708051235,20.469744402182));
#37349=CARTESIAN_POINT('Ctrl Pts',(133.587247521374,36.9578424914445,20.4639405180399));
#37350=CARTESIAN_POINT('Ctrl Pts',(133.643010266116,36.852022153747,20.4581366338979));
#37351=CARTESIAN_POINT('Ctrl Pts',(133.694034661703,36.7439417760174,20.4523327497559));
#37352=CARTESIAN_POINT('Ctrl Pts',(133.745051520445,36.6358773629053,20.4465297229091));
#37353=CARTESIAN_POINT('Ctrl Pts',(133.791331247645,36.5255539428036,20.4407266960623));
#37354=CARTESIAN_POINT('Ctrl Pts',(133.832681929684,36.4134264133219,20.4349236692155));
#37355=CARTESIAN_POINT('Ctrl Pts',(133.87403626256,36.3012889841392,20.4291201300214));
#37356=CARTESIAN_POINT('Ctrl Pts',(133.910460543732,36.1873475120151,20.4233165908274));
#37357=CARTESIAN_POINT('Ctrl Pts',(133.941811928858,36.0720744925205,20.4175130516333));
#37358=CARTESIAN_POINT('Ctrl Pts',(133.973173480877,35.9567640913145,20.4117076304184));
#37359=CARTESIAN_POINT('Ctrl Pts',(133.999458758044,35.8401216777956,20.4059022092035));
#37360=CARTESIAN_POINT('Ctrl Pts',(134.020575614029,35.7226318093414,20.4000967879886));
#37361=CARTESIAN_POINT('Ctrl Pts',(134.041715854984,35.6050118316994,20.3942849378054));
#37362=CARTESIAN_POINT('Ctrl Pts',(134.057676177786,35.4865429279749,20.3884730876222));
#37363=CARTESIAN_POINT('Ctrl Pts',(134.06841607087,35.367716839817,20.382661237439));
#37364=CARTESIAN_POINT('Ctrl Pts',(134.079163017976,35.2488127060289,20.3768455700005));
#37365=CARTESIAN_POINT('Ctrl Pts',(134.084682687974,35.1295513275569,20.3710299025621));
#37366=CARTESIAN_POINT('Ctrl Pts',(134.084986697936,35.010424859097,20.3652142351236));
#37367=CARTESIAN_POINT('Ctrl Pts',(134.085291143359,34.8911277547944,20.3593902373676));
#37368=CARTESIAN_POINT('Ctrl Pts',(134.080365034098,34.7719663527491,20.3535662396115));
#37369=CARTESIAN_POINT('Ctrl Pts',(134.070271860309,34.6534282423887,20.3477422418555));
#37370=CARTESIAN_POINT('Ctrl Pts',(134.067594084752,34.6219794175441,20.3461971026191));
#37371=CARTESIAN_POINT('Ctrl Pts',(134.064552893823,34.59057440942,20.3446519633827));
#37372=CARTESIAN_POINT('Ctrl Pts',(134.061150073727,34.5592221890063,20.3431068241463));
#37373=CARTESIAN_POINT('Ctrl Pts',(134.048324924256,34.4410564024724,20.3372832304498));
#37374=CARTESIAN_POINT('Ctrl Pts',(134.030317473102,34.3232602823623,20.3314596367534));
#37375=CARTESIAN_POINT('Ctrl Pts',(134.007156478495,34.2063237707623,20.3256360430569));
#37376=CARTESIAN_POINT('Ctrl Pts',(133.984024704926,34.0895347919567,20.3198197966896));
#37377=CARTESIAN_POINT('Ctrl Pts',(133.95575239879,33.9736036615937,20.3140035503224));
#37378=CARTESIAN_POINT('Ctrl Pts',(133.922420097489,33.8590155220973,20.3081873039552));
#37379=CARTESIAN_POINT('Ctrl Pts',(133.88912116201,33.7445420859765,20.3023768796834));
#37380=CARTESIAN_POINT('Ctrl Pts',(133.850772421122,33.6314093561535,20.2965664554117));
#37381=CARTESIAN_POINT('Ctrl Pts',(133.807505391998,33.5200919995129,20.2907560311399));
#37382=CARTESIAN_POINT('Ctrl Pts',(133.762600616579,33.4045610513189,20.2847256703248));
#37383=CARTESIAN_POINT('Ctrl Pts',(133.712397948555,33.2909860626496,20.2786953095098));
#37384=CARTESIAN_POINT('Ctrl Pts',(133.657101307583,33.1798804912659,20.2726649486947));
#37385=CARTESIAN_POINT('Ctrl Pts',(133.603881390284,33.0729476067983,20.2668610644402));
#37386=CARTESIAN_POINT('Ctrl Pts',(133.545943417349,32.968302399856,20.2610571801857));
#37387=CARTESIAN_POINT('Ctrl Pts',(133.483517821575,32.8663813398906,20.2552532959313));
#37388=CARTESIAN_POINT('Ctrl Pts',(133.421101446739,32.7644753347703,20.2494502689734));
#37389=CARTESIAN_POINT('Ctrl Pts',(133.354198980522,32.6652930245269,20.2436472420155));
#37390=CARTESIAN_POINT('Ctrl Pts',(133.28308568611,32.5692442784881,20.2378442150577));
#37391=CARTESIAN_POINT('Ctrl Pts',(133.211966113147,32.4731870523636,20.2320406757541));
#37392=CARTESIAN_POINT('Ctrl Pts',(133.136635215808,32.3802642687055,20.2262371364504));
#37393=CARTESIAN_POINT('Ctrl Pts',(133.057409873693,32.2908544032772,20.2204335971468));
#37394=CARTESIAN_POINT('Ctrl Pts',(132.978158839736,32.2014155432858,20.214628175824));
#37395=CARTESIAN_POINT('Ctrl Pts',(132.895011120002,32.1154921725934,20.2088227545011));
#37396=CARTESIAN_POINT('Ctrl Pts',(132.808321473045,32.0334269764534,20.2030173331783));
#37397=CARTESIAN_POINT('Ctrl Pts',(132.721535825349,31.9512709007244,20.19720548289));
#37398=CARTESIAN_POINT('Ctrl Pts',(132.631200717785,31.8729818088505,20.1913936326018));
#37399=CARTESIAN_POINT('Ctrl Pts',(132.537705221925,31.7988631384122,20.1855817823136));
#37400=CARTESIAN_POINT('Ctrl Pts',(132.444148317733,31.7246957864433,20.1797661147717));
#37401=CARTESIAN_POINT('Ctrl Pts',(132.347427221364,31.6547045498409,20.1739504472298));
#37402=CARTESIAN_POINT('Ctrl Pts',(132.247959924866,31.5891494937191,20.1681347796878));
#37403=CARTESIAN_POINT('Ctrl Pts',(132.148350152228,31.5235005370726,20.1623107818314));
#37404=CARTESIAN_POINT('Ctrl Pts',(132.045986677373,31.4623006526354,20.1564867839751));
#37405=CARTESIAN_POINT('Ctrl Pts',(131.941312109028,31.4057640178554,20.1506627861187));
#37406=CARTESIAN_POINT('Ctrl Pts',(131.913541379017,31.3907645423858,20.1491176479384));
#37407=CARTESIAN_POINT('Ctrl Pts',(131.885608085199,31.3760930353291,20.1475725097581));
#37408=CARTESIAN_POINT('Ctrl Pts',(131.857520709764,31.3617529203202,20.1460273715779));
#37409=CARTESIAN_POINT('Ctrl Pts',(131.751659969633,31.3077053218923,20.1402037775669));
#37410=CARTESIAN_POINT('Ctrl Pts',(131.643267658667,31.2581946893293,20.134380183556));
#37411=CARTESIAN_POINT('Ctrl Pts',(131.532769314566,31.213465538474,20.1285565895451));
#37412=CARTESIAN_POINT('Ctrl Pts',(131.422410380504,31.1687928200722,20.1227403428612));
#37413=CARTESIAN_POINT('Ctrl Pts',(131.309951073329,31.1288897366471,20.1169240961773));
#37414=CARTESIAN_POINT('Ctrl Pts',(131.195841299892,31.0939548664318,20.1111078494933));
#37415=CARTESIAN_POINT('Ctrl Pts',(131.081845750943,31.0590549662062,20.1052974249031));
#37416=CARTESIAN_POINT('Ctrl Pts',(130.966203410636,31.0291135044589,20.0994870003129));
#37417=CARTESIAN_POINT('Ctrl Pts',(130.849383369636,31.0042806791034,20.0936765757226));
#37418=CARTESIAN_POINT('Ctrl Pts',(130.728141458162,30.9785078820077,20.0876462150263));
#37419=CARTESIAN_POINT('Ctrl Pts',(130.605631343258,30.9582382749794,20.0816158543299));
#37420=CARTESIAN_POINT('Ctrl Pts',(130.482394247442,30.943582764306,20.0755854936335));
#37421=CARTESIAN_POINT('Ctrl Pts',(130.363785441842,30.9294776557354,20.069781609058));
#37422=CARTESIAN_POINT('Ctrl Pts',(130.244503717505,30.9205726148075,20.0639777244826));
#37423=CARTESIAN_POINT('Ctrl Pts',(130.125040439799,30.9169141708244,20.0581738399072));
#37424=CARTESIAN_POINT('Ctrl Pts',(130.005594808104,30.9132562672328,20.052370812628));
#37425=CARTESIAN_POINT('Ctrl Pts',(129.885968084407,30.9148434318936,20.0465677853488));
#37426=CARTESIAN_POINT('Ctrl Pts',(129.766653960882,30.9216701180474,20.0407647580696));
#37427=CARTESIAN_POINT('Ctrl Pts',(129.647329303186,30.928497406925,20.0349612184447));
#37428=CARTESIAN_POINT('Ctrl Pts',(129.528317708227,30.9405651137181,20.0291576788197));
#37429=CARTESIAN_POINT('Ctrl Pts',(129.410109424112,30.9578156760882,20.0233541391948));
#37430=CARTESIAN_POINT('Ctrl Pts',(129.291862806457,30.9750718326105,20.017548717551));
#37431=CARTESIAN_POINT('Ctrl Pts',(129.174420421579,30.9975141283841,20.0117432959072));
#37432=CARTESIAN_POINT('Ctrl Pts',(129.058263347298,31.0250337011544,20.0059378742634));
#37433=CARTESIAN_POINT('Ctrl Pts',(128.941977639887,31.0525837492859,20.0001260236563));
#37434=CARTESIAN_POINT('Ctrl Pts',(128.826980481798,31.0852222034352,19.9943141730493));
#37435=CARTESIAN_POINT('Ctrl Pts',(128.713738934376,31.1227899887859,19.9885023224423));
#37436=CARTESIAN_POINT('Ctrl Pts',(128.600423009333,31.1603824488475,19.9826866545824));
#37437=CARTESIAN_POINT('Ctrl Pts',(128.488865372048,31.2029105427706,19.9768709867226));
#37438=CARTESIAN_POINT('Ctrl Pts',(128.379512661538,31.2501672322775,19.9710553188628));
#37439=CARTESIAN_POINT('Ctrl Pts',(128.270003315182,31.297491611845,19.9652313206922));
#37440=CARTESIAN_POINT('Ctrl Pts',(128.162705565496,31.3495579282979,19.9594073225216));
#37441=CARTESIAN_POINT('Ctrl Pts',(128.05804116635,31.4061134007303,19.953583324351));
#37442=CARTESIAN_POINT('Ctrl Pts',(128.030273190889,31.4211178433444,19.9520381892371));
#37443=CARTESIAN_POINT('Ctrl Pts',(128.002690406456,31.4364380287196,19.9504930541233));
#37444=CARTESIAN_POINT('Ctrl Pts',(127.975300326065,31.4520687393403,19.9489479190094));
#37445=CARTESIAN_POINT('Ctrl Pts',(127.872067493297,31.5109806706853,19.9431243262148));
#37446=CARTESIAN_POINT('Ctrl Pts',(127.771241531522,31.5744969326317,19.9373007334202));
#37447=CARTESIAN_POINT('Ctrl Pts',(127.673260210899,31.6423956525798,19.9314771406255));
#37448=CARTESIAN_POINT('Ctrl Pts',(127.575402508281,31.7102087081967,19.9256608951591));
#37449=CARTESIAN_POINT('Ctrl Pts',(127.48038264117,31.7823929939895,19.9198446496927));
#37450=CARTESIAN_POINT('Ctrl Pts',(127.388613317128,31.8586810743706,19.9140284042263));
#37451=CARTESIAN_POINT('Ctrl Pts',(127.296935854679,31.934892789967,19.9082179808534));
#37452=CARTESIAN_POINT('Ctrl Pts',(127.208502774446,32.0151998684178,19.9024075574804));
#37453=CARTESIAN_POINT('Ctrl Pts',(127.123696835961,32.0992923090149,19.8965971341075));
#37454=CARTESIAN_POINT('Ctrl Pts',(127.035680799239,32.1865678403263,19.8905667729547));
#37455=CARTESIAN_POINT('Ctrl Pts',(126.951572289371,32.2779207098561,19.8845364118019));
#37456=CARTESIAN_POINT('Ctrl Pts',(126.871760743885,32.3729590493298,19.8785060506492));
#37457=CARTESIAN_POINT('Ctrl Pts',(126.794946621221,32.4644281046105,19.8727021672827));
#37458=CARTESIAN_POINT('Ctrl Pts',(126.722112813876,32.559310456321,19.8668982839163));
#37459=CARTESIAN_POINT('Ctrl Pts',(126.653567586128,32.6572206464574,19.8610944005499));
#37460=CARTESIAN_POINT('Ctrl Pts',(126.585032483189,32.755116374288,19.8552913744746));
#37461=CARTESIAN_POINT('Ctrl Pts',(126.520784934205,32.8560387167024,19.8494883483992));
#37462=CARTESIAN_POINT('Ctrl Pts',(126.461090924009,32.9595717234202,19.8436853223239));
#37463=CARTESIAN_POINT('Ctrl Pts',(126.401391643397,33.0631138711207,19.8378817838964));
#37464=CARTESIAN_POINT('Ctrl Pts',(126.346246904886,33.1692667876409,19.8320782454689));
#37465=CARTESIAN_POINT('Ctrl Pts',(126.295877301067,33.2775888901753,19.8262747070414));
#37466=CARTESIAN_POINT('Ctrl Pts',(126.245491362913,33.3859461204306,19.8204692865874));
#37467=CARTESIAN_POINT('Ctrl Pts',(126.199883811203,33.496473565618,19.8146638661333));
#37468=CARTESIAN_POINT('Ctrl Pts',(126.159227305938,33.6087091919549,19.8088584456792));
#37469=CARTESIAN_POINT('Ctrl Pts',(126.118525777253,33.7210691091459,19.8030465962445));
#37470=CARTESIAN_POINT('Ctrl Pts',(126.082786378384,33.8351405992439,19.7972347468098));
#37471=CARTESIAN_POINT('Ctrl Pts',(126.05213208967,33.9504458267486,19.7914228973751));
#37472=CARTESIAN_POINT('Ctrl Pts',(126.021457667015,34.0658267874974,19.7856072306788));
#37473=CARTESIAN_POINT('Ctrl Pts',(125.995875093377,34.1824427015039,19.7797915639825));
#37474=CARTESIAN_POINT('Ctrl Pts',(125.975456039064,34.2998065220979,19.7739758972863));
#37475=CARTESIAN_POINT('Ctrl Pts',(125.955007736599,34.4173384540524,19.7681519002576));
#37476=CARTESIAN_POINT('Ctrl Pts',(125.939737767967,34.5356200273075,19.7623279032289));
#37477=CARTESIAN_POINT('Ctrl Pts',(125.929665904531,34.6541599339824,19.7565039062002));
#37478=CARTESIAN_POINT('Ctrl Pts',(125.926993769684,34.6856093889272,19.7549587596138));
#37479=CARTESIAN_POINT('Ctrl Pts',(125.924687233368,34.7170770343997,19.7534136130274));
#37480=CARTESIAN_POINT('Ctrl Pts',(125.922746050155,34.7485537264753,19.751868466441));
#37481=CARTESIAN_POINT('Ctrl Pts',(125.917614677709,34.8317600046202,19.7477839871591));
#37482=CARTESIAN_POINT('Ctrl Pts',(125.915030089811,34.9151249404383,19.7436995078773));
#37483=CARTESIAN_POINT('Ctrl Pts',(125.915000261185,34.9985392197775,19.7396150285955));
#37484=CARTESIAN_POINT('Origin',(130.,35.,32.7603849714045));
#37485=CARTESIAN_POINT('',(132.487160689988,38.2405642567579,21.7969524304342));
#37486=CARTESIAN_POINT('',(132.487160689988,38.2405642567579,21.6925409181329));
#37487=CARTESIAN_POINT('',(132.487160689988,38.2405642567579,32.7603849714045));
#37488=CARTESIAN_POINT('',(125.915001474033,34.9965297189326,20.8853849714288));
#37489=CARTESIAN_POINT('Ctrl Pts',(132.487160689988,38.2405642567579,21.6925409181329));
#37490=CARTESIAN_POINT('Ctrl Pts',(132.581750090941,38.1679660852364,21.6867311890074));
#37491=CARTESIAN_POINT('Ctrl Pts',(132.673252114311,38.09115093877,21.6809214598819));
#37492=CARTESIAN_POINT('Ctrl Pts',(132.761272906671,38.010414744663,21.6751117307563));
#37493=CARTESIAN_POINT('Ctrl Pts',(132.851093350277,37.9280278383955,21.6691832173529));
#37494=CARTESIAN_POINT('Ctrl Pts',(132.937288287603,37.8415580245174,21.6632547039495));
#37495=CARTESIAN_POINT('Ctrl Pts',(133.019473914611,37.7513637125949,21.6573261905461));
#37496=CARTESIAN_POINT('Ctrl Pts',(133.099929353202,37.6630681895418,21.6515224854041));
#37497=CARTESIAN_POINT('Ctrl Pts',(133.176542345868,37.5712037625444,21.6457187802621));
#37498=CARTESIAN_POINT('Ctrl Pts',(133.248990095402,37.4761438488063,21.6399150751201));
#37499=CARTESIAN_POINT('Ctrl Pts',(133.321429243592,37.3810952210364,21.6341120590217));
#37500=CARTESIAN_POINT('Ctrl Pts',(133.389703884664,37.2828521857437,21.6283090429234));
#37501=CARTESIAN_POINT('Ctrl Pts',(133.453532325283,37.1818202213349,21.6225060268251));
#37502=CARTESIAN_POINT('Ctrl Pts',(133.517368251397,37.0807764083789,21.6167023301767));
#37503=CARTESIAN_POINT('Ctrl Pts',(133.57675672216,36.9769433611896,21.6108986335283));
#37504=CARTESIAN_POINT('Ctrl Pts',(133.631460439649,36.8707538788577,21.6050949368799));
#37505=CARTESIAN_POINT('Ctrl Pts',(133.688224583038,36.7605647495264,21.5990726428961));
#37506=CARTESIAN_POINT('Ctrl Pts',(133.739943909793,36.6478386067895,21.5930503489123));
#37507=CARTESIAN_POINT('Ctrl Pts',(133.786407181534,36.5330837079656,21.5870280549285));
#37508=CARTESIAN_POINT('Ctrl Pts',(133.83125090894,36.4223287566105,21.5812156766853));
#37509=CARTESIAN_POINT('Ctrl Pts',(133.871198793406,36.3096845276156,21.5754032984421));
#37510=CARTESIAN_POINT('Ctrl Pts',(133.906111590045,36.1956242077342,21.5695909201989));
#37511=CARTESIAN_POINT('Ctrl Pts',(133.941048500748,36.0814851070565,21.56377452738));
#37512=CARTESIAN_POINT('Ctrl Pts',(133.970943296275,35.965928361928,21.5579581345612));
#37513=CARTESIAN_POINT('Ctrl Pts',(133.995707691937,35.8494380734306,21.5521417417423));
#37514=CARTESIAN_POINT('Ctrl Pts',(134.020506526533,35.7327857861762,21.54631726028));
#37515=CARTESIAN_POINT('Ctrl Pts',(134.040160658276,35.6151977659667,21.5404927788177));
#37516=CARTESIAN_POINT('Ctrl Pts',(134.054633518213,35.4971639900348,21.5346682973554));
#37517=CARTESIAN_POINT('Ctrl Pts',(134.056158284461,35.4847287202569,21.5340546679283));
#37518=CARTESIAN_POINT('Ctrl Pts',(134.057625589601,35.4722885030589,21.5334410385013));
#37519=CARTESIAN_POINT('Ctrl Pts',(134.059035424522,35.4598439109867,21.5328274090742));
#37520=CARTESIAN_POINT('Ctrl Pts',(134.072415333228,35.3417396540498,21.5270038154121));
#37521=CARTESIAN_POINT('Ctrl Pts',(134.080657885567,35.2228604950866,21.52118022175));
#37522=CARTESIAN_POINT('Ctrl Pts',(134.083683781112,35.1036907704711,21.5153566280879));
#37523=CARTESIAN_POINT('Ctrl Pts',(134.086705859041,34.9846713961642,21.5095403817543));
#37524=CARTESIAN_POINT('Ctrl Pts',(134.084524360526,34.8653625899546,21.5037241354206));
#37525=CARTESIAN_POINT('Ctrl Pts',(134.077111557626,34.7462553514382,21.4979078890869));
#37526=CARTESIAN_POINT('Ctrl Pts',(134.069706174982,34.6272673399242,21.4920974648479));
#37527=CARTESIAN_POINT('Ctrl Pts',(134.057079930669,34.5084808999122,21.4862870406089));
#37528=CARTESIAN_POINT('Ctrl Pts',(134.039257132993,34.3903879811164,21.4804766163699));
#37529=CARTESIAN_POINT('Ctrl Pts',(134.02075970552,34.267825000818,21.4744462555422));
#37530=CARTESIAN_POINT('Ctrl Pts',(133.996664539723,34.1460095296057,21.4684158947145));
#37531=CARTESIAN_POINT('Ctrl Pts',(133.967058086598,34.0254872306836,21.4623855338869));
#37532=CARTESIAN_POINT('Ctrl Pts',(133.938563535254,33.9094912746623,21.4565816496628));
#37533=CARTESIAN_POINT('Ctrl Pts',(133.904964301934,33.7946935418835,21.4507777654388));
#37534=CARTESIAN_POINT('Ctrl Pts',(133.866389576651,33.6815703880888,21.4449738812147));
#37535=CARTESIAN_POINT('Ctrl Pts',(133.827820549267,33.5684639437924,21.4391708542864));
#37536=CARTESIAN_POINT('Ctrl Pts',(133.784277623226,33.4570319729531,21.433367827358));
#37537=CARTESIAN_POINT('Ctrl Pts',(133.735939558197,33.3477347012361,21.4275648004297));
#37538=CARTESIAN_POINT('Ctrl Pts',(133.687597225422,33.2384277797115,21.4217612611547));
#37539=CARTESIAN_POINT('Ctrl Pts',(133.634459077085,33.1312563054996,21.4159577218797));
#37540=CARTESIAN_POINT('Ctrl Pts',(133.576751357029,33.0266589929783,21.4101541826047));
#37541=CARTESIAN_POINT('Ctrl Pts',(133.519024923031,32.9220277607668,21.4043487613095));
#37542=CARTESIAN_POINT('Ctrl Pts',(133.456726167385,32.8199727077647,21.3985433400143));
#37543=CARTESIAN_POINT('Ctrl Pts',(133.390126134964,32.7209059279976,21.3927379187191));
#37544=CARTESIAN_POINT('Ctrl Pts',(133.323452349169,32.6217294409386,21.386926068457));
#37545=CARTESIAN_POINT('Ctrl Pts',(133.252468006667,32.5255481717115,21.3811142181949));
#37546=CARTESIAN_POINT('Ctrl Pts',(133.177486231652,32.4327434394553,21.3753023679327));
#37547=CARTESIAN_POINT('Ctrl Pts',(133.102455208204,32.3398777525513,21.3694867004161));
#37548=CARTESIAN_POINT('Ctrl Pts',(133.023421793114,32.2503933246318,21.3636710328994));
#37549=CARTESIAN_POINT('Ctrl Pts',(132.940736832276,32.1646354937511,21.3578553653828));
#37550=CARTESIAN_POINT('Ctrl Pts',(132.857933434157,32.0787548240348,21.3520313675502));
#37551=CARTESIAN_POINT('Ctrl Pts',(132.771468345597,31.9966116858572,21.3462073697176));
#37552=CARTESIAN_POINT('Ctrl Pts',(132.681726486134,31.9185120390361,21.340383371885));
#37553=CARTESIAN_POINT('Ctrl Pts',(132.657917480278,31.8977917758313,21.3388382334252));
#37554=CARTESIAN_POINT('Ctrl Pts',(132.633877994582,31.877355888102,21.3372930949655));
#37555=CARTESIAN_POINT('Ctrl Pts',(132.60961555488,31.8572095749588,21.3357479565057));
#37556=CARTESIAN_POINT('Ctrl Pts',(132.518170940721,31.7812785533999,21.3299243628355));
#37557=CARTESIAN_POINT('Ctrl Pts',(132.423262109218,31.7092194954134,21.3241007691653));
#37558=CARTESIAN_POINT('Ctrl Pts',(132.325250675735,31.6413642211468,21.3182771754951));
#37559=CARTESIAN_POINT('Ctrl Pts',(132.227362898236,31.5735945563889,21.3124609291534));
#37560=CARTESIAN_POINT('Ctrl Pts',(132.126380637163,31.5100183568043,21.3066446828117));
#37561=CARTESIAN_POINT('Ctrl Pts',(132.022699350964,31.4509279613385,21.30082843647));
#37562=CARTESIAN_POINT('Ctrl Pts',(131.919121850307,31.3918967156854,21.2950180122231));
#37563=CARTESIAN_POINT('Ctrl Pts',(131.812851052025,31.3373425422531,21.2892075879762));
#37564=CARTESIAN_POINT('Ctrl Pts',(131.704311733595,31.2875147791901,21.2833971637293));
#37565=CARTESIAN_POINT('Ctrl Pts',(131.591663977427,31.2358009322168,21.2773668029046));
#37566=CARTESIAN_POINT('Ctrl Pts',(131.476572940032,31.189178629305,21.2713364420799));
#37567=CARTESIAN_POINT('Ctrl Pts',(131.359542387655,31.147874678029,21.2653060812553));
#37568=CARTESIAN_POINT('Ctrl Pts',(131.246907041727,31.1081219404262,21.2595021970237));
#37569=CARTESIAN_POINT('Ctrl Pts',(131.13247565441,31.0732954338841,21.2536983127921));
#37570=CARTESIAN_POINT('Ctrl Pts',(131.016717453162,31.0435482284708,21.2478944285605));
#37571=CARTESIAN_POINT('Ctrl Pts',(130.90097635064,31.0138054170383,21.2420914016247));
#37572=CARTESIAN_POINT('Ctrl Pts',(130.783909219319,30.989140516294,21.236288374689));
#37573=CARTESIAN_POINT('Ctrl Pts',(130.665998968207,30.969656295755,21.2304853477532));
#37574=CARTESIAN_POINT('Ctrl Pts',(130.548078306854,30.9501703549633,21.224681808471));
#37575=CARTESIAN_POINT('Ctrl Pts',(130.429314780602,30.9358660703749,21.2188782691887));
#37576=CARTESIAN_POINT('Ctrl Pts',(130.310199336132,30.9267947054116,21.2130747299064));
#37577=CARTESIAN_POINT('Ctrl Pts',(130.191045263914,30.9177203987105,21.2072693086041));
#37578=CARTESIAN_POINT('Ctrl Pts',(130.071539453462,30.9138824175259,21.2014638873018));
#37579=CARTESIAN_POINT('Ctrl Pts',(129.952175145256,30.9152799626818,21.1956584659995));
#37580=CARTESIAN_POINT('Ctrl Pts',(129.832678652129,30.9166790554896,21.1898466157305));
#37581=CARTESIAN_POINT('Ctrl Pts',(129.713324382588,30.9233252428812,21.1840347654616));
#37582=CARTESIAN_POINT('Ctrl Pts',(129.594602904237,30.9351656620784,21.1782229151926));
#37583=CARTESIAN_POINT('Ctrl Pts',(129.475803448983,30.9470138581263,21.1724072476693));
#37584=CARTESIAN_POINT('Ctrl Pts',(129.357638015862,30.9640630220881,21.1665915801459));
#37585=CARTESIAN_POINT('Ctrl Pts',(129.240587756598,30.9862090183255,21.1607759126225));
#37586=CARTESIAN_POINT('Ctrl Pts',(129.123369835479,31.008386736311,21.1549519147835));
#37587=CARTESIAN_POINT('Ctrl Pts',(129.007270672566,31.0356757651948,21.1491279169445));
#37588=CARTESIAN_POINT('Ctrl Pts',(128.892757162696,31.0679218854099,21.1433039191054));
#37589=CARTESIAN_POINT('Ctrl Pts',(128.862376103998,31.0764769569655,21.141758780716));
#37590=CARTESIAN_POINT('Ctrl Pts',(128.832106548079,31.085380679455,21.1402136423267));
#37591=CARTESIAN_POINT('Ctrl Pts',(128.801956968712,31.0946296084517,21.1386685039373));
#37592=CARTESIAN_POINT('Ctrl Pts',(128.688323845554,31.1294886250555,21.1328449102228));
#37593=CARTESIAN_POINT('Ctrl Pts',(128.576030163277,31.1693674825615,21.1270213165084));
#37594=CARTESIAN_POINT('Ctrl Pts',(128.465551671054,31.2141456280259,21.1211977227939));
#37595=CARTESIAN_POINT('Ctrl Pts',(128.355212563856,31.25886727921,21.1153814764078));
#37596=CARTESIAN_POINT('Ctrl Pts',(128.246684466793,31.3084757721005,21.1095652300216));
#37597=CARTESIAN_POINT('Ctrl Pts',(128.140428659644,31.362800606218,21.1037489836355));
#37598=CARTESIAN_POINT('Ctrl Pts',(128.034279215143,31.417071060878,21.0979385593439));
#37599=CARTESIAN_POINT('Ctrl Pts',(127.930397897057,31.4760482799395,21.0921281350523));
#37600=CARTESIAN_POINT('Ctrl Pts',(127.829226092164,31.5395136698642,21.0863177107608));
#37601=CARTESIAN_POINT('Ctrl Pts',(127.724224726258,31.6053813553999,21.0802873499528));
#37602=CARTESIAN_POINT('Ctrl Pts',(127.622142463116,31.6760835298159,21.0742569891448));
#37603=CARTESIAN_POINT('Ctrl Pts',(127.523445144343,31.7513231852151,21.0682266283368));
#37604=CARTESIAN_POINT('Ctrl Pts',(127.428454507002,31.8237371363593,21.0624227440604));
#37605=CARTESIAN_POINT('Ctrl Pts',(127.33659950276,31.9003536251871,21.056618859784));
#37606=CARTESIAN_POINT('Ctrl Pts',(127.248265368412,31.9808641108226,21.0508149755076));
#37607=CARTESIAN_POINT('Ctrl Pts',(127.159944281962,32.061362704197,21.0450119485271));
#37608=CARTESIAN_POINT('Ctrl Pts',(127.075143332861,32.1457538755285,21.0392089215466));
#37609=CARTESIAN_POINT('Ctrl Pts',(126.994213187701,32.2336900681575,21.0334058945661));
#37610=CARTESIAN_POINT('Ctrl Pts',(126.913275897258,32.3216340246304,21.0276023552391));
#37611=CARTESIAN_POINT('Ctrl Pts',(126.836210366775,32.4131233242236,21.0217988159121));
#37612=CARTESIAN_POINT('Ctrl Pts',(126.763328590591,32.5077754540341,21.0159952765852));
#37613=CARTESIAN_POINT('Ctrl Pts',(126.6904231797,32.6024582784232,21.0101898552383));
#37614=CARTESIAN_POINT('Ctrl Pts',(126.621704470357,32.7003056494819,21.0043844338914));
#37615=CARTESIAN_POINT('Ctrl Pts',(126.557442170625,32.8009045970199,20.9985790125445));
#37616=CARTESIAN_POINT('Ctrl Pts',(126.49310870635,32.9016149485715,20.9927671622313));
#37617=CARTESIAN_POINT('Ctrl Pts',(126.433241722442,33.0050826145845,20.9869553119182));
#37618=CARTESIAN_POINT('Ctrl Pts',(126.378065917296,33.1108683210143,20.9811434616051));
#37619=CARTESIAN_POINT('Ctrl Pts',(126.322853872387,33.2167235080591,20.9753277940377));
#37620=CARTESIAN_POINT('Ctrl Pts',(126.272339314883,33.3248993984854,20.9695121264703));
#37621=CARTESIAN_POINT('Ctrl Pts',(126.226698898596,33.4349364875044,20.963696458903));
#37622=CARTESIAN_POINT('Ctrl Pts',(126.180993107347,33.5451311927576,20.9578724610206));
#37623=CARTESIAN_POINT('Ctrl Pts',(126.140175531625,33.6571920354107,20.9520484631381));
#37624=CARTESIAN_POINT('Ctrl Pts',(126.104373121381,33.7706439805395,20.9462244652557));
#37625=CARTESIAN_POINT('Ctrl Pts',(126.094874549382,33.8007433917773,20.9446793272934));
#37626=CARTESIAN_POINT('Ctrl Pts',(126.085728700532,33.8309406629967,20.9431341893312));
#37627=CARTESIAN_POINT('Ctrl Pts',(126.076937339023,33.8612268188767,20.9415890513689));
#37628=CARTESIAN_POINT('Ctrl Pts',(126.035980316616,34.0023233673116,20.9343905929645));
#37629=CARTESIAN_POINT('Ctrl Pts',(126.00261494991,34.1457149065662,20.9271921345601));
#37630=CARTESIAN_POINT('Ctrl Pts',(125.977056286359,34.290670121258,20.9199936761557));
#37631=CARTESIAN_POINT('Ctrl Pts',(125.951848625682,34.4336346333908,20.9128940757993));
#37632=CARTESIAN_POINT('Ctrl Pts',(125.93423472575,34.578120220996,20.9057944754429));
#37633=CARTESIAN_POINT('Ctrl Pts',(125.924374885705,34.7234047583076,20.8986948750864));
#37634=CARTESIAN_POINT('Ctrl Pts',(125.918213340712,34.8141949951977,20.8942582405339));
#37635=CARTESIAN_POINT('Ctrl Pts',(125.915078978048,34.9052968247186,20.8898216059814));
#37636=CARTESIAN_POINT('Ctrl Pts',(125.915001474033,34.9965297189326,20.8853849714288));
#37637=CARTESIAN_POINT('Ctrl Pts',(125.915001474033,34.9965297194327,20.8853849714045));
#37638=CARTESIAN_POINT('Ctrl Pts',(125.914898933796,35.1172337107693,20.8795151642127));
#37639=CARTESIAN_POINT('Ctrl Pts',(125.920150846961,35.2380430349758,20.8736453570208));
#37640=CARTESIAN_POINT('Ctrl Pts',(125.930756371624,35.3584428726101,20.867775549829));
#37641=CARTESIAN_POINT('Ctrl Pts',(125.941161880961,35.4765720245721,20.8620164445065));
#37642=CARTESIAN_POINT('Ctrl Pts',(125.956720796162,35.5943065688732,20.8562573391839));
#37643=CARTESIAN_POINT('Ctrl Pts',(125.97737978277,35.7111621389884,20.8504982338614));
#37644=CARTESIAN_POINT('Ctrl Pts',(125.998035648517,35.8280000562575,20.844739998541));
#37645=CARTESIAN_POINT('Ctrl Pts',(126.023789981673,35.9439588544505,20.8389817632207));
#37646=CARTESIAN_POINT('Ctrl Pts',(126.0545379871,36.0585624708827,20.8332235279003));
#37647=CARTESIAN_POINT('Ctrl Pts',(126.085288892145,36.1731768947406,20.8274647495631));
#37648=CARTESIAN_POINT('Ctrl Pts',(126.121034297587,36.2864354817355,20.8217059712258));
#37649=CARTESIAN_POINT('Ctrl Pts',(126.161619205866,36.397876203111,20.8159471928886));
#37650=CARTESIAN_POINT('Ctrl Pts',(126.203573824738,36.5130779662902,20.8099940600479));
#37651=CARTESIAN_POINT('Ctrl Pts',(126.250700225613,36.626336539789,20.8040409272072));
#37652=CARTESIAN_POINT('Ctrl Pts',(126.302773206647,36.7371640793301,20.7980877943665));
#37653=CARTESIAN_POINT('Ctrl Pts',(126.353220680841,36.8445320334945,20.7923204941394));
#37654=CARTESIAN_POINT('Ctrl Pts',(126.408310257637,36.9496181249756,20.7865531939122));
#37655=CARTESIAN_POINT('Ctrl Pts',(126.467791010032,37.0520050319609,20.780785893685));
#37656=CARTESIAN_POINT('Ctrl Pts',(126.53014662499,37.1593405697867,20.7747398445376));
#37657=CARTESIAN_POINT('Ctrl Pts',(126.597328220367,37.2637090356662,20.7686937953902));
#37658=CARTESIAN_POINT('Ctrl Pts',(126.668997397388,37.3646662896468,20.7626477462427));
#37659=CARTESIAN_POINT('Ctrl Pts',(126.740666574409,37.4656235436273,20.7566016970953));
#37660=CARTESIAN_POINT('Ctrl Pts',(126.816822954775,37.5631692246295,20.7505556479479));
#37661=CARTESIAN_POINT('Ctrl Pts',(126.897082912045,37.6569024342794,20.7445095988004));
#37662=CARTESIAN_POINT('Ctrl Pts',(126.974389822698,37.7471868688851,20.7386860051039));
#37663=CARTESIAN_POINT('Ctrl Pts',(127.055765126527,37.8342400373365,20.7328624114073));
#37664=CARTESIAN_POINT('Ctrl Pts',(127.140908444354,37.9176738125491,20.7270388177108));
#37665=CARTESIAN_POINT('Ctrl Pts',(127.225944341228,38.00100232365,20.7212225713435));
#37666=CARTESIAN_POINT('Ctrl Pts',(127.314738507605,38.0807202407039,20.7154063249762));
#37667=CARTESIAN_POINT('Ctrl Pts',(127.406950539365,38.1564726348727,20.7095900786089));
#37668=CARTESIAN_POINT('Ctrl Pts',(127.49907026636,38.232149200467,20.7037796543371));
#37669=CARTESIAN_POINT('Ctrl Pts',(127.594600738774,38.3038678823147,20.6979692300653));
#37670=CARTESIAN_POINT('Ctrl Pts',(127.69316539218,38.3713111829319,20.6921588057935));
#37671=CARTESIAN_POINT('Ctrl Pts',(127.795460921016,38.4413073515857,20.6861284449784));
#37672=CARTESIAN_POINT('Ctrl Pts',(127.901024549234,38.5066977662147,20.6800980841633));
#37673=CARTESIAN_POINT('Ctrl Pts',(128.009398053129,38.5671737957537,20.6740677233483));
#37674=CARTESIAN_POINT('Ctrl Pts',(128.113701475785,38.6253785842204,20.6682638390937));
#37675=CARTESIAN_POINT('Ctrl Pts',(128.22060713591,38.6790312437783,20.6624599548392));
#37676=CARTESIAN_POINT('Ctrl Pts',(128.329678398805,38.7279016548969,20.6566560705846));
#37677=CARTESIAN_POINT('Ctrl Pts',(128.438733550694,38.7767648473262,20.6508530436267));
#37678=CARTESIAN_POINT('Ctrl Pts',(128.549953296667,38.8208470291823,20.6450500166687));
#37679=CARTESIAN_POINT('Ctrl Pts',(128.662879021701,38.8599653482115,20.6392469897108));
#37680=CARTESIAN_POINT('Ctrl Pts',(128.77581471688,38.8990871209735,20.6334434504071));
#37681=CARTESIAN_POINT('Ctrl Pts',(128.890456304727,38.9332440258836,20.6276399111034));
#37682=CARTESIAN_POINT('Ctrl Pts',(129.006328549086,38.9623026193918,20.6218363717997));
#37683=CARTESIAN_POINT('Ctrl Pts',(129.122238369446,38.9913706362585,20.6160309504767));
#37684=CARTESIAN_POINT('Ctrl Pts',(129.239379244144,39.0153369543624,20.6102255291538));
#37685=CARTESIAN_POINT('Ctrl Pts',(129.357264883265,39.0341190574542,20.6044201078308));
#37686=CARTESIAN_POINT('Ctrl Pts',(129.475281069791,39.0529219599822,20.5986082575425));
#37687=CARTESIAN_POINT('Ctrl Pts',(129.594043263537,39.0665291236107,20.5927964072542));
#37688=CARTESIAN_POINT('Ctrl Pts',(129.713059015985,39.0749097992093,20.5869845569659));
#37689=CARTESIAN_POINT('Ctrl Pts',(129.832152938601,39.0832959792795,20.5811688894239));
#37690=CARTESIAN_POINT('Ctrl Pts',(129.951500344329,39.0864488240838,20.5753532218819));
#37691=CARTESIAN_POINT('Ctrl Pts',(130.070609405738,39.084389711061,20.5695375543399));
#37692=CARTESIAN_POINT('Ctrl Pts',(130.189889077989,39.0823276485817,20.5637135564834));
#37693=CARTESIAN_POINT('Ctrl Pts',(130.308929318374,39.0750387522796,20.5578895586269));
#37694=CARTESIAN_POINT('Ctrl Pts',(130.427243892813,39.0625961719145,20.5520655607704));
#37695=CARTESIAN_POINT('Ctrl Pts',(130.458633390312,39.0592950879432,20.5505204225909));
#37696=CARTESIAN_POINT('Ctrl Pts',(130.489971870865,39.0556315297765,20.5489752844114));
#37697=CARTESIAN_POINT('Ctrl Pts',(130.521250400697,39.051607461215,20.547430146232));
#37698=CARTESIAN_POINT('Ctrl Pts',(130.639133823974,39.0364414358271,20.5416067849997));
#37699=CARTESIAN_POINT('Ctrl Pts',(130.756544891981,39.0161018747522,20.5357834237673));
#37700=CARTESIAN_POINT('Ctrl Pts',(130.872994388094,38.9906272437245,20.529960062535));
#37701=CARTESIAN_POINT('Ctrl Pts',(130.989303093201,38.9651834123056,20.5241437419246));
#37702=CARTESIAN_POINT('Ctrl Pts',(131.104652142888,38.9346169431329,20.5183274213143));
#37703=CARTESIAN_POINT('Ctrl Pts',(131.218558069069,38.8990179830705,20.5125111007039));
#37704=CARTESIAN_POINT('Ctrl Pts',(131.332533735131,38.8633972272391,20.5066912190014));
#37705=CARTESIAN_POINT('Ctrl Pts',(131.445064103599,38.822737875531,20.5008713372988));
#37706=CARTESIAN_POINT('Ctrl Pts',(131.555674912321,38.7771815639674,20.4950514555963));
#37707=CARTESIAN_POINT('Ctrl Pts',(131.666021161126,38.7317342143953,20.4892454939386));
#37708=CARTESIAN_POINT('Ctrl Pts',(131.774456635541,38.6814134370787,20.4834395322809));
#37709=CARTESIAN_POINT('Ctrl Pts',(131.880526444515,38.6264094213808,20.4776335706232));
#37710=CARTESIAN_POINT('Ctrl Pts',(131.98697771394,38.5712075939134,20.4718067288982));
#37711=CARTESIAN_POINT('Ctrl Pts',(132.091045879827,38.5112889201177,20.4659798871732));
#37712=CARTESIAN_POINT('Ctrl Pts',(132.192293114386,38.4468936596034,20.4601530454482));
#37713=CARTESIAN_POINT('Ctrl Pts',(132.293540348946,38.3824983990892,20.4543262037232));
#37714=CARTESIAN_POINT('Ctrl Pts',(132.391966295005,38.3136267663548,20.4484993619982));
#37715=CARTESIAN_POINT('Ctrl Pts',(132.487160689988,38.2405642567579,20.4426725202732));
#37716=CARTESIAN_POINT('',(125.915001496759,35.0034969295637,20.989615028551));
#37717=CARTESIAN_POINT('Ctrl Pts',(125.915001496759,35.0034969295637,20.989615028551));
#37718=CARTESIAN_POINT('Ctrl Pts',(125.91512689229,35.1499798789446,20.9824905061117));
#37719=CARTESIAN_POINT('Ctrl Pts',(125.923135046557,35.2961228105776,20.9753659836725));
#37720=CARTESIAN_POINT('Ctrl Pts',(125.938894207773,35.4411856121167,20.9682414612332));
#37721=CARTESIAN_POINT('Ctrl Pts',(125.954891578429,35.5884411273641,20.9610092472435));
#37722=CARTESIAN_POINT('Ctrl Pts',(125.97887600381,35.7345836830536,20.9537770332538));
#37723=CARTESIAN_POINT('Ctrl Pts',(126.010660788168,35.8788615664252,20.9465448192641));
#37724=CARTESIAN_POINT('Ctrl Pts',(126.028532809329,35.9599864642905,20.9424782734599));
#37725=CARTESIAN_POINT('Ctrl Pts',(126.048870132568,36.0405222218269,20.9384117276558));
#37726=CARTESIAN_POINT('Ctrl Pts',(126.071632971448,36.1203381136909,20.9343451818516));
#37727=CARTESIAN_POINT('Ctrl Pts',(126.104231036441,36.2346403606165,20.9285215881814));
#37728=CARTESIAN_POINT('Ctrl Pts',(126.14187452446,36.3477030067233,20.9226979945112));
#37729=CARTESIAN_POINT('Ctrl Pts',(126.184452343526,36.4590480050958,20.916874400841));
#37730=CARTESIAN_POINT('Ctrl Pts',(126.226976444347,36.5702525252123,20.9110581544994));
#37731=CARTESIAN_POINT('Ctrl Pts',(126.274422349496,36.6797433298009,20.9052419081577));
#37732=CARTESIAN_POINT('Ctrl Pts',(126.32662874226,36.7870558477034,20.8994256618161));
#37733=CARTESIAN_POINT('Ctrl Pts',(126.378782876136,36.8942609451816,20.8936152375692));
#37734=CARTESIAN_POINT('Ctrl Pts',(126.435687840096,36.9992917286827,20.8878048133223));
#37735=CARTESIAN_POINT('Ctrl Pts',(126.497133839223,37.1017025621347,20.8819943890754));
#37736=CARTESIAN_POINT('Ctrl Pts',(126.56090569653,37.2079898574904,20.8759640282507));
#37737=CARTESIAN_POINT('Ctrl Pts',(126.629568996516,37.3114545241766,20.869933667426));
#37738=CARTESIAN_POINT('Ctrl Pts',(126.702836030425,37.4116249206166,20.8639033066014));
#37739=CARTESIAN_POINT('Ctrl Pts',(126.773351443211,37.5080333116351,20.8580994223698));
#37740=CARTESIAN_POINT('Ctrl Pts',(126.84813076695,37.6013900505575,20.8522955381382));
#37741=CARTESIAN_POINT('Ctrl Pts',(126.926873163261,37.6913038559994,20.8464916539067));
#37742=CARTESIAN_POINT('Ctrl Pts',(127.005603928478,37.7812043802096,20.840688626971));
#37743=CARTESIAN_POINT('Ctrl Pts',(127.088296333164,37.8676626751938,20.8348856000352));
#37744=CARTESIAN_POINT('Ctrl Pts',(127.174609845077,37.950321249028,20.8290825730995));
#37745=CARTESIAN_POINT('Ctrl Pts',(127.26093097757,38.0329871207488,20.8232790338173));
#37746=CARTESIAN_POINT('Ctrl Pts',(127.350873558014,38.1118523218728,20.817475494535));
#37747=CARTESIAN_POINT('Ctrl Pts',(127.444061337677,38.1865973317067,20.8116719552528));
#37748=CARTESIAN_POINT('Ctrl Pts',(127.537279337048,38.2613665804747,20.8058665339505));
#37749=CARTESIAN_POINT('Ctrl Pts',(127.633744310216,38.3320127253313,20.8000611126482));
#37750=CARTESIAN_POINT('Ctrl Pts',(127.733048718338,38.3982579193712,20.7942556913459));
#37751=CARTESIAN_POINT('Ctrl Pts',(127.832463096898,38.4645764738308,20.788443841077));
#37752=CARTESIAN_POINT('Ctrl Pts',(127.934722847035,38.5264841225207,20.7826319908081));
#37753=CARTESIAN_POINT('Ctrl Pts',(128.039393238391,38.583747497569,20.7768201405392));
#37754=CARTESIAN_POINT('Ctrl Pts',(128.14413237782,38.6410484835088,20.7710044730158));
#37755=CARTESIAN_POINT('Ctrl Pts',(128.25128494605,38.6936989412284,20.7651888054925));
#37756=CARTESIAN_POINT('Ctrl Pts',(128.360395032919,38.7415131366766,20.7593731379692));
#37757=CARTESIAN_POINT('Ctrl Pts',(128.469661408204,38.7893958207961,20.7535491401302));
#37758=CARTESIAN_POINT('Ctrl Pts',(128.58089051915,38.8324282690709,20.7477251422912));
#37759=CARTESIAN_POINT('Ctrl Pts',(128.693609942561,38.8704741334653,20.7419011444522));
#37760=CARTESIAN_POINT('Ctrl Pts',(128.723515020342,38.8805679087839,20.7403560060625));
#37761=CARTESIAN_POINT('Ctrl Pts',(128.753524935728,38.8903109713712,20.7388108676728));
#37762=CARTESIAN_POINT('Ctrl Pts',(128.783630750152,38.8997013793397,20.7372657292832));
#37763=CARTESIAN_POINT('Ctrl Pts',(128.897101477997,38.9350944237508,20.7314420044962));
#37764=CARTESIAN_POINT('Ctrl Pts',(129.01230123453,38.9655878970989,20.7256182797092));
#37765=CARTESIAN_POINT('Ctrl Pts',(129.128769267178,38.9910126547265,20.7197945549222));
#37766=CARTESIAN_POINT('Ctrl Pts',(129.245089716665,39.0164051952208,20.7139782097027));
#37767=CARTESIAN_POINT('Ctrl Pts',(129.36267485024,39.0367417088495,20.7081618644833));
#37768=CARTESIAN_POINT('Ctrl Pts',(129.481047661256,39.0519024507152,20.7023455192638));
#37769=CARTESIAN_POINT('Ctrl Pts',(129.59930132911,39.0670479331754,20.6965350282415));
#37770=CARTESIAN_POINT('Ctrl Pts',(129.718340694445,39.077027956149,20.6907245372191));
#37771=CARTESIAN_POINT('Ctrl Pts',(129.837678020953,39.0817737045454,20.6849140461967));
#37772=CARTESIAN_POINT('Ctrl Pts',(129.956926128178,39.086515904913,20.6791078992288));
#37773=CARTESIAN_POINT('Ctrl Pts',(130.076471346657,39.0860316017462,20.6733017522609));
#37774=CARTESIAN_POINT('Ctrl Pts',(130.195820874239,39.0803038104058,20.667495605293));
#37775=CARTESIAN_POINT('Ctrl Pts',(130.315122580235,39.0745783141066,20.6616917847621));
#37776=CARTESIAN_POINT('Ctrl Pts',(130.434228344052,39.0636135270521,20.6558879642312));
#37777=CARTESIAN_POINT('Ctrl Pts',(130.552645896426,39.0474445657925,20.6500841437003));
#37778=CARTESIAN_POINT('Ctrl Pts',(130.671043947295,39.0312782673062,20.6442812789672));
#37779=CARTESIAN_POINT('Ctrl Pts',(130.788753607771,39.0099095547256,20.6384784142341));
#37780=CARTESIAN_POINT('Ctrl Pts',(130.905288900066,38.9834252857832,20.632675549501));
#37781=CARTESIAN_POINT('Ctrl Pts',(131.021832502854,38.9569391281655,20.6268722709477));
#37782=CARTESIAN_POINT('Ctrl Pts',(131.137201172945,38.9253367799129,20.6210689923943));
#37783=CARTESIAN_POINT('Ctrl Pts',(131.250920904916,38.8887558279795,20.6152657138409));
#37784=CARTESIAN_POINT('Ctrl Pts',(131.364740372946,38.8521427933116,20.6094573456156));
#37785=CARTESIAN_POINT('Ctrl Pts',(131.476907624348,38.8105425571125,20.6036489773903));
#37786=CARTESIAN_POINT('Ctrl Pts',(131.58696538028,38.7641421176404,20.5978406091649));
#37787=CARTESIAN_POINT('Ctrl Pts',(131.69707088304,38.7177215480663,20.5920297210703));
#37788=CARTESIAN_POINT('Ctrl Pts',(131.805064697077,38.6664967994386,20.5862188329756));
#37789=CARTESIAN_POINT('Ctrl Pts',(131.910512544746,38.6107017069218,20.5804079448809));
#37790=CARTESIAN_POINT('Ctrl Pts',(132.016116110569,38.5548242200367,20.574588475665));
#37791=CARTESIAN_POINT('Ctrl Pts',(132.119165843905,38.4943631085868,20.5687690064491));
#37792=CARTESIAN_POINT('Ctrl Pts',(132.219254498625,38.4295968378704,20.5629495372332));
#37793=CARTESIAN_POINT('Ctrl Pts',(132.311149254851,38.3701327490009,20.5576064870498));
#37794=CARTESIAN_POINT('Ctrl Pts',(132.400548059744,38.3070401887662,20.5522634368664));
#37795=CARTESIAN_POINT('Ctrl Pts',(132.487160689988,38.2405642567579,20.546920386683));
#37796=CARTESIAN_POINT('Ctrl Pts',(132.487160689988,38.2405642567579,21.7969524304342));
#37797=CARTESIAN_POINT('Ctrl Pts',(132.581957177288,38.1678071446994,21.791146991881));
#37798=CARTESIAN_POINT('Ctrl Pts',(132.673521086805,38.0909156600229,21.7853415533277));
#37799=CARTESIAN_POINT('Ctrl Pts',(132.761485648567,38.010219595438,21.7795361147745));
#37800=CARTESIAN_POINT('Ctrl Pts',(132.849547686816,37.9294341088323,21.7737242430197));
#37801=CARTESIAN_POINT('Ctrl Pts',(132.934002114785,37.844835903111,21.7679123712649));
#37802=CARTESIAN_POINT('Ctrl Pts',(133.01451890325,37.7567917552742,21.7621004995101));
#37803=CARTESIAN_POINT('Ctrl Pts',(133.095088689876,37.6686896545807,21.7562848022362));
#37804=CARTESIAN_POINT('Ctrl Pts',(133.171715413802,37.577137407004,21.7504691049623));
#37805=CARTESIAN_POINT('Ctrl Pts',(133.244110279065,37.4825336850213,21.7446534076884));
#37806=CARTESIAN_POINT('Ctrl Pts',(133.316608713784,37.3877946211746,21.7388293903686));
#37807=CARTESIAN_POINT('Ctrl Pts',(133.384862973331,37.2899957033854,21.7330053730487));
#37808=CARTESIAN_POINT('Ctrl Pts',(133.448628308412,37.189563378945,21.7271813557289));
#37809=CARTESIAN_POINT('Ctrl Pts',(133.465118356053,37.1635910569523,21.7256752345277));
#37810=CARTESIAN_POINT('Ctrl Pts',(133.481308443058,37.137442740957,21.7241691133266));
#37811=CARTESIAN_POINT('Ctrl Pts',(133.497194851732,37.1111260429021,21.7226629921254));
#37812=CARTESIAN_POINT('Ctrl Pts',(133.558621507787,37.0093694537885,21.7168393984549));
#37813=CARTESIAN_POINT('Ctrl Pts',(133.615702371735,36.9047655862021,21.7110158047843));
#37814=CARTESIAN_POINT('Ctrl Pts',(133.668163334243,36.7977215449891,21.7051922111138));
#37815=CARTESIAN_POINT('Ctrl Pts',(133.720558109454,36.690812555734,21.6993759647717));
#37816=CARTESIAN_POINT('Ctrl Pts',(133.768344398241,36.581469879636,21.6935597184296));
#37817=CARTESIAN_POINT('Ctrl Pts',(133.811292182913,36.4701281904866,21.6877434720874));
#37818=CARTESIAN_POINT('Ctrl Pts',(133.854196976616,36.3588979549822,21.68193304784));
#37819=CARTESIAN_POINT('Ctrl Pts',(133.892272755379,36.2456730660014,21.6761226235926));
#37820=CARTESIAN_POINT('Ctrl Pts',(133.925336397825,36.1309107674382,21.6703121993451));
#37821=CARTESIAN_POINT('Ctrl Pts',(133.959651567533,36.01180447848,21.6642818385206));
#37822=CARTESIAN_POINT('Ctrl Pts',(133.988567467094,35.8910424945094,21.6582514776961));
#37823=CARTESIAN_POINT('Ctrl Pts',(134.011935046681,35.7691567988476,21.6522211168716));
#37824=CARTESIAN_POINT('Ctrl Pts',(134.03442503205,35.6518486496693,21.6464172326392));
#37825=CARTESIAN_POINT('Ctrl Pts',(134.051775844245,35.5335001081353,21.6406133484069));
#37826=CARTESIAN_POINT('Ctrl Pts',(134.063906187566,35.4145979964538,21.6348094641745));
#37827=CARTESIAN_POINT('Ctrl Pts',(134.076034739105,35.2957134478856,21.629006437238));
#37828=CARTESIAN_POINT('Ctrl Pts',(134.082944313849,35.1762758978996,21.6232034103014));
#37829=CARTESIAN_POINT('Ctrl Pts',(134.084605395569,35.0567781867096,21.6174003833648));
#37830=CARTESIAN_POINT('Ctrl Pts',(134.086266623946,34.9372699251213,21.6115968440816));
#37831=CARTESIAN_POINT('Ctrl Pts',(134.082678432297,34.8177019000858,21.6057933047984));
#37832=CARTESIAN_POINT('Ctrl Pts',(134.073863433234,34.6985672092126,21.5999897655152));
#37833=CARTESIAN_POINT('Ctrl Pts',(134.065045575569,34.5793938843484,21.5941843442119));
#37834=CARTESIAN_POINT('Ctrl Pts',(134.050997569646,34.4606545801337,21.5883789229086));
#37835=CARTESIAN_POINT('Ctrl Pts',(134.031793849583,34.3428368889937,21.5825735016053));
#37836=CARTESIAN_POINT('Ctrl Pts',(134.012568863177,34.2248887256653,21.5767616513353));
#37837=CARTESIAN_POINT('Ctrl Pts',(133.988176831755,34.1078646158765,21.5709498010652));
#37838=CARTESIAN_POINT('Ctrl Pts',(133.958743270378,33.9922417357144,21.5651379507951));
#37839=CARTESIAN_POINT('Ctrl Pts',(133.92929037688,33.8765429138237,21.5593222832706));
#37840=CARTESIAN_POINT('Ctrl Pts',(133.894789476611,33.7622475444473,21.553506615746));
#37841=CARTESIAN_POINT('Ctrl Pts',(133.855415376923,33.6498158379754,21.5476909482215));
#37842=CARTESIAN_POINT('Ctrl Pts',(133.81598487809,33.5372230852242,21.5418669503811));
#37843=CARTESIAN_POINT('Ctrl Pts',(133.771667398672,33.4264997012987,21.5360429525408));
#37844=CARTESIAN_POINT('Ctrl Pts',(133.722685139917,33.3180843216608,21.5302189547005));
#37845=CARTESIAN_POINT('Ctrl Pts',(133.709689879603,33.2893211303304,21.5286738163193));
#37846=CARTESIAN_POINT('Ctrl Pts',(133.696366524453,33.2607202477137,21.5271286779382));
#37847=CARTESIAN_POINT('Ctrl Pts',(133.682719745472,33.2322895383264,21.525583539557));
#37848=CARTESIAN_POINT('Ctrl Pts',(133.631285325959,33.1251347997844,21.5197599458861));
#37849=CARTESIAN_POINT('Ctrl Pts',(133.575087319942,33.0200539820138,21.5139363522152));
#37850=CARTESIAN_POINT('Ctrl Pts',(133.514315961415,32.9174995021992,21.5081127585444));
#37851=CARTESIAN_POINT('Ctrl Pts',(133.453621274985,32.8150744100946,21.502296512202));
#37852=CARTESIAN_POINT('Ctrl Pts',(133.3883649187,32.7151696645755,21.4964802658595));
#37853=CARTESIAN_POINT('Ctrl Pts',(133.318784353857,32.6182159181412,21.4906640195171));
#37854=CARTESIAN_POINT('Ctrl Pts',(133.249273439543,32.5213592229423,21.4848535952694));
#37855=CARTESIAN_POINT('Ctrl Pts',(133.175447164514,32.4274479801172,21.4790431710217));
#37856=CARTESIAN_POINT('Ctrl Pts',(133.097587573901,32.3368859915481,21.473232746774));
#37857=CARTESIAN_POINT('Ctrl Pts',(133.016780836731,32.2428960443836,21.4672023859496));
#37858=CARTESIAN_POINT('Ctrl Pts',(132.93162964079,32.1525142992767,21.4611720251252));
#37859=CARTESIAN_POINT('Ctrl Pts',(132.842497217893,32.0661570310819,21.4551416643008));
#37860=CARTESIAN_POINT('Ctrl Pts',(132.756712257601,31.9830430016163,21.4493377800682));
#37861=CARTESIAN_POINT('Ctrl Pts',(132.667240035615,31.9036569231099,21.4435338958356));
#37862=CARTESIAN_POINT('Ctrl Pts',(132.574443152638,31.8283336471449,21.437730011603));
#37863=CARTESIAN_POINT('Ctrl Pts',(132.481659976754,31.7530214972334,21.4319269846662));
#37864=CARTESIAN_POINT('Ctrl Pts',(132.385553433453,31.6817712136875,21.4261239577293));
#37865=CARTESIAN_POINT('Ctrl Pts',(132.286519540348,31.6148776400836,21.4203209307925));
#37866=CARTESIAN_POINT('Ctrl Pts',(132.187476903586,31.5479781604763,21.4145173915091));
#37867=CARTESIAN_POINT('Ctrl Pts',(132.085506741543,31.485436384164,21.4087138522256));
#37868=CARTESIAN_POINT('Ctrl Pts',(131.981033862242,31.4275036967617,21.4029103129421));
#37869=CARTESIAN_POINT('Ctrl Pts',(131.876527103605,31.3695522224648,21.3971048916386));
#37870=CARTESIAN_POINT('Ctrl Pts',(131.769516370539,31.316213007569,21.3912994703351));
#37871=CARTESIAN_POINT('Ctrl Pts',(131.660450273352,31.2676910779353,21.3854940490316));
#37872=CARTESIAN_POINT('Ctrl Pts',(131.551263395558,31.2191154147557,21.3796821987613));
#37873=CARTESIAN_POINT('Ctrl Pts',(131.440016983603,31.1753678514284,21.373870348491));
#37874=CARTESIAN_POINT('Ctrl Pts',(131.327178936584,31.1366049813295,21.3680584982208));
#37875=CARTESIAN_POINT('Ctrl Pts',(131.214266776929,31.0978166515693,21.362242830696));
#37876=CARTESIAN_POINT('Ctrl Pts',(131.099761291014,31.0640196505654,21.3564271631713));
#37877=CARTESIAN_POINT('Ctrl Pts',(130.984143208553,31.0353200450656,21.3506114956465));
#37878=CARTESIAN_POINT('Ctrl Pts',(130.868359515674,31.00657933048,21.344787497806));
#37879=CARTESIAN_POINT('Ctrl Pts',(130.751460444184,30.9829506653462,21.3389634999656));
#37880=CARTESIAN_POINT('Ctrl Pts',(130.633934658758,30.9644886509359,21.3331395021251));
#37881=CARTESIAN_POINT('Ctrl Pts',(130.602754427147,30.95959057786,21.3315943637462));
#37882=CARTESIAN_POINT('Ctrl Pts',(130.571530096222,30.9550558855625,21.3300492253674));
#37883=CARTESIAN_POINT('Ctrl Pts',(130.540270804111,30.9508849783904,21.3285040869885));
#37884=CARTESIAN_POINT('Ctrl Pts',(130.422455197195,30.9351649179955,21.3226804933118));
#37885=CARTESIAN_POINT('Ctrl Pts',(130.303762933155,30.9245658317405,21.316856899635));
#37886=CARTESIAN_POINT('Ctrl Pts',(130.184676680017,30.9191766120233,21.3110333059582));
#37887=CARTESIAN_POINT('Ctrl Pts',(130.065740671877,30.9137941916072,21.3052170596099));
#37888=CARTESIAN_POINT('Ctrl Pts',(129.946412067636,30.9136085824429,21.2994008132616));
#37889=CARTESIAN_POINT('Ctrl Pts',(129.827181220253,30.9186572467671,21.2935845669133));
#37890=CARTESIAN_POINT('Ctrl Pts',(129.708069723606,30.9237008573504,21.2877741426596));
#37891=CARTESIAN_POINT('Ctrl Pts',(129.589056194773,30.9339683008373,21.281963718406));
#37892=CARTESIAN_POINT('Ctrl Pts',(129.470632968865,30.9494450323014,21.2761532941524));
#37893=CARTESIAN_POINT('Ctrl Pts',(129.347727179069,30.965507590043,21.2701229333302));
#37894=CARTESIAN_POINT('Ctrl Pts',(129.225457711304,30.9871816126831,21.264092572508));
#37895=CARTESIAN_POINT('Ctrl Pts',(129.104371836297,31.0143914903265,21.2580622116858));
#37896=CARTESIAN_POINT('Ctrl Pts',(128.987833469492,31.0405794722142,21.2522583274473));
#37897=CARTESIAN_POINT('Ctrl Pts',(128.872391830745,31.0718949003306,21.2464544432088));
#37898=CARTESIAN_POINT('Ctrl Pts',(128.758525744759,31.1082180593493,21.2406505589702));
#37899=CARTESIAN_POINT('Ctrl Pts',(128.644676478012,31.144535853049,21.2348475320275));
#37900=CARTESIAN_POINT('Ctrl Pts',(128.532402690125,31.1858597825661,21.2290445050847));
#37901=CARTESIAN_POINT('Ctrl Pts',(128.422168062189,31.2320202527054,21.223241478142));
#37902=CARTESIAN_POINT('Ctrl Pts',(128.311923701688,31.2781847983314,21.2174379388526));
#37903=CARTESIAN_POINT('Ctrl Pts',(128.20371923576,31.3291865758626,21.2116343995633));
#37904=CARTESIAN_POINT('Ctrl Pts',(128.097997780366,31.3848080885647,21.205830860274));
#37905=CARTESIAN_POINT('Ctrl Pts',(127.992242040738,31.4404476386743,21.2000254389646));
#37906=CARTESIAN_POINT('Ctrl Pts',(127.888971274215,31.5007097133633,21.1942200176552));
#37907=CARTESIAN_POINT('Ctrl Pts',(127.788602870344,31.5653314956245,21.1884145963458));
#37908=CARTESIAN_POINT('Ctrl Pts',(127.688123317757,31.6300248405274,21.1826027460697));
#37909=CARTESIAN_POINT('Ctrl Pts',(127.590552886969,31.6990873088665,21.1767908957936));
#37910=CARTESIAN_POINT('Ctrl Pts',(127.496279033403,31.7722134021245,21.1709790455175));
#37911=CARTESIAN_POINT('Ctrl Pts',(127.401943260266,31.8453875249926,21.165163377987));
#37912=CARTESIAN_POINT('Ctrl Pts',(127.310908687063,31.9226303246013,21.1593477104565));
#37913=CARTESIAN_POINT('Ctrl Pts',(127.223527543484,32.0035978744157,21.153532042926));
#37914=CARTESIAN_POINT('Ctrl Pts',(127.136021235853,32.0846814015008,21.1477080450798));
#37915=CARTESIAN_POINT('Ctrl Pts',(127.052179088958,32.1695000383912,21.1418840472337));
#37916=CARTESIAN_POINT('Ctrl Pts',(126.972314637902,32.257675010481,21.1360600493875));
#37917=CARTESIAN_POINT('Ctrl Pts',(126.951126164419,32.2810683104198,21.134514911065));
#37918=CARTESIAN_POINT('Ctrl Pts',(126.930217438476,32.3046976858427,21.1329697727426));
#37919=CARTESIAN_POINT('Ctrl Pts',(126.909593807446,32.3285557155312,21.1314246344201));
#37920=CARTESIAN_POINT('Ctrl Pts',(126.830727378882,32.4197907454494,21.1255159008441));
#37921=CARTESIAN_POINT('Ctrl Pts',(126.755762331176,32.5146859737786,21.119607167268));
#37922=CARTESIAN_POINT('Ctrl Pts',(126.685059339014,32.6128692088321,21.113698433692));
#37923=CARTESIAN_POINT('Ctrl Pts',(126.616054083285,32.7086948455693,21.1079315819792));
#37924=CARTESIAN_POINT('Ctrl Pts',(126.551108816856,32.8076520357571,21.1021647302665));
#37925=CARTESIAN_POINT('Ctrl Pts',(126.490521185756,32.9093581243135,21.0963978785537));
#37926=CARTESIAN_POINT('Ctrl Pts',(126.429989538291,33.0109702353308,21.0906363554751));
#37927=CARTESIAN_POINT('Ctrl Pts',(126.373807733832,33.1153258409295,21.0848748323964));
#37928=CARTESIAN_POINT('Ctrl Pts',(126.322231234451,33.2220118371735,21.0791133093178));
#37929=CARTESIAN_POINT('Ctrl Pts',(126.270689699325,33.3286255098504,21.0733556920367));
#37930=CARTESIAN_POINT('Ctrl Pts',(126.223747441911,33.4375660589538,21.0675980747555));
#37931=CARTESIAN_POINT('Ctrl Pts',(126.181614543347,33.5483948524396,21.0618404574744));
#37932=CARTESIAN_POINT('Ctrl Pts',(126.137570474999,33.6642508965696,21.0558216717345));
#37933=CARTESIAN_POINT('Ctrl Pts',(126.098782575629,33.7821701062652,21.0498028859946));
#37934=CARTESIAN_POINT('Ctrl Pts',(126.065434963677,33.901627123905,21.0437841002547));
#37935=CARTESIAN_POINT('Ctrl Pts',(126.033547892698,34.0158522266135,21.0380289220918));
#37936=CARTESIAN_POINT('Ctrl Pts',(126.00663474156,34.1314828411935,21.032273743929));
#37937=CARTESIAN_POINT('Ctrl Pts',(125.984805368352,34.248044502657,21.0265185657661));
#37938=CARTESIAN_POINT('Ctrl Pts',(125.962975205302,34.3646103816137,21.0207631793664));
#37939=CARTESIAN_POINT('Ctrl Pts',(125.946229255171,34.4821069644494,21.0150077929668));
#37940=CARTESIAN_POINT('Ctrl Pts',(125.934625988469,34.6000510703047,21.0092524065671));
#37941=CARTESIAN_POINT('Ctrl Pts',(125.923016652512,34.718056868503,21.0034940097307));
#37942=CARTESIAN_POINT('Ctrl Pts',(125.916555398921,34.8365102423957,20.9977356128943));
#37943=CARTESIAN_POINT('Ctrl Pts',(125.915248694863,34.9549247830873,20.9919772160579));
#37944=CARTESIAN_POINT('Ctrl Pts',(125.915070017821,34.9711166359783,20.9911898202371));
#37945=CARTESIAN_POINT('Ctrl Pts',(125.91498763816,34.9873077646516,20.9904024244163));
#37946=CARTESIAN_POINT('Ctrl Pts',(125.915001496758,35.0034969286478,20.9896150285955));
#37947=CARTESIAN_POINT('Origin',(130.,35.,32.7603849714045));
#37948=CARTESIAN_POINT('',(132.487160689988,38.2405642567579,23.046779218902));
#37949=CARTESIAN_POINT('',(132.487160689988,38.2405642567579,22.9427607387674));
#37950=CARTESIAN_POINT('',(132.487160689988,38.2405642567579,32.7603849714045));
#37951=CARTESIAN_POINT('',(125.915000225098,35.0013561159219,22.1353849714387));
#37952=CARTESIAN_POINT('Ctrl Pts',(132.487160689988,38.2405642567579,22.9427607387674));
#37953=CARTESIAN_POINT('Ctrl Pts',(132.581883195482,38.1678639263663,22.9369379450951));
#37954=CARTESIAN_POINT('Ctrl Pts',(132.673310088235,38.0910879523884,22.9311151514228));
#37955=CARTESIAN_POINT('Ctrl Pts',(132.761090362255,38.010582171518,22.9252923577505));
#37956=CARTESIAN_POINT('Ctrl Pts',(132.825958211529,37.9510900257316,22.9209894308514));
#37957=CARTESIAN_POINT('Ctrl Pts',(132.888835416071,37.8895618693979,22.9166865039523));
#37958=CARTESIAN_POINT('Ctrl Pts',(132.949594421577,37.82614892534,22.9123835770533));
#37959=CARTESIAN_POINT('Ctrl Pts',(133.031825834812,37.7403256640177,22.9065599833817));
#37960=CARTESIAN_POINT('Ctrl Pts',(133.110440991607,37.6507720417041,22.9007363897102));
#37961=CARTESIAN_POINT('Ctrl Pts',(133.185083236695,37.5578252042159,22.8949127960387));
#37962=CARTESIAN_POINT('Ctrl Pts',(133.259631309504,37.4649956329692,22.8890965496956));
#37963=CARTESIAN_POINT('Ctrl Pts',(133.330216186761,37.3687816770207,22.8832803033525));
#37964=CARTESIAN_POINT('Ctrl Pts',(133.396518192138,37.2695570427899,22.8774640570094));
#37965=CARTESIAN_POINT('Ctrl Pts',(133.462753828841,37.1704317329654,22.8716536327609));
#37966=CARTESIAN_POINT('Ctrl Pts',(133.524714896913,37.0683020778175,22.8658432085125));
#37967=CARTESIAN_POINT('Ctrl Pts',(133.582122530858,36.9635740815967,22.8600327842641));
#37968=CARTESIAN_POINT('Ctrl Pts',(133.641703162486,36.8548819141061,22.8540024234399));
#37969=CARTESIAN_POINT('Ctrl Pts',(133.696378554533,36.7433911632705,22.8479720626158));
#37970=CARTESIAN_POINT('Ctrl Pts',(133.74588670753,36.6295882223287,22.8419417017917));
#37971=CARTESIAN_POINT('Ctrl Pts',(133.793535529379,36.5200592714251,22.8361378175583));
#37972=CARTESIAN_POINT('Ctrl Pts',(133.836398057633,36.4083890800444,22.830333933325));
#37973=CARTESIAN_POINT('Ctrl Pts',(133.874288296302,36.2950348246802,22.8245300490917));
#37974=CARTESIAN_POINT('Ctrl Pts',(133.912172938179,36.1816973129518,22.8187270221542));
#37975=CARTESIAN_POINT('Ctrl Pts',(133.945086621664,36.0666766191031,22.8129239952166));
#37976=CARTESIAN_POINT('Ctrl Pts',(133.972892553101,35.9504471376738,22.8071209682791));
#37977=CARTESIAN_POINT('Ctrl Pts',(134.000700939511,35.8342073943968,22.8013174289949));
#37978=CARTESIAN_POINT('Ctrl Pts',(134.023400582241,35.7167590484978,22.7955138897108));
#37979=CARTESIAN_POINT('Ctrl Pts',(134.040905493144,35.598588168512,22.7897103504266));
#37980=CARTESIAN_POINT('Ctrl Pts',(134.058416080684,35.480378967088,22.7839049291224));
#37981=CARTESIAN_POINT('Ctrl Pts',(134.070728526322,35.3614471693103,22.7780995078181));
#37982=CARTESIAN_POINT('Ctrl Pts',(134.077808610295,35.2422848278376,22.7722940865139));
#37983=CARTESIAN_POINT('Ctrl Pts',(134.084896534807,35.1229905251014,22.7664822362429));
#37984=CARTESIAN_POINT('Ctrl Pts',(134.086740507389,35.0034655769178,22.7606703859719));
#37985=CARTESIAN_POINT('Ctrl Pts',(134.083358430272,34.8842030659968,22.7548585357009));
#37986=CARTESIAN_POINT('Ctrl Pts',(134.079974131789,34.7648622228184,22.7490428681754));
#37987=CARTESIAN_POINT('Ctrl Pts',(134.071356977107,34.6457845665179,22.7432272006499));
#37988=CARTESIAN_POINT('Ctrl Pts',(134.057576680408,34.5274574277291,22.7374115331245));
#37989=CARTESIAN_POINT('Ctrl Pts',(134.043776644923,34.4089607980912,22.7315875352833));
#37990=CARTESIAN_POINT('Ctrl Pts',(134.024798770866,34.29121723338,22.7257635374421));
#37991=CARTESIAN_POINT('Ctrl Pts',(134.000763742125,34.1747033989525,22.7199395396009));
#37992=CARTESIAN_POINT('Ctrl Pts',(133.994387117992,34.1437916435994,22.7183944012289));
#37993=CARTESIAN_POINT('Ctrl Pts',(133.987654806676,34.1129663576886,22.7168492628568));
#37994=CARTESIAN_POINT('Ctrl Pts',(133.980569642328,34.0822362381437,22.7153041244848));
#37995=CARTESIAN_POINT('Ctrl Pts',(133.953865808544,33.9664150709629,22.7094805308134));
#37996=CARTESIAN_POINT('Ctrl Pts',(133.9220597084,33.8515735882992,22.7036569371421));
#37997=CARTESIAN_POINT('Ctrl Pts',(133.885237815503,33.7381948973842,22.6978333434707));
#37998=CARTESIAN_POINT('Ctrl Pts',(133.848462378892,33.6249592505289,22.6920170971277));
#37999=CARTESIAN_POINT('Ctrl Pts',(133.806683861123,33.5131831096538,22.6862008507848));
#38000=CARTESIAN_POINT('Ctrl Pts',(133.760039584541,33.4033386950636,22.6803846044418));
#38001=CARTESIAN_POINT('Ctrl Pts',(133.713441999138,33.2936042353385,22.6745741801936));
#38002=CARTESIAN_POINT('Ctrl Pts',(133.661988503165,33.1857980287977,22.6687637559453));
#38003=CARTESIAN_POINT('Ctrl Pts',(133.605865802955,33.0803758672377,22.6629533316971));
#38004=CARTESIAN_POINT('Ctrl Pts',(133.547618742458,32.9709632588102,22.6569229708729));
#38005=CARTESIAN_POINT('Ctrl Pts',(133.48434215393,32.8641191697739,22.6508926100487));
#38006=CARTESIAN_POINT('Ctrl Pts',(133.416299224074,32.7603293519825,22.6448622492245));
#38007=CARTESIAN_POINT('Ctrl Pts',(133.350811718553,32.6604374707826,22.6390583649913));
#38008=CARTESIAN_POINT('Ctrl Pts',(133.280909669464,32.5633749574022,22.6332544807582));
#38009=CARTESIAN_POINT('Ctrl Pts',(133.206873489809,32.4695479810198,22.627450596525));
#38010=CARTESIAN_POINT('Ctrl Pts',(133.13284824609,32.3757348638852,22.6216475695876));
#38011=CARTESIAN_POINT('Ctrl Pts',(133.054690339081,32.2851566537826,22.6158445426502));
#38012=CARTESIAN_POINT('Ctrl Pts',(132.972721553387,32.1981878067883,22.6100415157128));
#38013=CARTESIAN_POINT('Ctrl Pts',(132.890745530706,32.1112112813543,22.6042379764288));
#38014=CARTESIAN_POINT('Ctrl Pts',(132.804958240457,32.0278450497876,22.5984344371448));
#38015=CARTESIAN_POINT('Ctrl Pts',(132.715719080768,31.948427475161,22.5926308978608));
#38016=CARTESIAN_POINT('Ctrl Pts',(132.62645098186,31.8689841463411,22.5868254765567));
#38017=CARTESIAN_POINT('Ctrl Pts',(132.533729092154,31.7934922924173,22.5810200552526));
#38018=CARTESIAN_POINT('Ctrl Pts',(132.437946192268,31.7222502591559,22.5752146339485));
#38019=CARTESIAN_POINT('Ctrl Pts',(132.342057221687,31.6509293319369,22.5694027836777));
#38020=CARTESIAN_POINT('Ctrl Pts',(132.243100802464,31.5838678633661,22.5635909334068));
#38021=CARTESIAN_POINT('Ctrl Pts',(132.141499148099,31.521321170517,22.557779083136));
#38022=CARTESIAN_POINT('Ctrl Pts',(132.039830761221,31.4587333966643,22.5519634156107));
#38023=CARTESIAN_POINT('Ctrl Pts',(131.935514035084,31.4006665022058,22.5461477480853));
#38024=CARTESIAN_POINT('Ctrl Pts',(131.828994773743,31.347329317113,22.54033208056));
#38025=CARTESIAN_POINT('Ctrl Pts',(131.722322935062,31.2939157322621,22.534508082719));
#38026=CARTESIAN_POINT('Ctrl Pts',(131.613442635645,31.2452455449521,22.5286840848779));
#38027=CARTESIAN_POINT('Ctrl Pts',(131.502818699154,31.201479109249,22.5228600870369));
#38028=CARTESIAN_POINT('Ctrl Pts',(131.473469565799,31.1898676352888,22.5213149486634));
#38029=CARTESIAN_POINT('Ctrl Pts',(131.443997778231,31.1786010472255,22.5197698102899));
#38030=CARTESIAN_POINT('Ctrl Pts',(131.414412163886,31.1676817419932,22.5182246719164));
#38031=CARTESIAN_POINT('Ctrl Pts',(131.302904612573,31.1265271127782,22.512401078245));
#38032=CARTESIAN_POINT('Ctrl Pts',(131.189419564544,31.0901768992921,22.5065774845737));
#38033=CARTESIAN_POINT('Ctrl Pts',(131.07440847843,31.0588235992945,22.5007538909023));
#38034=CARTESIAN_POINT('Ctrl Pts',(130.959542495884,31.0275098561421,22.4949376445594));
#38035=CARTESIAN_POINT('Ctrl Pts',(130.843154695164,31.0011805937281,22.4891213982165));
#38036=CARTESIAN_POINT('Ctrl Pts',(130.725715302816,30.9799798135757,22.4833051518736));
#38037=CARTESIAN_POINT('Ctrl Pts',(130.608393467947,30.9588002555212,22.4774947276254));
#38038=CARTESIAN_POINT('Ctrl Pts',(130.490022535097,30.9427390391147,22.4716843033771));
#38039=CARTESIAN_POINT('Ctrl Pts',(130.371086060982,30.9318898570289,22.4658738791289));
#38040=CARTESIAN_POINT('Ctrl Pts',(130.247647595317,30.9206300109608,22.4598435183047));
#38041=CARTESIAN_POINT('Ctrl Pts',(130.123600361081,30.9149846857911,22.4538131574805));
#38042=CARTESIAN_POINT('Ctrl Pts',(129.999494896475,30.9150000312276,22.4477827966563));
#38043=CARTESIAN_POINT('Ctrl Pts',(129.880050344106,30.91501480035,22.4419789124232));
#38044=CARTESIAN_POINT('Ctrl Pts',(129.760552301349,30.9202727227172,22.43617502819));
#38045=CARTESIAN_POINT('Ctrl Pts',(129.641494188579,30.930761916135,22.4303711439569));
#38046=CARTESIAN_POINT('Ctrl Pts',(129.522453661966,30.9412495601867,22.4245681170196));
#38047=CARTESIAN_POINT('Ctrl Pts',(129.403853342763,30.9569669027769,22.4187650900822));
#38048=CARTESIAN_POINT('Ctrl Pts',(129.286182805827,30.9778500757303,22.4129620631448));
#38049=CARTESIAN_POINT('Ctrl Pts',(129.168501879813,30.9987350924494,22.4071585238609));
#38050=CARTESIAN_POINT('Ctrl Pts',(129.051751301354,31.0247867749896,22.4013549845769));
#38051=CARTESIAN_POINT('Ctrl Pts',(128.936411076524,31.0558900114399,22.395551445293));
#38052=CARTESIAN_POINT('Ctrl Pts',(128.821033448205,31.087003334307,22.3897460239889));
#38053=CARTESIAN_POINT('Ctrl Pts',(128.707067477153,31.123171362753,22.3839406026848));
#38054=CARTESIAN_POINT('Ctrl Pts',(128.594977999189,31.1642291286838,22.3781351813808));
#38055=CARTESIAN_POINT('Ctrl Pts',(128.482764392503,31.2053323622901,22.37232333111));
#38056=CARTESIAN_POINT('Ctrl Pts',(128.372431810507,31.2513360015191,22.3665114808392));
#38057=CARTESIAN_POINT('Ctrl Pts',(128.264425235097,31.3020268747014,22.3606996305683));
#38058=CARTESIAN_POINT('Ctrl Pts',(128.156347720387,31.3527510419214,22.3548839630431));
#38059=CARTESIAN_POINT('Ctrl Pts',(128.050599615635,31.4081683851012,22.3490682955178));
#38060=CARTESIAN_POINT('Ctrl Pts',(127.947599953747,31.4680205195754,22.3432526279925));
#38061=CARTESIAN_POINT('Ctrl Pts',(127.844452755965,31.5279583857694,22.3374286301515));
#38062=CARTESIAN_POINT('Ctrl Pts',(127.744062201283,31.5923435025609,22.3316046323105));
#38063=CARTESIAN_POINT('Ctrl Pts',(127.646817204615,31.6608750051096,22.3257806344695));
#38064=CARTESIAN_POINT('Ctrl Pts',(127.621017576916,31.6790567863011,22.3242354960956));
#38065=CARTESIAN_POINT('Ctrl Pts',(127.595439167258,31.6975302058238,22.3226903577218));
#38066=CARTESIAN_POINT('Ctrl Pts',(127.570088819246,31.7162891945781,22.321145219348));
#38067=CARTESIAN_POINT('Ctrl Pts',(127.475346633759,31.7863974073423,22.315370553598));
#38068=CARTESIAN_POINT('Ctrl Pts',(127.383475506378,31.8607319425041,22.309595887848));
#38069=CARTESIAN_POINT('Ctrl Pts',(127.29488013663,31.9390276831043,22.3038212220981));
#38070=CARTESIAN_POINT('Ctrl Pts',(127.206396987135,32.017224249585,22.2980538708889));
#38071=CARTESIAN_POINT('Ctrl Pts',(127.121181654223,32.0993717724542,22.2922865196798));
#38072=CARTESIAN_POINT('Ctrl Pts',(127.039608898643,32.1851626109122,22.2865191684707));
#38073=CARTESIAN_POINT('Ctrl Pts',(126.958117264671,32.2708681330083,22.2807575527157));
#38074=CARTESIAN_POINT('Ctrl Pts',(126.880261289031,32.3602094655443,22.2749959369607));
#38075=CARTESIAN_POINT('Ctrl Pts',(126.806381191527,32.4528400312956,22.2692343212058));
#38076=CARTESIAN_POINT('Ctrl Pts',(126.732553088089,32.5454054070996,22.2634767602617));
#38077=CARTESIAN_POINT('Ctrl Pts',(126.662695556032,32.6412550877788,22.2577191993177));
#38078=CARTESIAN_POINT('Ctrl Pts',(126.597110128044,32.7400076284779,22.2519616383736));
#38079=CARTESIAN_POINT('Ctrl Pts',(126.531548751071,32.838723955358,22.2462061888008));
#38080=CARTESIAN_POINT('Ctrl Pts',(126.470256594024,32.9403406802227,22.2404507392279));
#38081=CARTESIAN_POINT('Ctrl Pts',(126.413492877873,33.0444459447694,22.234695289655));
#38082=CARTESIAN_POINT('Ctrl Pts',(126.356735998232,33.1485386710813,22.2289405332573));
#38083=CARTESIAN_POINT('Ctrl Pts',(126.304506673963,33.2551189758186,22.2231857768595));
#38084=CARTESIAN_POINT('Ctrl Pts',(126.257018645827,33.3637495355807,22.2174310204618));
#38085=CARTESIAN_POINT('Ctrl Pts',(126.209524641705,33.4723937656241,22.2116755398743));
#38086=CARTESIAN_POINT('Ctrl Pts',(126.166773285702,33.5830883820817,22.2059200592868));
#38087=CARTESIAN_POINT('Ctrl Pts',(126.128930263854,33.6953758786946,22.2001645786993));
#38088=CARTESIAN_POINT('Ctrl Pts',(126.091051218588,33.8077702636893,22.1944036193717));
#38089=CARTESIAN_POINT('Ctrl Pts',(126.058089971145,33.9217601619959,22.1886426600441));
#38090=CARTESIAN_POINT('Ctrl Pts',(126.030162393893,34.0368726038889,22.1828817007166));
#38091=CARTESIAN_POINT('Ctrl Pts',(126.002220875287,34.1520425095357,22.177117865537));
#38092=CARTESIAN_POINT('Ctrl Pts',(125.979318111483,34.2683356667431,22.1713540303574));
#38093=CARTESIAN_POINT('Ctrl Pts',(125.961518545287,34.3852703521541,22.1655901951778));
#38094=CARTESIAN_POINT('Ctrl Pts',(125.943692203765,34.5023809387283,22.1598176896425));
#38095=CARTESIAN_POINT('Ctrl Pts',(125.930984437042,34.6201345674989,22.1540451841073));
#38096=CARTESIAN_POINT('Ctrl Pts',(125.923407691792,34.7380455141447,22.148272678572));
#38097=CARTESIAN_POINT('Ctrl Pts',(125.917769073044,34.8257949174097,22.1439767761942));
#38098=CARTESIAN_POINT('Ctrl Pts',(125.914971102718,34.9136313779439,22.1396808738165));
#38099=CARTESIAN_POINT('Ctrl Pts',(125.915000225098,35.0013561159219,22.1353849714387));
#38100=CARTESIAN_POINT('Ctrl Pts',(125.915000225098,35.0013561166197,22.1353849714045));
#38101=CARTESIAN_POINT('Ctrl Pts',(125.915025803142,35.078404287374,22.1316119031962));
#38102=CARTESIAN_POINT('Ctrl Pts',(125.917231078305,35.1554131039327,22.1278388349879));
#38103=CARTESIAN_POINT('Ctrl Pts',(125.921610227948,35.2322969376113,22.1240657667795));
#38104=CARTESIAN_POINT('Ctrl Pts',(125.928369286289,35.3509643410231,22.118242173109));
#38105=CARTESIAN_POINT('Ctrl Pts',(125.940322775489,35.4695278608721,22.1124185794384));
#38106=CARTESIAN_POINT('Ctrl Pts',(125.957467056685,35.5874967252762,22.1065949857679));
#38107=CARTESIAN_POINT('Ctrl Pts',(125.974589707823,35.7053167544351,22.1007787394258));
#38108=CARTESIAN_POINT('Ctrl Pts',(125.99689006703,35.8225432198411,22.0949624930836));
#38109=CARTESIAN_POINT('Ctrl Pts',(126.024312538453,35.9386874922439,22.0891462467415));
#38110=CARTESIAN_POINT('Ctrl Pts',(126.05170755983,36.0547155035892,22.0833358224941));
#38111=CARTESIAN_POINT('Ctrl Pts',(126.084214400078,36.1696630818593,22.0775253982467));
#38112=CARTESIAN_POINT('Ctrl Pts',(126.121726014142,36.2830494497948,22.0717149739992));
#38113=CARTESIAN_POINT('Ctrl Pts',(126.160657520395,36.400727726305,22.0656846131747));
#38114=CARTESIAN_POINT('Ctrl Pts',(126.204980104197,36.5167238235885,22.0596542523502));
#38115=CARTESIAN_POINT('Ctrl Pts',(126.254516398774,36.6305145178578,22.0536238915257));
#38116=CARTESIAN_POINT('Ctrl Pts',(126.302192305306,36.7400316820007,22.0478200072933));
#38117=CARTESIAN_POINT('Ctrl Pts',(126.354697194334,36.8475057002338,22.042016123061));
#38118=CARTESIAN_POINT('Ctrl Pts',(126.411823279439,36.9524888788482,22.0362122388286));
#38119=CARTESIAN_POINT('Ctrl Pts',(126.468940926411,37.0574565503245,22.0304092118921));
#38120=CARTESIAN_POINT('Ctrl Pts',(126.530678216865,37.1599337552884,22.0246061849555));
#38121=CARTESIAN_POINT('Ctrl Pts',(126.596781231034,37.259497070269,22.0188031580189));
#38122=CARTESIAN_POINT('Ctrl Pts',(126.662890081407,37.3590691756493,22.0129996187357));
#38123=CARTESIAN_POINT('Ctrl Pts',(126.733365195989,37.4557265393365,22.0071960794525));
#38124=CARTESIAN_POINT('Ctrl Pts',(126.807909486028,37.5490749597867,22.0013925401693));
#38125=CARTESIAN_POINT('Ctrl Pts',(126.882477949912,37.6424536520411,21.995587118866));
#38126=CARTESIAN_POINT('Ctrl Pts',(126.961117958937,37.7325209480832,21.9897816975627));
#38127=CARTESIAN_POINT('Ctrl Pts',(127.043492762843,37.8189164508089,21.9839762762594));
#38128=CARTESIAN_POINT('Ctrl Pts',(127.125958789221,37.9054076285574,21.9781644259893));
#38129=CARTESIAN_POINT('Ctrl Pts',(127.212167584224,37.9882186008555,21.9723525757192));
#38130=CARTESIAN_POINT('Ctrl Pts',(127.301746120356,38.0670264102195,21.9665407254491));
#38131=CARTESIAN_POINT('Ctrl Pts',(127.391383492151,38.1458859809759,21.9607250579246));
#38132=CARTESIAN_POINT('Ctrl Pts',(127.48439469546,38.2207368970648,21.9549093904001));
#38133=CARTESIAN_POINT('Ctrl Pts',(127.580375599856,38.2912980360687,21.9490937228755));
#38134=CARTESIAN_POINT('Ctrl Pts',(127.676493986535,38.3619602462851,21.9432697250352));
#38135=CARTESIAN_POINT('Ctrl Pts',(127.775590226523,38.4283201886456,21.9374457271949));
#38136=CARTESIAN_POINT('Ctrl Pts',(127.877233255863,38.4901413080254,21.9316217293546));
#38137=CARTESIAN_POINT('Ctrl Pts',(127.904199705734,38.5065427880636,21.9300765909734));
#38138=CARTESIAN_POINT('Ctrl Pts',(127.931345296024,38.5226250517945,21.9285314525923));
#38139=CARTESIAN_POINT('Ctrl Pts',(127.958661730927,38.5383842458413,21.9269863142111));
#38140=CARTESIAN_POINT('Ctrl Pts',(128.061616792656,38.5977803127745,21.9211627205402));
#38141=CARTESIAN_POINT('Ctrl Pts',(128.167332366969,38.6527749624344,21.9153391268693));
#38142=CARTESIAN_POINT('Ctrl Pts',(128.275395991734,38.703102214991,21.9095155331985));
#38143=CARTESIAN_POINT('Ctrl Pts',(128.383323278184,38.753365972243,21.903699286856));
#38144=CARTESIAN_POINT('Ctrl Pts',(128.493592356013,38.798973873836,21.8978830405136));
#38145=CARTESIAN_POINT('Ctrl Pts',(128.605764074193,38.8397045697801,21.8920667941712));
#38146=CARTESIAN_POINT('Ctrl Pts',(128.717823507865,38.8803944940726,21.8862563699235));
#38147=CARTESIAN_POINT('Ctrl Pts',(128.831781411403,38.916216786502,21.8804459456757));
#38148=CARTESIAN_POINT('Ctrl Pts',(128.947176998382,38.9469974318795,21.874635521428));
#38149=CARTESIAN_POINT('Ctrl Pts',(129.066940547024,38.9789431883545,21.8686051606036));
#38150=CARTESIAN_POINT('Ctrl Pts',(129.188252361852,39.0054578937423,21.8625747997792));
#38151=CARTESIAN_POINT('Ctrl Pts',(129.310577607581,39.026403080273,21.8565444389548));
#38152=CARTESIAN_POINT('Ctrl Pts',(129.428308799066,39.0465616481256,21.8507405547222));
#38153=CARTESIAN_POINT('Ctrl Pts',(129.546978234583,39.061561416186,21.8449366704896));
#38154=CARTESIAN_POINT('Ctrl Pts',(129.666097575086,39.0713307616351,21.839132786257));
#38155=CARTESIAN_POINT('Ctrl Pts',(129.785199320388,39.0810986640474,21.8333297593201));
#38156=CARTESIAN_POINT('Ctrl Pts',(129.904750431655,39.0856376469167,21.8275267323833));
#38157=CARTESIAN_POINT('Ctrl Pts',(130.024257580145,39.0849279760854,21.8217237054465));
#38158=CARTESIAN_POINT('Ctrl Pts',(130.143775279867,39.0842182425977,21.815920166163));
#38159=CARTESIAN_POINT('Ctrl Pts',(130.263248600746,39.0782589364807,21.8101166268796));
#38160=CARTESIAN_POINT('Ctrl Pts',(130.382184990753,39.0670824472641,21.8043130875962));
#38161=CARTESIAN_POINT('Ctrl Pts',(130.501159950443,39.0559023336424,21.7985076662927));
#38162=CARTESIAN_POINT('Ctrl Pts',(130.619597226639,39.0395017103539,21.7927022449891));
#38163=CARTESIAN_POINT('Ctrl Pts',(130.737010799373,39.0179646690342,21.7868968236856));
#38164=CARTESIAN_POINT('Ctrl Pts',(130.854554396771,38.9964037774347,21.7810849734153));
#38165=CARTESIAN_POINT('Ctrl Pts',(130.971071625958,38.9696951875696,21.7752731231451));
#38166=CARTESIAN_POINT('Ctrl Pts',(131.086087894525,38.9379738553431,21.7694612728748));
#38167=CARTESIAN_POINT('Ctrl Pts',(131.201179706396,38.9062316883752,21.7636456053501));
#38168=CARTESIAN_POINT('Ctrl Pts',(131.31476820672,38.8694703475989,21.7578299378253));
#38169=CARTESIAN_POINT('Ctrl Pts',(131.426396743239,38.8278737349704,21.7520142703006));
#38170=CARTESIAN_POINT('Ctrl Pts',(131.538185175584,38.7862175396861,21.7461902724601));
#38171=CARTESIAN_POINT('Ctrl Pts',(131.648007665954,38.7397124072811,21.7403662746196));
#38172=CARTESIAN_POINT('Ctrl Pts',(131.755430072909,38.6885891963088,21.7345422767792));
#38173=CARTESIAN_POINT('Ctrl Pts',(131.783929823129,38.6750259297199,21.7329971384003));
#38174=CARTESIAN_POINT('Ctrl Pts',(131.812260788293,38.6611378525022,21.7314520000215));
#38175=CARTESIAN_POINT('Ctrl Pts',(131.840415198091,38.6469297907468,21.7299068616426));
#38176=CARTESIAN_POINT('Ctrl Pts',(131.946546836177,38.5933706900952,21.7240822654818));
#38177=CARTESIAN_POINT('Ctrl Pts',(132.050509721288,38.535088452653,21.7182576693209));
#38178=CARTESIAN_POINT('Ctrl Pts',(132.151855068785,38.4722823564543,21.71243307316));
#38179=CARTESIAN_POINT('Ctrl Pts',(132.253060538413,38.4095629458616,21.7066165161654));
#38180=CARTESIAN_POINT('Ctrl Pts',(132.351655314935,38.3423323141637,21.7007999591708));
#38181=CARTESIAN_POINT('Ctrl Pts',(132.447213477525,38.2708364672387,21.6949834021762));
#38182=CARTESIAN_POINT('Ctrl Pts',(132.460589047044,38.2608289739493,21.6941692408284));
#38183=CARTESIAN_POINT('Ctrl Pts',(132.473905160772,38.250737988423,21.6933550794807));
#38184=CARTESIAN_POINT('Ctrl Pts',(132.487160689988,38.2405642567579,21.6925409181329));
#38185=CARTESIAN_POINT('',(125.915000722565,34.9975703175708,22.2396150286373));
#38186=CARTESIAN_POINT('Ctrl Pts',(125.915000722565,34.9975703184334,22.2396150285955));
#38187=CARTESIAN_POINT('Ctrl Pts',(125.914929010373,35.1181393078882,22.233766442302));
#38188=CARTESIAN_POINT('Ctrl Pts',(125.920199535175,35.2387276668891,22.2279178560086));
#38189=CARTESIAN_POINT('Ctrl Pts',(125.930790852349,35.35883410188,22.2220692697151));
#38190=CARTESIAN_POINT('Ctrl Pts',(125.941383317302,35.4789535527799,22.2162200496116));
#38191=CARTESIAN_POINT('Ctrl Pts',(125.957297687507,35.598590577951,22.2103708295081));
#38192=CARTESIAN_POINT('Ctrl Pts',(125.978460616567,35.7172489020554,22.2045216094045));
#38193=CARTESIAN_POINT('Ctrl Pts',(125.999630529126,35.8359463819032,22.1986704591325));
#38194=CARTESIAN_POINT('Ctrl Pts',(126.026052377496,35.9536641249839,22.1928193088604));
#38195=CARTESIAN_POINT('Ctrl Pts',(126.057601774297,36.069916459344,22.1869681585884));
#38196=CARTESIAN_POINT('Ctrl Pts',(126.089190817938,36.1863148832701,22.1811096554145));
#38197=CARTESIAN_POINT('Ctrl Pts',(126.12592017732,36.3012438337314,22.1752511522406));
#38198=CARTESIAN_POINT('Ctrl Pts',(126.167615514836,36.4142327099436,22.1693926490667));
#38199=CARTESIAN_POINT('Ctrl Pts',(126.209337132695,36.5272928024257,22.1635304533103));
#38200=CARTESIAN_POINT('Ctrl Pts',(126.256030811639,36.6384100158507,22.157668257554));
#38201=CARTESIAN_POINT('Ctrl Pts',(126.307474687367,36.7471353169011,22.1518060617976));
#38202=CARTESIAN_POINT('Ctrl Pts',(126.359011363293,36.8560567487707,22.145933291159));
#38203=CARTESIAN_POINT('Ctrl Pts',(126.415315175186,36.9625772912076,22.1400605205204));
#38204=CARTESIAN_POINT('Ctrl Pts',(126.476118646655,37.0662732654585,22.1341877498818));
#38205=CARTESIAN_POINT('Ctrl Pts',(126.536050842732,37.1684833418082,22.128399132342));
#38206=CARTESIAN_POINT('Ctrl Pts',(126.600354320997,37.2679490084583,22.1226105148022));
#38207=CARTESIAN_POINT('Ctrl Pts',(126.668734188096,37.3642954744359,22.1168218972623));
#38208=CARTESIAN_POINT('Ctrl Pts',(126.73752722176,37.461224087471,22.110998303591));
#38209=CARTESIAN_POINT('Ctrl Pts',(126.81066514483,37.5553040447173,22.1051747099196));
#38210=CARTESIAN_POINT('Ctrl Pts',(126.887884046831,37.6461215569259,22.0993511162483));
#38211=CARTESIAN_POINT('Ctrl Pts',(126.965005525716,37.736824489353,22.0935348699054));
#38212=CARTESIAN_POINT('Ctrl Pts',(127.046197480592,37.8242728551419,22.0877186235625));
#38213=CARTESIAN_POINT('Ctrl Pts',(127.131153127974,37.9080822933454,22.0819023772196));
#38214=CARTESIAN_POINT('Ctrl Pts',(127.216023734286,37.9918078378393,22.0760919529713));
#38215=CARTESIAN_POINT('Ctrl Pts',(127.304650249154,38.0719014161008,22.0702815287231));
#38216=CARTESIAN_POINT('Ctrl Pts',(127.396686480553,38.1480126618971,22.0644711044748));
#38217=CARTESIAN_POINT('Ctrl Pts',(127.492206473676,38.2270048757737,22.0584407436506));
#38218=CARTESIAN_POINT('Ctrl Pts',(127.591399122868,38.3017069799212,22.0524103828264));
#38219=CARTESIAN_POINT('Ctrl Pts',(127.693836109116,38.3717700260225,22.0463800220022));
#38220=CARTESIAN_POINT('Ctrl Pts',(127.792425965794,38.4392017801822,22.0405761377691));
#38221=CARTESIAN_POINT('Ctrl Pts',(127.894020497764,38.502336390691,22.034772253536));
#38222=CARTESIAN_POINT('Ctrl Pts',(127.998205759725,38.5609050562464,22.0289683693028));
#38223=CARTESIAN_POINT('Ctrl Pts',(128.102375632408,38.6194650705837,22.0231653423655));
#38224=CARTESIAN_POINT('Ctrl Pts',(128.209135118203,38.6734602811682,22.0173623154281));
#38225=CARTESIAN_POINT('Ctrl Pts',(128.318044091939,38.722666963796,22.0115592884908));
#38226=CARTESIAN_POINT('Ctrl Pts',(128.426962681199,38.7718779908594,22.0057557492068));
#38227=CARTESIAN_POINT('Ctrl Pts',(128.538030763587,38.8162994812468,21.9999522099228));
#38228=CARTESIAN_POINT('Ctrl Pts',(128.650787176773,38.8557554068741,21.9941486706389));
#38229=CARTESIAN_POINT('Ctrl Pts',(128.763580155547,38.8952241275978,21.9883432493348));
#38230=CARTESIAN_POINT('Ctrl Pts',(128.878062168761,38.9297239462904,21.9825378280307));
#38231=CARTESIAN_POINT('Ctrl Pts',(128.993756423475,38.9591285486457,21.9767324067267));
#38232=CARTESIAN_POINT('Ctrl Pts',(129.109578798867,38.9885657138764,21.9709205564559));
#38233=CARTESIAN_POINT('Ctrl Pts',(129.226615699405,39.0128962992518,21.9651087061851));
#38234=CARTESIAN_POINT('Ctrl Pts',(129.344379500267,39.032044984909,21.9592968559143));
#38235=CARTESIAN_POINT('Ctrl Pts',(129.462220649026,39.0512062475257,21.953481188389));
#38236=CARTESIAN_POINT('Ctrl Pts',(129.580789244328,39.0651787845898,21.9476655208637));
#38237=CARTESIAN_POINT('Ctrl Pts',(129.699593548546,39.0739392440149,21.9418498533385));
#38238=CARTESIAN_POINT('Ctrl Pts',(129.818568027101,39.0827122518522,21.9360258554975));
#38239=CARTESIAN_POINT('Ctrl Pts',(129.937778481751,39.0862582687448,21.9302018576565));
#38240=CARTESIAN_POINT('Ctrl Pts',(130.056734045959,39.0846060089107,21.9243778598155));
#38241=CARTESIAN_POINT('Ctrl Pts',(130.088293605571,39.0841676553702,21.9228327214416));
#38242=CARTESIAN_POINT('Ctrl Pts',(130.119835259209,39.08336369314,21.9212875830677));
#38243=CARTESIAN_POINT('Ctrl Pts',(130.151349931726,39.0821952670305,21.9197424446939));
#38244=CARTESIAN_POINT('Ctrl Pts',(130.27011093384,39.0777921289183,21.9139196908137));
#38245=CARTESIAN_POINT('Ctrl Pts',(130.388871112726,39.0681950208969,21.9080969369335));
#38246=CARTESIAN_POINT('Ctrl Pts',(130.507139933391,39.0533978447668,21.9022741830533));
#38247=CARTESIAN_POINT('Ctrl Pts',(130.62526825698,39.0386182468959,21.8964583462954));
#38248=CARTESIAN_POINT('Ctrl Pts',(130.742905981608,39.0186509139388,21.8906425095375));
#38249=CARTESIAN_POINT('Ctrl Pts',(130.859563574334,38.9935417190357,21.8848266727795));
#38250=CARTESIAN_POINT('Ctrl Pts',(130.976110128426,38.9684564239118,21.8790163717313));
#38251=CARTESIAN_POINT('Ctrl Pts',(131.09167800926,38.9382390860377,21.8732060706831));
#38252=CARTESIAN_POINT('Ctrl Pts',(131.205784439578,38.9029871746231,21.8673957696348));
#38253=CARTESIAN_POINT('Ctrl Pts',(131.321068741101,38.8673713730115,21.8615254913681));
#38254=CARTESIAN_POINT('Ctrl Pts',(131.434860828287,38.8266165141782,21.8556552131014));
#38255=CARTESIAN_POINT('Ctrl Pts',(131.546674680978,38.7808758814883,21.8497849348347));
#38256=CARTESIAN_POINT('Ctrl Pts',(131.657218090426,38.7356549596963,21.8439813554178));
#38257=CARTESIAN_POINT('Ctrl Pts',(131.765827603802,38.6855611445331,21.8381777760008));
#38258=CARTESIAN_POINT('Ctrl Pts',(131.872050999628,38.6307919321813,21.8323741965839));
#38259=CARTESIAN_POINT('Ctrl Pts',(131.98010558733,38.5750785498944,21.8264705688923));
#38260=CARTESIAN_POINT('Ctrl Pts',(132.085690620244,38.5145272308984,21.8205669412007));
#38261=CARTESIAN_POINT('Ctrl Pts',(132.188354536684,38.4493955154161,21.8146633135091));
#38262=CARTESIAN_POINT('Ctrl Pts',(132.291018453125,38.3842637999337,21.8087596858175));
#38263=CARTESIAN_POINT('Ctrl Pts',(132.390760881023,38.3145519318612,21.8028560581259));
#38264=CARTESIAN_POINT('Ctrl Pts',(132.487160689988,38.2405642567579,21.7969524304342));
#38265=CARTESIAN_POINT('Ctrl Pts',(132.487160689988,38.2405642567579,23.046779218902));
#38266=CARTESIAN_POINT('Ctrl Pts',(132.583414831562,38.1666883826194,23.0408775725951));
#38267=CARTESIAN_POINT('Ctrl Pts',(132.67644286449,38.0884679419452,23.0349759262882));
#38268=CARTESIAN_POINT('Ctrl Pts',(132.765836782572,38.006222196075,23.0290742799813));
#38269=CARTESIAN_POINT('Ctrl Pts',(132.853746494384,37.9253419754465,23.0232706186451));
#38270=CARTESIAN_POINT('Ctrl Pts',(132.938141535144,37.8405693820216,23.0174669573089));
#38271=CARTESIAN_POINT('Ctrl Pts',(133.018667715259,37.752248212799,23.0116632959726));
#38272=CARTESIAN_POINT('Ctrl Pts',(133.099184950673,37.6639368541298,23.0058602792965));
#38273=CARTESIAN_POINT('Ctrl Pts',(133.175833905052,37.5720780052852,23.0000572626203));
#38274=CARTESIAN_POINT('Ctrl Pts',(133.24829854086,37.4770509864441,22.9942542459441));
#38275=CARTESIAN_POINT('Ctrl Pts',(133.320772229082,37.3820120966564,22.9884505043446));
#38276=CARTESIAN_POINT('Ctrl Pts',(133.389060311758,37.2838045746224,22.9826467627452));
#38277=CARTESIAN_POINT('Ctrl Pts',(133.452888595304,37.1828388278622,22.9768430211457));
#38278=CARTESIAN_POINT('Ctrl Pts',(133.518603378227,37.0788889523138,22.9708677450115));
#38279=CARTESIAN_POINT('Ctrl Pts',(133.579590382795,36.9720156591103,22.9648924688774));
#38280=CARTESIAN_POINT('Ctrl Pts',(133.635600513666,36.8626953333903,22.9589171927433));
#38281=CARTESIAN_POINT('Ctrl Pts',(133.690084473718,36.7563537811241,22.9531047316557));
#38282=CARTESIAN_POINT('Ctrl Pts',(133.739859158313,36.6476972275852,22.9472922705682));
#38283=CARTESIAN_POINT('Ctrl Pts',(133.784744135206,36.5371847094689,22.9414798094807));
#38284=CARTESIAN_POINT('Ctrl Pts',(133.831515047203,36.4220287794182,22.9354231258233));
#38285=CARTESIAN_POINT('Ctrl Pts',(133.872976214816,36.3048579910485,22.9293664421658));
#38286=CARTESIAN_POINT('Ctrl Pts',(133.908981333389,36.1862082174812,22.9233097585084));
#38287=CARTESIAN_POINT('Ctrl Pts',(133.944986451961,36.0675584439138,22.917253074851));
#38288=CARTESIAN_POINT('Ctrl Pts',(133.975535466143,35.9474301811147,22.9111963911935));
#38289=CARTESIAN_POINT('Ctrl Pts',(134.00054240192,35.8263688585874,22.9051397075361));
#38290=CARTESIAN_POINT('Ctrl Pts',(134.024586951902,35.7099665513837,22.8993161138646));
#38291=CARTESIAN_POINT('Ctrl Pts',(134.043585686199,35.5923262426363,22.8934925201932));
#38292=CARTESIAN_POINT('Ctrl Pts',(134.057415670364,35.4739230716969,22.8876689265217));
#38293=CARTESIAN_POINT('Ctrl Pts',(134.071228205949,35.355669283945,22.8818526801787));
#38294=CARTESIAN_POINT('Ctrl Pts',(134.079884914853,35.236654950324,22.8760364338357));
#38295=CARTESIAN_POINT('Ctrl Pts',(134.083313617438,35.1173665269401,22.8702201874926));
#38296=CARTESIAN_POINT('Ctrl Pts',(134.086738887873,34.9981975119262,22.8644097632443));
#38297=CARTESIAN_POINT('Ctrl Pts',(134.084946551254,34.8787553587877,22.8585993389959));
#38298=CARTESIAN_POINT('Ctrl Pts',(134.077916163162,34.7595321929578,22.8527889147476));
#38299=CARTESIAN_POINT('Ctrl Pts',(134.070619660339,34.6357961837054,22.8467585539234));
#38300=CARTESIAN_POINT('Ctrl Pts',(134.05768067683,34.5122965127613,22.8407281930993));
#38301=CARTESIAN_POINT('Ctrl Pts',(134.039135779025,34.3895844377817,22.8346978322751));
#38302=CARTESIAN_POINT('Ctrl Pts',(134.021287354509,34.2714809448121,22.8288939480419));
#38303=CARTESIAN_POINT('Ctrl Pts',(133.998246560816,34.1541073966982,22.8230900638086));
#38304=CARTESIAN_POINT('Ctrl Pts',(133.970098817708,34.0379499089793,22.8172861795754));
#38305=CARTESIAN_POINT('Ctrl Pts',(133.941955232323,33.9218095789634,22.8114831526379));
#38306=CARTESIAN_POINT('Ctrl Pts',(133.908706293831,33.806885348869,22.8056801257005));
#38307=CARTESIAN_POINT('Ctrl Pts',(133.870488251105,33.6936517699877,22.799877098763));
#38308=CARTESIAN_POINT('Ctrl Pts',(133.832266834126,33.5804081937656,22.7940735594789));
#38309=CARTESIAN_POINT('Ctrl Pts',(133.789075571222,33.4688559524485,22.7882700201949));
#38310=CARTESIAN_POINT('Ctrl Pts',(133.741099951931,33.3594524847903,22.7824664809108));
#38311=CARTESIAN_POINT('Ctrl Pts',(133.693108774706,33.2500135388629,22.7766610596066));
#38312=CARTESIAN_POINT('Ctrl Pts',(133.640330319395,33.1427251261848,22.7708556383024));
#38313=CARTESIAN_POINT('Ctrl Pts',(133.582997107868,33.0380222414584,22.7650502169982));
#38314=CARTESIAN_POINT('Ctrl Pts',(133.525600405115,32.9332034079791,22.7592383667273));
#38315=CARTESIAN_POINT('Ctrl Pts',(133.463639074184,32.8309761760786,22.7534265164563));
#38316=CARTESIAN_POINT('Ctrl Pts',(133.397390335891,32.7317487119825,22.7476146661854));
#38317=CARTESIAN_POINT('Ctrl Pts',(133.331098085071,32.6324560747552,22.74179899866));
#38318=CARTESIAN_POINT('Ctrl Pts',(133.26051305963,32.5361674577333,22.7359833311347));
#38319=CARTESIAN_POINT('Ctrl Pts',(133.185953312242,32.4432586184335,22.7301676636093));
#38320=CARTESIAN_POINT('Ctrl Pts',(133.111286766067,32.3502166972537,22.7243436657682));
#38321=CARTESIAN_POINT('Ctrl Pts',(133.032634402644,32.2605645223657,22.718519667927));
#38322=CARTESIAN_POINT('Ctrl Pts',(132.950351781855,32.1746417283278,22.7126956700859));
#38323=CARTESIAN_POINT('Ctrl Pts',(132.928521754052,32.1518459427206,22.7111505317131));
#38324=CARTESIAN_POINT('Ctrl Pts',(132.906436386135,32.1293124389526,22.7096053933404));
#38325=CARTESIAN_POINT('Ctrl Pts',(132.884102700967,32.1070470777639,22.7080602549676));
#38326=CARTESIAN_POINT('Ctrl Pts',(132.799927516468,32.0231294048895,22.7022366612962));
#38327=CARTESIAN_POINT('Ctrl Pts',(132.711950970825,31.9427532793061,22.6964130676247));
#38328=CARTESIAN_POINT('Ctrl Pts',(132.620503068697,31.8662819739243,22.6905894739533));
#38329=CARTESIAN_POINT('Ctrl Pts',(132.52917054168,31.7899071484529,22.6847732276102));
#38330=CARTESIAN_POINT('Ctrl Pts',(132.434375679649,31.7174276041057,22.6789569812672));
#38331=CARTESIAN_POINT('Ctrl Pts',(132.336485774206,31.649170367367,22.6731407349242));
#38332=CARTESIAN_POINT('Ctrl Pts',(132.238693857099,31.5809814564991,22.6673303106759));
#38333=CARTESIAN_POINT('Ctrl Pts',(132.137813393001,31.5170066772483,22.6615198864275));
#38334=CARTESIAN_POINT('Ctrl Pts',(132.034244774538,31.4575328939755,22.6557094621792));
#38335=CARTESIAN_POINT('Ctrl Pts',(131.926755869649,31.3958079049927,22.649679101355));
#38336=CARTESIAN_POINT('Ctrl Pts',(131.816371628907,31.3389316760974,22.6436487405309));
#38337=CARTESIAN_POINT('Ctrl Pts',(131.703573152673,31.2871758035839,22.6376183797067));
#38338=CARTESIAN_POINT('Ctrl Pts',(131.595010942742,31.2373636777067,22.6318144954735));
#38339=CARTESIAN_POINT('Ctrl Pts',(131.484212969967,31.1922944287699,22.6260106112402));
#38340=CARTESIAN_POINT('Ctrl Pts',(131.37163263136,31.1521630849803,22.620206727007));
#38341=CARTESIAN_POINT('Ctrl Pts',(131.259068922073,31.1120376690194,22.6144037000696));
#38342=CARTESIAN_POINT('Ctrl Pts',(131.144723755051,31.0768488447679,22.6086006731321));
#38343=CARTESIAN_POINT('Ctrl Pts',(131.02906871797,31.0467427893324,22.6027976461946));
#38344=CARTESIAN_POINT('Ctrl Pts',(130.913403469759,31.0166340758469,22.5969941069106));
#38345=CARTESIAN_POINT('Ctrl Pts',(130.796428516742,30.9916091262824,22.5911905676265));
#38346=CARTESIAN_POINT('Ctrl Pts',(130.678628126101,30.9717635538037,22.5853870283424));
#38347=CARTESIAN_POINT('Ctrl Pts',(130.560789534168,30.9519115456373,22.5795816070382));
#38348=CARTESIAN_POINT('Ctrl Pts',(130.442125374713,30.9372423227259,22.573776185734));
#38349=CARTESIAN_POINT('Ctrl Pts',(130.323126924773,30.927799858739,22.5679707644298));
#38350=CARTESIAN_POINT('Ctrl Pts',(130.203996695066,30.9183469380971,22.5621589141589));
#38351=CARTESIAN_POINT('Ctrl Pts',(130.084531843231,30.914132362345,22.556347063888));
#38352=CARTESIAN_POINT('Ctrl Pts',(129.965225710076,30.9151480138492,22.5505352136171));
#38353=CARTESIAN_POINT('Ctrl Pts',(129.845841216012,30.9161643324387,22.5447195460917));
#38354=CARTESIAN_POINT('Ctrl Pts',(129.726616055079,30.9224176983156,22.5389038785664));
#38355=CARTESIAN_POINT('Ctrl Pts',(129.608038844912,30.9338480779855,22.533088211041));
#38356=CARTESIAN_POINT('Ctrl Pts',(129.489291785694,30.9452948304402,22.5272642131999));
#38357=CARTESIAN_POINT('Ctrl Pts',(129.371194932627,30.9619333408839,22.5214402153588));
#38358=CARTESIAN_POINT('Ctrl Pts',(129.254227251232,30.9836524045852,22.5156162175177));
#38359=CARTESIAN_POINT('Ctrl Pts',(129.223195087787,30.9894145905719,22.5140710791449));
#38360=CARTESIAN_POINT('Ctrl Pts',(129.192242321155,30.9955341090142,22.512525940772));
#38361=CARTESIAN_POINT('Ctrl Pts',(129.161377702766,31.0020082988353,22.5109808023992));
#38362=CARTESIAN_POINT('Ctrl Pts',(129.04504961236,31.0264093826046,22.5051572087277));
#38363=CARTESIAN_POINT('Ctrl Pts',(128.929599802198,31.0559311623785,22.4993336150561));
#38364=CARTESIAN_POINT('Ctrl Pts',(128.815512999794,31.0904967647611,22.4935100213846));
#38365=CARTESIAN_POINT('Ctrl Pts',(128.701570134838,31.125018757502,22.4876937750415));
#38366=CARTESIAN_POINT('Ctrl Pts',(128.588987244671,31.1645717985791,22.4818775286984));
#38367=CARTESIAN_POINT('Ctrl Pts',(128.47823918069,31.2090279599011,22.4760612823553));
#38368=CARTESIAN_POINT('Ctrl Pts',(128.367601976132,31.25343962036,22.4702508581069));
#38369=CARTESIAN_POINT('Ctrl Pts',(128.258796320696,31.3027444858643,22.4644404338585));
#38370=CARTESIAN_POINT('Ctrl Pts',(128.152281620112,31.3567649281685,22.4586300096101));
#38371=CARTESIAN_POINT('Ctrl Pts',(128.041735117801,31.4128301559468,22.452599648786));
#38372=CARTESIAN_POINT('Ctrl Pts',(127.933656860862,31.4739748727617,22.4465692879619));
#38373=CARTESIAN_POINT('Ctrl Pts',(127.828537726293,31.5399455793491,22.4405389271377));
#38374=CARTESIAN_POINT('Ctrl Pts',(127.727366452212,31.6034386861449,22.4347350429044));
#38375=CARTESIAN_POINT('Ctrl Pts',(127.628936419793,31.6714015928606,22.4289311586711));
#38376=CARTESIAN_POINT('Ctrl Pts',(127.533659280729,31.7435619986761,22.4231272744378));
#38377=CARTESIAN_POINT('Ctrl Pts',(127.438396215118,31.815711745628,22.4173242475002));
#38378=CARTESIAN_POINT('Ctrl Pts',(127.346285442125,31.8920575121955,22.4115212205627));
#38379=CARTESIAN_POINT('Ctrl Pts',(127.257707727254,31.9722850050182,22.4057181936251));
#38380=CARTESIAN_POINT('Ctrl Pts',(127.169122191897,32.0525195810893,22.399914654341));
#38381=CARTESIAN_POINT('Ctrl Pts',(127.084070637523,32.1366362906841,22.3941111150568));
#38382=CARTESIAN_POINT('Ctrl Pts',(127.002898489856,32.2242825183578,22.3883075757727));
#38383=CARTESIAN_POINT('Ctrl Pts',(126.921700019009,32.311957168681,22.3825021544684));
#38384=CARTESIAN_POINT('Ctrl Pts',(126.844383734156,32.403163313961,22.3766967331642));
#38385=CARTESIAN_POINT('Ctrl Pts',(126.771255713786,32.4975141690231,22.37089131186));
#38386=CARTESIAN_POINT('Ctrl Pts',(126.698046710902,32.5919695089241,22.365079461589));
#38387=CARTESIAN_POINT('Ctrl Pts',(126.629035480871,32.6895761869886,22.359267611318));
#38388=CARTESIAN_POINT('Ctrl Pts',(126.564485665802,32.7899171374091,22.353455761047));
#38389=CARTESIAN_POINT('Ctrl Pts',(126.499893454068,32.890323992304,22.3476400935216));
#38390=CARTESIAN_POINT('Ctrl Pts',(126.439768698191,32.9934683441391,22.3418244259961));
#38391=CARTESIAN_POINT('Ctrl Pts',(126.384329030281,33.098908619048,22.3360087584707));
#38392=CARTESIAN_POINT('Ctrl Pts',(126.328809951032,33.2044999257654,22.3301847606295));
#38393=CARTESIAN_POINT('Ctrl Pts',(126.27798952769,33.3123933514493,22.3243607627883));
#38394=CARTESIAN_POINT('Ctrl Pts',(126.232037303278,33.4221273447744,22.3185367649471));
#38395=CARTESIAN_POINT('Ctrl Pts',(126.219845927669,33.4512403713306,22.316991626575));
#38396=CARTESIAN_POINT('Ctrl Pts',(126.207996937056,33.4804828693213,22.3154464882029));
#38397=CARTESIAN_POINT('Ctrl Pts',(126.196492903007,33.5098460605958,22.3139013498308));
#38398=CARTESIAN_POINT('Ctrl Pts',(126.147593400052,33.6346584048845,22.3073335234432));
#38399=CARTESIAN_POINT('Ctrl Pts',(126.104798671119,33.7619885269551,22.3007656970556));
#38400=CARTESIAN_POINT('Ctrl Pts',(126.06834304772,33.8912626056695,22.294197870668));
#38401=CARTESIAN_POINT('Ctrl Pts',(126.032001969344,34.0201305000708,22.287650680653));
#38402=CARTESIAN_POINT('Ctrl Pts',(126.001960341605,34.1509299687405,22.281103490638));
#38403=CARTESIAN_POINT('Ctrl Pts',(125.978403669591,34.2830704670304,22.274556300623));
#38404=CARTESIAN_POINT('Ctrl Pts',(125.95498504246,34.414436606382,22.2680474779153));
#38405=CARTESIAN_POINT('Ctrl Pts',(125.937975683312,34.5471279041211,22.2615386552076));
#38406=CARTESIAN_POINT('Ctrl Pts',(125.927510148758,34.6805451338116,22.2550298324999));
#38407=CARTESIAN_POINT('Ctrl Pts',(125.919248328881,34.7858688623325,22.2498915645457));
#38408=CARTESIAN_POINT('Ctrl Pts',(125.915063725241,34.8916445871987,22.2447532965915));
#38409=CARTESIAN_POINT('Ctrl Pts',(125.915000722565,34.9975703175707,22.2396150286373));
#38410=CARTESIAN_POINT('Origin',(130.,35.,32.7603849714045));
#38411=CARTESIAN_POINT('',(132.487160689988,38.2405642567579,24.2969444281512));
#38412=CARTESIAN_POINT('',(132.487160689988,38.2405642567579,24.1926561440539));
#38413=CARTESIAN_POINT('',(132.487160689988,38.2405642567579,32.7603849714045));
#38414=CARTESIAN_POINT('',(125.915000507333,35.0020359057478,23.3853849713659));
#38415=CARTESIAN_POINT('Ctrl Pts',(132.487160689988,38.2405642567579,24.1926561440539));
#38416=CARTESIAN_POINT('Ctrl Pts',(132.581972335864,38.1677955103636,24.1868529351341));
#38417=CARTESIAN_POINT('Ctrl Pts',(132.673586459642,38.0908633554204,24.1810497262143));
#38418=CARTESIAN_POINT('Ctrl Pts',(132.761628091852,38.0100889160108,24.1752465172945));
#38419=CARTESIAN_POINT('Ctrl Pts',(132.849691138964,37.9292948293431,24.1694418968249));
#38420=CARTESIAN_POINT('Ctrl Pts',(132.934179665622,37.844656875635,24.1636372763553));
#38421=CARTESIAN_POINT('Ctrl Pts',(133.014754852225,37.7565337257115,24.1578326558858));
#38422=CARTESIAN_POINT('Ctrl Pts',(133.095416153948,37.668316393746,24.1520218317));
#38423=CARTESIAN_POINT('Ctrl Pts',(133.172155488284,37.5766067295761,24.1462110075143));
#38424=CARTESIAN_POINT('Ctrl Pts',(133.244673577683,37.4817974079864,24.1404001833285));
#38425=CARTESIAN_POINT('Ctrl Pts',(133.317234025714,37.3869327072038,24.1345859649749));
#38426=CARTESIAN_POINT('Ctrl Pts',(133.385568083947,37.28896507707,24.1287717466213));
#38427=CARTESIAN_POINT('Ctrl Pts',(133.449420133897,37.1883157313022,24.1229575282677));
#38428=CARTESIAN_POINT('Ctrl Pts',(133.513369630861,37.0875127807842,24.1171344366169));
#38429=CARTESIAN_POINT('Ctrl Pts',(133.572823255309,36.984020294514,24.1113113449661));
#38430=CARTESIAN_POINT('Ctrl Pts',(133.627571432369,36.8782839250383,24.1054882533153));
#38431=CARTESIAN_POINT('Ctrl Pts',(133.660879138846,36.8139560122651,24.1019455996981));
#38432=CARTESIAN_POINT('Ctrl Pts',(133.692446166234,36.7487979930244,24.098402946081));
#38433=CARTESIAN_POINT('Ctrl Pts',(133.722234217902,36.6829133747994,24.0948602924639));
#38434=CARTESIAN_POINT('Ctrl Pts',(133.771201327851,36.5746088982088,24.0890366987924));
#38435=CARTESIAN_POINT('Ctrl Pts',(133.81551653434,36.4639908317772,24.0832131051209));
#38436=CARTESIAN_POINT('Ctrl Pts',(133.854955774648,36.3514958288903,24.0773895114494));
#38437=CARTESIAN_POINT('Ctrl Pts',(133.894345256496,36.2391427551591,24.0715732651064));
#38438=CARTESIAN_POINT('Ctrl Pts',(133.928870873956,36.1249178368819,24.0657570187633));
#38439=CARTESIAN_POINT('Ctrl Pts',(133.958355605775,36.0092798909276,24.0599407724203));
#38440=CARTESIAN_POINT('Ctrl Pts',(133.987810823214,35.8937576991956,24.0541303481719));
#38441=CARTESIAN_POINT('Ctrl Pts',(134.012235093006,35.7768256870598,24.0483199239236));
#38442=CARTESIAN_POINT('Ctrl Pts',(134.03150062945,35.6589595395331,24.0425094996752));
#38443=CARTESIAN_POINT('Ctrl Pts',(134.051495406297,35.5366319145338,24.0364791388511));
#38444=CARTESIAN_POINT('Ctrl Pts',(134.065933047646,35.4132984619357,24.0304487780269));
#38445=CARTESIAN_POINT('Ctrl Pts',(134.074728435545,35.2895050544698,24.0244184172028));
#38446=CARTESIAN_POINT('Ctrl Pts',(134.08319350333,35.1703608396006,24.0186145329695));
#38447=CARTESIAN_POINT('Ctrl Pts',(134.086432445026,35.05079103895,24.0128106487363));
#38448=CARTESIAN_POINT('Ctrl Pts',(134.084422083151,34.9312886714402,24.007006764503));
#38449=CARTESIAN_POINT('Ctrl Pts',(134.082412018227,34.8118039557081,24.0012037375655));
#38450=CARTESIAN_POINT('Ctrl Pts',(134.075154198583,34.6923870614772,23.995400710628));
#38451=CARTESIAN_POINT('Ctrl Pts',(134.062677574554,34.5735308625269,23.9895976836906));
#38452=CARTESIAN_POINT('Ctrl Pts',(134.050199848969,34.4546641698173,23.9837941444065));
#38453=CARTESIAN_POINT('Ctrl Pts',(134.032502445518,34.3363586769388,23.9779906051224));
#38454=CARTESIAN_POINT('Ctrl Pts',(134.009666108294,34.2191013510092,23.9721870658384));
#38455=CARTESIAN_POINT('Ctrl Pts',(133.986822365513,34.1018059998969,23.9663816445342));
#38456=CARTESIAN_POINT('Ctrl Pts',(133.958836452693,33.9855598923348,23.9605762232301));
#38457=CARTESIAN_POINT('Ctrl Pts',(133.925839921305,33.870838402935,23.9547708019259));
#38458=CARTESIAN_POINT('Ctrl Pts',(133.892806849312,33.7559898701031,23.948958951655));
#38459=CARTESIAN_POINT('Ctrl Pts',(133.854752195816,33.6426697182315,23.943147101384));
#38460=CARTESIAN_POINT('Ctrl Pts',(133.811857003736,33.5313369402508,23.9373352511131));
#38461=CARTESIAN_POINT('Ctrl Pts',(133.768933637862,33.4199310383039,23.9315195835877));
#38462=CARTESIAN_POINT('Ctrl Pts',(133.721163564774,33.3105154831865,23.9257039160623));
#38463=CARTESIAN_POINT('Ctrl Pts',(133.668774768513,33.2035265941507,23.9198882485369));
#38464=CARTESIAN_POINT('Ctrl Pts',(133.616310930958,33.0963844550843,23.9140642506958));
#38465=CARTESIAN_POINT('Ctrl Pts',(133.559215360203,32.9916762771116,23.9082402528546));
#38466=CARTESIAN_POINT('Ctrl Pts',(133.497760551462,32.8898113533061,23.9024162550135));
#38467=CARTESIAN_POINT('Ctrl Pts',(133.481456255726,32.8627860337759,23.9008711166408));
#38468=CARTESIAN_POINT('Ctrl Pts',(133.464845352462,32.8359606696453,23.8993259782681));
#38469=CARTESIAN_POINT('Ctrl Pts',(133.447933409606,32.8093425181181,23.8977808398955));
#38470=CARTESIAN_POINT('Ctrl Pts',(133.384192656586,32.7090192710078,23.891957246224));
#38471=CARTESIAN_POINT('Ctrl Pts',(133.315966879742,32.6113185160414,23.8861336525526));
#38472=CARTESIAN_POINT('Ctrl Pts',(133.243498460342,32.5166670102944,23.8803100588811));
#38473=CARTESIAN_POINT('Ctrl Pts',(133.171121470617,32.4221349214812,23.8744938125381));
#38474=CARTESIAN_POINT('Ctrl Pts',(133.094512730826,32.3306447514966,23.8686775661951));
#38475=CARTESIAN_POINT('Ctrl Pts',(133.013958945554,32.2425960625046,23.862861319852));
#38476=CARTESIAN_POINT('Ctrl Pts',(132.933485795066,32.1546355107361,23.8570508956037));
#38477=CARTESIAN_POINT('Ctrl Pts',(132.849075729215,32.0701098862198,23.8512404713554));
#38478=CARTESIAN_POINT('Ctrl Pts',(132.761056549753,31.989386818426,23.845430047107));
#38479=CARTESIAN_POINT('Ctrl Pts',(132.669705662293,31.9056082155521,23.8393996862829));
#38480=CARTESIAN_POINT('Ctrl Pts',(132.574467310382,31.8259260824054,23.8333693254587));
#38481=CARTESIAN_POINT('Ctrl Pts',(132.475751387658,31.7507108367356,23.8273389646345));
#38482=CARTESIAN_POINT('Ctrl Pts',(132.380742846018,31.6783203793199,23.8215350804013));
#38483=CARTESIAN_POINT('Ctrl Pts',(132.28251358474,31.6100676123452,23.815731196168));
#38484=CARTESIAN_POINT('Ctrl Pts',(132.181463245575,31.5462421758025,23.8099273119348));
#38485=CARTESIAN_POINT('Ctrl Pts',(132.080427832626,31.4824261669595,23.8041242849973));
#38486=CARTESIAN_POINT('Ctrl Pts',(131.976572515625,31.4230364060209,23.7983212580598));
#38487=CARTESIAN_POINT('Ctrl Pts',(131.8703253895,31.3683188552144,23.7925182311224));
#38488=CARTESIAN_POINT('Ctrl Pts',(131.764068882865,31.3135964734205,23.7867146918383));
#38489=CARTESIAN_POINT('Ctrl Pts',(131.655420510287,31.26354730889,23.7809111525542));
#38490=CARTESIAN_POINT('Ctrl Pts',(131.544831817983,31.2183707672292,23.7751076132702));
#38491=CARTESIAN_POINT('Ctrl Pts',(131.434207263056,31.1731795753427,23.769302191966));
#38492=CARTESIAN_POINT('Ctrl Pts',(131.321641514838,31.1328643031993,23.7634967706618));
#38493=CARTESIAN_POINT('Ctrl Pts',(131.207604274663,31.097575507993,23.7576913493577));
#38494=CARTESIAN_POINT('Ctrl Pts',(131.093440748799,31.0622476337123,23.7518794990868));
#38495=CARTESIAN_POINT('Ctrl Pts',(130.977802868592,31.0319574680796,23.7460676488158));
#38496=CARTESIAN_POINT('Ctrl Pts',(130.861173763619,31.0068051952284,23.7402557985449));
#38497=CARTESIAN_POINT('Ctrl Pts',(130.744468056023,30.9816364022294,23.7344401310195));
#38498=CARTESIAN_POINT('Ctrl Pts',(130.626770228722,30.9616122909336,23.7286244634941));
#38499=CARTESIAN_POINT('Ctrl Pts',(130.508570179098,30.9467813563869,23.7228087959687));
#38500=CARTESIAN_POINT('Ctrl Pts',(130.390200820666,30.931929178128,23.7169847981276));
#38501=CARTESIAN_POINT('Ctrl Pts',(130.271328209624,30.9222850566915,23.7111608002865));
#38502=CARTESIAN_POINT('Ctrl Pts',(130.152444038842,30.917845444496,23.7053368024453));
#38503=CARTESIAN_POINT('Ctrl Pts',(130.120903420317,30.9166675911811,23.7037916640726));
#38504=CARTESIAN_POINT('Ctrl Pts',(130.089361967641,30.9158557838219,23.7022465256998));
#38505=CARTESIAN_POINT('Ctrl Pts',(130.057828802667,30.915409343694,23.700701387327));
#38506=CARTESIAN_POINT('Ctrl Pts',(129.938980974396,30.9137267203452,23.6948777936555));
#38507=CARTESIAN_POINT('Ctrl Pts',(129.81986799618,30.9172327961846,23.6890541999841));
#38508=CARTESIAN_POINT('Ctrl Pts',(129.700979659909,30.9259587831967,23.6832306063126));
#38509=CARTESIAN_POINT('Ctrl Pts',(129.582241318934,30.93467376108,23.6774143599696));
#38510=CARTESIAN_POINT('Ctrl Pts',(129.463727459842,30.94859552172,23.6715981136265));
#38511=CARTESIAN_POINT('Ctrl Pts',(129.345929425908,30.9677032990977,23.6657818672835));
#38512=CARTESIAN_POINT('Ctrl Pts',(129.228249308457,30.9867919494848,23.6599714430351));
#38513=CARTESIAN_POINT('Ctrl Pts',(129.111283991439,31.0110562242926,23.6541610187868));
#38514=CARTESIAN_POINT('Ctrl Pts',(128.995520638518,31.0404234806793,23.6483505945384));
#38515=CARTESIAN_POINT('Ctrl Pts',(128.875375403249,31.070902348462,23.6423202337143));
#38516=CARTESIAN_POINT('Ctrl Pts',(128.75652537064,31.1068781148392,23.6362898728901));
#38517=CARTESIAN_POINT('Ctrl Pts',(128.639505036172,31.1482110061169,23.6302595120659));
#38518=CARTESIAN_POINT('Ctrl Pts',(128.526879524368,31.1879915968636,23.6244556278327));
#38519=CARTESIAN_POINT('Ctrl Pts',(128.415949176261,31.2327340357753,23.6186517435995));
#38520=CARTESIAN_POINT('Ctrl Pts',(128.307175307434,31.2822628441164,23.6128478593662));
#38521=CARTESIAN_POINT('Ctrl Pts',(128.19841750567,31.3317843365228,23.6070448324287));
#38522=CARTESIAN_POINT('Ctrl Pts',(128.091815921246,31.3860906231938,23.6012418054913));
#38523=CARTESIAN_POINT('Ctrl Pts',(127.987810935919,31.4449584854194,23.5954387785538));
#38524=CARTESIAN_POINT('Ctrl Pts',(127.883796768038,31.5038315450616,23.5896352392697));
#38525=CARTESIAN_POINT('Ctrl Pts',(127.782380010443,31.5672667798531,23.5838316999857));
#38526=CARTESIAN_POINT('Ctrl Pts',(127.683974961419,31.6349958364567,23.5780281607016));
#38527=CARTESIAN_POINT('Ctrl Pts',(127.585538000784,31.7027468568034,23.5722227393974));
#38528=CARTESIAN_POINT('Ctrl Pts',(127.490115027274,31.7747942368127,23.5664173180933));
#38529=CARTESIAN_POINT('Ctrl Pts',(127.398089435742,31.8508276618127,23.5606118967891));
#38530=CARTESIAN_POINT('Ctrl Pts',(127.305961934386,31.9269452867933,23.5548000465182));
#38531=CARTESIAN_POINT('Ctrl Pts',(127.217239639832,32.0070575075962,23.5489881962472));
#38532=CARTESIAN_POINT('Ctrl Pts',(127.132271177237,32.0908151658766,23.5431763459763));
#38533=CARTESIAN_POINT('Ctrl Pts',(127.047246906899,32.1746278366364,23.5373606784509));
#38534=CARTESIAN_POINT('Ctrl Pts',(126.965981656005,32.2620904148143,23.5315450109256));
#38535=CARTESIAN_POINT('Ctrl Pts',(126.888784528312,32.3528197475937,23.5257293434002));
#38536=CARTESIAN_POINT('Ctrl Pts',(126.81147682407,32.4436790403455,23.5199053455591));
#38537=CARTESIAN_POINT('Ctrl Pts',(126.738249123527,32.5378141061151,23.5140813477179));
#38538=CARTESIAN_POINT('Ctrl Pts',(126.669367987711,32.6348117625195,23.5082573498768));
#38539=CARTESIAN_POINT('Ctrl Pts',(126.651093446921,32.660545769479,23.506712211504));
#38540=CARTESIAN_POINT('Ctrl Pts',(126.633124599155,32.6864811271597,23.5051670731313));
#38541=CARTESIAN_POINT('Ctrl Pts',(126.615465877015,32.7126098342537,23.5036219347586));
#38542=CARTESIAN_POINT('Ctrl Pts',(126.547946051236,32.8125154637126,23.4977139492936));
#38543=CARTESIAN_POINT('Ctrl Pts',(126.484750138236,32.915565828757,23.4918059638287));
#38544=CARTESIAN_POINT('Ctrl Pts',(126.426178854133,33.0213571779229,23.4858979783637));
#38545=CARTESIAN_POINT('Ctrl Pts',(126.367686936568,33.1270051753913,23.4799979984658));
#38546=CARTESIAN_POINT('Ctrl Pts',(126.313807367996,33.2353864267341,23.474098018568));
#38547=CARTESIAN_POINT('Ctrl Pts',(126.264798248165,33.346067452075,23.4681980386701));
#38548=CARTESIAN_POINT('Ctrl Pts',(126.215845205529,33.4566218340164,23.462304809645));
#38549=CARTESIAN_POINT('Ctrl Pts',(126.171751679285,33.5694703964249,23.4564115806198));
#38550=CARTESIAN_POINT('Ctrl Pts',(126.132730167001,33.6841546296112,23.4505183515946));
#38551=CARTESIAN_POINT('Ctrl Pts',(126.093751609523,33.7987126186111,23.4446316098248));
#38552=CARTESIAN_POINT('Ctrl Pts',(126.059834070599,33.9151018831637,23.438744868055));
#38553=CARTESIAN_POINT('Ctrl Pts',(126.03114191344,34.032844123862,23.4328581262852));
#38554=CARTESIAN_POINT('Ctrl Pts',(126.002468405446,34.1505098351301,23.4269752107462));
#38555=CARTESIAN_POINT('Ctrl Pts',(125.979013612726,34.269526392017,23.4210922952072));
#38556=CARTESIAN_POINT('Ctrl Pts',(125.96089200761,34.3894006012016,23.4152093796682));
#38557=CARTESIAN_POINT('Ctrl Pts',(125.942777952188,34.5092248692456,23.4093289150277));
#38558=CARTESIAN_POINT('Ctrl Pts',(125.929992721259,34.6299056907607,23.4034484503871));
#38559=CARTESIAN_POINT('Ctrl Pts',(125.922599567219,34.7509403469827,23.3975679857466));
#38560=CARTESIAN_POINT('Ctrl Pts',(125.917493910484,34.8345259728802,23.3935069809659));
#38561=CARTESIAN_POINT('Ctrl Pts',(125.914958764663,34.9182801351293,23.3894459761852));
#38562=CARTESIAN_POINT('Ctrl Pts',(125.915000507333,35.0020359049515,23.3853849714045));
#38563=CARTESIAN_POINT('Ctrl Pts',(125.915000507333,35.0020359057478,23.3853849713659));
#38564=CARTESIAN_POINT('Ctrl Pts',(125.915068041878,35.1375424641031,23.3788147639346));
#38565=CARTESIAN_POINT('Ctrl Pts',(125.921882638121,35.2728211146023,23.3722445565033));
#38566=CARTESIAN_POINT('Ctrl Pts',(125.935349060719,35.4072318035249,23.365674349072));
#38567=CARTESIAN_POINT('Ctrl Pts',(125.948524496332,35.5387381011079,23.359246112891));
#38568=CARTESIAN_POINT('Ctrl Pts',(125.968067066153,35.6694133588767,23.35281787671));
#38569=CARTESIAN_POINT('Ctrl Pts',(125.993836675525,35.7986741623662,23.346389640529));
#38570=CARTESIAN_POINT('Ctrl Pts',(126.020459989606,35.9322171633448,23.3397484474725));
#38571=CARTESIAN_POINT('Ctrl Pts',(126.053729887509,36.064250078893,23.333107254416));
#38572=CARTESIAN_POINT('Ctrl Pts',(126.093437848864,36.1941512296656,23.3264660613596));
#38573=CARTESIAN_POINT('Ctrl Pts',(126.13314581022,36.3240523804383,23.3198248683031));
#38574=CARTESIAN_POINT('Ctrl Pts',(126.179291657195,36.4518215248695,23.3131836752466));
#38575=CARTESIAN_POINT('Ctrl Pts',(126.231614536202,36.576862706844,23.3065424821901));
#38576=CARTESIAN_POINT('Ctrl Pts',(126.277495928968,36.6865100292193,23.3007188885187));
#38577=CARTESIAN_POINT('Ctrl Pts',(126.328240832554,36.7943300130216,23.2948952948472));
#38578=CARTESIAN_POINT('Ctrl Pts',(126.38368242305,36.8998610956174,23.2890717011758));
#38579=CARTESIAN_POINT('Ctrl Pts',(126.439054065743,37.0052590350772,23.2832554548327));
#38580=CARTESIAN_POINT('Ctrl Pts',(126.499110421294,37.1083734587737,23.2774392084897));
#38581=CARTESIAN_POINT('Ctrl Pts',(126.563636386211,37.208762122508,23.2716229621467));
#38582=CARTESIAN_POINT('Ctrl Pts',(126.628097760281,37.3090502966359,23.2658125378983));
#38583=CARTESIAN_POINT('Ctrl Pts',(126.697019623523,37.4066177972911,23.26000211365));
#38584=CARTESIAN_POINT('Ctrl Pts',(126.770140972507,37.501046913299,23.2541916894017));
#38585=CARTESIAN_POINT('Ctrl Pts',(126.846030115791,37.5990503666608,23.2481613285775));
#38586=CARTESIAN_POINT('Ctrl Pts',(126.926442736364,37.693672755502,23.2421309677533));
#38587=CARTESIAN_POINT('Ctrl Pts',(127.0110373891,37.7844797558322,23.2361006069292));
#38588=CARTESIAN_POINT('Ctrl Pts',(127.092455000009,37.8718764030399,23.2302967226959));
#38589=CARTESIAN_POINT('Ctrl Pts',(127.177745883189,37.9557387498791,23.2244928384627));
#38590=CARTESIAN_POINT('Ctrl Pts',(127.26656505548,38.0357138211753,23.2186889542294));
#38591=CARTESIAN_POINT('Ctrl Pts',(127.355371108229,38.1156770792981,23.212885927292));
#38592=CARTESIAN_POINT('Ctrl Pts',(127.447704110287,38.1917539306043,23.2070829003545));
#38593=CARTESIAN_POINT('Ctrl Pts',(127.54318365727,38.2636296447502,23.201279873417));
#38594=CARTESIAN_POINT('Ctrl Pts',(127.638671634098,38.33551170477,23.195476334133));
#38595=CARTESIAN_POINT('Ctrl Pts',(127.73730638195,38.4031916445622,23.1896727948489));
#38596=CARTESIAN_POINT('Ctrl Pts',(127.838676519036,38.4663966608907,23.1838692555648));
#38597=CARTESIAN_POINT('Ctrl Pts',(127.940079529276,38.529622173869,23.1780638342607));
#38598=CARTESIAN_POINT('Ctrl Pts',(128.044219346578,38.588369661408,23.1722584129565));
#38599=CARTESIAN_POINT('Ctrl Pts',(128.150658444778,38.6424114007245,23.1664529916523));
#38600=CARTESIAN_POINT('Ctrl Pts',(128.257215414427,38.6965129862652,23.1606411413814));
#38601=CARTESIAN_POINT('Ctrl Pts',(128.366076383177,38.7458982366508,23.1548292911105));
#38602=CARTESIAN_POINT('Ctrl Pts',(128.476782081956,38.7903868106238,23.1490174408395));
#38603=CARTESIAN_POINT('Ctrl Pts',(128.587560492833,38.8349046049311,23.1432017733141));
#38604=CARTESIAN_POINT('Ctrl Pts',(128.700185662412,38.8745191825761,23.1373861057887));
#38605=CARTESIAN_POINT('Ctrl Pts',(128.814182921208,38.9091000058385,23.1315704382634));
#38606=CARTESIAN_POINT('Ctrl Pts',(128.928343468769,38.943730362396,23.1257464404222));
#38607=CARTESIAN_POINT('Ctrl Pts',(129.043879634147,38.9733124722603,23.1199224425811));
#38608=CARTESIAN_POINT('Ctrl Pts',(129.160306188626,38.997766789489,23.11409844474));
#38609=CARTESIAN_POINT('Ctrl Pts',(129.191194788149,39.0042546531456,23.1125533063672));
#38610=CARTESIAN_POINT('Ctrl Pts',(129.222146031754,39.0103818700825,23.1110081679945));
#38611=CARTESIAN_POINT('Ctrl Pts',(129.253150813995,39.0161475686737,23.1094630296217));
#38612=CARTESIAN_POINT('Ctrl Pts',(129.370019603657,39.0378806745759,23.1036388167605));
#38613=CARTESIAN_POINT('Ctrl Pts',(129.488026301745,39.0545433209723,23.0978146038993));
#38614=CARTESIAN_POINT('Ctrl Pts',(129.606693270703,39.066021989204,23.0919903910381));
#38615=CARTESIAN_POINT('Ctrl Pts',(129.725207575949,39.0774858902588,23.0861736709608));
#38616=CARTESIAN_POINT('Ctrl Pts',(129.844380059345,39.0837790401912,23.0803569508835));
#38617=CARTESIAN_POINT('Ctrl Pts',(129.963722808179,39.0848389154719,23.0745402308063));
#38618=CARTESIAN_POINT('Ctrl Pts',(130.082924450889,39.0858975375981,23.0687303881877));
#38619=CARTESIAN_POINT('Ctrl Pts',(130.202295552219,39.0817352005574,23.0629205455691));
#38620=CARTESIAN_POINT('Ctrl Pts',(130.321343825432,39.0723412364212,23.0571107029505));
#38621=CARTESIAN_POINT('Ctrl Pts',(130.440313011482,39.0629535129633,23.0513047199761));
#38622=CARTESIAN_POINT('Ctrl Pts',(130.558959390372,39.0483411060576,23.0454987370016));
#38623=CARTESIAN_POINT('Ctrl Pts',(130.676791649192,39.0285454029443,23.0396927540272));
#38624=CARTESIAN_POINT('Ctrl Pts',(130.794573438413,39.008758178674,23.033889257856));
#38625=CARTESIAN_POINT('Ctrl Pts',(130.911541399292,38.9837921422135,23.0280857616847));
#38626=CARTESIAN_POINT('Ctrl Pts',(131.027210946424,38.9537403394188,23.0222822655135));
#38627=CARTESIAN_POINT('Ctrl Pts',(131.142858248279,38.9236943161113,23.0164798854561));
#38628=CARTESIAN_POINT('Ctrl Pts',(131.257207238654,38.888564576425,23.0106775053986));
#38629=CARTESIAN_POINT('Ctrl Pts',(131.369785731834,38.8484947770346,23.0048751253412));
#38630=CARTESIAN_POINT('Ctrl Pts',(131.482409236858,38.8084089566845,22.9990704253396));
#38631=CARTESIAN_POINT('Ctrl Pts',(131.593260444399,38.7633792645602,22.993265725338));
#38632=CARTESIAN_POINT('Ctrl Pts',(131.701884602901,38.7135984972002,22.9874610253364));
#38633=CARTESIAN_POINT('Ctrl Pts',(131.810531700835,38.6638072170545,22.9816550994886));
#38634=CARTESIAN_POINT('Ctrl Pts',(131.916950446241,38.6092630430451,22.9758491736407));
#38635=CARTESIAN_POINT('Ctrl Pts',(132.020709414015,38.5502054115374,22.9700432477929));
#38636=CARTESIAN_POINT('Ctrl Pts',(132.124565043898,38.4910927617963,22.9642319131304));
#38637=CARTESIAN_POINT('Ctrl Pts',(132.225755598352,38.4274584690791,22.9584205784678));
#38638=CARTESIAN_POINT('Ctrl Pts',(132.323877385381,38.3595861200027,22.9526092438053));
#38639=CARTESIAN_POINT('Ctrl Pts',(132.379306586531,38.3212448891362,22.9493264087927));
#38640=CARTESIAN_POINT('Ctrl Pts',(132.433757053346,38.2815520030995,22.94604357378));
#38641=CARTESIAN_POINT('Ctrl Pts',(132.487160689988,38.2405642567579,22.9427607387674));
#38642=CARTESIAN_POINT('',(125.915000083441,34.9991743389388,23.4896150285496));
#38643=CARTESIAN_POINT('Ctrl Pts',(125.915000083441,34.9991743389388,23.4896150285496));
#38644=CARTESIAN_POINT('Ctrl Pts',(125.914976188112,35.1173976913889,23.4838237303786));
#38645=CARTESIAN_POINT('Ctrl Pts',(125.920088782344,35.2358210967536,23.4780324322077));
#38646=CARTESIAN_POINT('Ctrl Pts',(125.930363891994,35.3539589643083,23.4722411340368));
#38647=CARTESIAN_POINT('Ctrl Pts',(125.940626165892,35.4719492530606,23.4664570704035));
#38648=CARTESIAN_POINT('Ctrl Pts',(125.956038095578,35.5896543051829,23.4606730067702));
#38649=CARTESIAN_POINT('Ctrl Pts',(125.976573711133,35.7065875020528,23.4548889431369));
#38650=CARTESIAN_POINT('Ctrl Pts',(125.997089184842,35.8234060079085,23.4491105526584));
#38651=CARTESIAN_POINT('Ctrl Pts',(126.022718277938,35.9394537594368,23.4433321621799));
#38652=CARTESIAN_POINT('Ctrl Pts',(126.053383190379,36.0542489070512,23.4375537717014));
#38653=CARTESIAN_POINT('Ctrl Pts',(126.0840271413,36.1689655844951,23.4317793311397));
#38654=CARTESIAN_POINT('Ctrl Pts',(126.119699958342,36.2824309630115,23.4260048905781));
#38655=CARTESIAN_POINT('Ctrl Pts',(126.160272822346,36.3941736624924,23.4202304500164));
#38656=CARTESIAN_POINT('Ctrl Pts',(126.200831076437,36.5058761244586,23.4144580887775));
#38657=CARTESIAN_POINT('Ctrl Pts',(126.246285729108,36.6158567524298,23.4086857275385));
#38658=CARTESIAN_POINT('Ctrl Pts',(126.296458370552,36.7236601750191,23.4029133662996));
#38659=CARTESIAN_POINT('Ctrl Pts',(126.346625133143,36.8314509660127,23.3971416814227));
#38660=CARTESIAN_POINT('Ctrl Pts',(126.401508610812,36.9370646841817,23.3913699965457));
#38661=CARTESIAN_POINT('Ctrl Pts',(126.46088288993,37.0400674207511,23.3855983116687));
#38662=CARTESIAN_POINT('Ctrl Pts',(126.520264635338,37.1430831098706,23.3798259010049));
#38663=CARTESIAN_POINT('Ctrl Pts',(126.584138098126,37.2434868066722,23.374053490341));
#38664=CARTESIAN_POINT('Ctrl Pts',(126.652232561365,37.3408712431088,23.3682810796771));
#38665=CARTESIAN_POINT('Ctrl Pts',(126.720394941295,37.4383528097444,23.3625029116724));
#38666=CARTESIAN_POINT('Ctrl Pts',(126.792786493865,37.5328087612892,23.3567247436676));
#38667=CARTESIAN_POINT('Ctrl Pts',(126.869094375303,37.6238626048713,23.3509465756629));
#38668=CARTESIAN_POINT('Ctrl Pts',(126.94543975801,37.7149611965786,23.3451655679956));
#38669=CARTESIAN_POINT('Ctrl Pts',(127.025705024388,37.8026540447933,23.3393845603284));
#38670=CARTESIAN_POINT('Ctrl Pts',(127.109539652372,37.8866007653973,23.3336035526611));
#38671=CARTESIAN_POINT('Ctrl Pts',(127.193510877074,37.9706842653575,23.3278131256562));
#38672=CARTESIAN_POINT('Ctrl Pts',(127.281062779313,38.0510091615353,23.3220226986513));
#38673=CARTESIAN_POINT('Ctrl Pts',(127.37181044764,38.1272743206927,23.3162322716464));
#38674=CARTESIAN_POINT('Ctrl Pts',(127.460271975996,38.2016181871945,23.3105877186552));
#38675=CARTESIAN_POINT('Ctrl Pts',(127.551769842018,38.2721042776296,23.3049431656641));
#38676=CARTESIAN_POINT('Ctrl Pts',(127.645922334694,38.338494173382,23.299298612673));
#38677=CARTESIAN_POINT('Ctrl Pts',(127.743061268699,38.4069899032227,23.2934750190015));
#38678=CARTESIAN_POINT('Ctrl Pts',(127.8433488203,38.4713529449552,23.28765142533));
#38679=CARTESIAN_POINT('Ctrl Pts',(127.946398371878,38.5312809790464,23.2818278316586));
#38680=CARTESIAN_POINT('Ctrl Pts',(128.04931791114,38.5911334050212,23.2760115853155));
#38681=CARTESIAN_POINT('Ctrl Pts',(128.154992169571,38.6465617490467,23.2701953389725));
#38682=CARTESIAN_POINT('Ctrl Pts',(128.263003899946,38.6973057147599,23.2643790926295));
#38683=CARTESIAN_POINT('Ctrl Pts',(128.370907509982,38.7479988854833,23.2585686683812));
#38684=CARTESIAN_POINT('Ctrl Pts',(128.481143569717,38.794016833623,23.2527582441328));
#38685=CARTESIAN_POINT('Ctrl Pts',(128.593268989434,38.8351444384681,23.2469478198845));
#38686=CARTESIAN_POINT('Ctrl Pts',(128.709638588204,38.8778288082233,23.2409174590603));
#38687=CARTESIAN_POINT('Ctrl Pts',(128.828043017951,38.915245075191,23.2348870982362));
#38688=CARTESIAN_POINT('Ctrl Pts',(128.947962219256,38.9472067982166,23.228856737412));
#38689=CARTESIAN_POINT('Ctrl Pts',(129.063377727881,38.9779681648651,23.2230528531788));
#38690=CARTESIAN_POINT('Ctrl Pts',(129.180195852156,39.0036771868587,23.2172489689455));
#38691=CARTESIAN_POINT('Ctrl Pts',(129.297936769711,39.0242182123583,23.2114450847123));
#38692=CARTESIAN_POINT('Ctrl Pts',(129.415660295673,39.0447562037287,23.2056420577748));
#38693=CARTESIAN_POINT('Ctrl Pts',(129.534305941693,39.0601276465444,23.1998390308373));
#38694=CARTESIAN_POINT('Ctrl Pts',(129.653384206569,39.070268110548,23.1940360038998));
#38695=CARTESIAN_POINT('Ctrl Pts',(129.772472984811,39.0804094698486,23.1882324646158));
#38696=CARTESIAN_POINT('Ctrl Pts',(129.891994050966,39.0853188974369,23.1824289253317));
#38697=CARTESIAN_POINT('Ctrl Pts',(130.011453946273,39.0849839420877,23.1766253860476));
#38698=CARTESIAN_POINT('Ctrl Pts',(130.130952581032,39.0846488781165,23.1708199647434));
#38699=CARTESIAN_POINT('Ctrl Pts',(130.250389597366,39.0790660500591,23.1650145434393));
#38700=CARTESIAN_POINT('Ctrl Pts',(130.369273348812,39.0682750882724,23.1592091221351));
#38701=CARTESIAN_POINT('Ctrl Pts',(130.488288753008,39.0574721764943,23.1533972718641));
#38702=CARTESIAN_POINT('Ctrl Pts',(130.606749262428,39.0414496554454,23.1475854215932));
#38703=CARTESIAN_POINT('Ctrl Pts',(130.724169994242,39.020298847031,23.1417735713223));
#38704=CARTESIAN_POINT('Ctrl Pts',(130.841667848624,38.9991341466521,23.1359579037969));
#38705=CARTESIAN_POINT('Ctrl Pts',(130.958124167934,38.9728345406235,23.1301422362715));
#38706=CARTESIAN_POINT('Ctrl Pts',(131.073067492794,38.9415417232231,23.1243265687461));
#38707=CARTESIAN_POINT('Ctrl Pts',(131.188175461555,38.9102040822408,23.118502570905));
#38708=CARTESIAN_POINT('Ctrl Pts',(131.301765722717,38.8738590784098,23.1126785730638));
#38709=CARTESIAN_POINT('Ctrl Pts',(131.413384972727,38.8326972119995,23.1068545752227));
#38710=CARTESIAN_POINT('Ctrl Pts',(131.44299816817,38.8217767444755,23.10530943685));
#38711=CARTESIAN_POINT('Ctrl Pts',(131.472472757078,38.810517487096,23.1037642984772));
#38712=CARTESIAN_POINT('Ctrl Pts',(131.50180056317,38.7989235407499,23.1022191601045));
#38713=CARTESIAN_POINT('Ctrl Pts',(131.612327895283,38.7552295817026,23.0963960166497));
#38714=CARTESIAN_POINT('Ctrl Pts',(131.721124991532,38.7066375787159,23.090572873195));
#38715=CARTESIAN_POINT('Ctrl Pts',(131.827727178123,38.6533051285585,23.0847497297402));
#38716=CARTESIAN_POINT('Ctrl Pts',(131.934210987083,38.6000319020367,23.0789330526623));
#38717=CARTESIAN_POINT('Ctrl Pts',(132.038504368927,38.5420288721397,23.0731163755845));
#38718=CARTESIAN_POINT('Ctrl Pts',(132.140160799598,38.4795023712974,23.0672996985067));
#38719=CARTESIAN_POINT('Ctrl Pts',(132.241707615457,38.4170432919709,23.0614892934764));
#38720=CARTESIAN_POINT('Ctrl Pts',(132.340622792899,38.3500706613965,23.0556788884461));
#38721=CARTESIAN_POINT('Ctrl Pts',(132.436483529595,38.2788371429535,23.0498684834158));
#38722=CARTESIAN_POINT('Ctrl Pts',(132.453472544451,38.2662127114628,23.0488387285779));
#38723=CARTESIAN_POINT('Ctrl Pts',(132.470365686899,38.2534545647911,23.0478089737399));
#38724=CARTESIAN_POINT('Ctrl Pts',(132.487160689988,38.2405642567579,23.046779218902));
#38725=CARTESIAN_POINT('Ctrl Pts',(132.487160689988,38.2405642567579,24.2969444281512));
#38726=CARTESIAN_POINT('Ctrl Pts',(132.553405712622,38.1897206372063,24.2928615772725));
#38727=CARTESIAN_POINT('Ctrl Pts',(132.618025640998,38.1368950920944,24.2887787263938));
#38728=CARTESIAN_POINT('Ctrl Pts',(132.680900483629,38.0822066116468,24.2846958755152));
#38729=CARTESIAN_POINT('Ctrl Pts',(132.770582312949,38.0042014387652,24.2788722818436));
#38730=CARTESIAN_POINT('Ctrl Pts',(132.857001403456,37.9221530692289,24.2730486881721));
#38731=CARTESIAN_POINT('Ctrl Pts',(132.939771970637,37.8363648849645,24.2672250945006));
#38732=CARTESIAN_POINT('Ctrl Pts',(133.022438110453,37.7506849352373,24.2614088481575));
#38733=CARTESIAN_POINT('Ctrl Pts',(133.101464601485,37.6612748467026,24.2555926018144));
#38734=CARTESIAN_POINT('Ctrl Pts',(133.176499167056,37.5684777674127,24.2497763554713));
#38735=CARTESIAN_POINT('Ctrl Pts',(133.251458622613,37.4757735785112,24.2439659312229));
#38736=CARTESIAN_POINT('Ctrl Pts',(133.322433846866,37.3796894593263,24.2381555069745));
#38737=CARTESIAN_POINT('Ctrl Pts',(133.389110273962,37.280604426666,24.232345082726));
#38738=CARTESIAN_POINT('Ctrl Pts',(133.458310541732,37.1777688205781,24.2263147219019));
#38739=CARTESIAN_POINT('Ctrl Pts',(133.522879834287,37.0717009532646,24.2202843610778));
#38740=CARTESIAN_POINT('Ctrl Pts',(133.58251308558,36.9628614295592,24.2142540002536));
#38741=CARTESIAN_POINT('Ctrl Pts',(133.63990674693,36.8581094894984,24.2084501160203));
#38742=CARTESIAN_POINT('Ctrl Pts',(133.692728223576,36.750790713992,24.202646231787));
#38743=CARTESIAN_POINT('Ctrl Pts',(133.740750791123,36.6413435102733,24.1968423475537));
#38744=CARTESIAN_POINT('Ctrl Pts',(133.788766265222,36.531912473077,24.1910393206161));
#38745=CARTESIAN_POINT('Ctrl Pts',(133.831984075877,36.4203540067187,24.1852362936786));
#38746=CARTESIAN_POINT('Ctrl Pts',(133.870224935108,36.3071281313119,24.179433266741));
#38747=CARTESIAN_POINT('Ctrl Pts',(133.908469170607,36.1938922592443,24.1736297274569));
#38748=CARTESIAN_POINT('Ctrl Pts',(133.941735450357,36.0789890723168,24.1678261881727));
#38749=CARTESIAN_POINT('Ctrl Pts',(133.969894022572,35.9628948278725,24.1620226488886));
#38750=CARTESIAN_POINT('Ctrl Pts',(133.998061726284,35.8467629354186,24.1562172275843));
#38751=CARTESIAN_POINT('Ctrl Pts',(134.021118332114,35.7294396139184,24.1504118062801));
#38752=CARTESIAN_POINT('Ctrl Pts',(134.038985099818,35.6114117789552,24.1446063849758));
#38753=CARTESIAN_POINT('Ctrl Pts',(134.056871653315,35.4932532390895,24.1387945347048));
#38754=CARTESIAN_POINT('Ctrl Pts',(134.069556835499,35.3743890324245,24.1329826844338));
#38755=CARTESIAN_POINT('Ctrl Pts',(134.077013719479,35.2553118312562,24.1271708341628));
#38756=CARTESIAN_POINT('Ctrl Pts',(134.084475501181,35.1361564195428,24.1213551666374));
#38757=CARTESIAN_POINT('Ctrl Pts',(134.086702138233,35.0167881420473,24.1155394991119));
#38758=CARTESIAN_POINT('Ctrl Pts',(134.083718823924,34.8976986455048,24.1097238315864));
#38759=CARTESIAN_POINT('Ctrl Pts',(134.080731236339,34.778438566118,24.1038998337452));
#38760=CARTESIAN_POINT('Ctrl Pts',(134.072518830281,34.6594584706342,24.098075835904));
#38761=CARTESIAN_POINT('Ctrl Pts',(134.059158526398,34.5412440108601,24.0922518380628));
#38762=CARTESIAN_POINT('Ctrl Pts',(134.055613964955,34.5098810703326,24.0907066996908));
#38763=CARTESIAN_POINT('Ctrl Pts',(134.051707336022,34.4785719579602,24.0891615613188));
#38764=CARTESIAN_POINT('Ctrl Pts',(134.047440672667,34.4473255920128,24.0876164229467));
#38765=CARTESIAN_POINT('Ctrl Pts',(134.031359709197,34.3295587031176,24.0817928292753));
#38766=CARTESIAN_POINT('Ctrl Pts',(134.010108618132,34.2123043416824,24.0759692356038));
#38767=CARTESIAN_POINT('Ctrl Pts',(133.983729666343,34.0960514696623,24.0701456419324));
#38768=CARTESIAN_POINT('Ctrl Pts',(133.95738399552,33.9799452679082,24.0643293955894));
#38769=CARTESIAN_POINT('Ctrl Pts',(133.925923421333,33.8648384371461,24.0585131492463));
#38770=CARTESIAN_POINT('Ctrl Pts',(133.88944183767,33.7512137126879,24.0526969029033));
#38771=CARTESIAN_POINT('Ctrl Pts',(133.852996772274,33.6377027272058,24.046886478655));
#38772=CARTESIAN_POINT('Ctrl Pts',(133.811540820233,33.5256712831501,24.0410760544067));
#38773=CARTESIAN_POINT('Ctrl Pts',(133.765218546725,33.4155902375328,24.0352656301583));
#38774=CARTESIAN_POINT('Ctrl Pts',(133.717142879353,33.3013423966518,24.0292352693342));
#38775=CARTESIAN_POINT('Ctrl Pts',(133.663825310019,33.189195961943,24.02320490851));
#38776=CARTESIAN_POINT('Ctrl Pts',(133.605483849221,33.079658568637,24.0171745476858));
#38777=CARTESIAN_POINT('Ctrl Pts',(133.549333463805,32.97423496821,24.0113706634526));
#38778=CARTESIAN_POINT('Ctrl Pts',(133.488529946166,32.8712283654428,24.0055667792194));
#38779=CARTESIAN_POINT('Ctrl Pts',(133.423315685409,32.7710687049548,23.9997628949861));
#38780=CARTESIAN_POINT('Ctrl Pts',(133.358111057495,32.6709238391197,23.9939598680487));
#38781=CARTESIAN_POINT('Ctrl Pts',(133.288497204862,32.5736254213771,23.9881568411112));
#38782=CARTESIAN_POINT('Ctrl Pts',(133.21476059592,32.4795755692898,23.9823538141738));
#38783=CARTESIAN_POINT('Ctrl Pts',(133.141017476806,32.3855174135841,23.9765502748897));
#38784=CARTESIAN_POINT('Ctrl Pts',(133.063151129624,32.2947087151536,23.9707467356057));
#38785=CARTESIAN_POINT('Ctrl Pts',(132.981488757071,32.2075190615763,23.9649431963216));
#38786=CARTESIAN_POINT('Ctrl Pts',(132.899799902363,32.1203011334112,23.9591377750174));
#38787=CARTESIAN_POINT('Ctrl Pts',(132.814312853082,32.0367048820292,23.9533323537133));
#38788=CARTESIAN_POINT('Ctrl Pts',(132.72539168884,31.957063072885,23.9475269324091));
#38789=CARTESIAN_POINT('Ctrl Pts',(132.63637205264,31.8773330678088,23.9417150821382));
#38790=CARTESIAN_POINT('Ctrl Pts',(132.543911014787,31.8015665187781,23.9359032318673));
#38791=CARTESIAN_POINT('Ctrl Pts',(132.448405871834,31.730056011677,23.9300913815964));
#38792=CARTESIAN_POINT('Ctrl Pts',(132.35283800059,31.6584985360909,23.924275714071));
#38793=CARTESIAN_POINT('Ctrl Pts',(132.254222378932,31.5912028991635,23.9184600465456));
#38794=CARTESIAN_POINT('Ctrl Pts',(132.152984016046,31.5284175327888,23.9126443790203));
#38795=CARTESIAN_POINT('Ctrl Pts',(132.051600640138,31.4655422331564,23.9068203811791));
#38796=CARTESIAN_POINT('Ctrl Pts',(131.947587379505,31.4071902979126,23.900996383338));
#38797=CARTESIAN_POINT('Ctrl Pts',(131.841392584402,31.35356360948,23.8951723854969));
#38798=CARTESIAN_POINT('Ctrl Pts',(131.813218526412,31.3393361567288,23.893627247124));
#38799=CARTESIAN_POINT('Ctrl Pts',(131.784891016527,31.3254410334131,23.8920821087512));
#38800=CARTESIAN_POINT('Ctrl Pts',(131.756418628184,31.3118814278052,23.8905369703783));
#38801=CARTESIAN_POINT('Ctrl Pts',(131.649106801958,31.260775562601,23.8847133767068));
#38802=CARTESIAN_POINT('Ctrl Pts',(131.539389563276,31.2142747918228,23.8788897830354));
#38803=CARTESIAN_POINT('Ctrl Pts',(131.427699034967,31.1726117958123,23.8730661893639));
#38804=CARTESIAN_POINT('Ctrl Pts',(131.31614942085,31.1310013638599,23.8672499430209));
#38805=CARTESIAN_POINT('Ctrl Pts',(131.202631848072,31.0942167082698,23.8614336966779));
#38806=CARTESIAN_POINT('Ctrl Pts',(131.087601531727,31.0624439168204,23.8556174503348));
#38807=CARTESIAN_POINT('Ctrl Pts',(130.972686361364,31.0307029301105,23.8498070260865));
#38808=CARTESIAN_POINT('Ctrl Pts',(130.856261851212,31.0039639351245,23.8439966018382));
#38809=CARTESIAN_POINT('Ctrl Pts',(130.738801057856,30.9823641283821,23.8381861775898));
#38810=CARTESIAN_POINT('Ctrl Pts',(130.61689413052,30.9599467242784,23.8321558167656));
#38811=CARTESIAN_POINT('Ctrl Pts',(130.493871338943,30.9430654100478,23.8261254559415));
#38812=CARTESIAN_POINT('Ctrl Pts',(130.370276759999,30.9318161151436,23.8200950951173));
#38813=CARTESIAN_POINT('Ctrl Pts',(130.251323906435,30.9209892994301,23.8142912108841));
#38814=CARTESIAN_POINT('Ctrl Pts',(130.131841882371,30.9153791393266,23.8084873266508));
#38815=CARTESIAN_POINT('Ctrl Pts',(130.012323149958,30.9150185875606,23.8026834424176));
#38816=CARTESIAN_POINT('Ctrl Pts',(129.892822071739,30.914658089052,23.7968804154801));
#38817=CARTESIAN_POINT('Ctrl Pts',(129.77328470418,30.9195456580404,23.7910773885427));
#38818=CARTESIAN_POINT('Ctrl Pts',(129.654204398354,30.9296621268152,23.7852743616052));
#38819=CARTESIAN_POINT('Ctrl Pts',(129.535113578983,30.9397794887685,23.7794708223211));
#38820=CARTESIAN_POINT('Ctrl Pts',(129.416480308469,30.9551266338267,23.7736672830371));
#38821=CARTESIAN_POINT('Ctrl Pts',(129.298793059801,30.9756324935443,23.767863743753));
#38822=CARTESIAN_POINT('Ctrl Pts',(129.18106764653,30.9961450030731,23.7620583224488));
#38823=CARTESIAN_POINT('Ctrl Pts',(129.064289267297,31.0218194842469,23.7562529011446));
#38824=CARTESIAN_POINT('Ctrl Pts',(128.948935812708,31.0525338412861,23.7504474798405));
#38825=CARTESIAN_POINT('Ctrl Pts',(128.833454614845,31.0832822116328,23.7446356295696));
#38826=CARTESIAN_POINT('Ctrl Pts',(128.719401886217,31.1190814932634,23.7388237792986));
#38827=CARTESIAN_POINT('Ctrl Pts',(128.607240120712,31.1597597837314,23.7330119290277));
#38828=CARTESIAN_POINT('Ctrl Pts',(128.495004686758,31.200464791919,23.7271962615023));
#38829=CARTESIAN_POINT('Ctrl Pts',(128.384663065917,31.2460550353343,23.7213805939769));
#38830=CARTESIAN_POINT('Ctrl Pts',(128.276656014013,31.2963112298734,23.7155649264516));
#38831=CARTESIAN_POINT('Ctrl Pts',(128.168494253669,31.3466394109844,23.7097409286104));
#38832=CARTESIAN_POINT('Ctrl Pts',(128.062674097764,31.4016466953972,23.7039169307693));
#38833=CARTESIAN_POINT('Ctrl Pts',(127.95961016421,31.4610687604865,23.6980929329282));
#38834=CARTESIAN_POINT('Ctrl Pts',(127.932266740855,31.4768337582534,23.6965477945554));
#38835=CARTESIAN_POINT('Ctrl Pts',(127.905117151512,31.4929092696491,23.6950026561826));
#38836=CARTESIAN_POINT('Ctrl Pts',(127.878168762405,31.5092898717932,23.6934575178098));
#38837=CARTESIAN_POINT('Ctrl Pts',(127.776600856886,31.5710280129601,23.6876339241383));
#38838=CARTESIAN_POINT('Ctrl Pts',(127.677565959971,31.6373023167307,23.6818103304669));
#38839=CARTESIAN_POINT('Ctrl Pts',(127.581495552781,31.7078789149269,23.6759867367954));
#38840=CARTESIAN_POINT('Ctrl Pts',(127.48554635268,31.7783664702613,23.6701704904523));
#38841=CARTESIAN_POINT('Ctrl Pts',(127.392554529425,31.8531452842667,23.6643542441093));
#38842=CARTESIAN_POINT('Ctrl Pts',(127.302925253798,31.9319366347155,23.6585379977663));
#38843=CARTESIAN_POINT('Ctrl Pts',(127.213385697571,32.0106491145877,23.6527275735179));
#38844=CARTESIAN_POINT('Ctrl Pts',(127.127202297795,32.0933658723822,23.6469171492695));
#38845=CARTESIAN_POINT('Ctrl Pts',(127.044749114069,32.1797664633571,23.6411067250212));
#38846=CARTESIAN_POINT('Ctrl Pts',(126.959174906797,32.2694374954071,23.635076364197));
#38847=CARTESIAN_POINT('Ctrl Pts',(126.877619249221,32.3630764869371,23.6290460033729));
#38848=CARTESIAN_POINT('Ctrl Pts',(126.800460617091,32.4602809727813,23.6230156425487));
#38849=CARTESIAN_POINT('Ctrl Pts',(126.726199759154,32.5538348411556,23.6172117583155));
#38850=CARTESIAN_POINT('Ctrl Pts',(126.65601188945,32.650690873066,23.6114078740822));
#38851=CARTESIAN_POINT('Ctrl Pts',(126.590194518505,32.7504552508632,23.6056039898489));
#38852=CARTESIAN_POINT('Ctrl Pts',(126.52438686949,32.850204892395,23.5998009629115));
#38853=CARTESIAN_POINT('Ctrl Pts',(126.462948660204,32.9528616847348,23.593997935974));
#38854=CARTESIAN_POINT('Ctrl Pts',(126.406134296418,33.0580024962384,23.5881949090365));
#38855=CARTESIAN_POINT('Ctrl Pts',(126.349314916517,33.1631525905762,23.5823913697524));
#38856=CARTESIAN_POINT('Ctrl Pts',(126.297120387921,33.270786780864,23.5765878304683));
#38857=CARTESIAN_POINT('Ctrl Pts',(126.249759034133,33.3804575652569,23.5707842911842));
#38858=CARTESIAN_POINT('Ctrl Pts',(126.20238232161,33.4901639146062,23.56497886988));
#38859=CARTESIAN_POINT('Ctrl Pts',(126.159842062791,33.6019077968527,23.5591734485759));
#38860=CARTESIAN_POINT('Ctrl Pts',(126.122298102512,33.7152225896231,23.5533680272717));
#38861=CARTESIAN_POINT('Ctrl Pts',(126.084712565772,33.8286628680381,23.5475561770007));
#38862=CARTESIAN_POINT('Ctrl Pts',(126.052134500293,33.9436771415982,23.5417443267298));
#38863=CARTESIAN_POINT('Ctrl Pts',(126.024673654135,34.0597843630996,23.5359324764588));
#38864=CARTESIAN_POINT('Ctrl Pts',(125.997194771546,34.1759678444474,23.5301168089334));
#38865=CARTESIAN_POINT('Ctrl Pts',(125.97483987811,34.2932453031681,23.5243011414081));
#38866=CARTESIAN_POINT('Ctrl Pts',(125.957667177219,34.4111279002503,23.5184854738827));
#38867=CARTESIAN_POINT('Ctrl Pts',(125.940469878288,34.5291793514236,23.5126614760415));
#38868=CARTESIAN_POINT('Ctrl Pts',(125.92846962861,34.6478372662121,23.5068374782004));
#38869=CARTESIAN_POINT('Ctrl Pts',(125.921672634806,34.7666099781222,23.5010134803592));
#38870=CARTESIAN_POINT('Ctrl Pts',(125.919869355301,34.7981210259965,23.4994683419866));
#38871=CARTESIAN_POINT('Ctrl Pts',(125.91843203318,34.829640168958,23.497923203614));
#38872=CARTESIAN_POINT('Ctrl Pts',(125.917360170799,34.8611582734836,23.4963780652414));
#38873=CARTESIAN_POINT('Ctrl Pts',(125.915796331449,34.9071429567317,23.4941237196927));
#38874=CARTESIAN_POINT('Ctrl Pts',(125.91500938505,34.9531542090983,23.4918693741441));
#38875=CARTESIAN_POINT('Ctrl Pts',(125.915000083442,34.9991743380008,23.4896150285955));
#38876=CARTESIAN_POINT('Origin',(130.,35.,32.7603849714045));
#38877=CARTESIAN_POINT('',(132.487160689988,38.2405642567579,25.5469383384863));
#38878=CARTESIAN_POINT('',(132.487160689988,38.2405642567579,25.4425452635723));
#38879=CARTESIAN_POINT('',(132.487160689988,38.2405642567579,32.7603849714045));
#38880=CARTESIAN_POINT('',(125.915001572211,34.9964160126988,24.6353849714487));
#38881=CARTESIAN_POINT('Ctrl Pts',(132.487160689988,38.2405642567579,25.4425452635723));
#38882=CARTESIAN_POINT('Ctrl Pts',(132.581714449096,38.1679934406562,25.4367339314664));
#38883=CARTESIAN_POINT('Ctrl Pts',(132.673191731151,38.0912022458023,25.4309225993606));
#38884=CARTESIAN_POINT('Ctrl Pts',(132.761197162703,38.0104842183082,25.4251112672547));
#38885=CARTESIAN_POINT('Ctrl Pts',(132.849133422777,37.9298296344581,25.4193045028035));
#38886=CARTESIAN_POINT('Ctrl Pts',(132.933602962308,37.8452546342454,25.4134977383524));
#38887=CARTESIAN_POINT('Ctrl Pts',(133.014243166955,37.7570932393496,25.4076909739013));
#38888=CARTESIAN_POINT('Ctrl Pts',(133.094848377427,37.6689701024821,25.4018867293214));
#38889=CARTESIAN_POINT('Ctrl Pts',(133.171627281874,37.5772639660214,25.3960824847415));
#38890=CARTESIAN_POINT('Ctrl Pts',(133.244254201368,37.4823455998115,25.3902782401616));
#38891=CARTESIAN_POINT('Ctrl Pts',(133.316866735388,37.3874460344237,25.3844751452492));
#38892=CARTESIAN_POINT('Ctrl Pts',(133.385328671829,37.2893358286794,25.3786720503369));
#38893=CARTESIAN_POINT('Ctrl Pts',(133.449355121551,37.1884182062456,25.3728689554245));
#38894=CARTESIAN_POINT('Ctrl Pts',(133.513383999606,37.0874967563074,25.3670656404181));
#38895=CARTESIAN_POINT('Ctrl Pts',(133.572976837807,36.9837680228594,25.3612623254117));
#38896=CARTESIAN_POINT('Ctrl Pts',(133.627892878756,36.877662978351,25.3554590104053));
#38897=CARTESIAN_POINT('Ctrl Pts',(133.682823962638,36.7715288689096,25.3496541057199));
#38898=CARTESIAN_POINT('Ctrl Pts',(133.733075513914,36.6630175164213,25.3438492010345));
#38899=CARTESIAN_POINT('Ctrl Pts',(133.778453692629,36.5525825880322,25.338044296349));
#38900=CARTESIAN_POINT('Ctrl Pts',(133.823881049005,36.4420279780761,25.3322331007184));
#38901=CARTESIAN_POINT('Ctrl Pts',(133.864424332967,36.3295460082749,25.3264219050877));
#38902=CARTESIAN_POINT('Ctrl Pts',(133.899938580265,36.2156085184639,25.320610709457));
#38903=CARTESIAN_POINT('Ctrl Pts',(133.935474549376,36.101601340314,25.3147959594864));
#38904=CARTESIAN_POINT('Ctrl Pts',(133.965975251114,35.9861372631882,25.3089812095157));
#38905=CARTESIAN_POINT('Ctrl Pts',(133.991346554824,35.8696997638825,25.3031664595451));
#38906=CARTESIAN_POINT('Ctrl Pts',(134.016755660803,35.7530887771672,25.29734304582));
#38907=CARTESIAN_POINT('Ctrl Pts',(134.037020039342,35.6355018738937,25.2915196320948));
#38908=CARTESIAN_POINT('Ctrl Pts',(134.052097211822,35.5174294018909,25.2856962183697));
#38909=CARTESIAN_POINT('Ctrl Pts',(134.059311380028,35.4609337509584,25.2829098148713));
#38910=CARTESIAN_POINT('Ctrl Pts',(134.065338727778,35.4043269619072,25.280123411373));
#38911=CARTESIAN_POINT('Ctrl Pts',(134.07017882144,35.347662712266,25.2773370078746));
#38912=CARTESIAN_POINT('Ctrl Pts',(134.080294635191,35.2292342198261,25.2715134142025));
#38913=CARTESIAN_POINT('Ctrl Pts',(134.085253665983,35.1101728820045,25.2656898205305));
#38914=CARTESIAN_POINT('Ctrl Pts',(134.084990008492,34.9909650389812,25.2598662268584));
#38915=CARTESIAN_POINT('Ctrl Pts',(134.084726683644,34.8719075943584,25.2540499805148));
#38916=CARTESIAN_POINT('Ctrl Pts',(134.079253777168,34.7527044169091,25.2482337341712));
#38917=CARTESIAN_POINT('Ctrl Pts',(134.068557120453,34.6338470843927,25.2424174878276));
#38918=CARTESIAN_POINT('Ctrl Pts',(134.057871171151,34.5151087287217,25.2366070635786));
#38919=CARTESIAN_POINT('Ctrl Pts',(134.041971910454,34.396715933632,25.2307966393297));
#38920=CARTESIAN_POINT('Ctrl Pts',(134.020897212403,34.2791597907377,25.2249862150807));
#38921=CARTESIAN_POINT('Ctrl Pts',(133.999024793444,34.1571539047043,25.2189558542568));
#38922=CARTESIAN_POINT('Ctrl Pts',(133.971577394719,34.0360497085776,25.2129254934328));
#38923=CARTESIAN_POINT('Ctrl Pts',(133.938656491479,33.9163902722225,25.2068951326089));
#38924=CARTESIAN_POINT('Ctrl Pts',(133.90697196764,33.8012247727823,25.201091248375));
#38925=CARTESIAN_POINT('Ctrl Pts',(133.87021776973,33.687397900253,25.1952873641412));
#38926=CARTESIAN_POINT('Ctrl Pts',(133.828536183256,33.5753822640807,25.1894834799073));
#38927=CARTESIAN_POINT('Ctrl Pts',(133.786860753599,33.4633831738158,25.1836804529692));
#38928=CARTESIAN_POINT('Ctrl Pts',(133.740259525162,33.3531951704548,25.1778774260311));
#38929=CARTESIAN_POINT('Ctrl Pts',(133.688923889136,33.2452733716717,25.172074399093));
#38930=CARTESIAN_POINT('Ctrl Pts',(133.637583720709,33.1373420445223,25.1662708598083));
#38931=CARTESIAN_POINT('Ctrl Pts',(133.581508489022,33.0316776885258,25.1604673205236));
#38932=CARTESIAN_POINT('Ctrl Pts',(133.520936457764,32.9287126079691,25.1546637812389));
#38933=CARTESIAN_POINT('Ctrl Pts',(133.460344783703,32.8257141370377,25.1488583599341));
#38934=CARTESIAN_POINT('Ctrl Pts',(133.395253616862,32.7254170341788,25.1430529386293));
#38935=CARTESIAN_POINT('Ctrl Pts',(133.325945270333,32.6282257572131,25.1372475173245));
#38936=CARTESIAN_POINT('Ctrl Pts',(133.256560171226,32.5309268499041,25.1314356670529));
#38937=CARTESIAN_POINT('Ctrl Pts',(133.182948807664,32.4367409665134,25.1256238167814));
#38938=CARTESIAN_POINT('Ctrl Pts',(133.105434706827,32.3460406405456,25.1198119665098));
#38939=CARTESIAN_POINT('Ctrl Pts',(133.027869694312,32.2552807421168,25.1139962989838));
#38940=CARTESIAN_POINT('Ctrl Pts',(132.946397117583,32.1680112581697,25.1081806314578));
#38941=CARTESIAN_POINT('Ctrl Pts',(132.861377218282,32.0845677139234,25.1023649639318));
#38942=CARTESIAN_POINT('Ctrl Pts',(132.776235537156,32.0010046458104,25.09654096609));
#38943=CARTESIAN_POINT('Ctrl Pts',(132.687536694358,31.9212787276694,25.0907169682483));
#38944=CARTESIAN_POINT('Ctrl Pts',(132.595673905589,31.8456851812407,25.0848929704065));
#38945=CARTESIAN_POINT('Ctrl Pts',(132.571302207099,31.8256298014067,25.0833478320397));
#38946=CARTESIAN_POINT('Ctrl Pts',(132.546707963692,31.8058650486462,25.0818026936729));
#38947=CARTESIAN_POINT('Ctrl Pts',(132.521898841803,31.7863959124194,25.0802575553061));
#38948=CARTESIAN_POINT('Ctrl Pts',(132.428393788576,31.713017151686,25.0744339616348));
#38949=CARTESIAN_POINT('Ctrl Pts',(132.331532681142,31.6436044726346,25.0686103679634));
#38950=CARTESIAN_POINT('Ctrl Pts',(132.231686153495,31.5784795905477,25.0627867742921));
#38951=CARTESIAN_POINT('Ctrl Pts',(132.131965597074,31.5134368731729,25.0569705279491));
#38952=CARTESIAN_POINT('Ctrl Pts',(132.029267451023,31.4526714141239,25.0511542816062));
#38953=CARTESIAN_POINT('Ctrl Pts',(131.92399509008,31.3964645286401,25.0453380352633));
#38954=CARTESIAN_POINT('Ctrl Pts',(131.818828107351,31.3403139065589,25.0395276110151));
#38955=CARTESIAN_POINT('Ctrl Pts',(131.711092394101,31.2887129714239,25.0337171867669));
#38956=CARTESIAN_POINT('Ctrl Pts',(131.601219446355,31.2418992450154,25.0279067625186));
#38957=CARTESIAN_POINT('Ctrl Pts',(131.487187580277,31.1933135222336,25.0218764016944));
#38958=CARTESIAN_POINT('Ctrl Pts',(131.37085386077,31.1498848252301,25.0158460408702));
#38959=CARTESIAN_POINT('Ctrl Pts',(131.252728120834,31.111825974153,25.009815680046));
#38960=CARTESIAN_POINT('Ctrl Pts',(131.139038718239,31.0751964635588,25.0040117958129));
#38961=CARTESIAN_POINT('Ctrl Pts',(131.023689893895,31.0435408685883,24.9982079115798));
#38962=CARTESIAN_POINT('Ctrl Pts',(130.907154920439,31.0169992530349,24.9924040273466));
#38963=CARTESIAN_POINT('Ctrl Pts',(130.790637160444,30.9904615579621,24.9866010004093));
#38964=CARTESIAN_POINT('Ctrl Pts',(130.6729339978,30.9690364307302,24.9807979734719));
#38965=CARTESIAN_POINT('Ctrl Pts',(130.554530993477,30.9528132762037,24.9749949465345));
#38966=CARTESIAN_POINT('Ctrl Pts',(130.436117535407,30.9365886893422,24.9691914072506));
#38967=CARTESIAN_POINT('Ctrl Pts',(130.317004517383,30.925567043779,24.9633878679666));
#38968=CARTESIAN_POINT('Ctrl Pts',(130.197684113714,30.9197860361024,24.9575843286827));
#38969=CARTESIAN_POINT('Ctrl Pts',(130.07832501583,30.9140031537125,24.9517789073786));
#38970=CARTESIAN_POINT('Ctrl Pts',(129.958758806199,30.9134643088372,24.9459734860746));
#38971=CARTESIAN_POINT('Ctrl Pts',(129.839478515427,30.918155091997,24.9401680647705));
#38972=CARTESIAN_POINT('Ctrl Pts',(129.720066132773,30.9228510697649,24.9343562144997));
#38973=CARTESIAN_POINT('Ctrl Pts',(129.600940709258,30.9327882195011,24.9285443642289));
#38974=CARTESIAN_POINT('Ctrl Pts',(129.482591166975,30.9479001617053,24.9227325139581));
#38975=CARTESIAN_POINT('Ctrl Pts',(129.364163892077,30.9630220295143,24.9169168464328));
#38976=CARTESIAN_POINT('Ctrl Pts',(129.24651391476,30.9833253893675,24.9111011789075));
#38977=CARTESIAN_POINT('Ctrl Pts',(129.130119329984,31.0086928682532,24.9052855113822));
#38978=CARTESIAN_POINT('Ctrl Pts',(129.013558022534,31.0340966833132,24.8994615135412));
#38979=CARTESIAN_POINT('Ctrl Pts',(128.898256090136,31.0645789916075,24.8936375157002));
#38980=CARTESIAN_POINT('Ctrl Pts',(128.78467599426,31.0999727486757,24.8878135178592));
#38981=CARTESIAN_POINT('Ctrl Pts',(128.754542575699,31.1093629053571,24.8862683794854));
#38982=CARTESIAN_POINT('Ctrl Pts',(128.724530238221,31.119098503364,24.8847232411115));
#38983=CARTESIAN_POINT('Ctrl Pts',(128.694647357325,31.129175865754,24.8831781027377));
#38984=CARTESIAN_POINT('Ctrl Pts',(128.582019414728,31.1671572302927,24.8773545090663));
#38985=CARTESIAN_POINT('Ctrl Pts',(128.470868921732,31.2101195632545,24.8715309153949));
#38986=CARTESIAN_POINT('Ctrl Pts',(128.361668119774,31.2579292296597,24.8657073217235));
#38987=CARTESIAN_POINT('Ctrl Pts',(128.252605090848,31.3056785770691,24.8598910753806));
#38988=CARTESIAN_POINT('Ctrl Pts',(128.145487231186,31.3582629317509,24.8540748290376));
#38989=CARTESIAN_POINT('Ctrl Pts',(128.040770940076,31.4154991294813,24.8482585826947));
#38990=CARTESIAN_POINT('Ctrl Pts',(127.936159470551,31.4726780334621,24.8424481584464));
#38991=CARTESIAN_POINT('Ctrl Pts',(127.833945143399,31.5344993222014,24.8366377341982));
#38992=CARTESIAN_POINT('Ctrl Pts',(127.734563145388,31.6007323056627,24.8308273099499));
#38993=CARTESIAN_POINT('Ctrl Pts',(127.631419333193,31.6694723445425,24.8247969491257));
#38994=CARTESIAN_POINT('Ctrl Pts',(127.531326916347,31.7429644809081,24.8187665883015));
#38995=CARTESIAN_POINT('Ctrl Pts',(127.434743363362,31.8208989654019,24.8127362274773));
#38996=CARTESIAN_POINT('Ctrl Pts',(127.341787108057,31.8959065377445,24.8069323432442));
#38997=CARTESIAN_POINT('Ctrl Pts',(127.252081257699,31.9750285219347,24.801128459011));
#38998=CARTESIAN_POINT('Ctrl Pts',(127.166002388425,32.0579458642664,24.7953245747778));
#38999=CARTESIAN_POINT('Ctrl Pts',(127.07993623392,32.14085095882,24.7895215478404));
#39000=CARTESIAN_POINT('Ctrl Pts',(126.997496289081,32.2275500134187,24.783718520903));
#39001=CARTESIAN_POINT('Ctrl Pts',(126.919023496395,32.3176859273693,24.7779154939656));
#39002=CARTESIAN_POINT('Ctrl Pts',(126.840543775381,32.4078297993785,24.7721119546817));
#39003=CARTESIAN_POINT('Ctrl Pts',(126.766032171056,32.5014108260591,24.7663084153977));
#39004=CARTESIAN_POINT('Ctrl Pts',(126.695790003786,32.5980380309179,24.7605048761137));
#39005=CARTESIAN_POINT('Ctrl Pts',(126.6255250578,32.6946965708524,24.7546994548096));
#39006=CARTESIAN_POINT('Ctrl Pts',(126.559532542362,32.7944029234367,24.7488940335055));
#39007=CARTESIAN_POINT('Ctrl Pts',(126.498070667218,32.8967368333466,24.7430886122014));
#39008=CARTESIAN_POINT('Ctrl Pts',(126.436540728737,32.9991840685898,24.7372767619306));
#39009=CARTESIAN_POINT('Ctrl Pts',(126.379551655807,33.1042643190611,24.7314649116597));
#39010=CARTESIAN_POINT('Ctrl Pts',(126.327315939812,33.2115322776071,24.7256530613889));
#39011=CARTESIAN_POINT('Ctrl Pts',(126.275045915119,33.318870690324,24.7198373938636));
#39012=CARTESIAN_POINT('Ctrl Pts',(126.227535627084,33.4283992989842,24.7140217263383));
#39013=CARTESIAN_POINT('Ctrl Pts',(126.184948982552,33.5396538991489,24.708206058813));
#39014=CARTESIAN_POINT('Ctrl Pts',(126.14230133725,33.651067859515,24.7023820609719));
#39015=CARTESIAN_POINT('Ctrl Pts',(126.104591540685,33.7642123599422,24.6965580631309));
#39016=CARTESIAN_POINT('Ctrl Pts',(126.071933386224,33.8786090433122,24.6907340652898));
#39017=CARTESIAN_POINT('Ctrl Pts',(126.063268999828,33.90895910698,24.6891889269163));
#39018=CARTESIAN_POINT('Ctrl Pts',(126.054959902828,33.9393972602767,24.6876437885428));
#39019=CARTESIAN_POINT('Ctrl Pts',(126.047007611079,33.9699144826103,24.6860986501693));
#39020=CARTESIAN_POINT('Ctrl Pts',(126.008453455647,34.1178675218615,24.6786075385627));
#39021=CARTESIAN_POINT('Ctrl Pts',(125.978189862157,34.2680627700817,24.6711164269561));
#39022=CARTESIAN_POINT('Ctrl Pts',(125.956429349326,34.4196885379352,24.6636253153494));
#39023=CARTESIAN_POINT('Ctrl Pts',(125.935075376485,34.5684815628806,24.6562741561637));
#39024=CARTESIAN_POINT('Ctrl Pts',(125.921909712315,34.7186523616112,24.6489229969779));
#39025=CARTESIAN_POINT('Ctrl Pts',(125.917087813762,34.8694125600498,24.6415718377922));
#39026=CARTESIAN_POINT('Ctrl Pts',(125.915735081896,34.9117067150295,24.639509549011));
#39027=CARTESIAN_POINT('Ctrl Pts',(125.915038744708,34.9540471158435,24.6374472602299));
#39028=CARTESIAN_POINT('Ctrl Pts',(125.915001572211,34.9964160126988,24.6353849714487));
#39029=CARTESIAN_POINT('Ctrl Pts',(125.915001572211,34.9964160136077,24.6353849714045));
#39030=CARTESIAN_POINT('Ctrl Pts',(125.914897993777,35.1144738661888,24.629638553561));
#39031=CARTESIAN_POINT('Ctrl Pts',(125.919916516331,35.2326545958854,24.6238921357174));
#39032=CARTESIAN_POINT('Ctrl Pts',(125.930062305213,35.3504741938474,24.6181457178739));
#39033=CARTESIAN_POINT('Ctrl Pts',(125.940202397681,35.4682276412864,24.6124025263913));
#39034=CARTESIAN_POINT('Ctrl Pts',(125.955463997557,35.5856199446566,24.6066593349086));
#39035=CARTESIAN_POINT('Ctrl Pts',(125.975800204933,35.7021687898124,24.600916143426));
#39036=CARTESIAN_POINT('Ctrl Pts',(125.996130870098,35.8186858719973,24.5951745171311));
#39037=CARTESIAN_POINT('Ctrl Pts',(126.021533322221,35.9343595413328,24.5894328908362));
#39038=CARTESIAN_POINT('Ctrl Pts',(126.051909088729,36.0487150024369,24.5836912645414));
#39039=CARTESIAN_POINT('Ctrl Pts',(126.082284131011,36.1630677370576,24.5779497751393));
#39040=CARTESIAN_POINT('Ctrl Pts',(126.11763214416,36.2761019219958,24.5722082857373));
#39041=CARTESIAN_POINT('Ctrl Pts',(126.157804255104,36.3873560674535,24.5664667963353));
#39042=CARTESIAN_POINT('Ctrl Pts',(126.197985399101,36.4986352293892,24.5607240159087));
#39043=CARTESIAN_POINT('Ctrl Pts',(126.242992654503,36.6081331633545,24.554981235482));
#39044=CARTESIAN_POINT('Ctrl Pts',(126.292628585109,36.7154072962566,24.5492384550554));
#39045=CARTESIAN_POINT('Ctrl Pts',(126.34231651387,36.8227938085766,24.5434896585436));
#39046=CARTESIAN_POINT('Ctrl Pts',(126.396642621412,36.9279514897126,24.5377408620317));
#39047=CARTESIAN_POINT('Ctrl Pts',(126.455362953409,37.0304613288446,24.5319920655199));
#39048=CARTESIAN_POINT('Ctrl Pts',(126.514117959328,37.133031699279,24.5262398743862));
#39049=CARTESIAN_POINT('Ctrl Pts',(126.577272131778,37.2329507626782,24.5204876832526));
#39050=CARTESIAN_POINT('Ctrl Pts',(126.644538532043,37.3298290360142,24.5147354921189));
#39051=CARTESIAN_POINT('Ctrl Pts',(126.711905430002,37.4268520479276,24.5089747070669));
#39052=CARTESIAN_POINT('Ctrl Pts',(126.783396567164,37.5208248695185,24.503213922015));
#39053=CARTESIAN_POINT('Ctrl Pts',(126.858685058135,37.6113914750605,24.4974531369631));
#39054=CARTESIAN_POINT('Ctrl Pts',(126.895426495388,37.6555887648685,24.4946418238423));
#39055=CARTESIAN_POINT('Ctrl Pts',(126.933071724442,37.6989754169815,24.4918305107216));
#39056=CARTESIAN_POINT('Ctrl Pts',(126.971579748943,37.7415134110539,24.4890191976008));
#39057=CARTESIAN_POINT('Ctrl Pts',(127.051348553824,37.829630238471,24.4831956039294));
#39058=CARTESIAN_POINT('Ctrl Pts',(127.135095038228,37.9144047658769,24.4773720102579));
#39059=CARTESIAN_POINT('Ctrl Pts',(127.22250822728,37.9954573027292,24.4715484165865));
#39060=CARTESIAN_POINT('Ctrl Pts',(127.30981113161,38.076407579767,24.4657321702435));
#39061=CARTESIAN_POINT('Ctrl Pts',(127.400771242611,38.1536449309834,24.4599159239005));
#39062=CARTESIAN_POINT('Ctrl Pts',(127.495038491786,38.2268239558998,24.4540996775574));
#39063=CARTESIAN_POINT('Ctrl Pts',(127.589211378925,38.2999297282083,24.4482892533091));
#39064=CARTESIAN_POINT('Ctrl Pts',(127.686684497781,38.3689850069155,24.4424788290608));
#39065=CARTESIAN_POINT('Ctrl Pts',(127.787072666214,38.4336828064603,24.4366684048125));
#39066=CARTESIAN_POINT('Ctrl Pts',(127.89126073446,38.5008295515361,24.4306380439883));
#39067=CARTESIAN_POINT('Ctrl Pts',(127.998588565236,38.5632821156029,24.4246076831641));
#39068=CARTESIAN_POINT('Ctrl Pts',(128.108589592872,38.6207446294659,24.4185773223399));
#39069=CARTESIAN_POINT('Ctrl Pts',(128.21445941535,38.6760490777296,24.4127734381067));
#39070=CARTESIAN_POINT('Ctrl Pts',(128.322804871712,38.7267313236994,24.4069695538735));
#39071=CARTESIAN_POINT('Ctrl Pts',(128.433183143552,38.7725733840906,24.4011656696403));
#39072=CARTESIAN_POINT('Ctrl Pts',(128.54354511134,38.8184086731193,24.3953626427028));
#39073=CARTESIAN_POINT('Ctrl Pts',(128.655938920462,38.8594050417968,24.3895596157653));
#39074=CARTESIAN_POINT('Ctrl Pts',(128.769901084859,38.895392362647,24.3837565888279));
#39075=CARTESIAN_POINT('Ctrl Pts',(128.883873310923,38.9313828608012,24.3779530495438));
#39076=CARTESIAN_POINT('Ctrl Pts',(128.99941377817,38.9623633088683,24.3721495102598));
#39077=CARTESIAN_POINT('Ctrl Pts',(129.116043749136,38.9882134279095,24.3663459709757));
#39078=CARTESIAN_POINT('Ctrl Pts',(129.232711541841,39.014071929843,24.3605405496715));
#39079=CARTESIAN_POINT('Ctrl Pts',(129.350469142469,39.0347967057002,24.3547351283673));
#39080=CARTESIAN_POINT('Ctrl Pts',(129.468828169307,39.050318689471,24.3489297070631));
#39081=CARTESIAN_POINT('Ctrl Pts',(129.58731826781,39.0658578624019,24.3431178567922));
#39082=CARTESIAN_POINT('Ctrl Pts',(129.706410716854,39.0761826894508,24.3373060065213));
#39083=CARTESIAN_POINT('Ctrl Pts',(129.825612406944,39.0812760219554,24.3314941562504));
#39084=CARTESIAN_POINT('Ctrl Pts',(129.944892389344,39.0863726997882,24.325678488725));
#39085=CARTESIAN_POINT('Ctrl Pts',(130.064281348285,39.0862310405327,24.3198628211997));
#39086=CARTESIAN_POINT('Ctrl Pts',(130.183288233519,39.0808859851083,24.3140471536743));
#39087=CARTESIAN_POINT('Ctrl Pts',(130.302465583266,39.0755332734691,24.3082231558332));
#39088=CARTESIAN_POINT('Ctrl Pts',(130.42125936168,39.0649623253379,24.302399157992));
#39089=CARTESIAN_POINT('Ctrl Pts',(130.539185538355,39.0492596798957,24.2965751601509));
#39090=CARTESIAN_POINT('Ctrl Pts',(130.570471995822,39.0450936824675,24.2950300217781));
#39091=CARTESIAN_POINT('Ctrl Pts',(130.601697453545,39.0405667565578,24.2934848834052));
#39092=CARTESIAN_POINT('Ctrl Pts',(130.632853035338,39.035681111741,24.2919397450324));
#39093=CARTESIAN_POINT('Ctrl Pts',(130.750277186331,39.0172673103726,24.2861161798426));
#39094=CARTESIAN_POINT('Ctrl Pts',(130.867086359088,38.9936946159999,24.2802926146529));
#39095=CARTESIAN_POINT('Ctrl Pts',(130.982792533448,38.9650149856211,24.2744690494631));
#39096=CARTESIAN_POINT('Ctrl Pts',(131.09835807508,38.9363702133184,24.2686525624077));
#39097=CARTESIAN_POINT('Ctrl Pts',(131.212822891387,38.9026309457919,24.2628360753524));
#39098=CARTESIAN_POINT('Ctrl Pts',(131.325706145027,38.8639006479251,24.257019588297));
#39099=CARTESIAN_POINT('Ctrl Pts',(131.438460699236,38.8252145068943,24.2512097326821));
#39100=CARTESIAN_POINT('Ctrl Pts',(131.549636896164,38.7815487945288,24.2453998770673));
#39101=CARTESIAN_POINT('Ctrl Pts',(131.658766976276,38.7330573419674,24.2395900214524));
#39102=CARTESIAN_POINT('Ctrl Pts',(131.767824304215,38.6845982165012,24.2337840390099));
#39103=CARTESIAN_POINT('Ctrl Pts',(131.874837856289,38.6313199139055,24.2279780565674));
#39104=CARTESIAN_POINT('Ctrl Pts',(131.979358124367,38.5734250258685,24.2221720741249));
#39105=CARTESIAN_POINT('Ctrl Pts',(132.083838706936,38.5155521200567,24.2163682961674));
#39106=CARTESIAN_POINT('Ctrl Pts',(132.185827530776,38.4530663107781,24.21056451821));
#39107=CARTESIAN_POINT('Ctrl Pts',(132.284898567803,38.3862166993345,24.2047607402525));
#39108=CARTESIAN_POINT('Ctrl Pts',(132.353774100659,38.339741939934,24.200725874853));
#39109=CARTESIAN_POINT('Ctrl Pts',(132.421239880535,38.2911590399292,24.1966910094534));
#39110=CARTESIAN_POINT('Ctrl Pts',(132.487160689988,38.2405642567579,24.1926561440539));
#39111=CARTESIAN_POINT('',(125.915001332191,35.0032990905112,24.7396150285626));
#39112=CARTESIAN_POINT('Ctrl Pts',(125.915001332191,35.0032990905112,24.7396150285626));
#39113=CARTESIAN_POINT('Ctrl Pts',(125.915116126591,35.1454397707582,24.73270773086));
#39114=CARTESIAN_POINT('Ctrl Pts',(125.922653598402,35.2872683007052,24.7258004331575));
#39115=CARTESIAN_POINT('Ctrl Pts',(125.937493194041,35.4280928071526,24.7188931354549));
#39116=CARTESIAN_POINT('Ctrl Pts',(125.952505705088,35.5705582428807,24.711905351853));
#39117=CARTESIAN_POINT('Ctrl Pts',(125.974991434027,35.7119960748056,24.7049175682512));
#39118=CARTESIAN_POINT('Ctrl Pts',(126.004776161893,35.8517109154073,24.6979297846493));
#39119=CARTESIAN_POINT('Ctrl Pts',(126.031877926701,35.9788404553204,24.6915714499835));
#39120=CARTESIAN_POINT('Ctrl Pts',(126.065022300519,36.1045436835966,24.6852131153178));
#39121=CARTESIAN_POINT('Ctrl Pts',(126.104043775727,36.2283118897705,24.678854780652));
#39122=CARTESIAN_POINT('Ctrl Pts',(126.139783513885,36.3416710915234,24.6730311869807));
#39123=CARTESIAN_POINT('Ctrl Pts',(126.180532547933,36.4536519397547,24.6672075933093));
#39124=CARTESIAN_POINT('Ctrl Pts',(126.226166636842,36.5637796350878,24.661383999638));
#39125=CARTESIAN_POINT('Ctrl Pts',(126.271743151569,36.6737683879751,24.6555677532951));
#39126=CARTESIAN_POINT('Ctrl Pts',(126.322192307714,36.7819082643388,24.6497515069522));
#39127=CARTESIAN_POINT('Ctrl Pts',(126.377340030494,36.8877393213422,24.6439352606093));
#39128=CARTESIAN_POINT('Ctrl Pts',(126.432432550099,36.9934644408733,24.6381248363611));
#39129=CARTESIAN_POINT('Ctrl Pts',(126.49221409211,37.0968849787328,24.6323144121128));
#39130=CARTESIAN_POINT('Ctrl Pts',(126.556462644497,37.1975612576805,24.6265039878646));
#39131=CARTESIAN_POINT('Ctrl Pts',(126.623143137483,37.3020483420238,24.6204736270404));
#39132=CARTESIAN_POINT('Ctrl Pts',(126.694635322155,37.403578896778,24.6144432662162));
#39133=CARTESIAN_POINT('Ctrl Pts',(126.770638584712,37.5016893990765,24.608412905392));
#39134=CARTESIAN_POINT('Ctrl Pts',(126.843787464204,37.5961152574942,24.6026090211589));
#39135=CARTESIAN_POINT('Ctrl Pts',(126.921114422886,37.6873729663813,24.5968051369258));
#39136=CARTESIAN_POINT('Ctrl Pts',(127.002307939814,37.7750796947647,24.5910012526926));
#39137=CARTESIAN_POINT('Ctrl Pts',(127.08348946359,37.8627734679264,24.5851982257553));
#39138=CARTESIAN_POINT('Ctrl Pts',(127.168536132488,37.946917004116,24.5793951988179));
#39139=CARTESIAN_POINT('Ctrl Pts',(127.257097679211,38.0271623442769,24.5735921718806));
#39140=CARTESIAN_POINT('Ctrl Pts',(127.345667044992,38.1074147692622,24.5677886325966));
#39141=CARTESIAN_POINT('Ctrl Pts',(127.437751602993,38.1837680397314,24.5619850933127));
#39142=CARTESIAN_POINT('Ctrl Pts',(127.532966430815,38.2559131389697,24.5561815540288));
#39143=CARTESIAN_POINT('Ctrl Pts',(127.628212135696,38.3280816340225,24.5503761327247));
#39144=CARTESIAN_POINT('Ctrl Pts',(127.726589803929,38.3960389973639,24.5445707114206));
#39145=CARTESIAN_POINT('Ctrl Pts',(127.82768438488,38.4595187336255,24.5387652901166));
#39146=CARTESIAN_POINT('Ctrl Pts',(127.928890918722,38.5230687678194,24.5329534398458));
#39147=CARTESIAN_POINT('Ctrl Pts',(128.032820024943,38.5821310599545,24.527141589575));
#39148=CARTESIAN_POINT('Ctrl Pts',(128.139030699114,38.6364843270883,24.5213297393042));
#39149=CARTESIAN_POINT('Ctrl Pts',(128.245311133025,38.6908732937396,24.5155140717789));
#39150=CARTESIAN_POINT('Ctrl Pts',(128.353875748817,38.7405469062713,24.5096984042536));
#39151=CARTESIAN_POINT('Ctrl Pts',(128.464263684739,38.7853320818639,24.5038827367284));
#39152=CARTESIAN_POINT('Ctrl Pts',(128.57480973946,38.8301814073847,24.4980587388874));
#39153=CARTESIAN_POINT('Ctrl Pts',(128.687183943756,38.8701281837541,24.4922347410464));
#39154=CARTESIAN_POINT('Ctrl Pts',(128.800910291905,38.9050491510276,24.4864107432054));
#39155=CARTESIAN_POINT('Ctrl Pts',(128.831082511993,38.9143138739999,24.4848656048314));
#39156=CARTESIAN_POINT('Ctrl Pts',(128.861349852103,38.923225124881,24.4833204664575));
#39157=CARTESIAN_POINT('Ctrl Pts',(128.891703323487,38.9317812091761,24.4817753280836));
#39158=CARTESIAN_POINT('Ctrl Pts',(129.006109646572,38.9640302436215,24.4759514933802));
#39159=CARTESIAN_POINT('Ctrl Pts',(129.122109200102,38.9913336746322,24.4701276586767));
#39160=CARTESIAN_POINT('Ctrl Pts',(129.239236713012,39.0135351276863,24.4643038239732));
#39161=CARTESIAN_POINT('Ctrl Pts',(129.356215278892,39.035708347916,24.4584873952401));
#39162=CARTESIAN_POINT('Ctrl Pts',(129.474318553341,39.0527924198107,24.452670966507));
#39163=CARTESIAN_POINT('Ctrl Pts',(129.593066386042,39.0646808034372,24.4468545377739));
#39164=CARTESIAN_POINT('Ctrl Pts',(129.711694163112,39.0765571677505,24.4410439895273));
#39165=CARTESIAN_POINT('Ctrl Pts',(129.830964797949,39.0832482538911,24.4352334412806));
#39166=CARTESIAN_POINT('Ctrl Pts',(129.950388826311,39.0846987320297,24.429422893034));
#39167=CARTESIAN_POINT('Ctrl Pts',(130.06972128596,39.0861480980101,24.4236168000417));
#39168=CARTESIAN_POINT('Ctrl Pts',(130.18920649813,39.0823648482055,24.4178107070494));
#39169=CARTESIAN_POINT('Ctrl Pts',(130.308351393325,39.0733456050567,24.4120046140571));
#39170=CARTESIAN_POINT('Ctrl Pts',(130.427447782066,39.0643300338361,24.4062008848503));
#39171=CARTESIAN_POINT('Ctrl Pts',(130.546203722888,39.0500827393781,24.4003971556436));
#39172=CARTESIAN_POINT('Ctrl Pts',(130.664128126283,39.0306524077226,24.3945934264368));
#39173=CARTESIAN_POINT('Ctrl Pts',(130.782032350306,39.0112254010099,24.3887906903715));
#39174=CARTESIAN_POINT('Ctrl Pts',(130.899104917338,38.9866171881897,24.3829879543062));
#39175=CARTESIAN_POINT('Ctrl Pts',(131.014862463638,38.9569279978158,24.3771852182409));
#39176=CARTESIAN_POINT('Ctrl Pts',(131.130627519588,38.9272368813867,24.3713821057291));
#39177=CARTESIAN_POINT('Ctrl Pts',(131.245076990016,38.89246423446,24.3655789932174));
#39178=CARTESIAN_POINT('Ctrl Pts',(131.357740886639,38.8527606575999,24.3597758807056));
#39179=CARTESIAN_POINT('Ctrl Pts',(131.47049454896,38.8130254466545,24.3539681445259));
#39180=CARTESIAN_POINT('Ctrl Pts',(131.581459410512,38.7683515950809,24.3481604083462));
#39181=CARTESIAN_POINT('Ctrl Pts',(131.69018367222,38.7189385789711,24.3423526721665));
#39182=CARTESIAN_POINT('Ctrl Pts',(131.798954823004,38.6695042527084,24.3365424313078));
#39183=CARTESIAN_POINT('Ctrl Pts',(131.905483084016,38.6153268732889,24.330732190449));
#39184=CARTESIAN_POINT('Ctrl Pts',(132.009340932926,38.556652079592,24.3249219495903));
#39185=CARTESIAN_POINT('Ctrl Pts',(132.113332546574,38.497901715118,24.3191042253747));
#39186=CARTESIAN_POINT('Ctrl Pts',(132.214646531527,38.4346425819258,24.3132865011591));
#39187=CARTESIAN_POINT('Ctrl Pts',(132.312883826795,38.3671640001268,24.3074687769436));
#39188=CARTESIAN_POINT('Ctrl Pts',(132.372121398138,38.3264740840157,24.3039606606794));
#39189=CARTESIAN_POINT('Ctrl Pts',(132.430240844462,38.2842507233904,24.3004525444153));
#39190=CARTESIAN_POINT('Ctrl Pts',(132.487160689988,38.2405642567579,24.2969444281512));
#39191=CARTESIAN_POINT('Ctrl Pts',(132.487160689988,38.2405642567579,25.5469383384863));
#39192=CARTESIAN_POINT('Ctrl Pts',(132.581965737722,38.1678005744939,25.5411336424445));
#39193=CARTESIAN_POINT('Ctrl Pts',(132.673546042516,38.0908953076657,25.5353289464028));
#39194=CARTESIAN_POINT('Ctrl Pts',(132.76153287122,38.0101762741028,25.529524250361));
#39195=CARTESIAN_POINT('Ctrl Pts',(132.849614100948,37.9293706371293,25.5237133264638));
#39196=CARTESIAN_POINT('Ctrl Pts',(132.93409385506,37.8447433396171,25.5179024025666));
#39197=CARTESIAN_POINT('Ctrl Pts',(133.014639843564,37.7566595026581,25.5120914786694));
#39198=CARTESIAN_POINT('Ctrl Pts',(133.095233487448,37.6685235505189,25.5062771167141));
#39199=CARTESIAN_POINT('Ctrl Pts',(133.171888467963,37.5769272981436,25.5004627547588));
#39200=CARTESIAN_POINT('Ctrl Pts',(133.244313509706,37.4822680859934,25.4946483928035));
#39201=CARTESIAN_POINT('Ctrl Pts',(133.316848358064,37.3874653570778,25.4888252154524));
#39202=CARTESIAN_POINT('Ctrl Pts',(133.385140226788,37.2895907287106,25.4830020381014));
#39203=CARTESIAN_POINT('Ctrl Pts',(133.448941598171,37.189069860102,25.4771788607503));
#39204=CARTESIAN_POINT('Ctrl Pts',(133.485486007905,37.1314931069743,25.4738434374755));
#39205=CARTESIAN_POINT('Ctrl Pts',(133.520558014452,37.0730486299488,25.4705080142006));
#39206=CARTESIAN_POINT('Ctrl Pts',(133.554118108443,37.0138196223183,25.4671725909258));
#39207=CARTESIAN_POINT('Ctrl Pts',(133.612713475523,36.9104067580779,25.4613489972493));
#39208=CARTESIAN_POINT('Ctrl Pts',(133.666886136783,36.8042676185213,25.4555254035728));
#39209=CARTESIAN_POINT('Ctrl Pts',(133.71637332103,36.6958167173178,25.4497018098963));
#39210=CARTESIAN_POINT('Ctrl Pts',(133.765798069844,36.587502643034,25.4438855635482));
#39211=CARTESIAN_POINT('Ctrl Pts',(133.810548931311,36.4768829764279,25.4380693172001));
#39212=CARTESIAN_POINT('Ctrl Pts',(133.850407969834,36.3643985729397,25.4322530708519));
#39213=CARTESIAN_POINT('Ctrl Pts',(133.890227109239,36.2520267669589,25.4264426465985));
#39214=CARTESIAN_POINT('Ctrl Pts',(133.92516403156,36.1377943201641,25.420632222345));
#39215=CARTESIAN_POINT('Ctrl Pts',(133.955048302462,36.022163355434,25.4148217980915));
#39216=CARTESIAN_POINT('Ctrl Pts',(133.986063754791,35.9021555196673,25.4087914372692));
#39217=CARTESIAN_POINT('Ctrl Pts',(134.011636305304,35.780641608255,25.402761076447));
#39218=CARTESIAN_POINT('Ctrl Pts',(134.031631640618,35.6581575148611,25.3967307156247));
#39219=CARTESIAN_POINT('Ctrl Pts',(134.05087602995,35.5402734412426,25.3909268313862));
#39220=CARTESIAN_POINT('Ctrl Pts',(134.064954494204,35.4214911831432,25.3851229471477));
#39221=CARTESIAN_POINT('Ctrl Pts',(134.073799202137,35.3022996206876,25.3793190629092));
#39222=CARTESIAN_POINT('Ctrl Pts',(134.082642603612,35.1831256640998,25.3735160359664));
#39223=CARTESIAN_POINT('Ctrl Pts',(134.086253755971,35.0635429304962,25.3677130090237));
#39224=CARTESIAN_POINT('Ctrl Pts',(134.084616753787,34.9440448868994,25.3619099820809));
#39225=CARTESIAN_POINT('Ctrl Pts',(134.082979607073,34.8245362928745,25.3561064427915));
#39226=CARTESIAN_POINT('Ctrl Pts',(134.076093390145,34.7051128120416,25.3503029035021));
#39227=CARTESIAN_POINT('Ctrl Pts',(134.063994313667,34.5862667302641,25.3444993642127));
#39228=CARTESIAN_POINT('Ctrl Pts',(134.051891313599,34.4673821080882,25.3386939429032));
#39229=CARTESIAN_POINT('Ctrl Pts',(134.034572133354,34.3490756633815,25.3328885215937));
#39230=CARTESIAN_POINT('Ctrl Pts',(134.012124633458,34.2318327489431,25.3270831002842));
#39231=CARTESIAN_POINT('Ctrl Pts',(133.989652275035,34.1144599988288,25.321271250008));
#39232=CARTESIAN_POINT('Ctrl Pts',(133.962040337743,33.9981535311854,25.3154593997317));
#39233=CARTESIAN_POINT('Ctrl Pts',(133.929427456172,33.8833868768994,25.3096475494554));
#39234=CARTESIAN_POINT('Ctrl Pts',(133.896793154285,33.7685448432586,25.3038318819247));
#39235=CARTESIAN_POINT('Ctrl Pts',(133.859151495108,33.6552450237393,25.298016214394));
#39236=CARTESIAN_POINT('Ctrl Pts',(133.816689918595,33.5439426298069,25.2922005468632));
#39237=CARTESIAN_POINT('Ctrl Pts',(133.774167520459,33.4324808072145,25.2863765490168));
#39238=CARTESIAN_POINT('Ctrl Pts',(133.726811586519,33.3230224942386,25.2805525511703));
#39239=CARTESIAN_POINT('Ctrl Pts',(133.674856337234,33.2160000278322,25.2747285533238));
#39240=CARTESIAN_POINT('Ctrl Pts',(133.661072326864,33.1876063850914,25.2731834150017));
#39241=CARTESIAN_POINT('Ctrl Pts',(133.646964825408,33.1593840427803,25.2716382766795));
#39242=CARTESIAN_POINT('Ctrl Pts',(133.632538719108,33.1313407335263,25.2700931383574));
#39243=CARTESIAN_POINT('Ctrl Pts',(133.578167029443,33.0256460938044,25.2642695446866));
#39244=CARTESIAN_POINT('Ctrl Pts',(133.519090795536,32.9221560327778,25.2584459510158));
#39245=CARTESIAN_POINT('Ctrl Pts',(133.455512663061,32.8213175459866,25.252622357345));
#39246=CARTESIAN_POINT('Ctrl Pts',(133.392014743844,32.7206062819248,25.2468061110026));
#39247=CARTESIAN_POINT('Ctrl Pts',(133.324026438936,32.6225402806349,25.2409898646602));
#39248=CARTESIAN_POINT('Ctrl Pts',(133.251797002751,32.5275434780567,25.2351736183179));
#39249=CARTESIAN_POINT('Ctrl Pts',(133.179639868629,32.4326417678017,25.2293631940702));
#39250=CARTESIAN_POINT('Ctrl Pts',(133.103250294645,32.3408034675099,25.2235527698225));
#39251=CARTESIAN_POINT('Ctrl Pts',(133.022921361145,32.2524244424704,25.2177423455748));
#39252=CARTESIAN_POINT('Ctrl Pts',(132.93955181135,32.1607000885202,25.2117119847504));
#39253=CARTESIAN_POINT('Ctrl Pts',(132.851939022808,32.0727024447851,25.2056816239259));
#39254=CARTESIAN_POINT('Ctrl Pts',(132.760457575814,31.9888376044902,25.1996512631015));
#39255=CARTESIAN_POINT('Ctrl Pts',(132.672411811515,31.9081223971538,25.193847378869));
#39256=CARTESIAN_POINT('Ctrl Pts',(132.58078305967,31.8312354684651,25.1880434946364));
#39257=CARTESIAN_POINT('Ctrl Pts',(132.48594302289,31.7585015367975,25.1822396104038));
#39258=CARTESIAN_POINT('Ctrl Pts',(132.391116994998,31.6857783487093,25.1764365834669));
#39259=CARTESIAN_POINT('Ctrl Pts',(132.293080949418,31.6172071861275,25.1706335565301));
#39260=CARTESIAN_POINT('Ctrl Pts',(132.192238888955,31.5530718525396,25.1648305295933));
#39261=CARTESIAN_POINT('Ctrl Pts',(132.091387925192,31.4889308564725,25.1590269903099));
#39262=CARTESIAN_POINT('Ctrl Pts',(131.987730798546,31.429226687216,25.1532234510264));
#39263=CARTESIAN_POINT('Ctrl Pts',(131.881699092076,31.3741989123944,25.147419911743));
#39264=CARTESIAN_POINT('Ctrl Pts',(131.775633000759,31.3191532927071,25.1416144904395));
#39265=CARTESIAN_POINT('Ctrl Pts',(131.667191160414,31.2687872714294,25.1358090691359));
#39266=CARTESIAN_POINT('Ctrl Pts',(131.556827668057,31.2232934172784,25.1300036478324));
#39267=CARTESIAN_POINT('Ctrl Pts',(131.446341958347,31.1777491828949,25.1241917975621));
#39268=CARTESIAN_POINT('Ctrl Pts',(131.333930726595,31.1370880411794,25.1183799472918));
#39269=CARTESIAN_POINT('Ctrl Pts',(131.220066014801,31.1014536145473,25.1125680970215));
#39270=CARTESIAN_POINT('Ctrl Pts',(131.106126516054,31.0657957830323,25.1067524294967));
#39271=CARTESIAN_POINT('Ctrl Pts',(130.990732029815,31.0351713462691,25.1009367619719));
#39272=CARTESIAN_POINT('Ctrl Pts',(130.874366029576,31.0096730652335,25.0951210944471));
#39273=CARTESIAN_POINT('Ctrl Pts',(130.757833347607,30.9841382606636,25.0892970966066));
#39274=CARTESIAN_POINT('Ctrl Pts',(130.640326774996,30.963744336958,25.0834730987661));
#39275=CARTESIAN_POINT('Ctrl Pts',(130.522336297019,30.9485323902546,25.0776491009256));
#39276=CARTESIAN_POINT('Ctrl Pts',(130.491032779941,30.9444965778603,25.0761039625467));
#39277=CARTESIAN_POINT('Ctrl Pts',(130.459695207566,30.9408252247593,25.0745588241678));
#39278=CARTESIAN_POINT('Ctrl Pts',(130.428332725702,30.9375184829844,25.0730136857889));
#39279=CARTESIAN_POINT('Ctrl Pts',(130.310128198923,30.9250554436,25.0671900921183));
#39280=CARTESIAN_POINT('Ctrl Pts',(130.191188658355,30.9177356190145,25.0613664984476));
#39281=CARTESIAN_POINT('Ctrl Pts',(130.071999041145,30.915634548908,25.055542904777));
#39282=CARTESIAN_POINT('Ctrl Pts',(129.952959799343,30.9135361296135,25.0497266584348));
#39283=CARTESIAN_POINT('Ctrl Pts',(129.833671513114,30.9166433760446,25.0439104120926));
#39284=CARTESIAN_POINT('Ctrl Pts',(129.714625382436,30.9249802052444,25.0380941657504));
#39285=CARTESIAN_POINT('Ctrl Pts',(129.595698417591,30.9333086892322,25.0322837415029));
#39286=CARTESIAN_POINT('Ctrl Pts',(129.477013531073,30.9468563135583,25.0264733172554));
#39287=CARTESIAN_POINT('Ctrl Pts',(129.359062469156,30.9655949532111,25.0206628930079));
#39288=CARTESIAN_POINT('Ctrl Pts',(129.236646715558,30.9850428891366,25.0146325321834));
#39289=CARTESIAN_POINT('Ctrl Pts',(129.115021885922,31.0100825943153,25.008602171359));
#39290=CARTESIAN_POINT('Ctrl Pts',(128.994732956179,31.0406233861114,25.0025718105345));
#39291=CARTESIAN_POINT('Ctrl Pts',(128.878961604683,31.0700171861025,24.9967679263021));
#39292=CARTESIAN_POINT('Ctrl Pts',(128.764428051714,31.1045062164083,24.9909640420697));
#39293=CARTESIAN_POINT('Ctrl Pts',(128.651607636186,31.1439575944749,24.9851601578374));
#39294=CARTESIAN_POINT('Ctrl Pts',(128.538803885439,31.1834031451509,24.9793571309008));
#39295=CARTESIAN_POINT('Ctrl Pts',(128.427713154245,31.2278094511495,24.9735541039642));
#39296=CARTESIAN_POINT('Ctrl Pts',(128.318794267271,31.2769941869184,24.9677510770276));
#39297=CARTESIAN_POINT('Ctrl Pts',(128.209865763899,31.3261832651849,24.9619475377444));
#39298=CARTESIAN_POINT('Ctrl Pts',(128.103109858166,31.3801514439701,24.9561439984613));
#39299=CARTESIAN_POINT('Ctrl Pts',(127.998963495633,31.4386690819032,24.9503404591781));
#39300=CARTESIAN_POINT('Ctrl Pts',(127.89478335965,31.497205696424,24.9445350378748));
#39301=CARTESIAN_POINT('Ctrl Pts',(127.793214805663,31.5602945042832,24.9387296165715));
#39302=CARTESIAN_POINT('Ctrl Pts',(127.694667812036,31.6276612709962,24.9329241952683));
#39303=CARTESIAN_POINT('Ctrl Pts',(127.596011686736,31.6951026401677,24.9271123449983));
#39304=CARTESIAN_POINT('Ctrl Pts',(127.500384138194,31.7668311939581,24.9213004947282));
#39305=CARTESIAN_POINT('Ctrl Pts',(127.408164044287,31.8425308586352,24.9154886444582));
#39306=CARTESIAN_POINT('Ctrl Pts',(127.315883379726,31.9182802432584,24.9096729769338));
#39307=CARTESIAN_POINT('Ctrl Pts',(127.227014930153,31.9980056611063,24.9038573094093));
#39308=CARTESIAN_POINT('Ctrl Pts',(127.141901300727,32.0813535970907,24.8980416418848));
#39309=CARTESIAN_POINT('Ctrl Pts',(127.056665755219,32.164820919993,24.8922176440446));
#39310=CARTESIAN_POINT('Ctrl Pts',(126.97519604275,32.2519208205696,24.8863936462044));
#39311=CARTESIAN_POINT('Ctrl Pts',(126.897795127026,32.3422660166799,24.8805696483642));
#39312=CARTESIAN_POINT('Ctrl Pts',(126.87726024207,32.3662350897981,24.879024509983));
#39313=CARTESIAN_POINT('Ctrl Pts',(126.857011512479,32.3904324290943,24.8774793716017));
#39314=CARTESIAN_POINT('Ctrl Pts',(126.837054078806,32.4148504686183,24.8759342332205));
#39315=CARTESIAN_POINT('Ctrl Pts',(126.762195742137,32.5064400914854,24.8701385737665));
#39316=CARTESIAN_POINT('Ctrl Pts',(126.691190191979,32.6014415258938,24.8643429143124));
#39317=CARTESIAN_POINT('Ctrl Pts',(126.624365980108,32.6994957153382,24.8585472548584));
#39318=CARTESIAN_POINT('Ctrl Pts',(126.557622092834,32.7974320408669,24.8527585619513));
#39319=CARTESIAN_POINT('Ctrl Pts',(126.495049783105,32.8984134903318,24.8469698690443));
#39320=CARTESIAN_POINT('Ctrl Pts',(126.436938220602,33.0020471086147,24.8411811761372));
#39321=CARTESIAN_POINT('Ctrl Pts',(126.378882465277,33.1055812028186,24.8353980423754));
#39322=CARTESIAN_POINT('Ctrl Pts',(126.325279140325,33.2117620446582,24.8296149086135));
#39323=CARTESIAN_POINT('Ctrl Pts',(126.276374442191,33.3201673579696,24.8238317748516));
#39324=CARTESIAN_POINT('Ctrl Pts',(126.227504892711,33.4284947585027,24.8180527975283));
#39325=CARTESIAN_POINT('Ctrl Pts',(126.183327422776,33.5390430764458,24.8122738202049));
#39326=CARTESIAN_POINT('Ctrl Pts',(126.144042212233,33.6513656763384,24.8064948428816));
#39327=CARTESIAN_POINT('Ctrl Pts',(126.104770622543,33.7636493320684,24.8007178692283));
#39328=CARTESIAN_POINT('Ctrl Pts',(126.070388060113,33.8777056596514,24.794940895575));
#39329=CARTESIAN_POINT('Ctrl Pts',(126.041046289915,33.9930687603403,24.7891639219217));
#39330=CARTESIAN_POINT('Ctrl Pts',(126.011711368872,34.1084049321902,24.7833882967689));
#39331=CARTESIAN_POINT('Ctrl Pts',(125.98741499763,34.2250468699919,24.7776126716161));
#39332=CARTESIAN_POINT('Ctrl Pts',(125.968258611743,34.3425151117976,24.7718370464633));
#39333=CARTESIAN_POINT('Ctrl Pts',(125.949095050159,34.4600273554534,24.7660592578475));
#39334=CARTESIAN_POINT('Ctrl Pts',(125.935075389371,34.5783661145012,24.7602814692317));
#39335=CARTESIAN_POINT('Ctrl Pts',(125.926249593193,34.6970435294684,24.7545036806159));
#39336=CARTESIAN_POINT('Ctrl Pts',(125.918668595408,34.7989825729109,24.7495407966091));
#39337=CARTESIAN_POINT('Ctrl Pts',(125.914918852587,34.9011712043574,24.7445779126023));
#39338=CARTESIAN_POINT('Ctrl Pts',(125.91500133219,35.0032990898339,24.7396150285955));
#39339=CARTESIAN_POINT('Origin',(130.,35.,32.7603849714045));
#39340=CARTESIAN_POINT('',(132.487160689988,38.2405642567579,26.7967734493137));
#39341=CARTESIAN_POINT('',(132.487160689988,38.2405642567579,26.6927660706478));
#39342=CARTESIAN_POINT('',(132.487160689988,38.2405642567579,32.7603849714045));
#39343=CARTESIAN_POINT('',(125.91500046357,35.0019461147839,25.8853849714464));
#39344=CARTESIAN_POINT('Ctrl Pts',(132.487160689988,38.2405642567579,26.6927660706478));
#39345=CARTESIAN_POINT('Ctrl Pts',(132.584486306372,38.1658660165692,26.6867872548488));
#39346=CARTESIAN_POINT('Ctrl Pts',(132.678341590377,38.0868578909177,26.6808084390498));
#39347=CARTESIAN_POINT('Ctrl Pts',(132.768344338777,38.0039132181141,26.6748296232508));
#39348=CARTESIAN_POINT('Ctrl Pts',(132.858347087177,37.9209685453105,26.6688508074517));
#39349=CARTESIAN_POINT('Ctrl Pts',(132.944497019818,37.8340876999327,26.6628719916527));
#39350=CARTESIAN_POINT('Ctrl Pts',(133.02645672952,37.7436808605129,26.6568931758537));
#39351=CARTESIAN_POINT('Ctrl Pts',(133.106288598548,37.6556211664249,26.6510695822666));
#39352=CARTESIAN_POINT('Ctrl Pts',(133.182402651793,37.563932319849,26.6452459886796));
#39353=CARTESIAN_POINT('Ctrl Pts',(133.254451673087,37.4689611798372,26.6394223950925));
#39354=CARTESIAN_POINT('Ctrl Pts',(133.32640979382,37.3741098600497,26.6336061488353));
#39355=CARTESIAN_POINT('Ctrl Pts',(133.39431283873,37.275984805828,26.6277899025781));
#39356=CARTESIAN_POINT('Ctrl Pts',(133.457851565369,37.1749684024999,26.6219736563209));
#39357=CARTESIAN_POINT('Ctrl Pts',(133.521326689378,37.0740531171726,26.6161632321596));
#39358=CARTESIAN_POINT('Ctrl Pts',(133.580445969959,36.9702525841654,26.6103528079983));
#39359=CARTESIAN_POINT('Ctrl Pts',(133.634941851192,36.8639803481948,26.604542383837));
#39360=CARTESIAN_POINT('Ctrl Pts',(133.691500515394,36.7536854860428,26.5985120229807));
#39361=CARTESIAN_POINT('Ctrl Pts',(133.743078583032,36.6407284626116,26.5924816621244));
#39362=CARTESIAN_POINT('Ctrl Pts',(133.789427576046,36.5256027156187,26.5864513012681));
#39363=CARTESIAN_POINT('Ctrl Pts',(133.834035882586,36.4148006403525,26.5806474171245));
#39364=CARTESIAN_POINT('Ctrl Pts',(133.873800632328,36.3019902142375,26.574843532981));
#39365=CARTESIAN_POINT('Ctrl Pts',(133.908548515556,36.1876335720844,26.5690396488374));
#39366=CARTESIAN_POINT('Ctrl Pts',(133.943291266146,36.0732938216467,26.5632366219905));
#39367=CARTESIAN_POINT('Ctrl Pts',(133.973018505244,35.9574086999655,26.5574335951435));
#39368=CARTESIAN_POINT('Ctrl Pts',(133.997606581845,35.8404561956399,26.5516305682966));
#39369=CARTESIAN_POINT('Ctrl Pts',(134.022196829313,35.7234933656456,26.5458270291037));
#39370=CARTESIAN_POINT('Ctrl Pts',(134.041646928137,35.6054633652587,26.5400234899109));
#39371=CARTESIAN_POINT('Ctrl Pts',(134.05588433561,35.4868544506889,26.5342199507181));
#39372=CARTESIAN_POINT('Ctrl Pts',(134.070126360107,35.3682070726434,26.5284145295058));
#39373=CARTESIAN_POINT('Ctrl Pts',(134.079152282759,35.2489808122703,26.5226091082934));
#39374=CARTESIAN_POINT('Ctrl Pts',(134.082941474663,35.1296684791143,26.5168036870811));
#39375=CARTESIAN_POINT('Ctrl Pts',(134.086734862746,35.0102240186003,26.5109918369025));
#39376=CARTESIAN_POINT('Ctrl Pts',(134.085279931423,34.8906937034143,26.5051799867239));
#39377=CARTESIAN_POINT('Ctrl Pts',(134.078608182355,34.7715699344925,26.4993681365453));
#39378=CARTESIAN_POINT('Ctrl Pts',(134.071932051247,34.6523679244463,26.4935524691127));
#39379=CARTESIAN_POINT('Ctrl Pts',(134.060032319172,34.5335733978143,26.48773680168));
#39380=CARTESIAN_POINT('Ctrl Pts',(134.042992121292,34.4156715759345,26.4819211342473));
#39381=CARTESIAN_POINT('Ctrl Pts',(134.025927515168,34.2976008724203,26.4760971364987));
#39382=CARTESIAN_POINT('Ctrl Pts',(134.003707822574,34.1804258256439,26.4702731387502));
#39383=CARTESIAN_POINT('Ctrl Pts',(133.976466834666,34.0646195892561,26.4644491410016));
#39384=CARTESIAN_POINT('Ctrl Pts',(133.969239647923,34.0338955457959,26.4629040017628));
#39385=CARTESIAN_POINT('Ctrl Pts',(133.961659295102,34.0032677538822,26.461358862524));
#39386=CARTESIAN_POINT('Ctrl Pts',(133.953728849266,33.9727448289353,26.4598137232852));
#39387=CARTESIAN_POINT('Ctrl Pts',(133.923839184085,33.8577046375087,26.4539901295726));
#39388=CARTESIAN_POINT('Ctrl Pts',(133.888876229057,33.7437845508683,26.44816653586));
#39389=CARTESIAN_POINT('Ctrl Pts',(133.848939755856,33.6314651061112,26.4423429421474));
#39390=CARTESIAN_POINT('Ctrl Pts',(133.809053668444,33.519287369007,26.4365266957627));
#39391=CARTESIAN_POINT('Ctrl Pts',(133.764206678945,33.4087066385016,26.4307104493781));
#39392=CARTESIAN_POINT('Ctrl Pts',(133.714549087991,33.3001911657764,26.4248942029934));
#39393=CARTESIAN_POINT('Ctrl Pts',(133.664941204556,33.1917843176292,26.419083778703));
#39394=CARTESIAN_POINT('Ctrl Pts',(133.610532468321,33.0854389837292,26.4132733544126));
#39395=CARTESIAN_POINT('Ctrl Pts',(133.551522091769,32.98160563029,26.4074629301222));
#39396=CARTESIAN_POINT('Ctrl Pts',(133.490278051012,32.8738419707181,26.4014325693136));
#39397=CARTESIAN_POINT('Ctrl Pts',(133.42407727388,32.7687846385915,26.3954022085051));
#39398=CARTESIAN_POINT('Ctrl Pts',(133.353196250823,32.6669119383383,26.3893718476965));
#39399=CARTESIAN_POINT('Ctrl Pts',(133.284977239016,32.568865174316,26.3835679634204));
#39400=CARTESIAN_POINT('Ctrl Pts',(133.212423438947,32.4737685168427,26.3777640791442));
#39401=CARTESIAN_POINT('Ctrl Pts',(133.135826364783,32.3820202426427,26.3719601948681));
#39402=CARTESIAN_POINT('Ctrl Pts',(133.059240604823,32.2902855206403,26.3661571678875));
#39403=CARTESIAN_POINT('Ctrl Pts',(132.978613020103,32.2018985116969,26.360354140907));
#39404=CARTESIAN_POINT('Ctrl Pts',(132.894275605537,32.1172246498917,26.3545511139264));
#39405=CARTESIAN_POINT('Ctrl Pts',(132.809930744858,32.0325433122674,26.348747574599));
#39406=CARTESIAN_POINT('Ctrl Pts',(132.721875691282,31.9515760629171,26.3429440352717));
#39407=CARTESIAN_POINT('Ctrl Pts',(132.630479042968,31.8746512187425,26.3371404959443));
#39408=CARTESIAN_POINT('Ctrl Pts',(132.539052755784,31.7977014287365,26.3313350745967));
#39409=CARTESIAN_POINT('Ctrl Pts',(132.444283030994,31.7247969138078,26.3255296532491));
#39410=CARTESIAN_POINT('Ctrl Pts',(132.346570732286,31.656225067625,26.3197242319015));
#39411=CARTESIAN_POINT('Ctrl Pts',(132.248750226252,31.5875772844704,26.3139123815872));
#39412=CARTESIAN_POINT('Ctrl Pts',(132.147980976242,31.5232719820419,26.3081005312729));
#39413=CARTESIAN_POINT('Ctrl Pts',(132.044692080272,31.4635527295215,26.3022886809585));
#39414=CARTESIAN_POINT('Ctrl Pts',(131.9413353436,31.4037942530754,26.2964730133897));
#39415=CARTESIAN_POINT('Ctrl Pts',(131.835456026457,31.3486280135417,26.2906573458209));
#39416=CARTESIAN_POINT('Ctrl Pts',(131.727505525656,31.2982504597383,26.2848416782521));
#39417=CARTESIAN_POINT('Ctrl Pts',(131.619400397425,31.2478007455318,26.2790176803678));
#39418=CARTESIAN_POINT('Ctrl Pts',(131.509218539976,31.2021535635289,26.2731936824835));
#39419=CARTESIAN_POINT('Ctrl Pts',(131.397429024825,31.1614563802691,26.2673696845992));
#39420=CARTESIAN_POINT('Ctrl Pts',(131.367770665239,31.1506591986764,26.2658245466384));
#39421=CARTESIAN_POINT('Ctrl Pts',(131.33799921508,31.1402101560168,26.2642794086776));
#39422=CARTESIAN_POINT('Ctrl Pts',(131.308123564557,31.1301114047234,26.2627342707168));
#39423=CARTESIAN_POINT('Ctrl Pts',(131.195522843021,31.0920494157021,26.2569106770474));
#39424=CARTESIAN_POINT('Ctrl Pts',(131.081077952103,31.0588445804792,26.251087083378));
#39425=CARTESIAN_POINT('Ctrl Pts',(130.965245490355,31.0306768658436,26.2452634897086));
#39426=CARTESIAN_POINT('Ctrl Pts',(130.849559168461,31.0025446889636,26.2394472433676));
#39427=CARTESIAN_POINT('Ctrl Pts',(130.732489150968,30.9794370882101,26.2336309970266));
#39428=CARTESIAN_POINT('Ctrl Pts',(130.614509458979,30.9614850347156,26.2278147506856));
#39429=CARTESIAN_POINT('Ctrl Pts',(130.49664786531,30.9435509513255,26.2220043264392));
#39430=CARTESIAN_POINT('Ctrl Pts',(130.377878810019,30.9307622096322,26.2161939021928));
#39431=CARTESIAN_POINT('Ctrl Pts',(130.258688251068,30.923199123239,26.2103834779464));
#39432=CARTESIAN_POINT('Ctrl Pts',(130.134986082876,30.915349758379,26.2043531171215));
#39433=CARTESIAN_POINT('Ctrl Pts',(130.010830306498,30.9131295749625,26.1983227562966));
#39434=CARTESIAN_POINT('Ctrl Pts',(129.88677252396,30.9165695134275,26.1922923954716));
#39435=CARTESIAN_POINT('Ctrl Pts',(129.767373862957,30.9198802613568,26.1864885112402));
#39436=CARTESIAN_POINT('Ctrl Pts',(129.648066412887,30.9284336419937,26.1806846270087));
#39437=CARTESIAN_POINT('Ctrl Pts',(129.529343078354,30.9422041620965,26.1748807427772));
#39438=CARTESIAN_POINT('Ctrl Pts',(129.410637280526,30.9559726481463,26.1690777158414));
#39439=CARTESIAN_POINT('Ctrl Pts',(129.29251583216,30.9749566940936,26.1632746889056));
#39440=CARTESIAN_POINT('Ctrl Pts',(129.175466359288,30.9990789466257,26.1574716619699));
#39441=CARTESIAN_POINT('Ctrl Pts',(129.05840655217,31.0232033289008,26.1516681226874));
#39442=CARTESIAN_POINT('Ctrl Pts',(128.942419308674,31.0524667373019,26.1458645834049));
#39443=CARTESIAN_POINT('Ctrl Pts',(128.827981275663,31.0867408583377,26.1400610441225));
#39444=CARTESIAN_POINT('Ctrl Pts',(128.713506131731,31.1210260940716,26.1342556228199));
#39445=CARTESIAN_POINT('Ctrl Pts',(128.600581588393,31.1603251569359,26.1284502015172));
#39446=CARTESIAN_POINT('Ctrl Pts',(128.489667752289,31.2044603148532,26.1226447802146));
#39447=CARTESIAN_POINT('Ctrl Pts',(128.378631089375,31.2486443483737,26.1168329299451));
#39448=CARTESIAN_POINT('Ctrl Pts',(128.269609957951,31.2976750159768,26.1110210796756));
#39449=CARTESIAN_POINT('Ctrl Pts',(128.16304328815,31.3513269482195,26.1052092294061));
#39450=CARTESIAN_POINT('Ctrl Pts',(128.056406624787,31.40501411934,26.099393561882));
#39451=CARTESIAN_POINT('Ctrl Pts',(127.952227989088,31.4633284009306,26.093577894358));
#39452=CARTESIAN_POINT('Ctrl Pts',(127.85091912446,31.5259999438126,26.087762226834));
#39453=CARTESIAN_POINT('Ctrl Pts',(127.749465145822,31.5887612569136,26.0819382289941));
#39454=CARTESIAN_POINT('Ctrl Pts',(127.650889479172,31.6558920595854,26.0761142311542));
#39455=CARTESIAN_POINT('Ctrl Pts',(127.555572589185,31.7270808697345,26.0702902333143));
#39456=CARTESIAN_POINT('Ctrl Pts',(127.530284498452,31.7459676493019,26.0687450949257));
#39457=CARTESIAN_POINT('Ctrl Pts',(127.505225589071,31.7651398518029,26.067199956537));
#39458=CARTESIAN_POINT('Ctrl Pts',(127.480402534567,31.7845912216043,26.0656548181484));
#39459=CARTESIAN_POINT('Ctrl Pts',(127.387890871814,31.8570834510718,26.0598963277298));
#39460=CARTESIAN_POINT('Ctrl Pts',(127.298344601785,31.9337015222224,26.0541378373113));
#39461=CARTESIAN_POINT('Ctrl Pts',(127.212159759072,32.0141715067564,26.0483793468928));
#39462=CARTESIAN_POINT('Ctrl Pts',(127.126084184855,32.0945394683149,26.0426281573123));
#39463=CARTESIAN_POINT('Ctrl Pts',(127.043361868386,32.1787493515523,26.0368769677318));
#39464=CARTESIAN_POINT('Ctrl Pts',(126.964357841701,32.2664854698104,26.0311257781514));
#39465=CARTESIAN_POINT('Ctrl Pts',(126.885432208038,32.3541345304871,26.0253802952817));
#39466=CARTESIAN_POINT('Ctrl Pts',(126.810217805867,32.4453025593198,26.0196348124121));
#39467=CARTESIAN_POINT('Ctrl Pts',(126.739044130039,32.5396358370833,26.0138893295424));
#39468=CARTESIAN_POINT('Ctrl Pts',(126.667920512356,32.6339027680003,26.0081478876081));
#39469=CARTESIAN_POINT('Ctrl Pts',(126.600832219958,32.731330187218,26.0024064456737));
#39470=CARTESIAN_POINT('Ctrl Pts',(126.538069144984,32.8315305501143,25.9966650037393));
#39471=CARTESIAN_POINT('Ctrl Pts',(126.47532866335,32.9316948430618,25.990925628599));
#39472=CARTESIAN_POINT('Ctrl Pts',(126.416910526326,33.0346297414538,25.9851862534588));
#39473=CARTESIAN_POINT('Ctrl Pts',(126.363061503255,33.1399184504729,25.9794468783185));
#39474=CARTESIAN_POINT('Ctrl Pts',(126.309218443451,33.2451954997685,25.9737081387594));
#39475=CARTESIAN_POINT('Ctrl Pts',(126.259943681612,33.3528254686493,25.9679693992004));
#39476=CARTESIAN_POINT('Ctrl Pts',(126.215437817399,33.4623673761183,25.9622306596413));
#39477=CARTESIAN_POINT('Ctrl Pts',(126.170925788959,33.5719244555462,25.9564911252456));
#39478=CARTESIAN_POINT('Ctrl Pts',(126.131184127378,33.6833936117948,25.9507515908499));
#39479=CARTESIAN_POINT('Ctrl Pts',(126.09636482613,33.7963150622686,25.9450120564542));
#39480=CARTESIAN_POINT('Ctrl Pts',(126.061513761249,33.9093395244424,25.9392672862137));
#39481=CARTESIAN_POINT('Ctrl Pts',(126.031594144115,34.0238185252172,25.9335225159732));
#39482=CARTESIAN_POINT('Ctrl Pts',(126.006707715964,34.1392783642426,25.9277777457326));
#39483=CARTESIAN_POINT('Ctrl Pts',(125.981808406242,34.2547979669366,25.9220300019166));
#39484=CARTESIAN_POINT('Ctrl Pts',(125.961947542634,34.3712990066402,25.9162822581006));
#39485=CARTESIAN_POINT('Ctrl Pts',(125.947175220413,34.4883005706798,25.9105345142846));
#39486=CARTESIAN_POINT('Ctrl Pts',(125.932382690921,34.6054621828346,25.9047789080475));
#39487=CARTESIAN_POINT('Ctrl Pts',(125.922692631631,34.7231252698855,25.8990233018104));
#39488=CARTESIAN_POINT('Ctrl Pts',(125.91810307506,34.8408067395617,25.8932676955733));
#39489=CARTESIAN_POINT('Ctrl Pts',(125.916007830481,34.8945312024069,25.8906401208644));
#39490=CARTESIAN_POINT('Ctrl Pts',(125.914974887006,34.9482595324203,25.8880125461554));
#39491=CARTESIAN_POINT('Ctrl Pts',(125.91500046357,35.0019461147839,25.8853849714464));
#39492=CARTESIAN_POINT('Ctrl Pts',(125.91500046357,35.0019461156404,25.8853849714045));
#39493=CARTESIAN_POINT('Ctrl Pts',(125.915055004632,35.1164306863377,25.879781769463));
#39494=CARTESIAN_POINT('Ctrl Pts',(125.919921914211,35.2307950927835,25.8741785675215));
#39495=CARTESIAN_POINT('Ctrl Pts',(125.92957331797,35.3447486420832,25.8685753655799));
#39496=CARTESIAN_POINT('Ctrl Pts',(125.939604342104,35.4631843465316,25.8627517719035));
#39497=CARTESIAN_POINT('Ctrl Pts',(125.954824952508,35.5813728704778,25.856928178227));
#39498=CARTESIAN_POINT('Ctrl Pts',(125.975217969216,35.6988237293334,25.8511045845505));
#39499=CARTESIAN_POINT('Ctrl Pts',(125.995585257104,35.8161264064861,25.8452883382024));
#39500=CARTESIAN_POINT('Ctrl Pts',(126.021111902476,35.932692870866,25.8394720918543));
#39501=CARTESIAN_POINT('Ctrl Pts',(126.051728847284,36.0480362134157,25.8336558455062));
#39502=CARTESIAN_POINT('Ctrl Pts',(126.082315144361,36.1632640966445,25.8278454212528));
#39503=CARTESIAN_POINT('Ctrl Pts',(126.117981500012,36.2772709013383,25.8220349969993));
#39504=CARTESIAN_POINT('Ctrl Pts',(126.158607643251,36.3895789871435,25.8162245727458));
#39505=CARTESIAN_POINT('Ctrl Pts',(126.20077156999,36.5061381661497,25.8101942119235));
#39506=CARTESIAN_POINT('Ctrl Pts',(126.248278102885,36.6208670436773,25.8041638511013));
#39507=CARTESIAN_POINT('Ctrl Pts',(126.300935504727,36.7332474894862,25.798133490279));
#39508=CARTESIAN_POINT('Ctrl Pts',(126.351615302105,36.8414073686986,25.7923296060405));
#39509=CARTESIAN_POINT('Ctrl Pts',(126.407065864032,36.9473916277977,25.7865257218021));
#39510=CARTESIAN_POINT('Ctrl Pts',(126.467067129435,37.050758477266,25.7807218375636));
#39511=CARTESIAN_POINT('Ctrl Pts',(126.527059532009,37.1541100583459,25.7749188106208));
#39512=CARTESIAN_POINT('Ctrl Pts',(126.59160109635,37.2548446456019,25.7691157836781));
#39513=CARTESIAN_POINT('Ctrl Pts',(126.660426315324,37.352545983529,25.7633127567354));
#39514=CARTESIAN_POINT('Ctrl Pts',(126.729257610845,37.4502559474628,25.757509217446));
#39515=CARTESIAN_POINT('Ctrl Pts',(126.802373077781,37.5449317957676,25.7517056781567));
#39516=CARTESIAN_POINT('Ctrl Pts',(126.879464862812,37.6361876749538,25.7459021388673));
#39517=CARTESIAN_POINT('Ctrl Pts',(126.956581647811,37.7274731473578,25.7400967175578));
#39518=CARTESIAN_POINT('Ctrl Pts',(127.037677051997,37.8153361332125,25.7342912962484));
#39519=CARTESIAN_POINT('Ctrl Pts',(127.12240450845,37.8994256650257,25.7284858749389));
#39520=CARTESIAN_POINT('Ctrl Pts',(127.207225792718,37.9836083182119,25.7226740246626));
#39521=CARTESIAN_POINT('Ctrl Pts',(127.295686867834,38.0640088883964,25.7168621743864));
#39522=CARTESIAN_POINT('Ctrl Pts',(127.387405936573,38.1403148344941,25.7110503241102));
#39523=CARTESIAN_POINT('Ctrl Pts',(127.479185246888,38.2166708987469,25.7052346565794));
#39524=CARTESIAN_POINT('Ctrl Pts',(127.574226488114,38.2889267363997,25.6994189890488));
#39525=CARTESIAN_POINT('Ctrl Pts',(127.672117926347,38.3568124837658,25.6936033215181));
#39526=CARTESIAN_POINT('Ctrl Pts',(127.770149583495,38.4247954701341,25.6877793236716));
#39527=CARTESIAN_POINT('Ctrl Pts',(127.871039242095,38.4883956552465,25.6819553258252));
#39528=CARTESIAN_POINT('Ctrl Pts',(127.97434947477,38.5473884689492,25.6761313279788));
#39529=CARTESIAN_POINT('Ctrl Pts',(128.001758241705,38.5630395834591,25.6745861896563));
#39530=CARTESIAN_POINT('Ctrl Pts',(128.029337272291,38.5783666599941,25.6730410513339));
#39531=CARTESIAN_POINT('Ctrl Pts',(128.057078167552,38.5933660755618,25.6714959130115));
#39532=CARTESIAN_POINT('Ctrl Pts',(128.161633015309,38.6498985557273,25.6656723193407));
#39533=CARTESIAN_POINT('Ctrl Pts',(128.268825870595,38.7019551203421,25.6598487256699));
#39534=CARTESIAN_POINT('Ctrl Pts',(128.378237088824,38.7492812724484,25.6540251319991));
#39535=CARTESIAN_POINT('Ctrl Pts',(128.487510268548,38.7965477155841,25.6482088856567));
#39536=CARTESIAN_POINT('Ctrl Pts',(128.598995873004,38.8390954559754,25.6423926393143));
#39537=CARTESIAN_POINT('Ctrl Pts',(128.712248810399,38.8767153459701,25.636576392972));
#39538=CARTESIAN_POINT('Ctrl Pts',(128.825388380978,38.9142975782473,25.6307659687243));
#39539=CARTESIAN_POINT('Ctrl Pts',(128.940291379782,38.9469616453496,25.6249555444766));
#39540=CARTESIAN_POINT('Ctrl Pts',(129.056492394029,38.9745463134143,25.6191451202289));
#39541=CARTESIAN_POINT('Ctrl Pts',(129.177091857028,39.0031751182245,25.6131147594045));
#39542=CARTESIAN_POINT('Ctrl Pts',(129.299089130788,39.0263322167952,25.6070843985801));
#39543=CARTESIAN_POINT('Ctrl Pts',(129.42194576277,39.0438939524696,25.6010540377557));
#39544=CARTESIAN_POINT('Ctrl Pts',(129.540188383733,39.0607961385487,25.5952501535231));
#39545=CARTESIAN_POINT('Ctrl Pts',(129.65922653817,39.0725155991235,25.5894462692905));
#39546=CARTESIAN_POINT('Ctrl Pts',(129.778570096612,39.0789942140049,25.5836423850578));
#39547=CARTESIAN_POINT('Ctrl Pts',(129.897896026733,39.0854718719255,25.577839358121));
#39548=CARTESIAN_POINT('Ctrl Pts',(130.017526863521,39.0867102015225,25.5720363311842));
#39549=CARTESIAN_POINT('Ctrl Pts',(130.13696892154,39.0827030891962,25.5662333042473));
#39550=CARTESIAN_POINT('Ctrl Pts',(130.256421525044,39.0786956230838,25.5604297649639));
#39551=CARTESIAN_POINT('Ctrl Pts',(130.375684908514,39.0694418079503,25.5546262256805));
#39552=CARTESIAN_POINT('Ctrl Pts',(130.494267601246,39.0549876126023,25.548822686397));
#39553=CARTESIAN_POINT('Ctrl Pts',(130.612888748963,39.0405287299273,25.5430172650935));
#39554=CARTESIAN_POINT('Ctrl Pts',(130.730828361813,39.0208661625053,25.5372118437899));
#39555=CARTESIAN_POINT('Ctrl Pts',(130.84760292535,38.9960973813133,25.5314064224864));
#39556=CARTESIAN_POINT('Ctrl Pts',(130.964506805907,38.9713011709886,25.5255945722161));
#39557=CARTESIAN_POINT('Ctrl Pts',(131.080242662145,38.9413875444868,25.5197827219458));
#39558=CARTESIAN_POINT('Ctrl Pts',(131.194339806388,38.9065045023494,25.5139708716754));
#39559=CARTESIAN_POINT('Ctrl Pts',(131.308511890249,38.8715985488427,25.5081552041507));
#39560=CARTESIAN_POINT('Ctrl Pts',(131.421042734611,38.8317168155747,25.5023395366259));
#39561=CARTESIAN_POINT('Ctrl Pts',(131.531480935746,38.7870557354556,25.4965238691011));
#39562=CARTESIAN_POINT('Ctrl Pts',(131.642077327679,38.7423306831618,25.4906998712606));
#39563=CARTESIAN_POINT('Ctrl Pts',(131.750574723409,38.6928127889152,25.48487587342));
#39564=CARTESIAN_POINT('Ctrl Pts',(131.856545517186,38.6387448031729,25.4790518755795));
#39565=CARTESIAN_POINT('Ctrl Pts',(131.884660146514,38.6244002717834,25.4775067372007));
#39566=CARTESIAN_POINT('Ctrl Pts',(131.91259709215,38.6097357109502,25.4759615988218));
#39567=CARTESIAN_POINT('Ctrl Pts',(131.940348719912,38.594756159343,25.474416460443));
#39568=CARTESIAN_POINT('Ctrl Pts',(132.044926391121,38.5383080606497,25.4685938479917));
#39569=CARTESIAN_POINT('Ctrl Pts',(132.147207370059,38.4772016462083,25.4627712355404));
#39570=CARTESIAN_POINT('Ctrl Pts',(132.246748991069,38.4116482777579,25.456948623089));
#39571=CARTESIAN_POINT('Ctrl Pts',(132.3288274834,38.3575952937399,25.4521475032501));
#39572=CARTESIAN_POINT('Ctrl Pts',(132.409043673025,38.3005197331551,25.4473463834112));
#39573=CARTESIAN_POINT('Ctrl Pts',(132.487160689988,38.2405642567579,25.4425452635723));
#39574=CARTESIAN_POINT('',(125.915000988625,34.9971579821973,25.9896150286367));
#39575=CARTESIAN_POINT('Ctrl Pts',(125.915000988624,34.997157983046,25.9896150285955));
#39576=CARTESIAN_POINT('Ctrl Pts',(125.914917631215,35.1169725160829,25.98379925565));
#39577=CARTESIAN_POINT('Ctrl Pts',(125.920109897601,35.2368329689649,25.9779834827046));
#39578=CARTESIAN_POINT('Ctrl Pts',(125.930563220773,35.3562433155562,25.9721677097591));
#39579=CARTESIAN_POINT('Ctrl Pts',(125.94101582311,35.4756454279067,25.9663523378549));
#39580=CARTESIAN_POINT('Ctrl Pts',(125.956728725647,35.594597091786,25.9605369659506));
#39581=CARTESIAN_POINT('Ctrl Pts',(125.977635392703,35.7126064593879,25.9547215940464));
#39582=CARTESIAN_POINT('Ctrl Pts',(125.998545461783,35.8306350299897,25.9489052758395));
#39583=CARTESIAN_POINT('Ctrl Pts',(126.024650905994,35.9477206000163,25.9430889576325));
#39584=CARTESIAN_POINT('Ctrl Pts',(126.055833996177,36.0633811801447,25.9372726394256));
#39585=CARTESIAN_POINT('Ctrl Pts',(126.087029385138,36.1790873774281,25.9314540272315));
#39586=CARTESIAN_POINT('Ctrl Pts',(126.123306298704,36.2933670755061,25.9256354150373));
#39587=CARTESIAN_POINT('Ctrl Pts',(126.164497225096,36.4057536995169,25.9198168028432));
#39588=CARTESIAN_POINT('Ctrl Pts',(126.205738353568,36.5182772964668,25.9139910991253));
#39589=CARTESIAN_POINT('Ctrl Pts',(126.251905311341,36.6289028324717,25.9081653954074));
#39590=CARTESIAN_POINT('Ctrl Pts',(126.302782435844,36.7371837218019,25.9023396916895));
#39591=CARTESIAN_POINT('Ctrl Pts',(126.353695625473,36.8455413679057,25.8965098583212));
#39592=CARTESIAN_POINT('Ctrl Pts',(126.40932544393,36.9515506989297,25.8906800249529));
#39593=CARTESIAN_POINT('Ctrl Pts',(126.469411107916,37.0547912485437,25.8848501915846));
#39594=CARTESIAN_POINT('Ctrl Pts',(126.529589512789,37.1581911476518,25.879011359998));
#39595=CARTESIAN_POINT('Ctrl Pts',(126.594237274574,37.2588133939343,25.8731725284114));
#39596=CARTESIAN_POINT('Ctrl Pts',(126.663051158455,37.3562676904181,25.8673336968249));
#39597=CARTESIAN_POINT('Ctrl Pts',(126.686630918671,37.3896613722392,25.8653329632375));
#39598=CARTESIAN_POINT('Ctrl Pts',(126.710699509632,37.422683385099,25.8633322296501));
#39599=CARTESIAN_POINT('Ctrl Pts',(126.735243706803,37.4553189906879,25.8613314960627));
#39600=CARTESIAN_POINT('Ctrl Pts',(126.80668521814,37.5503124007564,25.8555079023934));
#39601=CARTESIAN_POINT('Ctrl Pts',(126.882391357813,37.6423383457659,25.849684308724));
#39602=CARTESIAN_POINT('Ctrl Pts',(126.962086897633,37.7309904764516,25.8438607150547));
#39603=CARTESIAN_POINT('Ctrl Pts',(127.041681889693,37.8195307593073,25.8380444687137));
#39604=CARTESIAN_POINT('Ctrl Pts',(127.125256000358,37.9047053930594,25.8322282223727));
#39605=CARTESIAN_POINT('Ctrl Pts',(127.212491956809,37.9861386285879,25.8264119760317));
#39606=CARTESIAN_POINT('Ctrl Pts',(127.299640589587,38.067490348999,25.8206015517854));
#39607=CARTESIAN_POINT('Ctrl Pts',(127.390443479258,38.1451078446809,25.814791127539));
#39608=CARTESIAN_POINT('Ctrl Pts',(127.484544897527,38.2186504357325,25.8089807032926));
#39609=CARTESIAN_POINT('Ctrl Pts',(127.582208249157,38.2949767660032,25.8029503424677));
#39610=CARTESIAN_POINT('Ctrl Pts',(127.683424475913,38.3669132759528,25.7969199816428));
#39611=CARTESIAN_POINT('Ctrl Pts',(127.787755792911,38.4341229692894,25.7908896208178));
#39612=CARTESIAN_POINT('Ctrl Pts',(127.888168836699,38.4988085313446,25.7850857365864));
#39613=CARTESIAN_POINT('Ctrl Pts',(127.9914668351,38.5591156742766,25.7792818523549));
#39614=CARTESIAN_POINT('Ctrl Pts',(128.097228583066,38.6147871216571,25.7734779681235));
#39615=CARTESIAN_POINT('Ctrl Pts',(128.202974708892,38.6704503457703,25.7676749411877));
#39616=CARTESIAN_POINT('Ctrl Pts',(128.311183499321,38.7214790459172,25.761871914252));
#39617=CARTESIAN_POINT('Ctrl Pts',(128.421408823275,38.7676617280172,25.7560688873162));
#39618=CARTESIAN_POINT('Ctrl Pts',(128.531643878974,38.8138484875657,25.7502653480338));
#39619=CARTESIAN_POINT('Ctrl Pts',(128.643895445548,38.8551882205887,25.7444618087514));
#39620=CARTESIAN_POINT('Ctrl Pts',(128.757697678908,38.8915176914681,25.738658269469));
#39621=CARTESIAN_POINT('Ctrl Pts',(128.871536817006,38.9278589435716,25.7328528481664));
#39622=CARTESIAN_POINT('Ctrl Pts',(128.986927233176,38.9591865781146,25.7270474268638));
#39623=CARTESIAN_POINT('Ctrl Pts',(129.103388830487,38.9853874856412,25.7212420055612));
#39624=CARTESIAN_POINT('Ctrl Pts',(129.219979398241,39.0116174082482,25.7154301552917));
#39625=CARTESIAN_POINT('Ctrl Pts',(129.337643116344,39.0327091816321,25.7096183050222));
#39626=CARTESIAN_POINT('Ctrl Pts',(129.455890467265,39.0486009702596,25.7038064547528));
#39627=CARTESIAN_POINT('Ctrl Pts',(129.574215483682,39.0645031966995,25.6979907872288));
#39628=CARTESIAN_POINT('Ctrl Pts',(129.693124490574,39.0751986000751,25.6921751197048));
#39629=CARTESIAN_POINT('Ctrl Pts',(129.812125293181,39.0806774063307,25.6863594521808));
#39630=CARTESIAN_POINT('Ctrl Pts',(129.931296551591,39.0861640603848,25.6805354543409));
#39631=CARTESIAN_POINT('Ctrl Pts',(130.05055946127,39.0864192023192,25.6747114565011));
#39632=CARTESIAN_POINT('Ctrl Pts',(130.16942413495,39.0814850805187,25.6688874586612));
#39633=CARTESIAN_POINT('Ctrl Pts',(130.200959581124,39.080176031096,25.6673423202722));
#39634=CARTESIAN_POINT('Ctrl Pts',(130.23246703944,39.0785020063004,25.6657971818833));
#39635=CARTESIAN_POINT('Ctrl Pts',(130.263937469796,39.0764644009285,25.6642520434943));
#39636=CARTESIAN_POINT('Ctrl Pts',(130.382535283496,39.0687855881652,25.6584291159804));
#39637=CARTESIAN_POINT('Ctrl Pts',(130.500988941927,39.0559144961333,25.6526061884665));
#39638=CARTESIAN_POINT('Ctrl Pts',(130.618807884703,39.037858566348,25.6467832609526));
#39639=CARTESIAN_POINT('Ctrl Pts',(130.736486110335,39.0198242016761,25.6409672880565));
#39640=CARTESIAN_POINT('Ctrl Pts',(130.853530727797,38.9966173737414,25.6351513151605));
#39641=CARTESIAN_POINT('Ctrl Pts',(130.969453622282,38.9682974528435,25.6293353422645));
#39642=CARTESIAN_POINT('Ctrl Pts',(131.085265436093,38.9400046689139,25.6235249424021));
#39643=CARTESIAN_POINT('Ctrl Pts',(131.199957270419,38.906608633073,25.6177145425397));
#39644=CARTESIAN_POINT('Ctrl Pts',(131.313049197558,38.8682201081106,25.6119041426773));
#39645=CARTESIAN_POINT('Ctrl Pts',(131.426056890354,38.8298601761014,25.6060980705793));
#39646=CARTESIAN_POINT('Ctrl Pts',(131.537466661937,38.7865152853884,25.6002919984813));
#39647=CARTESIAN_POINT('Ctrl Pts',(131.646812448058,38.738346393918,25.5944859263833));
#39648=CARTESIAN_POINT('Ctrl Pts',(131.756109391884,38.6901990184048,25.5886824477267));
#39649=CARTESIAN_POINT('Ctrl Pts',(131.863343811702,38.6372320940027,25.5828789690701));
#39650=CARTESIAN_POINT('Ctrl Pts',(131.968068894652,38.5796549869927,25.5770754904136));
#39651=CARTESIAN_POINT('Ctrl Pts',(132.072791333086,38.5220793339191,25.5712721583064));
#39652=CARTESIAN_POINT('Ctrl Pts',(132.175004198713,38.4598939186473,25.5654688261992));
#39653=CARTESIAN_POINT('Ctrl Pts',(132.274284934972,38.3933542453682,25.559665494092));
#39654=CARTESIAN_POINT('Ctrl Pts',(132.346861709583,38.3447120308537,25.5554231088901));
#39655=CARTESIAN_POINT('Ctrl Pts',(132.417872043576,38.2937438835033,25.5511807236882));
#39656=CARTESIAN_POINT('Ctrl Pts',(132.487160689988,38.2405642567579,25.5469383384863));
#39657=CARTESIAN_POINT('Ctrl Pts',(132.487160689988,38.2405642567579,26.7967734493137));
#39658=CARTESIAN_POINT('Ctrl Pts',(132.581820861397,38.1679117683082,26.7909668267509));
#39659=CARTESIAN_POINT('Ctrl Pts',(132.673369460366,38.0910510166544,26.7851602041881));
#39660=CARTESIAN_POINT('Ctrl Pts',(132.761416222849,38.0102832830462,26.7793535816253));
#39661=CARTESIAN_POINT('Ctrl Pts',(132.849425891177,37.9295495769333,26.7735494053961));
#39662=CARTESIAN_POINT('Ctrl Pts',(132.933936355778,37.8449124368826,26.7677452291669));
#39663=CARTESIAN_POINT('Ctrl Pts',(133.014590961074,37.7567129588351,26.7619410529378));
#39664=CARTESIAN_POINT('Ctrl Pts',(133.09523030081,37.6685301743726,26.7561379752696));
#39665=CARTESIAN_POINT('Ctrl Pts',(133.17201495707,37.5767866939246,26.7503348976015));
#39666=CARTESIAN_POINT('Ctrl Pts',(133.244626098886,37.4818594799925,26.7445318199333));
#39667=CARTESIAN_POINT('Ctrl Pts',(133.317240633817,37.386927830117,26.7387284710877));
#39668=CARTESIAN_POINT('Ctrl Pts',(133.385681018521,37.2888124753689,26.732925122242));
#39669=CARTESIAN_POINT('Ctrl Pts',(133.449669983221,37.1879218466071,26.7271217733964));
#39670=CARTESIAN_POINT('Ctrl Pts',(133.513677039465,37.0870026931285,26.7213167837751));
#39671=CARTESIAN_POINT('Ctrl Pts',(133.573229954184,36.9833070498957,26.7155117941538));
#39672=CARTESIAN_POINT('Ctrl Pts',(133.628096231385,36.8772700220825,26.7097068045326));
#39673=CARTESIAN_POINT('Ctrl Pts',(133.683022200258,36.7711176314681,26.7038954993829));
#39674=CARTESIAN_POINT('Ctrl Pts',(133.733251164245,36.6626191337229,26.6980841942332));
#39675=CARTESIAN_POINT('Ctrl Pts',(133.778597745551,36.5522319663369,26.6922728890835));
#39676=CARTESIAN_POINT('Ctrl Pts',(133.823972420527,36.4417764105393,26.6864579836428));
#39677=CARTESIAN_POINT('Ctrl Pts',(133.864458550049,36.3294302381281,26.6806430782021));
#39678=CARTESIAN_POINT('Ctrl Pts',(133.89992038785,36.2156668821802,26.6748281727614));
#39679=CARTESIAN_POINT('Ctrl Pts',(133.935434699861,36.1017351863354,26.6690046627874));
#39680=CARTESIAN_POINT('Ctrl Pts',(133.965909772143,35.9863825138731,26.6631811528134));
#39681=CARTESIAN_POINT('Ctrl Pts',(133.991260721223,35.8700935899234,26.6573576428394));
#39682=CARTESIAN_POINT('Ctrl Pts',(134.002446051436,35.8187846621822,26.6547881973384));
#39683=CARTESIAN_POINT('Ctrl Pts',(134.012634523012,35.7672935534363,26.6522187518375));
#39684=CARTESIAN_POINT('Ctrl Pts',(134.021822060171,35.7156621523631,26.6496493063365));
#39685=CARTESIAN_POINT('Ctrl Pts',(134.042645419236,35.5986406715131,26.6438257123367));
#39686=CARTESIAN_POINT('Ctrl Pts',(134.058390721623,35.4805208961929,26.638002118337));
#39687=CARTESIAN_POINT('Ctrl Pts',(134.068948190853,35.3617811771706,26.6321785243373));
#39688=CARTESIAN_POINT('Ctrl Pts',(134.079492340275,35.2431912658604,26.6263622776624));
#39689=CARTESIAN_POINT('Ctrl Pts',(134.084861638982,35.1239833696746,26.6205460309876));
#39690=CARTESIAN_POINT('Ctrl Pts',(134.08499735826,35.004645751279,26.6147297843128));
#39691=CARTESIAN_POINT('Ctrl Pts',(134.085132941683,34.885427590427,26.6089193597295));
#39692=CARTESIAN_POINT('Ctrl Pts',(134.080045367236,34.7660803716804,26.6031089351462));
#39693=CARTESIAN_POINT('Ctrl Pts',(134.069727778162,34.6470965972725,26.5972985105629));
#39694=CARTESIAN_POINT('Ctrl Pts',(134.059019647839,34.5236090505677,26.5912681498631));
#39695=CARTESIAN_POINT('Ctrl Pts',(134.042677707309,34.4005134524778,26.5852377891634));
#39696=CARTESIAN_POINT('Ctrl Pts',(134.020753720616,34.2783598416417,26.5792074284636));
#39697=CARTESIAN_POINT('Ctrl Pts',(133.999653110801,34.1607938297783,26.5734035438897));
#39698=CARTESIAN_POINT('Ctrl Pts',(133.973382250782,34.0441007646693,26.5675996593159));
#39699=CARTESIAN_POINT('Ctrl Pts',(133.94203994183,33.9287642196906,26.561795774742));
#39700=CARTESIAN_POINT('Ctrl Pts',(133.910702262464,33.8134447111223,26.5559927474624));
#39701=CARTESIAN_POINT('Ctrl Pts',(133.874294730951,33.6994817181475,26.5501897201829));
#39702=CARTESIAN_POINT('Ctrl Pts',(133.832966639211,33.5873458517037,26.5443866929033));
#39703=CARTESIAN_POINT('Ctrl Pts',(133.791634898624,33.4752000848145,26.538583153276));
#39704=CARTESIAN_POINT('Ctrl Pts',(133.745381875263,33.3648821483549,26.5327796136487));
#39705=CARTESIAN_POINT('Ctrl Pts',(133.694405610753,33.2568441884794,26.5269760740214));
#39706=CARTESIAN_POINT('Ctrl Pts',(133.643412815229,33.1487711931414,26.5211706523733));
#39707=CARTESIAN_POINT('Ctrl Pts',(133.587693906521,33.0429800139307,26.5153652307251));
#39708=CARTESIAN_POINT('Ctrl Pts',(133.527493321346,32.9398990636727,26.509559809077));
#39709=CARTESIAN_POINT('Ctrl Pts',(133.467226069606,32.8367039608211,26.5037479584627));
#39710=CARTESIAN_POINT('Ctrl Pts',(133.402467440795,32.7362254306461,26.4979361078484));
#39711=CARTESIAN_POINT('Ctrl Pts',(133.333505813242,32.6388638342777,26.4921242572341));
#39712=CARTESIAN_POINT('Ctrl Pts',(133.264498891324,32.5414382902933,26.4863085893653));
#39713=CARTESIAN_POINT('Ctrl Pts',(133.191283722793,32.447134079003,26.4804929214966));
#39714=CARTESIAN_POINT('Ctrl Pts',(133.114188607991,32.3563180384441,26.4746772536278));
#39715=CARTESIAN_POINT('Ctrl Pts',(133.036983062804,32.2653719137611,26.4688532554458));
#39716=CARTESIAN_POINT('Ctrl Pts',(132.955886755349,32.1779242307475,26.4630292572638));
#39717=CARTESIAN_POINT('Ctrl Pts',(132.871264482113,32.0943046832542,26.4572052590819));
#39718=CARTESIAN_POINT('Ctrl Pts',(132.848813780563,32.0721200097315,26.4556601239772));
#39719=CARTESIAN_POINT('Ctrl Pts',(132.82611507466,32.0502045629611,26.4541149888726));
#39720=CARTESIAN_POINT('Ctrl Pts',(132.803175546272,32.0285640076244,26.452569853768));
#39721=CARTESIAN_POINT('Ctrl Pts',(132.716716768458,31.9470010419913,26.4467462600813));
#39722=CARTESIAN_POINT('Ctrl Pts',(132.626555803418,31.8690831708606,26.4409226663946));
#39723=CARTESIAN_POINT('Ctrl Pts',(132.5330325544,31.7951644225721,26.4350990727078));
#39724=CARTESIAN_POINT('Ctrl Pts',(132.439627298836,31.7213389337506,26.4292828263485));
#39725=CARTESIAN_POINT('Ctrl Pts',(132.342868514105,31.6515027833869,26.4234665799891));
#39726=CARTESIAN_POINT('Ctrl Pts',(132.24313237601,31.5859727382908,26.4176503336298));
#39727=CARTESIAN_POINT('Ctrl Pts',(132.143496074322,31.5205082891196,26.4118399093641));
#39728=CARTESIAN_POINT('Ctrl Pts',(132.040888687605,31.4593415930756,26.4060294850984));
#39729=CARTESIAN_POINT('Ctrl Pts',(131.935718371835,31.4027483567394,26.4002190608327));
#39730=CARTESIAN_POINT('Ctrl Pts',(131.82656714252,31.344012949588,26.3941887000147));
#39731=CARTESIAN_POINT('Ctrl Pts',(131.714655477875,31.2902043508118,26.3881583391966));
#39732=CARTESIAN_POINT('Ctrl Pts',(131.60047178956,31.2415807776645,26.3821279783786));
#39733=CARTESIAN_POINT('Ctrl Pts',(131.49057639017,31.194783314124,26.3763240941255));
#39734=CARTESIAN_POINT('Ctrl Pts',(131.378576955507,31.1527886157344,26.3705202098724));
#39735=CARTESIAN_POINT('Ctrl Pts',(131.264932091598,31.1157791252756,26.3647163256193));
#39736=CARTESIAN_POINT('Ctrl Pts',(131.151304014234,31.0787751015087,26.3589132986611));
#39737=CARTESIAN_POINT('Ctrl Pts',(131.036031379132,31.0467549476782,26.3531102717029));
#39738=CARTESIAN_POINT('Ctrl Pts',(130.919589628044,31.0198517721077,26.3473072447447));
#39739=CARTESIAN_POINT('Ctrl Pts',(130.803137596349,30.9929462212639,26.341503705439));
#39740=CARTESIAN_POINT('Ctrl Pts',(130.685516641316,30.9711586388476,26.3357001661333));
#39741=CARTESIAN_POINT('Ctrl Pts',(130.567213484101,30.9545712386134,26.3298966268277));
#39742=CARTESIAN_POINT('Ctrl Pts',(130.448871962534,30.9379784592763,26.324091205501));
#39743=CARTESIAN_POINT('Ctrl Pts',(130.329848202982,30.9265892725787,26.3182857841744));
#39744=CARTESIAN_POINT('Ctrl Pts',(130.210634508829,30.9204340790116,26.3124803628477));
#39745=CARTESIAN_POINT('Ctrl Pts',(130.091288796521,30.9142720691361,26.3066685125532));
#39746=CARTESIAN_POINT('Ctrl Pts',(129.971753137802,30.9133556430981,26.3008566622587));
#39747=CARTESIAN_POINT('Ctrl Pts',(129.852520461619,30.9176630729741,26.2950448119641));
#39748=CARTESIAN_POINT('Ctrl Pts',(129.733209472761,30.9219733319937,26.2892291444144));
#39749=CARTESIAN_POINT('Ctrl Pts',(129.61420226885,30.9315142474071,26.2834134768647));
#39750=CARTESIAN_POINT('Ctrl Pts',(129.49598562488,30.9462123255316,26.277597809315));
#39751=CARTESIAN_POINT('Ctrl Pts',(129.377599648315,30.960931457068,26.2717738114487));
#39752=CARTESIAN_POINT('Ctrl Pts',(129.260006893072,30.9808224276629,26.2659498135824));
#39753=CARTESIAN_POINT('Ctrl Pts',(129.143683073674,31.005760858225,26.2601258157161));
#39754=CARTESIAN_POINT('Ctrl Pts',(129.112821734468,31.0123771589003,26.2585806775439));
#39755=CARTESIAN_POINT('Ctrl Pts',(129.082049622144,31.0193484649703,26.2570355393718));
#39756=CARTESIAN_POINT('Ctrl Pts',(129.051375411368,31.0266718748834,26.2554904011996));
#39757=CARTESIAN_POINT('Ctrl Pts',(128.935764949877,31.0542736543036,26.2496668076129));
#39758=CARTESIAN_POINT('Ctrl Pts',(128.82117373592,31.086969944146,26.2438432140263));
#39759=CARTESIAN_POINT('Ctrl Pts',(128.708084191153,31.1246705246067,26.2380196204396));
#39760=CARTESIAN_POINT('Ctrl Pts',(128.595137325676,31.1623235401752,26.2322033741828));
#39761=CARTESIAN_POINT('Ctrl Pts',(128.483688745079,31.2049681606443,26.226387127926));
#39762=CARTESIAN_POINT('Ctrl Pts',(128.374209589848,31.2524634034799,26.2205708816692));
#39763=CARTESIAN_POINT('Ctrl Pts',(128.26484002388,31.2999111033045,26.2147604575083));
#39764=CARTESIAN_POINT('Ctrl Pts',(128.157436333859,31.352199604498,26.2089500333474));
#39765=CARTESIAN_POINT('Ctrl Pts',(128.052452849047,31.4091386695092,26.2031396091865));
#39766=CARTESIAN_POINT('Ctrl Pts',(127.943495519968,31.4682329971073,26.1971092483301));
#39767=CARTESIAN_POINT('Ctrl Pts',(127.837145661094,31.5323367701793,26.1910788874736));
#39768=CARTESIAN_POINT('Ctrl Pts',(127.733886967399,31.6011830406042,26.1850485266171));
#39769=CARTESIAN_POINT('Ctrl Pts',(127.634506265441,31.6674437150053,26.179244642474));
#39770=CARTESIAN_POINT('Ctrl Pts',(127.537989102006,31.738096844609,26.1734407583309));
#39771=CARTESIAN_POINT('Ctrl Pts',(127.444739458086,31.8128588730749,26.1676368741878));
#39772=CARTESIAN_POINT('Ctrl Pts',(127.351503588149,31.8876098583789,26.1618338473412));
#39773=CARTESIAN_POINT('Ctrl Pts',(127.261534596394,31.9664682802003,26.1560308204947));
#39774=CARTESIAN_POINT('Ctrl Pts',(127.175204430632,32.04910945793,26.1502277936482));
#39775=CARTESIAN_POINT('Ctrl Pts',(127.088866642829,32.1317579320015,26.1444242544558));
#39776=CARTESIAN_POINT('Ctrl Pts',(127.006168614767,32.2181895436282,26.1386207152633));
#39777=CARTESIAN_POINT('Ctrl Pts',(126.927445910466,32.3080422798845,26.1328171760709));
#39778=CARTESIAN_POINT('Ctrl Pts',(126.848697677319,32.397924154326,26.127011754859));
#39779=CARTESIAN_POINT('Ctrl Pts',(126.773927600712,32.4912290528291,26.1212063336472));
#39780=CARTESIAN_POINT('Ctrl Pts',(126.703430969524,32.5875618915072,26.1154009124353));
#39781=CARTESIAN_POINT('Ctrl Pts',(126.632856269847,32.6840014098815,26.1095890622571));
#39782=CARTESIAN_POINT('Ctrl Pts',(126.566564703245,32.7834752319111,26.1037772120789));
#39783=CARTESIAN_POINT('Ctrl Pts',(126.504808302805,32.8855591756076,26.0979653619008));
#39784=CARTESIAN_POINT('Ctrl Pts',(126.443011340433,32.9877101685807,26.0921496944685));
#39785=CARTESIAN_POINT('Ctrl Pts',(126.385755671798,33.0924743398825,26.0863340270363));
#39786=CARTESIAN_POINT('Ctrl Pts',(126.333246661229,33.19940427841,26.080518359604));
#39787=CARTESIAN_POINT('Ctrl Pts',(126.280662437169,33.306487382533,26.0746943618559));
#39788=CARTESIAN_POINT('Ctrl Pts',(126.232838604917,33.415742073018,26.0688703641078));
#39789=CARTESIAN_POINT('Ctrl Pts',(126.189931906767,33.5267022958927,26.0630463663596));
#39790=CARTESIAN_POINT('Ctrl Pts',(126.17854851928,33.5561406648911,26.0615012271168));
#39791=CARTESIAN_POINT('Ctrl Pts',(126.167510959468,33.5856990082987,26.059956087874));
#39792=CARTESIAN_POINT('Ctrl Pts',(126.156821555699,33.6153684803317,26.0584109486312));
#39793=CARTESIAN_POINT('Ctrl Pts',(126.110323273242,33.7444289518687,26.0516896831146));
#39794=CARTESIAN_POINT('Ctrl Pts',(126.070293444538,33.8759349209088,26.0449684175981));
#39795=CARTESIAN_POINT('Ctrl Pts',(126.036959458656,34.0092756853371,26.0382471520816));
#39796=CARTESIAN_POINT('Ctrl Pts',(126.003758284162,34.1420851850052,26.0315526658589));
#39797=CARTESIAN_POINT('Ctrl Pts',(125.977199802163,34.2767147548031,26.0248581796363));
#39798=CARTESIAN_POINT('Ctrl Pts',(125.957461778025,34.4125395980401,26.0181636934136));
#39799=CARTESIAN_POINT('Ctrl Pts',(125.937867450412,34.5473756108934,26.0115179443087));
#39800=CARTESIAN_POINT('Ctrl Pts',(125.924994719636,34.6833894081815,26.0048721952038));
#39801=CARTESIAN_POINT('Ctrl Pts',(125.918969827263,34.8199507589276,25.9982264460989));
#39802=CARTESIAN_POINT('Ctrl Pts',(125.916367519002,34.8789351704621,25.9953559736115));
#39803=CARTESIAN_POINT('Ctrl Pts',(125.915042131088,34.9380215056026,25.9924855011241));
#39804=CARTESIAN_POINT('Ctrl Pts',(125.915000988625,34.9971579821973,25.9896150286367));
#39805=CARTESIAN_POINT('Origin',(130.,35.,32.7603849714045));
#39806=CARTESIAN_POINT('',(132.487160689988,38.2405642567579,28.0469635225512));
#39807=CARTESIAN_POINT('',(132.487160689988,38.2405642567579,27.9426397356904));
#39808=CARTESIAN_POINT('',(132.487160689988,38.2405642567579,32.7603849714045));
#39809=CARTESIAN_POINT('',(125.915000279441,35.001510971197,27.1353849713731));
#39810=CARTESIAN_POINT('Ctrl Pts',(132.487160689988,38.2405642567579,27.9426397356904));
#39811=CARTESIAN_POINT('Ctrl Pts',(132.581967895796,38.1677989181535,27.9368366805219));
#39812=CARTESIAN_POINT('Ctrl Pts',(132.67358627189,38.0908641165998,27.9310336253533));
#39813=CARTESIAN_POINT('Ctrl Pts',(132.761639023741,38.010078886433,27.9252305701847));
#39814=CARTESIAN_POINT('Ctrl Pts',(132.849706660417,37.9292799999757,27.9194265340421));
#39815=CARTESIAN_POINT('Ctrl Pts',(132.934207173398,37.8446296666309,27.9136224978996));
#39816=CARTESIAN_POINT('Ctrl Pts',(133.014799649079,37.7564847316669,27.907818461757));
#39817=CARTESIAN_POINT('Ctrl Pts',(133.095475204053,37.6682489319074,27.902008442485));
#39818=CARTESIAN_POINT('Ctrl Pts',(133.172234398533,37.5765116365957,27.896198423213));
#39819=CARTESIAN_POINT('Ctrl Pts',(133.244775590758,37.4816640315769,27.8903884039409));
#39820=CARTESIAN_POINT('Ctrl Pts',(133.317354327839,37.38676733666,27.8845753776003));
#39821=CARTESIAN_POINT('Ctrl Pts',(133.385710479367,37.288757459556,27.8787623512597));
#39822=CARTESIAN_POINT('Ctrl Pts',(133.4495858686,37.1880544634797,27.8729493249191));
#39823=CARTESIAN_POINT('Ctrl Pts',(133.51356454696,37.087188626525,27.8671268986763));
#39824=CARTESIAN_POINT('Ctrl Pts',(133.573047781196,36.9836213230422,27.8613044724335));
#39825=CARTESIAN_POINT('Ctrl Pts',(133.627823186965,36.877797625975,27.8554820461907));
#39826=CARTESIAN_POINT('Ctrl Pts',(133.678349078126,36.7801838059562,27.8501113278819));
#39827=CARTESIAN_POINT('Ctrl Pts',(133.724869709531,36.6806505966967,27.8447406095731));
#39828=CARTESIAN_POINT('Ctrl Pts',(133.767255489852,36.5795604053595,27.8393698912644));
#39829=CARTESIAN_POINT('Ctrl Pts',(133.813215309703,36.4699461208672,27.8335463050505));
#39830=CARTESIAN_POINT('Ctrl Pts',(133.854461171629,36.3581474944634,27.8277227188367));
#39831=CARTESIAN_POINT('Ctrl Pts',(133.890781146696,36.2446071944646,27.8218991326229));
#39832=CARTESIAN_POINT('Ctrl Pts',(133.927055297973,36.1312101447551,27.8160828938479));
#39833=CARTESIAN_POINT('Ctrl Pts',(133.958415800245,36.0160761775544,27.8102666550729));
#39834=CARTESIAN_POINT('Ctrl Pts',(133.984698359649,35.8996688182933,27.8044504162979));
#39835=CARTESIAN_POINT('Ctrl Pts',(134.010954609579,35.7833779856037,27.7986399997181));
#39836=CARTESIAN_POINT('Ctrl Pts',(134.03214293951,35.6658166927262,27.7928295831383));
#39837=CARTESIAN_POINT('Ctrl Pts',(134.048148737804,35.5474639683296,27.7870191665584));
#39838=CARTESIAN_POINT('Ctrl Pts',(134.064760418407,35.4246311286238,27.7809888028975));
#39839=CARTESIAN_POINT('Ctrl Pts',(134.075789319717,35.3009461827978,27.7749584392366));
#39840=CARTESIAN_POINT('Ctrl Pts',(134.081165417923,35.1769571460836,27.7689280755756));
#39841=CARTESIAN_POINT('Ctrl Pts',(134.086339601614,35.0576248669875,27.7631241992128));
#39842=CARTESIAN_POINT('Ctrl Pts',(134.086277919083,34.9380113716758,27.7573203228499));
#39843=CARTESIAN_POINT('Ctrl Pts',(134.080970805455,34.818610129774,27.7515164464871));
#39844=CARTESIAN_POINT('Ctrl Pts',(134.075664475803,34.699226525991,27.745713427481));
#39845=CARTESIAN_POINT('Ctrl Pts',(134.065114274137,34.5800555210893,27.7399104084748));
#39846=CARTESIAN_POINT('Ctrl Pts',(134.049362739548,34.4615890012616,27.7341073894687));
#39847=CARTESIAN_POINT('Ctrl Pts',(134.033609814403,34.343112023136,27.7283038581685));
#39848=CARTESIAN_POINT('Ctrl Pts',(134.012654697202,34.2253400585338,27.7225003268683));
#39849=CARTESIAN_POINT('Ctrl Pts',(133.986591538088,34.108757660092,27.7166967955681));
#39850=CARTESIAN_POINT('Ctrl Pts',(133.960519927182,33.9921374561701,27.7108913822917));
#39851=CARTESIAN_POINT('Ctrl Pts',(133.929337069116,33.8767079838822,27.7050859690154));
#39852=CARTESIAN_POINT('Ctrl Pts',(133.89318758219,33.7629408058307,27.6992805557391));
#39853=CARTESIAN_POINT('Ctrl Pts',(133.856998063155,33.6490476414779,27.6934687135212));
#39854=CARTESIAN_POINT('Ctrl Pts',(133.815831060382,33.5368208352156,27.6876568713032));
#39855=CARTESIAN_POINT('Ctrl Pts',(133.769880212744,33.4267142085565,27.6818450290853));
#39856=CARTESIAN_POINT('Ctrl Pts',(133.723899184492,33.3165352636299,27.6760293696369));
#39857=CARTESIAN_POINT('Ctrl Pts',(133.673128227175,33.2084796403079,27.6702137101886));
#39858=CARTESIAN_POINT('Ctrl Pts',(133.617807277261,33.1029771997682,27.6643980507403));
#39859=CARTESIAN_POINT('Ctrl Pts',(133.562407085701,32.9973236376917,27.6585740609501));
#39860=CARTESIAN_POINT('Ctrl Pts',(133.50244409774,32.8942309096409,27.65275007116));
#39861=CARTESIAN_POINT('Ctrl Pts',(133.438201998309,32.7941006326619,27.6469260813698));
#39862=CARTESIAN_POINT('Ctrl Pts',(133.421157358906,32.7675341835642,27.6453808671452));
#39863=CARTESIAN_POINT('Ctrl Pts',(133.403811716603,32.7411760946367,27.6438356529206));
#39864=CARTESIAN_POINT('Ctrl Pts',(133.386170838338,32.7150334677315,27.6422904386959));
#39865=CARTESIAN_POINT('Ctrl Pts',(133.319685978813,32.616507257681,27.6364668425507));
#39866=CARTESIAN_POINT('Ctrl Pts',(133.248790165876,32.5207263059491,27.6306432464055));
#39867=CARTESIAN_POINT('Ctrl Pts',(133.173737465054,32.4281105189154,27.6248196502604));
#39868=CARTESIAN_POINT('Ctrl Pts',(133.098779454018,32.3356115800302,27.6190034014201));
#39869=CARTESIAN_POINT('Ctrl Pts',(133.019675241128,32.2462701776917,27.6131871525798));
#39870=CARTESIAN_POINT('Ctrl Pts',(132.936722447901,32.1604778106176,27.6073709037396));
#39871=CARTESIAN_POINT('Ctrl Pts',(132.853852690552,32.07477132184,27.6015604769737));
#39872=CARTESIAN_POINT('Ctrl Pts',(132.767142299016,31.9926070927561,27.5957500502078));
#39873=CARTESIAN_POINT('Ctrl Pts',(132.676929095141,31.9143435674743,27.5899396234419));
#39874=CARTESIAN_POINT('Ctrl Pts',(132.583301190007,31.8331176536858,27.5839092635538));
#39875=CARTESIAN_POINT('Ctrl Pts',(132.485900342307,31.756093921046,27.5778789036657));
#39876=CARTESIAN_POINT('Ctrl Pts',(132.385146510728,31.6836313349749,27.5718485437776));
#39877=CARTESIAN_POINT('Ctrl Pts',(132.288176538371,31.6138901166196,27.5660446569924));
#39878=CARTESIAN_POINT('Ctrl Pts',(132.188101247688,31.5483738906348,27.5602407702073));
#39879=CARTESIAN_POINT('Ctrl Pts',(132.085328121047,31.4873611589618,27.5544368834221));
#39880=CARTESIAN_POINT('Ctrl Pts',(131.982570174944,31.4263574394312,27.5486338539245));
#39881=CARTESIAN_POINT('Ctrl Pts',(131.877115536391,31.3698560997177,27.5428308244269));
#39882=CARTESIAN_POINT('Ctrl Pts',(131.769398924827,31.3180911954772,27.5370277949292));
#39883=CARTESIAN_POINT('Ctrl Pts',(131.661672802915,31.2663217208905,27.5312242530796));
#39884=CARTESIAN_POINT('Ctrl Pts',(131.55168467898,31.2192896901016,27.5254207112299));
#39885=CARTESIAN_POINT('Ctrl Pts',(131.439891430112,31.1771819727471,27.5196171693803));
#39886=CARTESIAN_POINT('Ctrl Pts',(131.328061927962,31.1350606003377,27.5138117455078));
#39887=CARTESIAN_POINT('Ctrl Pts',(131.21442651862,31.0978668610919,27.5080063216354));
#39888=CARTESIAN_POINT('Ctrl Pts',(131.099458879435,31.0657382938559,27.502200897763));
#39889=CARTESIAN_POINT('Ctrl Pts',(130.984363924466,31.0335741472714,27.4963890449329));
#39890=CARTESIAN_POINT('Ctrl Pts',(130.867934188295,31.0064864791049,27.4905771921028));
#39891=CARTESIAN_POINT('Ctrl Pts',(130.750655381388,30.9845621037809,27.4847653392727));
#39892=CARTESIAN_POINT('Ctrl Pts',(130.633299545212,30.9626233284244,27.4789496691905));
#39893=CARTESIAN_POINT('Ctrl Pts',(130.515093931039,30.9458546569408,27.4731339991082));
#39894=CARTESIAN_POINT('Ctrl Pts',(130.396529588248,30.9342910475977,27.467318329026));
#39895=CARTESIAN_POINT('Ctrl Pts',(130.277795415379,30.9227108746858,27.4614943286509));
#39896=CARTESIAN_POINT('Ctrl Pts',(130.158701894607,30.9163506667168,27.4556703282757));
#39897=CARTESIAN_POINT('Ctrl Pts',(130.039740434039,30.9151933096042,27.4498463279006));
#39898=CARTESIAN_POINT('Ctrl Pts',(130.008179823231,30.9148862614457,27.4483012139762));
#39899=CARTESIAN_POINT('Ctrl Pts',(129.976628479121,30.9149451312888,27.4467561000519));
#39900=CARTESIAN_POINT('Ctrl Pts',(129.945095500927,30.9153689890051,27.4452109861275));
#39901=CARTESIAN_POINT('Ctrl Pts',(129.826246487297,30.9169665251206,27.4393873920247));
#39902=CARTESIAN_POINT('Ctrl Pts',(129.707275603486,30.9237581021851,27.4335637979218));
#39903=CARTESIAN_POINT('Ctrl Pts',(129.588673316226,30.9357614047382,27.427740203819));
#39904=CARTESIAN_POINT('Ctrl Pts',(129.470220663086,30.9477495633707,27.4219239570313));
#39905=CARTESIAN_POINT('Ctrl Pts',(129.352136084225,30.9649363285143,27.4161077102436));
#39906=CARTESIAN_POINT('Ctrl Pts',(129.234910162862,30.9872873836881,27.4102914634559));
#39907=CARTESIAN_POINT('Ctrl Pts',(129.117801585028,31.0096160653829,27.4044810387502));
#39908=CARTESIAN_POINT('Ctrl Pts',(129.001550353591,31.0370986770465,27.3986706140445));
#39909=CARTESIAN_POINT('Ctrl Pts',(128.88664144223,31.0696491604642,27.3928601893387));
#39910=CARTESIAN_POINT('Ctrl Pts',(128.767383003585,31.1034317434123,27.3868298286812));
#39911=CARTESIAN_POINT('Ctrl Pts',(128.649570957668,31.1426733911688,27.3807994680238));
#39912=CARTESIAN_POINT('Ctrl Pts',(128.533735739348,31.1872196341864,27.3747691073663));
#39913=CARTESIAN_POINT('Ctrl Pts',(128.422250822974,31.230092900621,27.3689652226467));
#39914=CARTESIAN_POINT('Ctrl Pts',(128.312597344001,31.2778793496121,27.3631613379271));
#39915=CARTESIAN_POINT('Ctrl Pts',(128.205231600169,31.3303908394807,27.3573574532075));
#39916=CARTESIAN_POINT('Ctrl Pts',(128.097881715221,31.3828945729307,27.3515544257738));
#39917=CARTESIAN_POINT('Ctrl Pts',(127.992819260116,31.4401217799373,27.3457513983401));
#39918=CARTESIAN_POINT('Ctrl Pts',(127.890478289381,31.5018371746835,27.3399483709064));
#39919=CARTESIAN_POINT('Ctrl Pts',(127.788128282844,31.5635580183531,27.3341448311167));
#39920=CARTESIAN_POINT('Ctrl Pts',(127.688500588112,31.629767626759,27.3283412913271));
#39921=CARTESIAN_POINT('Ctrl Pts',(127.592001940709,31.7001863164031,27.3225377515374));
#39922=CARTESIAN_POINT('Ctrl Pts',(127.495471999776,31.7706278421129,27.3167323297187));
#39923=CARTESIAN_POINT('Ctrl Pts',(127.402073453898,31.845280923083,27.3109269079));
#39924=CARTESIAN_POINT('Ctrl Pts',(127.31218098904,31.9238247832211,27.3051214860814));
#39925=CARTESIAN_POINT('Ctrl Pts',(127.222188976442,32.002455623551,27.2993096352853));
#39926=CARTESIAN_POINT('Ctrl Pts',(127.135711102675,32.0849855747184,27.2934977844892));
#39927=CARTESIAN_POINT('Ctrl Pts',(127.053086225376,32.1710559911988,27.2876859336931));
#39928=CARTESIAN_POINT('Ctrl Pts',(126.970407079522,32.2571829392871,27.2818702656357));
#39929=CARTESIAN_POINT('Ctrl Pts',(126.891586239002,32.3468546777902,27.2760545975783));
#39930=CARTESIAN_POINT('Ctrl Pts',(126.816922117047,32.4396796702254,27.2702389295209));
#39931=CARTESIAN_POINT('Ctrl Pts',(126.742151046733,32.5326376245228,27.2644149311418));
#39932=CARTESIAN_POINT('Ctrl Pts',(126.671548819826,32.6287575199072,27.2585909327626));
#39933=CARTESIAN_POINT('Ctrl Pts',(126.605370494381,32.727618975704,27.2527669343835));
#39934=CARTESIAN_POINT('Ctrl Pts',(126.587813079677,32.7538473755006,27.2512218007753));
#39935=CARTESIAN_POINT('Ctrl Pts',(126.570566795796,32.7802686127526,27.2496766671671));
#39936=CARTESIAN_POINT('Ctrl Pts',(126.553635852822,32.8068745669608,27.248131533559));
#39937=CARTESIAN_POINT('Ctrl Pts',(126.488371803229,32.9094330787663,27.2421754756724));
#39938=CARTESIAN_POINT('Ctrl Pts',(126.427594206498,33.015056667611,27.2362194177857));
#39939=CARTESIAN_POINT('Ctrl Pts',(126.371595291591,33.1233262744958,27.2302633598991));
#39940=CARTESIAN_POINT('Ctrl Pts',(126.315676623204,33.2314407308912,27.2243158370513));
#39941=CARTESIAN_POINT('Ctrl Pts',(126.264523181674,33.3421933208752,27.2183683142034));
#39942=CARTESIAN_POINT('Ctrl Pts',(126.218383658613,33.4551366252794,27.2124207913556));
#39943=CARTESIAN_POINT('Ctrl Pts',(126.172301362892,33.5679398449035,27.2064806452835));
#39944=CARTESIAN_POINT('Ctrl Pts',(126.131220750027,33.6829280171375,27.2005404992115));
#39945=CARTESIAN_POINT('Ctrl Pts',(126.095344190094,33.7996300544536,27.1946003531394));
#39946=CARTESIAN_POINT('Ctrl Pts',(126.059514012288,33.9161812164208,27.1886678866386));
#39947=CARTESIAN_POINT('Ctrl Pts',(126.02887459329,34.0344414634443,27.1827354201378));
#39948=CARTESIAN_POINT('Ctrl Pts',(126.003579608595,34.153921365851,27.176802953637));
#39949=CARTESIAN_POINT('Ctrl Pts',(125.978303893947,34.2733102469177,27.1708750065662));
#39950=CARTESIAN_POINT('Ctrl Pts',(125.958364588403,34.3939165600159,27.1649470594953));
#39951=CARTESIAN_POINT('Ctrl Pts',(125.9438651346,34.5152372191622,27.1590191124245));
#39952=CARTESIAN_POINT('Ctrl Pts',(125.929375293507,34.6364774462863,27.1530950954079));
#39953=CARTESIAN_POINT('Ctrl Pts',(125.92031816485,34.7584306959922,27.1471710783913));
#39954=CARTESIAN_POINT('Ctrl Pts',(125.916745755823,34.8805856900996,27.1412470613746));
#39955=CARTESIAN_POINT('Ctrl Pts',(125.91556740094,34.920878370092,27.1392930313846));
#39956=CARTESIAN_POINT('Ctrl Pts',(125.914985366504,34.9611929501148,27.1373390013945));
#39957=CARTESIAN_POINT('Ctrl Pts',(125.915000279441,35.0015109705496,27.1353849714045));
#39958=CARTESIAN_POINT('Ctrl Pts',(125.915000279441,35.001510971197,27.1353849713731));
#39959=CARTESIAN_POINT('Ctrl Pts',(125.915048271955,35.1312615634159,27.1290965537948));
#39960=CARTESIAN_POINT('Ctrl Pts',(125.921282283117,35.2608260686367,27.1228081362166));
#39961=CARTESIAN_POINT('Ctrl Pts',(125.93362428894,35.3896326173498,27.1165197186383));
#39962=CARTESIAN_POINT('Ctrl Pts',(125.946018781118,35.5189869365177,27.1102045585582));
#39963=CARTESIAN_POINT('Ctrl Pts',(125.964573240673,35.6475765570869,27.1038893984782));
#39964=CARTESIAN_POINT('Ctrl Pts',(125.989158035468,35.7748365863507,27.0975742383981));
#39965=CARTESIAN_POINT('Ctrl Pts',(126.01379677885,35.9023758735403,27.0912452204043));
#39966=CARTESIAN_POINT('Ctrl Pts',(126.044492226899,36.0285794609645,27.0849162024105));
#39967=CARTESIAN_POINT('Ctrl Pts',(126.081064803515,36.1528971878489,27.0785871844168));
#39968=CARTESIAN_POINT('Ctrl Pts',(126.117752827032,36.2776073425498,27.0722381879149));
#39969=CARTESIAN_POINT('Ctrl Pts',(126.160355004852,36.4004194525701,27.065889191413));
#39970=CARTESIAN_POINT('Ctrl Pts',(126.208642673224,36.5208006512037,27.0595401949112));
#39971=CARTESIAN_POINT('Ctrl Pts',(126.230161624026,36.5744474139953,27.0567108236043));
#39972=CARTESIAN_POINT('Ctrl Pts',(126.252809073841,36.6276117300588,27.0538814522974));
#39973=CARTESIAN_POINT('Ctrl Pts',(126.276561884097,36.6802480760414,27.0510520809906));
#39974=CARTESIAN_POINT('Ctrl Pts',(126.325451445855,36.788587588709,27.0452284869925));
#39975=CARTESIAN_POINT('Ctrl Pts',(126.379152242878,36.8949662532005,27.0394048929945));
#39976=CARTESIAN_POINT('Ctrl Pts',(126.437484778236,36.9989272859964,27.0335812989965));
#39977=CARTESIAN_POINT('Ctrl Pts',(126.495743718476,37.102757156578,27.0277650523234));
#39978=CARTESIAN_POINT('Ctrl Pts',(126.558622576169,37.2041751092696,27.0219488056503));
#39979=CARTESIAN_POINT('Ctrl Pts',(126.625894126271,37.3027450038749,27.0161325589771));
#39980=CARTESIAN_POINT('Ctrl Pts',(126.693098337221,37.4012162295303,27.0103221343956));
#39981=CARTESIAN_POINT('Ctrl Pts',(126.76468626422,37.4968447333148,27.004511709814));
#39982=CARTESIAN_POINT('Ctrl Pts',(126.840385476734,37.589220165294,26.9987012852324));
#39983=CARTESIAN_POINT('Ctrl Pts',(126.918950054896,37.6850921909736,26.992670924532));
#39984=CARTESIAN_POINT('Ctrl Pts',(127.001943089512,37.7774596175838,26.9866405638316));
#39985=CARTESIAN_POINT('Ctrl Pts',(127.08901128064,37.8658977085305,26.9806102031311));
#39986=CARTESIAN_POINT('Ctrl Pts',(127.1728095402,37.9510144199724,26.9748063185591));
#39987=CARTESIAN_POINT('Ctrl Pts',(127.260382070995,38.0324912962786,26.969002433987));
#39988=CARTESIAN_POINT('Ctrl Pts',(127.351374281094,38.1099850162262,26.9631985494149));
#39989=CARTESIAN_POINT('Ctrl Pts',(127.442353050695,38.1874672895432,26.9573955221371));
#39990=CARTESIAN_POINT('Ctrl Pts',(127.53675018428,38.2609673118662,26.9515924948594));
#39991=CARTESIAN_POINT('Ctrl Pts',(127.634176737521,38.3301809696641,26.9457894675816));
#39992=CARTESIAN_POINT('Ctrl Pts',(127.731611892525,38.3994007383172,26.9399859279561));
#39993=CARTESIAN_POINT('Ctrl Pts',(127.832076666072,38.4643331535117,26.9341823883306));
#39994=CARTESIAN_POINT('Ctrl Pts',(127.93515230517,38.5247168676583,26.9283788487051));
#39995=CARTESIAN_POINT('Ctrl Pts',(128.038261370507,38.5851201635458,26.9225734270587));
#39996=CARTESIAN_POINT('Ctrl Pts',(128.143982633088,38.6409716184659,26.9167680054124));
#39997=CARTESIAN_POINT('Ctrl Pts',(128.251872449466,38.6920556695512,26.910962583766));
#39998=CARTESIAN_POINT('Ctrl Pts',(128.359881743812,38.743196291486,26.9051507331535));
#39999=CARTESIAN_POINT('Ctrl Pts',(128.470064016221,38.7895587964898,26.899338882541));
#40000=CARTESIAN_POINT('Ctrl Pts',(128.581955196081,38.8309755851582,26.8935270319286));
#40001=CARTESIAN_POINT('Ctrl Pts',(128.693919866665,38.8724195765945,26.8877113640616));
#40002=CARTESIAN_POINT('Ctrl Pts',(128.807595292124,38.9089112579561,26.8818956961946));
#40003=CARTESIAN_POINT('Ctrl Pts',(128.922503381589,38.9403332393737,26.8760800283276));
#40004=CARTESIAN_POINT('Ctrl Pts',(129.037576064424,38.9718002293703,26.8702560301474));
#40005=CARTESIAN_POINT('Ctrl Pts',(129.153884538615,38.9981829352654,26.8644320319673));
#40006=CARTESIAN_POINT('Ctrl Pts',(129.270941565159,39.0194152309243,26.8586080337871));
#40007=CARTESIAN_POINT('Ctrl Pts',(129.301997365204,39.0250482625156,26.8570628986654));
#40008=CARTESIAN_POINT('Ctrl Pts',(129.333105833467,39.0303190576262,26.8555177635438));
#40009=CARTESIAN_POINT('Ctrl Pts',(129.364257843975,39.0352269962237,26.8539726284221));
#40010=CARTESIAN_POINT('Ctrl Pts',(129.481684253281,39.053727298362,26.8481482958581));
#40011=CARTESIAN_POINT('Ctrl Pts',(129.600108263132,39.0671274622222,26.8423239632942));
#40012=CARTESIAN_POINT('Ctrl Pts',(129.719049255623,39.0753271867709,26.8364996307302));
#40013=CARTESIAN_POINT('Ctrl Pts',(129.841350910667,39.0837585934895,26.8305107323934));
#40014=CARTESIAN_POINT('Ctrl Pts',(129.964198791598,39.0866911624357,26.8245218340567));
#40015=CARTESIAN_POINT('Ctrl Pts',(130.087058568312,39.0840722086765,26.8185329357199));
#40016=CARTESIAN_POINT('Ctrl Pts',(130.206242812632,39.0815316048023,26.812723204157));
#40017=CARTESIAN_POINT('Ctrl Pts',(130.325437804712,39.0737668911315,26.8069134725942));
#40018=CARTESIAN_POINT('Ctrl Pts',(130.444151133482,39.0607825318068,26.8011037410314));
#40019=CARTESIAN_POINT('Ctrl Pts',(130.562785665313,39.0478067909563,26.7952978657252));
#40020=CARTESIAN_POINT('Ctrl Pts',(130.680938765249,39.029618339027,26.7894919904189));
#40021=CARTESIAN_POINT('Ctrl Pts',(130.798120612488,39.0062736411684,26.7836861151127));
#40022=CARTESIAN_POINT('Ctrl Pts',(130.915252335739,38.9829389288958,26.7778827232427));
#40023=CARTESIAN_POINT('Ctrl Pts',(131.031413233102,38.9544524383411,26.7720793313726));
#40024=CARTESIAN_POINT('Ctrl Pts',(131.146121812408,38.9209220587922,26.7662759395025));
#40025=CARTESIAN_POINT('Ctrl Pts',(131.260808396864,38.8873981085414,26.7604736604065));
#40026=CARTESIAN_POINT('Ctrl Pts',(131.374042826227,38.8488323097756,26.7546713813104));
#40027=CARTESIAN_POINT('Ctrl Pts',(131.485357573226,38.805382750744,26.7488691022144));
#40028=CARTESIAN_POINT('Ctrl Pts',(131.596710419228,38.7619183205032,26.7430648372085));
#40029=CARTESIAN_POINT('Ctrl Pts',(131.706141889195,38.7135669378079,26.7372605722027));
#40030=CARTESIAN_POINT('Ctrl Pts',(131.813203483573,38.6605352241386,26.7314563071968));
#40031=CARTESIAN_POINT('Ctrl Pts',(131.920288084238,38.6074921145727,26.7256507949221));
#40032=CARTESIAN_POINT('Ctrl Pts',(132.025001434137,38.5497668617555,26.7198452826475));
#40033=CARTESIAN_POINT('Ctrl Pts',(132.126919784333,38.4876119668069,26.7140397703728));
#40034=CARTESIAN_POINT('Ctrl Pts',(132.228918119051,38.4254082933057,26.7082297019889));
#40035=CARTESIAN_POINT('Ctrl Pts',(132.328116733961,38.3587682615466,26.7024196336051));
#40036=CARTESIAN_POINT('Ctrl Pts',(132.424121131059,38.2879874911491,26.6966095652212));
#40037=CARTESIAN_POINT('Ctrl Pts',(132.445290840541,38.2723797857573,26.6953284003634));
#40038=CARTESIAN_POINT('Ctrl Pts',(132.466305362836,38.2565708981207,26.6940472355056));
#40039=CARTESIAN_POINT('Ctrl Pts',(132.487160689988,38.2405642567579,26.6927660706478));
#40040=CARTESIAN_POINT('',(125.915000003014,34.9998430692718,27.2396150285593));
#40041=CARTESIAN_POINT('Ctrl Pts',(125.915000003014,34.9998430692718,27.2396150285593));
#40042=CARTESIAN_POINT('Ctrl Pts',(125.914995442005,35.1185688455264,27.233798040471));
#40043=CARTESIAN_POINT('Ctrl Pts',(125.920171118825,35.2374883957075,27.2279810523828));
#40044=CARTESIAN_POINT('Ctrl Pts',(125.930551771767,35.3561125071268,27.2221640642946));
#40045=CARTESIAN_POINT('Ctrl Pts',(125.940919324587,35.4745869179101,27.2163544170986));
#40046=CARTESIAN_POINT('Ctrl Pts',(125.956478754098,35.5927662272477,27.2105447699026));
#40047=CARTESIAN_POINT('Ctrl Pts',(125.977202804292,35.7101603496408,27.2047351227065));
#40048=CARTESIAN_POINT('Ctrl Pts',(125.997906137723,35.8274371191898,27.1989312831149));
#40049=CARTESIAN_POINT('Ctrl Pts',(126.023763750782,35.9439298623713,27.1931274435233));
#40050=CARTESIAN_POINT('Ctrl Pts',(126.054696570429,36.0591533640682,27.1873236039317));
#40051=CARTESIAN_POINT('Ctrl Pts',(126.086567251909,36.1778703631443,27.1813437959126));
#40052=CARTESIAN_POINT('Ctrl Pts',(126.123825766443,36.2952394869812,27.1753639878935));
#40053=CARTESIAN_POINT('Ctrl Pts',(126.166328678407,36.4107406558232,27.1693841798744));
#40054=CARTESIAN_POINT('Ctrl Pts',(126.207534872459,36.5227180088249,27.1635868093356));
#40055=CARTESIAN_POINT('Ctrl Pts',(126.25366995735,36.6329393186652,27.1577894387969));
#40056=CARTESIAN_POINT('Ctrl Pts',(126.304552755165,36.7409464841407,27.1519920682581));
#40057=CARTESIAN_POINT('Ctrl Pts',(126.355428249845,36.8489381475025,27.1461955298076));
#40058=CARTESIAN_POINT('Ctrl Pts',(126.411049927902,36.9547159282086,27.1403989913572));
#40059=CARTESIAN_POINT('Ctrl Pts',(126.471189154825,37.0578432931049,27.1346024529067));
#40060=CARTESIAN_POINT('Ctrl Pts',(126.531334033706,37.1609803500354,27.1288053696905));
#40061=CARTESIAN_POINT('Ctrl Pts',(126.595997099273,37.2614661422752,27.1230082864743));
#40062=CARTESIAN_POINT('Ctrl Pts',(126.664904941967,37.3588908312773,27.1172112032582));
#40063=CARTESIAN_POINT('Ctrl Pts',(126.733835626964,37.4563478156505,27.1114121983633));
#40064=CARTESIAN_POINT('Ctrl Pts',(126.807013651039,37.5507413448013,27.1056131934684));
#40065=CARTESIAN_POINT('Ctrl Pts',(126.884124077338,37.6416930621432,27.0998141885735));
#40066=CARTESIAN_POINT('Ctrl Pts',(126.961320031876,37.7327456600085,27.0940087516214));
#40067=CARTESIAN_POINT('Ctrl Pts',(127.042456829378,37.8203485141111,27.0882033146693));
#40068=CARTESIAN_POINT('Ctrl Pts',(127.127181195765,37.9041585903719,27.0823978777172));
#40069=CARTESIAN_POINT('Ctrl Pts',(127.211961990312,37.9880244858578,27.0765885742253));
#40070=CARTESIAN_POINT('Ctrl Pts',(127.300334809232,38.0680922990568,27.0707792707334));
#40071=CARTESIAN_POINT('Ctrl Pts',(127.391912961667,38.1440590007952,27.0649699672416));
#40072=CARTESIAN_POINT('Ctrl Pts',(127.483621025753,38.2201334679702,27.0591524227426));
#40073=CARTESIAN_POINT('Ctrl Pts',(127.578543172832,38.2920949669791,27.0533348782437));
#40074=CARTESIAN_POINT('Ctrl Pts',(127.67626334802,38.3596834631023,27.0475173337447));
#40075=CARTESIAN_POINT('Ctrl Pts',(127.69703133574,38.3740477134203,27.0462809596543));
#40076=CARTESIAN_POINT('Ctrl Pts',(127.717925613344,38.3882146140039,27.0450445855638));
#40077=CARTESIAN_POINT('Ctrl Pts',(127.738942050042,38.4021819391287,27.0438082114734));
#40078=CARTESIAN_POINT('Ctrl Pts',(127.837934092801,38.467971114801,27.0379846173702));
#40079=CARTESIAN_POINT('Ctrl Pts',(127.93995951586,38.5295422912216,27.0321610232671));
#40080=CARTESIAN_POINT('Ctrl Pts',(128.044623506409,38.5866039324562,27.026337429164));
#40081=CARTESIAN_POINT('Ctrl Pts',(128.149155448036,38.6435935820906,27.0205211823759));
#40082=CARTESIAN_POINT('Ctrl Pts',(128.256318980616,38.6960848189604,27.0147049355879));
#40083=CARTESIAN_POINT('Ctrl Pts',(128.365689833005,38.7438289595088,27.0088886887999));
#40084=CARTESIAN_POINT('Ctrl Pts',(128.474951204815,38.7915253080173,27.0030782640938));
#40085=CARTESIAN_POINT('Ctrl Pts',(128.586415128756,38.8344838510123,26.9972678393877));
#40086=CARTESIAN_POINT('Ctrl Pts',(128.699632747636,38.8725017764978,26.9914574146816));
#40087=CARTESIAN_POINT('Ctrl Pts',(128.817135875057,38.9119587548976,26.9854270540242));
#40088=CARTESIAN_POINT('Ctrl Pts',(128.936527688606,38.946093487041,26.9793966933669));
#40089=CARTESIAN_POINT('Ctrl Pts',(129.057283182258,38.9747339535555,26.9733663327095));
#40090=CARTESIAN_POINT('Ctrl Pts',(129.173503588349,39.0022988000752,26.9675624479895));
#40091=CARTESIAN_POINT('Ctrl Pts',(129.290986660056,39.0247745208024,26.9617585632694));
#40092=CARTESIAN_POINT('Ctrl Pts',(129.409249566314,39.0420587483484,26.9559546785494));
#40093=CARTESIAN_POINT('Ctrl Pts',(129.52749500408,39.059340422859,26.9501516511152));
#40094=CARTESIAN_POINT('Ctrl Pts',(129.646519643388,39.0714320701358,26.9443486236811));
#40095=CARTESIAN_POINT('Ctrl Pts',(129.765832391457,39.0782827919492,26.9385455962469));
#40096=CARTESIAN_POINT('Ctrl Pts',(129.885155673786,39.0851341186208,26.9327420564567));
#40097=CARTESIAN_POINT('Ctrl Pts',(130.004766707767,39.0867435764065,26.9269385166666));
#40098=CARTESIAN_POINT('Ctrl Pts',(130.124171878897,39.0831123355219,26.9211349768764));
#40099=CARTESIAN_POINT('Ctrl Pts',(130.243615771911,39.0794799170628,26.9153295550572));
#40100=CARTESIAN_POINT('Ctrl Pts',(130.362853261368,39.0706034324065,26.909524133238));
#40101=CARTESIAN_POINT('Ctrl Pts',(130.481393981532,39.0565360635085,26.9037187114188));
#40102=CARTESIAN_POINT('Ctrl Pts',(130.600065974779,39.0424531162769,26.8979068606221));
#40103=CARTESIAN_POINT('Ctrl Pts',(130.718039252805,39.0231678585879,26.8920950098255));
#40104=CARTESIAN_POINT('Ctrl Pts',(130.834831637331,38.998784957623,26.8862831590288));
#40105=CARTESIAN_POINT('Ctrl Pts',(130.951700731853,38.9743860418104,26.8804674909709));
#40106=CARTESIAN_POINT('Ctrl Pts',(131.067386993449,38.9448829154418,26.8746518229129));
#40107=CARTESIAN_POINT('Ctrl Pts',(131.181423052175,38.9104302284774,26.8688361548549));
#40108=CARTESIAN_POINT('Ctrl Pts',(131.295622455345,38.8759281917278,26.8630121564751));
#40109=CARTESIAN_POINT('Ctrl Pts',(131.408166553786,38.8364625783396,26.8571881580953));
#40110=CARTESIAN_POINT('Ctrl Pts',(131.518607473237,38.7922363246809,26.8513641597155));
#40111=CARTESIAN_POINT('Ctrl Pts',(131.547907958011,38.780502895818,26.849819026112));
#40112=CARTESIAN_POINT('Ctrl Pts',(131.577060541272,38.768434632946,26.8482738925085));
#40113=CARTESIAN_POINT('Ctrl Pts',(131.606057163088,38.7560358609703,26.8467287589049));
#40114=CARTESIAN_POINT('Ctrl Pts',(131.71534415374,38.7093054354188,26.8409052183987));
#40115=CARTESIAN_POINT('Ctrl Pts',(131.822766155655,38.6577259138305,26.8350816778925));
#40116=CARTESIAN_POINT('Ctrl Pts',(131.92786292703,38.6014676917309,26.8292581373863));
#40117=CARTESIAN_POINT('Ctrl Pts',(132.032811661782,38.5452887135238,26.8234427997703));
#40118=CARTESIAN_POINT('Ctrl Pts',(132.13544132709,38.4844443406247,26.8176274621543));
#40119=CARTESIAN_POINT('Ctrl Pts',(132.235311565709,38.4191529951451,26.8118121245382));
#40120=CARTESIAN_POINT('Ctrl Pts',(132.321400925854,38.3628710613767,26.8067992327967));
#40121=CARTESIAN_POINT('Ctrl Pts',(132.405440001865,38.3032855814883,26.8017863410552));
#40122=CARTESIAN_POINT('Ctrl Pts',(132.487160689988,38.2405642567579,26.7967734493137));
#40123=CARTESIAN_POINT('Ctrl Pts',(132.487160689988,38.2405642567579,28.0469635225512));
#40124=CARTESIAN_POINT('Ctrl Pts',(132.583285477107,38.166787663266,28.0410441731393));
#40125=CARTESIAN_POINT('Ctrl Pts',(132.675995746464,38.0888295148761,28.0351248237274));
#40126=CARTESIAN_POINT('Ctrl Pts',(132.764929492593,38.0070566840336,28.0292054743156));
#40127=CARTESIAN_POINT('Ctrl Pts',(132.852423572582,37.9266075978979,28.0233819477751));
#40128=CARTESIAN_POINT('Ctrl Pts',(132.93654471212,37.8422069564201,28.0175584212346));
#40129=CARTESIAN_POINT('Ctrl Pts',(133.016915646074,37.7541686557783,28.0117348946941));
#40130=CARTESIAN_POINT('Ctrl Pts',(133.097185165944,37.6662414440985,28.0059187164272));
#40131=CARTESIAN_POINT('Ctrl Pts',(133.173713619382,37.5746860017517,28.0001025381602));
#40132=CARTESIAN_POINT('Ctrl Pts',(133.246158332574,37.4798550521875,27.9942863598933));
#40133=CARTESIAN_POINT('Ctrl Pts',(133.318530516696,37.3851190439971,27.9884760045772));
#40134=CARTESIAN_POINT('Ctrl Pts',(133.386826847656,37.2871143750181,27.9826656492611));
#40135=CARTESIAN_POINT('Ctrl Pts',(133.450743337022,37.186228584115,27.976855293945));
#40136=CARTESIAN_POINT('Ctrl Pts',(133.517080265402,37.0815223721155,27.9708249076034));
#40137=CARTESIAN_POINT('Ctrl Pts',(133.57869877448,36.9737128468161,27.9647945212618));
#40138=CARTESIAN_POINT('Ctrl Pts',(133.63530660868,36.8632688643578,27.9587641349203));
#40139=CARTESIAN_POINT('Ctrl Pts',(133.689787582147,36.7569744660143,27.9529603213155));
#40140=CARTESIAN_POINT('Ctrl Pts',(133.739627405286,36.6482403978658,27.9471565077107));
#40141=CARTESIAN_POINT('Ctrl Pts',(133.784611536174,36.5375111447598,27.9413526941059));
#40142=CARTESIAN_POINT('Ctrl Pts',(133.829589018434,36.4267982573705,27.9355497383013));
#40143=CARTESIAN_POINT('Ctrl Pts',(133.869712082004,36.314091149679,27.9297467824967));
#40144=CARTESIAN_POINT('Ctrl Pts',(133.904814199417,36.1998546028725,27.923943826692));
#40145=CARTESIAN_POINT('Ctrl Pts',(133.939919413428,36.0856079784762,27.9181403589688));
#40146=CARTESIAN_POINT('Ctrl Pts',(133.970002680679,35.9698320370626,27.9123368912457));
#40147=CARTESIAN_POINT('Ctrl Pts',(133.994947438924,35.8530064244976,27.9065334235225));
#40148=CARTESIAN_POINT('Ctrl Pts',(134.01990028505,35.7361429333669,27.9007280741311));
#40149=CARTESIAN_POINT('Ctrl Pts',(134.039711223514,35.6182294933733,27.8949227247398));
#40150=CARTESIAN_POINT('Ctrl Pts',(134.05431497822,35.4997549973523,27.8891173753485));
#40151=CARTESIAN_POINT('Ctrl Pts',(134.068934905027,35.3811493034675,27.8833055971521));
#40152=CARTESIAN_POINT('Ctrl Pts',(134.078336087863,35.2619817188892,27.8774938189557));
#40153=CARTESIAN_POINT('Ctrl Pts',(134.082505203085,35.1427454615142,27.8716820407593));
#40154=CARTESIAN_POINT('Ctrl Pts',(134.086677056511,35.0234308918224,27.8658664454873));
#40155=CARTESIAN_POINT('Ctrl Pts',(134.085610002428,34.9040479669033,27.8600508502152));
#40156=CARTESIAN_POINT('Ctrl Pts',(134.079342789243,34.7850874413916,27.8542352549432));
#40157=CARTESIAN_POINT('Ctrl Pts',(134.073066598532,34.6659565097759,27.848411329068));
#40158=CARTESIAN_POINT('Ctrl Pts',(134.061575420097,34.5472495902595,27.8425874031927));
#40159=CARTESIAN_POINT('Ctrl Pts',(134.044959544605,34.4294500175206,27.8367634773175));
#40160=CARTESIAN_POINT('Ctrl Pts',(134.040549267299,34.3981830052858,27.835217658794));
#40161=CARTESIAN_POINT('Ctrl Pts',(134.035778227379,34.3669798459467,27.8336718402706));
#40162=CARTESIAN_POINT('Ctrl Pts',(134.030648706343,34.3358494101089,27.8321260217471));
#40163=CARTESIAN_POINT('Ctrl Pts',(134.011324098492,34.2185707284023,27.8263024104256));
#40164=CARTESIAN_POINT('Ctrl Pts',(133.986845442737,34.1019470596537,27.8204787991041));
#40165=CARTESIAN_POINT('Ctrl Pts',(133.957268485043,33.9864660157217,27.8146551877826));
#40166=CARTESIAN_POINT('Ctrl Pts',(133.927728842282,33.8711306651854,27.8088389236557));
#40167=CARTESIAN_POINT('Ctrl Pts',(133.893103791357,33.7569354643154,27.8030226595288));
#40168=CARTESIAN_POINT('Ctrl Pts',(133.85350051373,33.6443603758074,27.797206395402));
#40169=CARTESIAN_POINT('Ctrl Pts',(133.813936878326,33.531897973091,27.7913959532588));
#40170=CARTESIAN_POINT('Ctrl Pts',(133.769405064257,33.4210528395336,27.7855855111156));
#40171=CARTESIAN_POINT('Ctrl Pts',(133.720062577152,33.312291665579,27.7797750689724));
#40172=CARTESIAN_POINT('Ctrl Pts',(133.668852589176,33.1994141286498,27.7737447148143));
#40173=CARTESIAN_POINT('Ctrl Pts',(133.612460699163,33.0887818482519,27.7677143606563));
#40174=CARTESIAN_POINT('Ctrl Pts',(133.551118842144,32.9808962461116,27.7616840064982));
#40175=CARTESIAN_POINT('Ctrl Pts',(133.492080494645,32.8770619642861,27.7558801042097));
#40176=CARTESIAN_POINT('Ctrl Pts',(133.42845745895,32.7757721807581,27.7500762019212));
#40177=CARTESIAN_POINT('Ctrl Pts',(133.36050389807,32.6774499895463,27.7442722996327));
#40178=CARTESIAN_POINT('Ctrl Pts',(133.292560374304,32.5791423210627,27.7384692546125));
#40179=CARTESIAN_POINT('Ctrl Pts',(133.220287829496,32.4838017090188,27.7326662095923));
#40180=CARTESIAN_POINT('Ctrl Pts',(133.14398372125,32.3918222145501,27.7268631645721));
#40181=CARTESIAN_POINT('Ctrl Pts',(133.06767287607,32.299834599159,27.7210596071977));
#40182=CARTESIAN_POINT('Ctrl Pts',(132.987330020464,32.2112090056498,27.7152560498233));
#40183=CARTESIAN_POINT('Ctrl Pts',(132.903292433126,32.1263058534778,27.7094524924489));
#40184=CARTESIAN_POINT('Ctrl Pts',(132.819227593641,32.0413751684698,27.7036470530667));
#40185=CARTESIAN_POINT('Ctrl Pts',(132.731465926685,31.9601696155756,27.6978416136845));
#40186=CARTESIAN_POINT('Ctrl Pts',(132.640380557726,31.8830117885395,27.6920361743024));
#40187=CARTESIAN_POINT('Ctrl Pts',(132.54919432219,31.8057685180788,27.6862243060634));
#40188=CARTESIAN_POINT('Ctrl Pts',(132.454677349579,31.7325821848003,27.6804124378244));
#40189=CARTESIAN_POINT('Ctrl Pts',(132.35723486092,31.6637343015785,27.6746005695854));
#40190=CARTESIAN_POINT('Ctrl Pts',(132.259728372431,31.5948411993473,27.668784884135));
#40191=CARTESIAN_POINT('Ctrl Pts',(132.159292883962,31.5302924422394,27.6629691986846));
#40192=CARTESIAN_POINT('Ctrl Pts',(132.056360100272,31.4703246412723,27.6571535132342));
#40193=CARTESIAN_POINT('Ctrl Pts',(131.953279880483,31.4102709452354,27.6513294976683));
#40194=CARTESIAN_POINT('Ctrl Pts',(131.847695586173,31.3548114910392,27.6455054821024));
#40195=CARTESIAN_POINT('Ctrl Pts',(131.740060969837,31.3041357139024,27.6396814665365));
#40196=CARTESIAN_POINT('Ctrl Pts',(131.71150819594,31.2906926966291,27.6381365007506));
#40197=CARTESIAN_POINT('Ctrl Pts',(131.682811231503,31.2775860416633,27.6365915349646));
#40198=CARTESIAN_POINT('Ctrl Pts',(131.653978731735,31.2648186985144,27.6350465691787));
#40199=CARTESIAN_POINT('Ctrl Pts',(131.545297395629,31.2166934258846,27.6292229691716));
#40200=CARTESIAN_POINT('Ctrl Pts',(131.43433863683,31.1732378844396,27.6233993691645));
#40201=CARTESIAN_POINT('Ctrl Pts',(131.321540835858,31.1346727410012,27.6175757691575));
#40202=CARTESIAN_POINT('Ctrl Pts',(131.208885343006,31.0961562521731,27.6117595163288));
#40203=CARTESIAN_POINT('Ctrl Pts',(131.094395805726,31.0625180206387,27.6059432635002));
#40204=CARTESIAN_POINT('Ctrl Pts',(130.978532402161,31.0339315011057,27.6001270106715));
#40205=CARTESIAN_POINT('Ctrl Pts',(130.862784975558,31.0053735961101,27.5943165797962));
#40206=CARTESIAN_POINT('Ctrl Pts',(130.745666812655,30.9818574407616,27.5885061489209));
#40207=CARTESIAN_POINT('Ctrl Pts',(130.627654577018,30.9635071247495,27.5826957180457));
#40208=CARTESIAN_POINT('Ctrl Pts',(130.505175523237,30.9444622407201,27.5766653596525));
#40209=CARTESIAN_POINT('Ctrl Pts',(130.381733801461,30.9309821262726,27.5706350012594));
#40210=CARTESIAN_POINT('Ctrl Pts',(130.257875927179,30.9231476595072,27.5646046428662));
#40211=CARTESIAN_POINT('Ctrl Pts',(130.138669476049,30.9156074123892,27.5588007516946));
#40212=CARTESIAN_POINT('Ctrl Pts',(130.019078009738,30.9132964485294,27.5529968605229));
#40213=CARTESIAN_POINT('Ctrl Pts',(129.899594713185,30.9162341180744,27.5471929693512));
#40214=CARTESIAN_POINT('Ctrl Pts',(129.780129063444,30.919171353747,27.541389935372));
#40215=CARTESIAN_POINT('Ctrl Pts',(129.660771959791,30.9273556711925,27.5355869013928));
#40216=CARTESIAN_POINT('Ctrl Pts',(129.542016037412,30.9407542954371,27.5297838674136));
#40217=CARTESIAN_POINT('Ctrl Pts',(129.423249628174,30.9541541028605,27.5239803209917));
#40218=CARTESIAN_POINT('Ctrl Pts',(129.305084911542,30.9727690867957,27.5181767745699));
#40219=CARTESIAN_POINT('Ctrl Pts',(129.18800821421,30.9965147259158,27.512373228148));
#40220=CARTESIAN_POINT('Ctrl Pts',(129.070893548525,31.0202680658237,27.5065677996172));
#40221=CARTESIAN_POINT('Ctrl Pts',(128.954868003857,31.0491552888899,27.5007623710865));
#40222=CARTESIAN_POINT('Ctrl Pts',(128.840405920406,31.0830411579172,27.4949569425557));
#40223=CARTESIAN_POINT('Ctrl Pts',(128.725817079056,31.1169645529219,27.4891450849621));
#40224=CARTESIAN_POINT('Ctrl Pts',(128.61279554674,31.155897527465,27.4833332273686));
#40225=CARTESIAN_POINT('Ctrl Pts',(128.501798898363,31.1996554815314,27.477521369775));
#40226=CARTESIAN_POINT('Ctrl Pts',(128.39072934565,31.2434421765072,27.4717056948624));
#40227=CARTESIAN_POINT('Ctrl Pts',(128.281687697644,31.2920599964923,27.4658900199498));
#40228=CARTESIAN_POINT('Ctrl Pts',(128.175108491949,31.3452775777301,27.4600743450371));
#40229=CARTESIAN_POINT('Ctrl Pts',(128.06837662253,31.3985713876661,27.4542503397698));
#40230=CARTESIAN_POINT('Ctrl Pts',(127.964114591217,31.4564779119516,27.4484263345025));
#40231=CARTESIAN_POINT('Ctrl Pts',(127.862729564812,31.5187214867423,27.4426023292352));
#40232=CARTESIAN_POINT('Ctrl Pts',(127.835832773983,31.5352343039789,27.4410572583602));
#40233=CARTESIAN_POINT('Ctrl Pts',(127.809138294224,31.5520521409498,27.4395121874852));
#40234=CARTESIAN_POINT('Ctrl Pts',(127.782653338354,31.5691693743226,27.4379671166102));
#40235=CARTESIAN_POINT('Ctrl Pts',(127.682827870344,31.6336865983971,27.4321435304219));
#40236=CARTESIAN_POINT('Ctrl Pts',(127.585659605872,31.7026683513086,27.4263199442336));
#40237=CARTESIAN_POINT('Ctrl Pts',(127.491573407953,31.775868949265,27.4204963580452));
#40238=CARTESIAN_POINT('Ctrl Pts',(127.397605915691,31.8489771922829,27.4146801192961));
#40239=CARTESIAN_POINT('Ctrl Pts',(127.306713075196,31.9262934449156,27.408863880547));
#40240=CARTESIAN_POINT('Ctrl Pts',(127.219292211587,32.0075279123338,27.4030476417979));
#40241=CARTESIAN_POINT('Ctrl Pts',(127.131958858376,32.0886810620874,27.3972372252443));
#40242=CARTESIAN_POINT('Ctrl Pts',(127.048090865319,32.173744347478,27.3914268086907));
#40243=CARTESIAN_POINT('Ctrl Pts',(126.968053307013,32.2623871254526,27.3856163921371));
#40244=CARTESIAN_POINT('Ctrl Pts',(126.884986012364,32.3543853811768,27.3795860284665));
#40245=CARTESIAN_POINT('Ctrl Pts',(126.806045230369,32.4502392046965,27.3735556647959));
#40246=CARTESIAN_POINT('Ctrl Pts',(126.731598188848,32.549535839712,27.3675253011252));
#40247=CARTESIAN_POINT('Ctrl Pts',(126.659947216176,32.6451031092299,27.3617214247893));
#40248=CARTESIAN_POINT('Ctrl Pts',(126.592458788309,32.743858889048,27.3559175484534));
#40249=CARTESIAN_POINT('Ctrl Pts',(126.529419435327,32.8454013032322,27.3501136721175));
#40250=CARTESIAN_POINT('Ctrl Pts',(126.466389394609,32.946928717425,27.3443106531385));
#40251=CARTESIAN_POINT('Ctrl Pts',(126.407807337083,33.0512416005238,27.3385076341595));
#40252=CARTESIAN_POINT('Ctrl Pts',(126.353915895638,33.1579099631354,27.3327046151806));
#40253=CARTESIAN_POINT('Ctrl Pts',(126.300019696624,33.2645877424926,27.3269010839077));
#40254=CARTESIAN_POINT('Ctrl Pts',(126.250815121148,33.3736210503216,27.3210975526348));
#40255=CARTESIAN_POINT('Ctrl Pts',(126.20649806493,33.4845568078543,27.315294021362));
#40256=CARTESIAN_POINT('Ctrl Pts',(126.162166637525,33.5955285397647,27.3094886081131));
#40257=CARTESIAN_POINT('Ctrl Pts',(126.122726032854,33.7084035693056,27.3036831948643));
#40258=CARTESIAN_POINT('Ctrl Pts',(126.088323158834,33.8227110421468,27.2978777816155));
#40259=CARTESIAN_POINT('Ctrl Pts',(126.053882186911,33.9371450996128,27.2920659394252));
#40260=CARTESIAN_POINT('Ctrl Pts',(126.024490199166,34.0530143755138,27.2862540972348));
#40261=CARTESIAN_POINT('Ctrl Pts',(126.000243627778,34.1698349785303,27.2804422550445));
#40262=CARTESIAN_POINT('Ctrl Pts',(125.975981131191,34.2867323095666,27.2746265956239));
#40263=CARTESIAN_POINT('Ctrl Pts',(125.956870846573,34.4045818099437,27.2688109362033));
#40264=CARTESIAN_POINT('Ctrl Pts',(125.942957466058,34.5228932218206,27.2629952767826));
#40265=CARTESIAN_POINT('Ctrl Pts',(125.929024156037,34.6413741027878,27.2571712870201));
#40266=CARTESIAN_POINT('Ctrl Pts',(125.920302637767,34.7603178100554,27.2513472972576));
#40267=CARTESIAN_POINT('Ctrl Pts',(125.916785548389,34.879232694178,27.2455233074951));
#40268=CARTESIAN_POINT('Ctrl Pts',(125.915852398148,34.9107830589372,27.2439780930107));
#40269=CARTESIAN_POINT('Ctrl Pts',(125.915285325455,34.9423314174167,27.2424328785262));
#40270=CARTESIAN_POINT('Ctrl Pts',(125.915083580702,34.9738686519398,27.2408876640418));
#40271=CARTESIAN_POINT('Ctrl Pts',(125.915028195182,34.9825266522665,27.2404634522263));
#40272=CARTESIAN_POINT('Ctrl Pts',(125.915000335634,34.9911848288518,27.2400392404109));
#40273=CARTESIAN_POINT('Ctrl Pts',(125.915000003014,34.999843068532,27.2396150285955));
#40274=CARTESIAN_POINT('Origin',(130.,35.,32.7603849714045));
#40275=CARTESIAN_POINT('',(132.487160689988,38.2405642567579,29.2969312480094));
#40276=CARTESIAN_POINT('',(132.487160689988,38.2405642567579,29.1925548573102));
#40277=CARTESIAN_POINT('',(132.487160689988,38.2405642567579,32.7603849714045));
#40278=CARTESIAN_POINT('',(125.917751830235,34.9961206828433,29.7396160661079));
#40279=CARTESIAN_POINT('Ctrl Pts',(125.915001824241,34.996139424357,29.7396150285955));
#40280=CARTESIAN_POINT('Ctrl Pts',(125.914889749838,35.1147289232925,29.7338556081825));
#40281=CARTESIAN_POINT('Ctrl Pts',(125.919946015895,35.2333981463432,29.7280961877695));
#40282=CARTESIAN_POINT('Ctrl Pts',(125.930164564399,35.3516596751537,29.7223367673564));
#40283=CARTESIAN_POINT('Ctrl Pts',(125.940380529293,35.4698913032599,29.7165788031289));
#40284=CARTESIAN_POINT('Ctrl Pts',(125.955756146661,35.5877150288388,29.7108208389015));
#40285=CARTESIAN_POINT('Ctrl Pts',(125.976233330414,35.7046465700795,29.705062874674));
#40286=CARTESIAN_POINT('Ctrl Pts',(125.996710352475,35.8215771880147,29.699304955912));
#40287=CARTESIAN_POINT('Ctrl Pts',(126.022288789158,35.937615226823,29.6935470371501));
#40288=CARTESIAN_POINT('Ctrl Pts',(126.052859197963,36.0522853647639,29.6877891183882));
#40289=CARTESIAN_POINT('Ctrl Pts',(126.083436853566,36.1669826855672,29.6820298346963));
#40290=CARTESIAN_POINT('Ctrl Pts',(126.11900872687,36.280311059955,29.6762705510044));
#40291=CARTESIAN_POINT('Ctrl Pts',(126.159415358592,36.3918098333407,29.6705112673124));
#40292=CARTESIAN_POINT('Ctrl Pts',(126.199867100876,36.5034330856062,29.664745553871));
#40293=CARTESIAN_POINT('Ctrl Pts',(126.245164237707,36.6132222675609,29.6589798404296));
#40294=CARTESIAN_POINT('Ctrl Pts',(126.29509887264,36.7207360740361,29.6532141269882));
#40295=CARTESIAN_POINT('Ctrl Pts',(126.345063092839,36.8283135802748,29.6474449974777));
#40296=CARTESIAN_POINT('Ctrl Pts',(126.399670090961,36.9336126589249,29.6416758679673));
#40297=CARTESIAN_POINT('Ctrl Pts',(126.458666546603,37.0362176631811,29.6359067384569));
#40298=CARTESIAN_POINT('Ctrl Pts',(126.517759864122,37.1389911269355,29.6301281370433));
#40299=CARTESIAN_POINT('Ctrl Pts',(126.581256810047,37.2390613324478,29.6243495356297));
#40300=CARTESIAN_POINT('Ctrl Pts',(126.648861158634,37.3360422654332,29.6185709342161));
#40301=CARTESIAN_POINT('Ctrl Pts',(126.69850364912,37.4072562500898,29.6143276544318));
#40302=CARTESIAN_POINT('Ctrl Pts',(126.750360003743,37.4768051112654,29.6100843746475));
#40303=CARTESIAN_POINT('Ctrl Pts',(126.804299961969,37.5445483424232,29.6058410948631));
#40304=CARTESIAN_POINT('Ctrl Pts',(126.878347528946,37.6375447334366,29.600016015379));
#40305=CARTESIAN_POINT('Ctrl Pts',(126.956578022739,37.7274571730994,29.5941909358949));
#40306=CARTESIAN_POINT('Ctrl Pts',(127.038705298708,37.8138867589329,29.5883658564108));
#40307=CARTESIAN_POINT('Ctrl Pts',(127.120727860562,37.900206145111,29.5825482040334));
#40308=CARTESIAN_POINT('Ctrl Pts',(127.206637043737,37.9830512167573,29.5767305516559));
#40309=CARTESIAN_POINT('Ctrl Pts',(127.296105493946,38.0620547839862,29.5709128992785));
#40310=CARTESIAN_POINT('Ctrl Pts',(127.38548316037,38.1409781861636,29.5651011500826));
#40311=CARTESIAN_POINT('Ctrl Pts',(127.47841260485,38.2160675699333,29.5592894008868));
#40312=CARTESIAN_POINT('Ctrl Pts',(127.574528968689,38.2869918278376,29.5534776516909));
#40313=CARTESIAN_POINT('Ctrl Pts',(127.674252076596,38.3605775019278,29.547447817966));
#40314=CARTESIAN_POINT('Ctrl Pts',(127.777405659419,38.4296790098314,29.5414179842412));
#40315=CARTESIAN_POINT('Ctrl Pts',(127.883543317398,38.4939713952275,29.5353881505164));
#40316=CARTESIAN_POINT('Ctrl Pts',(127.985723378708,38.5558664851201,29.5295831535772));
#40317=CARTESIAN_POINT('Ctrl Pts',(128.090668581765,38.6133044408925,29.523778156638));
#40318=CARTESIAN_POINT('Ctrl Pts',(128.197950853518,38.666039262428,29.5179731596989));
#40319=CARTESIAN_POINT('Ctrl Pts',(128.305215790772,38.7187655631543,29.5121691007219));
#40320=CARTESIAN_POINT('Ctrl Pts',(128.414816679574,38.7667900609737,29.506365041745));
#40321=CARTESIAN_POINT('Ctrl Pts',(128.526301742813,38.8099131810009,29.5005609827681));
#40322=CARTESIAN_POINT('Ctrl Pts',(128.637795070035,38.8530394975884,29.4947564935573));
#40323=CARTESIAN_POINT('Ctrl Pts',(128.751172468688,38.8912635668722,29.4889520043466));
#40324=CARTESIAN_POINT('Ctrl Pts',(128.865963731343,38.9244345760084,29.4831475151359));
#40325=CARTESIAN_POINT('Ctrl Pts',(128.980790559682,38.9576158624917,29.4773412275249));
#40326=CARTESIAN_POINT('Ctrl Pts',(129.097031731301,38.9857408620556,29.471534939914));
#40327=CARTESIAN_POINT('Ctrl Pts',(129.214204113059,39.0087092466362,29.465728652303));
#40328=CARTESIAN_POINT('Ctrl Pts',(129.331503629525,39.0317025524383,29.4599160647375));
#40329=CARTESIAN_POINT('Ctrl Pts',(129.449735972206,39.0495279964193,29.454103477172));
#40330=CARTESIAN_POINT('Ctrl Pts',(129.568409950964,39.062136756631,29.4482908896064));
#40331=CARTESIAN_POINT('Ctrl Pts',(129.687160346985,39.0747536359515,29.4424745591645));
#40332=CARTESIAN_POINT('Ctrl Pts',(129.806352538996,39.0821471161672,29.4366582287226));
#40333=CARTESIAN_POINT('Ctrl Pts',(129.925494024779,39.0843204893417,29.4308418982807));
#40334=CARTESIAN_POINT('Ctrl Pts',(130.044803802069,39.0864969324816,29.4250173520691));
#40335=CARTESIAN_POINT('Ctrl Pts',(130.164062323563,39.0834385615248,29.4191928058575));
#40336=CARTESIAN_POINT('Ctrl Pts',(130.282780763463,39.0752006134441,29.4133682596459));
#40337=CARTESIAN_POINT('Ctrl Pts',(130.314078791113,39.0730288233917,29.4118327205288));
#40338=CARTESIAN_POINT('Ctrl Pts',(130.345339331425,39.0704973189299,29.4102971814117));
#40339=CARTESIAN_POINT('Ctrl Pts',(130.376553548765,39.0676077029272,29.4087616422947));
#40340=CARTESIAN_POINT('Ctrl Pts',(130.495101696714,39.0566332606825,29.4029298344217));
#40341=CARTESIAN_POINT('Ctrl Pts',(130.613354340383,39.0404549061107,29.3970980265487));
#40342=CARTESIAN_POINT('Ctrl Pts',(130.730819924737,39.0190953257677,29.3912662186756));
#40343=CARTESIAN_POINT('Ctrl Pts',(130.848147554704,38.9977608306259,29.385441259817));
#40344=CARTESIAN_POINT('Ctrl Pts',(130.964689566696,38.9712572826434,29.3796163009584));
#40345=CARTESIAN_POINT('Ctrl Pts',(131.079958497732,38.9396592039384,29.3737913420998));
#40346=CARTESIAN_POINT('Ctrl Pts',(131.195119026777,38.9080908409133,29.3679718611886));
#40347=CARTESIAN_POINT('Ctrl Pts',(131.30900846612,38.8714375842934,29.3621523802774));
#40348=CARTESIAN_POINT('Ctrl Pts',(131.421149147708,38.8298250743302,29.3563328993662));
#40349=CARTESIAN_POINT('Ctrl Pts',(131.533206202672,38.7882435960469,29.3505177582141));
#40350=CARTESIAN_POINT('Ctrl Pts',(131.643516715352,38.7417103665766,29.3447026170619));
#40351=CARTESIAN_POINT('Ctrl Pts',(131.751618452759,38.6904007635967,29.3388874759098));
#40352=CARTESIAN_POINT('Ctrl Pts',(131.859673491464,38.6391133257726,29.3330748468315));
#40353=CARTESIAN_POINT('Ctrl Pts',(131.965521286858,38.5830537948526,29.3272622177532));
#40354=CARTESIAN_POINT('Ctrl Pts',(132.068720326361,38.5224453453957,29.3214495886748));
#40355=CARTESIAN_POINT('Ctrl Pts',(132.171909973374,38.4618424121171,29.3156374886234));
#40356=CARTESIAN_POINT('Ctrl Pts',(132.272450991652,38.3966915867888,29.3098253885719));
#40357=CARTESIAN_POINT('Ctrl Pts',(132.369927599751,38.327261362132,29.3040132885205));
#40358=CARTESIAN_POINT('Ctrl Pts',(132.409519329725,38.2990611327622,29.3016526083501));
#40359=CARTESIAN_POINT('Ctrl Pts',(132.448605844018,38.270155429686,29.2992919281797));
#40360=CARTESIAN_POINT('Ctrl Pts',(132.487160689988,38.2405642567579,29.2969312480094));
#40361=CARTESIAN_POINT('',(128.942095577027,31.0543614925016,30.));
#40362=CARTESIAN_POINT('Ctrl Pts',(128.942095577027,31.0543614925016,30.));
#40363=CARTESIAN_POINT('Ctrl Pts',(127.639207105396,31.4036918921719,29.9343068491439));
#40364=CARTESIAN_POINT('Ctrl Pts',(126.178813659546,32.7814902171539,29.8475123998616));
#40365=CARTESIAN_POINT('Ctrl Pts',(125.916229948997,34.5620777500272,29.7607179505793));
#40366=CARTESIAN_POINT('Ctrl Pts',(125.919305187798,34.9961100965856,29.7396166521532));
#40367=CARTESIAN_POINT('',(131.058681707805,31.0545699801468,29.9999998737456));
#40368=CARTESIAN_POINT('Origin',(130.,35.,30.));
#40369=CARTESIAN_POINT('',(125.915000700078,35.0023915761614,29.6353849714475));
#40370=CARTESIAN_POINT('Ctrl Pts',(131.058681707805,31.0545699801468,29.9999998737456));
#40371=CARTESIAN_POINT('Ctrl Pts',(130.944553694239,31.0239458809479,29.9942106310195));
#40372=CARTESIAN_POINT('Ctrl Pts',(130.828901062776,30.9982256960231,29.9884213882935));
#40373=CARTESIAN_POINT('Ctrl Pts',(130.71218552957,30.9775608430368,29.9826321455674));
#40374=CARTESIAN_POINT('Ctrl Pts',(130.595617536489,30.9569221124944,29.976850221024));
#40375=CARTESIAN_POINT('Ctrl Pts',(130.477989717063,30.941326078079,29.9710682964807));
#40376=CARTESIAN_POINT('Ctrl Pts',(130.359778326282,30.9308742270682,29.9652863719373));
#40377=CARTESIAN_POINT('Ctrl Pts',(130.241684578543,30.920432777657,29.9595102015195));
#40378=CARTESIAN_POINT('Ctrl Pts',(130.123008824251,30.9151253657466,29.9537340311018));
#40379=CARTESIAN_POINT('Ctrl Pts',(130.004236212763,30.915002196512,29.9479578606841));
#40380=CARTESIAN_POINT('Ctrl Pts',(129.885547348981,30.9148791141253,29.9421857630994));
#40381=CARTESIAN_POINT('Ctrl Pts',(129.76676217621,30.9199330037176,29.9364136655148));
#40382=CARTESIAN_POINT('Ctrl Pts',(129.648369007186,30.9301620861645,29.9306415679301));
#40383=CARTESIAN_POINT('Ctrl Pts',(129.530019950461,30.9403873573414,29.9248716209805));
#40384=CARTESIAN_POINT('Ctrl Pts',(129.412063018777,30.9557839527955,29.9191016740308));
#40385=CARTESIAN_POINT('Ctrl Pts',(129.294983975858,30.9762980471084,29.9133317270811));
#40386=CARTESIAN_POINT('Ctrl Pts',(129.177920061441,30.9968094906693,29.9075625257017));
#40387=CARTESIAN_POINT('Ctrl Pts',(129.061734217666,31.0224370467372,29.9017933243223));
#40388=CARTESIAN_POINT('Ctrl Pts',(128.946903845468,31.0530754391158,29.8960241229428));
#40389=CARTESIAN_POINT('Ctrl Pts',(128.832060363897,31.0837173292635,29.8902542629344));
#40390=CARTESIAN_POINT('Ctrl Pts',(128.718573061178,31.1193710858633,29.8844844029259));
#40391=CARTESIAN_POINT('Ctrl Pts',(128.606905268368,31.1598812428911,29.8787145429175));
#40392=CARTESIAN_POINT('Ctrl Pts',(128.495128598352,31.2004308977242,29.8729390572382));
#40393=CARTESIAN_POINT('Ctrl Pts',(128.385175371563,31.2458462698854,29.867163571559));
#40394=CARTESIAN_POINT('Ctrl Pts',(128.277490140854,31.2959232209435,29.8613880858797));
#40395=CARTESIAN_POINT('Ctrl Pts',(128.169752954189,31.3460243331225,29.8556098136449));
#40396=CARTESIAN_POINT('Ctrl Pts',(128.064286310647,31.4007913138103,29.8498315414101));
#40397=CARTESIAN_POINT('Ctrl Pts',(127.961509692585,31.4599742562271,29.8440532691753));
#40398=CARTESIAN_POINT('Ctrl Pts',(127.858568541823,31.5192519432417,29.8382657466387));
#40399=CARTESIAN_POINT('Ctrl Pts',(127.758326370728,31.5829594952617,29.8324782241021));
#40400=CARTESIAN_POINT('Ctrl Pts',(127.661173674137,31.6508036161713,29.8266907015654));
#40401=CARTESIAN_POINT('Ctrl Pts',(127.568700420687,31.7153799666809,29.8211819400266));
#40402=CARTESIAN_POINT('Ctrl Pts',(127.479026186404,31.7837034796188,29.8156731784877));
#40403=CARTESIAN_POINT('Ctrl Pts',(127.392457758307,31.855489154449,29.8101644169488));
#40404=CARTESIAN_POINT('Ctrl Pts',(127.302025752593,31.9304786477225,29.8044097975579));
#40405=CARTESIAN_POINT('Ctrl Pts',(127.214671299808,32.0095052659351,29.798655178167));
#40406=CARTESIAN_POINT('Ctrl Pts',(127.130781969864,32.0922839038963,29.7929005587761));
#40407=CARTESIAN_POINT('Ctrl Pts',(127.046997055345,32.1749595088883,29.7871531020486));
#40408=CARTESIAN_POINT('Ctrl Pts',(126.966668984812,32.2613775576429,29.7814056453211));
#40409=CARTESIAN_POINT('Ctrl Pts',(126.890153096931,32.351212118822,29.7756581885937));
#40410=CARTESIAN_POINT('Ctrl Pts',(126.812342378029,32.4425668946896,29.7698134712126));
#40411=CARTESIAN_POINT('Ctrl Pts',(126.73847439577,32.5374546098222,29.7639687538315));
#40412=CARTESIAN_POINT('Ctrl Pts',(126.668884897651,32.635492191829,29.7581240364504));
#40413=CARTESIAN_POINT('Ctrl Pts',(126.600566657509,32.7317388274777,29.7523860901166));
#40414=CARTESIAN_POINT('Ctrl Pts',(126.536372168709,32.8310208696339,29.7466481437828));
#40415=CARTESIAN_POINT('Ctrl Pts',(126.476578752887,32.9329422563966,29.7409101974491));
#40416=CARTESIAN_POINT('Ctrl Pts',(126.416805312543,33.0348295937833,29.7351741680191));
#40417=CARTESIAN_POINT('Ctrl Pts',(126.361430234331,33.1393541620145,29.7294381385891));
#40418=CARTESIAN_POINT('Ctrl Pts',(126.310686796147,33.2460920537632,29.7237021091591));
#40419=CARTESIAN_POINT('Ctrl Pts',(126.259947629509,33.3528209603905,29.7179665625841));
#40420=CARTESIAN_POINT('Ctrl Pts',(126.213839506695,33.461762441258,29.7122310160091));
#40421=CARTESIAN_POINT('Ctrl Pts',(126.172548779272,33.5724699117186,29.7064954694341));
#40422=CARTESIAN_POINT('Ctrl Pts',(126.129887861217,33.6868510965559,29.7005695946018));
#40423=CARTESIAN_POINT('Ctrl Pts',(126.092369808768,33.8031170769029,29.6946437197696));
#40424=CARTESIAN_POINT('Ctrl Pts',(126.060144907995,33.9207563509546,29.6887178449374));
#40425=CARTESIAN_POINT('Ctrl Pts',(126.028921947958,34.0347379696549,29.6829762181632));
#40426=CARTESIAN_POINT('Ctrl Pts',(126.002667911715,34.1500083207628,29.677234591389));
#40427=CARTESIAN_POINT('Ctrl Pts',(125.981467580148,34.2660911564792,29.6714929646148));
#40428=CARTESIAN_POINT('Ctrl Pts',(125.959246774748,34.3877616168948,29.6654749657536));
#40429=CARTESIAN_POINT('Ctrl Pts',(125.942578397506,34.5103242084155,29.6594569668924));
#40430=CARTESIAN_POINT('Ctrl Pts',(125.931498882735,34.6332253296512,29.6534389680311));
#40431=CARTESIAN_POINT('Ctrl Pts',(125.920419367963,34.7561264508869,29.6474209691699));
#40432=CARTESIAN_POINT('Ctrl Pts',(125.914928674105,34.8793655759917,29.6414029703087));
#40433=CARTESIAN_POINT('Ctrl Pts',(125.915000700078,35.0023915761614,29.6353849714475));
#40434=CARTESIAN_POINT('Ctrl Pts',(125.915000700078,35.0023915770396,29.6353849714045));
#40435=CARTESIAN_POINT('Ctrl Pts',(125.915089665438,35.1543513193162,29.6279516357298));
#40436=CARTESIAN_POINT('Ctrl Pts',(125.923657514619,35.3060550304906,29.6205183000551));
#40437=CARTESIAN_POINT('Ctrl Pts',(125.940621235519,35.4568030718808,29.6130849643803));
#40438=CARTESIAN_POINT('Ctrl Pts',(125.953900081771,35.5748054887038,29.6072663045385));
#40439=CARTESIAN_POINT('Ctrl Pts',(125.972350307904,35.6924218713687,29.6014476446966));
#40440=CARTESIAN_POINT('Ctrl Pts',(125.995942053243,35.8091631226211,29.5956289848548));
#40441=CARTESIAN_POINT('Ctrl Pts',(126.019503759575,35.9257557290356,29.5898177338229));
#40442=CARTESIAN_POINT('Ctrl Pts',(126.048193884333,36.0414750228149,29.584006482791));
#40443=CARTESIAN_POINT('Ctrl Pts',(126.081930799845,36.1558368149516,29.5781952317592));
#40444=CARTESIAN_POINT('Ctrl Pts',(126.115633595803,36.2700829482247,29.5723898578885));
#40445=CARTESIAN_POINT('Ctrl Pts',(126.154372914053,36.3829739208238,29.5665844840179));
#40446=CARTESIAN_POINT('Ctrl Pts',(126.198016172837,36.4940361367748,29.5607791101473));
#40447=CARTESIAN_POINT('Ctrl Pts',(126.243364900283,36.6094383844783,29.5547468768833));
#40448=CARTESIAN_POINT('Ctrl Pts',(126.294008557267,36.7228655953719,29.5487146436193));
#40449=CARTESIAN_POINT('Ctrl Pts',(126.34974131207,36.833803836618,29.5426824103553));
#40450=CARTESIAN_POINT('Ctrl Pts',(126.403316678513,36.940447711448,29.5368836819645));
#40451=CARTESIAN_POINT('Ctrl Pts',(126.461594280714,37.0447913246213,29.5310849535736));
#40452=CARTESIAN_POINT('Ctrl Pts',(126.524342668129,37.1463995693751,29.5252862251827));
#40453=CARTESIAN_POINT('Ctrl Pts',(126.58708145292,37.2479922646317,29.5194883841933));
#40454=CARTESIAN_POINT('Ctrl Pts',(126.654289447445,37.3468500758802,29.513690543204));
#40455=CARTESIAN_POINT('Ctrl Pts',(126.725690452848,37.442564633623,29.5078927022146));
#40456=CARTESIAN_POINT('Ctrl Pts',(126.797097465056,37.5382872436164,29.5020943734659));
#40457=CARTESIAN_POINT('Ctrl Pts',(126.872697944781,37.6308657464102,29.4962960447173));
#40458=CARTESIAN_POINT('Ctrl Pts',(126.952174179912,37.7199233023017,29.4904977159686));
#40459=CARTESIAN_POINT('Ctrl Pts',(127.031675949859,37.8090094713801,29.4846975242824));
#40460=CARTESIAN_POINT('Ctrl Pts',(127.115055679291,37.8945721387752,29.4788973325961));
#40461=CARTESIAN_POINT('Ctrl Pts',(127.201957902164,37.9762703873701,29.4730971409099));
#40462=CARTESIAN_POINT('Ctrl Pts',(127.288956415624,38.0580591603736,29.4672905224161));
#40463=CARTESIAN_POINT('Ctrl Pts',(127.379484914967,38.1359746871951,29.4614839039223));
#40464=CARTESIAN_POINT('Ctrl Pts',(127.473153764485,38.2097154238444,29.4556772854286));
#40465=CARTESIAN_POINT('Ctrl Pts',(127.566884071184,38.283504542617,29.4498668571473));
#40466=CARTESIAN_POINT('Ctrl Pts',(127.663758499734,38.3531131782535,29.4440564288661));
#40467=CARTESIAN_POINT('Ctrl Pts',(127.763358663228,38.4182832724397,29.4382460005849));
#40468=CARTESIAN_POINT('Ctrl Pts',(127.863102118224,38.4835471247119,29.4324272130302));
#40469=CARTESIAN_POINT('Ctrl Pts',(127.965578784413,38.5443594823737,29.4266084254756));
#40470=CARTESIAN_POINT('Ctrl Pts',(128.070345840423,38.6005082730676,29.420789637921));
#40471=CARTESIAN_POINT('Ctrl Pts',(128.099058511997,38.6158965243734,29.4191949292179));
#40472=CARTESIAN_POINT('Ctrl Pts',(128.12794310216,38.6309347754804,29.4176002205149));
#40473=CARTESIAN_POINT('Ctrl Pts',(128.156990257709,38.6456193012738,29.4160055118118));
#40474=CARTESIAN_POINT('Ctrl Pts',(128.263076081415,38.6992500263856,29.4101813275454));
#40475=CARTESIAN_POINT('Ctrl Pts',(128.371675713506,38.7483327447696,29.4043571432789));
#40476=CARTESIAN_POINT('Ctrl Pts',(128.482362553069,38.7926246294185,29.3985329590124));
#40477=CARTESIAN_POINT('Ctrl Pts',(128.592909718891,38.8368606229313,29.3927161241797));
#40478=CARTESIAN_POINT('Ctrl Pts',(128.70553847789,38.8763176567245,29.3868992893471));
#40479=CARTESIAN_POINT('Ctrl Pts',(128.819798047079,38.9107989401556,29.3810824545145));
#40480=CARTESIAN_POINT('Ctrl Pts',(128.933943197743,38.9452456943333,29.375271444609));
#40481=CARTESIAN_POINT('Ctrl Pts',(129.049715521187,38.9747264933347,29.3694604347034));
#40482=CARTESIAN_POINT('Ctrl Pts',(129.166645246435,38.9990930040086,29.3636494247979));
#40483=CARTESIAN_POINT('Ctrl Pts',(129.287984334121,39.0243783638176,29.3576192845665));
#40484=CARTESIAN_POINT('Ctrl Pts',(129.41056941624,39.0441559609298,29.3515891443351));
#40485=CARTESIAN_POINT('Ctrl Pts',(129.533858961883,39.058317081326,29.3455590041036));
#40486=CARTESIAN_POINT('Ctrl Pts',(129.65253432744,39.0719482138845,29.3397545452373));
#40487=CARTESIAN_POINT('Ctrl Pts',(129.771861932216,39.0803756644309,29.3339500863711));
#40488=CARTESIAN_POINT('Ctrl Pts',(129.891350147677,39.0835548495876,29.3281456275048));
#40489=CARTESIAN_POINT('Ctrl Pts',(130.010820609899,39.0867335623894,29.3223420310495));
#40490=CARTESIAN_POINT('Ctrl Pts',(130.130451227362,39.084665549682,29.3165384345942));
#40491=CARTESIAN_POINT('Ctrl Pts',(130.249748250667,39.0773583128404,29.3107348381389));
#40492=CARTESIAN_POINT('Ctrl Pts',(130.369055686952,39.0700504381781,29.3049307351099));
#40493=CARTESIAN_POINT('Ctrl Pts',(130.488029063686,39.0575024550998,29.2991266320808));
#40494=CARTESIAN_POINT('Ctrl Pts',(130.6061782799,39.0397738665644,29.2933225290518));
#40495=CARTESIAN_POINT('Ctrl Pts',(130.72436567581,39.0220395490693,29.287516550438));
#40496=CARTESIAN_POINT('Ctrl Pts',(130.84172797802,38.9991213572441,29.2817105718241));
#40497=CARTESIAN_POINT('Ctrl Pts',(130.957784456089,38.9711300577636,29.2759045932102));
#40498=CARTESIAN_POINT('Ctrl Pts',(131.073969195103,38.9431078234264,29.2700921980626));
#40499=CARTESIAN_POINT('Ctrl Pts',(131.188844832233,38.910001385947,29.264279802915));
#40500=CARTESIAN_POINT('Ctrl Pts',(131.301944849458,38.8719716694431,29.2584674077674));
#40501=CARTESIAN_POINT('Ctrl Pts',(131.415119015703,38.8339170204391,29.2526512019802));
#40502=CARTESIAN_POINT('Ctrl Pts',(131.526514863675,38.7909328108809,29.2468349961931));
#40503=CARTESIAN_POINT('Ctrl Pts',(131.635686482147,38.7432278493461,29.2410187904059));
#40504=CARTESIAN_POINT('Ctrl Pts',(131.745014202512,38.6954546756252,29.2351942681649));
#40505=CARTESIAN_POINT('Ctrl Pts',(131.852110980245,38.6429474561582,29.2293697459239));
#40506=CARTESIAN_POINT('Ctrl Pts',(131.956555965445,38.5859606459191,29.2235452236829));
#40507=CARTESIAN_POINT('Ctrl Pts',(131.984166159126,38.5708960943285,29.2220055022031));
#40508=CARTESIAN_POINT('Ctrl Pts',(132.011591202502,38.5555187329759,29.2204657807233));
#40509=CARTESIAN_POINT('Ctrl Pts',(132.038823681523,38.5398337525458,29.2189260592435));
#40510=CARTESIAN_POINT('Ctrl Pts',(132.141833725687,38.4805034754318,29.2131018822557));
#40511=CARTESIAN_POINT('Ctrl Pts',(132.242417367041,38.4165776982603,29.2072777052679));
#40512=CARTESIAN_POINT('Ctrl Pts',(132.34013773286,38.3482802139672,29.2014535282802));
#40513=CARTESIAN_POINT('Ctrl Pts',(132.389906217135,38.3134966532983,29.1984873046235));
#40514=CARTESIAN_POINT('Ctrl Pts',(132.438932345851,38.2775799219866,29.1955210809668));
#40515=CARTESIAN_POINT('Ctrl Pts',(132.487160689988,38.2405642567579,29.1925548573102));
#40516=CARTESIAN_POINT('Origin',(130.,35.,23.));
#40517=CARTESIAN_POINT('',(126.821241978387,36.1772436037332,17.9148965215314));
#40518=CARTESIAN_POINT('',(126.821241918358,36.1772434416438,17.5703600964394));
#40519=CARTESIAN_POINT('',(126.821241918358,36.1772434416438,23.));
#40520=CARTESIAN_POINT('',(133.378768828602,34.7273715616999,17.));
#40521=CARTESIAN_POINT('Ctrl Pts',(126.821241918358,36.1772434416438,17.5703600964394));
#40522=CARTESIAN_POINT('Ctrl Pts',(126.857212034457,36.2743688901323,17.564266760725));
#40523=CARTESIAN_POINT('Ctrl Pts',(126.897684533608,36.3699708793764,17.5581734250105));
#40524=CARTESIAN_POINT('Ctrl Pts',(126.942506728596,36.463605123598,17.5520800892961));
#40525=CARTESIAN_POINT('Ctrl Pts',(126.987285374674,36.5571483934848,17.5459926738213));
#40526=CARTESIAN_POINT('Ctrl Pts',(127.036405128703,36.6487273364925,17.5399052583465));
#40527=CARTESIAN_POINT('Ctrl Pts',(127.089664831134,36.737916645688,17.5338178428716));
#40528=CARTESIAN_POINT('Ctrl Pts',(127.142890869842,36.827049581227,17.5277342750538));
#40529=CARTESIAN_POINT('Ctrl Pts',(127.200251435528,36.9137955199106,17.521650707236));
#40530=CARTESIAN_POINT('Ctrl Pts',(127.261499337811,36.9977535347711,17.5155671394182));
#40531=CARTESIAN_POINT('Ctrl Pts',(127.322727742955,37.0816848231479,17.5094855081918));
#40532=CARTESIAN_POINT('Ctrl Pts',(127.387840773444,37.162829606467,17.5034038769654));
#40533=CARTESIAN_POINT('Ctrl Pts',(127.456548273972,37.240816453855,17.4973222457391));
#40534=CARTESIAN_POINT('Ctrl Pts',(127.525251681103,37.3187986550072,17.4912409768391));
#40535=CARTESIAN_POINT('Ctrl Pts',(127.597548849614,37.3936229736636,17.4851597079391));
#40536=CARTESIAN_POINT('Ctrl Pts',(127.673110352901,37.4649522576963,17.4790784390392));
#40537=CARTESIAN_POINT('Ctrl Pts',(127.748686906051,37.5362957486466,17.4729959589104));
#40538=CARTESIAN_POINT('Ctrl Pts',(127.827528775038,37.6041425282067,17.4669134787816));
#40539=CARTESIAN_POINT('Ctrl Pts',(127.909271498311,37.6681940324353,17.4608309986528));
#40540=CARTESIAN_POINT('Ctrl Pts',(127.99110242648,37.732314651762,17.4547419551932));
#40541=CARTESIAN_POINT('Ctrl Pts',(128.075840121827,37.7926315545442,17.4486529117336));
#40542=CARTESIAN_POINT('Ctrl Pts',(128.163089061849,37.8488880756887,17.442563868274));
#40543=CARTESIAN_POINT('Ctrl Pts',(128.250388792041,37.9051773454059,17.4364712802034));
#40544=CARTESIAN_POINT('Ctrl Pts',(128.34020230886,37.9574013112638,17.4303786921328));
#40545=CARTESIAN_POINT('Ctrl Pts',(128.432109016913,38.0053490525485,17.4242861040622));
#40546=CARTESIAN_POINT('Ctrl Pts',(128.524163516949,38.0533738969294,17.4181837187125));
#40547=CARTESIAN_POINT('Ctrl Pts',(128.618317543001,38.0971086033436,17.4120813333628));
#40548=CARTESIAN_POINT('Ctrl Pts',(128.714129913534,38.1363901516284,17.4059789480131));
#40549=CARTESIAN_POINT('Ctrl Pts',(128.775991314876,38.1617523424422,17.402038933721));
#40550=CARTESIAN_POINT('Ctrl Pts',(128.838543662247,38.1852591658188,17.3980989194289));
#40551=CARTESIAN_POINT('Ctrl Pts',(128.901665328744,38.2068779229052,17.3941589051368));
#40552=CARTESIAN_POINT('Ctrl Pts',(128.998656487735,38.2400967591959,17.3881047786563));
#40553=CARTESIAN_POINT('Ctrl Pts',(129.097334659593,38.2689724799459,17.3820506521758));
#40554=CARTESIAN_POINT('Ctrl Pts',(129.197271488593,38.2933314439143,17.3759965256953));
#40555=CARTESIAN_POINT('Ctrl Pts',(129.297075621052,38.317658063948,17.3699504379094));
#40556=CARTESIAN_POINT('Ctrl Pts',(129.398134670601,38.3374797432278,17.3639043501235));
#40557=CARTESIAN_POINT('Ctrl Pts',(129.50000249191,38.3526717039406,17.3578582623376));
#40558=CARTESIAN_POINT('Ctrl Pts',(129.601765401025,38.367848018673,17.3518184013299));
#40559=CARTESIAN_POINT('Ctrl Pts',(129.704334998244,38.3784040286015,17.3457785403222));
#40560=CARTESIAN_POINT('Ctrl Pts',(129.807253184598,38.3842656112741,17.3397386793146));
#40561=CARTESIAN_POINT('Ctrl Pts',(129.910101948709,38.3901232400856,17.3337028924236));
#40562=CARTESIAN_POINT('Ctrl Pts',(130.013298401426,38.3912927099096,17.3276671055327));
#40563=CARTESIAN_POINT('Ctrl Pts',(130.116378419083,38.3877516328786,17.3216313186417));
#40564=CARTESIAN_POINT('Ctrl Pts',(130.219422807154,38.3842117798201,17.3155976180191));
#40565=CARTESIAN_POINT('Ctrl Pts',(130.322350405517,38.3759646290582,17.3095639173966));
#40566=CARTESIAN_POINT('Ctrl Pts',(130.424697118526,38.363039907586,17.303530216774));
#40567=CARTESIAN_POINT('Ctrl Pts',(130.527036045825,38.350116169322,17.2974969751465));
#40568=CARTESIAN_POINT('Ctrl Pts',(130.628793743683,38.3325156220224,17.2914637335191));
#40569=CARTESIAN_POINT('Ctrl Pts',(130.729512283087,38.3103197566588,17.2854304918916));
#40570=CARTESIAN_POINT('Ctrl Pts',(130.830250313128,38.2881195960425,17.2793960827361));
#40571=CARTESIAN_POINT('Ctrl Pts',(130.929948360132,38.2613224445899,17.2733616735805));
#40572=CARTESIAN_POINT('Ctrl Pts',(131.028160713027,38.2300604654848,17.267327264425));
#40573=CARTESIAN_POINT('Ctrl Pts',(131.126487251052,38.1987621401049,17.2612858394534));
#40574=CARTESIAN_POINT('Ctrl Pts',(131.223324230169,38.1629887538537,17.2552444144819));
#40575=CARTESIAN_POINT('Ctrl Pts',(131.318243140881,38.1229217223651,17.2492029895103));
#40576=CARTESIAN_POINT('Ctrl Pts',(131.413218328448,38.082830935373,17.243157982614));
#40577=CARTESIAN_POINT('Ctrl Pts',(131.506272791327,38.0384416233783,17.2371129757177));
#40578=CARTESIAN_POINT('Ctrl Pts',(131.597001957699,37.9899815734557,17.2310679688214));
#40579=CARTESIAN_POINT('Ctrl Pts',(131.687895393117,37.9414337845353,17.2250120171809));
#40580=CARTESIAN_POINT('Ctrl Pts',(131.776454748566,37.8888007586748,17.2189560655405));
#40581=CARTESIAN_POINT('Ctrl Pts',(131.862303584688,37.8323542188361,17.2129001139001));
#40582=CARTESIAN_POINT('Ctrl Pts',(131.937061191894,37.7832002821719,17.2076265601229));
#40583=CARTESIAN_POINT('Ctrl Pts',(132.009763752858,37.731155332992,17.2023530063457));
#40584=CARTESIAN_POINT('Ctrl Pts',(132.08018436874,37.6764226225598,17.1970794525685));
#40585=CARTESIAN_POINT('Ctrl Pts',(132.163723907917,37.6114935481666,17.1908234684812));
#40586=CARTESIAN_POINT('Ctrl Pts',(132.244339475961,37.5425575647275,17.184567484394));
#40587=CARTESIAN_POINT('Ctrl Pts',(132.32163556536,37.4699014887554,17.1783115003068));
#40588=CARTESIAN_POINT('Ctrl Pts',(132.398818569831,37.397351709326,17.1720646687848));
#40589=CARTESIAN_POINT('Ctrl Pts',(132.472691470397,37.3210929417983,17.1658178372629));
#40590=CARTESIAN_POINT('Ctrl Pts',(132.542890861188,37.2414529061721,17.159571005741));
#40591=CARTESIAN_POINT('Ctrl Pts',(132.613003795704,37.161910953744,17.1533318677014));
#40592=CARTESIAN_POINT('Ctrl Pts',(132.679451961912,37.0789963218649,17.1470927296619));
#40593=CARTESIAN_POINT('Ctrl Pts',(132.741908352732,36.9930739192816,17.1408535916224));
#40594=CARTESIAN_POINT('Ctrl Pts',(132.804291895857,36.9072517346084,17.1346217307697));
#40595=CARTESIAN_POINT('Ctrl Pts',(132.862692703684,36.8184290914577,17.128389869917));
#40596=CARTESIAN_POINT('Ctrl Pts',(132.91682416608,36.7270037193567,17.1221580090643));
#40597=CARTESIAN_POINT('Ctrl Pts',(132.970918848672,36.6356404665325,17.1159303824704));
#40598=CARTESIAN_POINT('Ctrl Pts',(133.020749755062,36.5416783486704,17.1097027558765));
#40599=CARTESIAN_POINT('Ctrl Pts',(133.066073812794,36.4455436475593,17.1034751292826));
#40600=CARTESIAN_POINT('Ctrl Pts',(133.111376567789,36.3494541306691,17.0972504297323));
#40601=CARTESIAN_POINT('Ctrl Pts',(133.152176520114,36.2511944258449,17.091025730182));
#40602=CARTESIAN_POINT('Ctrl Pts',(133.188277021192,36.1512144451147,17.0848010306316));
#40603=CARTESIAN_POINT('Ctrl Pts',(133.224368111105,36.0512605285103,17.0785779538197));
#40604=CARTESIAN_POINT('Ctrl Pts',(133.255762053786,35.9495876065114,17.0723548770077));
#40605=CARTESIAN_POINT('Ctrl Pts',(133.28231094227,35.846664007002,17.0661318001958));
#40606=CARTESIAN_POINT('Ctrl Pts',(133.308865996869,35.7437165029613,17.0599072780425));
#40607=CARTESIAN_POINT('Ctrl Pts',(133.3305736438,35.6395181286387,17.0536827558892));
#40608=CARTESIAN_POINT('Ctrl Pts',(133.347336361986,35.5345505983788,17.0474582337359));
#40609=CARTESIAN_POINT('Ctrl Pts',(133.364100783892,35.4295723994877,17.041233078938));
#40610=CARTESIAN_POINT('Ctrl Pts',(133.375919219294,35.323825286508,17.0350079241402));
#40611=CARTESIAN_POINT('Ctrl Pts',(133.38274577431,35.2177982756766,17.0287827693424));
#40612=CARTESIAN_POINT('Ctrl Pts',(133.389577148137,35.1116964212249,17.0225532202575));
#40613=CARTESIAN_POINT('Ctrl Pts',(133.391409583697,35.00531467558,17.0163236711726));
#40614=CARTESIAN_POINT('Ctrl Pts',(133.3882492794,34.8991442458638,17.0100941220878));
#40615=CARTESIAN_POINT('Ctrl Pts',(133.386542334164,34.8417994169385,17.0067294147252));
#40616=CARTESIAN_POINT('Ctrl Pts',(133.383379756271,34.7845162190167,17.0033647073626));
#40617=CARTESIAN_POINT('Ctrl Pts',(133.378768828602,34.7273715616999,17.));
#40618=CARTESIAN_POINT('',(126.821241918358,36.1772434416438,17.));
#40619=CARTESIAN_POINT('Origin',(130.,35.,17.));
#40620=CARTESIAN_POINT('',(126.821241918358,36.1772434416438,16.));
#40621=CARTESIAN_POINT('',(126.821241918358,36.1772434416438,23.));
#40622=CARTESIAN_POINT('Origin',(130.,35.,16.));
#40623=CARTESIAN_POINT('',(129.213982665103,31.6996256275318,16.9983013856386));
#40624=CARTESIAN_POINT('Origin',(130.,35.,17.));
#40625=CARTESIAN_POINT('Ctrl Pts',(129.214786777099,31.7024485967492,16.9966190365833));
#40626=CARTESIAN_POINT('Ctrl Pts',(129.256053829841,31.6926220826116,16.9991917406743));
#40627=CARTESIAN_POINT('Ctrl Pts',(129.297500078023,31.6835714753038,17.0018012218908));
#40628=CARTESIAN_POINT('Ctrl Pts',(129.548086858706,31.6337588604023,17.0176889557332));
#40629=CARTESIAN_POINT('Ctrl Pts',(129.760512272923,31.6120146819001,17.0315845883753));
#40630=CARTESIAN_POINT('Ctrl Pts',(130.135243116705,31.6090921467174,17.0556509826498));
#40631=CARTESIAN_POINT('Ctrl Pts',(130.29681991899,31.6194001831478,17.0658890691968));
#40632=CARTESIAN_POINT('Ctrl Pts',(130.520207798137,31.6497984413332,17.0797091662821));
#40633=CARTESIAN_POINT('Ctrl Pts',(130.583104281854,31.6601711351688,17.0835647414702));
#40634=CARTESIAN_POINT('Ctrl Pts',(130.677489035867,31.6784846893831,17.0892993156514));
#40635=CARTESIAN_POINT('Ctrl Pts',(130.709214482815,31.6851138363018,17.0912181161196));
#40636=CARTESIAN_POINT('Ctrl Pts',(130.764319284931,31.6974555291198,17.0945368170202));
#40637=CARTESIAN_POINT('Ctrl Pts',(130.787741520862,31.702963862566,17.0959429544309));
#40638=CARTESIAN_POINT('Ctrl Pts',(130.840719066106,31.7160196622147,17.0991141296805));
#40639=CARTESIAN_POINT('Ctrl Pts',(130.870235354469,31.7237176676327,17.1008743302695));
#40640=CARTESIAN_POINT('Ctrl Pts',(130.950332475085,31.7457662628929,17.1056355540019));
#40641=CARTESIAN_POINT('Ctrl Pts',(131.000690775141,31.7608971289618,17.1086120847421));
#40642=CARTESIAN_POINT('Ctrl Pts',(131.238908929887,31.8385594907758,17.1226431799184));
#40643=CARTESIAN_POINT('Ctrl Pts',(131.421406384604,31.9162985684089,17.133216313784));
#40644=CARTESIAN_POINT('Ctrl Pts',(131.725430740833,32.0785638487485,17.1515544639106));
#40645=CARTESIAN_POINT('Ctrl Pts',(131.850152450992,32.1559128162313,17.159325683362));
#40646=CARTESIAN_POINT('Ctrl Pts',(132.030118336166,32.2843826609484,17.1714595483403));
#40647=CARTESIAN_POINT('Ctrl Pts',(132.089320185824,32.329663387505,17.1756172476579));
#40648=CARTESIAN_POINT('Ctrl Pts',(132.165497339867,32.3920124481424,17.1812605520124));
#40649=CARTESIAN_POINT('Ctrl Pts',(132.183855379003,32.4073655454486,17.1826440849071));
#40650=CARTESIAN_POINT('Ctrl Pts',(132.214046292267,32.433162819123,17.1849617166224));
#40651=CARTESIAN_POINT('Ctrl Pts',(132.225971876318,32.4434978415772,17.1858883880591));
#40652=CARTESIAN_POINT('Ctrl Pts',(132.248662271818,32.4634410634607,17.1876740525311));
#40653=CARTESIAN_POINT('Ctrl Pts',(132.259438741034,32.4730354553383,17.1885320010811));
#40654=CARTESIAN_POINT('Ctrl Pts',(132.289089160876,32.4997748000613,17.1909192311729));
#40655=CARTESIAN_POINT('Ctrl Pts',(132.30783102106,32.5170640099366,17.1924584541783));
#40656=CARTESIAN_POINT('Ctrl Pts',(132.388244092172,32.5929414102011,17.1991883157391));
#40657=CARTESIAN_POINT('Ctrl Pts',(132.447888831647,32.6536242931822,17.2045056416654));
#40658=CARTESIAN_POINT('Ctrl Pts',(132.638301290146,32.8625203523798,17.2224225312086));
#40659=CARTESIAN_POINT('Ctrl Pts',(132.758393696422,33.0199194313757,17.2352902026146));
#40660=CARTESIAN_POINT('Ctrl Pts',(132.921444906087,33.2774837773379,17.254725338315));
#40661=CARTESIAN_POINT('Ctrl Pts',(132.974470512632,33.3707576341683,17.2614776983359));
#40662=CARTESIAN_POINT('Ctrl Pts',(133.056883876579,33.5332079471359,17.2727195785379));
#40663=CARTESIAN_POINT('Ctrl Pts',(133.088556623231,33.6011300106074,17.2772753840721));
#40664=CARTESIAN_POINT('Ctrl Pts',(133.131415650891,33.7016093502931,17.2838090485015));
#40665=CARTESIAN_POINT('Ctrl Pts',(133.144397524753,33.7333719593913,17.2858453465296));
#40666=CARTESIAN_POINT('Ctrl Pts',(133.166618610394,33.7901883355841,17.2894377257179));
#40667=CARTESIAN_POINT('Ctrl Pts',(133.176048108349,33.8151640785858,17.2909999390836));
#40668=CARTESIAN_POINT('Ctrl Pts',(133.195419414843,33.8683661369843,17.2942929285406));
#40669=CARTESIAN_POINT('Ctrl Pts',(133.205284517565,33.8966180713018,17.2960211040488));
#40670=CARTESIAN_POINT('Ctrl Pts',(133.231105658644,33.9738357080404,17.3006914072849));
#40671=CARTESIAN_POINT('Ctrl Pts',(133.246322378529,34.0230412821123,17.3036098254026));
#40672=CARTESIAN_POINT('Ctrl Pts',(133.32887334135,34.3132540723406,17.3205224061402));
#40673=CARTESIAN_POINT('Ctrl Pts',(133.370475705977,34.5607707380538,17.3336730298819));
#40674=CARTESIAN_POINT('Ctrl Pts',(133.3910920424,34.9292245629098,17.3532786977632));
#40675=CARTESIAN_POINT('Ctrl Pts',(133.391489250819,35.0480822365796,17.3596215874846));
#40676=CARTESIAN_POINT('Ctrl Pts',(133.382391868143,35.2328396975454,17.3698126049527));
#40677=CARTESIAN_POINT('Ctrl Pts',(133.377198846605,35.2988576339488,17.3735208978539));
#40678=CARTESIAN_POINT('Ctrl Pts',(133.367621652711,35.3873630947391,17.3786313817447));
#40679=CARTESIAN_POINT('Ctrl Pts',(133.364937805755,35.4100234940586,17.3799521708365));
#40680=CARTESIAN_POINT('Ctrl Pts',(133.360059674416,35.4479299655111,17.3821848132151));
#40681=CARTESIAN_POINT('Ctrl Pts',(133.357989823929,35.4631917550789,17.3830900428655));
#40682=CARTESIAN_POINT('Ctrl Pts',(133.353490979985,35.4947470832102,17.3849757365669));
#40683=CARTESIAN_POINT('Ctrl Pts',(133.351047108622,35.5110378458802,17.3859569407812));
#40684=CARTESIAN_POINT('Ctrl Pts',(133.344091127534,35.5552092178813,17.3886371281077));
#40685=CARTESIAN_POINT('Ctrl Pts',(133.339349241684,35.5830516901481,17.3903478967372));
#40686=CARTESIAN_POINT('Ctrl Pts',(133.307519271215,35.7567977261702,17.4011439813479));
#40687=CARTESIAN_POINT('Ctrl Pts',(133.271224299842,35.9008385191964,17.4106199888271));
#40688=CARTESIAN_POINT('Ctrl Pts',(133.149206735442,36.2785475651372,17.4361683743766));
#40689=CARTESIAN_POINT('Ctrl Pts',(133.047002676611,36.5059859337552,17.4522420755618));
#40690=CARTESIAN_POINT('Ctrl Pts',(132.886706005581,36.7781607319369,17.4716546143215));
#40691=CARTESIAN_POINT('Ctrl Pts',(132.850861697118,36.8350792068487,17.4757307172299));
#40692=CARTESIAN_POINT('Ctrl Pts',(132.795064660788,36.918096088445,17.4817027646984));
#40693=CARTESIAN_POINT('Ctrl Pts',(132.776389620987,36.9450295238551,17.483644769349));
#40694=CARTESIAN_POINT('Ctrl Pts',(132.742022944406,36.9930899243442,17.4871194115867));
#40695=CARTESIAN_POINT('Ctrl Pts',(132.726470514619,37.0143127525817,17.4886571324941));
#40696=CARTESIAN_POINT('Ctrl Pts',(132.692444659841,37.0596282080693,17.4919488491056));
#40697=CARTESIAN_POINT('Ctrl Pts',(132.673891398734,37.0836581956447,17.49369958371));
#40698=CARTESIAN_POINT('Ctrl Pts',(132.621997465262,37.1490358758255,17.4984797980984));
#40699=CARTESIAN_POINT('Ctrl Pts',(132.58800326071,37.1898551219723,17.501483430422));
#40700=CARTESIAN_POINT('Ctrl Pts',(132.434371431055,37.3657547803364,17.5145418678149));
#40701=CARTESIAN_POINT('Ctrl Pts',(132.305015769537,37.4919612267376,17.5241999022469));
#40702=CARTESIAN_POINT('Ctrl Pts',(132.037011113224,37.714628667599,17.5426817072915));
#40703=CARTESIAN_POINT('Ctrl Pts',(131.900011104562,37.8122188774766,17.5514967832702));
#40704=CARTESIAN_POINT('Ctrl Pts',(131.70981897151,37.9274364229952,17.5636359301029));
#40705=CARTESIAN_POINT('Ctrl Pts',(131.662616984004,37.9544998130361,17.5666422126796));
#40706=CARTESIAN_POINT('Ctrl Pts',(131.580493160447,37.9989944457297,17.5718963707584));
#40707=CARTESIAN_POINT('Ctrl Pts',(131.545883218952,38.0169804634852,17.5741176902827));
#40708=CARTESIAN_POINT('Ctrl Pts',(131.494308721456,38.0426621619099,17.5774493246284));
#40709=CARTESIAN_POINT('Ctrl Pts',(131.477577550123,38.0508222064118,17.5785334219615));
#40710=CARTESIAN_POINT('Ctrl Pts',(131.447365767591,38.0652501352356,17.5804983809761));
#40711=CARTESIAN_POINT('Ctrl Pts',(131.433909895837,38.0715677502068,17.5813762555213));
#40712=CARTESIAN_POINT('Ctrl Pts',(131.403191513728,38.0857443797491,17.5833864630216));
#40713=CARTESIAN_POINT('Ctrl Pts',(131.385904250794,38.0935471827659,17.5845219643156));
#40714=CARTESIAN_POINT('Ctrl Pts',(131.331448069326,38.1175785448481,17.5881099995059));
#40715=CARTESIAN_POINT('Ctrl Pts',(131.294054099791,38.1332847973099,17.5905899529291));
#40716=CARTESIAN_POINT('Ctrl Pts',(131.056162769399,38.2282194003898,17.6064281276034));
#40717=CARTESIAN_POINT('Ctrl Pts',(130.848781323682,38.2888360148737,17.6204724988471));
#40718=CARTESIAN_POINT('Ctrl Pts',(130.440745680061,38.3669123578759,17.6471661438228));
#40719=CARTESIAN_POINT('Ctrl Pts',(130.241469432651,38.387044316396,17.6597903817292));
#40720=CARTESIAN_POINT('Ctrl Pts',(129.996506531816,38.3900475755061,17.6746051661624));
#40721=CARTESIAN_POINT('Ctrl Pts',(129.951449604967,38.3897017450249,17.6773027627754));
#40722=CARTESIAN_POINT('Ctrl Pts',(129.877902889586,38.3876703951481,17.6816632465928));
#40723=CARTESIAN_POINT('Ctrl Pts',(129.849404953391,38.386523234332,17.6833423620265));
#40724=CARTESIAN_POINT('Ctrl Pts',(129.793967616118,38.3835904615584,17.6865893445222));
#40725=CARTESIAN_POINT('Ctrl Pts',(129.767028459358,38.3818424087642,17.6881582385486));
#40726=CARTESIAN_POINT('Ctrl Pts',(129.703132675972,38.3769291443102,17.6918595795546));
#40727=CARTESIAN_POINT('Ctrl Pts',(129.666201066581,38.3734787799783,17.6939831299917));
#40728=CARTESIAN_POINT('Ctrl Pts',(129.54189455585,38.3598039193035,17.7010839038258));
#40729=CARTESIAN_POINT('Ctrl Pts',(129.454860058891,38.3467845966391,17.7059763365416));
#40730=CARTESIAN_POINT('Ctrl Pts',(129.10221998013,38.2799100549687,17.7256263531402));
#40731=CARTESIAN_POINT('Ctrl Pts',(128.843045855803,38.1976971015985,17.739581742613));
#40732=CARTESIAN_POINT('Ctrl Pts',(128.536169929559,38.0581022270475,17.7578433972716));
#40733=CARTESIAN_POINT('Ctrl Pts',(128.476728958214,38.0289325129175,17.761473224389));
#40734=CARTESIAN_POINT('Ctrl Pts',(128.378398813746,37.9770519101292,17.7676955224079));
#40735=CARTESIAN_POINT('Ctrl Pts',(128.33903808698,37.9552721714332,17.7702470670211));
#40736=CARTESIAN_POINT('Ctrl Pts',(128.283021334896,37.9228034683209,17.7739834723889));
#40737=CARTESIAN_POINT('Ctrl Pts',(128.26600578852,37.9127409573522,17.77513270959));
#40738=CARTESIAN_POINT('Ctrl Pts',(128.236261987666,37.8947983289512,17.7771685689308));
#40739=CARTESIAN_POINT('Ctrl Pts',(128.223496403707,37.8869818326433,17.7780512402675));
#40740=CARTESIAN_POINT('Ctrl Pts',(128.195387142569,37.8695132089198,17.7800150093219));
#40741=CARTESIAN_POINT('Ctrl Pts',(128.180069046386,37.8598225317122,17.781098428686));
#40742=CARTESIAN_POINT('Ctrl Pts',(128.13452235746,37.8304942363568,17.7843579676676));
#40743=CARTESIAN_POINT('Ctrl Pts',(128.104529426571,37.8104973827608,17.7865550862689));
#40744=CARTESIAN_POINT('Ctrl Pts',(127.950110117423,37.7039470079332,17.7981104116921));
#40745=CARTESIAN_POINT('Ctrl Pts',(127.831281128646,37.6096032713602,17.8078309064383));
#40746=CARTESIAN_POINT('Ctrl Pts',(127.620279360132,37.41768599197,17.8262053149537));
#40747=CARTESIAN_POINT('Ctrl Pts',(127.526789265926,37.3219619234952,17.8348348817654));
#40748=CARTESIAN_POINT('Ctrl Pts',(127.345742658711,37.1132124023311,17.8523761566041));
#40749=CARTESIAN_POINT('Ctrl Pts',(127.259176362926,36.9996606608383,17.861249438756));
#40750=CARTESIAN_POINT('Ctrl Pts',(127.156629279089,36.8459208960606,17.8723961566983));
#40751=CARTESIAN_POINT('Ctrl Pts',(127.133899662632,36.8104281557498,17.8749143843333));
#40752=CARTESIAN_POINT('Ctrl Pts',(127.097225695315,36.7507385372235,17.8790605106294));
#40753=CARTESIAN_POINT('Ctrl Pts',(127.082908338469,36.7267774603061,17.8807017188277));
#40754=CARTESIAN_POINT('Ctrl Pts',(127.055322243062,36.6792877698506,17.8839102545656));
#40755=CARTESIAN_POINT('Ctrl Pts',(127.042035574973,36.6557720338785,17.8854781361535));
#40756=CARTESIAN_POINT('Ctrl Pts',(127.013288075251,36.6034419352456,17.888922594587));
#40757=CARTESIAN_POINT('Ctrl Pts',(126.997960158449,36.5745574159066,17.8907944549291));
#40758=CARTESIAN_POINT('Ctrl Pts',(126.945863854365,36.4728580197233,17.8972879241734));
#40759=CARTESIAN_POINT('Ctrl Pts',(126.911306278239,36.3989391827768,17.9018351064256));
#40760=CARTESIAN_POINT('Ctrl Pts',(126.858898761487,36.2754044254345,17.9092032564979));
#40761=CARTESIAN_POINT('Ctrl Pts',(126.839493178286,36.2265249486466,17.9120613358438));
#40762=CARTESIAN_POINT('Ctrl Pts',(126.821241978387,36.177243603733,17.9148965215314));
#40763=CARTESIAN_POINT('Origin',(130.,35.,23.));
#40764=CARTESIAN_POINT('',(126.821241918361,36.1772434416541,19.1602707349979));
#40765=CARTESIAN_POINT('',(126.821241895921,36.1772433810614,18.8206074156906));
#40766=CARTESIAN_POINT('',(126.821241918358,36.1772434416438,23.));
#40767=CARTESIAN_POINT('',(126.610251067793,35.0026905576773,17.6410178032139));
#40768=CARTESIAN_POINT('Ctrl Pts',(126.821241895921,36.1772433810614,18.8206074156907));
#40769=CARTESIAN_POINT('Ctrl Pts',(126.87248024585,36.315595673116,18.8127842064404));
#40770=CARTESIAN_POINT('Ctrl Pts',(126.932707594695,36.450485456493,18.8049940225583));
#40771=CARTESIAN_POINT('Ctrl Pts',(127.037872295089,36.64992988607,18.7926712384784));
#40772=CARTESIAN_POINT('Ctrl Pts',(127.076553861729,36.7175360552938,18.7883412642631));
#40773=CARTESIAN_POINT('Ctrl Pts',(127.130542646606,36.8047801705939,18.7824702309081));
#40774=CARTESIAN_POINT('Ctrl Pts',(127.143788989377,36.8256712611168,18.7810422009026));
#40775=CARTESIAN_POINT('Ctrl Pts',(127.164997599031,36.8583240058767,18.7787719917869));
#40776=CARTESIAN_POINT('Ctrl Pts',(127.172807439942,36.870184198587,18.7779393462207));
#40777=CARTESIAN_POINT('Ctrl Pts',(127.189337259138,36.8949465745617,18.7761831728303));
#40778=CARTESIAN_POINT('Ctrl Pts',(127.198071961823,36.9078382534364,18.7752586153802));
#40779=CARTESIAN_POINT('Ctrl Pts',(127.220391954919,36.940296781993,18.7729055925757));
#40780=CARTESIAN_POINT('Ctrl Pts',(127.234095108078,36.9597812493265,18.7714697071747));
#40781=CARTESIAN_POINT('Ctrl Pts',(127.292177676172,37.0405460258041,18.7654248830377));
#40782=CARTESIAN_POINT('Ctrl Pts',(127.338394516333,37.1004724244658,18.7607137757227));
#40783=CARTESIAN_POINT('Ctrl Pts',(127.482317041684,37.274704071611,18.7464417876623));
#40784=CARTESIAN_POINT('Ctrl Pts',(127.585661973826,37.3841089498847,18.7367066242889));
#40785=CARTESIAN_POINT('Ctrl Pts',(127.843966419205,37.6234829787011,18.7140370578109));
#40786=CARTESIAN_POINT('Ctrl Pts',(128.003984501788,37.747196078182,18.7012121749373));
#40787=CARTESIAN_POINT('Ctrl Pts',(128.218745600126,37.8845013835324,18.6856911020411));
#40788=CARTESIAN_POINT('Ctrl Pts',(128.2640760315,37.9120068540927,18.6824995257721));
#40789=CARTESIAN_POINT('Ctrl Pts',(128.336414869096,37.953610612944,18.6775354148027));
#40790=CARTESIAN_POINT('Ctrl Pts',(128.362998474652,37.9684267275989,18.6757377687823));
#40791=CARTESIAN_POINT('Ctrl Pts',(128.413061686458,37.9954518727168,18.6724006678971));
#40792=CARTESIAN_POINT('Ctrl Pts',(128.436491538058,38.0077477422027,18.6708582659369));
#40793=CARTESIAN_POINT('Ctrl Pts',(128.489529580288,38.034794592065,18.6674089100431));
#40794=CARTESIAN_POINT('Ctrl Pts',(128.519214766559,38.0493891695994,18.6655074397703));
#40795=CARTESIAN_POINT('Ctrl Pts',(128.610903412516,38.092812745173,18.6597190466952));
#40796=CARTESIAN_POINT('Ctrl Pts',(128.673571107819,38.1202030814715,18.6558802750143));
#40797=CARTESIAN_POINT('Ctrl Pts',(128.824331379956,38.1807324572684,18.64688316939));
#40798=CARTESIAN_POINT('Ctrl Pts',(128.913060165231,38.212136213326,18.6417758581226));
#40799=CARTESIAN_POINT('Ctrl Pts',(129.210781287315,38.3037565930303,18.6250582816421));
#40800=CARTESIAN_POINT('Ctrl Pts',(129.424236175831,38.3475605703756,18.6137674282016));
#40801=CARTESIAN_POINT('Ctrl Pts',(129.728487297146,38.3800196392524,18.5971371931572));
#40802=CARTESIAN_POINT('Ctrl Pts',(129.816897734108,38.3859596899436,18.59223721716));
#40803=CARTESIAN_POINT('Ctrl Pts',(129.931167798521,38.3891488672371,18.585705185037));
#40804=CARTESIAN_POINT('Ctrl Pts',(129.956910246894,38.3895738823913,18.5842206373326));
#40805=CARTESIAN_POINT('Ctrl Pts',(129.998628598167,38.3897873635103,18.5817901210079));
#40806=CARTESIAN_POINT('Ctrl Pts',(130.014603017186,38.3897561829211,18.5808535925426));
#40807=CARTESIAN_POINT('Ctrl Pts',(130.046312262046,38.3894701472027,18.5789819174312));
#40808=CARTESIAN_POINT('Ctrl Pts',(130.062046655227,38.389218625304,18.5780469586368));
#40809=CARTESIAN_POINT('Ctrl Pts',(130.102436035239,38.3882916411268,18.5756319814212));
#40810=CARTESIAN_POINT('Ctrl Pts',(130.127086084326,38.387456632403,18.5741437579073));
#40811=CARTESIAN_POINT('Ctrl Pts',(130.236230461578,38.3825664672057,18.5674971535528));
#40812=CARTESIAN_POINT('Ctrl Pts',(130.320559300819,38.3756184991256,18.5622105756659));
#40813=CARTESIAN_POINT('Ctrl Pts',(130.590813244682,38.343134227466,18.5449549781606));
#40814=CARTESIAN_POINT('Ctrl Pts',(130.774911066735,38.3053169292088,18.5327388934676));
#40815=CARTESIAN_POINT('Ctrl Pts',(131.119295622711,38.2042043830394,18.5097818407508));
#40816=CARTESIAN_POINT('Ctrl Pts',(131.27977958601,38.1435531476361,18.4990361545404));
#40817=CARTESIAN_POINT('Ctrl Pts',(131.475320558502,38.0521818814147,18.4859895638434));
#40818=CARTESIAN_POINT('Ctrl Pts',(131.515259546502,38.0325523535024,18.4833261619053));
#40819=CARTESIAN_POINT('Ctrl Pts',(131.580009801197,37.9991296790951,18.4790086222447));
#40820=CARTESIAN_POINT('Ctrl Pts',(131.605053872544,37.9858017253813,18.4773387763856));
#40821=CARTESIAN_POINT('Ctrl Pts',(131.653591430057,37.9591838044692,18.47410165509));
#40822=CARTESIAN_POINT('Ctrl Pts',(131.677099256104,37.9459245667767,18.4725334619888));
#40823=CARTESIAN_POINT('Ctrl Pts',(131.732712118216,37.9136754975161,18.4688212471967));
#40824=CARTESIAN_POINT('Ctrl Pts',(131.764667350311,37.8944335349394,18.4666863555279));
#40825=CARTESIAN_POINT('Ctrl Pts',(131.877453359147,37.8239567092158,18.4591374887046));
#40826=CARTESIAN_POINT('Ctrl Pts',(131.956427564045,37.7698295925829,18.4538275268168));
#40827=CARTESIAN_POINT('Ctrl Pts',(132.159302616883,37.617771402432,18.439991554405));
#40828=CARTESIAN_POINT('Ctrl Pts',(132.278833958426,37.5144052792231,18.4316396574227));
#40829=CARTESIAN_POINT('Ctrl Pts',(132.523367481538,37.271128920475,18.4133518658377));
#40830=CARTESIAN_POINT('Ctrl Pts',(132.644838726892,37.1284321186654,18.4034405792336));
#40831=CARTESIAN_POINT('Ctrl Pts',(132.774104647215,36.9483194160737,18.3909149737066));
#40832=CARTESIAN_POINT('Ctrl Pts',(132.793870030508,36.9198685370061,18.3889355758593));
#40833=CARTESIAN_POINT('Ctrl Pts',(132.823265666583,36.8761401540952,18.3858839425556));
#40834=CARTESIAN_POINT('Ctrl Pts',(132.833216153357,36.8610795518944,18.3848312703753));
#40835=CARTESIAN_POINT('Ctrl Pts',(132.851183787997,36.8334065020716,18.3828926576297));
#40836=CARTESIAN_POINT('Ctrl Pts',(132.859238491519,36.8208194904161,18.3820091395464));
#40837=CARTESIAN_POINT('Ctrl Pts',(132.877759974971,36.7914501869744,18.3799437546177));
#40838=CARTESIAN_POINT('Ctrl Pts',(132.888163360505,36.7746291464406,18.378758040084));
#40839=CARTESIAN_POINT('Ctrl Pts',(132.921850621045,36.7190799866892,18.3748357670751));
#40840=CARTESIAN_POINT('Ctrl Pts',(132.94450642991,36.6799787255777,18.3720644432014));
#40841=CARTESIAN_POINT('Ctrl Pts',(132.998624479861,36.5821181130448,18.3651244156822));
#40842=CARTESIAN_POINT('Ctrl Pts',(133.029147782316,36.5228622104135,18.3609187463534));
#40843=CARTESIAN_POINT('Ctrl Pts',(133.177029559179,36.2137125720987,18.3390896502157));
#40844=CARTESIAN_POINT('Ctrl Pts',(133.265305735195,35.9510135113245,18.3210225740503));
#40845=CARTESIAN_POINT('Ctrl Pts',(133.337662414383,35.5979305862962,18.2986410848175));
#40846=CARTESIAN_POINT('Ctrl Pts',(133.351500474047,35.5147405082691,18.2934893926472));
#40847=CARTESIAN_POINT('Ctrl Pts',(133.3664294725,35.3983108026939,18.2864478760855));
#40848=CARTESIAN_POINT('Ctrl Pts',(133.370155552454,35.3654456968944,18.2844786248739));
#40849=CARTESIAN_POINT('Ctrl Pts',(133.376058769605,35.3055597069388,18.2809226777195));
#40850=CARTESIAN_POINT('Ctrl Pts',(133.378393897172,35.2785575155212,18.2793312477473));
#40851=CARTESIAN_POINT('Ctrl Pts',(133.382467060372,35.2238166823131,18.2761281486082));
#40852=CARTESIAN_POINT('Ctrl Pts',(133.384188303239,35.1960788540938,18.274517114199));
#40853=CARTESIAN_POINT('Ctrl Pts',(133.387630458186,35.1268447406939,18.2705242179988));
#40854=CARTESIAN_POINT('Ctrl Pts',(133.388930281703,35.085331514346,18.2681553830466));
#40855=CARTESIAN_POINT('Ctrl Pts',(133.39121103627,34.9088494569434,18.2581801986537));
#40856=CARTESIAN_POINT('Ctrl Pts',(133.384893898044,34.773904426956,18.2507957250303));
#40857=CARTESIAN_POINT('Ctrl Pts',(133.355829856776,34.5020268851899,18.2360960643925));
#40858=CARTESIAN_POINT('Ctrl Pts',(133.332694452756,34.3653980004879,18.2288011249671));
#40859=CARTESIAN_POINT('Ctrl Pts',(133.263075714489,34.066697281545,18.2125024725059));
#40860=CARTESIAN_POINT('Ctrl Pts',(133.212737920476,33.9059160707499,18.203491929951));
#40861=CARTESIAN_POINT('Ctrl Pts',(133.140089443307,33.7228673456335,18.1922828968995));
#40862=CARTESIAN_POINT('Ctrl Pts',(133.129159010321,33.6963154900323,18.1906324624966));
#40863=CARTESIAN_POINT('Ctrl Pts',(133.111371025662,33.6546183926077,18.187996918356));
#40864=CARTESIAN_POINT('Ctrl Pts',(133.104736852428,33.6393786784438,18.1870243375158));
#40865=CARTESIAN_POINT('Ctrl Pts',(133.091756152517,33.6101493121529,18.1851398192257));
#40866=CARTESIAN_POINT('Ctrl Pts',(133.08542617895,33.596153035037,18.1842288214532));
#40867=CARTESIAN_POINT('Ctrl Pts',(133.069542392545,33.5616585886085,18.1819630452997));
#40868=CARTESIAN_POINT('Ctrl Pts',(133.059878228435,33.5412122559957,18.1806019539656));
#40869=CARTESIAN_POINT('Ctrl Pts',(133.021778943699,33.4626506641772,18.1753064284028));
#40870=CARTESIAN_POINT('Ctrl Pts',(132.991888301063,33.4052604415645,18.1712980687489));
#40871=CARTESIAN_POINT('Ctrl Pts',(132.904593433789,33.2487560246889,18.160042703045));
#40872=CARTESIAN_POINT('Ctrl Pts',(132.843781303579,33.1516429017063,18.1526878848765));
#40873=CARTESIAN_POINT('Ctrl Pts',(132.631458231587,32.8479305530217,18.1288191297898));
#40874=CARTESIAN_POINT('Ctrl Pts',(132.461408326268,32.6553285333291,18.1123734291639));
#40875=CARTESIAN_POINT('Ctrl Pts',(132.233805168996,32.4498890057896,18.0937501968404));
#40876=CARTESIAN_POINT('Ctrl Pts',(132.195593123958,32.4169160178009,18.0907182864872));
#40877=CARTESIAN_POINT('Ctrl Pts',(132.133794797976,32.3659531135047,18.0859603433323));
#40878=CARTESIAN_POINT('Ctrl Pts',(132.110685336914,32.3473992512977,18.0842120789908));
#40879=CARTESIAN_POINT('Ctrl Pts',(132.066359913357,32.3127578375997,18.0809159306526));
#40880=CARTESIAN_POINT('Ctrl Pts',(132.045192050467,32.2966126309671,18.0793658686812));
#40881=CARTESIAN_POINT('Ctrl Pts',(131.996184423646,32.2601385210175,18.0758306015773));
#40882=CARTESIAN_POINT('Ctrl Pts',(131.968220136515,32.2399813776653,18.0738520336952));
#40883=CARTESIAN_POINT('Ctrl Pts',(131.877339669921,32.1765569597681,18.0675401299282));
#40884=CARTESIAN_POINT('Ctrl Pts',(131.813265558445,32.1349862074306,18.0632690241334));
#40885=CARTESIAN_POINT('Ctrl Pts',(131.653357551499,32.0387547600556,18.0529816333626));
#40886=CARTESIAN_POINT('Ctrl Pts',(131.556154469199,31.9865385307356,18.0470404414384));
#40887=CARTESIAN_POINT('Ctrl Pts',(131.264104201861,31.8475597544215,18.0297869175985));
#40888=CARTESIAN_POINT('Ctrl Pts',(131.063437966269,31.7743331077711,18.0186943680113));
#40889=CARTESIAN_POINT('Ctrl Pts',(130.790473298534,31.7029832373987,18.003195016087));
#40890=CARTESIAN_POINT('Ctrl Pts',(130.72319256574,31.6875750852163,17.9993403335762));
#40891=CARTESIAN_POINT('Ctrl Pts',(130.632160906495,31.6696331739001,17.9940233385062));
#40892=CARTESIAN_POINT('Ctrl Pts',(130.608781531844,31.6652802837068,17.9926488624029));
#40893=CARTESIAN_POINT('Ctrl Pts',(130.571551987399,31.6587532444534,17.9904432298382));
#40894=CARTESIAN_POINT('Ctrl Pts',(130.557730357359,31.6564183292848,17.989620690504));
#40895=CARTESIAN_POINT('Ctrl Pts',(130.528428062453,31.6516549773845,17.9878683284136));
#40896=CARTESIAN_POINT('Ctrl Pts',(130.512944460081,31.6492480608296,17.9869372731682));
#40897=CARTESIAN_POINT('Ctrl Pts',(130.473115642621,31.6433392178584,17.9845301810449));
#40898=CARTESIAN_POINT('Ctrl Pts',(130.448748292474,31.639994805001,17.9830459200954));
#40899=CARTESIAN_POINT('Ctrl Pts',(130.340346950717,31.6263169313836,17.9763979586799));
#40900=CARTESIAN_POINT('Ctrl Pts',(130.255985054799,31.6188695819594,17.9711048865904));
#40901=CARTESIAN_POINT('Ctrl Pts',(129.983738169625,31.6050827755293,17.9538160869072));
#40902=CARTESIAN_POINT('Ctrl Pts',(129.795572970168,31.611204142361,17.9415699169901));
#40903=CARTESIAN_POINT('Ctrl Pts',(129.437554275498,31.6527907012639,17.9185000912174));
#40904=CARTESIAN_POINT('Ctrl Pts',(129.267974550023,31.685741688705,17.9076742440456));
#40905=CARTESIAN_POINT('Ctrl Pts',(129.058756573483,31.7432467112076,17.8945574509352));
#40906=CARTESIAN_POINT('Ctrl Pts',(129.016127209777,31.75587056552,17.891896477551));
#40907=CARTESIAN_POINT('Ctrl Pts',(128.946809468332,31.7778897900518,17.8875869577688));
#40908=CARTESIAN_POINT('Ctrl Pts',(128.919969596392,31.7867868260764,17.8859226090341));
#40909=CARTESIAN_POINT('Ctrl Pts',(128.867868723641,31.8047841156217,17.8826992466475));
#40910=CARTESIAN_POINT('Ctrl Pts',(128.842598396971,31.8138506995025,17.8811392774795));
#40911=CARTESIAN_POINT('Ctrl Pts',(128.782755637444,31.8361272520725,17.8774519681663));
#40912=CARTESIAN_POINT('Ctrl Pts',(128.748286211656,31.8496052075382,17.8753336019401));
#40913=CARTESIAN_POINT('Ctrl Pts',(128.626836571071,31.8994015414512,17.8678825385324));
#40914=CARTESIAN_POINT('Ctrl Pts',(128.541154632015,31.938781142968,17.8626508409049));
#40915=CARTESIAN_POINT('Ctrl Pts',(128.320114402638,32.0517634781844,17.8490983991985));
#40916=CARTESIAN_POINT('Ctrl Pts',(128.187938268294,32.1311065329734,17.8409428588115));
#40917=CARTESIAN_POINT('Ctrl Pts',(127.903307425618,32.3295090783609,17.8225563427342));
#40918=CARTESIAN_POINT('Ctrl Pts',(127.754731619268,32.4531597390088,17.8123579889865));
#40919=CARTESIAN_POINT('Ctrl Pts',(127.592922670229,32.6130401575447,17.7995059555737));
#40920=CARTESIAN_POINT('Ctrl Pts',(127.568721838565,32.6376950092199,17.7975319177641));
#40921=CARTESIAN_POINT('Ctrl Pts',(127.532494092718,32.6757488220761,17.7944887760614));
#40922=CARTESIAN_POINT('Ctrl Pts',(127.520189449006,32.688881539147,17.7934392115406));
#40923=CARTESIAN_POINT('Ctrl Pts',(127.497850604482,32.7131075244158,17.7915028825141));
#40924=CARTESIAN_POINT('Ctrl Pts',(127.487784409678,32.7241701314554,17.7906184884705));
#40925=CARTESIAN_POINT('Ctrl Pts',(127.464539050253,32.7500585961633,17.7885487090714));
#40926=CARTESIAN_POINT('Ctrl Pts',(127.451416408212,32.7649339646857,17.7873594230574));
#40927=CARTESIAN_POINT('Ctrl Pts',(127.40876029033,32.8141515543885,17.7834269456304));
#40928=CARTESIAN_POINT('Ctrl Pts',(127.379785658728,32.8489693060977,17.7806489412827));
#40929=CARTESIAN_POINT('Ctrl Pts',(127.309831191951,32.9365421781534,17.7736927242533));
#40930=CARTESIAN_POINT('Ctrl Pts',(127.269697128841,32.9899473311812,17.7694775166303));
#40931=CARTESIAN_POINT('Ctrl Pts',(127.078820544506,33.2602132837539,17.7484013821303));
#40932=CARTESIAN_POINT('Ctrl Pts',(126.952181650762,33.4930239990634,17.7311279219902));
#40933=CARTESIAN_POINT('Ctrl Pts',(126.819019163725,33.8250425217869,17.7088163251872));
#40934=CARTESIAN_POINT('Ctrl Pts',(126.787790788331,33.9133176097124,17.7030777165375));
#40935=CARTESIAN_POINT('Ctrl Pts',(126.749044769385,34.0391946533027,17.6951654139186));
#40936=CARTESIAN_POINT('Ctrl Pts',(126.738450107674,34.0757980185335,17.692895841337));
#40937=CARTESIAN_POINT('Ctrl Pts',(126.721411621202,34.1386109226143,17.689052750274));
#40938=CARTESIAN_POINT('Ctrl Pts',(126.714659686153,34.1647323873027,17.6874696153411));
#40939=CARTESIAN_POINT('Ctrl Pts',(126.70146453161,34.2184183036083,17.6842456706485));
#40940=CARTESIAN_POINT('Ctrl Pts',(126.695053272865,34.2459884712467,17.6826059764113));
#40941=CARTESIAN_POINT('Ctrl Pts',(126.682822066228,34.3017424608683,17.6793207038594));
#40942=CARTESIAN_POINT('Ctrl Pts',(126.677014194088,34.3299265414582,17.6776756166388));
#40943=CARTESIAN_POINT('Ctrl Pts',(126.663704420292,34.3989503009543,17.6736825629904));
#40944=CARTESIAN_POINT('Ctrl Pts',(126.656592556841,34.4398609086381,17.6713463499338));
#40945=CARTESIAN_POINT('Ctrl Pts',(126.623481629572,34.6535237469232,17.659285139113));
#40946=CARTESIAN_POINT('Ctrl Pts',(126.610113399899,34.8279690245501,17.6499298854475));
#40947=CARTESIAN_POINT('Ctrl Pts',(126.610251052227,35.0026708751785,17.6406473680219));
#40948=CARTESIAN_POINT('Ctrl Pts',(126.610251067793,35.0026905576773,17.6410178032139));
#40949=CARTESIAN_POINT('Ctrl Pts',(126.610355874084,35.1347327056219,17.6332712403869));
#40950=CARTESIAN_POINT('Ctrl Pts',(126.618179561376,35.2664475840005,17.6255246775599));
#40951=CARTESIAN_POINT('Ctrl Pts',(126.633586026562,35.3970667726449,17.6177781147329));
#40952=CARTESIAN_POINT('Ctrl Pts',(126.649300794567,35.5302998161686,17.6098765334033));
#40953=CARTESIAN_POINT('Ctrl Pts',(126.672904863042,35.6623931370086,17.6019749520736));
#40954=CARTESIAN_POINT('Ctrl Pts',(126.704205303174,35.7925543381198,17.594073370744));
#40955=CARTESIAN_POINT('Ctrl Pts',(126.70794873765,35.808121209563,17.5931283663978));
#40956=CARTESIAN_POINT('Ctrl Pts',(126.711802200231,35.8236604689481,17.5921833620516));
#40957=CARTESIAN_POINT('Ctrl Pts',(126.715765315128,35.8391707795115,17.5912383577054));
#40958=CARTESIAN_POINT('Ctrl Pts',(126.741359185109,35.9393366546373,17.5851355019987));
#40959=CARTESIAN_POINT('Ctrl Pts',(126.771582343066,36.0384975902312,17.5790326462921));
#40960=CARTESIAN_POINT('Ctrl Pts',(126.806339543602,36.1361945043616,17.5729297905854));
#40961=CARTESIAN_POINT('Ctrl Pts',(126.811217881386,36.149906729173,17.5720732258701));
#40962=CARTESIAN_POINT('Ctrl Pts',(126.816185454427,36.1635901266068,17.5712166611547));
#40963=CARTESIAN_POINT('Ctrl Pts',(126.821241918358,36.1772434416438,17.5703600964394));
#40964=CARTESIAN_POINT('Ctrl Pts',(126.821241978387,36.177243603733,17.9148965215314));
#40965=CARTESIAN_POINT('Ctrl Pts',(126.742546241387,35.9647517248556,17.9271213083101));
#40966=CARTESIAN_POINT('Ctrl Pts',(126.685311358021,35.7447864351744,17.9388787175516));
#40967=CARTESIAN_POINT('Ctrl Pts',(126.640195531105,35.4545256772944,17.9547792722127));
#40968=CARTESIAN_POINT('Ctrl Pts',(126.631880982833,35.3881405025059,17.9584446854921));
#40969=CARTESIAN_POINT('Ctrl Pts',(126.621238178706,35.2764532248012,17.9647213719342));
#40970=CARTESIAN_POINT('Ctrl Pts',(126.617845166975,35.2312706375423,17.9672906172474));
#40971=CARTESIAN_POINT('Ctrl Pts',(126.614272277592,35.1662673452647,17.9710470344894));
#40972=CARTESIAN_POINT('Ctrl Pts',(126.613358944124,35.1464901294407,17.9721979026875));
#40973=CARTESIAN_POINT('Ctrl Pts',(126.612060269939,35.1117712954401,17.9742339924007));
#40974=CARTESIAN_POINT('Ctrl Pts',(126.611600418236,35.0968333602536,17.9751152105004));
#40975=CARTESIAN_POINT('Ctrl Pts',(126.61080362177,35.0638614028776,17.9770721062152));
#40976=CARTESIAN_POINT('Ctrl Pts',(126.610511814138,35.0458276635016,17.9781500494998));
#40977=CARTESIAN_POINT('Ctrl Pts',(126.610071561826,34.9921342820039,17.9813805203113));
#40978=CARTESIAN_POINT('Ctrl Pts',(126.610341901981,34.9564747577097,17.9835535674568));
#40979=CARTESIAN_POINT('Ctrl Pts',(126.615219407709,34.7477020361011,17.9964122326283));
#40980=CARTESIAN_POINT('Ctrl Pts',(126.632524599149,34.5751536643685,18.0075755379586));
#40981=CARTESIAN_POINT('Ctrl Pts',(126.692217018682,34.2405378086125,18.0294866602718));
#40982=CARTESIAN_POINT('Ctrl Pts',(126.733577150869,34.0787502140273,18.0402038879868));
#40983=CARTESIAN_POINT('Ctrl Pts',(126.818119250642,33.8270600122975,18.0567902395979));
#40984=CARTESIAN_POINT('Ctrl Pts',(126.853633551103,33.7348777119108,18.0628493365591));
#40985=CARTESIAN_POINT('Ctrl Pts',(126.908200170215,33.6098202123117,18.0710429882789));
#40986=CARTESIAN_POINT('Ctrl Pts',(126.923851153912,33.5755230860111,18.0732875477297));
#40987=CARTESIAN_POINT('Ctrl Pts',(126.951712557756,33.517070223067,18.0771099676546));
#40988=CARTESIAN_POINT('Ctrl Pts',(126.963645872865,33.4927870980784,18.0786970237425));
#40989=CARTESIAN_POINT('Ctrl Pts',(126.988628967601,33.4434501732003,18.0819206478605));
#40990=CARTESIAN_POINT('Ctrl Pts',(127.001703758499,33.4184113756944,18.0835561967026));
#40991=CARTESIAN_POINT('Ctrl Pts',(127.035892868566,33.3548857959607,18.0877063705702));
#40992=CARTESIAN_POINT('Ctrl Pts',(127.05744490944,33.3166397834125,18.0902055783659));
#40993=CARTESIAN_POINT('Ctrl Pts',(127.158033903537,33.1459737895013,18.1013762506651));
#40994=CARTESIAN_POINT('Ctrl Pts',(127.24531105253,33.0186165773679,18.1097523459911));
#40995=CARTESIAN_POINT('Ctrl Pts',(127.361761445937,32.8713321806519,18.1197876019496));
#40996=CARTESIAN_POINT('Ctrl Pts',(127.382946724188,32.8453395766729,18.1215733837784));
#40997=CARTESIAN_POINT('Ctrl Pts',(127.527380692029,32.6734043649703,18.1335084875933));
#40998=CARTESIAN_POINT('Ctrl Pts',(127.662381895831,32.5378006275309,18.1435045424293));
#40999=CARTESIAN_POINT('Ctrl Pts',(127.859996595019,32.3702806282698,18.1577440844689));
#41000=CARTESIAN_POINT('Ctrl Pts',(127.913230917842,32.3278412987898,18.1615479663073));
#41001=CARTESIAN_POINT('Ctrl Pts',(127.986638331475,32.2728513773428,18.1668048627691));
#41002=CARTESIAN_POINT('Ctrl Pts',(128.005721201017,32.2588657780271,18.1681724601006));
#41003=CARTESIAN_POINT('Ctrl Pts',(128.036321696988,32.236927720345,18.1703698026233));
#41004=CARTESIAN_POINT('Ctrl Pts',(128.047745232028,32.2288446081433,18.171191040011));
#41005=CARTESIAN_POINT('Ctrl Pts',(128.072168384419,32.2117891373327,18.1729495671063));
#41006=CARTESIAN_POINT('Ctrl Pts',(128.085181247708,32.2028364948273,18.173888171196));
#41007=CARTESIAN_POINT('Ctrl Pts',(128.118876410211,32.1800000679827,18.1763217913346));
#41008=CARTESIAN_POINT('Ctrl Pts',(128.139649702765,32.1662529631809,18.177825228659));
#41009=CARTESIAN_POINT('Ctrl Pts',(128.233893786655,32.1053681125815,18.1846531334195));
#41010=CARTESIAN_POINT('Ctrl Pts',(128.30901250583,32.06085321654,18.1901140412535));
#41011=CARTESIAN_POINT('Ctrl Pts',(128.562546017882,31.9235489159507,18.2084097286551));
#41012=CARTESIAN_POINT('Ctrl Pts',(128.747499924802,31.8437250689561,18.221516927988));
#41013=CARTESIAN_POINT('Ctrl Pts',(129.086235515022,31.7320253942136,18.244250922917));
#41014=CARTESIAN_POINT('Ctrl Pts',(129.237225025532,31.6935202390104,18.2539748213305));
#41015=CARTESIAN_POINT('Ctrl Pts',(129.433609078563,31.6576144940119,18.2660366970994));
#41016=CARTESIAN_POINT('Ctrl Pts',(129.477025933926,31.6505466199134,18.2686683877804));
#41017=CARTESIAN_POINT('Ctrl Pts',(129.548562908793,31.6403260226463,18.2729490669459));
#41018=CARTESIAN_POINT('Ctrl Pts',(129.576605739499,31.6366769328558,18.2746132132756));
#41019=CARTESIAN_POINT('Ctrl Pts',(129.63157699661,31.6302222115512,18.2778492054007));
#41020=CARTESIAN_POINT('Ctrl Pts',(129.658499792333,31.6273874335503,18.279421837717));
#41021=CARTESIAN_POINT('Ctrl Pts',(129.722982761085,31.6213779237874,18.2831606566718));
#41022=CARTESIAN_POINT('Ctrl Pts',(129.760568002501,31.6185065187469,18.2853173810689));
#41023=CARTESIAN_POINT('Ctrl Pts',(129.896594485887,31.6103939202397,18.2930490414176));
#41024=CARTESIAN_POINT('Ctrl Pts',(129.995208673525,31.608820047677,18.2985129515031));
#41025=CARTESIAN_POINT('Ctrl Pts',(130.259959113656,31.6161456368023,18.3129483022094));
#41026=CARTESIAN_POINT('Ctrl Pts',(130.425602307241,31.6329664633323,18.3217237909728));
#41027=CARTESIAN_POINT('Ctrl Pts',(130.760475617407,31.6920881649874,18.3397647250944));
#41028=CARTESIAN_POINT('Ctrl Pts',(130.929013609413,31.7354134548875,18.3490111740306));
#41029=CARTESIAN_POINT('Ctrl Pts',(131.127200967488,31.8029555699515,18.3608338450197));
#41030=CARTESIAN_POINT('Ctrl Pts',(131.160748774204,31.814982389136,18.3628694454939));
#41031=CARTESIAN_POINT('Ctrl Pts',(131.210982991434,31.8338902892475,18.3659782457726));
#41032=CARTESIAN_POINT('Ctrl Pts',(131.227815254768,31.8403797420406,18.3670303206979));
#41033=CARTESIAN_POINT('Ctrl Pts',(131.258501465979,31.8524926272814,18.3689687542648));
#41034=CARTESIAN_POINT('Ctrl Pts',(131.272371144512,31.8580738001621,18.3698527063661));
#41035=CARTESIAN_POINT('Ctrl Pts',(131.304535273696,31.871264575023,18.3719206601585));
#41036=CARTESIAN_POINT('Ctrl Pts',(131.322800363333,31.8789430000731,18.3731085350634));
#41037=CARTESIAN_POINT('Ctrl Pts',(131.382696251912,31.9047427205764,18.3770461251084));
#41038=CARTESIAN_POINT('Ctrl Pts',(131.424028728645,31.9235396463993,18.3798309649126));
#41039=CARTESIAN_POINT('Ctrl Pts',(131.525477260062,31.9721581395079,18.3868134968949));
#41040=CARTESIAN_POINT('Ctrl Pts',(131.585108234746,32.002945082609,18.3910486898686));
#41041=CARTESIAN_POINT('Ctrl Pts',(131.890825315708,32.1724607189888,18.4133193928842));
#41042=CARTESIAN_POINT('Ctrl Pts',(132.119819874756,32.3398120099157,18.4318065454864));
#41043=CARTESIAN_POINT('Ctrl Pts',(132.382931237471,32.5878854709709,18.454201068933));
#41044=CARTESIAN_POINT('Ctrl Pts',(132.438552519559,32.6441305380867,18.4590234769016));
#41045=CARTESIAN_POINT('Ctrl Pts',(132.514053240739,32.7260200908385,18.4656985686129));
#41046=CARTESIAN_POINT('Ctrl Pts',(132.535607369955,32.750079179548,18.4676201817227));
#41047=CARTESIAN_POINT('Ctrl Pts',(132.574478959797,32.7947365278488,18.471116463134));
#41048=CARTESIAN_POINT('Ctrl Pts',(132.591901152447,32.8152397444662,18.4726953321628));
#41049=CARTESIAN_POINT('Ctrl Pts',(132.626974786088,32.8575260971522,18.4758993192026));
#41050=CARTESIAN_POINT('Ctrl Pts',(132.644603806424,32.8793251718146,18.477523471693));
#41051=CARTESIAN_POINT('Ctrl Pts',(132.688455542825,32.9349471654516,18.4816004990672));
#41052=CARTESIAN_POINT('Ctrl Pts',(132.71431232592,32.969053116442,18.4840390888703));
#41053=CARTESIAN_POINT('Ctrl Pts',(132.828963321908,33.1263836979172,18.4950279302835));
#41054=CARTESIAN_POINT('Ctrl Pts',(132.910064047675,33.2550055622229,18.5032906401355));
#41055=CARTESIAN_POINT('Ctrl Pts',(133.003568860762,33.428062806557,18.513815122184));
#41056=CARTESIAN_POINT('Ctrl Pts',(133.024083442999,33.4678995292755,18.5162003376815));
#41057=CARTESIAN_POINT('Ctrl Pts',(133.132772115783,33.689652903948,18.5293176883215));
#41058=CARTESIAN_POINT('Ctrl Pts',(133.205318101077,33.8787537201437,18.5398966152786));
#41059=CARTESIAN_POINT('Ctrl Pts',(133.275454673363,34.1254940731038,18.5541310903519));
#41060=CARTESIAN_POINT('Ctrl Pts',(133.289065123496,34.1781643232198,18.5571949839945));
#41061=CARTESIAN_POINT('Ctrl Pts',(133.306337299053,34.2523288043128,18.561573042761));
#41062=CARTESIAN_POINT('Ctrl Pts',(133.311068548516,34.2735679208276,18.5628340847204));
#41063=CARTESIAN_POINT('Ctrl Pts',(133.318754853112,34.3097087284038,18.5649944377829));
#41064=CARTESIAN_POINT('Ctrl Pts',(133.321814883292,34.3245877626973,18.5658880420751));
#41065=CARTESIAN_POINT('Ctrl Pts',(133.328071979391,34.3560836357715,18.5677892266493));
#41066=CARTESIAN_POINT('Ctrl Pts',(133.331244750567,34.3727044005923,18.5687980055136));
#41067=CARTESIAN_POINT('Ctrl Pts',(133.339727786571,34.4190236110607,18.5716232609083));
#41068=CARTESIAN_POINT('Ctrl Pts',(133.344766074707,34.4487695380154,18.573453546162));
#41069=CARTESIAN_POINT('Ctrl Pts',(133.375784942935,34.6480221962763,18.5858023000113));
#41070=CARTESIAN_POINT('Ctrl Pts',(133.389265015778,34.8192101094648,18.5968266613978));
#41071=CARTESIAN_POINT('Ctrl Pts',(133.390420937885,35.2389850114804,18.623882369893));
#41072=CARTESIAN_POINT('Ctrl Pts',(133.363816223294,35.486667187147,18.6398130228803));
#41073=CARTESIAN_POINT('Ctrl Pts',(133.299433756028,35.7789289146008,18.6580061864668));
#41074=CARTESIAN_POINT('Ctrl Pts',(133.287371268884,35.8283621941867,18.6610652605315));
#41075=CARTESIAN_POINT('Ctrl Pts',(133.266441994318,35.9064545728802,18.6658708893789));
#41076=CARTESIAN_POINT('Ctrl Pts',(133.258300210081,35.9352983600492,18.6676399863917));
#41077=CARTESIAN_POINT('Ctrl Pts',(133.242237231528,35.989447126699,18.67095104707));
#41078=CARTESIAN_POINT('Ctrl Pts',(133.234399629447,36.0147743482699,18.6724955426171));
#41079=CARTESIAN_POINT('Ctrl Pts',(133.215909066259,36.072134957112,18.6759851024794));
#41080=CARTESIAN_POINT('Ctrl Pts',(133.205073027559,36.1041066496398,18.6779241033504));
#41081=CARTESIAN_POINT('Ctrl Pts',(133.169539064105,36.2040149040705,18.6839686999769));
#41082=CARTESIAN_POINT('Ctrl Pts',(133.143144040371,36.2713285665895,18.6880194187991));
#41083=CARTESIAN_POINT('Ctrl Pts',(133.074418379635,36.4313390057888,18.6976408883267));
#41084=CARTESIAN_POINT('Ctrl Pts',(133.030021848069,36.523072290355,18.7031496040599));
#41085=CARTESIAN_POINT('Ctrl Pts',(132.959071284069,36.6542480354957,18.7111278680029));
#41086=CARTESIAN_POINT('Ctrl Pts',(132.935715629613,36.6953504833347,18.7136433451992));
#41087=CARTESIAN_POINT('Ctrl Pts',(132.805291792699,36.9140950918857,18.7271664321003));
#41088=CARTESIAN_POINT('Ctrl Pts',(132.682960009724,37.0820980196311,18.7380208971892));
#41089=CARTESIAN_POINT('Ctrl Pts',(132.51435251491,37.2739268041217,18.7522611643245));
#41090=CARTESIAN_POINT('Ctrl Pts',(132.481884300105,37.3093205768481,18.7549764757324));
#41091=CARTESIAN_POINT('Ctrl Pts',(132.43562723658,37.3576431369403,18.7588279989734));
#41092=CARTESIAN_POINT('Ctrl Pts',(132.422464293886,37.3711659382404,18.7599221570405));
#41093=CARTESIAN_POINT('Ctrl Pts',(132.398522361287,37.3953549798407,18.7619105862145));
#41094=CARTESIAN_POINT('Ctrl Pts',(132.387783216076,37.4060603283625,18.7628018996168));
#41095=CARTESIAN_POINT('Ctrl Pts',(132.365157085566,37.4283145770245,18.7646793874163));
#41096=CARTESIAN_POINT('Ctrl Pts',(132.353256762334,37.4398488292339,18.7656665265122));
#41097=CARTESIAN_POINT('Ctrl Pts',(132.320642396286,37.4709993515242,18.7683697897685));
#41098=CARTESIAN_POINT('Ctrl Pts',(132.299764975184,37.4904417016217,18.770097933796));
#41099=CARTESIAN_POINT('Ctrl Pts',(132.156781517908,37.6202657074694,18.781903085186));
#41100=CARTESIAN_POINT('Ctrl Pts',(132.027030599381,37.7218809890255,18.7924574440581));
#41101=CARTESIAN_POINT('Ctrl Pts',(131.673834989838,37.9591841060868,18.8198717167916));
#41102=CARTESIAN_POINT('Ctrl Pts',(131.441125990381,38.0792356839474,18.8366487595532));
#41103=CARTESIAN_POINT('Ctrl Pts',(131.150174562146,38.1890437212003,18.8555318610879));
#41104=CARTESIAN_POINT('Ctrl Pts',(131.103043680384,38.2056507009389,18.8585329874527));
#41105=CARTESIAN_POINT('Ctrl Pts',(131.027522097631,38.2303984271242,18.8632528745699));
#41106=CARTESIAN_POINT('Ctrl Pts',(130.999363862019,38.2392202167762,18.8649933376576));
#41107=CARTESIAN_POINT('Ctrl Pts',(130.945605667774,38.2552945622307,18.868280525615));
#41108=CARTESIAN_POINT('Ctrl Pts',(130.920028642327,38.2626155339666,18.8698293423279));
#41109=CARTESIAN_POINT('Ctrl Pts',(130.861011504662,38.2787589307017,18.8733696216589));
#41110=CARTESIAN_POINT('Ctrl Pts',(130.827516976007,38.2873723118489,18.8753543221127));
#41111=CARTESIAN_POINT('Ctrl Pts',(130.718830584855,38.3135554052211,18.8817203776833));
#41112=CARTESIAN_POINT('Ctrl Pts',(130.643166270144,38.3290697197368,18.8860377990188));
#41113=CARTESIAN_POINT('Ctrl Pts',(130.456433095637,38.3607526820474,18.8964725612023));
#41114=CARTESIAN_POINT('Ctrl Pts',(130.344964319985,38.3740171372746,18.9025115751598));
#41115=CARTESIAN_POINT('Ctrl Pts',(130.008601358767,38.3971962179771,18.9204871399848));
#41116=CARTESIAN_POINT('Ctrl Pts',(129.783202324511,38.3902800222877,18.9321782231361));
#41117=CARTESIAN_POINT('Ctrl Pts',(129.503449075565,38.3536718245008,18.9478013513118));
#41118=CARTESIAN_POINT('Ctrl Pts',(129.446927449652,38.3448150198062,18.9510179170686));
#41119=CARTESIAN_POINT('Ctrl Pts',(129.368811794962,38.3305404688155,18.9555799362431));
#41120=CARTESIAN_POINT('Ctrl Pts',(129.347003575775,38.3263334135453,18.9568662782091));
#41121=CARTESIAN_POINT('Ctrl Pts',(129.310425472703,38.3189035125199,18.9590475939386));
#41122=CARTESIAN_POINT('Ctrl Pts',(129.295632541086,38.3157955351844,18.9599363506415));
#41123=CARTESIAN_POINT('Ctrl Pts',(129.264560332171,38.3090499826678,18.961817842263));
#41124=CARTESIAN_POINT('Ctrl Pts',(129.248286507376,38.3053910649048,18.9628116548701));
#41125=CARTESIAN_POINT('Ctrl Pts',(129.203764717212,38.2950352391742,18.9655523172462));
#41126=CARTESIAN_POINT('Ctrl Pts',(129.175575370177,38.2880954609688,18.9673117239182));
#41127=CARTESIAN_POINT('Ctrl Pts',(128.968963945849,38.2344071168139,18.9803678973837));
#41128=CARTESIAN_POINT('Ctrl Pts',(128.794546970786,38.1735305746779,18.992258032739));
#41129=CARTESIAN_POINT('Ctrl Pts',(128.410956614533,38.0034418956255,19.0193064456423));
#41130=CARTESIAN_POINT('Ctrl Pts',(128.206424363278,37.8859729330732,19.0343583198718));
#41131=CARTESIAN_POINT('Ctrl Pts',(127.97346294431,37.7177683206549,19.051842332571));
#41132=CARTESIAN_POINT('Ctrl Pts',(127.931947756927,37.6863129848495,19.0549758765532));
#41133=CARTESIAN_POINT('Ctrl Pts',(127.867505825599,37.6351067140699,19.059870547961));
#41134=CARTESIAN_POINT('Ctrl Pts',(127.84409164397,37.6159851007693,19.0616556511919));
#41135=CARTESIAN_POINT('Ctrl Pts',(127.800848156695,37.5796945423823,19.0649662175627));
#41136=CARTESIAN_POINT('Ctrl Pts',(127.780956426011,37.5626038389947,19.0664946315759));
#41137=CARTESIAN_POINT('Ctrl Pts',(127.736316380893,37.5233401409695,19.0699385334073));
#41138=CARTESIAN_POINT('Ctrl Pts',(127.711691529643,37.501030477779,19.0718482369088));
#41139=CARTESIAN_POINT('Ctrl Pts',(127.636778639792,37.4311279729294,19.0776930075945));
#41140=CARTESIAN_POINT('Ctrl Pts',(127.587616103598,37.3823524623555,19.0815784721774));
#41141=CARTESIAN_POINT('Ctrl Pts',(127.474094213918,37.2626038158982,19.0907118047235));
#41142=CARTESIAN_POINT('Ctrl Pts',(127.411180981337,37.1903410253636,19.0959063479186));
#41143=CARTESIAN_POINT('Ctrl Pts',(127.268165118088,37.0112868643171,19.1081957732661));
#41144=CARTESIAN_POINT('Ctrl Pts',(127.191144049104,36.9022421973285,19.1152224965472));
#41145=CARTESIAN_POINT('Ctrl Pts',(127.040808513353,36.66028164785,19.1303671904146));
#41146=CARTESIAN_POINT('Ctrl Pts',(126.969589237825,36.5264178094058,19.1384873583599));
#41147=CARTESIAN_POINT('Ctrl Pts',(126.892808770643,36.3553840947005,19.1490687482448));
#41148=CARTESIAN_POINT('Ctrl Pts',(126.878577645659,36.3222804727807,19.1511261932591));
#41149=CARTESIAN_POINT('Ctrl Pts',(126.857989616,36.2722043574716,19.1542615354382));
#41150=CARTESIAN_POINT('Ctrl Pts',(126.851236298365,36.2553964710475,19.1553177519522));
#41151=CARTESIAN_POINT('Ctrl Pts',(126.839211380758,36.22476093345,19.1572512624016));
#41152=CARTESIAN_POINT('Ctrl Pts',(126.833895150909,36.21095173283,19.1581259722701));
#41153=CARTESIAN_POINT('Ctrl Pts',(126.826172897444,36.1904942512583,19.1594263879238));
#41154=CARTESIAN_POINT('Ctrl Pts',(126.823697025162,36.1838726487564,19.1598479919515));
#41155=CARTESIAN_POINT('Ctrl Pts',(126.821241918361,36.1772434416541,19.1602707349979));
#41156=CARTESIAN_POINT('Origin',(130.,35.,23.));
#41157=CARTESIAN_POINT('',(126.821241918623,36.1772434423597,20.4155867593643));
#41158=CARTESIAN_POINT('',(126.821241918282,36.1772434414401,20.0676575318486));
#41159=CARTESIAN_POINT('',(126.821241918358,36.1772434416438,23.));
#41160=CARTESIAN_POINT('Ctrl Pts',(126.821241918282,36.1772434414401,20.0676575318486));
#41161=CARTESIAN_POINT('Ctrl Pts',(126.838313316203,36.223339127512,20.0646699192867));
#41162=CARTESIAN_POINT('Ctrl Pts',(126.856386171251,36.2690602397116,20.0617137706984));
#41163=CARTESIAN_POINT('Ctrl Pts',(126.88719367022,36.3422963180723,20.0569885070641));
#41164=CARTESIAN_POINT('Ctrl Pts',(126.899313304811,36.3700601299697,20.0551994726895));
#41165=CARTESIAN_POINT('Ctrl Pts',(126.922717144669,36.4217720843826,20.051870578595));
#41166=CARTESIAN_POINT('Ctrl Pts',(126.933912790088,36.4457575562487,20.0503278929043));
#41167=CARTESIAN_POINT('Ctrl Pts',(126.959808776478,36.499582844253,20.0468678737414));
#41168=CARTESIAN_POINT('Ctrl Pts',(126.974669814071,36.5293425910029,20.0449561846332));
#41169=CARTESIAN_POINT('Ctrl Pts',(127.021899865511,36.6205388731543,20.0390980357143));
#41170=CARTESIAN_POINT('Ctrl Pts',(127.055721265314,36.6812050115015,20.0352015225534));
#41171=CARTESIAN_POINT('Ctrl Pts',(127.21935292679,36.954610185972,20.0175670034843));
#41172=CARTESIAN_POINT('Ctrl Pts',(127.370504130951,37.1536608253841,20.0045824710504));
#41173=CARTESIAN_POINT('Ctrl Pts',(127.641910865143,37.4394306972192,19.9835579244436));
#41174=CARTESIAN_POINT('Ctrl Pts',(127.748335192292,37.5379920054062,19.9757264785971));
#41175=CARTESIAN_POINT('Ctrl Pts',(127.882496567301,37.647144119824,19.9658745128229));
#41176=CARTESIAN_POINT('Ctrl Pts',(127.904485999794,37.6645850981208,19.9642602295987));
#41177=CARTESIAN_POINT('Ctrl Pts',(127.939721701358,37.6918264767577,19.9616697763209));
#41178=CARTESIAN_POINT('Ctrl Pts',(127.952827692047,37.7018071666238,19.9607054477949));
#41179=CARTESIAN_POINT('Ctrl Pts',(127.978176842652,37.7208211386307,19.9588376341886));
#41180=CARTESIAN_POINT('Ctrl Pts',(127.990408913683,37.7298681618174,19.957935087149));
#41181=CARTESIAN_POINT('Ctrl Pts',(128.021098991778,37.7522489627446,19.9556682852218));
#41182=CARTESIAN_POINT('Ctrl Pts',(128.039631072615,37.7654795533561,19.9542974387843));
#41183=CARTESIAN_POINT('Ctrl Pts',(128.108443954546,37.8135678359851,19.9492039622959));
#41184=CARTESIAN_POINT('Ctrl Pts',(128.159530009071,37.8472473567515,19.9454163695027));
#41185=CARTESIAN_POINT('Ctrl Pts',(128.378371716914,37.9831723539694,19.9292536977309));
#41186=CARTESIAN_POINT('Ctrl Pts',(128.553936282953,38.0721152533477,19.9164623009833));
#41187=CARTESIAN_POINT('Ctrl Pts',(128.897764879805,38.2102642207699,19.8926891645032));
#41188=CARTESIAN_POINT('Ctrl Pts',(129.064097228688,38.2626397742953,19.881699514965));
#41189=CARTESIAN_POINT('Ctrl Pts',(129.285170060892,38.3139419251281,19.8678891337791));
#41190=CARTESIAN_POINT('Ctrl Pts',(129.336877393315,38.3246746912017,19.8647123190013));
#41191=CARTESIAN_POINT('Ctrl Pts',(129.418409882472,38.3396202157039,19.8597842710571));
#41192=CARTESIAN_POINT('Ctrl Pts',(129.448074724989,38.3446507782061,19.8580079200008));
#41193=CARTESIAN_POINT('Ctrl Pts',(129.503982091926,38.3533674542995,19.8546903828047));
#41194=CARTESIAN_POINT('Ctrl Pts',(129.530208317651,38.3571420706641,19.8531465580247));
#41195=CARTESIAN_POINT('Ctrl Pts',(129.589760971225,38.3650016557467,19.8496679083141));
#41196=CARTESIAN_POINT('Ctrl Pts',(129.623109508572,38.3688998021047,19.8477389910857));
#41197=CARTESIAN_POINT('Ctrl Pts',(129.727362141837,38.3795185421538,19.8417640328731));
#41198=CARTESIAN_POINT('Ctrl Pts',(129.798425793449,38.3845008186541,19.837770994365));
#41199=CARTESIAN_POINT('Ctrl Pts',(130.116659500623,38.3967522467673,19.8201643971113));
#41200=CARTESIAN_POINT('Ctrl Pts',(130.36401463301,38.3792059167859,19.8072817520666));
#41201=CARTESIAN_POINT('Ctrl Pts',(130.749143077332,38.3090762602486,19.7863955276807));
#41202=CARTESIAN_POINT('Ctrl Pts',(130.889211108111,38.2742168663908,19.7786002792756));
#41203=CARTESIAN_POINT('Ctrl Pts',(131.053345896833,38.2220574163343,19.7687897292882));
#41204=CARTESIAN_POINT('Ctrl Pts',(131.079966213413,38.213232709006,19.7671766465327));
#41205=CARTESIAN_POINT('Ctrl Pts',(131.122040160227,38.1987032022382,19.7645876738518));
#41206=CARTESIAN_POINT('Ctrl Pts',(131.137567536321,38.1932141132004,19.7636236022546));
#41207=CARTESIAN_POINT('Ctrl Pts',(131.1673634614,38.1824360428259,19.7617559037374));
#41208=CARTESIAN_POINT('Ctrl Pts',(131.181637392499,38.1771637756751,19.7608532097101));
#41209=CARTESIAN_POINT('Ctrl Pts',(131.217193461896,38.1637579279225,19.75858546073));
#41210=CARTESIAN_POINT('Ctrl Pts',(131.238429816801,38.1555056135505,19.7572138024292));
#41211=CARTESIAN_POINT('Ctrl Pts',(131.316470494942,38.1242703795731,19.7521136189361));
#41212=CARTESIAN_POINT('Ctrl Pts',(131.372728919534,38.0999636022879,19.7483199184271));
#41213=CARTESIAN_POINT('Ctrl Pts',(131.628498753288,37.9811291799073,19.7306248670867));
#41214=CARTESIAN_POINT('Ctrl Pts',(131.819134171518,37.8687784602382,19.7161983189973));
#41215=CARTESIAN_POINT('Ctrl Pts',(132.087568468324,37.6729932815203,19.6949729183076));
#41216=CARTESIAN_POINT('Ctrl Pts',(132.174354804678,37.6028868133298,19.6879373289241));
#41217=CARTESIAN_POINT('Ctrl Pts',(132.31489246437,37.4774160618863,19.6762954007704));
#41218=CARTESIAN_POINT('Ctrl Pts',(132.37049516893,37.4242672157061,19.6716154379592));
#41219=CARTESIAN_POINT('Ctrl Pts',(132.448379216812,37.3445759730336,19.6649482415669));
#41220=CARTESIAN_POINT('Ctrl Pts',(132.472134907321,37.3195142627256,19.6628984280716));
#41221=CARTESIAN_POINT('Ctrl Pts',(132.513503416582,37.2745137862741,19.6592984039978));
#41222=CARTESIAN_POINT('Ctrl Pts',(132.531271939957,37.2547227800684,19.6577417481747));
#41223=CARTESIAN_POINT('Ctrl Pts',(132.568275239355,37.2125188107682,19.6544767718267));
#41224=CARTESIAN_POINT('Ctrl Pts',(132.587453801296,37.1900593825253,19.6527708188554));
#41225=CARTESIAN_POINT('Ctrl Pts',(132.638365249114,37.128836100136,19.6482022830898));
#41226=CARTESIAN_POINT('Ctrl Pts',(132.669537019233,37.0896140299767,19.6453619244202));
#41227=CARTESIAN_POINT('Ctrl Pts',(132.85702833402,36.8426554166803,19.6279691714365));
#41228=CARTESIAN_POINT('Ctrl Pts',(132.989885680575,36.6182040441577,19.6143479070092));
#41229=CARTESIAN_POINT('Ctrl Pts',(133.141860843739,36.2774617212924,19.5945150488444));
#41230=CARTESIAN_POINT('Ctrl Pts',(133.18273122213,36.1719287943705,19.5884639721829));
#41231=CARTESIAN_POINT('Ctrl Pts',(133.238413724641,36.0035958223691,19.5786863703352));
#41232=CARTESIAN_POINT('Ctrl Pts',(133.256841611507,35.9420773275853,19.5750872065185));
#41233=CARTESIAN_POINT('Ctrl Pts',(133.279358595488,35.8583237513932,19.5701073453748));
#41234=CARTESIAN_POINT('Ctrl Pts',(133.284989717365,35.8365135731561,19.5688033183606));
#41235=CARTESIAN_POINT('Ctrl Pts',(133.29408504791,35.7997771598081,19.5665922812221));
#41236=CARTESIAN_POINT('Ctrl Pts',(133.297666278472,35.7848801931986,19.5656916638655));
#41237=CARTESIAN_POINT('Ctrl Pts',(133.304919996886,35.7537803918626,19.5638022668399));
#41238=CARTESIAN_POINT('Ctrl Pts',(133.30857452461,35.7375741688122,19.5628126139723));
#41239=CARTESIAN_POINT('Ctrl Pts',(133.318220915109,35.6932818660515,19.560095236951));
#41240=CARTESIAN_POINT('Ctrl Pts',(133.323975084396,35.6651460794271,19.5583552909788));
#41241=CARTESIAN_POINT('Ctrl Pts',(133.361081287394,35.4711874685795,19.546281753768));
#41242=CARTESIAN_POINT('Ctrl Pts',(133.380366464866,35.3033109185356,19.5354479155878));
#41243=CARTESIAN_POINT('Ctrl Pts',(133.392592144583,34.9959244576744,19.5156240732214));
#41244=CARTESIAN_POINT('Ctrl Pts',(133.38957661798,34.8569204630671,19.5066632203482));
#41245=CARTESIAN_POINT('Ctrl Pts',(133.366891386618,34.584705020195,19.4893666414945));
#41246=CARTESIAN_POINT('Ctrl Pts',(133.347803882861,34.4516901609415,19.4810349002571));
#41247=CARTESIAN_POINT('Ctrl Pts',(133.312558489191,34.2795278009172,19.4704419343739));
#41248=CARTESIAN_POINT('Ctrl Pts',(133.303498608372,34.239065635466,19.4679657641418));
#41249=CARTESIAN_POINT('Ctrl Pts',(133.28713513935,34.1717979330685,19.4638700483873));
#41250=CARTESIAN_POINT('Ctrl Pts',(133.280240473037,34.1448984881648,19.4622378426566));
#41251=CARTESIAN_POINT('Ctrl Pts',(133.265965941213,34.0919219173324,19.4590334806381));
#41252=CARTESIAN_POINT('Ctrl Pts',(133.258602358757,34.0658425918495,19.4574609444333));
#41253=CARTESIAN_POINT('Ctrl Pts',(133.239769558168,34.0020772464524,19.4536266016018));
#41254=CARTESIAN_POINT('Ctrl Pts',(133.227954509137,33.9644969911269,19.4513760038306));
#41255=CARTESIAN_POINT('Ctrl Pts',(133.182615305874,33.8286113604183,19.4432629137138));
#41256=CARTESIAN_POINT('Ctrl Pts',(133.145231859928,33.7316503843303,19.4375236190794));
#41257=CARTESIAN_POINT('Ctrl Pts',(133.001643736974,33.4048179298836,19.4181281512654));
#41258=CARTESIAN_POINT('Ctrl Pts',(132.874208001904,33.1852299619745,19.4050647672162));
#41259=CARTESIAN_POINT('Ctrl Pts',(132.6849716892,32.9298488920332,19.3878357014475));
#41260=CARTESIAN_POINT('Ctrl Pts',(132.644936544191,32.8789369577672,19.3842823130487));
#41261=CARTESIAN_POINT('Ctrl Pts',(132.575117343171,32.7952016260257,19.378177452747));
#41262=CARTESIAN_POINT('Ctrl Pts',(132.546102549189,32.7617581393349,19.3756650870185));
#41263=CARTESIAN_POINT('Ctrl Pts',(132.503296450845,32.714327902328,19.371977315955));
#41264=CARTESIAN_POINT('Ctrl Pts',(132.490024432862,32.6998764505742,19.3708364209009));
#41265=CARTESIAN_POINT('Ctrl Pts',(132.46652399942,32.6747293889774,19.3688189032017));
#41266=CARTESIAN_POINT('Ctrl Pts',(132.456349846543,32.6639842737757,19.3679462246099));
#41267=CARTESIAN_POINT('Ctrl Pts',(132.433566691075,32.6402359734058,19.3659933978659));
#41268=CARTESIAN_POINT('Ctrl Pts',(132.420923784493,32.627267166686,19.3649108086282));
#41269=CARTESIAN_POINT('Ctrl Pts',(132.382828919204,32.5888117526327,19.3616537484923));
#41270=CARTESIAN_POINT('Ctrl Pts',(132.35707478753,32.5636296165956,19.3594582945023));
#41271=CARTESIAN_POINT('Ctrl Pts',(132.221046275514,32.4347979361299,19.347918580759));
#41272=CARTESIAN_POINT('Ctrl Pts',(132.104329592541,32.3382152625028,19.3382127669818));
#41273=CARTESIAN_POINT('Ctrl Pts',(131.873582654614,32.1719608252962,19.3198902792961));
#41274=CARTESIAN_POINT('Ctrl Pts',(131.761110457621,32.1005845308409,19.3112980290594));
#41275=CARTESIAN_POINT('Ctrl Pts',(131.519273404115,31.9663884424842,19.2937356517235));
#41276=CARTESIAN_POINT('Ctrl Pts',(131.389512599476,31.9048014737679,19.2848074402785));
#41277=CARTESIAN_POINT('Ctrl Pts',(131.21703212536,31.8359806477901,19.2736057126022));
#41278=CARTESIAN_POINT('Ctrl Pts',(131.177549883331,31.8210753125312,19.271084092216));
#41279=CARTESIAN_POINT('Ctrl Pts',(131.111503703831,31.7975409807139,19.2669344341869));
#41280=CARTESIAN_POINT('Ctrl Pts',(131.085093875232,31.7884963637949,19.2652930201818));
#41281=CARTESIAN_POINT('Ctrl Pts',(131.032938182203,31.7713513618545,19.2620855462872));
#41282=CARTESIAN_POINT('Ctrl Pts',(131.007201388366,31.7632301994539,19.260518913496));
#41283=CARTESIAN_POINT('Ctrl Pts',(130.950128104293,31.7459675809355,19.2570789735167));
#41284=CARTESIAN_POINT('Ctrl Pts',(130.918750827823,31.7369695956267,19.2552103495467));
#41285=CARTESIAN_POINT('Ctrl Pts',(130.808833596239,31.7071601493692,19.248738127973));
#41286=CARTESIAN_POINT('Ctrl Pts',(130.72967672223,31.6887193812411,19.2442083350159));
#41287=CARTESIAN_POINT('Ctrl Pts',(130.375379926847,31.6195046218141,19.2243840733658));
#41288=CARTESIAN_POINT('Ctrl Pts',(130.095267838498,31.6000627146817,19.2100006264721));
#41289=CARTESIAN_POINT('Ctrl Pts',(129.749159321002,31.6188819426312,19.1912383501271));
#41290=CARTESIAN_POINT('Ctrl Pts',(129.682485705748,31.6244905362487,19.1875727259415));
#41291=CARTESIAN_POINT('Ctrl Pts',(129.571009799945,31.6371997976817,19.1812958833176));
#41292=CARTESIAN_POINT('Ctrl Pts',(129.526103981189,31.6432337067365,19.1787267069632));
#41293=CARTESIAN_POINT('Ctrl Pts',(129.461771518752,31.6531944985399,19.1749704832532));
#41294=CARTESIAN_POINT('Ctrl Pts',(129.44223558273,31.6563947935735,19.1738197457957));
#41295=CARTESIAN_POINT('Ctrl Pts',(129.408000793346,31.6623113670737,19.1717837322616));
#41296=CARTESIAN_POINT('Ctrl Pts',(129.393290128869,31.6649540345882,19.1709024567523));
#41297=CARTESIAN_POINT('Ctrl Pts',(129.360859074363,31.6710017252495,19.1689450798905));
#41298=CARTESIAN_POINT('Ctrl Pts',(129.34314831837,31.6744509517548,19.1678667074907));
#41299=CARTESIAN_POINT('Ctrl Pts',(129.291571290214,31.6849238210788,19.1647003864993));
#41300=CARTESIAN_POINT('Ctrl Pts',(129.257784896839,31.6923244036375,19.162593565563));
#41301=CARTESIAN_POINT('Ctrl Pts',(129.040878762479,31.7433260956211,19.148882121011));
#41302=CARTESIAN_POINT('Ctrl Pts',(128.861558937872,31.8015972045417,19.1367083555732));
#41303=CARTESIAN_POINT('Ctrl Pts',(128.543161218256,31.9352477836216,19.1144553900244));
#41304=CARTESIAN_POINT('Ctrl Pts',(128.402697262378,32.006053317412,19.1043862980713));
#41305=CARTESIAN_POINT('Ctrl Pts',(128.185600072744,32.1351320462352,19.0886319858509));
#41306=CARTESIAN_POINT('Ctrl Pts',(128.105649233421,32.1873583046328,19.0827812912004));
#41307=CARTESIAN_POINT('Ctrl Pts',(127.997684446767,32.2645791948164,19.0748138624817));
#41308=CARTESIAN_POINT('Ctrl Pts',(127.967724402689,32.2867638106526,19.0725951371822));
#41309=CARTESIAN_POINT('Ctrl Pts',(127.916708904024,32.3258586460368,19.068802150162));
#41310=CARTESIAN_POINT('Ctrl Pts',(127.89547881506,32.3425342116142,19.067219076462));
#41311=CARTESIAN_POINT('Ctrl Pts',(127.852330015534,32.3772676416313,19.0639910175615));
#41312=CARTESIAN_POINT('Ctrl Pts',(127.830434449913,32.3953509294012,19.0623472121573));
#41313=CARTESIAN_POINT('Ctrl Pts',(127.774750041403,32.4425294494292,19.058149906065));
#41314=CARTESIAN_POINT('Ctrl Pts',(127.741302807031,32.4720205210908,19.0556125216747));
#41315=CARTESIAN_POINT('Ctrl Pts',(127.579358418923,32.6205908415125,19.0432273776828));
#41316=CARTESIAN_POINT('Ctrl Pts',(127.459639173474,32.7488514927911,19.0337718430185));
#41317=CARTESIAN_POINT('Ctrl Pts',(127.251122778964,33.0101769008517,19.0159734992701));
#41318=CARTESIAN_POINT('Ctrl Pts',(127.160767145408,33.1413779889753,19.0076257709077));
#41319=CARTESIAN_POINT('Ctrl Pts',(127.043624215135,33.3400702720867,18.9951759296494));
#41320=CARTESIAN_POINT('Ctrl Pts',(127.009248185643,33.4028378244243,18.9912669950647));
#41321=CARTESIAN_POINT('Ctrl Pts',(126.955399667325,33.5090036900048,18.984619844174));
#41322=CARTESIAN_POINT('Ctrl Pts',(126.934807447617,33.5518096346547,18.9819303912349));
#41323=CARTESIAN_POINT('Ctrl Pts',(126.906767773882,33.6133761243421,18.9780296576747));
#41324=CARTESIAN_POINT('Ctrl Pts',(126.8985771034,33.6317941125114,18.9768586467859));
#41325=CARTESIAN_POINT('Ctrl Pts',(126.88458751446,33.6640230359214,18.974800619948));
#41326=CARTESIAN_POINT('Ctrl Pts',(126.878715093955,33.6778011007988,18.9739179233641));
#41327=CARTESIAN_POINT('Ctrl Pts',(126.866067290281,33.7080296737048,18.9719745837945));
#41328=CARTESIAN_POINT('Ctrl Pts',(126.8593300736,33.7244946352306,18.9709119097829));
#41329=CARTESIAN_POINT('Ctrl Pts',(126.840325171231,33.7720039581988,18.9678352076368));
#41330=CARTESIAN_POINT('Ctrl Pts',(126.828386367307,33.8031766683817,18.9658038103239));
#41331=CARTESIAN_POINT('Ctrl Pts',(126.745805523571,34.0287164216908,18.9510412492212));
#41332=CARTESIAN_POINT('Ctrl Pts',(126.69262624817,34.2289997088213,18.9376151077583));
#41333=CARTESIAN_POINT('Ctrl Pts',(126.626335361854,34.6196328651339,18.9121062604779));
#41334=CARTESIAN_POINT('Ctrl Pts',(126.610349292147,34.8087500903616,18.9000496557075));
#41335=CARTESIAN_POINT('Ctrl Pts',(126.610221451071,35.0538508416271,18.8850414854699));
#41336=CARTESIAN_POINT('Ctrl Pts',(126.611561327143,35.1094642706032,18.8816749265113));
#41337=CARTESIAN_POINT('Ctrl Pts',(126.615917242948,35.1988338719619,18.8763258610371));
#41338=CARTESIAN_POINT('Ctrl Pts',(126.618071689148,35.232619947923,18.8743176435631));
#41339=CARTESIAN_POINT('Ctrl Pts',(126.622816080097,35.2928092606606,18.8707637878997));
#41340=CARTESIAN_POINT('Ctrl Pts',(126.625210499963,35.3192246571491,18.8692122757323));
#41341=CARTESIAN_POINT('Ctrl Pts',(126.630964759736,35.3753684772599,18.8659310449551));
#41342=CARTESIAN_POINT('Ctrl Pts',(126.634408632626,35.4050861321382,18.8642040567425));
#41343=CARTESIAN_POINT('Ctrl Pts',(126.644909116979,35.4862814016571,18.8595099690902));
#41344=CARTESIAN_POINT('Ctrl Pts',(126.652756686038,35.5376495456957,18.856567332348));
#41345=CARTESIAN_POINT('Ctrl Pts',(126.690907102404,35.7539373965398,18.8442657023842));
#41346=CARTESIAN_POINT('Ctrl Pts',(126.73224342609,35.9166743742564,18.8352430771744));
#41347=CARTESIAN_POINT('Ctrl Pts',(126.796850563314,36.1097421483453,18.8244143192971));
#41348=CARTESIAN_POINT('Ctrl Pts',(126.808780385848,36.1435951764742,18.8225100726071));
#41349=CARTESIAN_POINT('Ctrl Pts',(126.821241895921,36.1772433810614,18.8206074156907));
#41350=CARTESIAN_POINT('',(126.610251372965,35.0022124562256,19.2361965387239));
#41351=CARTESIAN_POINT('Ctrl Pts',(126.821241918361,36.1772434416541,19.1602707349979));
#41352=CARTESIAN_POINT('Ctrl Pts',(126.816884277129,36.1654770670927,19.1610210740581));
#41353=CARTESIAN_POINT('Ctrl Pts',(126.81259205494,36.1536867351834,19.1617750013141));
#41354=CARTESIAN_POINT('Ctrl Pts',(126.79345944527,36.1002094234563,19.1652030231718));
#41355=CARTESIAN_POINT('Ctrl Pts',(126.779371421115,36.0582600185024,19.1679151873821));
#41356=CARTESIAN_POINT('Ctrl Pts',(126.746713334263,35.9543155480196,19.174672025003));
#41357=CARTESIAN_POINT('Ctrl Pts',(126.729090018245,35.892042234783,19.1787514066441));
#41358=CARTESIAN_POINT('Ctrl Pts',(126.645037231307,35.5589208321272,19.2006150216373));
#41359=CARTESIAN_POINT('Ctrl Pts',(126.610433081745,35.281113965657,19.2188765528856));
#41360=CARTESIAN_POINT('Ctrl Pts',(126.610250724592,35.0022163872186,19.2361974238064));
#41361=CARTESIAN_POINT('Ctrl Pts',(126.61025072207,35.002212526495,19.2361976635757));
#41362=CARTESIAN_POINT('Ctrl Pts',(126.610215475997,34.9482130149684,19.2395512894302));
#41363=CARTESIAN_POINT('Ctrl Pts',(126.611470566056,34.8942177721856,19.242871423061));
#41364=CARTESIAN_POINT('Ctrl Pts',(126.615959719839,34.7990542651036,19.2486629964747));
#41365=CARTESIAN_POINT('Ctrl Pts',(126.618656662605,34.7578734542219,19.2511494081819));
#41366=CARTESIAN_POINT('Ctrl Pts',(126.624315581862,34.6903878890029,19.2551924379648));
#41367=CARTESIAN_POINT('Ctrl Pts',(126.626834801365,34.6640512652279,19.2567623423169));
#41368=CARTESIAN_POINT('Ctrl Pts',(126.632351176298,34.6127279931673,19.2598068611335));
#41369=CARTESIAN_POINT('Ctrl Pts',(126.635318749466,34.5877399604904,19.2612822844822));
#41370=CARTESIAN_POINT('Ctrl Pts',(126.64220756733,34.5347765169189,19.2643957347701));
#41371=CARTESIAN_POINT('Ctrl Pts',(126.64620082992,34.506812300338,19.2660314093717));
#41372=CARTESIAN_POINT('Ctrl Pts',(126.657283871333,34.4355741254906,19.2701791168379));
#41373=CARTESIAN_POINT('Ctrl Pts',(126.664864724642,34.3923811822919,19.2726757978637));
#41374=CARTESIAN_POINT('Ctrl Pts',(126.703952825049,34.1925282584387,19.2841595650102));
#41375=CARTESIAN_POINT('Ctrl Pts',(126.745675022395,34.0380675173494,19.2928265120144));
#41376=CARTESIAN_POINT('Ctrl Pts',(126.846191473988,33.7488743124589,19.3091736487917));
#41377=CARTESIAN_POINT('Ctrl Pts',(126.903141208669,33.6138945107815,19.3168610374973));
#41378=CARTESIAN_POINT('Ctrl Pts',(127.00896571753,33.4024266075271,19.32951259195));
#41379=CARTESIAN_POINT('Ctrl Pts',(127.052492408531,33.3234785901044,19.3343850312158));
#41380=CARTESIAN_POINT('Ctrl Pts',(127.118914203371,33.2136027453504,19.3415086168363));
#41381=CARTESIAN_POINT('Ctrl Pts',(127.139271258006,33.1811813274849,19.3436550925338));
#41382=CARTESIAN_POINT('Ctrl Pts',(127.176554363478,33.1239776239996,19.3475351285399));
#41383=CARTESIAN_POINT('Ctrl Pts',(127.193268909451,33.0990618967346,19.3492574520608));
#41384=CARTESIAN_POINT('Ctrl Pts',(127.219904039347,33.0604751456602,19.3519811636848));
#41385=CARTESIAN_POINT('Ctrl Pts',(127.229600213642,33.0466502596012,19.3529685483001));
#41386=CARTESIAN_POINT('Ctrl Pts',(127.24822240275,33.0205161538322,19.3548582693453));
#41387=CARTESIAN_POINT('Ctrl Pts',(127.257128544283,33.0081936879496,19.3557593455908));
#41388=CARTESIAN_POINT('Ctrl Pts',(127.27903030596,32.9783160342607,19.3579681317384));
#41389=CARTESIAN_POINT('Ctrl Pts',(127.29211316751,32.960825907217,19.3592815020715));
#41390=CARTESIAN_POINT('Ctrl Pts',(127.338673867667,32.8998183941126,19.363931200705));
#41391=CARTESIAN_POINT('Ctrl Pts',(127.373037585497,32.8569910574747,19.3673193409019));
#41392=CARTESIAN_POINT('Ctrl Pts',(127.538429896875,32.6608214414603,19.3833578502994));
#41393=CARTESIAN_POINT('Ctrl Pts',(127.681933424734,32.5185394030912,19.3964933842812));
#41394=CARTESIAN_POINT('Ctrl Pts',(127.868724280745,32.3637636657869,19.4120639340809));
#41395=CARTESIAN_POINT('Ctrl Pts',(127.900691026352,32.3382373999543,19.4146815651004));
#41396=CARTESIAN_POINT('Ctrl Pts',(128.056011306919,32.2187491707369,19.4271647980074));
#41397=CARTESIAN_POINT('Ctrl Pts',(128.185264214849,32.1327377679348,19.436844872648));
#41398=CARTESIAN_POINT('Ctrl Pts',(128.357316725156,32.0345580619004,19.4488028814114));
#41399=CARTESIAN_POINT('Ctrl Pts',(128.395068961342,32.0139573268592,19.4513741070718));
#41400=CARTESIAN_POINT('Ctrl Pts',(128.458100352968,31.9811030575805,19.4555826658498));
#41401=CARTESIAN_POINT('Ctrl Pts',(128.483157179875,31.9684358492142,19.4572341720212));
#41402=CARTESIAN_POINT('Ctrl Pts',(128.532503490119,31.9442543629499,19.4604457364178));
#41403=CARTESIAN_POINT('Ctrl Pts',(128.556778206111,31.932714829135,19.4620065706786));
#41404=CARTESIAN_POINT('Ctrl Pts',(128.610418075977,31.9079936926775,19.4654152814497));
#41405=CARTESIAN_POINT('Ctrl Pts',(128.639839081657,31.8949390819526,19.4672587930637));
#41406=CARTESIAN_POINT('Ctrl Pts',(128.741511200457,31.8515478495679,19.4735446997745));
#41407=CARTESIAN_POINT('Ctrl Pts',(128.814628140774,31.823297336191,19.4779189981552));
#41408=CARTESIAN_POINT('Ctrl Pts',(129.113363869955,31.7196261181302,19.4953116820124));
#41409=CARTESIAN_POINT('Ctrl Pts',(129.345642425038,31.6655142638856,19.5077026835536));
#41410=CARTESIAN_POINT('Ctrl Pts',(129.676644533757,31.6243512293255,19.525513086473));
#41411=CARTESIAN_POINT('Ctrl Pts',(129.772064593741,31.6165687833369,19.5306728352778));
#41412=CARTESIAN_POINT('Ctrl Pts',(129.90737668874,31.6112828082849,19.538173803025));
#41413=CARTESIAN_POINT('Ctrl Pts',(129.947095925998,31.6104300863342,19.5403981242804));
#41414=CARTESIAN_POINT('Ctrl Pts',(130.01768011138,31.610155626858,19.5444049381334));
#41415=CARTESIAN_POINT('Ctrl Pts',(130.04853988523,31.6104570811399,19.5461750907755));
#41416=CARTESIAN_POINT('Ctrl Pts',(130.096452395897,31.611579530182,19.5489577493476));
#41417=CARTESIAN_POINT('Ctrl Pts',(130.113511052364,31.6121080951875,19.5499552468336));
#41418=CARTESIAN_POINT('Ctrl Pts',(130.145695236496,31.6133486690801,19.5518511789087));
#41419=CARTESIAN_POINT('Ctrl Pts',(130.160821042584,31.6140332403618,19.5527481627375));
#41420=CARTESIAN_POINT('Ctrl Pts',(130.197356008177,31.6159321086878,19.5549285505349));
#41421=CARTESIAN_POINT('Ctrl Pts',(130.218758977666,31.6172482585219,19.5562172644105));
#41422=CARTESIAN_POINT('Ctrl Pts',(130.292321933773,31.6224729663525,19.5606825525034));
#41423=CARTESIAN_POINT('Ctrl Pts',(130.344400844976,31.6273855222876,19.563905875816));
#41424=CARTESIAN_POINT('Ctrl Pts',(130.598851739203,31.6573423427301,19.5798944445524));
#41425=CARTESIAN_POINT('Ctrl Pts',(130.798788946252,31.6994068819552,19.5931753681602));
#41426=CARTESIAN_POINT('Ctrl Pts',(131.037416819557,31.7725769276712,19.6091988973403));
#41427=CARTESIAN_POINT('Ctrl Pts',(131.080832171088,31.7868558527562,19.6121229553687));
#41428=CARTESIAN_POINT('Ctrl Pts',(131.267340977157,31.8524050832161,19.6247062034626));
#41429=CARTESIAN_POINT('Ctrl Pts',(131.40719715903,31.9123936512726,19.6341869007031));
#41430=CARTESIAN_POINT('Ctrl Pts',(131.580681828565,32.0010531908516,19.6459455090507));
#41431=CARTESIAN_POINT('Ctrl Pts',(131.618423355812,32.0212514204674,19.6485043627907));
#41432=CARTESIAN_POINT('Ctrl Pts',(131.680236057183,32.0558536396961,19.6526982152746));
#41433=CARTESIAN_POINT('Ctrl Pts',(131.70452825394,32.0698507715849,19.6543471872561));
#41434=CARTESIAN_POINT('Ctrl Pts',(131.751785854678,32.0978671435549,19.6575576304384));
#41435=CARTESIAN_POINT('Ctrl Pts',(131.774763468423,32.111861587575,19.659119827834));
#41436=CARTESIAN_POINT('Ctrl Pts',(131.824951892556,32.1432538505546,19.6625360124278));
#41437=CARTESIAN_POINT('Ctrl Pts',(131.852085745882,32.1607700931624,19.6643855583066));
#41438=CARTESIAN_POINT('Ctrl Pts',(131.945453727437,32.2229518873537,19.6707635209743));
#41439=CARTESIAN_POINT('Ctrl Pts',(132.010358611324,32.2695703624621,19.6752207033964));
#41440=CARTESIAN_POINT('Ctrl Pts',(132.296512356373,32.490843439481,19.6951027662234));
#41441=CARTESIAN_POINT('Ctrl Pts',(132.497079056264,32.6903631863241,19.7095900446456));
#41442=CARTESIAN_POINT('Ctrl Pts',(132.71193065259,32.9652192616336,19.7284720558489));
#41443=CARTESIAN_POINT('Ctrl Pts',(132.751644429959,33.0192545477198,19.7321455607671));
#41444=CARTESIAN_POINT('Ctrl Pts',(132.815505665414,33.1117753924046,19.738434448976));
#41445=CARTESIAN_POINT('Ctrl Pts',(132.840529738639,33.149633897141,19.7410075794933));
#41446=CARTESIAN_POINT('Ctrl Pts',(132.875373842545,33.204722109738,19.7447685587133));
#41447=CARTESIAN_POINT('Ctrl Pts',(132.885815397581,33.2215549241941,19.7459199700929));
#41448=CARTESIAN_POINT('Ctrl Pts',(132.903876512259,33.2512490999676,19.7479567284362));
#41449=CARTESIAN_POINT('Ctrl Pts',(132.911559461917,33.26407085494,19.7488380645543));
#41450=CARTESIAN_POINT('Ctrl Pts',(132.928325555692,33.2924755344085,19.7507950343929));
#41451=CARTESIAN_POINT('Ctrl Pts',(132.937369181284,33.3080801965146,19.751872931568));
#41452=CARTESIAN_POINT('Ctrl Pts',(132.963908493675,33.3547276074281,19.7551016980135));
#41453=CARTESIAN_POINT('Ctrl Pts',(132.981039163648,33.3859739491876,19.7572730398491));
#41454=CARTESIAN_POINT('Ctrl Pts',(133.065042432382,33.5450966522167,19.7683519239015));
#41455=CARTESIAN_POINT('Ctrl Pts',(133.12418869657,33.6768721730859,19.7775891689094));
#41456=CARTESIAN_POINT('Ctrl Pts',(133.218141340569,33.9279473334658,19.7948513252321));
#41457=CARTESIAN_POINT('Ctrl Pts',(133.255145042948,34.0461850538247,19.8028503594678));
#41458=CARTESIAN_POINT('Ctrl Pts',(133.311610149504,34.268682164028,19.8174851066821));
#41459=CARTESIAN_POINT('Ctrl Pts',(133.332813066236,34.3723475531884,19.8241425327511));
#41460=CARTESIAN_POINT('Ctrl Pts',(133.360583704125,34.550128626364,19.8352447292932));
#41461=CARTESIAN_POINT('Ctrl Pts',(133.369623624833,34.6237753526897,19.8397542238034));
#41462=CARTESIAN_POINT('Ctrl Pts',(133.37927968976,34.7316063198114,19.8462282611237));
#41463=CARTESIAN_POINT('Ctrl Pts',(133.381807227682,34.7655935342041,19.8482503908452));
#41464=CARTESIAN_POINT('Ctrl Pts',(133.38539109811,34.8261126414777,19.8518195887479));
#41465=CARTESIAN_POINT('Ctrl Pts',(133.386649027488,34.8526292949401,19.8533727220192));
#41466=CARTESIAN_POINT('Ctrl Pts',(133.388657002526,34.9089196459588,19.8566480451033));
#41467=CARTESIAN_POINT('Ctrl Pts',(133.389326419478,34.9386940821686,19.8583676302957));
#41468=CARTESIAN_POINT('Ctrl Pts',(133.390080505381,35.0197721314512,19.8630175474119));
#41469=CARTESIAN_POINT('Ctrl Pts',(133.389393065676,35.0710760452747,19.8659242135125));
#41470=CARTESIAN_POINT('Ctrl Pts',(133.378519205452,35.3721523378395,19.8828075085769));
#41471=CARTESIAN_POINT('Ctrl Pts',(133.3418949116,35.6201926046446,19.8959386289498));
#41472=CARTESIAN_POINT('Ctrl Pts',(133.248186194223,35.976596114098,19.9155099675868));
#41473=CARTESIAN_POINT('Ctrl Pts',(133.21205675139,36.0895603652594,19.9218371819471));
#41474=CARTESIAN_POINT('Ctrl Pts',(133.146694708057,36.2621733250101,19.9320033556803));
#41475=CARTESIAN_POINT('Ctrl Pts',(133.12150147322,36.3232522451485,19.9357024722337));
#41476=CARTESIAN_POINT('Ctrl Pts',(133.085256002473,36.4043212047064,19.94079961858));
#41477=CARTESIAN_POINT('Ctrl Pts',(133.075761638448,36.424995764854,19.942116272941));
#41478=CARTESIAN_POINT('Ctrl Pts',(133.059508800271,36.4594680427605,19.944342360807));
#41479=CARTESIAN_POINT('Ctrl Pts',(133.052863128391,36.4733186278345,19.9452451975962));
#41480=CARTESIAN_POINT('Ctrl Pts',(133.038870526682,36.5019801294892,19.9471318765351));
#41481=CARTESIAN_POINT('Ctrl Pts',(133.031509081146,36.5167831265571,19.9481165035166));
#41482=CARTESIAN_POINT('Ctrl Pts',(133.011235405754,36.5568139115607,19.9508057499079));
#41483=CARTESIAN_POINT('Ctrl Pts',(132.998114880788,36.5819340287823,19.9525221906066));
#41484=CARTESIAN_POINT('Ctrl Pts',(132.911121095869,36.7435190886185,19.963737286436));
#41485=CARTESIAN_POINT('Ctrl Pts',(132.828271729794,36.8749280251083,19.9736614331718));
#41486=CARTESIAN_POINT('Ctrl Pts',(132.663495844683,37.1003799075204,19.9916405905087));
#41487=CARTESIAN_POINT('Ctrl Pts',(132.584819242997,37.1964782963118,19.9996605192366));
#41488=CARTESIAN_POINT('Ctrl Pts',(132.429157746115,37.3666308130073,20.0143671888637));
#41489=CARTESIAN_POINT('Ctrl Pts',(132.353598703044,37.4417872405959,20.0210745655852));
#41490=CARTESIAN_POINT('Ctrl Pts',(132.219354394296,37.5632844868713,20.0322484271455));
#41491=CARTESIAN_POINT('Ctrl Pts',(132.162450354701,37.6114691349756,20.0367807790335));
#41492=CARTESIAN_POINT('Ctrl Pts',(132.077233120315,37.6789313407534,20.0432807784136));
#41493=CARTESIAN_POINT('Ctrl Pts',(132.05014671505,37.6997164923903,20.0453066711331));
#41494=CARTESIAN_POINT('Ctrl Pts',(132.001443936004,37.7359335193256,20.0488800443693));
#41495=CARTESIAN_POINT('Ctrl Pts',(131.979951853488,37.7515269885172,20.0504336415287));
#41496=CARTESIAN_POINT('Ctrl Pts',(131.933999042895,37.7840505623483,20.0537074751487));
#41497=CARTESIAN_POINT('Ctrl Pts',(131.909494112783,37.8009145196306,20.0554251400922));
#41498=CARTESIAN_POINT('Ctrl Pts',(131.842272486488,37.8458832343145,20.0600635680516));
#41499=CARTESIAN_POINT('Ctrl Pts',(131.799135953524,37.8733481346034,20.0629608712329));
#41500=CARTESIAN_POINT('Ctrl Pts',(131.540255949763,38.0300595587384,20.0799218042565));
#41501=CARTESIAN_POINT('Ctrl Pts',(131.311296675074,38.13594665252,20.09312732666));
#41502=CARTESIAN_POINT('Ctrl Pts',(130.912063395239,38.2691324831501,20.1154815794123));
#41503=CARTESIAN_POINT('Ctrl Pts',(130.747636453235,38.3106063008307,20.1245383787699));
#41504=CARTESIAN_POINT('Ctrl Pts',(130.551302308289,38.3447523832865,20.1358630227778));
#41505=CARTESIAN_POINT('Ctrl Pts',(130.521718428879,38.3494943635632,20.1375830440217));
#41506=CARTESIAN_POINT('Ctrl Pts',(130.475377767808,38.3562934759243,20.1403039214023));
#41507=CARTESIAN_POINT('Ctrl Pts',(130.458661187484,38.3586187350332,20.1412908218481));
#41508=CARTESIAN_POINT('Ctrl Pts',(130.426850202386,38.3628016962361,20.1431802661079));
#41509=CARTESIAN_POINT('Ctrl Pts',(130.411759624031,38.364682796465,20.1440815590659));
#41510=CARTESIAN_POINT('Ctrl Pts',(130.3749451936,38.3690204993416,20.1462918044247));
#41511=CARTESIAN_POINT('Ctrl Pts',(130.353209454592,38.3713685721479,20.1476064351758));
#41512=CARTESIAN_POINT('Ctrl Pts',(130.276685573544,38.3788871836712,20.1522652030586));
#41513=CARTESIAN_POINT('Ctrl Pts',(130.221798175942,38.3829333966169,20.1556614032598));
#41514=CARTESIAN_POINT('Ctrl Pts',(129.939814673572,38.3968291765303,20.1733101359939));
#41515=CARTESIAN_POINT('Ctrl Pts',(129.712245570642,38.385153868756,20.1881747003921));
#41516=CARTESIAN_POINT('Ctrl Pts',(129.3208767496,38.325301460879,20.2134766473903));
#41517=CARTESIAN_POINT('Ctrl Pts',(129.156310677016,38.2874062313545,20.2240419260026));
#41518=CARTESIAN_POINT('Ctrl Pts',(128.953410942571,38.2244338557998,20.2368754455562));
#41519=CARTESIAN_POINT('Ctrl Pts',(128.911845984703,38.2106453328931,20.2394950603042));
#41520=CARTESIAN_POINT('Ctrl Pts',(128.843937732295,38.1866474939306,20.2437611512652));
#41521=CARTESIAN_POINT('Ctrl Pts',(128.817435123822,38.1769077108209,20.2454225912506));
#41522=CARTESIAN_POINT('Ctrl Pts',(128.766036147631,38.1572861026596,20.2486389291301));
#41523=CARTESIAN_POINT('Ctrl Pts',(128.741129183889,38.1474381092643,20.2501947938823));
#41524=CARTESIAN_POINT('Ctrl Pts',(128.681546192648,38.1230590745161,20.2539116027744));
#41525=CARTESIAN_POINT('Ctrl Pts',(128.646989697383,38.1082441515366,20.2560629736201));
#41526=CARTESIAN_POINT('Ctrl Pts',(128.5295892068,38.0555836605759,20.2633642096277));
#41527=CARTESIAN_POINT('Ctrl Pts',(128.448024481866,38.0149748403744,20.2684222294066));
#41528=CARTESIAN_POINT('Ctrl Pts',(128.133258071286,37.8420979863815,20.2880480871323));
#41529=CARTESIAN_POINT('Ctrl Pts',(127.914475180346,37.6856699827746,20.301851211184));
#41530=CARTESIAN_POINT('Ctrl Pts',(127.667622304673,37.4606455684475,20.3199420153383));
#41531=CARTESIAN_POINT('Ctrl Pts',(127.620151193681,37.4147631596853,20.3235610891487));
#41532=CARTESIAN_POINT('Ctrl Pts',(127.542706359243,37.3354072977552,20.3297666890232));
#41533=CARTESIAN_POINT('Ctrl Pts',(127.512002969112,37.3026701152911,20.3323124026134));
#41534=CARTESIAN_POINT('Ctrl Pts',(127.468755201416,37.2546826570976,20.3360403655702));
#41535=CARTESIAN_POINT('Ctrl Pts',(127.455678794946,37.2399159983098,20.3371870531825));
#41536=CARTESIAN_POINT('Ctrl Pts',(127.432924454016,37.2137640941348,20.3392187472868));
#41537=CARTESIAN_POINT('Ctrl Pts',(127.423191772147,37.2024276759358,20.3400998173157));
#41538=CARTESIAN_POINT('Ctrl Pts',(127.401835537115,37.1772170435596,20.3420603521003));
#41539=CARTESIAN_POINT('Ctrl Pts',(127.390248090003,37.1633140240806,20.3431421393011));
#41540=CARTESIAN_POINT('Ctrl Pts',(127.356676801105,37.1223717696203,20.346327893368));
#41541=CARTESIAN_POINT('Ctrl Pts',(127.334998547728,37.0950862795405,20.3484510631975));
#41542=CARTESIAN_POINT('Ctrl Pts',(127.202225605103,36.9225752233857,20.361849984847));
#41543=CARTESIAN_POINT('Ctrl Pts',(127.102620100327,36.7689028080485,20.3736611928492));
#41544=CARTESIAN_POINT('Ctrl Pts',(126.941073937568,36.4691009803107,20.395611037577));
#41545=CARTESIAN_POINT('Ctrl Pts',(126.876029297552,36.325178709834,20.4057321322366));
#41546=CARTESIAN_POINT('Ctrl Pts',(126.821241918623,36.1772434423596,20.4155867593643));
#41547=CARTESIAN_POINT('Origin',(130.,35.,23.));
#41548=CARTESIAN_POINT('',(126.821242031451,36.1772437470164,21.6644319010721));
#41549=CARTESIAN_POINT('',(126.821241909055,36.1772434165241,21.3230640339373));
#41550=CARTESIAN_POINT('',(126.821241918358,36.1772434416438,23.));
#41551=CARTESIAN_POINT('',(126.610250158159,34.9989645099258,20.1438717258877));
#41552=CARTESIAN_POINT('Ctrl Pts',(126.821241909055,36.1772434165241,21.3230640339373));
#41553=CARTESIAN_POINT('Ctrl Pts',(126.859773903997,36.2812863773632,21.3161350653242));
#41554=CARTESIAN_POINT('Ctrl Pts',(126.903394320183,36.3833843634471,21.3090329747309));
#41555=CARTESIAN_POINT('Ctrl Pts',(127.068467069802,36.7226249430287,21.2847520874349));
#41556=CARTESIAN_POINT('Ctrl Pts',(127.212819820697,36.9475604108426,21.2675616869289));
#41557=CARTESIAN_POINT('Ctrl Pts',(127.416491132104,37.1951831280408,21.2480209068817));
#41558=CARTESIAN_POINT('Ctrl Pts',(127.451948183293,37.2362422683576,21.2447531923312));
#41559=CARTESIAN_POINT('Ctrl Pts',(127.508986235131,37.2991731708688,21.2396986178727));
#41560=CARTESIAN_POINT('Ctrl Pts',(127.52990385391,37.3216313161839,21.2378851049007));
#41561=CARTESIAN_POINT('Ctrl Pts',(127.569399031353,37.362897068256,21.2345335289934));
#41562=CARTESIAN_POINT('Ctrl Pts',(127.58789702295,37.3817772587843,21.2329922850979));
#41563=CARTESIAN_POINT('Ctrl Pts',(127.629780723482,37.4235378802346,21.2295644274639));
#41564=CARTESIAN_POINT('Ctrl Pts',(127.653280823025,37.4463001629194,21.2276829950934));
#41565=CARTESIAN_POINT('Ctrl Pts',(127.725455321044,37.5142113314142,21.2220259185415));
#41566=CARTESIAN_POINT('Ctrl Pts',(127.775131198867,37.5582751482987,21.2182951812326));
#41567=CARTESIAN_POINT('Ctrl Pts',(127.895325328536,37.6587396365478,21.2096088609643));
#41568=CARTESIAN_POINT('Ctrl Pts',(127.966866282428,37.7138387320578,21.2046993131418));
#41569=CARTESIAN_POINT('Ctrl Pts',(128.153677743463,37.8461778372522,21.1923912548147));
#41570=CARTESIAN_POINT('Ctrl Pts',(128.271644792969,37.919318963708,21.1850850707741));
#41571=CARTESIAN_POINT('Ctrl Pts',(128.542152146433,38.0648786214799,21.1687631300698));
#41572=CARTESIAN_POINT('Ctrl Pts',(128.696276544516,38.1335433499011,21.1597407285242));
#41573=CARTESIAN_POINT('Ctrl Pts',(128.881868478032,38.2001580021678,21.1485178132625));
#41574=CARTESIAN_POINT('Ctrl Pts',(128.909011949439,38.2095130934921,21.1468675771204));
#41575=CARTESIAN_POINT('Ctrl Pts',(128.95204259432,38.2237348350978,21.1442327676826));
#41576=CARTESIAN_POINT('Ctrl Pts',(128.967852925842,38.2288315848197,21.1432607386928));
#41577=CARTESIAN_POINT('Ctrl Pts',(128.99831762532,38.238405822477,21.1413790499639));
#41578=CARTESIAN_POINT('Ctrl Pts',(129.012965885151,38.2429004721552,21.1404703491986));
#41579=CARTESIAN_POINT('Ctrl Pts',(129.049227118738,38.2537583814401,21.1382119370871));
#41580=CARTESIAN_POINT('Ctrl Pts',(129.070873840434,38.2600057049292,21.1368559570382));
#41581=CARTESIAN_POINT('Ctrl Pts',(129.154484328788,38.2832356286813,21.1315928515003));
#41582=CARTESIAN_POINT('Ctrl Pts',(129.21686063471,38.2986701251505,21.1276125975374));
#41583=CARTESIAN_POINT('Ctrl Pts',(129.390261968804,38.3363815928937,21.1164673879257));
#41584=CARTESIAN_POINT('Ctrl Pts',(129.502021381481,38.3548826352365,21.1091963482551));
#41585=CARTESIAN_POINT('Ctrl Pts',(129.872530616487,38.3972950443711,21.0851686096351));
#41586=CARTESIAN_POINT('Ctrl Pts',(130.133154773504,38.3970831089794,21.0684730652064));
#41587=CARTESIAN_POINT('Ctrl Pts',(130.441009027953,38.3613134515819,21.0496518691833));
#41588=CARTESIAN_POINT('Ctrl Pts',(130.490661591863,38.3544252393884,21.0466410324632));
#41589=CARTESIAN_POINT('Ctrl Pts',(130.569305440546,38.3417314150562,21.0419096513212));
#41590=CARTESIAN_POINT('Ctrl Pts',(130.598403569848,38.3366436407367,21.0401672201116));
#41591=CARTESIAN_POINT('Ctrl Pts',(130.653567164916,38.3262534918557,21.0368784958857));
#41592=CARTESIAN_POINT('Ctrl Pts',(130.679643832563,38.3210234343219,21.0353300796019));
#41593=CARTESIAN_POINT('Ctrl Pts',(130.73941873039,38.3083011510789,21.0317937564636));
#41594=CARTESIAN_POINT('Ctrl Pts',(130.773069759708,38.3005999207,21.0298125585877));
#41595=CARTESIAN_POINT('Ctrl Pts',(130.88121963861,38.2741043937956,21.0234714993874));
#41596=CARTESIAN_POINT('Ctrl Pts',(130.955201323526,38.2532905287884,21.0191748438486));
#41597=CARTESIAN_POINT('Ctrl Pts',(131.134521171187,38.1961956236317,21.0088046393751));
#41598=CARTESIAN_POINT('Ctrl Pts',(131.238901799692,38.1572027677842,21.002808042536));
#41599=CARTESIAN_POINT('Ctrl Pts',(131.543169920483,38.0261204288703,20.9851405701074));
#41600=CARTESIAN_POINT('Ctrl Pts',(131.736196387073,37.9196551404937,20.9737041402769));
#41601=CARTESIAN_POINT('Ctrl Pts',(131.968740899677,37.7601304575795,20.958142263));
#41602=CARTESIAN_POINT('Ctrl Pts',(132.018967873357,37.7236058168674,20.9546606472044));
#41603=CARTESIAN_POINT('Ctrl Pts',(132.086300708757,37.671755720168,20.9497838716541));
#41604=CARTESIAN_POINT('Ctrl Pts',(132.104298621711,37.6576035304019,20.9484590681646));
#41605=CARTESIAN_POINT('Ctrl Pts',(132.134032912165,37.6337313382546,20.9462321289046));
#41606=CARTESIAN_POINT('Ctrl Pts',(132.145849962852,37.6241122616264,20.9453368325388));
#41607=CARTESIAN_POINT('Ctrl Pts',(132.170274514188,37.603955371336,20.9434640348684));
#41608=CARTESIAN_POINT('Ctrl Pts',(132.182870819327,37.5934050983523,20.9424857228924));
#41609=CARTESIAN_POINT('Ctrl Pts',(132.216622668194,37.5647155000754,20.9398316931834));
#41610=CARTESIAN_POINT('Ctrl Pts',(132.237631596953,37.5464065615667,20.9381446477804));
#41611=CARTESIAN_POINT('Ctrl Pts',(132.361877603458,37.4354033020382,20.9279682533703));
#41612=CARTESIAN_POINT('Ctrl Pts',(132.45956161267,37.3367080852637,20.9191370598177));
#41613=CARTESIAN_POINT('Ctrl Pts',(132.737038599959,37.0196293690367,20.8920590685854));
#41614=CARTESIAN_POINT('Ctrl Pts',(132.895867974043,36.7844559407551,20.8737590725844));
#41615=CARTESIAN_POINT('Ctrl Pts',(133.047326312648,36.4855798004533,20.8533670879347));
#41616=CARTESIAN_POINT('Ctrl Pts',(133.069903827152,36.4383448640673,20.8502169691593));
#41617=CARTESIAN_POINT('Ctrl Pts',(133.103803420997,36.3629844389975,20.8453025190111));
#41618=CARTESIAN_POINT('Ctrl Pts',(133.115857154668,36.3351990630656,20.8435138872781));
#41619=CARTESIAN_POINT('Ctrl Pts',(133.137647747116,36.2830662512792,20.8402001431143));
#41620=CARTESIAN_POINT('Ctrl Pts',(133.1474775322,36.2587603550308,20.8386720278866));
#41621=CARTESIAN_POINT('Ctrl Pts',(133.169092669416,36.20347624448,20.8352331414668));
#41622=CARTESIAN_POINT('Ctrl Pts',(133.180707762597,36.1724340742095,20.8333280839539));
#41623=CARTESIAN_POINT('Ctrl Pts',(133.21501571764,36.076479003973,20.8275144436089));
#41624=CARTESIAN_POINT('Ctrl Pts',(133.236190933134,36.0110401764402,20.8236546678834));
#41625=CARTESIAN_POINT('Ctrl Pts',(133.28180126676,35.8539203223413,20.8145961836113));
#41626=CARTESIAN_POINT('Ctrl Pts',(133.304407701448,35.7617682263128,20.809449534563));
#41627=CARTESIAN_POINT('Ctrl Pts',(133.349653796137,35.5369453069032,20.7971459936452));
#41628=CARTESIAN_POINT('Ctrl Pts',(133.368317781167,35.403641728636,20.7900615511808));
#41629=CARTESIAN_POINT('Ctrl Pts',(133.392117086667,35.1053354404899,20.7741527820009));
#41630=CARTESIAN_POINT('Ctrl Pts',(133.393226501035,34.9403686561349,20.7653174067637));
#41631=CARTESIAN_POINT('Ctrl Pts',(133.380454588038,34.747519728963,20.7543148342302));
#41632=CARTESIAN_POINT('Ctrl Pts',(133.37820921087,34.7190695405162,20.7526741829412));
#41633=CARTESIAN_POINT('Ctrl Pts',(133.374092343868,34.6741462786159,20.7500511983063));
#41634=CARTESIAN_POINT('Ctrl Pts',(133.372458705202,34.6576521517151,20.7490812203024));
#41635=CARTESIAN_POINT('Ctrl Pts',(133.369080253733,34.6259162492986,20.747200458455));
#41636=CARTESIAN_POINT('Ctrl Pts',(133.367352831741,34.610673298244,20.746290592111));
#41637=CARTESIAN_POINT('Ctrl Pts',(133.362821118539,34.5729738311149,20.7440248689902));
#41638=CARTESIAN_POINT('Ctrl Pts',(133.359895304586,34.5505328647262,20.7426626541281));
#41639=CARTESIAN_POINT('Ctrl Pts',(133.347686779179,34.463686173746,20.7373427594258));
#41640=CARTESIAN_POINT('Ctrl Pts',(133.336775458194,34.399527092683,20.7333100066618));
#41641=CARTESIAN_POINT('Ctrl Pts',(133.301371734932,34.2223668785452,20.7219583603378));
#41642=CARTESIAN_POINT('Ctrl Pts',(133.272934966972,34.1102456245439,20.7145292406759));
#41643=CARTESIAN_POINT('Ctrl Pts',(133.163511984265,33.7559135697023,20.6906320529056));
#41644=CARTESIAN_POINT('Ctrl Pts',(133.060876093169,33.5212720577741,20.6742366225189));
#41645=CARTESIAN_POINT('Ctrl Pts',(132.907439745488,33.2565070191544,20.6556449589559));
#41646=CARTESIAN_POINT('Ctrl Pts',(132.88104667393,33.2132308134881,20.6525993914144));
#41647=CARTESIAN_POINT('Ctrl Pts',(132.83768829327,33.1455972621944,20.6478268030638));
#41648=CARTESIAN_POINT('Ctrl Pts',(132.821357398191,33.1208441046411,20.6460772340298));
#41649=CARTESIAN_POINT('Ctrl Pts',(132.789781765757,33.0743238296701,20.6427826614634));
#41650=CARTESIAN_POINT('Ctrl Pts',(132.774601874469,33.052515594185,20.6412354241289));
#41651=CARTESIAN_POINT('Ctrl Pts',(132.739239630386,33.0029651817673,20.6377123150111));
#41652=CARTESIAN_POINT('Ctrl Pts',(132.718889245161,32.9753461498168,20.6357429701379));
#41653=CARTESIAN_POINT('Ctrl Pts',(132.652402776801,32.8879230786819,20.6294865179868));
#41654=CARTESIAN_POINT('Ctrl Pts',(132.604684550671,32.8293482663888,20.625260173382));
#41655=CARTESIAN_POINT('Ctrl Pts',(132.483691850073,32.6905693739704,20.615106945444));
#41656=CARTESIAN_POINT('Ctrl Pts',(132.408442874244,32.6121976473872,20.609252488354));
#41657=CARTESIAN_POINT('Ctrl Pts',(132.181477407186,32.3974791597942,20.5925767954797));
#41658=CARTESIAN_POINT('Ctrl Pts',(132.021070943205,32.271040157098,20.5819558147157));
#41659=CARTESIAN_POINT('Ctrl Pts',(131.784297425951,32.1167915523867,20.5665191552995));
#41660=CARTESIAN_POINT('Ctrl Pts',(131.716831735546,32.0761164095478,20.5621417253791));
#41661=CARTESIAN_POINT('Ctrl Pts',(131.626327066921,32.0257637355334,20.5562158652508));
#41662=CARTESIAN_POINT('Ctrl Pts',(131.6045068089,32.0139358833589,20.5547831804933));
#41663=CARTESIAN_POINT('Ctrl Pts',(131.569987930202,31.995712222606,20.5525074075938));
#41664=CARTESIAN_POINT('Ctrl Pts',(131.557375158093,31.9891546450765,20.5516739359601));
#41665=CARTESIAN_POINT('Ctrl Pts',(131.530878723303,31.975589767939,20.5499182048072));
#41666=CARTESIAN_POINT('Ctrl Pts',(131.516987548718,31.968598399602,20.5489949393953));
#41667=CARTESIAN_POINT('Ctrl Pts',(131.481777788953,31.951180088561,20.5466486102724));
#41668=CARTESIAN_POINT('Ctrl Pts',(131.460397114415,31.9408810962929,20.5452182023479));
#41669=CARTESIAN_POINT('Ctrl Pts',(131.371145206879,31.8990376669984,20.5392291788145));
#41670=CARTESIAN_POINT('Ctrl Pts',(131.302350761252,31.8695228087357,20.5345705861357));
#41671=CARTESIAN_POINT('Ctrl Pts',(131.095389043063,31.7887328491178,20.5205443409293));
#41672=CARTESIAN_POINT('Ctrl Pts',(130.95479400898,31.7441622139968,20.5110080389748));
#41673=CARTESIAN_POINT('Ctrl Pts',(130.611692869122,31.6595367409439,20.4882519648145));
#41674=CARTESIAN_POINT('Ctrl Pts',(130.407528221975,31.6285306872071,20.4751468618438));
#41675=CARTESIAN_POINT('Ctrl Pts',(130.148915167921,31.6131083825935,20.4593722385477));
#41676=CARTESIAN_POINT('Ctrl Pts',(130.095973493688,31.6111948836301,20.4561835158768));
#41677=CARTESIAN_POINT('Ctrl Pts',(130.012590694451,31.610136905362,20.4512230206748));
#41678=CARTESIAN_POINT('Ctrl Pts',(129.982170472456,31.6101603984439,20.4494261852978));
#41679=CARTESIAN_POINT('Ctrl Pts',(129.92530224412,31.6109698819658,20.446090163745));
#41680=CARTESIAN_POINT('Ctrl Pts',(129.898855346249,31.6116560515182,20.4445480376383));
#41681=CARTESIAN_POINT('Ctrl Pts',(129.839362280935,31.6138968034491,20.4410987729732));
#41682=CARTESIAN_POINT('Ctrl Pts',(129.806325140639,31.6156256865156,20.4391971252134));
#41683=CARTESIAN_POINT('Ctrl Pts',(129.705056377855,31.6224130111299,20.4334062744793));
#41684=CARTESIAN_POINT('Ctrl Pts',(129.636946332503,31.6290537658916,20.4295653003918));
#41685=CARTESIAN_POINT('Ctrl Pts',(129.475680747019,31.6497222200078,20.4205614437672));
#41686=CARTESIAN_POINT('Ctrl Pts',(129.382816476291,31.6655798147327,20.4154497086736));
#41687=CARTESIAN_POINT('Ctrl Pts',(129.077472695527,31.7309162045898,20.3986922981087));
#41688=CARTESIAN_POINT('Ctrl Pts',(128.869130297171,31.7970184268176,20.3873681541716));
#41689=CARTESIAN_POINT('Ctrl Pts',(128.587761860459,31.9171906427938,20.3707332724647));
#41690=CARTESIAN_POINT('Ctrl Pts',(128.508312514633,31.954840539049,20.3658698027734));
#41691=CARTESIAN_POINT('Ctrl Pts',(128.407672868194,32.0074161413867,20.3593810107789));
#41692=CARTESIAN_POINT('Ctrl Pts',(128.38505984811,32.0195584107695,20.357900896062));
#41693=CARTESIAN_POINT('Ctrl Pts',(128.348615685208,32.0396639487203,20.3554758637301));
#41694=CARTESIAN_POINT('Ctrl Pts',(128.334698658286,32.047470387921,20.354540308711));
#41695=CARTESIAN_POINT('Ctrl Pts',(128.307145219324,32.0631826410323,20.3526680653655));
#41696=CARTESIAN_POINT('Ctrl Pts',(128.293507841715,32.0710858673643,20.3517315367736));
#41697=CARTESIAN_POINT('Ctrl Pts',(128.258594996109,32.0916453962602,20.3493094458053));
#41698=CARTESIAN_POINT('Ctrl Pts',(128.237402478598,32.1044399871423,20.3478156042256));
#41699=CARTESIAN_POINT('Ctrl Pts',(128.143631372421,32.1624634244914,20.3411064620515));
#41700=CARTESIAN_POINT('Ctrl Pts',(128.07264436121,32.2101942251539,20.335760233844));
#41701=CARTESIAN_POINT('Ctrl Pts',(127.848305813625,32.3736878745157,20.3181572849215));
#41702=CARTESIAN_POINT('Ctrl Pts',(127.702966406556,32.4998118061851,20.3056452067832));
#41703=CARTESIAN_POINT('Ctrl Pts',(127.453505989063,32.756502987286,20.2827775880254));
#41704=CARTESIAN_POINT('Ctrl Pts',(127.346793561227,32.8837725196323,20.2723879688226));
#41705=CARTESIAN_POINT('Ctrl Pts',(127.223880129731,33.0543556399103,20.2596804544436));
#41706=CARTESIAN_POINT('Ctrl Pts',(127.198651510759,33.090858718767,20.2570250430092));
#41707=CARTESIAN_POINT('Ctrl Pts',(127.158487004763,33.1514836200856,20.2527163680742));
#41708=CARTESIAN_POINT('Ctrl Pts',(127.143124962111,33.1753153697732,20.2510475468043));
#41709=CARTESIAN_POINT('Ctrl Pts',(127.113710024129,33.2222302374069,20.2478096195621));
#41710=CARTESIAN_POINT('Ctrl Pts',(127.099630619469,33.2452941351801,20.2462396326081));
#41711=CARTESIAN_POINT('Ctrl Pts',(127.06671350127,33.300695515867,20.2425186396044));
#41712=CARTESIAN_POINT('Ctrl Pts',(127.048132349975,33.3331817892836,20.2403768604267));
#41713=CARTESIAN_POINT('Ctrl Pts',(126.983557705921,33.450548501849,20.2327741049604));
#41714=CARTESIAN_POINT('Ctrl Pts',(126.940654870642,33.5370804321079,20.2274191296354));
#41715=CARTESIAN_POINT('Ctrl Pts',(126.795984085469,33.8631679062537,20.207957924295));
#41716=CARTESIAN_POINT('Ctrl Pts',(126.718206510932,34.1123465852793,20.1945374888264));
#41717=CARTESIAN_POINT('Ctrl Pts',(126.651263973486,34.4650764323385,20.1751129278367));
#41718=CARTESIAN_POINT('Ctrl Pts',(126.637091299803,34.5629439251915,20.1696701320848));
#41719=CARTESIAN_POINT('Ctrl Pts',(126.62457323614,34.687592483876,20.1625187030953));
#41720=CARTESIAN_POINT('Ctrl Pts',(126.622238986294,34.7139322864057,20.1609951523383));
#41721=CARTESIAN_POINT('Ctrl Pts',(126.618977841705,34.7563727802128,20.1585166094253));
#41722=CARTESIAN_POINT('Ctrl Pts',(126.617857237686,34.7724579839795,20.1575717579423));
#41723=CARTESIAN_POINT('Ctrl Pts',(126.615979814494,34.8024963275471,20.1557960863792));
#41724=CARTESIAN_POINT('Ctrl Pts',(126.615194436786,34.8164472993528,20.1549668525351));
#41725=CARTESIAN_POINT('Ctrl Pts',(126.613711945883,34.8460407510556,20.1531987661108));
#41726=CARTESIAN_POINT('Ctrl Pts',(126.613036918084,34.8616840679095,20.1522587723144));
#41727=CARTESIAN_POINT('Ctrl Pts',(126.611002638902,34.9178611839555,20.1488652024303));
#41728=CARTESIAN_POINT('Ctrl Pts',(126.610262545954,34.9584121894217,20.1463820977784));
#41729=CARTESIAN_POINT('Ctrl Pts',(126.610250158159,34.9989645099258,20.1438717258877));
#41730=CARTESIAN_POINT('Ctrl Pts',(126.610250159371,34.9989605517602,20.1438719709159));
#41731=CARTESIAN_POINT('Ctrl Pts',(126.610184366452,35.2135181673577,20.1305898943176));
#41732=CARTESIAN_POINT('Ctrl Pts',(126.630489346633,35.4275956772245,20.1166108704707));
#41733=CARTESIAN_POINT('Ctrl Pts',(126.705189704235,35.817192544607,20.0911256084591));
#41734=CARTESIAN_POINT('Ctrl Pts',(126.753851883876,35.9930339018189,20.0796019086335));
#41735=CARTESIAN_POINT('Ctrl Pts',(126.818016155968,36.1685056986385,20.068223916931));
#41736=CARTESIAN_POINT('Ctrl Pts',(126.819624542574,36.1728762511695,20.06794058377));
#41737=CARTESIAN_POINT('Ctrl Pts',(126.821241918282,36.1772434414401,20.0676575318486));
#41738=CARTESIAN_POINT('Ctrl Pts',(126.821241918623,36.1772434423597,20.4155867593643));
#41739=CARTESIAN_POINT('Ctrl Pts',(126.820287669406,36.174666806722,20.4157584005415));
#41740=CARTESIAN_POINT('Ctrl Pts',(126.819336531962,36.1720889539246,20.4159299649612));
#41741=CARTESIAN_POINT('Ctrl Pts',(126.785050662335,36.0788154230474,20.4221319007212));
#41742=CARTESIAN_POINT('Ctrl Pts',(126.755603836689,35.9867310859727,20.4280573351828));
#41743=CARTESIAN_POINT('Ctrl Pts',(126.720262772976,35.8573972608461,20.4361063917783));
#41744=CARTESIAN_POINT('Ctrl Pts',(126.710994149601,35.8211254629107,20.4383348157629));
#41745=CARTESIAN_POINT('Ctrl Pts',(126.69607245493,35.7584181214976,20.442139148177));
#41746=CARTESIAN_POINT('Ctrl Pts',(126.690131386026,35.7320553881174,20.4437240062198));
#41747=CARTESIAN_POINT('Ctrl Pts',(126.678604941951,35.6778964257731,20.446951220593));
#41748=CARTESIAN_POINT('Ctrl Pts',(126.673051753982,35.6500954814279,20.4485924542259));
#41749=CARTESIAN_POINT('Ctrl Pts',(126.659707162139,35.5786325369141,20.452773846614));
#41750=CARTESIAN_POINT('Ctrl Pts',(126.652422551288,35.5348806749159,20.4552981377726));
#41751=CARTESIAN_POINT('Ctrl Pts',(126.622062486016,35.3274909900031,20.4671126870272));
#41752=CARTESIAN_POINT('Ctrl Pts',(126.610113320875,35.1624456778701,20.4760587111048));
#41753=CARTESIAN_POINT('Ctrl Pts',(126.610434020872,34.7779706240709,20.4965624622672));
#41754=CARTESIAN_POINT('Ctrl Pts',(126.631878457629,34.5593210766636,20.507961576881));
#41755=CARTESIAN_POINT('Ctrl Pts',(126.686426682109,34.2826552361581,20.5235152352456));
#41756=CARTESIAN_POINT('Ctrl Pts',(126.70028919491,34.221373477112,20.5270361444065));
#41757=CARTESIAN_POINT('Ctrl Pts',(126.721539855484,34.1382385085309,20.5319594782805));
#41758=CARTESIAN_POINT('Ctrl Pts',(126.727460770062,34.1160199585576,20.533289798393));
#41759=CARTESIAN_POINT('Ctrl Pts',(126.737685091135,34.0791638455968,20.5355233342974));
#41760=CARTESIAN_POINT('Ctrl Pts',(126.74186223254,34.064491545674,20.536419620563));
#41761=CARTESIAN_POINT('Ctrl Pts',(126.750734768655,34.0341069269045,20.5382914133885));
#41762=CARTESIAN_POINT('Ctrl Pts',(126.755445343906,34.0183997599718,20.5392676946189));
#41763=CARTESIAN_POINT('Ctrl Pts',(126.768423535529,33.9762389134624,20.5419104104396));
#41764=CARTESIAN_POINT('Ctrl Pts',(126.776901763124,33.9498519837033,20.5435880158197));
#41765=CARTESIAN_POINT('Ctrl Pts',(126.8284236133,33.7960036005473,20.553496121321));
#41766=CARTESIAN_POINT('Ctrl Pts',(126.878697867504,33.6711017771715,20.5620484131386));
#41767=CARTESIAN_POINT('Ctrl Pts',(127.060272604103,33.28757172159,20.5893018313336));
#41768=CARTESIAN_POINT('Ctrl Pts',(127.217403944963,33.0425469118861,20.6080877805358));
#41769=CARTESIAN_POINT('Ctrl Pts',(127.436521563445,32.7815387563258,20.6288048290108));
#41770=CARTESIAN_POINT('Ctrl Pts',(127.470097988527,32.7433236350366,20.631863060392));
#41771=CARTESIAN_POINT('Ctrl Pts',(127.524804312639,32.6838157681659,20.6366677502469));
#41772=CARTESIAN_POINT('Ctrl Pts',(127.545377605051,32.6620239370128,20.6384367326263));
#41773=CARTESIAN_POINT('Ctrl Pts',(127.584692459151,32.6214715722403,20.6417478041207));
#41774=CARTESIAN_POINT('Ctrl Pts',(127.603370306727,32.6026526804182,20.6432924218791));
#41775=CARTESIAN_POINT('Ctrl Pts',(127.646331362137,32.5603711392118,20.6467825642812));
#41776=CARTESIAN_POINT('Ctrl Pts',(127.670748388758,32.5370480954941,20.6487220199996));
#41777=CARTESIAN_POINT('Ctrl Pts',(127.748548846851,32.4649253843845,20.6547693392371));
#41778=CARTESIAN_POINT('Ctrl Pts',(127.803149466954,32.4174655174925,20.6588222590061));
#41779=CARTESIAN_POINT('Ctrl Pts',(127.938265608477,32.3074087680611,20.6684502553522));
#41780=CARTESIAN_POINT('Ctrl Pts',(128.020168665936,32.2466264303729,20.6739631819367));
#41781=CARTESIAN_POINT('Ctrl Pts',(128.144183891671,32.1629908780481,20.6819651990938));
#41782=CARTESIAN_POINT('Ctrl Pts',(128.184234826507,32.1371917433332,20.6845000248636));
#41783=CARTESIAN_POINT('Ctrl Pts',(128.402268225455,32.0031605395511,20.6980894910399));
#41784=CARTESIAN_POINT('Ctrl Pts',(128.589380262871,31.9106748871943,20.7089910326984));
#41785=CARTESIAN_POINT('Ctrl Pts',(128.827680218912,31.8190749870077,20.7232378679673));
#41786=CARTESIAN_POINT('Ctrl Pts',(128.87193031137,31.8031146505917,20.725899008975));
#41787=CARTESIAN_POINT('Ctrl Pts',(128.934229248945,31.7820988161614,20.7296857708342));
#41788=CARTESIAN_POINT('Ctrl Pts',(128.952011469793,31.7762637624649,20.7307711629529));
#41789=CARTESIAN_POINT('Ctrl Pts',(128.98425221572,31.765979231962,20.7327487512041));
#41790=CARTESIAN_POINT('Ctrl Pts',(128.998694184847,31.7614786478996,20.733638100551));
#41791=CARTESIAN_POINT('Ctrl Pts',(129.029098164828,31.752226603529,20.7355185633058));
#41792=CARTESIAN_POINT('Ctrl Pts',(129.045065670042,31.7474959172843,20.7365107268351));
#41793=CARTESIAN_POINT('Ctrl Pts',(129.088842768182,31.7348762404121,20.7392421568406));
#41794=CARTESIAN_POINT('Ctrl Pts',(129.116718823208,31.727225197413,20.7409938469677));
#41795=CARTESIAN_POINT('Ctrl Pts',(129.325058703135,31.6728984170947,20.7541603296649));
#41796=CARTESIAN_POINT('Ctrl Pts',(129.508986324946,31.6408267906926,20.7661819326654));
#41797=CARTESIAN_POINT('Ctrl Pts',(129.926976852332,31.603013975896,20.7932358590426));
#41798=CARTESIAN_POINT('Ctrl Pts',(130.160937842385,31.6060383054034,20.8081622060412));
#41799=CARTESIAN_POINT('Ctrl Pts',(130.444559696523,31.6391233791211,20.8255380488592));
#41800=CARTESIAN_POINT('Ctrl Pts',(130.496216949364,31.6463610546961,20.8286762925382));
#41801=CARTESIAN_POINT('Ctrl Pts',(130.577535758621,31.6596748321647,20.8335765730972));
#41802=CARTESIAN_POINT('Ctrl Pts',(130.607316618918,31.6649608109426,20.8353626776652));
#41803=CARTESIAN_POINT('Ctrl Pts',(130.662778275836,31.6755725888658,20.8386741440546));
#41804=CARTESIAN_POINT('Ctrl Pts',(130.688475529499,31.6807991689149,20.8402024715004));
#41805=CARTESIAN_POINT('Ctrl Pts',(130.74656647488,31.6933179922378,20.8436449407203));
#41806=CARTESIAN_POINT('Ctrl Pts',(130.778919122243,31.7007891073026,20.8455533183412));
#41807=CARTESIAN_POINT('Ctrl Pts',(130.878248844127,31.7252696793858,20.8513891928279));
#41808=CARTESIAN_POINT('Ctrl Pts',(130.944821585727,31.7438530789242,20.8552673151768));
#41809=CARTESIAN_POINT('Ctrl Pts',(131.101938643297,31.7929364568094,20.8643792360567));
#41810=CARTESIAN_POINT('Ctrl Pts',(131.191853802399,31.8252541049068,20.8695600737131));
#41811=CARTESIAN_POINT('Ctrl Pts',(131.404081399756,31.9118233395886,20.8818533413628));
#41812=CARTESIAN_POINT('Ctrl Pts',(131.524780047811,31.9695997064192,20.8888964031794));
#41813=CARTESIAN_POINT('Ctrl Pts',(131.77439522822,32.1077840022079,20.9040647518095));
#41814=CARTESIAN_POINT('Ctrl Pts',(131.901952122942,32.1900246943164,20.9121919779557));
#41815=CARTESIAN_POINT('Ctrl Pts',(132.052479283903,32.3020317102068,20.9227817179465));
#41816=CARTESIAN_POINT('Ctrl Pts',(132.081048559259,32.324006580663,20.9248397193474));
#41817=CARTESIAN_POINT('Ctrl Pts',(132.123442417569,32.3577044918861,20.9279757442792));
#41818=CARTESIAN_POINT('Ctrl Pts',(132.137533085632,32.3690903609842,20.929032073311));
#41819=CARTESIAN_POINT('Ctrl Pts',(132.162966379457,32.3899807513462,20.9309656897006));
#41820=CARTESIAN_POINT('Ctrl Pts',(132.174339003062,32.3994473833754,20.9318403911967));
#41821=CARTESIAN_POINT('Ctrl Pts',(132.200642199068,32.4216354573315,20.933886879027));
#41822=CARTESIAN_POINT('Ctrl Pts',(132.215524654352,32.434412295685,20.9350624661483));
#41823=CARTESIAN_POINT('Ctrl Pts',(132.263607093785,32.4764222253639,20.9389161380733));
#41824=CARTESIAN_POINT('Ctrl Pts',(132.29634464679,32.5061750806288,20.9416274153544));
#41825=CARTESIAN_POINT('Ctrl Pts',(132.375493863726,32.5809883328067,20.948381507485));
#41826=CARTESIAN_POINT('Ctrl Pts',(132.421215260218,32.6267523580759,20.9524589968842));
#41827=CARTESIAN_POINT('Ctrl Pts',(132.638672508756,32.8572400759333,20.9726242675964));
#41828=CARTESIAN_POINT('Ctrl Pts',(132.790754797264,33.0594537018878,20.9891203864687));
#41829=CARTESIAN_POINT('Ctrl Pts',(132.972198604104,33.3667846683902,21.0114902674266));
#41830=CARTESIAN_POINT('Ctrl Pts',(133.021204514989,33.4593236646684,21.0179317523213));
#41831=CARTESIAN_POINT('Ctrl Pts',(133.082695836451,33.5896985382098,21.0266040484989));
#41832=CARTESIAN_POINT('Ctrl Pts',(133.098913237366,33.6256998951742,21.0289584376606));
#41833=CARTESIAN_POINT('Ctrl Pts',(133.124229154205,33.6846274451366,21.032748565642));
#41834=CARTESIAN_POINT('Ctrl Pts',(133.133712615707,33.7073832524177,21.0341970572899));
#41835=CARTESIAN_POINT('Ctrl Pts',(133.153173107556,33.7555524684059,21.0372322118983));
#41836=CARTESIAN_POINT('Ctrl Pts',(133.163093099845,33.7809871163205,21.038816898363));
#41837=CARTESIAN_POINT('Ctrl Pts',(133.186437348435,33.8430456479946,21.0426415025806));
#41838=CARTESIAN_POINT('Ctrl Pts',(133.199539002191,33.8797872082199,21.0448707648528));
#41839=CARTESIAN_POINT('Ctrl Pts',(133.24697040297,34.0204283734803,21.0532802494469));
#41840=CARTESIAN_POINT('Ctrl Pts',(133.276898129637,34.1257465454927,21.0593204917051));
#41841=CARTESIAN_POINT('Ctrl Pts',(133.347709550343,34.4303023991381,21.0762830157843));
#41842=CARTESIAN_POINT('Ctrl Pts',(133.375839675054,34.6320037613424,21.0868954548715));
#41843=CARTESIAN_POINT('Ctrl Pts',(133.392343664284,34.9706808097004,21.1050193267405));
#41844=CARTESIAN_POINT('Ctrl Pts',(133.390793642338,35.1066127959693,21.112384072702));
#41845=CARTESIAN_POINT('Ctrl Pts',(133.379085931659,35.2701393055838,21.1217219058544));
#41846=CARTESIAN_POINT('Ctrl Pts',(133.376726926689,35.2981813731623,21.1233403616281));
#41847=CARTESIAN_POINT('Ctrl Pts',(133.372432363392,35.342603170114,21.1259359640332));
#41848=CARTESIAN_POINT('Ctrl Pts',(133.370725863199,35.359004328886,21.1269011884282));
#41849=CARTESIAN_POINT('Ctrl Pts',(133.367195944092,35.3906830635239,21.1287799559407));
#41850=CARTESIAN_POINT('Ctrl Pts',(133.365388065386,35.405961719006,21.1296926790283));
#41851=CARTESIAN_POINT('Ctrl Pts',(133.360633906574,35.4439234314898,21.1319760699028));
#41852=CARTESIAN_POINT('Ctrl Pts',(133.357561939875,35.4665897816774,21.133353311651));
#41853=CARTESIAN_POINT('Ctrl Pts',(133.344577054242,35.5556181563419,21.1388128579982));
#41854=CARTESIAN_POINT('Ctrl Pts',(133.332924560987,35.6217072160312,21.1429751290883));
#41855=CARTESIAN_POINT('Ctrl Pts',(133.294650135896,35.8065262997047,21.1548467295322));
#41856=CARTESIAN_POINT('Ctrl Pts',(133.263586818616,35.9242308620343,21.1626769769337));
#41857=CARTESIAN_POINT('Ctrl Pts',(133.151264191168,36.2726739904816,21.1862746419526));
#41858=CARTESIAN_POINT('Ctrl Pts',(133.051301348161,36.4965828054287,21.2019464876325));
#41859=CARTESIAN_POINT('Ctrl Pts',(132.90227437232,36.7520949652057,21.2199339447609));
#41860=CARTESIAN_POINT('Ctrl Pts',(132.875443286598,36.7957894181399,21.2230172403244));
#41861=CARTESIAN_POINT('Ctrl Pts',(132.831326582747,36.8641078543573,21.2278518923955));
#41862=CARTESIAN_POINT('Ctrl Pts',(132.81468751178,36.8891380598049,21.2296262519872));
#41863=CARTESIAN_POINT('Ctrl Pts',(132.784251648261,36.9336278309288,21.2327866148261));
#41864=CARTESIAN_POINT('Ctrl Pts',(132.77057835594,36.9531690776478,21.234177062109));
#41865=CARTESIAN_POINT('Ctrl Pts',(132.73790686114,36.9988281614496,21.2374323043555));
#41866=CARTESIAN_POINT('Ctrl Pts',(132.718739210369,37.0248222658681,21.2392905478241));
#41867=CARTESIAN_POINT('Ctrl Pts',(132.660423487591,37.1015854657769,21.2447967908453));
#41868=CARTESIAN_POINT('Ctrl Pts',(132.620202665668,37.1515234883054,21.2484034836183));
#41869=CARTESIAN_POINT('Ctrl Pts',(132.472626587217,37.3244722121546,21.2610287433338));
#41870=CARTESIAN_POINT('Ctrl Pts',(132.35782780728,37.4408415255019,21.269763344948));
#41871=CARTESIAN_POINT('Ctrl Pts',(132.077113861039,37.6870340645996,21.289586796411));
#41872=CARTESIAN_POINT('Ctrl Pts',(131.906619338272,37.8105764631581,21.3005838628485));
#41873=CARTESIAN_POINT('Ctrl Pts',(131.687006581584,37.9404840054754,21.3148470834164));
#41874=CARTESIAN_POINT('Ctrl Pts',(131.647753259046,37.9626586356544,21.3174009936397));
#41875=CARTESIAN_POINT('Ctrl Pts',(131.591879926439,37.9927682268302,21.3210589503074));
#41876=CARTESIAN_POINT('Ctrl Pts',(131.575618084752,38.0013615207472,21.3221262512647));
#41877=CARTESIAN_POINT('Ctrl Pts',(131.545787996981,38.0168154863686,21.3240903603761));
#41878=CARTESIAN_POINT('Ctrl Pts',(131.532241812037,38.0237181142276,21.3249846571824));
#41879=CARTESIAN_POINT('Ctrl Pts',(131.503551296207,38.0380954173613,21.3268845100766));
#41880=CARTESIAN_POINT('Ctrl Pts',(131.488397027897,38.0455483128494,21.3278912299232));
#41881=CARTESIAN_POINT('Ctrl Pts',(131.446160455547,38.0659298089003,21.330704669029));
#41882=CARTESIAN_POINT('Ctrl Pts',(131.418961832046,38.0786121615635,21.3325250179129));
#41883=CARTESIAN_POINT('Ctrl Pts',(131.356681694553,38.1066519328712,21.3367068885165));
#41884=CARTESIAN_POINT('Ctrl Pts',(131.321501375593,38.1217791943306,21.3390787615205));
#41885=CARTESIAN_POINT('Ctrl Pts',(131.202648939869,38.1705158194699,21.347106767073));
#41886=CARTESIAN_POINT('Ctrl Pts',(131.117896505443,38.2013810699406,21.3528550837187));
#41887=CARTESIAN_POINT('Ctrl Pts',(130.753003320304,38.3180105961848,21.3774516244916));
#41888=CARTESIAN_POINT('Ctrl Pts',(130.463543951183,38.3706665408219,21.3964461136882));
#41889=CARTESIAN_POINT('Ctrl Pts',(130.120162223955,38.3880003854235,21.4173366391746));
#41890=CARTESIAN_POINT('Ctrl Pts',(130.06937504214,38.3894207607509,21.4203894802327));
#41891=CARTESIAN_POINT('Ctrl Pts',(129.988896230471,38.3898617235049,21.4251706978793));
#41892=CARTESIAN_POINT('Ctrl Pts',(129.959217953193,38.3896345978137,21.4269217621508));
#41893=CARTESIAN_POINT('Ctrl Pts',(129.90298658836,38.3884656048035,21.4302175802166));
#41894=CARTESIAN_POINT('Ctrl Pts',(129.876434289955,38.3876012651165,21.4317645907531));
#41895=CARTESIAN_POINT('Ctrl Pts',(129.815667605839,38.3849077389183,21.4352850277209));
#41896=CARTESIAN_POINT('Ctrl Pts',(129.781465008626,38.3828717699949,21.4372519642436));
#41897=CARTESIAN_POINT('Ctrl Pts',(129.672243050639,38.3747066847006,21.443491326659));
#41898=CARTESIAN_POINT('Ctrl Pts',(129.59739225161,38.3665973862088,21.4477034772471));
#41899=CARTESIAN_POINT('Ctrl Pts',(129.415917493554,38.3407967056482,21.4578131898332));
#41900=CARTESIAN_POINT('Ctrl Pts',(129.30974910089,38.3204865320446,21.4636392133884));
#41901=CARTESIAN_POINT('Ctrl Pts',(129.00959545413,38.2480452890874,21.480122175672));
#41902=CARTESIAN_POINT('Ctrl Pts',(128.819043973823,38.1837139111959,21.4905852867816));
#41903=CARTESIAN_POINT('Ctrl Pts',(128.560090377842,38.069823851479,21.5060108365125));
#41904=CARTESIAN_POINT('Ctrl Pts',(128.486100203053,38.0340177310372,21.5105706512268));
#41905=CARTESIAN_POINT('Ctrl Pts',(128.391282482039,37.9838003465354,21.5167069468011));
#41906=CARTESIAN_POINT('Ctrl Pts',(128.369207311317,37.971792672351,21.5181569856169));
#41907=CARTESIAN_POINT('Ctrl Pts',(128.334804793392,37.9525808662684,21.5204537150655));
#41908=CARTESIAN_POINT('Ctrl Pts',(128.322385539367,37.9455421492811,21.5212904833712));
#41909=CARTESIAN_POINT('Ctrl Pts',(128.296577701063,37.9306991812168,21.5230461253651));
#41910=CARTESIAN_POINT('Ctrl Pts',(128.28319766692,37.9228812729825,21.5239659273597));
#41911=CARTESIAN_POINT('Ctrl Pts',(128.249701909015,37.9030004845914,21.5262919114362));
#41912=CARTESIAN_POINT('Ctrl Pts',(128.229657099984,37.8908201552578,21.5277051883446));
#41913=CARTESIAN_POINT('Ctrl Pts',(128.148395497582,37.840279005941,21.5335171321417));
#41914=CARTESIAN_POINT('Ctrl Pts',(128.088289628102,37.800176073527,21.5380088262062));
#41915=CARTESIAN_POINT('Ctrl Pts',(127.917054047593,37.6778431338006,21.5512788691473));
#41916=CARTESIAN_POINT('Ctrl Pts',(127.809616123247,37.590699415582,21.5602085555482));
#41917=CARTESIAN_POINT('Ctrl Pts',(127.546608694519,37.3492872954638,21.5832138659074));
#41918=CARTESIAN_POINT('Ctrl Pts',(127.40009855453,37.1860507072318,21.5971685226719));
#41919=CARTESIAN_POINT('Ctrl Pts',(127.239068679673,36.9673444094585,21.6137026321429));
#41920=CARTESIAN_POINT('Ctrl Pts',(127.208797091498,36.9241550278903,21.6168768179205));
#41921=CARTESIAN_POINT('Ctrl Pts',(127.16269914587,36.8550070492302,21.6218199817447));
#41922=CARTESIAN_POINT('Ctrl Pts',(127.146194008049,36.8295132521392,21.6236137343507));
#41923=CARTESIAN_POINT('Ctrl Pts',(127.11608736585,36.7816115783088,21.6269321404692));
#41924=CARTESIAN_POINT('Ctrl Pts',(127.102398969492,36.7592612717466,21.6284598716567));
#41925=CARTESIAN_POINT('Ctrl Pts',(127.072051513625,36.7083949263889,21.6318917102578));
#41926=CARTESIAN_POINT('Ctrl Pts',(127.055547070627,36.6797894570398,21.6337902039268));
#41927=CARTESIAN_POINT('Ctrl Pts',(127.006297779011,36.5914738478518,21.6395600208409));
#41928=CARTESIAN_POINT('Ctrl Pts',(126.974930943181,36.5310127555541,21.6433836457532));
#41929=CARTESIAN_POINT('Ctrl Pts',(126.899435868449,36.3740994249191,21.6530287941239));
#41930=CARTESIAN_POINT('Ctrl Pts',(126.858009975527,36.2765234378314,21.6587653597668));
#41931=CARTESIAN_POINT('Ctrl Pts',(126.821242031451,36.1772437470164,21.6644319010721));
#41932=CARTESIAN_POINT('Origin',(130.,35.,23.));
#41933=CARTESIAN_POINT('',(126.821241918358,36.1772434416445,22.9104377666251));
#41934=CARTESIAN_POINT('',(126.821241895364,36.1772433795577,22.5700842967619));
#41935=CARTESIAN_POINT('',(126.821241918358,36.1772434416438,23.));
#41936=CARTESIAN_POINT('Ctrl Pts',(126.821241895364,36.1772433795577,22.5700842967619));
#41937=CARTESIAN_POINT('Ctrl Pts',(126.875225501832,36.3230083331407,22.5618217349734));
#41938=CARTESIAN_POINT('Ctrl Pts',(126.939183478084,36.4649200608349,22.5536544970183));
#41939=CARTESIAN_POINT('Ctrl Pts',(127.04434190883,36.6610177047732,22.5416107837619));
#41940=CARTESIAN_POINT('Ctrl Pts',(127.077749652317,36.7191121465268,22.537939604011));
#41941=CARTESIAN_POINT('Ctrl Pts',(127.13662180678,36.8148078998927,22.5316542712977));
#41942=CARTESIAN_POINT('Ctrl Pts',(127.161160408686,36.8529575700016,22.5290823090787));
#41943=CARTESIAN_POINT('Ctrl Pts',(127.197501754479,36.9070398211168,22.5253227374369));
#41944=CARTESIAN_POINT('Ctrl Pts',(127.208691300128,36.9233806166307,22.5241715278098));
#41945=CARTESIAN_POINT('Ctrl Pts',(127.228576270911,36.9518808912746,22.5221349878048));
#41946=CARTESIAN_POINT('Ctrl Pts',(127.237209935267,36.9640823674703,22.5212536651132));
#41947=CARTESIAN_POINT('Ctrl Pts',(127.25644081933,36.990882587254,22.5192965508899));
#41948=CARTESIAN_POINT('Ctrl Pts',(127.267073906163,37.0054539106027,22.5182184934474));
#41949=CARTESIAN_POINT('Ctrl Pts',(127.29906426764,37.0485658205786,22.5149887532843));
#41950=CARTESIAN_POINT('Ctrl Pts',(127.320755364013,37.0768542835653,22.5128165804459));
#41951=CARTESIAN_POINT('Ctrl Pts',(127.432680584142,37.2181497589344,22.5017178884316));
#41952=CARTESIAN_POINT('Ctrl Pts',(127.529628601901,37.3256345071104,22.4924602846372));
#41953=CARTESIAN_POINT('Ctrl Pts',(127.721878273514,37.5131523681107,22.4751668518684));
#41954=CARTESIAN_POINT('Ctrl Pts',(127.815307407623,37.5947819406969,22.4671568954737));
#41955=CARTESIAN_POINT('Ctrl Pts',(127.996097781847,37.7360375827837,22.4525313924841));
#41956=CARTESIAN_POINT('Ctrl Pts',(128.082185171625,37.797054698561,22.4458932087927));
#41957=CARTESIAN_POINT('Ctrl Pts',(128.233316088329,37.8939098397905,22.4348186512555));
#41958=CARTESIAN_POINT('Ctrl Pts',(128.296944042274,37.9318062479353,22.4303179910704));
#41959=CARTESIAN_POINT('Ctrl Pts',(128.391579325192,37.9840488775618,22.4238539947896));
#41960=CARTESIAN_POINT('Ctrl Pts',(128.421639769832,38.0000573130537,22.4218333253232));
#41961=CARTESIAN_POINT('Ctrl Pts',(128.475550057008,38.0277321439586,22.4182657481259));
#41962=CARTESIAN_POINT('Ctrl Pts',(128.499304954907,38.0395762871399,22.4167127952853));
#41963=CARTESIAN_POINT('Ctrl Pts',(128.550014494159,38.0641205515884,22.4134368923964));
#41964=CARTESIAN_POINT('Ctrl Pts',(128.577002510905,38.0767468127269,22.4117165598567));
#41965=CARTESIAN_POINT('Ctrl Pts',(128.650963668166,38.1101679342132,22.4070621615483));
#41966=CARTESIAN_POINT('Ctrl Pts',(128.69824954404,38.1302539422821,22.4041518421853));
#41967=CARTESIAN_POINT('Ctrl Pts',(128.977648396678,38.2415096665208,22.3872995504473));
#41968=CARTESIAN_POINT('Ctrl Pts',(129.218791812696,38.3079166523496,22.374198100807));
#41969=CARTESIAN_POINT('Ctrl Pts',(129.582428971256,38.3660315475674,22.3546418414912));
#41970=CARTESIAN_POINT('Ctrl Pts',(129.70070353675,38.3786021360902,22.34829738838));
#41971=CARTESIAN_POINT('Ctrl Pts',(129.885466481718,38.3884607355536,22.33810705976));
#41972=CARTESIAN_POINT('Ctrl Pts',(129.951631511365,38.3900506531305,22.3344018227716));
#41973=CARTESIAN_POINT('Ctrl Pts',(130.040559845929,38.3895837741391,22.3292975034845));
#41974=CARTESIAN_POINT('Ctrl Pts',(130.063321105859,38.389234963834,22.3279800893559));
#41975=CARTESIAN_POINT('Ctrl Pts',(130.101436401956,38.3882667839256,22.3257530956019));
#41976=CARTESIAN_POINT('Ctrl Pts',(130.116793321593,38.3877721965517,22.3248501250248));
#41977=CARTESIAN_POINT('Ctrl Pts',(130.148661475368,38.3865289004955,22.3229636064933));
#41978=CARTESIAN_POINT('Ctrl Pts',(130.165171323603,38.3857638188142,22.3219792789654));
#41979=CARTESIAN_POINT('Ctrl Pts',(130.209951597913,38.3833603539918,22.3192916976235));
#41980=CARTESIAN_POINT('Ctrl Pts',(130.238207546472,38.3814884310336,22.3175766460016));
#41981=CARTESIAN_POINT('Ctrl Pts',(130.417174789027,38.367377879468,22.3066057982526));
#41982=CARTESIAN_POINT('Ctrl Pts',(130.566936597936,38.3454212194724,22.2969459503887));
#41983=CARTESIAN_POINT('Ctrl Pts',(130.901919672664,38.2731668387252,22.2748900726358));
#41984=CARTESIAN_POINT('Ctrl Pts',(131.085379166613,38.2169928459768,22.2625034731648));
#41985=CARTESIAN_POINT('Ctrl Pts',(131.361744336801,38.1060187485805,22.2438387105796));
#41986=CARTESIAN_POINT('Ctrl Pts',(131.458458241516,38.061797390988,22.2372999180053));
#41987=CARTESIAN_POINT('Ctrl Pts',(131.587288169342,37.9953988565946,22.2285878548181));
#41988=CARTESIAN_POINT('Ctrl Pts',(131.621329746082,37.9771106936778,22.2262852851839));
#41989=CARTESIAN_POINT('Ctrl Pts',(131.678818464032,37.9449474112908,22.2223943749332));
#41990=CARTESIAN_POINT('Ctrl Pts',(131.702424041903,37.9313647225282,22.2207960070167));
#41991=CARTESIAN_POINT('Ctrl Pts',(131.7499680119,37.9032398015578,22.2175742984434));
#41992=CARTESIAN_POINT('Ctrl Pts',(131.773894996457,37.8886823982747,22.2159516618953));
#41993=CARTESIAN_POINT('Ctrl Pts',(131.833805184936,37.8512073493534,22.2118837861877));
#41994=CARTESIAN_POINT('Ctrl Pts',(131.86954181389,37.8279035415976,22.209452697161));
#41995=CARTESIAN_POINT('Ctrl Pts',(132.017179617188,37.72760685592,22.1993764829358));
#41996=CARTESIAN_POINT('Ctrl Pts',(132.124846239559,37.6445957052157,22.1919544186748));
#41997=CARTESIAN_POINT('Ctrl Pts',(132.392861901169,37.4109917086358,22.1728582887691));
#41998=CARTESIAN_POINT('Ctrl Pts',(132.54403999127,37.2508935064661,22.1614542791697));
#41999=CARTESIAN_POINT('Ctrl Pts',(132.716289259051,37.0287799853229,22.1461834313152));
#42000=CARTESIAN_POINT('Ctrl Pts',(132.752591867791,36.9792455248811,22.1428062646297));
#42001=CARTESIAN_POINT('Ctrl Pts',(132.811778717054,36.8937059116401,22.1369729486467));
#42002=CARTESIAN_POINT('Ctrl Pts',(132.835365711525,36.8582041250205,22.1345515047984));
#42003=CARTESIAN_POINT('Ctrl Pts',(132.868670118405,36.8059652979876,22.1309735325103));
#42004=CARTESIAN_POINT('Ctrl Pts',(132.878924333038,36.789573567079,22.1298487260907));
#42005=CARTESIAN_POINT('Ctrl Pts',(132.89684151262,36.7603797613966,22.1278401021512));
#42006=CARTESIAN_POINT('Ctrl Pts',(132.904561037384,36.7476134636984,22.1269598753378));
#42007=CARTESIAN_POINT('Ctrl Pts',(132.921618874079,36.7189785353462,22.1249811132792));
#42008=CARTESIAN_POINT('Ctrl Pts',(132.930912256793,36.7030846600515,22.1238799647535));
#42009=CARTESIAN_POINT('Ctrl Pts',(132.958777235811,36.6545253861387,22.1205089946005));
#42010=CARTESIAN_POINT('Ctrl Pts',(132.976934989941,36.6216272071616,22.1182160662738));
#42011=CARTESIAN_POINT('Ctrl Pts',(133.096953143681,36.3953672704998,22.1024187225744));
#42012=CARTESIAN_POINT('Ctrl Pts',(133.180447730085,36.1928585939215,22.0881808117108));
#42013=CARTESIAN_POINT('Ctrl Pts',(133.30225564042,35.7911972523882,22.0612069892058));
#42014=CARTESIAN_POINT('Ctrl Pts',(133.343394346909,35.5938191217872,22.0484946449271));
#42015=CARTESIAN_POINT('Ctrl Pts',(133.372016799823,35.349194261321,22.0336000612373));
#42016=CARTESIAN_POINT('Ctrl Pts',(133.376359310997,35.3043550987991,22.0309029574918));
#42017=CARTESIAN_POINT('Ctrl Pts',(133.381987590566,35.2310340089054,22.0265446647513));
#42018=CARTESIAN_POINT('Ctrl Pts',(133.383809995617,35.2026000090199,22.0248672164181));
#42019=CARTESIAN_POINT('Ctrl Pts',(133.386658259316,35.1472317184419,22.0216244942526));
#42020=CARTESIAN_POINT('Ctrl Pts',(133.38772179104,35.1203015890409,22.0200581806794));
#42021=CARTESIAN_POINT('Ctrl Pts',(133.389483011235,35.0563795253591,22.0163647799393));
#42022=CARTESIAN_POINT('Ctrl Pts',(133.389896487049,35.0193828208012,22.0142465428893));
#42023=CARTESIAN_POINT('Ctrl Pts',(133.389250356096,34.8950410974227,22.0071861394184));
#42024=CARTESIAN_POINT('Ctrl Pts',(133.385420668719,34.8077425342614,22.002327584243));
#42025=CARTESIAN_POINT('Ctrl Pts',(133.355757611513,34.4489787566194,21.9826170830355));
#42026=CARTESIAN_POINT('Ctrl Pts',(133.300599176495,34.1809950061153,21.968585924795));
#42027=CARTESIAN_POINT('Ctrl Pts',(133.192848435691,33.859592772917,21.9502308017877));
#42028=CARTESIAN_POINT('Ctrl Pts',(133.169909921302,33.7973030358979,21.9465929370727));
#42029=CARTESIAN_POINT('Ctrl Pts',(133.128355978564,33.6939281494664,21.9403585656468));
#42030=CARTESIAN_POINT('Ctrl Pts',(133.110721862331,33.6524674769688,21.9378033659265));
#42031=CARTESIAN_POINT('Ctrl Pts',(133.084175508649,33.593352675142,21.9340639779516));
#42032=CARTESIAN_POINT('Ctrl Pts',(133.075926228343,33.575404246216,21.9329156532463));
#42033=CARTESIAN_POINT('Ctrl Pts',(133.061161522789,33.5440060039617,21.9308822090732));
#42034=CARTESIAN_POINT('Ctrl Pts',(133.054713295202,33.5305255847754,21.9300010518782));
#42035=CARTESIAN_POINT('Ctrl Pts',(133.04026788089,33.5008325489308,21.9280417733783));
#42036=CARTESIAN_POINT('Ctrl Pts',(133.032230115397,33.4846411880798,21.9269613502632));
#42037=CARTESIAN_POINT('Ctrl Pts',(133.007870204435,33.4365402075092,21.9237173050272));
#42038=CARTESIAN_POINT('Ctrl Pts',(132.991171536618,33.4048253049535,21.9215329345346));
#42039=CARTESIAN_POINT('Ctrl Pts',(132.902689487806,33.2430519876629,21.9101775712375));
#42040=CARTESIAN_POINT('Ctrl Pts',(132.822920210585,33.1175582039464,21.9006576360235));
#42041=CARTESIAN_POINT('Ctrl Pts',(132.660088279477,32.8951249345666,21.8829012537954));
#42042=CARTESIAN_POINT('Ctrl Pts',(132.579275751378,32.7968415221911,21.8746901964973));
#42043=CARTESIAN_POINT('Ctrl Pts',(132.424597550314,32.6289320037647,21.8601615863824));
#42044=CARTESIAN_POINT('Ctrl Pts',(132.35276416376,32.5576363565423,21.8538060371207));
#42045=CARTESIAN_POINT('Ctrl Pts',(132.224571216312,32.4413162128416,21.8431393918312));
#42046=CARTESIAN_POINT('Ctrl Pts',(132.169769836736,32.3946823919707,21.8387702700472));
#42047=CARTESIAN_POINT('Ctrl Pts',(132.087177638633,32.3288148588872,21.8324560743247));
#42048=CARTESIAN_POINT('Ctrl Pts',(132.060520106401,32.3081980816888,21.8304573818686));
#42049=CARTESIAN_POINT('Ctrl Pts',(132.012351936533,32.2720800341061,21.8269140471918));
#42050=CARTESIAN_POINT('Ctrl Pts',(131.990958816923,32.2564273828991,21.8253636606872));
#42051=CARTESIAN_POINT('Ctrl Pts',(131.944959874856,32.2235928568047,21.8220783379534));
#42052=CARTESIAN_POINT('Ctrl Pts',(131.920304944633,32.2064834808644,21.8203462197528));
#42053=CARTESIAN_POINT('Ctrl Pts',(131.853100366146,32.1611568530082,21.8156993653701));
#42054=CARTESIAN_POINT('Ctrl Pts',(131.810134328719,32.1335692100242,21.812807748968));
#42055=CARTESIAN_POINT('Ctrl Pts',(131.556048120684,31.9784179696819,21.7961286814565));
#42056=CARTESIAN_POINT('Ctrl Pts',(131.332136474049,31.873233737867,21.7831603941922));
#42057=CARTESIAN_POINT('Ctrl Pts',(130.984876951053,31.7542459941395,21.7636706808566));
#42058=CARTESIAN_POINT('Ctrl Pts',(130.868983640072,31.721316445292,21.7572480507225));
#42059=CARTESIAN_POINT('Ctrl Pts',(130.686566189901,31.6798375212574,21.7469483223157));
#42060=CARTESIAN_POINT('Ctrl Pts',(130.621122555579,31.6669747039963,21.7432154948441));
#42061=CARTESIAN_POINT('Ctrl Pts',(130.532830222228,31.6523115449429,21.7380788432203));
#42062=CARTESIAN_POINT('Ctrl Pts',(130.510277200969,31.6487997441104,21.7367580134896));
#42063=CARTESIAN_POINT('Ctrl Pts',(130.472474911686,31.6433038644206,21.7345269381371));
#42064=CARTESIAN_POINT('Ctrl Pts',(130.457244039303,31.6411952467991,21.7336233569919));
#42065=CARTESIAN_POINT('Ctrl Pts',(130.425633760551,31.6370379974408,21.7317375219648));
#42066=CARTESIAN_POINT('Ctrl Pts',(130.409253005887,31.6350052777425,21.730754511883));
#42067=CARTESIAN_POINT('Ctrl Pts',(130.364829611908,31.629821855153,21.7280742865907));
#42068=CARTESIAN_POINT('Ctrl Pts',(130.33676201517,31.6269016311466,21.7263653772958));
#42069=CARTESIAN_POINT('Ctrl Pts',(130.169927402457,31.6116467093522,21.7161285458181));
#42070=CARTESIAN_POINT('Ctrl Pts',(130.030554460559,31.6075270525656,21.7072577501609));
#42071=CARTESIAN_POINT('Ctrl Pts',(129.690943783304,31.6184192464574,21.685417818628));
#42072=CARTESIAN_POINT('Ctrl Pts',(129.491497665301,31.6426139686564,21.672422138017));
#42073=CARTESIAN_POINT('Ctrl Pts',(129.189019170228,31.7068962072239,21.6530221978412));
#42074=CARTESIAN_POINT('Ctrl Pts',(129.083826876762,31.734597552331,21.6463285350691));
#42075=CARTESIAN_POINT('Ctrl Pts',(128.943019836274,31.7790198771942,21.6374507415542));
#42076=CARTESIAN_POINT('Ctrl Pts',(128.906104177428,31.7913691180207,21.6351307402485));
#42077=CARTESIAN_POINT('Ctrl Pts',(128.843686304791,31.8134520040832,21.6312193777857));
#42078=CARTESIAN_POINT('Ctrl Pts',(128.818074673809,31.8228625965841,21.6296177321195));
#42079=CARTESIAN_POINT('Ctrl Pts',(128.769531151717,31.8413674059478,21.6265873791212));
#42080=CARTESIAN_POINT('Ctrl Pts',(128.74657957293,31.8504046719075,21.6251569239996));
#42081=CARTESIAN_POINT('Ctrl Pts',(128.692955641821,31.8721983003785,21.6218191680345));
#42082=CARTESIAN_POINT('Ctrl Pts',(128.662367820567,31.8851567151857,21.6199186555321));
#42083=CARTESIAN_POINT('Ctrl Pts',(128.553199972666,31.9333100016939,21.6131428853398));
#42084=CARTESIAN_POINT('Ctrl Pts',(128.475774026608,31.9710472649369,21.6083517238278));
#42085=CARTESIAN_POINT('Ctrl Pts',(128.158333326709,32.1410258953333,21.5886249461558));
#42086=CARTESIAN_POINT('Ctrl Pts',(127.933389135964,32.2991521472882,21.5745270887007));
#42087=CARTESIAN_POINT('Ctrl Pts',(127.680569579761,32.527134068082,21.556094768226));
#42088=CARTESIAN_POINT('Ctrl Pts',(127.632528014676,32.5730886075578,21.5524515315607));
#42089=CARTESIAN_POINT('Ctrl Pts',(127.55420970803,32.6525441222596,21.5462089383984));
#42090=CARTESIAN_POINT('Ctrl Pts',(127.523194271577,32.6852921932327,21.5436510307822));
#42091=CARTESIAN_POINT('Ctrl Pts',(127.479542962563,32.7332640393114,21.5399083815639));
#42092=CARTESIAN_POINT('Ctrl Pts',(127.466371364697,32.7479961166553,21.5387595898787));
#42093=CARTESIAN_POINT('Ctrl Pts',(127.443466587,32.7740697873581,21.5367256452948));
#42094=CARTESIAN_POINT('Ctrl Pts',(127.433678426781,32.7853618864472,21.5358444620217));
#42095=CARTESIAN_POINT('Ctrl Pts',(127.412219366511,32.8104514159602,21.5338855369812));
#42096=CARTESIAN_POINT('Ctrl Pts',(127.400584067443,32.824277502484,21.5328054992466));
#42097=CARTESIAN_POINT('Ctrl Pts',(127.366922243548,32.8649328908504,21.5296298020527));
#42098=CARTESIAN_POINT('Ctrl Pts',(127.345197240853,32.8920075566197,21.5275151123006));
#42099=CARTESIAN_POINT('Ctrl Pts',(127.209834375424,33.0661146729589,21.5139426893951));
#42100=CARTESIAN_POINT('Ctrl Pts',(127.108040904296,33.2219394164598,21.5019310810867));
#42101=CARTESIAN_POINT('Ctrl Pts',(126.943989974793,33.5247509189535,21.4797356075034));
#42102=CARTESIAN_POINT('Ctrl Pts',(126.878318044167,33.6693360963235,21.4695663874464));
#42103=CARTESIAN_POINT('Ctrl Pts',(126.789542813604,33.9079467108937,21.4536824040873));
#42104=CARTESIAN_POINT('Ctrl Pts',(126.759910304147,33.9992816673109,21.4477985235872));
#42105=CARTESIAN_POINT('Ctrl Pts',(126.724185335262,34.1277396397894,21.4397947847223));
#42106=CARTESIAN_POINT('Ctrl Pts',(126.714773733107,34.1638849382873,21.4375716957518));
#42107=CARTESIAN_POINT('Ctrl Pts',(126.699588558702,34.2264246655947,21.433773566213));
#42108=CARTESIAN_POINT('Ctrl Pts',(126.69352977043,34.2527455830424,21.4321896525567));
#42109=CARTESIAN_POINT('Ctrl Pts',(126.681751704066,34.3068632978764,21.4289618683418));
#42110=CARTESIAN_POINT('Ctrl Pts',(126.676065601162,34.3346651785275,21.4273191523017));
#42111=CARTESIAN_POINT('Ctrl Pts',(126.662363998139,34.4062242534203,21.4231287783674));
#42112=CARTESIAN_POINT('Ctrl Pts',(126.654859365269,34.4500744502077,21.4205971266899));
#42113=CARTESIAN_POINT('Ctrl Pts',(126.622801559386,34.6624533174749,21.4084917881885));
#42114=CARTESIAN_POINT('Ctrl Pts',(126.61010777198,34.8325294876978,21.3992862819136));
#42115=CARTESIAN_POINT('Ctrl Pts',(126.610452581497,35.2419956021854,21.37746966976));
#42116=CARTESIAN_POINT('Ctrl Pts',(126.635959427902,35.4804181016502,21.3650622408845));
#42117=CARTESIAN_POINT('Ctrl Pts',(126.695861190542,35.758365398044,21.3491546717281));
#42118=CARTESIAN_POINT('Ctrl Pts',(126.706275144155,35.8023886319201,21.3465894054795));
#42119=CARTESIAN_POINT('Ctrl Pts',(126.722452815536,35.8651431615641,21.3428499875696));
#42120=CARTESIAN_POINT('Ctrl Pts',(126.727503279873,35.8840550964243,21.3417121992618));
#42121=CARTESIAN_POINT('Ctrl Pts',(126.736701095165,35.9173380081169,21.3396889132985));
#42122=CARTESIAN_POINT('Ctrl Pts',(126.740780200762,35.9317269194778,21.3388072003617));
#42123=CARTESIAN_POINT('Ctrl Pts',(126.749966795925,35.9633336605928,21.3368545829451));
#42124=CARTESIAN_POINT('Ctrl Pts',(126.755115896357,35.9805379602028,21.335781488118));
#42125=CARTESIAN_POINT('Ctrl Pts',(126.770773350142,36.0313787552242,21.3325816397422));
#42126=CARTESIAN_POINT('Ctrl Pts',(126.781669494679,36.0648922204941,21.3304349308154));
#42127=CARTESIAN_POINT('Ctrl Pts',(126.802146327224,36.1246862090647,21.3265448387815));
#42128=CARTESIAN_POINT('Ctrl Pts',(126.811532577294,36.1510265641211,21.3248100025831));
#42129=CARTESIAN_POINT('Ctrl Pts',(126.821241909055,36.1772434165241,21.3230640339373));
#42130=CARTESIAN_POINT('',(126.610250132112,35.0009463898671,21.731083596192));
#42131=CARTESIAN_POINT('Ctrl Pts',(126.821242031451,36.1772437470164,21.6644319010721));
#42132=CARTESIAN_POINT('Ctrl Pts',(126.771125806647,36.0419214321994,21.6721556306702));
#42133=CARTESIAN_POINT('Ctrl Pts',(126.729663516346,35.9034336601396,21.6797462668355));
#42134=CARTESIAN_POINT('Ctrl Pts',(126.685081021759,35.7103480487699,21.690316211781));
#42135=CARTESIAN_POINT('Ctrl Pts',(126.674256076812,35.6578064126016,21.6931920485904));
#42136=CARTESIAN_POINT('Ctrl Pts',(126.647643771163,35.5111024721233,21.7012705643072));
#42137=CARTESIAN_POINT('Ctrl Pts',(126.63458172262,35.4165031357547,21.7065348522985));
#42138=CARTESIAN_POINT('Ctrl Pts',(126.623044385766,35.2954021725561,21.7134815653526));
#42139=CARTESIAN_POINT('Ctrl Pts',(126.620861883431,35.2692901106178,21.7149916946813));
#42140=CARTESIAN_POINT('Ctrl Pts',(126.617829448891,35.2271249790515,21.71745369822));
#42141=CARTESIAN_POINT('Ctrl Pts',(126.616790571976,35.2110860863636,21.7183956746774));
#42142=CARTESIAN_POINT('Ctrl Pts',(126.615063214498,35.1811148686936,21.7201671196711));
#42143=CARTESIAN_POINT('Ctrl Pts',(126.614346598988,35.1671845235815,21.7209950205717));
#42144=CARTESIAN_POINT('Ctrl Pts',(126.613006261138,35.1375678885332,21.7227642901828));
#42145=CARTESIAN_POINT('Ctrl Pts',(126.612405492064,35.1218808444769,21.7237068444695));
#42146=CARTESIAN_POINT('Ctrl Pts',(126.610814474486,35.0711182665403,21.7267732381405));
#42147=CARTESIAN_POINT('Ctrl Pts',(126.6102599279,35.0360326396975,21.728917842519));
#42148=CARTESIAN_POINT('Ctrl Pts',(126.610250132112,35.0009463898671,21.731083596192));
#42149=CARTESIAN_POINT('Ctrl Pts',(126.610250133166,35.0009501562718,21.7310833637049));
#42150=CARTESIAN_POINT('Ctrl Pts',(126.610185136217,34.7690689316006,21.7453965851487));
#42151=CARTESIAN_POINT('Ctrl Pts',(126.633913061281,34.5377934983256,21.7605470636322));
#42152=CARTESIAN_POINT('Ctrl Pts',(126.716100312233,34.1420372335761,21.7864708213844));
#42153=CARTESIAN_POINT('Ctrl Pts',(126.763954461802,33.9762227578437,21.7973414354496));
#42154=CARTESIAN_POINT('Ctrl Pts',(126.842599677253,33.765499429003,21.811026118617));
#42155=CARTESIAN_POINT('Ctrl Pts',(126.862124328879,33.7166819594367,21.8141885434586));
#42156=CARTESIAN_POINT('Ctrl Pts',(126.894578255613,33.6407122464022,21.8190995686375));
#42157=CARTESIAN_POINT('Ctrl Pts',(126.906746049075,33.6132456996012,21.8208729997598));
#42158=CARTESIAN_POINT('Ctrl Pts',(126.930333074148,33.5618580123141,21.8241879615392));
#42159=CARTESIAN_POINT('Ctrl Pts',(126.941670812141,33.537902174995,21.8257320873769));
#42160=CARTESIAN_POINT('Ctrl Pts',(126.968038171882,33.4838388311011,21.8292152256595));
#42161=CARTESIAN_POINT('Ctrl Pts',(126.983237604426,33.4538169636571,21.8311482672978));
#42162=CARTESIAN_POINT('Ctrl Pts',(127.032192968928,33.3605915734959,21.8371514658501));
#42163=CARTESIAN_POINT('Ctrl Pts',(127.067508237429,33.2982269201851,21.8411678669521));
#42164=CARTESIAN_POINT('Ctrl Pts',(127.258034536226,32.9853373475992,21.8614154016649));
#42165=CARTESIAN_POINT('Ctrl Pts',(127.44344388813,32.7547269176752,21.8765394219163));
#42166=CARTESIAN_POINT('Ctrl Pts',(127.705398385339,32.5040389620112,21.8961530042115));
#42167=CARTESIAN_POINT('Ctrl Pts',(127.755865992799,32.4585673920826,21.8998721234481));
#42168=CARTESIAN_POINT('Ctrl Pts',(127.842590023496,32.3850268828863,21.9062306761191));
#42169=CARTESIAN_POINT('Ctrl Pts',(127.878112364205,32.3561212867045,21.9088266313155));
#42170=CARTESIAN_POINT('Ctrl Pts',(127.929876783607,32.3157142356581,21.9126150773015));
#42171=CARTESIAN_POINT('Ctrl Pts',(127.94565295177,32.3036212507069,21.9137703940878));
#42172=CARTESIAN_POINT('Ctrl Pts',(127.973481738142,32.2826755056885,21.9158113613552));
#42173=CARTESIAN_POINT('Ctrl Pts',(127.985488004876,32.2737626509971,21.9166929395694));
#42174=CARTESIAN_POINT('Ctrl Pts',(128.012064958381,32.2543046774915,21.9186470586094));
#42175=CARTESIAN_POINT('Ctrl Pts',(128.026660646407,32.2437960348655,21.9197218150898));
#42176=CARTESIAN_POINT('Ctrl Pts',(128.070211164312,32.2129636638088,21.9229316467005));
#42177=CARTESIAN_POINT('Ctrl Pts',(128.099400434427,32.1929770986787,21.9250868550094));
#42178=CARTESIAN_POINT('Ctrl Pts',(128.277882386406,32.0748265122162,21.9382628217981));
#42179=CARTESIAN_POINT('Ctrl Pts',(128.434422509681,31.9881423050445,21.9497938095468));
#42180=CARTESIAN_POINT('Ctrl Pts',(128.745650283263,31.8466433242713,21.9718310495977));
#42181=CARTESIAN_POINT('Ctrl Pts',(128.898947753035,31.7898997732664,21.9823118455692));
#42182=CARTESIAN_POINT('Ctrl Pts',(129.149452635028,31.7172429949641,21.998596902524));
#42183=CARTESIAN_POINT('Ctrl Pts',(129.244293575863,31.6941211468368,22.0045819160143));
#42184=CARTESIAN_POINT('Ctrl Pts',(129.376845565108,31.6678094100864,22.0126958534776));
#42185=CARTESIAN_POINT('Ctrl Pts',(129.413803670408,31.6611095240125,22.0149318517724));
#42186=CARTESIAN_POINT('Ctrl Pts',(129.477552619862,31.6506440721136,22.0187449940313));
#42187=CARTESIAN_POINT('Ctrl Pts',(129.504290622375,31.6465825382578,22.0203311965248));
#42188=CARTESIAN_POINT('Ctrl Pts',(129.55911303108,31.6389249912598,22.0235576350993));
#42189=CARTESIAN_POINT('Ctrl Pts',(129.587199658606,31.6353599772693,22.0251967932837));
#42190=CARTESIAN_POINT('Ctrl Pts',(129.659204632036,31.6271356640919,22.0293656135273));
#42191=CARTESIAN_POINT('Ctrl Pts',(129.703176048789,31.6229819209446,22.0318796012494));
#42192=CARTESIAN_POINT('Ctrl Pts',(129.906611045155,31.6077688869603,22.0433805957766));
#42193=CARTESIAN_POINT('Ctrl Pts',(130.066655911016,31.6071372037975,22.0520479730548));
#42194=CARTESIAN_POINT('Ctrl Pts',(130.423029488387,31.6309673075347,22.0711159478476));
#42195=CARTESIAN_POINT('Ctrl Pts',(130.618361038132,31.6612940092652,22.0814055127796));
#42196=CARTESIAN_POINT('Ctrl Pts',(130.893989806104,31.7291163042595,22.0968578131764));
#42197=CARTESIAN_POINT('Ctrl Pts',(130.977214478109,31.7530094763389,22.1016545409279));
#42198=CARTESIAN_POINT('Ctrl Pts',(131.083028570371,31.787824486902,22.1080279089504));
#42199=CARTESIAN_POINT('Ctrl Pts',(131.106543561795,31.7958489923484,22.1094620890962));
#42200=CARTESIAN_POINT('Ctrl Pts',(131.144846209414,31.80939170831,22.1118306449235));
#42201=CARTESIAN_POINT('Ctrl Pts',(131.159687739289,31.81475614083,22.1127564590557));
#42202=CARTESIAN_POINT('Ctrl Pts',(131.18943990428,31.8257454836426,22.1146296188666));
#42203=CARTESIAN_POINT('Ctrl Pts',(131.204349367739,31.8313722847083,22.1155770442873));
#42204=CARTESIAN_POINT('Ctrl Pts',(131.24307597267,31.8463004335149,22.1180597315593));
#42205=CARTESIAN_POINT('Ctrl Pts',(131.266828093659,31.8557663374046,22.1196040350218));
#42206=CARTESIAN_POINT('Ctrl Pts',(131.371109441346,31.8986988450281,22.1264727344473));
#42207=CARTESIAN_POINT('Ctrl Pts',(131.450431645843,31.9349950042574,22.1319315290125));
#42208=CARTESIAN_POINT('Ctrl Pts',(131.723538170903,32.0729394316787,22.1513542509982));
#42209=CARTESIAN_POINT('Ctrl Pts',(131.908811211507,32.1902467193027,22.1656400187615));
#42210=CARTESIAN_POINT('Ctrl Pts',(132.155889216488,32.3824760425944,22.1855028250328));
#42211=CARTESIAN_POINT('Ctrl Pts',(132.227842605618,32.4434379493351,22.1914069512509));
#42212=CARTESIAN_POINT('Ctrl Pts',(132.347511495781,32.5537207462146,22.2014142791882));
#42213=CARTESIAN_POINT('Ctrl Pts',(132.39644239102,32.6016344557052,22.2055661635953));
#42214=CARTESIAN_POINT('Ctrl Pts',(132.466820776393,32.6748558788899,22.2116316019938));
#42215=CARTESIAN_POINT('Ctrl Pts',(132.489400375891,32.6990467602028,22.2135928873867));
#42216=CARTESIAN_POINT('Ctrl Pts',(132.529389047945,32.7431668255357,22.2170954949322));
#42217=CARTESIAN_POINT('Ctrl Pts',(132.546925606437,32.7629763194571,22.2186420499808));
#42218=CARTESIAN_POINT('Ctrl Pts',(132.584119253654,32.805995070664,22.2219461469238));
#42219=CARTESIAN_POINT('Ctrl Pts',(132.603699613965,32.8292677838951,22.2237005014157));
#42220=CARTESIAN_POINT('Ctrl Pts',(132.656497312567,32.8937641444607,22.2284752524685));
#42221=CARTESIAN_POINT('Ctrl Pts',(132.689067020178,32.9355081897514,22.2314702366486));
#42222=CARTESIAN_POINT('Ctrl Pts',(132.844777895187,33.1450206681745,22.2460733612258));
#42223=CARTESIAN_POINT('Ctrl Pts',(132.953268749604,33.3231208749942,22.2571329321252));
#42224=CARTESIAN_POINT('Ctrl Pts',(133.108862974259,33.6410835689277,22.2759002461628));
#42225=CARTESIAN_POINT('Ctrl Pts',(133.164451006296,33.7761012828577,22.2836121177139));
#42226=CARTESIAN_POINT('Ctrl Pts',(133.235008555733,33.9847832069708,22.2956830777815));
#42227=CARTESIAN_POINT('Ctrl Pts',(133.256518973634,34.0560571499957,22.2998326282347));
#42228=CARTESIAN_POINT('Ctrl Pts',(133.281758803934,34.1508678579977,22.3054558379164));
#42229=CARTESIAN_POINT('Ctrl Pts',(133.287612612132,34.173822363689,22.306825153783));
#42230=CARTESIAN_POINT('Ctrl Pts',(133.296907886937,34.2119358986912,22.3091146074694));
#42231=CARTESIAN_POINT('Ctrl Pts',(133.300486646168,34.2270611083601,22.310027283591));
#42232=CARTESIAN_POINT('Ctrl Pts',(133.307141211445,34.2560749947266,22.3117867817737));
#42233=CARTESIAN_POINT('Ctrl Pts',(133.310233832377,34.2699593403977,22.3126325494457));
#42234=CARTESIAN_POINT('Ctrl Pts',(133.318492379371,34.3081678375939,22.3149696093761));
#42235=CARTESIAN_POINT('Ctrl Pts',(133.323478071746,34.3325295209846,22.316470354316));
#42236=CARTESIAN_POINT('Ctrl Pts',(133.343231493596,34.4347650116555,22.322806569415));
#42237=CARTESIAN_POINT('Ctrl Pts',(133.355532632564,34.5130849098086,22.327752716831));
#42238=CARTESIAN_POINT('Ctrl Pts',(133.389570346978,34.7936523774992,22.3456386592823));
#42239=CARTESIAN_POINT('Ctrl Pts',(133.395844665388,34.9973401507769,22.3589026368601));
#42240=CARTESIAN_POINT('Ctrl Pts',(133.377410047656,35.3086717116608,22.3788060385034));
#42241=CARTESIAN_POINT('Ctrl Pts',(133.365800204845,35.4166161332438,22.3856444539914));
#42242=CARTESIAN_POINT('Ctrl Pts',(133.337366225192,35.5984063675791,22.3970057762071));
#42243=CARTESIAN_POINT('Ctrl Pts',(133.323212233505,35.6725810677805,22.4015975956624));
#42244=CARTESIAN_POINT('Ctrl Pts',(133.299041897516,35.7796819470606,22.4081650495854));
#42245=CARTESIAN_POINT('Ctrl Pts',(133.290984059915,35.8130224026534,22.4102006582429));
#42246=CARTESIAN_POINT('Ctrl Pts',(133.275788524362,35.8719636014081,22.4137848342835));
#42247=CARTESIAN_POINT('Ctrl Pts',(133.268853283851,35.8976130830391,22.415339651587));
#42248=CARTESIAN_POINT('Ctrl Pts',(133.25354022307,35.9517145561435,22.4186097633576));
#42249=CARTESIAN_POINT('Ctrl Pts',(133.245089091695,35.9801435849834,22.420322570466));
#42250=CARTESIAN_POINT('Ctrl Pts',(133.221182757798,36.0568618965568,22.4249319711405));
#42251=CARTESIAN_POINT('Ctrl Pts',(133.205015236119,36.1049222319788,22.4278056216876));
#42252=CARTESIAN_POINT('Ctrl Pts',(133.101020619476,36.3925418740706,22.4449531645621));
#42253=CARTESIAN_POINT('Ctrl Pts',(132.987456783248,36.6219169825006,22.4583380015484));
#42254=CARTESIAN_POINT('Ctrl Pts',(132.786553059797,36.93362593827,22.4780418999169));
#42255=CARTESIAN_POINT('Ctrl Pts',(132.718949908545,37.0275836869717,22.4842242586241));
#42256=CARTESIAN_POINT('Ctrl Pts',(132.606008170176,37.1687241021567,22.4941869821473));
#42257=CARTESIAN_POINT('Ctrl Pts',(132.563882135444,37.2183665425879,22.4978341145279));
#42258=CARTESIAN_POINT('Ctrl Pts',(132.505220196106,37.2835912821238,22.5028702924944));
#42259=CARTESIAN_POINT('Ctrl Pts',(132.489916645425,37.3002679005011,22.504180427774));
#42260=CARTESIAN_POINT('Ctrl Pts',(132.463962465363,37.3279882696322,22.5063987403585));
#42261=CARTESIAN_POINT('Ctrl Pts',(132.453401477663,37.3391155587159,22.5073004264546));
#42262=CARTESIAN_POINT('Ctrl Pts',(132.43127439494,37.3621144281745,22.5091884801486));
#42263=CARTESIAN_POINT('Ctrl Pts',(132.41969628198,37.3739733850324,22.5101756778734));
#42264=CARTESIAN_POINT('Ctrl Pts',(132.387949990605,37.4060162185056,22.5128792947267));
#42265=CARTESIAN_POINT('Ctrl Pts',(132.367613620259,37.4260306737635,22.514607738994));
#42266=CARTESIAN_POINT('Ctrl Pts',(132.228178273114,37.5598358087644,22.5264204747788));
#42267=CARTESIAN_POINT('Ctrl Pts',(132.101183941304,37.6650617429714,22.5369827699567));
#42268=CARTESIAN_POINT('Ctrl Pts',(131.857631240868,37.8386026935512,22.5562500815089));
#42269=CARTESIAN_POINT('Ctrl Pts',(131.743659762656,37.9100021336918,22.5649240664566));
#42270=CARTESIAN_POINT('Ctrl Pts',(131.501289119615,38.0424748851552,22.5824549145191));
#42271=CARTESIAN_POINT('Ctrl Pts',(131.372672852509,38.102627893106,22.5912768848468));
#42272=CARTESIAN_POINT('Ctrl Pts',(131.2014989398,38.1699488019296,22.6023707342677));
#42273=CARTESIAN_POINT('Ctrl Pts',(131.162061675625,38.184617404044,22.6048846454384));
#42274=CARTESIAN_POINT('Ctrl Pts',(131.096044621136,38.2077825716159,22.6090251267297));
#42275=CARTESIAN_POINT('Ctrl Pts',(131.069615551006,38.2166916981156,22.6106649514572));
#42276=CARTESIAN_POINT('Ctrl Pts',(131.017385630406,38.2335832653519,22.6138717852138));
#42277=CARTESIAN_POINT('Ctrl Pts',(130.991593427256,38.2415855366864,22.6154393351417));
#42278=CARTESIAN_POINT('Ctrl Pts',(130.934351213932,38.2585983118098,22.6188842563285));
#42279=CARTESIAN_POINT('Ctrl Pts',(130.902860639959,38.267463529833,22.6207568927906));
#42280=CARTESIAN_POINT('Ctrl Pts',(130.792270079824,38.2968760272587,22.6272596072203));
#42281=CARTESIAN_POINT('Ctrl Pts',(130.712556942729,38.3150184661321,22.6318149187634));
#42282=CARTESIAN_POINT('Ctrl Pts',(130.402005222193,38.3739777361348,22.6491692540504));
#42283=CARTESIAN_POINT('Ctrl Pts',(130.167842092549,38.3936948931545,22.6613789063015));
#42284=CARTESIAN_POINT('Ctrl Pts',(129.794137748322,38.3863636728052,22.6813432456586));
#42285=CARTESIAN_POINT('Ctrl Pts',(129.655076647279,38.3750345481003,22.688893227768));
#42286=CARTESIAN_POINT('Ctrl Pts',(129.489518099407,38.3512074144264,22.6984232142029));
#42287=CARTESIAN_POINT('Ctrl Pts',(129.46196371905,38.3468940466031,22.700027642007));
#42288=CARTESIAN_POINT('Ctrl Pts',(129.418261066098,38.3394992162868,22.7026059371517));
#42289=CARTESIAN_POINT('Ctrl Pts',(129.402076003878,38.3366393381747,22.7035681527394));
#42290=CARTESIAN_POINT('Ctrl Pts',(129.370929901212,38.33090197641,22.7054351061322));
#42291=CARTESIAN_POINT('Ctrl Pts',(129.355966417397,38.328041147202,22.7063389490415));
#42292=CARTESIAN_POINT('Ctrl Pts',(129.318578288807,38.3206314270518,22.708613824594));
#42293=CARTESIAN_POINT('Ctrl Pts',(129.29617966386,38.3159561961234,22.7099915478526));
#42294=CARTESIAN_POINT('Ctrl Pts',(129.213279648547,38.2977748473846,22.7151416779097));
#42295=CARTESIAN_POINT('Ctrl Pts',(129.153107918049,38.282837291225,22.7189808451553));
#42296=CARTESIAN_POINT('Ctrl Pts',(128.881368540787,38.2074105303201,22.7366819321574));
#42297=CARTESIAN_POINT('Ctrl Pts',(128.675591133847,38.1280600251235,22.7510597703895));
#42298=CARTESIAN_POINT('Ctrl Pts',(128.379428464306,37.9793549700602,22.7722300759681));
#42299=CARTESIAN_POINT('Ctrl Pts',(128.282417992703,37.9245039862599,22.7792576601911));
#42300=CARTESIAN_POINT('Ctrl Pts',(128.123336891405,37.8239058718173,22.7908882365194));
#42301=CARTESIAN_POINT('Ctrl Pts',(128.05980787254,37.7806410619385,22.7955646577103));
#42302=CARTESIAN_POINT('Ctrl Pts',(127.96994586295,37.714862217285,22.8022278624333));
#42303=CARTESIAN_POINT('Ctrl Pts',(127.942403788916,37.6940479993052,22.8042771196634));
#42304=CARTESIAN_POINT('Ctrl Pts',(127.894213733997,37.6564594001493,22.8078765330194));
#42305=CARTESIAN_POINT('Ctrl Pts',(127.873436587783,37.6398561431246,22.8094331265583));
#42306=CARTESIAN_POINT('Ctrl Pts',(127.830000583806,37.6043002963895,22.812698331685));
#42307=CARTESIAN_POINT('Ctrl Pts',(127.807389644208,37.5852925187517,22.8144045709163));
#42308=CARTESIAN_POINT('Ctrl Pts',(127.747091646594,37.5332431249565,22.8189747654545));
#42309=CARTESIAN_POINT('Ctrl Pts',(127.709883451692,37.4996566438239,22.8218164680694));
#42310=CARTESIAN_POINT('Ctrl Pts',(127.484500890073,37.2869534792309,22.839199694401));
#42311=CARTESIAN_POINT('Ctrl Pts',(127.316693390111,37.0875268759518,22.8528117594899));
#42312=CARTESIAN_POINT('Ctrl Pts',(127.110822079402,36.7764772119614,22.8726394952216));
#42313=CARTESIAN_POINT('Ctrl Pts',(127.05311350517,36.6790108527592,22.878695607623));
#42314=CARTESIAN_POINT('Ctrl Pts',(126.970468729821,36.5219962967475,22.8884803264613));
#42315=CARTESIAN_POINT('Ctrl Pts',(126.942169542937,36.4643101739823,22.8920813498675));
#42316=CARTESIAN_POINT('Ctrl Pts',(126.906184228397,36.3853579421258,22.8970634009128));
#42317=CARTESIAN_POINT('Ctrl Pts',(126.897045130289,36.364765061904,22.8983676727469));
#42318=CARTESIAN_POINT('Ctrl Pts',(126.882036745769,36.3300169098345,22.9005790065444));
#42319=CARTESIAN_POINT('Ctrl Pts',(126.876056766035,36.3159097612529,22.9014796719121));
#42320=CARTESIAN_POINT('Ctrl Pts',(126.863793174131,36.2864244106126,22.9033690317465));
#42321=CARTESIAN_POINT('Ctrl Pts',(126.857526691458,36.2710399279242,22.9043585977638));
#42322=CARTESIAN_POINT('Ctrl Pts',(126.841006255287,36.2296125222993,22.9070321642731));
#42323=CARTESIAN_POINT('Ctrl Pts',(126.830961582237,36.2034881918925,22.9087274645162));
#42324=CARTESIAN_POINT('Ctrl Pts',(126.821241918358,36.1772434416451,22.910437766625));
#42325=CARTESIAN_POINT('Origin',(130.,35.,23.));
#42326=CARTESIAN_POINT('',(126.821241956411,36.1772435443955,24.1659079080442));
#42327=CARTESIAN_POINT('',(126.821241887301,36.1772433577858,23.8178898623416));
#42328=CARTESIAN_POINT('',(126.821241918358,36.1772434416438,23.));
#42329=CARTESIAN_POINT('',(126.610250686301,34.9978429702395,22.6387451035351));
#42330=CARTESIAN_POINT('Ctrl Pts',(126.821241887301,36.1772433577858,23.8178898623416));
#42331=CARTESIAN_POINT('Ctrl Pts',(126.830547905651,36.2023711965905,23.8162403472402));
#42332=CARTESIAN_POINT('Ctrl Pts',(126.840153832804,36.2273939784003,23.8145991736083));
#42333=CARTESIAN_POINT('Ctrl Pts',(126.869647398543,36.3015795205453,23.8097380037057));
#42334=CARTESIAN_POINT('Ctrl Pts',(126.890390921278,36.3503882810981,23.806545709812));
#42335=CARTESIAN_POINT('Ctrl Pts',(126.924828261293,36.4264115288566,23.8015809576627));
#42336=CARTESIAN_POINT('Ctrl Pts',(126.937757562149,36.453960939806,23.7997833655218));
#42337=CARTESIAN_POINT('Ctrl Pts',(126.962616510146,36.5051266937263,23.7964466480327));
#42338=CARTESIAN_POINT('Ctrl Pts',(126.974454965761,36.5287845279524,23.7949045717327));
#42339=CARTESIAN_POINT('Ctrl Pts',(127.001710040821,36.5816938744458,23.7914563267144));
#42340=CARTESIAN_POINT('Ctrl Pts',(127.017280253988,36.610863500984,23.7895556341927));
#42341=CARTESIAN_POINT('Ctrl Pts',(127.066324063279,36.6995934450194,23.7837711528408));
#42342=CARTESIAN_POINT('Ctrl Pts',(127.10117437948,36.7583751788372,23.7799354319769));
#42343=CARTESIAN_POINT('Ctrl Pts',(127.272238822473,37.0279821809498,23.762251831542));
#42344=CARTESIAN_POINT('Ctrl Pts',(127.429812642212,37.2243053300573,23.7491758856208));
#42345=CARTESIAN_POINT('Ctrl Pts',(127.709945733416,37.5033815381431,23.728081293334));
#42346=CARTESIAN_POINT('Ctrl Pts',(127.818673349209,37.5986675706755,23.7202757994235));
#42347=CARTESIAN_POINT('Ctrl Pts',(127.955551895266,37.7039669215246,23.710441410592));
#42348=CARTESIAN_POINT('Ctrl Pts',(127.978185716253,37.7209322036546,23.7088148520134));
#42349=CARTESIAN_POINT('Ctrl Pts',(128.014370949682,37.7473542324302,23.7062092541366));
#42350=CARTESIAN_POINT('Ctrl Pts',(128.027784243159,37.7569989095818,23.7052422944716));
#42351=CARTESIAN_POINT('Ctrl Pts',(128.053810544193,37.7754257094152,23.7033628262939));
#42352=CARTESIAN_POINT('Ctrl Pts',(128.066413627713,37.7842207119801,23.702451173637));
#42353=CARTESIAN_POINT('Ctrl Pts',(128.097847731293,37.8058404969463,23.7001743599675));
#42354=CARTESIAN_POINT('Ctrl Pts',(128.116748914716,37.8185615898077,23.6988027053274));
#42355=CARTESIAN_POINT('Ctrl Pts',(128.191180318661,37.8675733649739,23.6933955439765));
#42356=CARTESIAN_POINT('Ctrl Pts',(128.247639746503,37.9024193366012,23.6892819250367));
#42357=CARTESIAN_POINT('Ctrl Pts',(128.408440789845,37.9952610783694,23.6776074624184));
#42358=CARTESIAN_POINT('Ctrl Pts',(128.514875751083,38.0494348778509,23.6699297970736));
#42359=CARTESIAN_POINT('Ctrl Pts',(128.851015294822,38.1987460251132,23.6462237163329));
#42360=CARTESIAN_POINT('Ctrl Pts',(129.088528564994,38.2743546591568,23.6302831421948));
#42361=CARTESIAN_POINT('Ctrl Pts',(129.382064297564,38.333338764372,23.6120820566831));
#42362=CARTESIAN_POINT('Ctrl Pts',(129.432149098051,38.3422354230369,23.6090239068376));
#42363=CARTESIAN_POINT('Ctrl Pts',(129.512032589675,38.354577599804,23.604219317334));
#42364=CARTESIAN_POINT('Ctrl Pts',(129.541707973085,38.3587604218032,23.6024503552779));
#42365=CARTESIAN_POINT('Ctrl Pts',(129.597735815717,38.3659012943057,23.5991393061216));
#42366=CARTESIAN_POINT('Ctrl Pts',(129.624074926968,38.3689447005368,23.5975946906248));
#42367=CARTESIAN_POINT('Ctrl Pts',(129.68403140195,38.3751605742381,23.5941045326031));
#42368=CARTESIAN_POINT('Ctrl Pts',(129.717666169719,38.3781404325842,23.5921650593183));
#42369=CARTESIAN_POINT('Ctrl Pts',(129.82347051327,38.3859228070902,23.5861176012113));
#42370=CARTESIAN_POINT('Ctrl Pts',(129.895754711126,38.3889186846575,23.5820645640413));
#42371=CARTESIAN_POINT('Ctrl Pts',(130.070020260236,38.3905595878107,23.5724362132522));
#42372=CARTESIAN_POINT('Ctrl Pts',(130.17195295865,38.3869206098284,23.5669230563533));
#42373=CARTESIAN_POINT('Ctrl Pts',(130.321069444576,38.3748467142612,23.5589198326161));
#42374=CARTESIAN_POINT('Ctrl Pts',(130.368481742101,38.3699995893997,23.5563840398085));
#42375=CARTESIAN_POINT('Ctrl Pts',(130.622548086591,38.3385994770582,23.542791210834));
#42376=CARTESIAN_POINT('Ctrl Pts',(130.8265038965,38.2940382507515,23.5318872718909));
#42377=CARTESIAN_POINT('Ctrl Pts',(131.069845818878,38.2168373985469,23.5176400665579));
#42378=CARTESIAN_POINT('Ctrl Pts',(131.114331281821,38.2016992789401,23.5149816532573));
#42379=CARTESIAN_POINT('Ctrl Pts',(131.176066206146,38.1792488579611,23.5111981605724));
#42380=CARTESIAN_POINT('Ctrl Pts',(131.193593337823,38.172710187193,23.5101132193481));
#42381=CARTESIAN_POINT('Ctrl Pts',(131.225191884207,38.1606231471985,23.508136190163));
#42382=CARTESIAN_POINT('Ctrl Pts',(131.239282227988,38.1551249397208,23.5072469433335));
#42383=CARTESIAN_POINT('Ctrl Pts',(131.268812697216,38.1433734881624,23.5053663292103));
#42384=CARTESIAN_POINT('Ctrl Pts',(131.284244114081,38.1371005046665,23.5043739073764));
#42385=CARTESIAN_POINT('Ctrl Pts',(131.326344230695,38.1196238204367,23.5016410214345));
#42386=CARTESIAN_POINT('Ctrl Pts',(131.352916149311,38.108192331765,23.4998881126267));
#42387=CARTESIAN_POINT('Ctrl Pts',(131.412672445447,38.0815731933556,23.495887621898));
#42388=CARTESIAN_POINT('Ctrl Pts',(131.445764155099,38.0661869790508,23.4936308696321));
#42389=CARTESIAN_POINT('Ctrl Pts',(131.553727501971,38.0138524095655,23.4861457701705));
#42390=CARTESIAN_POINT('Ctrl Pts',(131.627480454689,37.9746733292204,23.4808367979217));
#42391=CARTESIAN_POINT('Ctrl Pts',(131.928332473327,37.8003150156067,23.4585491224898));
#42392=CARTESIAN_POINT('Ctrl Pts',(132.140716566043,37.6415141943275,23.4413574051443));
#42393=CARTESIAN_POINT('Ctrl Pts',(132.38691259932,37.4080440285661,23.420413188827));
#42394=CARTESIAN_POINT('Ctrl Pts',(132.439598327208,37.3546526529745,23.415852934522));
#42395=CARTESIAN_POINT('Ctrl Pts',(132.513434973223,37.2746857799418,23.4093431375153));
#42396=CARTESIAN_POINT('Ctrl Pts',(132.53602388301,37.2494741055551,23.4073342022896));
#42397=CARTESIAN_POINT('Ctrl Pts',(132.575672454448,37.2038654966798,23.4037753068264));
#42398=CARTESIAN_POINT('Ctrl Pts',(132.592876651251,37.1835985096205,23.4022195207993));
#42399=CARTESIAN_POINT('Ctrl Pts',(132.62872346103,37.140348940527,23.3989521733954));
#42400=CARTESIAN_POINT('Ctrl Pts',(132.647307193935,37.1173203165586,23.3972430353738));
#42401=CARTESIAN_POINT('Ctrl Pts',(132.696706429265,37.0544383733391,23.392655528209));
#42402=CARTESIAN_POINT('Ctrl Pts',(132.726939589997,37.014135903102,23.3897997155891));
#42403=CARTESIAN_POINT('Ctrl Pts',(132.847162076772,36.8462008286175,23.3782171813563));
#42404=CARTESIAN_POINT('Ctrl Pts',(132.929181780527,36.7130937255067,23.3697791330597));
#42405=CARTESIAN_POINT('Ctrl Pts',(133.10783028303,36.372569395749,23.3492808596052));
#42406=CARTESIAN_POINT('Ctrl Pts',(133.193206456312,36.1601597270009,23.3374180636593));
#42407=CARTESIAN_POINT('Ctrl Pts',(133.271582899674,35.8888608463141,23.321743558704));
#42408=CARTESIAN_POINT('Ctrl Pts',(133.285343064003,35.8365695243158,23.3186975522804));
#42409=CARTESIAN_POINT('Ctrl Pts',(133.302866097039,35.7628576105985,23.3143411163534));
#42410=CARTESIAN_POINT('Ctrl Pts',(133.307683006941,35.7416935092293,23.3130831286661));
#42411=CARTESIAN_POINT('Ctrl Pts',(133.315523124015,35.7056500351109,23.3109263262032));
#42412=CARTESIAN_POINT('Ctrl Pts',(133.318650288667,35.6907936116608,23.3100331696896));
#42413=CARTESIAN_POINT('Ctrl Pts',(133.325056645912,35.6593106548338,23.308130896282));
#42414=CARTESIAN_POINT('Ctrl Pts',(133.328311078969,35.6426799924452,23.3071205554749));
#42415=CARTESIAN_POINT('Ctrl Pts',(133.337033955339,35.5962606050892,23.304286584668));
#42416=CARTESIAN_POINT('Ctrl Pts',(133.342227933832,35.5664226592599,23.3024490157616));
#42417=CARTESIAN_POINT('Ctrl Pts',(133.374400550104,35.3657174218867,23.2899998445854));
#42418=CARTESIAN_POINT('Ctrl Pts',(133.388663002471,35.1930834819671,23.2788744273161));
#42419=CARTESIAN_POINT('Ctrl Pts',(133.391152529776,34.7739231627998,23.2518569552887));
#42420=CARTESIAN_POINT('Ctrl Pts',(133.365785569443,34.5282486079279,23.2360675279682));
#42421=CARTESIAN_POINT('Ctrl Pts',(133.303275536915,34.2375130499535,23.21798619962));
#42422=CARTESIAN_POINT('Ctrl Pts',(133.291407094403,34.1878082825827,23.2149136047277));
#42423=CARTESIAN_POINT('Ctrl Pts',(133.270789250371,34.1093576719016,23.2100917453265));
#42424=CARTESIAN_POINT('Ctrl Pts',(133.26277406109,34.0804285835136,23.2083196827582));
#42425=CARTESIAN_POINT('Ctrl Pts',(133.24695981027,34.0261624493708,23.2050059264274));
#42426=CARTESIAN_POINT('Ctrl Pts',(133.239245800273,34.0008031781776,23.203461657858));
#42427=CARTESIAN_POINT('Ctrl Pts',(133.221055268759,33.9434288755988,23.1999764020385));
#42428=CARTESIAN_POINT('Ctrl Pts',(133.210397314652,33.9114740316752,23.1980414153903));
#42429=CARTESIAN_POINT('Ctrl Pts',(133.175517156584,33.8118675768563,23.1920248474812));
#42430=CARTESIAN_POINT('Ctrl Pts',(133.149618535503,33.7448219467027,23.1879973806875));
#42431=CARTESIAN_POINT('Ctrl Pts',(133.082242563894,33.5856508050343,23.1784453312118));
#42432=CARTESIAN_POINT('Ctrl Pts',(133.038740474553,33.4944565624926,23.1729814907204));
#42433=CARTESIAN_POINT('Ctrl Pts',(132.93131867709,33.2929574500799,23.1607615617631));
#42434=CARTESIAN_POINT('Ctrl Pts',(132.865122594727,33.1840439979205,23.1540517333381));
#42435=CARTESIAN_POINT('Ctrl Pts',(132.708732522234,32.9566539985611,23.1393728012354));
#42436=CARTESIAN_POINT('Ctrl Pts',(132.616554587467,32.8398776552014,23.1313965047221));
#42437=CARTESIAN_POINT('Ctrl Pts',(132.493011915511,32.7029188610765,23.1209841801166));
#42438=CARTESIAN_POINT('Ctrl Pts',(132.468580821941,32.6766836889493,23.11893692044));
#42439=CARTESIAN_POINT('Ctrl Pts',(132.431210834953,32.637809119185,23.1158140339933));
#42440=CARTESIAN_POINT('Ctrl Pts',(132.418578608063,32.6248769787422,23.1147598324543));
#42441=CARTESIAN_POINT('Ctrl Pts',(132.395316354249,32.6014404428891,23.1128197272405));
#42442=CARTESIAN_POINT('Ctrl Pts',(132.384719448506,32.5909044204095,23.1119362689814));
#42443=CARTESIAN_POINT('Ctrl Pts',(132.359954649903,32.5666054068545,23.1098725721881));
#42444=CARTESIAN_POINT('Ctrl Pts',(132.345735802835,32.5528958548086,23.1086885123181));
#42445=CARTESIAN_POINT('Ctrl Pts',(132.298701197794,32.5083325507467,23.1047768897899));
#42446=CARTESIAN_POINT('Ctrl Pts',(132.265391460201,32.478009716113,23.1020148030263));
#42447=CARTESIAN_POINT('Ctrl Pts',(132.181546914975,32.4046849973098,23.0951031576372));
#42448=CARTESIAN_POINT('Ctrl Pts',(132.130335470072,32.3624866248943,23.0909169836351));
#42449=CARTESIAN_POINT('Ctrl Pts',(131.862779027798,32.1548973696357,23.0693496036981));
#42450=CARTESIAN_POINT('Ctrl Pts',(131.628269995534,32.0144812308314,23.0515299962715));
#42451=CARTESIAN_POINT('Ctrl Pts',(131.299464897008,31.8679926929895,23.0291444801164));
#42452=CARTESIAN_POINT('Ctrl Pts',(131.218090485511,31.8354563651473,23.02378555024));
#42453=CARTESIAN_POINT('Ctrl Pts',(131.100659059866,31.7937053700561,23.0163067535523));
#42454=CARTESIAN_POINT('Ctrl Pts',(131.065575255356,31.7818755216247,23.0141037029132));
#42455=CARTESIAN_POINT('Ctrl Pts',(131.004625045332,31.7624299100802,23.0103288184475));
#42456=CARTESIAN_POINT('Ctrl Pts',(130.978849142318,31.7545437935648,23.0087483980022));
#42457=CARTESIAN_POINT('Ctrl Pts',(130.925648073195,31.7389584589469,23.0055181939572));
#42458=CARTESIAN_POINT('Ctrl Pts',(130.898214379346,31.7312957783666,23.0038696869105));
#42459=CARTESIAN_POINT('Ctrl Pts',(130.827195331541,31.712420638472,22.9996443693254));
#42460=CARTESIAN_POINT('Ctrl Pts',(130.783476719666,31.7017285327599,22.9970841078204));
#42461=CARTESIAN_POINT('Ctrl Pts',(130.544738045398,31.6483561138424,22.9833029529771));
#42462=CARTESIAN_POINT('Ctrl Pts',(130.346445874397,31.6220948758561,22.9726074116107));
#42463=CARTESIAN_POINT('Ctrl Pts',(129.931890220432,31.6041031151512,22.9505824317376));
#42464=CARTESIAN_POINT('Ctrl Pts',(129.716425650023,31.6152812506665,22.9393132303251));
#42465=CARTESIAN_POINT('Ctrl Pts',(129.463150866573,31.6527829477532,22.9249304985064));
#42466=CARTESIAN_POINT('Ctrl Pts',(129.422912539357,31.6594852576506,22.9226099237233));
#42467=CARTESIAN_POINT('Ctrl Pts',(129.364115777614,31.6703727456152,22.9191541130007));
#42468=CARTESIAN_POINT('Ctrl Pts',(129.345454626718,31.6739908726697,22.9180476369328));
#42469=CARTESIAN_POINT('Ctrl Pts',(129.312212399634,31.6807266479543,22.9160577735641));
#42470=CARTESIAN_POINT('Ctrl Pts',(129.297619999223,31.6837838300989,22.9151776850011));
#42471=CARTESIAN_POINT('Ctrl Pts',(129.264765924357,31.6908935041108,22.9131811625249));
#42472=CARTESIAN_POINT('Ctrl Pts',(129.246517414978,31.6950009219945,22.9120618461793));
#42473=CARTESIAN_POINT('Ctrl Pts',(129.190196259282,31.7081685089321,22.9085771179016));
#42474=CARTESIAN_POINT('Ctrl Pts',(129.152247076564,31.7177368533767,22.9061863826025));
#42475=CARTESIAN_POINT('Ctrl Pts',(129.061776074907,31.7422214033854,22.9003976787353));
#42476=CARTESIAN_POINT('Ctrl Pts',(129.009432914097,31.7577535863735,22.8969758089811));
#42477=CARTESIAN_POINT('Ctrl Pts',(128.796644150592,31.8265296703261,22.8828236366041));
#42478=CARTESIAN_POINT('Ctrl Pts',(128.63991552364,31.8904746514034,22.8718441817082));
#42479=CARTESIAN_POINT('Ctrl Pts',(128.329335624545,32.0451819352462,22.849567343045));
#42480=CARTESIAN_POINT('Ctrl Pts',(128.176536004306,32.1369486958906,22.8383220110877));
#42481=CARTESIAN_POINT('Ctrl Pts',(127.98867194196,32.2709435508528,22.8242737343379));
#42482=CARTESIAN_POINT('Ctrl Pts',(127.946430570228,32.3025859189739,22.8210972684933));
#42483=CARTESIAN_POINT('Ctrl Pts',(127.881063779893,32.3539771243669,22.816151388328));
#42484=CARTESIAN_POINT('Ctrl Pts',(127.857437065946,32.3730717697567,22.8143571542829));
#42485=CARTESIAN_POINT('Ctrl Pts',(127.813910549841,32.409226994761,22.8110383123983));
#42486=CARTESIAN_POINT('Ctrl Pts',(127.793945945349,32.4262056388246,22.8095106198039));
#42487=CARTESIAN_POINT('Ctrl Pts',(127.74928218921,32.4650908973408,22.8060794495788));
#42488=CARTESIAN_POINT('Ctrl Pts',(127.724701934007,32.4871303966919,22.8041815762958));
#42489=CARTESIAN_POINT('Ctrl Pts',(127.650462825326,32.5556783007006,22.7984158708846));
#42490=CARTESIAN_POINT('Ctrl Pts',(127.601877412958,32.6033268015824,22.7945956338806));
#42491=CARTESIAN_POINT('Ctrl Pts',(127.381317544598,32.8330611337664,22.7769546290891));
#42492=CARTESIAN_POINT('Ctrl Pts',(127.228435384902,33.0323729753638,22.7639032732564));
#42493=CARTESIAN_POINT('Ctrl Pts',(127.02369088658,33.3711564030175,22.7427901419689));
#42494=CARTESIAN_POINT('Ctrl Pts',(126.956575650725,33.5002977236927,22.7349353508669));
#42495=CARTESIAN_POINT('Ctrl Pts',(126.886557478309,33.6592236657159,22.7250457464277));
#42496=CARTESIAN_POINT('Ctrl Pts',(126.875475691326,33.68525544379,22.7234188436114));
#42497=CARTESIAN_POINT('Ctrl Pts',(126.858440665005,33.7267038866486,22.7208128210263));
#42498=CARTESIAN_POINT('Ctrl Pts',(126.852271858339,33.7420311733536,22.7198457875952));
#42499=CARTESIAN_POINT('Ctrl Pts',(126.84058188203,33.7717010133015,22.7179662888178));
#42500=CARTESIAN_POINT('Ctrl Pts',(126.835045811053,33.7860369888344,22.7170546808426));
#42501=CARTESIAN_POINT('Ctrl Pts',(126.821546146027,33.8217151985876,22.7147781430227));
#42502=CARTESIAN_POINT('Ctrl Pts',(126.813699917688,33.8431008260554,22.7134067229216));
#42503=CARTESIAN_POINT('Ctrl Pts',(126.783860381062,33.9270380335679,22.7080017489805));
#42504=CARTESIAN_POINT('Ctrl Pts',(126.763489976588,33.9901469809117,22.7038901598557));
#42505=CARTESIAN_POINT('Ctrl Pts',(126.711696343838,34.1683233903572,22.6922238737635));
#42506=CARTESIAN_POINT('Ctrl Pts',(126.684476017317,34.284510585506,22.6845525239304));
#42507=CARTESIAN_POINT('Ctrl Pts',(126.628177866672,34.5985676272096,22.6639883048161));
#42508=CARTESIAN_POINT('Ctrl Pts',(126.610377855726,34.7979975720025,22.6511321729077));
#42509=CARTESIAN_POINT('Ctrl Pts',(126.610250686301,34.9978429702395,22.6387451035351));
#42510=CARTESIAN_POINT('Ctrl Pts',(126.610250683863,34.9978468054472,22.6387448658165));
#42511=CARTESIAN_POINT('Ctrl Pts',(126.610218691457,35.0482120802422,22.6356230633535));
#42512=CARTESIAN_POINT('Ctrl Pts',(126.611309197226,35.0985740946989,22.6325308277824));
#42513=CARTESIAN_POINT('Ctrl Pts',(126.615250243622,35.1882091841631,22.6270804172804));
#42514=CARTESIAN_POINT('Ctrl Pts',(126.617663277397,35.2274908769275,22.6247100370017));
#42515=CARTESIAN_POINT('Ctrl Pts',(126.622844397037,35.2931329588712,22.6207786219727));
#42516=CARTESIAN_POINT('Ctrl Pts',(126.62523851526,35.3195181983972,22.6192063880327));
#42517=CARTESIAN_POINT('Ctrl Pts',(126.630507067345,35.3708834463182,22.6161606738392));
#42518=CARTESIAN_POINT('Ctrl Pts',(126.633350590916,35.3958648266516,22.61468634392));
#42519=CARTESIAN_POINT('Ctrl Pts',(126.639972341806,35.4487920358022,22.6115766609327));
#42520=CARTESIAN_POINT('Ctrl Pts',(126.643821894405,35.4767271217682,22.6099436367488));
#42521=CARTESIAN_POINT('Ctrl Pts',(126.654511193208,35.5477328674716,22.6058120864575));
#42522=CARTESIAN_POINT('Ctrl Pts',(126.661834417446,35.5907261954345,22.6033286663749));
#42523=CARTESIAN_POINT('Ctrl Pts',(126.699004962162,35.7860935711715,22.5921112890358));
#42524=CARTESIAN_POINT('Ctrl Pts',(126.738470652228,35.9364532919305,22.5836777855363));
#42525=CARTESIAN_POINT('Ctrl Pts',(126.798698710943,36.1149763763543,22.5736078810968));
#42526=CARTESIAN_POINT('Ctrl Pts',(126.809744069168,36.1461972859097,22.571844118041));
#42527=CARTESIAN_POINT('Ctrl Pts',(126.821241895364,36.1772433795577,22.5700842967619));
#42528=CARTESIAN_POINT('Ctrl Pts',(126.821241918358,36.1772434416451,22.910437766625));
#42529=CARTESIAN_POINT('Ctrl Pts',(126.820991045024,36.1765660408554,22.9104819110725));
#42530=CARTESIAN_POINT('Ctrl Pts',(126.820740388213,36.1758885598419,22.910526065518));
#42531=CARTESIAN_POINT('Ctrl Pts',(126.762030801805,36.0170509380546,22.9208793282995));
#42532=CARTESIAN_POINT('Ctrl Pts',(126.715459346813,35.8547629778948,22.9317036025874));
#42533=CARTESIAN_POINT('Ctrl Pts',(126.652004445497,35.5494179881511,22.951800467092));
#42534=CARTESIAN_POINT('Ctrl Pts',(126.631773956849,35.4074205119328,22.9610436925096));
#42535=CARTESIAN_POINT('Ctrl Pts',(126.613747492658,35.1771592767367,22.9756515719051));
#42536=CARTESIAN_POINT('Ctrl Pts',(126.610297959855,35.0895173841033,22.9811257237269));
#42537=CARTESIAN_POINT('Ctrl Pts',(126.61021530294,34.936818897916,22.990495850361));
#42538=CARTESIAN_POINT('Ctrl Pts',(126.612050631336,34.8718123052779,22.9944323613035));
#42539=CARTESIAN_POINT('Ctrl Pts',(126.617604134971,34.7744847340311,23.0002494805929));
#42540=CARTESIAN_POINT('Ctrl Pts',(126.619919012245,34.7421016690371,23.0021722891916));
#42541=CARTESIAN_POINT('Ctrl Pts',(126.624960740196,34.6834357428838,23.0056338348393));
#42542=CARTESIAN_POINT('Ctrl Pts',(126.627530341423,34.6571423114836,23.0071772781116));
#42543=CARTESIAN_POINT('Ctrl Pts',(126.63377053995,34.6001771296514,23.0105049024812));
#42544=CARTESIAN_POINT('Ctrl Pts',(126.637553553801,34.5695199278666,23.0122854721365));
#42545=CARTESIAN_POINT('Ctrl Pts',(126.649479639371,34.4826574774102,23.017304110355));
#42546=CARTESIAN_POINT('Ctrl Pts',(126.65861696993,34.4265979281773,23.0205114836055));
#42547=CARTESIAN_POINT('Ctrl Pts',(126.682685970458,34.2991837440657,23.0277482056169));
#42548=CARTESIAN_POINT('Ctrl Pts',(126.698519210454,34.2280276787483,23.0317509489949));
#42549=CARTESIAN_POINT('Ctrl Pts',(126.765573149121,33.966727513005,23.0463955133786));
#42550=CARTESIAN_POINT('Ctrl Pts',(126.831032523688,33.7806496754215,23.0566936698902));
#42551=CARTESIAN_POINT('Ctrl Pts',(126.971708529375,33.4700968552031,23.074882759498));
#42552=CARTESIAN_POINT('Ctrl Pts',(127.039440357402,33.3428244037929,23.082667918556));
#42553=CARTESIAN_POINT('Ctrl Pts',(127.129901144472,33.196188050055,23.0924795150934));
#42554=CARTESIAN_POINT('Ctrl Pts',(127.145050913647,33.1723045672683,23.0941059015776));
#42555=CARTESIAN_POINT('Ctrl Pts',(127.169520150061,33.1347756697802,23.0967112886611));
#42556=CARTESIAN_POINT('Ctrl Pts',(127.178643912913,33.1210035157388,23.0976782129999));
#42557=CARTESIAN_POINT('Ctrl Pts',(127.19644938804,33.0945485456536,23.0995576704975));
#42558=CARTESIAN_POINT('Ctrl Pts',(127.205117267785,33.0818572113629,23.1004693485746));
#42559=CARTESIAN_POINT('Ctrl Pts',(127.226849289932,33.0504976586988,23.1027463106372));
#42560=CARTESIAN_POINT('Ctrl Pts',(127.240015820666,33.0319015503762,23.1041180900225));
#42561=CARTESIAN_POINT('Ctrl Pts',(127.292254821801,32.9596755409366,23.1095263979743));
#42562=CARTESIAN_POINT('Ctrl Pts',(127.332708979584,32.9070677793248,23.1136410789785));
#42563=CARTESIAN_POINT('Ctrl Pts',(127.450209079257,32.7632103827999,23.1253198157197));
#42564=CARTESIAN_POINT('Ctrl Pts',(127.530570304436,32.6747954991554,23.1330007812015));
#42565=CARTESIAN_POINT('Ctrl Pts',(127.791955440177,32.4160809980237,23.1567044337723));
#42566=CARTESIAN_POINT('Ctrl Pts',(127.987184945043,32.2612575279601,23.1726390998777));
#42567=CARTESIAN_POINT('Ctrl Pts',(128.24068915341,32.1021010800925,23.1908355258845));
#42568=CARTESIAN_POINT('Ctrl Pts',(128.284376938729,32.0760248400111,23.193894256953));
#42569=CARTESIAN_POINT('Ctrl Pts',(128.354709592771,32.0361641971151,23.198699544249));
#42570=CARTESIAN_POINT('Ctrl Pts',(128.380977642128,32.0217337456721,23.2004686338976));
#42571=CARTESIAN_POINT('Ctrl Pts',(128.430838663937,31.9951970638158,23.2037797986568));
#42572=CARTESIAN_POINT('Ctrl Pts',(128.454388872636,31.983015696808,23.2053244040204));
#42573=CARTESIAN_POINT('Ctrl Pts',(128.508246680073,31.9559538642707,23.208814374949));
#42574=CARTESIAN_POINT('Ctrl Pts',(128.53863878219,31.9412472554738,23.2107536739851));
#42575=CARTESIAN_POINT('Ctrl Pts',(128.634795826577,31.8964776820407,23.216799912662));
#42576=CARTESIAN_POINT('Ctrl Pts',(128.701307848315,31.8680624329588,23.2208519378052));
#42577=CARTESIAN_POINT('Ctrl Pts',(128.863624101897,31.8047786907942,23.2304772598761));
#42578=CARTESIAN_POINT('Ctrl Pts',(128.960191680524,31.7720610390162,23.235988456712));
#42579=CARTESIAN_POINT('Ctrl Pts',(129.103717917692,31.730544464895,23.2439814001364));
#42580=CARTESIAN_POINT('Ctrl Pts',(129.149617640359,31.718306686686,23.2465089516658));
#42581=CARTESIAN_POINT('Ctrl Pts',(129.397777717585,31.6576985568789,23.2600731109844));
#42582=CARTESIAN_POINT('Ctrl Pts',(129.603888448419,31.6270590688178,23.27095660855));
#42583=CARTESIAN_POINT('Ctrl Pts',(129.858824964905,31.6128592080461,23.2852007357883));
#42584=CARTESIAN_POINT('Ctrl Pts',(129.906213163451,31.6112160430695,23.2878824759269));
#42585=CARTESIAN_POINT('Ctrl Pts',(129.972391352175,31.6103104361192,23.2916938983876));
#42586=CARTESIAN_POINT('Ctrl Pts',(129.991166314496,31.6102095184953,23.292782664308));
#42587=CARTESIAN_POINT('Ctrl Pts',(130.02508178269,31.6103089784608,23.2947644288915));
#42588=CARTESIAN_POINT('Ctrl Pts',(130.040222210535,31.6104548262273,23.2956545382912));
#42589=CARTESIAN_POINT('Ctrl Pts',(130.071981331099,31.6109735830995,23.2975338471957));
#42590=CARTESIAN_POINT('Ctrl Pts',(130.088598903804,31.61136730006,23.2985240637229));
#42591=CARTESIAN_POINT('Ctrl Pts',(130.133958814,31.6127758791287,23.3012445796611));
#42592=CARTESIAN_POINT('Ctrl Pts',(130.162691565614,31.614034326185,23.3029871457164));
#42593=CARTESIAN_POINT('Ctrl Pts',(130.376229576136,31.6261111143128,23.3160641770337));
#42594=CARTESIAN_POINT('Ctrl Pts',(130.559873031074,31.6516861656024,23.3279985546282));
#42595=CARTESIAN_POINT('Ctrl Pts',(130.96989532433,31.7434725746539,23.355083154748));
#42596=CARTESIAN_POINT('Ctrl Pts',(131.193367220304,31.8185579226155,23.3701269114653));
#42597=CARTESIAN_POINT('Ctrl Pts',(131.454634121712,31.9377863027415,23.387601101697));
#42598=CARTESIAN_POINT('Ctrl Pts',(131.501474843771,31.9604791663651,23.3907323072274));
#42599=CARTESIAN_POINT('Ctrl Pts',(131.574662293488,31.9980411443712,23.3956241861937));
#42600=CARTESIAN_POINT('Ctrl Pts',(131.601362983871,32.0121989704975,23.3974087898721));
#42601=CARTESIAN_POINT('Ctrl Pts',(131.648772484437,32.0381556152005,23.4005783762225));
#42602=CARTESIAN_POINT('Ctrl Pts',(131.669552665223,32.0498191909558,23.4019679515779));
#42603=CARTESIAN_POINT('Ctrl Pts',(131.718007520089,32.0776920565041,23.4052097407483));
#42604=CARTESIAN_POINT('Ctrl Pts',(131.745578826942,32.0940770458146,23.4070555858349));
#42605=CARTESIAN_POINT('Ctrl Pts',(131.826530492941,32.143752700186,23.4124822725332));
#42606=CARTESIAN_POINT('Ctrl Pts',(131.879222682775,32.1781415561559,23.4160236447469));
#42607=CARTESIAN_POINT('Ctrl Pts',(132.057432311223,32.3016546988483,23.428073826773));
#42608=CARTESIAN_POINT('Ctrl Pts',(132.177823293654,32.3978496884418,23.4363342755972));
#42609=CARTESIAN_POINT('Ctrl Pts',(132.432127201846,32.63109801115,23.4546769479585));
#42610=CARTESIAN_POINT('Ctrl Pts',(132.56179911577,32.771970541328,23.4646804442863));
#42611=CARTESIAN_POINT('Ctrl Pts',(132.720457988631,32.9766084235078,23.47891602236));
#42612=CARTESIAN_POINT('Ctrl Pts',(132.760394783603,33.0314409913902,23.482706807058));
#42613=CARTESIAN_POINT('Ctrl Pts',(132.811993998189,33.1069459781343,23.4879486872838));
#42614=CARTESIAN_POINT('Ctrl Pts',(132.825125672649,33.1265997111924,23.4893150808563));
#42615=CARTESIAN_POINT('Ctrl Pts',(132.845703569156,33.1581063717356,23.4915113048036));
#42616=CARTESIAN_POINT('Ctrl Pts',(132.853284004639,33.1698712299973,23.4923326570048));
#42617=CARTESIAN_POINT('Ctrl Pts',(132.869269014327,33.1950207291062,23.4940918737467));
#42618=CARTESIAN_POINT('Ctrl Pts',(132.877653218377,33.2084178011201,23.4950310599182));
#42619=CARTESIAN_POINT('Ctrl Pts',(132.899033692813,33.243118823249,23.4974680142256));
#42620=CARTESIAN_POINT('Ctrl Pts',(132.911888725901,33.2645081995834,23.4989742465192));
#42621=CARTESIAN_POINT('Ctrl Pts',(132.968914712133,33.36181066487,23.5058379633032));
#42622=CARTESIAN_POINT('Ctrl Pts',(133.010358336426,33.4392760928862,23.511333584811));
#42623=CARTESIAN_POINT('Ctrl Pts',(133.137864867407,33.7016256654425,23.5298467141323));
#42624=CARTESIAN_POINT('Ctrl Pts',(133.210261002052,33.8926611336612,23.5431419976502));
#42625=CARTESIAN_POINT('Ctrl Pts',(133.306029671718,34.2359172180919,23.5658384522539));
#42626=CARTESIAN_POINT('Ctrl Pts',(133.33705384553,34.3853974850939,23.5753580462178));
#42627=CARTESIAN_POINT('Ctrl Pts',(133.363899805667,34.5798776584258,23.5872178965381));
#42628=CARTESIAN_POINT('Ctrl Pts',(133.369049152793,34.6233930960738,23.5898391577689));
#42629=CARTESIAN_POINT('Ctrl Pts',(133.376127783568,34.6951004868767,23.5941072072472));
#42630=CARTESIAN_POINT('Ctrl Pts',(133.378550736231,34.7232374322677,23.5957689864142));
#42631=CARTESIAN_POINT('Ctrl Pts',(133.382608107839,34.7784126162215,23.5990033198744));
#42632=CARTESIAN_POINT('Ctrl Pts',(133.384270617865,34.8054465952889,23.6005766217203));
#42633=CARTESIAN_POINT('Ctrl Pts',(133.387476474141,34.8702445546798,23.6043217909962));
#42634=CARTESIAN_POINT('Ctrl Pts',(133.388712628199,34.9080205246988,23.6064841005087));
#42635=CARTESIAN_POINT('Ctrl Pts',(133.390905763929,35.0451912823862,23.6142670098139));
#42636=CARTESIAN_POINT('Ctrl Pts',(133.388123031745,35.1445990175517,23.6197744850507));
#42637=CARTESIAN_POINT('Ctrl Pts',(133.368841502354,35.4120495621755,23.6343835536587));
#42638=CARTESIAN_POINT('Ctrl Pts',(133.344157514212,35.5792162243197,23.6432824012548));
#42639=CARTESIAN_POINT('Ctrl Pts',(133.26969183767,35.9102871861453,23.6612890226236));
#42640=CARTESIAN_POINT('Ctrl Pts',(133.219749184025,36.0736437526889,23.6703765168606));
#42641=CARTESIAN_POINT('Ctrl Pts',(133.144827057556,36.2655937969484,23.6820129487764));
#42642=CARTESIAN_POINT('Ctrl Pts',(133.1314032994,36.2984521743423,23.6840405581058));
#42643=CARTESIAN_POINT('Ctrl Pts',(133.110394990774,36.3476543971864,23.6871394033429));
#42644=CARTESIAN_POINT('Ctrl Pts',(133.103191638882,36.3641594458443,23.6881897026809));
#42645=CARTESIAN_POINT('Ctrl Pts',(133.089767837894,36.3942608468924,23.6901263775985));
#42646=CARTESIAN_POINT('Ctrl Pts',(133.0835884648,36.4078745519811,23.6910103733047));
#42647=CARTESIAN_POINT('Ctrl Pts',(133.068997150984,36.4394635833291,23.6930803427733));
#42648=CARTESIAN_POINT('Ctrl Pts',(133.060517211234,36.4574063531588,23.6942702211598));
#42649=CARTESIAN_POINT('Ctrl Pts',(133.032033595689,36.5163300782826,23.6982220130355));
#42650=CARTESIAN_POINT('Ctrl Pts',(133.011361259614,36.5569802718885,23.7010193888895));
#42651=CARTESIAN_POINT('Ctrl Pts',(132.958064203014,36.6567496917963,23.7080412184183));
#42652=CARTESIAN_POINT('Ctrl Pts',(132.924481529621,36.7153338540979,23.7123036745727));
#42653=CARTESIAN_POINT('Ctrl Pts',(132.738283491129,37.0187726811197,23.7349893323835));
#42654=CARTESIAN_POINT('Ctrl Pts',(132.556585850692,37.2444488319313,23.7538714155686));
#42655=CARTESIAN_POINT('Ctrl Pts',(132.293511631862,37.4972028835449,23.7764070360628));
#42656=CARTESIAN_POINT('Ctrl Pts',(132.236763711803,37.5481576332396,23.7810461544241));
#42657=CARTESIAN_POINT('Ctrl Pts',(132.152250731834,37.6190420965966,23.7876451362553));
#42658=CARTESIAN_POINT('Ctrl Pts',(132.125830511446,37.6405320448692,23.7896667089465));
#42659=CARTESIAN_POINT('Ctrl Pts',(132.078197381649,37.678097965243,23.7932398168382));
#42660=CARTESIAN_POINT('Ctrl Pts',(132.057110854539,37.6943288701668,23.7947973476644));
#42661=CARTESIAN_POINT('Ctrl Pts',(132.012265725829,37.7280140481446,23.7980601752366));
#42662=CARTESIAN_POINT('Ctrl Pts',(131.98846606496,37.7454101307536,23.799763157209));
#42663=CARTESIAN_POINT('Ctrl Pts',(131.923833722239,37.7913709500654,23.8043139224174));
#42664=CARTESIAN_POINT('Ctrl Pts',(131.88259235047,37.8193499907959,23.8071397917898));
#42665=CARTESIAN_POINT('Ctrl Pts',(131.789320868149,37.8796677994977,23.8133717403897));
#42666=CARTESIAN_POINT('Ctrl Pts',(131.73700060635,37.9115262766809,23.8167612185983));
#42667=CARTESIAN_POINT('Ctrl Pts',(131.561399150871,38.0120328562038,23.8278361040226));
#42668=CARTESIAN_POINT('Ctrl Pts',(131.434694004551,38.0744048953099,23.8353450126785));
#42669=CARTESIAN_POINT('Ctrl Pts',(131.10572997947,38.2115616680426,23.8542478941376));
#42670=CARTESIAN_POINT('Ctrl Pts',(130.899573310751,38.2752883140285,23.8655532104072));
#42671=CARTESIAN_POINT('Ctrl Pts',(130.65672521931,38.3256863741634,23.8795955671347));
#42672=CARTESIAN_POINT('Ctrl Pts',(130.624561217351,38.331876497226,23.8814701677594));
#42673=CARTESIAN_POINT('Ctrl Pts',(130.574928707429,38.3406846312721,23.8843924439984));
#42674=CARTESIAN_POINT('Ctrl Pts',(130.557520153186,38.3436339621925,23.8854229991198));
#42675=CARTESIAN_POINT('Ctrl Pts',(130.526769470808,38.3485968761796,23.8872544429829));
#42676=CARTESIAN_POINT('Ctrl Pts',(130.513437148415,38.3506670065454,23.8880522249649));
#42677=CARTESIAN_POINT('Ctrl Pts',(130.480884563198,38.3555226519605,23.8900090586031));
#42678=CARTESIAN_POINT('Ctrl Pts',(130.461652481773,38.3582226217893,23.8911726467208));
#42679=CARTESIAN_POINT('Ctrl Pts',(130.399655828344,38.3663836529264,23.8949453846792));
#42680=CARTESIAN_POINT('Ctrl Pts',(130.356811493864,38.3711939828922,23.8975859109875));
#42681=CARTESIAN_POINT('Ctrl Pts',(130.251766331356,38.3809630900562,23.9041227367526));
#42682=CARTESIAN_POINT('Ctrl Pts',(130.189498662944,38.3850239569588,23.9080511176068));
#42683=CARTESIAN_POINT('Ctrl Pts',(129.898612138814,38.3959434993859,23.9265542163559));
#42684=CARTESIAN_POINT('Ctrl Pts',(129.669781057678,38.3813720790272,23.9414957920195));
#42685=CARTESIAN_POINT('Ctrl Pts',(129.318781102657,38.3230253186719,23.9639851571508));
#42686=CARTESIAN_POINT('Ctrl Pts',(129.194674386032,38.2951499315762,23.9718618640757));
#42687=CARTESIAN_POINT('Ctrl Pts',(129.032287390868,38.2489502747913,23.9820412920123));
#42688=CARTESIAN_POINT('Ctrl Pts',(128.992373167529,38.2367937811066,23.9845334932294));
#42689=CARTESIAN_POINT('Ctrl Pts',(128.926234481771,38.2153081587685,23.9886482177712));
#42690=CARTESIAN_POINT('Ctrl Pts',(128.899883057568,38.2063876443464,23.9902836527663));
#42691=CARTESIAN_POINT('Ctrl Pts',(128.84782491827,38.1880475212083,23.9935075624008));
#42692=CARTESIAN_POINT('Ctrl Pts',(128.822116604895,38.1786388892469,23.9950962482949));
#42693=CARTESIAN_POINT('Ctrl Pts',(128.759680990087,38.1549274230296,23.9989477398151));
#42694=CARTESIAN_POINT('Ctrl Pts',(128.723083265356,38.1402933185247,24.0011995144406));
#42695=CARTESIAN_POINT('Ctrl Pts',(128.582512723536,38.0812203131108,24.009835081339));
#42696=CARTESIAN_POINT('Ctrl Pts',(128.480528833962,38.0322268266604,24.0160683901573));
#42697=CARTESIAN_POINT('Ctrl Pts',(128.189384764534,37.8739745551613,24.0340189001853));
#42698=CARTESIAN_POINT('Ctrl Pts',(128.008117640186,37.7514467796381,24.0453716552373));
#42699=CARTESIAN_POINT('Ctrl Pts',(127.749340308102,37.5374676319088,24.0634136231478));
#42700=CARTESIAN_POINT('Ctrl Pts',(127.662751094931,37.4579409069669,24.0698319668873));
#42701=CARTESIAN_POINT('Ctrl Pts',(127.561244346807,37.3544913931816,24.078094280142));
#42702=CARTESIAN_POINT('Ctrl Pts',(127.542254843493,37.3346621811819,24.0796744303567));
#42703=CARTESIAN_POINT('Ctrl Pts',(127.512349870862,37.3026656238794,24.0822227743127));
#42704=CARTESIAN_POINT('Ctrl Pts',(127.501277537835,37.2906457982934,24.0831797785276));
#42705=CARTESIAN_POINT('Ctrl Pts',(127.479892913285,37.2670916849648,24.0850556278928));
#42706=CARTESIAN_POINT('Ctrl Pts',(127.469571957248,37.2555660761954,24.0859738261498));
#42707=CARTESIAN_POINT('Ctrl Pts',(127.443889210031,37.2264875442427,24.088290290962));
#42708=CARTESIAN_POINT('Ctrl Pts',(127.428629168646,37.2088461098056,24.08969553583));
#42709=CARTESIAN_POINT('Ctrl Pts',(127.367621990318,37.1368295411859,24.0954266649304));
#42710=CARTESIAN_POINT('Ctrl Pts',(127.323410459365,37.0811827145054,24.0998424907736));
#42711=CARTESIAN_POINT('Ctrl Pts',(127.200823775203,36.9165168970774,24.1127799937611));
#42712=CARTESIAN_POINT('Ctrl Pts',(127.127134082419,36.8041793887822,24.1214455738092));
#42713=CARTESIAN_POINT('Ctrl Pts',(126.966564982019,36.5245064497519,24.1422305717618));
#42714=CARTESIAN_POINT('Ctrl Pts',(126.886606077617,36.3537378025582,24.1542830667824));
#42715=CARTESIAN_POINT('Ctrl Pts',(126.821241956411,36.1772435443955,24.1659079080442));
#42716=CARTESIAN_POINT('Origin',(130.,35.,23.));
#42717=CARTESIAN_POINT('',(126.821241938915,36.1772434971514,25.4139333020124));
#42718=CARTESIAN_POINT('',(126.821241918346,36.177243441613,25.0733700900595));
#42719=CARTESIAN_POINT('',(126.821241918358,36.1772434416438,23.));
#42720=CARTESIAN_POINT('Ctrl Pts',(126.821241918346,36.177243441613,25.0733700900595));
#42721=CARTESIAN_POINT('Ctrl Pts',(126.82271653249,36.1812251513086,25.0731092436031));
#42722=CARTESIAN_POINT('Ctrl Pts',(126.82419862865,36.1852040924822,25.0728480699998));
#42723=CARTESIAN_POINT('Ctrl Pts',(126.878017473958,36.3288642286552,25.0634002377664));
#42724=CARTESIAN_POINT('Ctrl Pts',(126.939505830955,36.4649312183301,25.0538394440563));
#42725=CARTESIAN_POINT('Ctrl Pts',(127.070403672287,36.710104269745,25.0359364811992));
#42726=CARTESIAN_POINT('Ctrl Pts',(127.137487035384,36.820168375137,25.0276193832681));
#42727=CARTESIAN_POINT('Ctrl Pts',(127.295509549523,37.0490064349424,25.0099311780473));
#42728=CARTESIAN_POINT('Ctrl Pts',(127.388378504628,37.1661344711245,25.0006253155994));
#42729=CARTESIAN_POINT('Ctrl Pts',(127.517304576101,37.3083424273972,24.9890422439931));
#42730=CARTESIAN_POINT('Ctrl Pts',(127.546523102162,37.3393744227889,24.9864947018794));
#42731=CARTESIAN_POINT('Ctrl Pts',(127.59589385837,37.3898666469458,24.9823142908905));
#42732=CARTESIAN_POINT('Ctrl Pts',(127.615715302454,37.4096421895552,24.9806676307273));
#42733=CARTESIAN_POINT('Ctrl Pts',(127.655076205008,37.4479506745823,24.9774581674764));
#42734=CARTESIAN_POINT('Ctrl Pts',(127.674595955637,37.4665008009705,24.9758946841886));
#42735=CARTESIAN_POINT('Ctrl Pts',(127.718082686967,37.5068521989489,24.9724715083904));
#42736=CARTESIAN_POINT('Ctrl Pts',(127.742145505016,37.5285465692299,24.9706163286446));
#42737=CARTESIAN_POINT('Ctrl Pts',(127.8271058803,37.602964438754,24.9641957456165));
#42738=CARTESIAN_POINT('Ctrl Pts',(127.889570604981,37.6538616862496,24.9597028966585));
#42739=CARTESIAN_POINT('Ctrl Pts',(128.177804786523,37.8721001522049,24.9398385771984));
#42740=CARTESIAN_POINT('Ctrl Pts',(128.422018362977,38.0131908377763,24.9253936572409));
#42741=CARTESIAN_POINT('Ctrl Pts',(128.74253862518,38.1486001980156,24.9065604790743));
#42742=CARTESIAN_POINT('Ctrl Pts',(128.805001103423,38.1728329696394,24.9028901796026));
#42743=CARTESIAN_POINT('Ctrl Pts',(128.910884003884,38.2103407931495,24.8966061926021));
#42744=CARTESIAN_POINT('Ctrl Pts',(128.95392840177,38.2246233056361,24.8940346723486));
#42745=CARTESIAN_POINT('Ctrl Pts',(129.016161331327,38.2438956080628,24.8902756327486));
#42746=CARTESIAN_POINT('Ctrl Pts',(129.035129000958,38.2495878440407,24.88912449901));
#42747=CARTESIAN_POINT('Ctrl Pts',(129.068498970997,38.2592843278496,24.8870880405747));
#42748=CARTESIAN_POINT('Ctrl Pts',(129.082879577217,38.2633600192156,24.8862067223702));
#42749=CARTESIAN_POINT('Ctrl Pts',(129.114675297002,38.2721446576098,24.8842495518035));
#42750=CARTESIAN_POINT('Ctrl Pts',(129.132101114727,38.2768097263735,24.8831714325921));
#42751=CARTESIAN_POINT('Ctrl Pts',(129.18302160838,38.2900069988382,24.8800067532311));
#42752=CARTESIAN_POINT('Ctrl Pts',(129.216609628911,38.2981660165721,24.8779013511822));
#42753=CARTESIAN_POINT('Ctrl Pts',(129.434296841521,38.3475326872473,24.8641660483345));
#42754=CARTESIAN_POINT('Ctrl Pts',(129.621427295724,38.3738209592561,24.8519643974789));
#42755=CARTESIAN_POINT('Ctrl Pts',(129.966342192234,38.3932091969743,24.8297023463993));
#42756=CARTESIAN_POINT('Ctrl Pts',(130.123361105058,38.3911341618485,24.8196512098367));
#42757=CARTESIAN_POINT('Ctrl Pts',(130.37471179684,38.3703247082056,24.8039201482275));
#42758=CARTESIAN_POINT('Ctrl Pts',(130.469373115477,38.3584503993726,24.7980754131398));
#42759=CARTESIAN_POINT('Ctrl Pts',(130.600161296829,38.3364052710126,24.7901144095479));
#42760=CARTESIAN_POINT('Ctrl Pts',(130.636803982012,38.329605767872,24.7878963804327));
#42761=CARTESIAN_POINT('Ctrl Pts',(130.699784311125,38.316841216531,24.7841041267788));
#42762=CARTESIAN_POINT('Ctrl Pts',(130.726175947379,38.3111632840996,24.7825211016516));
#42763=CARTESIAN_POINT('Ctrl Pts',(130.780190833074,38.2988655624278,24.7792927435839));
#42764=CARTESIAN_POINT('Ctrl Pts',(130.807804390822,38.2922126104616,24.7776485956208));
#42765=CARTESIAN_POINT('Ctrl Pts',(130.878566618735,38.274219887414,24.7734495688047));
#42766=CARTESIAN_POINT('Ctrl Pts',(130.921581629802,38.2623737883231,24.7709108300149));
#42767=CARTESIAN_POINT('Ctrl Pts',(131.133354568796,38.1995296011032,24.7584622212581));
#42768=CARTESIAN_POINT('Ctrl Pts',(131.298195476021,38.1362684816494,24.7489501108485));
#42769=CARTESIAN_POINT('Ctrl Pts',(131.599920151667,37.9925883482364,24.7311617706115));
#42770=CARTESIAN_POINT('Ctrl Pts',(131.737537901828,37.9148393853149,24.7228771968075));
#42771=CARTESIAN_POINT('Ctrl Pts',(131.928961773157,37.7883037979966,24.7104917956709));
#42772=CARTESIAN_POINT('Ctrl Pts',(131.987422597113,37.7469404722855,24.7065802556947));
#42773=CARTESIAN_POINT('Ctrl Pts',(132.082431684908,37.6750965760221,24.6999291392002));
#42774=CARTESIAN_POINT('Ctrl Pts',(132.119727775011,37.6456411525219,24.6972383960315));
#42775=CARTESIAN_POINT('Ctrl Pts',(132.171946472495,37.6025871892222,24.6933360809495));
#42776=CARTESIAN_POINT('Ctrl Pts',(132.187387391413,37.5896231219281,24.6921648189547));
#42777=CARTESIAN_POINT('Ctrl Pts',(132.213995416233,37.5668754846209,24.6901142944988));
#42778=CARTESIAN_POINT('Ctrl Pts',(132.225215371392,37.5571550594972,24.6892394510666));
#42779=CARTESIAN_POINT('Ctrl Pts',(132.249693458435,37.5356653301166,24.6873079026262));
#42780=CARTESIAN_POINT('Ctrl Pts',(132.262923138087,37.5238657182528,24.6862491201064));
#42781=CARTESIAN_POINT('Ctrl Pts',(132.300576563752,37.4897484064354,24.683194423011));
#42782=CARTESIAN_POINT('Ctrl Pts',(132.324766285672,37.4671767659435,24.6811814997411));
#42783=CARTESIAN_POINT('Ctrl Pts',(132.532109292819,37.2679463388249,24.6635128909466));
#42784=CARTESIAN_POINT('Ctrl Pts',(132.695153236213,37.0715453116095,24.6468253878137));
#42785=CARTESIAN_POINT('Ctrl Pts',(132.922736348147,36.7244721202652,24.6202722312554));
#42786=CARTESIAN_POINT('Ctrl Pts',(133.001146238963,36.584084636616,24.6101776743207));
#42787=CARTESIAN_POINT('Ctrl Pts',(133.090956575874,36.3924772576549,24.5973181859773));
#42788=CARTESIAN_POINT('Ctrl Pts',(133.111555251576,36.3458193810396,24.5942532448596));
#42789=CARTESIAN_POINT('Ctrl Pts',(133.142479748108,36.2712628408236,24.5894576821353));
#42790=CARTESIAN_POINT('Ctrl Pts',(133.153504098035,36.2436640083246,24.5877041399732));
#42791=CARTESIAN_POINT('Ctrl Pts',(133.173690469567,36.191133550113,24.5844062592439));
#42792=CARTESIAN_POINT('Ctrl Pts',(133.182925124096,36.1662324143684,24.5828596258703));
#42793=CARTESIAN_POINT('Ctrl Pts',(133.203376567791,36.1090322236372,24.5793436065871));
#42794=CARTESIAN_POINT('Ctrl Pts',(133.214399340973,36.0766665715583,24.5773806495906));
#42795=CARTESIAN_POINT('Ctrl Pts',(133.247981639246,35.9729441667907,24.5711693902981));
#42796=CARTESIAN_POINT('Ctrl Pts',(133.268669534253,35.9010025931604,24.5669805668041));
#42797=CARTESIAN_POINT('Ctrl Pts',(133.357935429193,35.546823039581,24.5468302647766));
#42798=CARTESIAN_POINT('Ctrl Pts',(133.39242406578,35.257283833085,24.5319176245196));
#42799=CARTESIAN_POINT('Ctrl Pts',(133.388927898805,34.8992632458069,24.5125464010006));
#42800=CARTESIAN_POINT('Ctrl Pts',(133.386243137713,34.8316649530008,24.5088419110364));
#42801=CARTESIAN_POINT('Ctrl Pts',(133.378361933162,34.7186449031059,24.5025056889307));
#42802=CARTESIAN_POINT('Ctrl Pts',(133.374265627533,34.6731650266735,24.4999170401894));
#42803=CARTESIAN_POINT('Ctrl Pts',(133.367071915915,34.6080484395856,24.496137386194));
#42804=CARTESIAN_POINT('Ctrl Pts',(133.364718325639,34.5883328281089,24.4949833183686));
#42805=CARTESIAN_POINT('Ctrl Pts',(133.36028904894,34.5538093163656,24.4929437010232));
#42806=CARTESIAN_POINT('Ctrl Pts',(133.358288384133,34.5389926941861,24.4920622041559));
#42807=CARTESIAN_POINT('Ctrl Pts',(133.353662891379,34.5063662071838,24.490107189215));
#42808=CARTESIAN_POINT('Ctrl Pts',(133.350994216694,34.4885639452007,24.4890314403384));
#42809=CARTESIAN_POINT('Ctrl Pts',(133.342648310382,34.4357619861346,24.485815625139));
#42810=CARTESIAN_POINT('Ctrl Pts',(133.336563743955,34.4008302144195,24.4836553186297));
#42811=CARTESIAN_POINT('Ctrl Pts',(133.297838333236,34.197433709356,24.4709089808406));
#42812=CARTESIAN_POINT('Ctrl Pts',(133.25299285538,34.0315585005043,24.4598527647854));
#42813=CARTESIAN_POINT('Ctrl Pts',(133.140866228321,33.7145042549144,24.4381747162702));
#42814=CARTESIAN_POINT('Ctrl Pts',(133.074692391641,33.5634017689105,24.4275826689688));
#42815=CARTESIAN_POINT('Ctrl Pts',(132.965566413778,33.3566540262536,24.4129593814519));
#42816=CARTESIAN_POINT('Ctrl Pts',(132.931485431608,33.2966021409348,24.4086928614946));
#42817=CARTESIAN_POINT('Ctrl Pts',(132.86723814407,33.1910431817702,24.4011634332219));
#42818=CARTESIAN_POINT('Ctrl Pts',(132.837762450489,33.1451457912991,24.3978789274453));
#42819=CARTESIAN_POINT('Ctrl Pts',(132.79012974431,33.0747707846583,24.3928236838606));
#42820=CARTESIAN_POINT('Ctrl Pts',(132.772729620079,33.0497943528555,24.3910256360486));
#42821=CARTESIAN_POINT('Ctrl Pts',(132.739583274734,33.0035560940002,24.3876884986761));
#42822=CARTESIAN_POINT('Ctrl Pts',(132.723920105334,32.9822378467044,24.3861464515368));
#42823=CARTESIAN_POINT('Ctrl Pts',(132.688128175638,32.9346999204486,24.382698816871));
#42824=CARTESIAN_POINT('Ctrl Pts',(132.667862083083,32.9085867163374,24.3807986967854));
#42825=CARTESIAN_POINT('Ctrl Pts',(132.604581925559,32.8294660892734,24.3750180314103));
#42826=CARTESIAN_POINT('Ctrl Pts',(132.56034486121,32.7774565196872,24.3711854577915));
#42827=CARTESIAN_POINT('Ctrl Pts',(132.346586833336,32.5410003276086,24.3535313387853));
#42828=CARTESIAN_POINT('Ctrl Pts',(132.158535095543,32.3743800774479,24.3404784790741));
#42829=CARTESIAN_POINT('Ctrl Pts',(131.835025983022,32.14619138228,24.3193613756595));
#42830=CARTESIAN_POINT('Ctrl Pts',(131.710958647749,32.0701270076269,24.3115058145515));
#42831=CARTESIAN_POINT('Ctrl Pts',(131.557574337656,31.9891602907802,24.3016262553113));
#42832=CARTESIAN_POINT('Ctrl Pts',(131.532580304157,31.9763612856899,24.3000111829602));
#42833=CARTESIAN_POINT('Ctrl Pts',(131.492673083546,31.9565474187759,24.2974197564617));
#42834=CARTESIAN_POINT('Ctrl Pts',(131.477862251687,31.9493279939051,24.2964552591049));
#42835=CARTESIAN_POINT('Ctrl Pts',(131.449276575382,31.9356511449311,24.2945873789926));
#42836=CARTESIAN_POINT('Ctrl Pts',(131.43550994076,31.9291780132069,24.2936849377532));
#42837=CARTESIAN_POINT('Ctrl Pts',(131.401037847122,31.9132515330251,24.2914187854233));
#42838=CARTESIAN_POINT('Ctrl Pts',(131.380280042599,31.903913746401,24.2900484906706));
#42839=CARTESIAN_POINT('Ctrl Pts',(131.303443130607,31.8702753452325,24.2849595064262));
#42840=CARTESIAN_POINT('Ctrl Pts',(131.246806599505,31.8472848570331,24.2811759951212));
#42841=CARTESIAN_POINT('Ctrl Pts',(131.005583057582,31.7568812676487,24.2650145874468));
#42842=CARTESIAN_POINT('Ctrl Pts',(130.815941005054,31.7040549936868,24.2522197029305));
#42843=CARTESIAN_POINT('Ctrl Pts',(130.436574000226,31.6331470951516,24.2274589048701));
#42844=CARTESIAN_POINT('Ctrl Pts',(130.247740163927,31.6140085097161,24.2155244208395));
#42845=CARTESIAN_POINT('Ctrl Pts',(130.013592473202,31.6099827098066,24.2013666635207));
#42846=CARTESIAN_POINT('Ctrl Pts',(129.968899838689,31.6100980767917,24.1986915279217));
#42847=CARTESIAN_POINT('Ctrl Pts',(129.895810393906,31.6117324266804,24.1943593804851));
#42848=CARTESIAN_POINT('Ctrl Pts',(129.86740838946,31.6127249652942,24.1926864803077));
#42849=CARTESIAN_POINT('Ctrl Pts',(129.812066056633,31.6153561284719,24.1894463349443));
#42850=CARTESIAN_POINT('Ctrl Pts',(129.785126268043,31.616959556081,24.1878781331347));
#42851=CARTESIAN_POINT('Ctrl Pts',(129.721086394716,31.6215392087954,24.1841704405491));
#42852=CARTESIAN_POINT('Ctrl Pts',(129.684010130816,31.6248050908958,24.1820399948799));
#42853=CARTESIAN_POINT('Ctrl Pts',(129.558348289526,31.6379629592714,24.1748674863531));
#42854=CARTESIAN_POINT('Ctrl Pts',(129.470098812605,31.6507380196447,24.1699130175832));
#42855=CARTESIAN_POINT('Ctrl Pts',(129.116410617838,31.7162701641653,24.1502345285996));
#42856=CARTESIAN_POINT('Ctrl Pts',(128.857248031665,31.7972323911606,24.1363057336784));
#42857=CARTESIAN_POINT('Ctrl Pts',(128.550083144372,31.9352765604378,24.1180691868218));
#42858=CARTESIAN_POINT('Ctrl Pts',(128.490503849463,31.9641789997478,24.1144396757732));
#42859=CARTESIAN_POINT('Ctrl Pts',(128.391938584734,32.0156128959156,24.108218092932));
#42860=CARTESIAN_POINT('Ctrl Pts',(128.352484978957,32.0372104769931,24.10566710795));
#42861=CARTESIAN_POINT('Ctrl Pts',(128.296350899884,32.069407142396,24.1019327964897));
#42862=CARTESIAN_POINT('Ctrl Pts',(128.279313635703,32.0793779518064,24.1007851993323));
#42863=CARTESIAN_POINT('Ctrl Pts',(128.249534501907,32.0971567563929,24.0987525342358));
#42864=CARTESIAN_POINT('Ctrl Pts',(128.236755665565,32.1049010791081,24.0978714171118));
#42865=CARTESIAN_POINT('Ctrl Pts',(128.208622571135,32.1222058633255,24.0959115854776));
#42866=CARTESIAN_POINT('Ctrl Pts',(128.19329354969,32.1318047563406,24.0948305600288));
#42867=CARTESIAN_POINT('Ctrl Pts',(128.148705735776,32.1602244980731,24.091649182839));
#42868=CARTESIAN_POINT('Ctrl Pts',(128.119659811271,32.1793731323099,24.0895297033442));
#42869=CARTESIAN_POINT('Ctrl Pts',(127.938698375858,32.302709938872,24.0760511504062));
#42870=CARTESIAN_POINT('Ctrl Pts',(127.795202818095,32.4186829466646,24.06414825003));
#42871=CARTESIAN_POINT('Ctrl Pts',(127.546283476208,32.6558248076775,24.0419901982629));
#42872=CARTESIAN_POINT('Ctrl Pts',(127.438629656662,32.7739560411853,24.0317524860668));
#42873=CARTESIAN_POINT('Ctrl Pts',(127.279997535091,32.9748406075572,24.0157800362342));
#42874=CARTESIAN_POINT('Ctrl Pts',(127.223545612863,33.0529541029085,24.0098736573249));
#42875=CARTESIAN_POINT('Ctrl Pts',(127.149901930039,33.1645860521701,24.0018453776311));
#42876=CARTESIAN_POINT('Ctrl Pts',(127.129827604531,33.1961391526485,23.9996193968764));
#42877=CARTESIAN_POINT('Ctrl Pts',(127.096156545385,33.2510494297626,23.9958179073234));
#42878=CARTESIAN_POINT('Ctrl Pts',(127.082309752074,33.274248399653,23.9942334839521));
#42879=CARTESIAN_POINT('Ctrl Pts',(127.054498206573,33.3221357080055,23.9910060166966));
#42880=CARTESIAN_POINT('Ctrl Pts',(127.040562983593,33.3468387814902,23.9893641100284));
#42881=CARTESIAN_POINT('Ctrl Pts',(127.005606839114,33.4106646518103,23.9851786309603));
#42882=CARTESIAN_POINT('Ctrl Pts',(126.985041410932,33.4500315441084,23.982650989225));
#42883=CARTESIAN_POINT('Ctrl Pts',(126.890677085338,33.6396556115579,23.9707127367289));
#42884=CARTESIAN_POINT('Ctrl Pts',(126.827298718546,33.7948441014666,23.9616564167831));
#42885=CARTESIAN_POINT('Ctrl Pts',(126.716773322046,34.1355760686435,23.9425609732444));
#42886=CARTESIAN_POINT('Ctrl Pts',(126.673334989371,34.3216938884895,23.9325965252199));
#42887=CARTESIAN_POINT('Ctrl Pts',(126.633473070127,34.5948223413107,23.9175604296236));
#42888=CARTESIAN_POINT('Ctrl Pts',(126.62434924651,34.6796060877563,23.9128334293433));
#42889=CARTESIAN_POINT('Ctrl Pts',(126.616713754069,34.7893085292808,23.9065406226926));
#42890=CARTESIAN_POINT('Ctrl Pts',(126.615266654413,34.8139977935598,23.9051128761941));
#42891=CARTESIAN_POINT('Ctrl Pts',(126.613340085274,34.8544391205199,23.9027522086949));
#42892=CARTESIAN_POINT('Ctrl Pts',(126.612700057938,34.8701830829695,23.9018277383581));
#42893=CARTESIAN_POINT('Ctrl Pts',(126.611697666212,34.8999538572098,23.9000683741713));
#42894=CARTESIAN_POINT('Ctrl Pts',(126.611312583221,34.9139795863136,23.8992347927287));
#42895=CARTESIAN_POINT('Ctrl Pts',(126.610508420011,34.9518346299784,23.8969730259222));
#42896=CARTESIAN_POINT('Ctrl Pts',(126.610253568627,34.9756661873626,23.895536357727));
#42897=CARTESIAN_POINT('Ctrl Pts',(126.610238801927,35.0753183644395,23.8894809500956));
#42898=CARTESIAN_POINT('Ctrl Pts',(126.612771473415,35.1511127742874,23.8847595611865));
#42899=CARTESIAN_POINT('Ctrl Pts',(126.627938181166,35.3773337443965,23.8704393478627));
#42900=CARTESIAN_POINT('Ctrl Pts',(126.648078376497,35.5270679312864,23.8606650076194));
#42901=CARTESIAN_POINT('Ctrl Pts',(126.712847935603,35.8458382130121,23.8397261393574));
#42902=CARTESIAN_POINT('Ctrl Pts',(126.760697643102,36.0137635588549,23.828621481531));
#42903=CARTESIAN_POINT('Ctrl Pts',(126.821241887301,36.1772433577858,23.8178898623416));
#42904=CARTESIAN_POINT('',(126.61025139839,34.9970473867279,24.2343657983436));
#42905=CARTESIAN_POINT('Ctrl Pts',(126.821241956411,36.1772435443955,24.1659079080442));
#42906=CARTESIAN_POINT('Ctrl Pts',(126.81168092342,36.151427127163,24.1676083132325));
#42907=CARTESIAN_POINT('Ctrl Pts',(126.80243217331,36.1254882379945,24.1693001454415));
#42908=CARTESIAN_POINT('Ctrl Pts',(126.776459846116,36.0497397820318,24.174192253994));
#42909=CARTESIAN_POINT('Ctrl Pts',(126.760578224573,35.9996558173652,24.1773663332289));
#42910=CARTESIAN_POINT('Ctrl Pts',(126.73662887044,35.9175522658716,24.1824734265101));
#42911=CARTESIAN_POINT('Ctrl Pts',(126.72785381004,35.8857498048348,24.184428534445));
#42912=CARTESIAN_POINT('Ctrl Pts',(126.71288235402,35.828228310642,24.1879244880184));
#42913=CARTESIAN_POINT('Ctrl Pts',(126.706520203129,35.8025555678061,24.1894704820985));
#42914=CARTESIAN_POINT('Ctrl Pts',(126.693473213447,35.7471378305393,24.1927780457357));
#42915=CARTESIAN_POINT('Ctrl Pts',(126.686887822117,35.7173716694405,24.1945363630827));
#42916=CARTESIAN_POINT('Ctrl Pts',(126.674196589676,35.6560993459167,24.198120409506));
#42917=CARTESIAN_POINT('Ctrl Pts',(126.668134808744,35.6245871594675,24.1999446350986));
#42918=CARTESIAN_POINT('Ctrl Pts',(126.650875049431,35.5274458934978,24.2055140255797));
#42919=CARTESIAN_POINT('Ctrl Pts',(126.641161920763,35.4615675591525,24.2092152021343));
#42920=CARTESIAN_POINT('Ctrl Pts',(126.617863520246,35.2632165309681,24.2201815224655));
#42921=CARTESIAN_POINT('Ctrl Pts',(126.610135275629,35.1301874299042,24.2272962254604));
#42922=CARTESIAN_POINT('Ctrl Pts',(126.610251286806,34.9970463750651,24.2343660470093));
#42923=CARTESIAN_POINT('Ctrl Pts',(126.610251285916,34.9970473969534,24.2343659927468));
#42924=CARTESIAN_POINT('Ctrl Pts',(126.610447429808,34.7718635519805,24.2463233086417));
#42925=CARTESIAN_POINT('Ctrl Pts',(126.633081622873,34.5472763101012,24.258087103762));
#42926=CARTESIAN_POINT('Ctrl Pts',(126.683070643506,34.3006529531977,24.2722722320412));
#42927=CARTESIAN_POINT('Ctrl Pts',(126.688636419679,34.2747567277788,24.2737780767598));
#42928=CARTESIAN_POINT('Ctrl Pts',(126.699512643886,34.2268899970247,24.2765962743958));
#42929=CARTESIAN_POINT('Ctrl Pts',(126.704740505068,34.2049021026687,24.2779045359552));
#42930=CARTESIAN_POINT('Ctrl Pts',(126.713883912621,34.1680857684514,24.2801206168535));
#42931=CARTESIAN_POINT('Ctrl Pts',(126.717681038701,34.1532282136674,24.2810219752463));
#42932=CARTESIAN_POINT('Ctrl Pts',(126.725794642887,34.1223557468768,24.282910439008));
#42933=CARTESIAN_POINT('Ctrl Pts',(126.730128017045,34.1063460707788,24.2838983876695));
#42934=CARTESIAN_POINT('Ctrl Pts',(126.742250537134,34.0628282642698,24.2866062056763));
#42935=CARTESIAN_POINT('Ctrl Pts',(126.750270319019,34.0353864460355,24.288338160018));
#42936=CARTESIAN_POINT('Ctrl Pts',(126.807231399905,33.8492564327964,24.3002372164349));
#42937=CARTESIAN_POINT('Ctrl Pts',(126.867425924522,33.6942619355829,24.3108897090073));
#42938=CARTESIAN_POINT('Ctrl Pts',(127.016163420946,33.3814697637651,24.3332060381767));
#42939=CARTESIAN_POINT('Ctrl Pts',(127.106477103547,33.2250476844012,24.3448367477163));
#42940=CARTESIAN_POINT('Ctrl Pts',(127.248450231542,33.0190258451249,24.3604960373607));
#42941=CARTESIAN_POINT('Ctrl Pts',(127.289858387392,32.9627424904563,24.3648156908691));
#42942=CARTESIAN_POINT('Ctrl Pts',(127.366940528956,32.8644835421773,24.372427768452));
#42943=CARTESIAN_POINT('Ctrl Pts',(127.401953026644,32.8220226875458,24.3757425007528));
#42944=CARTESIAN_POINT('Ctrl Pts',(127.457979813729,32.7573518180865,24.3808333863997));
#42945=CARTESIAN_POINT('Ctrl Pts',(127.478285687131,32.7345432003817,24.3826374785126));
#42946=CARTESIAN_POINT('Ctrl Pts',(127.516745830408,32.6925006985616,24.3859802204642));
#42947=CARTESIAN_POINT('Ctrl Pts',(127.534822209134,32.673199016931,24.3875219154788));
#42948=CARTESIAN_POINT('Ctrl Pts',(127.575903451376,32.6303492816788,24.3909616223566));
#42949=CARTESIAN_POINT('Ctrl Pts',(127.599029364226,32.6069206617977,24.3928542809879));
#42950=CARTESIAN_POINT('Ctrl Pts',(127.670611620867,32.5364838035046,24.3985853569239));
#42951=CARTESIAN_POINT('Ctrl Pts',(127.720135416407,32.4905816229533,24.4023770449682));
#42952=CARTESIAN_POINT('Ctrl Pts',(127.997305819603,32.2486637775179,24.4227624606193));
#42953=CARTESIAN_POINT('Ctrl Pts',(128.248842370753,32.0821117198644,24.4381693914244));
#42954=CARTESIAN_POINT('Ctrl Pts',(128.58044252669,31.9210515451339,24.4581065741255));
#42955=CARTESIAN_POINT('Ctrl Pts',(128.642744017878,31.8930847670628,24.4618445005339));
#42956=CARTESIAN_POINT('Ctrl Pts',(128.748327533255,31.8494708530255,24.4682317414877));
#42957=CARTESIAN_POINT('Ctrl Pts',(128.791161440821,31.8327888003664,24.4708370675807));
#42958=CARTESIAN_POINT('Ctrl Pts',(128.853011371577,31.8101381829686,24.4746367848401));
#42959=CARTESIAN_POINT('Ctrl Pts',(128.871763127689,31.8034576737053,24.475793697469));
#42960=CARTESIAN_POINT('Ctrl Pts',(128.90470436756,31.7920479710327,24.4778363896447));
#42961=CARTESIAN_POINT('Ctrl Pts',(128.918868015395,31.7872469184201,24.4787180718346));
#42962=CARTESIAN_POINT('Ctrl Pts',(128.950115208986,31.7768850897746,24.4806710483873));
#42963=CARTESIAN_POINT('Ctrl Pts',(128.967211247072,31.7713663634649,24.4817445391054));
#42964=CARTESIAN_POINT('Ctrl Pts',(129.018001302014,31.7554156315153,24.4849467582556));
#42965=CARTESIAN_POINT('Ctrl Pts',(129.051814192271,31.7453736573283,24.4870954841807));
#42966=CARTESIAN_POINT('Ctrl Pts',(129.261689925548,31.6865914069688,24.5005106610348));
#42967=CARTESIAN_POINT('Ctrl Pts',(129.441285970382,31.651626172727,24.5123110674619));
#42968=CARTESIAN_POINT('Ctrl Pts',(129.78239976852,31.613431849617,24.5344343467374));
#42969=CARTESIAN_POINT('Ctrl Pts',(129.943070853665,31.6069246258301,24.5447373374876));
#42970=CARTESIAN_POINT('Ctrl Pts',(130.200226190926,31.6147882949694,24.5607939471277));
#42971=CARTESIAN_POINT('Ctrl Pts',(130.296679788106,31.6218743863781,24.5667216304026));
#42972=CARTESIAN_POINT('Ctrl Pts',(130.429892341415,31.6374118203363,24.5747731379311));
#42973=CARTESIAN_POINT('Ctrl Pts',(130.467005237902,31.6423649740295,24.5770018493834));
#42974=CARTESIAN_POINT('Ctrl Pts',(130.530752354692,31.6519502317445,24.5808065160665));
#42975=CARTESIAN_POINT('Ctrl Pts',(130.557426643587,31.6562878543893,24.5823914250385));
#42976=CARTESIAN_POINT('Ctrl Pts',(130.611969832366,31.6658282082056,24.5856186092044));
#42977=CARTESIAN_POINT('Ctrl Pts',(130.639831091482,31.6710625031052,24.5872597634095));
#42978=CARTESIAN_POINT('Ctrl Pts',(130.71109690653,31.6853789944296,24.5914406746976));
#42979=CARTESIAN_POINT('Ctrl Pts',(130.754395544021,31.694964623461,24.5939645715964));
#42980=CARTESIAN_POINT('Ctrl Pts',(130.957874859001,31.7442190484277,24.6057654217752));
#42981=CARTESIAN_POINT('Ctrl Pts',(131.115213722613,31.7947012189676,24.6146992424365));
#42982=CARTESIAN_POINT('Ctrl Pts',(131.447080315978,31.9285925129293,24.6337843744378));
#42983=CARTESIAN_POINT('Ctrl Pts',(131.619406117166,32.015858205226,24.6438502027838));
#42984=CARTESIAN_POINT('Ctrl Pts',(131.856220968248,32.1623623893905,24.659016375288));
#42985=CARTESIAN_POINT('Ctrl Pts',(131.927331681797,32.2101731566946,24.6637654562619));
#42986=CARTESIAN_POINT('Ctrl Pts',(132.016565812746,32.2752099431086,24.6700837818974));
#42987=CARTESIAN_POINT('Ctrl Pts',(132.036420849003,32.2900168671208,24.6715135810462));
#42988=CARTESIAN_POINT('Ctrl Pts',(132.068644763198,32.3146019967338,24.6738767655178));
#42989=CARTESIAN_POINT('Ctrl Pts',(132.08111121167,32.3242515629454,24.6748016648582));
#42990=CARTESIAN_POINT('Ctrl Pts',(132.104540416444,32.3426495515891,24.6765610933071));
#42991=CARTESIAN_POINT('Ctrl Pts',(132.115517084681,32.3513797518478,24.6773943015001));
#42992=CARTESIAN_POINT('Ctrl Pts',(132.144974007505,32.3751079964873,24.6796537077394));
#42993=CARTESIAN_POINT('Ctrl Pts',(132.163350650214,32.3902326890632,24.681088358577));
#42994=CARTESIAN_POINT('Ctrl Pts',(132.234507324077,32.4500653799052,24.6867373980346));
#42995=CARTESIAN_POINT('Ctrl Pts',(132.286070274267,32.4961887161915,24.6910355061395));
#42996=CARTESIAN_POINT('Ctrl Pts',(132.4904374177,32.6905740973933,24.7088047143256));
#42997=CARTESIAN_POINT('Ctrl Pts',(132.630525463145,32.8514975107663,24.7227046782548));
#42998=CARTESIAN_POINT('Ctrl Pts',(132.818794666682,33.1140156765076,24.7433331048796));
#42999=CARTESIAN_POINT('Ctrl Pts',(132.878596442633,33.2066160340188,24.7502809841382));
#43000=CARTESIAN_POINT('Ctrl Pts',(132.971992707294,33.3679823369029,24.7617983077101));
#43001=CARTESIAN_POINT('Ctrl Pts',(133.007962346652,33.4352680080159,24.766439260946));
#43002=CARTESIAN_POINT('Ctrl Pts',(133.056829933331,33.5346055044568,24.7730623541747));
#43003=CARTESIAN_POINT('Ctrl Pts',(133.071555357095,33.5657273312423,24.775105914292));
#43004=CARTESIAN_POINT('Ctrl Pts',(133.096806917742,33.6212691781546,24.7786989589256));
#43005=CARTESIAN_POINT('Ctrl Pts',(133.107524465589,33.645598464111,24.7802548025497));
#43006=CARTESIAN_POINT('Ctrl Pts',(133.129562955564,33.6972659053719,24.7835220116048));
#43007=CARTESIAN_POINT('Ctrl Pts',(133.140814443324,33.7246313760677,24.7852309571184));
#43008=CARTESIAN_POINT('Ctrl Pts',(133.170244114801,33.7989616552292,24.789817301271));
#43009=CARTESIAN_POINT('Ctrl Pts',(133.187736762664,33.8461908507874,24.792672163936));
#43010=CARTESIAN_POINT('Ctrl Pts',(133.288335586404,34.1375795050371,24.8099602120246));
#43011=CARTESIAN_POINT('Ctrl Pts',(133.344404117157,34.3901704856982,24.8234804305214));
#43012=CARTESIAN_POINT('Ctrl Pts',(133.383190034256,34.7602679168404,24.8432575552909));
#43013=CARTESIAN_POINT('Ctrl Pts',(133.389345019598,34.8743668732681,24.8493643286174));
#43014=CARTESIAN_POINT('Ctrl Pts',(133.389948807836,35.053139882388,24.8592205563777));
#43015=CARTESIAN_POINT('Ctrl Pts',(133.388320874856,35.1177172293669,24.8628401733385));
#43016=CARTESIAN_POINT('Ctrl Pts',(133.383636288177,35.2047438232886,24.8678440567895));
#43017=CARTESIAN_POINT('Ctrl Pts',(133.382197932421,35.2272699951454,24.8691507022791));
#43018=CARTESIAN_POINT('Ctrl Pts',(133.379405152333,35.2650676990335,24.8713648595265));
#43019=CARTESIAN_POINT('Ctrl Pts',(133.378171860723,35.2803478939223,24.8722659364183));
#43020=CARTESIAN_POINT('Ctrl Pts',(133.375387592872,35.3121523688025,24.8741547593598));
#43021=CARTESIAN_POINT('Ctrl Pts',(133.373818855669,35.328674317659,24.8751433601113));
#43022=CARTESIAN_POINT('Ctrl Pts',(133.369212581616,35.3736734011228,24.8778548276226));
#43023=CARTESIAN_POINT('Ctrl Pts',(133.365935442272,35.4021240002849,24.8795898314739));
#43024=CARTESIAN_POINT('Ctrl Pts',(133.341072275835,35.59629781435,24.8915573087641));
#43025=CARTESIAN_POINT('Ctrl Pts',(133.307617858633,35.7602559971378,24.9022809968109));
#43026=CARTESIAN_POINT('Ctrl Pts',(133.225151470969,36.0523352079134,24.9218370378831));
#43027=CARTESIAN_POINT('Ctrl Pts',(133.180195955434,36.1812569971406,24.9306394596573));
#43028=CARTESIAN_POINT('Ctrl Pts',(133.074427855882,36.434331530677,24.9480273139767));
#43029=CARTESIAN_POINT('Ctrl Pts',(133.013547358119,36.5581891518807,24.9565929592968));
#43030=CARTESIAN_POINT('Ctrl Pts',(132.924612389499,36.714290312089,24.9674255855323));
#43031=CARTESIAN_POINT('Ctrl Pts',(132.90327116899,36.7501901770647,24.969920237475));
#43032=CARTESIAN_POINT('Ctrl Pts',(132.866612505062,36.8093402465385,24.9740378686356));
#43033=CARTESIAN_POINT('Ctrl Pts',(132.851662718574,36.8328118262213,24.9756737981008));
#43034=CARTESIAN_POINT('Ctrl Pts',(132.821613487206,36.8787320502932,24.9788793047147));
#43035=CARTESIAN_POINT('Ctrl Pts',(132.806530999555,36.9011892589982,24.9804493412534));
#43036=CARTESIAN_POINT('Ctrl Pts',(132.772511337284,36.9505559401192,24.9839073559653));
#43037=CARTESIAN_POINT('Ctrl Pts',(132.753447802503,36.9773752544277,24.9857904655089));
#43038=CARTESIAN_POINT('Ctrl Pts',(132.684941748547,37.0708400197813,24.9923738442464));
#43039=CARTESIAN_POINT('Ctrl Pts',(132.633443984725,37.1359458861149,24.9969967699041));
#43040=CARTESIAN_POINT('Ctrl Pts',(132.399556463027,37.4103024955336,25.0167766399029));
#43041=CARTESIAN_POINT('Ctrl Pts',(132.194265716785,37.5985799501043,25.0310506831749));
#43042=CARTESIAN_POINT('Ctrl Pts',(131.913997413708,37.7984768509725,25.0496866726311));
#43043=CARTESIAN_POINT('Ctrl Pts',(131.858534996384,37.835613788992,25.0533438338818));
#43044=CARTESIAN_POINT('Ctrl Pts',(131.763706638497,37.8951320644387,25.0596077317867));
#43045=CARTESIAN_POINT('Ctrl Pts',(131.724922074287,37.918406107543,25.0621726507204));
#43046=CARTESIAN_POINT('Ctrl Pts',(131.668521724666,37.950734094796,25.0659237444595));
#43047=CARTESIAN_POINT('Ctrl Pts',(131.651272630055,37.9604214402965,25.0670737452924));
#43048=CARTESIAN_POINT('Ctrl Pts',(131.620844925697,37.977161429794,25.0691089889572));
#43049=CARTESIAN_POINT('Ctrl Pts',(131.607702929539,37.9842787622033,25.0699902431549));
#43050=CARTESIAN_POINT('Ctrl Pts',(131.578581429694,37.9998019438753,25.071948266341));
#43051=CARTESIAN_POINT('Ctrl Pts',(131.562581772992,38.0081670836478,25.0730273162781));
#43052=CARTESIAN_POINT('Ctrl Pts',(131.515695209553,38.0322059215152,25.0761973307467));
#43053=CARTESIAN_POINT('Ctrl Pts',(131.484634832915,38.0475340739827,25.0783072282422));
#43054=CARTESIAN_POINT('Ctrl Pts',(131.284116212006,38.1426962452932,25.0919658861486));
#43055=CARTESIAN_POINT('Ctrl Pts',(131.108532214178,38.2088378816644,25.1040779219534));
#43056=CARTESIAN_POINT('Ctrl Pts',(130.776768232748,38.3033154241358,25.1263084250582));
#43057=CARTESIAN_POINT('Ctrl Pts',(130.62229795282,38.335867860018,25.1364150119625));
#43058=CARTESIAN_POINT('Ctrl Pts',(130.371375341455,38.370702226433,25.1522179494702));
#43059=CARTESIAN_POINT('Ctrl Pts',(130.276118010768,38.3798394411623,25.1580811255089));
#43060=CARTESIAN_POINT('Ctrl Pts',(130.143343824484,38.3869232590374,25.1660622703433));
#43061=CARTESIAN_POINT('Ctrl Pts',(130.106061964611,38.3882956838372,25.1682826909218));
#43062=CARTESIAN_POINT('Ctrl Pts',(130.041768923691,38.3896001899669,25.1720777242948));
#43063=CARTESIAN_POINT('Ctrl Pts',(130.014767816664,38.3898253738495,25.1736611718897));
#43064=CARTESIAN_POINT('Ctrl Pts',(129.959376883647,38.3896254652524,25.1768892647164));
#43065=CARTESIAN_POINT('Ctrl Pts',(129.930989268454,38.3891663609864,25.1785327393529));
#43066=CARTESIAN_POINT('Ctrl Pts',(129.858078550014,38.387070720279,25.1827276839961));
#43067=CARTESIAN_POINT('Ctrl Pts',(129.813575176762,38.3849129688725,25.1852630772148));
#43068=CARTESIAN_POINT('Ctrl Pts',(129.596160792958,38.3700705132298,25.1975443971339));
#43069=CARTESIAN_POINT('Ctrl Pts',(129.424348479733,38.3450105578429,25.2069071459543));
#43070=CARTESIAN_POINT('Ctrl Pts',(129.098003392692,38.2715086729099,25.2247214112106));
#43071=CARTESIAN_POINT('Ctrl Pts',(128.94354396535,38.2249441057969,25.2331719602147));
#43072=CARTESIAN_POINT('Ctrl Pts',(128.726198435116,38.1421239681673,25.2457269512349));
#43073=CARTESIAN_POINT('Ctrl Pts',(128.660234936429,38.1145693093006,25.2496318737395));
#43074=CARTESIAN_POINT('Ctrl Pts',(128.55199965517,38.0652818529753,25.2562729645903));
#43075=CARTESIAN_POINT('Ctrl Pts',(128.509224142083,38.0447076566642,25.2589604887549));
#43076=CARTESIAN_POINT('Ctrl Pts',(128.448923614584,38.0141289324193,25.2628589435286));
#43077=CARTESIAN_POINT('Ctrl Pts',(128.431032401559,38.0048547064027,25.2640296727719));
#43078=CARTESIAN_POINT('Ctrl Pts',(128.399989746438,37.9884103790362,25.2660874213966));
#43079=CARTESIAN_POINT('Ctrl Pts',(128.386801440671,37.9813117588307,25.2669701264422));
#43080=CARTESIAN_POINT('Ctrl Pts',(128.35804723808,37.9655881109694,25.2689137524011));
#43081=CARTESIAN_POINT('Ctrl Pts',(128.342502171476,37.9569279047334,25.2699767081016));
#43082=CARTESIAN_POINT('Ctrl Pts',(128.297976550915,37.9316611133745,25.2730549741757));
#43083=CARTESIAN_POINT('Ctrl Pts',(128.269173098016,37.9147484899942,25.2750876788226));
#43084=CARTESIAN_POINT('Ctrl Pts',(128.02455975007,37.7662137832415,25.2926776380643));
#43085=CARTESIAN_POINT('Ctrl Pts',(127.823857573102,37.6112640181542,25.309249756168));
#43086=CARTESIAN_POINT('Ctrl Pts',(127.558342291236,37.3542200632127,25.3328981072242));
#43087=CARTESIAN_POINT('Ctrl Pts',(127.478681851734,37.2687007430472,25.3402833524193));
#43088=CARTESIAN_POINT('Ctrl Pts',(127.352596733101,37.1184788012222,25.3524186677325));
#43089=CARTESIAN_POINT('Ctrl Pts',(127.303749046362,37.0559496179156,25.3572510919676));
#43090=CARTESIAN_POINT('Ctrl Pts',(127.236618535366,36.9635038497255,25.3640902051661));
#43091=CARTESIAN_POINT('Ctrl Pts',(127.216537287754,36.9349315112926,25.3661640994209));
#43092=CARTESIAN_POINT('Ctrl Pts',(127.181918583736,36.8840201973484,25.3697911851142));
#43093=CARTESIAN_POINT('Ctrl Pts',(127.16719660003,36.8618109275741,25.3713511534022));
#43094=CARTESIAN_POINT('Ctrl Pts',(127.136819849693,36.8147906109674,25.3746083817646));
#43095=CARTESIAN_POINT('Ctrl Pts',(127.121222169293,36.7899451987181,25.3763034682859));
#43096=CARTESIAN_POINT('Ctrl Pts',(127.080368322498,36.7229537876915,25.3808071650417));
#43097=CARTESIAN_POINT('Ctrl Pts',(127.055702169725,36.6804551515435,25.38359467332));
#43098=CARTESIAN_POINT('Ctrl Pts',(126.950289583187,36.489383015487,25.3958449719673));
#43099=CARTESIAN_POINT('Ctrl Pts',(126.879871236484,36.3355525918427,25.404949309684));
#43100=CARTESIAN_POINT('Ctrl Pts',(126.821241938915,36.1772434971515,25.4139333020124));
#43101=CARTESIAN_POINT('Origin',(130.,35.,23.));
#43102=CARTESIAN_POINT('',(126.821241918426,36.1772434418289,26.660716603687));
#43103=CARTESIAN_POINT('',(126.821241849252,36.1772432550457,26.31957821124));
#43104=CARTESIAN_POINT('',(126.821241918358,36.1772434416438,23.));
#43105=CARTESIAN_POINT('',(126.610251050396,35.0026685497381,25.1397300250475));
#43106=CARTESIAN_POINT('Ctrl Pts',(126.821241849252,36.1772432550457,26.31957821124));
#43107=CARTESIAN_POINT('Ctrl Pts',(126.87264245335,36.3160336779512,26.3116710105479));
#43108=CARTESIAN_POINT('Ctrl Pts',(126.933098780024,36.4513660671469,26.3038949611646));
#43109=CARTESIAN_POINT('Ctrl Pts',(127.064471806615,36.7002495766796,26.2888430195471));
#43110=CARTESIAN_POINT('Ctrl Pts',(127.133591949016,36.8143517529012,26.2816081672139));
#43111=CARTESIAN_POINT('Ctrl Pts',(127.225173264532,36.9471850152158,26.2724176359797));
#43112=CARTESIAN_POINT('Ctrl Pts',(127.241391176002,36.9700939427004,26.2708032366146));
#43113=CARTESIAN_POINT('Ctrl Pts',(127.267576166349,37.0061247360562,26.2682126403952));
#43114=CARTESIAN_POINT('Ctrl Pts',(127.27735800387,37.0193803503733,26.267248287326));
#43115=CARTESIAN_POINT('Ctrl Pts',(127.296466527679,37.0448835682806,26.2653698664562));
#43116=CARTESIAN_POINT('Ctrl Pts',(127.305780647298,37.0571397836088,26.2644566006722));
#43117=CARTESIAN_POINT('Ctrl Pts',(127.329169140659,37.0874848214385,26.2621698788389));
#43118=CARTESIAN_POINT('Ctrl Pts',(127.343343989076,37.1054949858957,26.2607898080824));
#43119=CARTESIAN_POINT('Ctrl Pts',(127.399974450612,37.1759657061189,26.2553034920362));
#43120=CARTESIAN_POINT('Ctrl Pts',(127.443807805546,37.2272942873035,26.2511163237943));
#43121=CARTESIAN_POINT('Ctrl Pts',(127.571667889857,37.3682691100777,26.2391429553349));
#43122=CARTESIAN_POINT('Ctrl Pts',(127.659076980421,37.4547041023452,26.2312337022798));
#43123=CARTESIAN_POINT('Ctrl Pts',(127.932364382142,37.697046514249,26.207689429004));
#43124=CARTESIAN_POINT('Ctrl Pts',(128.130508809315,37.8379946657421,26.1921535343798));
#43125=CARTESIAN_POINT('Ctrl Pts',(128.386902116052,37.9817726221802,26.17427543981));
#43126=CARTESIAN_POINT('Ctrl Pts',(128.432351729646,38.0059161811603,26.1711804082734));
#43127=CARTESIAN_POINT('Ctrl Pts',(128.505227450478,38.0425262169856,26.1663317351438));
#43128=CARTESIAN_POINT('Ctrl Pts',(128.532298880287,38.0556773825983,26.1645548646702));
#43129=CARTESIAN_POINT('Ctrl Pts',(128.581126138749,38.0785987951777,26.1613922612648));
#43130=CARTESIAN_POINT('Ctrl Pts',(128.602816443469,38.0885031533155,26.1600020477003));
#43131=CARTESIAN_POINT('Ctrl Pts',(128.654075073801,38.1112586612751,26.1567501975345));
#43132=CARTESIAN_POINT('Ctrl Pts',(128.683726081199,38.1239186029037,26.1548950665848));
#43133=CARTESIAN_POINT('Ctrl Pts',(128.772584280695,38.1603681150139,26.1494088484061));
#43134=CARTESIAN_POINT('Ctrl Pts',(128.832288854038,38.1829117749427,26.1458186016252));
#43135=CARTESIAN_POINT('Ctrl Pts',(129.048071606726,38.2574987101007,26.1331377740165));
#43136=CARTESIAN_POINT('Ctrl Pts',(129.207260332334,38.2998538543804,26.124337407227));
#43137=CARTESIAN_POINT('Ctrl Pts',(129.576723672592,38.3698638535487,26.1043741331663));
#43138=CARTESIAN_POINT('Ctrl Pts',(129.787753451535,38.3897019476663,26.0933033377676));
#43139=CARTESIAN_POINT('Ctrl Pts',(130.043946239876,38.389760054611,26.0789633544154));
#43140=CARTESIAN_POINT('Ctrl Pts',(130.088654952422,38.3888854223028,26.0764267098409));
#43141=CARTESIAN_POINT('Ctrl Pts',(130.152803922758,38.3863602592305,26.072721704868));
#43142=CARTESIAN_POINT('Ctrl Pts',(130.17226935427,38.3854258335599,26.071588795585));
#43143=CARTESIAN_POINT('Ctrl Pts',(130.206650590422,38.3834781039575,26.0695707861939));
#43144=CARTESIAN_POINT('Ctrl Pts',(130.221569413043,38.3825338919106,26.0686893954738));
#43145=CARTESIAN_POINT('Ctrl Pts',(130.254461787232,38.3802335889637,26.0667331211767));
#43146=CARTESIAN_POINT('Ctrl Pts',(130.272430842172,38.3788328341725,26.0656559857006));
#43147=CARTESIAN_POINT('Ctrl Pts',(130.325827559845,38.3742416559427,26.0624318107928));
#43148=CARTESIAN_POINT('Ctrl Pts',(130.361216056157,38.370636897761,26.0602643813034));
#43149=CARTESIAN_POINT('Ctrl Pts',(130.537586020666,38.349862148799,26.0493305542498));
#43150=CARTESIAN_POINT('Ctrl Pts',(130.677438050956,38.3244016636897,26.0402448634844));
#43151=CARTESIAN_POINT('Ctrl Pts',(131.08246708357,38.2240422492453,26.0133805593485));
#43152=CARTESIAN_POINT('Ctrl Pts',(131.34065662137,38.1255196558237,25.9956390174097));
#43153=CARTESIAN_POINT('Ctrl Pts',(131.626504695175,37.9744221904537,25.9760379551903));
#43154=CARTESIAN_POINT('Ctrl Pts',(131.668423574384,37.951113013679,25.9731609197076));
#43155=CARTESIAN_POINT('Ctrl Pts',(131.734954666002,37.9122471864839,25.9685885124051));
#43156=CARTESIAN_POINT('Ctrl Pts',(131.759884553984,37.897250041651,25.9668737298206));
#43157=CARTESIAN_POINT('Ctrl Pts',(131.807330599159,37.8678693813019,25.9636063651761));
#43158=CARTESIAN_POINT('Ctrl Pts',(131.829875725273,37.8535370284893,25.962052101296));
#43159=CARTESIAN_POINT('Ctrl Pts',(131.881932201038,37.8195730820643,25.9584580536347));
#43160=CARTESIAN_POINT('Ctrl Pts',(131.91131004776,37.7997419899689,25.9564257681728));
#43161=CARTESIAN_POINT('Ctrl Pts',(132.008143089599,37.7321415902902,25.9497080831998));
#43162=CARTESIAN_POINT('Ctrl Pts',(132.074163993074,37.6823649142129,25.9450973998106));
#43163=CARTESIAN_POINT('Ctrl Pts',(132.234788411982,37.551781361527,25.9337265155938));
#43164=CARTESIAN_POINT('Ctrl Pts',(132.326888494108,37.468088325903,25.9270663574183));
#43165=CARTESIAN_POINT('Ctrl Pts',(132.54821820058,37.2435342966165,25.9103062668759));
#43166=CARTESIAN_POINT('Ctrl Pts',(132.670513129399,37.0964761975298,25.9003133042839));
#43167=CARTESIAN_POINT('Ctrl Pts',(132.818732974382,36.8840872040139,25.8860769683793));
#43168=CARTESIAN_POINT('Ctrl Pts',(132.856002022722,36.8270991760439,25.8822723042224));
#43169=CARTESIAN_POINT('Ctrl Pts',(132.903879701195,36.7488418879926,25.8770140992347));
#43170=CARTESIAN_POINT('Ctrl Pts',(132.916019656605,36.728523810385,25.8756459362484));
#43171=CARTESIAN_POINT('Ctrl Pts',(132.93500069655,36.6959870315647,25.8734476026125));
#43172=CARTESIAN_POINT('Ctrl Pts',(132.94198077563,36.6838498152629,25.8726259399405));
#43173=CARTESIAN_POINT('Ctrl Pts',(132.956675522467,36.657927758442,25.8708668952331));
#43174=CARTESIAN_POINT('Ctrl Pts',(132.964369373089,36.6441316226644,25.8699282004673));
#43175=CARTESIAN_POINT('Ctrl Pts',(132.983950690853,36.6084353461604,25.8674939828363));
#43176=CARTESIAN_POINT('Ctrl Pts',(132.995693410953,36.5864573414299,25.8659900298847));
#43177=CARTESIAN_POINT('Ctrl Pts',(133.047525731707,36.4868188324965,25.8591551186033));
#43178=CARTESIAN_POINT('Ctrl Pts',(133.084842396766,36.4077600312121,25.8536873818405));
#43179=CARTESIAN_POINT('Ctrl Pts',(133.198004361153,36.1418484801708,25.8353488398284));
#43180=CARTESIAN_POINT('Ctrl Pts',(133.260242317555,35.9496697544995,25.8222045439304));
#43181=CARTESIAN_POINT('Ctrl Pts',(133.339466945969,35.6019848610798,25.7994791137931));
#43182=CARTESIAN_POINT('Ctrl Pts',(133.363499014095,35.4486758660495,25.7897966691731));
#43183=CARTESIAN_POINT('Ctrl Pts',(133.38076981964,35.2504630202239,25.7777759482062));
#43184=CARTESIAN_POINT('Ctrl Pts',(133.383732882833,35.2066115861234,25.7751465260161));
#43185=CARTESIAN_POINT('Ctrl Pts',(133.387199324183,35.134479668877,25.7708687715386));
#43186=CARTESIAN_POINT('Ctrl Pts',(133.388202975418,35.1062295286911,25.7692053134859));
#43187=CARTESIAN_POINT('Ctrl Pts',(133.389475774857,35.0509087774348,25.7659701546745));
#43188=CARTESIAN_POINT('Ctrl Pts',(133.389774240179,35.0238410326868,25.7643976741705));
#43189=CARTESIAN_POINT('Ctrl Pts',(133.389712560619,34.9590702896442,25.7606584272523));
#43190=CARTESIAN_POINT('Ctrl Pts',(133.389047667075,34.9213707692248,25.758501137612));
#43191=CARTESIAN_POINT('Ctrl Pts',(133.384367769555,34.785060766706,25.7507627341517));
#43192=CARTESIAN_POINT('Ctrl Pts',(133.376676014068,34.6866223889589,25.7452929607711));
#43193=CARTESIAN_POINT('Ctrl Pts',(133.344483636244,34.4232978212859,25.7308350784544));
#43194=CARTESIAN_POINT('Ctrl Pts',(133.312105683326,34.2596519708269,25.7220438641197));
#43195=CARTESIAN_POINT('Ctrl Pts',(133.221735544961,33.9318720038138,25.70400576397));
#43196=CARTESIAN_POINT('Ctrl Pts',(133.162888210715,33.768495518124,25.6947779792037));
#43197=CARTESIAN_POINT('Ctrl Pts',(133.077193733931,33.5778343586207,25.6829752559101));
#43198=CARTESIAN_POINT('Ctrl Pts',(133.062064917946,33.5455466266999,25.6809386802711));
#43199=CARTESIAN_POINT('Ctrl Pts',(133.038519091335,33.4972916953319,25.6778288643346));
#43200=CARTESIAN_POINT('Ctrl Pts',(133.030478800909,33.4811422967099,25.6767767829516));
#43201=CARTESIAN_POINT('Ctrl Pts',(133.015541542629,33.4517307391704,25.674838548748));
#43202=CARTESIAN_POINT('Ctrl Pts',(133.008685216209,33.4384489305471,25.6739548057915));
#43203=CARTESIAN_POINT('Ctrl Pts',(132.992541568739,33.4076771178906,25.6718877323408));
#43204=CARTESIAN_POINT('Ctrl Pts',(132.983188613403,33.3902227307331,25.6707005355786));
#43205=CARTESIAN_POINT('Ctrl Pts',(132.951917647127,33.3330736923022,25.6667672911804));
#43206=CARTESIAN_POINT('Ctrl Pts',(132.929356903163,33.2937383487556,25.6639862159263));
#43207=CARTESIAN_POINT('Ctrl Pts',(132.871535182112,33.197452829823,25.6570153590091));
#43208=CARTESIAN_POINT('Ctrl Pts',(132.835362746079,33.1410734830857,25.6527882195708));
#43209=CARTESIAN_POINT('Ctrl Pts',(132.639006079875,32.8541032393692,25.6306365285972));
#43210=CARTESIAN_POINT('Ctrl Pts',(132.452264181817,32.6429546375871,25.6122624390381));
#43211=CARTESIAN_POINT('Ctrl Pts',(132.181292258157,32.4040731323764,25.589875439973));
#43212=CARTESIAN_POINT('Ctrl Pts',(132.119091277369,32.353053460872,25.5849683325483));
#43213=CARTESIAN_POINT('Ctrl Pts',(132.029276026751,32.2845809144214,25.578198178467));
#43214=CARTESIAN_POINT('Ctrl Pts',(132.003138992895,32.2652429196206,25.5762635710107));
#43215=CARTESIAN_POINT('Ctrl Pts',(131.954830320327,32.2305650364201,25.5727512295535));
#43216=CARTESIAN_POINT('Ctrl Pts',(131.932746386482,32.2151080690904,25.5711691474748));
#43217=CARTESIAN_POINT('Ctrl Pts',(131.887386013099,32.1841589696634,25.5679661862652));
#43218=CARTESIAN_POINT('Ctrl Pts',(131.864097545566,32.1686880992406,25.5663461775516));
#43219=CARTESIAN_POINT('Ctrl Pts',(131.805001488225,32.1304749837513,25.5622945397053));
#43220=CARTESIAN_POINT('Ctrl Pts',(131.768952950445,32.1081130942001,25.5598768199138));
#43221=CARTESIAN_POINT('Ctrl Pts',(131.606607890169,32.0115779258518,25.5492113476853));
#43222=CARTESIAN_POINT('Ctrl Pts',(131.475997249499,31.9449560043203,25.5412291398559));
#43223=CARTESIAN_POINT('Ctrl Pts',(131.22132791832,31.8352126308915,25.5263711250156));
#43224=CARTESIAN_POINT('Ctrl Pts',(131.098283021394,31.7904368309098,25.5194787483502));
#43225=CARTESIAN_POINT('Ctrl Pts',(130.828997171191,31.7097485671671,25.5045305015377));
#43226=CARTESIAN_POINT('Ctrl Pts',(130.68233902518,31.6762377148937,25.4964703057189));
#43227=CARTESIAN_POINT('Ctrl Pts',(130.498456122186,31.6469060568909,25.4859596860316));
#43228=CARTESIAN_POINT('Ctrl Pts',(130.462868124912,31.6418084658141,25.4839067701749));
#43229=CARTESIAN_POINT('Ctrl Pts',(130.409253524055,31.634997153606,25.4807769658108));
#43230=CARTESIAN_POINT('Ctrl Pts',(130.391282202642,31.6328601441163,25.479721644142));
#43231=CARTESIAN_POINT('Ctrl Pts',(130.358443858445,31.6292217027729,25.4777805449679));
#43232=CARTESIAN_POINT('Ctrl Pts',(130.343582797286,31.6276745168874,25.4768972316233));
#43233=CARTESIAN_POINT('Ctrl Pts',(130.309079654235,31.6243128229454,25.4748352944844));
#43234=CARTESIAN_POINT('Ctrl Pts',(130.289431510769,31.6225714649622,25.4736528728346));
#43235=CARTESIAN_POINT('Ctrl Pts',(130.22502662722,31.6174295582927,25.4697525053143));
#43236=CARTESIAN_POINT('Ctrl Pts',(130.180219119405,31.614746621804,25.4670002959944));
#43237=CARTESIAN_POINT('Ctrl Pts',(130.069405707223,31.6103176152723,25.4601193795781));
#43238=CARTESIAN_POINT('Ctrl Pts',(130.003377710681,31.6096089405565,25.4559544395889));
#43239=CARTESIAN_POINT('Ctrl Pts',(129.66928852897,31.6157822573266,25.4346767409217));
#43240=CARTESIAN_POINT('Ctrl Pts',(129.402695369103,31.6525300271691,25.417131426605));
#43241=CARTESIAN_POINT('Ctrl Pts',(129.055215597889,31.7433052671798,25.3947593741147));
#43242=CARTESIAN_POINT('Ctrl Pts',(128.968168005087,31.769829234072,25.3891878459411));
#43243=CARTESIAN_POINT('Ctrl Pts',(128.846812310557,31.8122146970748,25.3814696405325));
#43244=CARTESIAN_POINT('Ctrl Pts',(128.811545657411,31.8251939538447,25.3792324901097));
#43245=CARTESIAN_POINT('Ctrl Pts',(128.75152771164,31.8484227609361,25.3754338206403));
#43246=CARTESIAN_POINT('Ctrl Pts',(128.726669315714,31.8583839861758,25.3738630281188));
#43247=CARTESIAN_POINT('Ctrl Pts',(128.67584405608,31.8794530011107,25.3706557048513));
#43248=CARTESIAN_POINT('Ctrl Pts',(128.64989269087,31.8905928442706,25.3690203893503));
#43249=CARTESIAN_POINT('Ctrl Pts',(128.584039948951,31.9198405991372,25.3648748877376));
#43250=CARTESIAN_POINT('Ctrl Pts',(128.544344296766,31.9384004961606,25.3623800196358));
#43251=CARTESIAN_POINT('Ctrl Pts',(128.353189201532,32.0323346100762,25.3503687049164));
#43252=CARTESIAN_POINT('Ctrl Pts',(128.207150797338,32.1182081988254,25.3412166055121));
#43253=CARTESIAN_POINT('Ctrl Pts',(127.879500123245,32.3454607097316,25.3199622793837));
#43254=CARTESIAN_POINT('Ctrl Pts',(127.704672406112,32.4950945088724,25.3080395430783));
#43255=CARTESIAN_POINT('Ctrl Pts',(127.509777659561,32.6995646204442,25.2923472407908));
#43256=CARTESIAN_POINT('Ctrl Pts',(127.474140499753,32.7387518038192,25.2893613295922));
#43257=CARTESIAN_POINT('Ctrl Pts',(127.425326040319,32.795023163629,25.285076797935));
#43258=CARTESIAN_POINT('Ctrl Pts',(127.411369829445,32.8114245190411,25.2838283451315));
#43259=CARTESIAN_POINT('Ctrl Pts',(127.387860111398,32.8395926419919,25.281682635137));
#43260=CARTESIAN_POINT('Ctrl Pts',(127.378227311552,32.8512927806164,25.2807908857807));
#43261=CARTESIAN_POINT('Ctrl Pts',(127.357941376522,32.8762718880977,25.2788853008936));
#43262=CARTESIAN_POINT('Ctrl Pts',(127.347309469444,32.8895669200587,25.2778701625419));
#43263=CARTESIAN_POINT('Ctrl Pts',(127.3178144485,32.9270249898117,25.2750089145093));
#43264=CARTESIAN_POINT('Ctrl Pts',(127.29917875787,32.9513640632801,25.2731484505139));
#43265=CARTESIAN_POINT('Ctrl Pts',(127.257364293247,33.0075379643608,25.2688578647804));
#43266=CARTESIAN_POINT('Ctrl Pts',(127.234405232973,33.0395304332064,25.2664166500125));
#43267=CARTESIAN_POINT('Ctrl Pts',(127.134668923196,33.1837480192524,25.2554472395178));
#43268=CARTESIAN_POINT('Ctrl Pts',(127.064131195399,33.3001282548846,25.2466936191634));
#43269=CARTESIAN_POINT('Ctrl Pts',(126.894262048728,33.622667376736,25.2231960739732));
#43270=CARTESIAN_POINT('Ctrl Pts',(126.808462737676,33.8351950907283,25.2085328572233));
#43271=CARTESIAN_POINT('Ctrl Pts',(126.729578014188,34.1068658890098,25.1912280096834));
#43272=CARTESIAN_POINT('Ctrl Pts',(126.715701777672,34.1593251541287,25.1879466538432));
#43273=CARTESIAN_POINT('Ctrl Pts',(126.695310049173,34.2446525507826,25.1827045223549));
#43274=CARTESIAN_POINT('Ctrl Pts',(126.688012340768,34.2773221286277,25.1807196649533));
#43275=CARTESIAN_POINT('Ctrl Pts',(126.675808923711,34.3360269163641,25.17719147766));
#43276=CARTESIAN_POINT('Ctrl Pts',(126.670722329536,34.36202130172,25.1756425926482));
#43277=CARTESIAN_POINT('Ctrl Pts',(126.661453128464,34.4125241800118,25.1726583184754));
#43278=CARTESIAN_POINT('Ctrl Pts',(126.657234468223,34.4370242459116,25.171221895726));
#43279=CARTESIAN_POINT('Ctrl Pts',(126.64856716605,34.4908974144687,25.1680870208185));
#43280=CARTESIAN_POINT('Ctrl Pts',(126.644234333626,34.5202872178922,25.1663922073998));
#43281=CARTESIAN_POINT('Ctrl Pts',(126.632668429241,34.6065869431955,25.1614574667667));
#43282=CARTESIAN_POINT('Ctrl Pts',(126.626492777579,34.6636292772607,25.158249059291));
#43283=CARTESIAN_POINT('Ctrl Pts',(126.614019374351,34.8145552517435,25.1498746786886));
#43284=CARTESIAN_POINT('Ctrl Pts',(126.610176989097,34.9085915285476,25.1447743661338));
#43285=CARTESIAN_POINT('Ctrl Pts',(126.610251050396,35.0026685497381,25.1397300250475));
#43286=CARTESIAN_POINT('Ctrl Pts',(126.610251047997,35.0026655008656,25.1397301885258));
#43287=CARTESIAN_POINT('Ctrl Pts',(126.610411758205,35.2070425715522,25.1287716367825));
#43288=CARTESIAN_POINT('Ctrl Pts',(126.629055404885,35.410984343521,25.1181316552081));
#43289=CARTESIAN_POINT('Ctrl Pts',(126.677916805914,35.6771690046066,25.1034765027583));
#43290=CARTESIAN_POINT('Ctrl Pts',(126.691785958565,35.7419660293238,25.0998446330445));
#43291=CARTESIAN_POINT('Ctrl Pts',(126.71824746432,35.8500177327797,25.0936194389212));
#43292=CARTESIAN_POINT('Ctrl Pts',(126.729819636648,35.8935042484559,25.0910672634323));
#43293=CARTESIAN_POINT('Ctrl Pts',(126.74770960057,35.9557206995766,25.0873315179809));
#43294=CARTESIAN_POINT('Ctrl Pts',(126.75333139516,35.9746475401143,25.0861837152293));
#43295=CARTESIAN_POINT('Ctrl Pts',(126.763497891763,36.0078107303777,25.0841508300451));
#43296=CARTESIAN_POINT('Ctrl Pts',(126.767971885647,36.0220678160657,25.0832697016655));
#43297=CARTESIAN_POINT('Ctrl Pts',(126.778068619525,36.0535132963877,25.0813100266379));
#43298=CARTESIAN_POINT('Ctrl Pts',(126.783734654622,36.0706863601936,25.0802291716339));
#43299=CARTESIAN_POINT('Ctrl Pts',(126.799688454388,36.1177708137905,25.0772380051815));
#43300=CARTESIAN_POINT('Ctrl Pts',(126.81025760997,36.1475839355275,25.0753131189722));
#43301=CARTESIAN_POINT('Ctrl Pts',(126.821241918346,36.177243441613,25.0733700900595));
#43302=CARTESIAN_POINT('Ctrl Pts',(126.821241938915,36.1772434971515,25.4139333020124));
#43303=CARTESIAN_POINT('Ctrl Pts',(126.78724614494,36.0854490600593,25.4191426080237));
#43304=CARTESIAN_POINT('Ctrl Pts',(126.75721423552,35.9921489540796,25.424315204267));
#43305=CARTESIAN_POINT('Ctrl Pts',(126.688840915227,35.743156357095,25.4380512485099));
#43306=CARTESIAN_POINT('Ctrl Pts',(126.65743459532,35.5859191685083,25.446654728435));
#43307=CARTESIAN_POINT('Ctrl Pts',(126.633676918287,35.3988522521441,25.4573909038189));
#43308=CARTESIAN_POINT('Ctrl Pts',(126.63044856704,35.3705903905907,25.4590263632019));
#43309=CARTESIAN_POINT('Ctrl Pts',(126.625904666717,35.3258217551147,25.4616429440096));
#43310=CARTESIAN_POINT('Ctrl Pts',(126.624353675026,35.3093396156075,25.4626118119845));
#43311=CARTESIAN_POINT('Ctrl Pts',(126.62161264969,35.2777304569417,25.4644816173911));
#43312=CARTESIAN_POINT('Ctrl Pts',(126.62040335581,35.2626057591035,25.4653815253128));
#43313=CARTESIAN_POINT('Ctrl Pts',(126.617650048713,35.2249932407246,25.4676316781336));
#43314=CARTESIAN_POINT('Ctrl Pts',(126.616228744797,35.202497367276,25.4689883103746));
#43315=CARTESIAN_POINT('Ctrl Pts',(126.611870211821,35.1205288024494,25.4739668504102));
#43316=CARTESIAN_POINT('Ctrl Pts',(126.610275975868,35.0609985004644,25.4776501540227));
#43317=CARTESIAN_POINT('Ctrl Pts',(126.610205881451,34.8983686986595,25.4878439336558));
#43318=CARTESIAN_POINT('Ctrl Pts',(126.614864496924,34.7953329491614,25.494445207943));
#43319=CARTESIAN_POINT('Ctrl Pts',(126.648420604002,34.426737769577,25.5182664324351));
#43320=CARTESIAN_POINT('Ctrl Pts',(126.703976256081,34.1645450672507,25.5355023094875));
#43321=CARTESIAN_POINT('Ctrl Pts',(126.806981197994,33.8607384048183,25.5550453529368));
#43322=CARTESIAN_POINT('Ctrl Pts',(126.825421485116,33.810320296512,25.5582779957451));
#43323=CARTESIAN_POINT('Ctrl Pts',(126.856231288907,33.731907809254,25.5632908257431));
#43324=CARTESIAN_POINT('Ctrl Pts',(126.867794988551,33.7036083265279,25.5650969549421));
#43325=CARTESIAN_POINT('Ctrl Pts',(126.89007157606,33.6511303474066,25.5684415969058));
#43326=CARTESIAN_POINT('Ctrl Pts',(126.900687553983,33.6269134906624,25.5699831842844));
#43327=CARTESIAN_POINT('Ctrl Pts',(126.925135318675,33.5728725153561,25.5734202769261));
#43328=CARTESIAN_POINT('Ctrl Pts',(126.939119898247,33.5431201912837,25.5753104667458));
#43329=CARTESIAN_POINT('Ctrl Pts',(126.983029030392,33.4531273314043,25.581025207538));
#43330=CARTESIAN_POINT('Ctrl Pts',(127.014316419729,33.3935681546972,25.5848034347772));
#43331=CARTESIAN_POINT('Ctrl Pts',(127.16968743093,33.1180434245127,25.6023333111695));
#43332=CARTESIAN_POINT('Ctrl Pts',(127.315548531494,32.9152565506276,25.61532180848));
#43333=CARTESIAN_POINT('Ctrl Pts',(127.581383438689,32.620380279568,25.6364865904468));
#43334=CARTESIAN_POINT('Ctrl Pts',(127.687531554942,32.5171031700493,25.6444715927467));
#43335=CARTESIAN_POINT('Ctrl Pts',(127.821605590945,32.4027314406696,25.6545069939703));
#43336=CARTESIAN_POINT('Ctrl Pts',(127.843367457853,32.3846334601348,25.6561345442673));
#43337=CARTESIAN_POINT('Ctrl Pts',(127.878189226834,32.3564044989029,25.6587413672163));
#43338=CARTESIAN_POINT('Ctrl Pts',(127.891101451538,32.3460925001281,25.6597085409375));
#43339=CARTESIAN_POINT('Ctrl Pts',(127.916165700065,32.3263740320514,25.6615881019812));
#43340=CARTESIAN_POINT('Ctrl Pts',(127.928307110233,32.3169551359925,25.6624996291));
#43341=CARTESIAN_POINT('Ctrl Pts',(127.958599424219,32.2937835737672,25.6647756590725));
#43342=CARTESIAN_POINT('Ctrl Pts',(127.976825522163,32.2801307702699,25.6661466459358));
#43343=CARTESIAN_POINT('Ctrl Pts',(128.048605097628,32.2274828122752,25.6715475648451));
#43344=CARTESIAN_POINT('Ctrl Pts',(128.103156590736,32.1898794462459,25.6756553895023));
#43345=CARTESIAN_POINT('Ctrl Pts',(128.258751584076,32.0892202447363,25.687306516073));
#43346=CARTESIAN_POINT('Ctrl Pts',(128.362066891044,32.0298556554298,25.6949661579377));
#43347=CARTESIAN_POINT('Ctrl Pts',(128.690371120084,31.8635603569447,25.7186854876994));
#43348=CARTESIAN_POINT('Ctrl Pts',(128.924208690513,31.7758580474907,25.7346583254899));
#43349=CARTESIAN_POINT('Ctrl Pts',(129.215397055654,31.7019026503466,25.7529212870196));
#43350=CARTESIAN_POINT('Ctrl Pts',(129.2655070823,31.6903824246386,25.7560118907501));
#43351=CARTESIAN_POINT('Ctrl Pts',(129.345050879154,31.6739911476349,25.7608378746362));
#43352=CARTESIAN_POINT('Ctrl Pts',(129.374318569061,31.6683613538053,25.7625966722292));
#43353=CARTESIAN_POINT('Ctrl Pts',(129.429784426982,31.6584489102964,25.7658989883642));
#43354=CARTESIAN_POINT('Ctrl Pts',(129.455965899989,31.654086605747,25.7674448818136));
#43355=CARTESIAN_POINT('Ctrl Pts',(129.515836767469,31.6448323836095,25.7709518161791));
#43356=CARTESIAN_POINT('Ctrl Pts',(129.549554307204,31.6401395017706,25.7729065542013));
#43357=CARTESIAN_POINT('Ctrl Pts',(129.656724476378,31.6268656692521,25.7790600552336));
#43358=CARTESIAN_POINT('Ctrl Pts',(129.730392212804,31.6201795876266,25.7832009591173));
#43359=CARTESIAN_POINT('Ctrl Pts',(129.909322388081,31.6098281225146,25.793093700157));
#43360=CARTESIAN_POINT('Ctrl Pts',(130.014651704467,31.6086470070153,25.7987783263936));
#43361=CARTESIAN_POINT('Ctrl Pts',(130.243975894216,31.6167615507051,25.8110391674679));
#43362=CARTESIAN_POINT('Ctrl Pts',(130.367746273111,31.6279695479897,25.8175819437801));
#43363=CARTESIAN_POINT('Ctrl Pts',(130.633803766805,31.6668877327694,25.8318930272458));
#43364=CARTESIAN_POINT('Ctrl Pts',(130.775484295209,31.6969770022114,25.8396704604642));
#43365=CARTESIAN_POINT('Ctrl Pts',(130.949123581928,31.7456428349665,25.8498525113236));
#43366=CARTESIAN_POINT('Ctrl Pts',(130.983297479166,31.7558048782406,25.8518888877336));
#43367=CARTESIAN_POINT('Ctrl Pts',(131.034511431215,31.7719175054613,25.8549984614742));
#43368=CARTESIAN_POINT('Ctrl Pts',(131.051675652803,31.7774685754146,25.856050504868));
#43369=CARTESIAN_POINT('Ctrl Pts',(131.082979776073,31.7878693508187,25.8579887083869));
#43370=CARTESIAN_POINT('Ctrl Pts',(131.097133066253,31.7926759578876,25.8588724593206));
#43371=CARTESIAN_POINT('Ctrl Pts',(131.129963235379,31.8040681594395,25.8609396042834));
#43372=CARTESIAN_POINT('Ctrl Pts',(131.148614640574,31.8107239679616,25.8621268654764));
#43373=CARTESIAN_POINT('Ctrl Pts',(131.209782591993,31.8331580813246,25.8660605443639));
#43374=CARTESIAN_POINT('Ctrl Pts',(131.252039247815,31.8496255845609,25.8688419997517));
#43375=CARTESIAN_POINT('Ctrl Pts',(131.355864826834,31.8925053731902,25.8758140411302));
#43376=CARTESIAN_POINT('Ctrl Pts',(131.417004491463,31.9199042791809,25.8800419997484));
#43377=CARTESIAN_POINT('Ctrl Pts',(131.730132241768,32.0715249194986,25.9022057181325));
#43378=CARTESIAN_POINT('Ctrl Pts',(131.966819487439,32.2249357559728,25.9205912344941));
#43379=CARTESIAN_POINT('Ctrl Pts',(132.243507293534,32.457645169772,25.9429954439113));
#43380=CARTESIAN_POINT('Ctrl Pts',(132.303287253762,32.5116747601661,25.9479099168073));
#43381=CARTESIAN_POINT('Ctrl Pts',(132.384334489616,32.590351967441,25.9546800141562));
#43382=CARTESIAN_POINT('Ctrl Pts',(132.407255554415,32.6132500331549,25.9566075982063));
#43383=CARTESIAN_POINT('Ctrl Pts',(132.448620379695,32.6557755324814,25.9601112378114));
#43384=CARTESIAN_POINT('Ctrl Pts',(132.467165044618,32.6753007026878,25.9616915620214));
#43385=CARTESIAN_POINT('Ctrl Pts',(132.504513233249,32.7155739469466,25.9648949990808));
#43386=CARTESIAN_POINT('Ctrl Pts',(132.523296304224,32.7363381973103,25.9665171906052));
#43387=CARTESIAN_POINT('Ctrl Pts',(132.570016032277,32.789289959578,25.9705823052299));
#43388=CARTESIAN_POINT('Ctrl Pts',(132.597607346055,32.8217765052163,25.9730111193099));
#43389=CARTESIAN_POINT('Ctrl Pts',(132.719063148581,32.9703718918971,25.9838461330538));
#43390=CARTESIAN_POINT('Ctrl Pts',(132.805811734546,33.0920896922729,25.9919753845479));
#43391=CARTESIAN_POINT('Ctrl Pts',(132.951925418626,33.3287338390268,26.0068656823502));
#43392=CARTESIAN_POINT('Ctrl Pts',(133.013290750971,33.4420932688901,26.0136513860237));
#43393=CARTESIAN_POINT('Ctrl Pts',(133.131482263418,33.6936791587142,26.0284347397644));
#43394=CARTESIAN_POINT('Ctrl Pts',(133.185921183258,33.8327154831244,26.0364383115737));
#43395=CARTESIAN_POINT('Ctrl Pts',(133.241874225197,34.0090691483376,26.0468825065732));
#43396=CARTESIAN_POINT('Ctrl Pts',(133.252180978407,34.0434378672002,26.0489315242536));
#43397=CARTESIAN_POINT('Ctrl Pts',(133.266858912297,34.0953647398473,26.052056562586));
#43398=CARTESIAN_POINT('Ctrl Pts',(133.271638534392,34.1128058977298,26.0531111140671));
#43399=CARTESIAN_POINT('Ctrl Pts',(133.280112330254,34.1447272539749,26.0550515320572));
#43400=CARTESIAN_POINT('Ctrl Pts',(133.283850635073,34.1591948207184,26.0559349473256));
#43401=CARTESIAN_POINT('Ctrl Pts',(133.292306025392,34.192834646471,26.0579981028226));
#43402=CARTESIAN_POINT('Ctrl Pts',(133.296951381128,34.2120238443578,26.0591816571156));
#43403=CARTESIAN_POINT('Ctrl Pts',(133.311632672507,34.2750734231234,26.0630897934203));
#43404=CARTESIAN_POINT('Ctrl Pts',(133.320962611913,34.3190914771046,26.0658488186212));
#43405=CARTESIAN_POINT('Ctrl Pts',(133.341856562497,34.4283460588573,26.0727509315481));
#43406=CARTESIAN_POINT('Ctrl Pts',(133.352389240764,34.4937599307751,26.0769305157319));
#43407=CARTESIAN_POINT('Ctrl Pts',(133.396219226552,34.8281330854671,26.098407060591));
#43408=CARTESIAN_POINT('Ctrl Pts',(133.399095152849,35.1001269397107,26.1161406110915));
#43409=CARTESIAN_POINT('Ctrl Pts',(133.359869795336,35.4577713463583,26.1385272932438));
#43410=CARTESIAN_POINT('Ctrl Pts',(133.346734566545,35.5455726577009,26.1439580288845));
#43411=CARTESIAN_POINT('Ctrl Pts',(133.323231154039,35.6692686246362,26.15151456168));
#43412=CARTESIAN_POINT('Ctrl Pts',(133.315694867736,35.7056582062518,26.1537260469566));
#43413=CARTESIAN_POINT('Ctrl Pts',(133.301657185491,35.7682399477624,26.1575107106607));
#43414=CARTESIAN_POINT('Ctrl Pts',(133.295438710376,35.7944913823401,26.1590925960401));
#43415=CARTESIAN_POINT('Ctrl Pts',(133.282022805055,35.848257043926,26.1623217419977));
#43416=CARTESIAN_POINT('Ctrl Pts',(133.274791165663,35.8757605827778,26.1639677778107));
#43417=CARTESIAN_POINT('Ctrl Pts',(133.255282939054,35.9463314819004,26.1681781856861));
#43418=CARTESIAN_POINT('Ctrl Pts',(133.24249730694,35.9892531347847,26.1707262411519));
#43419=CARTESIAN_POINT('Ctrl Pts',(133.170354094127,36.214990446809,26.184079251524));
#43420=CARTESIAN_POINT('Ctrl Pts',(133.096376796749,36.3927700589008,26.19440126684));
#43421=CARTESIAN_POINT('Ctrl Pts',(132.914834846855,36.742040773895,26.2153105494072));
#43422=CARTESIAN_POINT('Ctrl Pts',(132.806214736876,36.9120967792971,26.2258502858973));
#43423=CARTESIAN_POINT('Ctrl Pts',(132.649393039,37.1152243554,26.2400812804722));
#43424=CARTESIAN_POINT('Ctrl Pts',(132.614567679247,37.1581224950231,26.2431916057995));
#43425=CARTESIAN_POINT('Ctrl Pts',(132.564499063996,37.2168060593527,26.2476256048923));
#43426=CARTESIAN_POINT('Ctrl Pts',(132.55012574811,37.2333255849865,26.2488943656532));
#43427=CARTESIAN_POINT('Ctrl Pts',(132.525497139745,37.2610839658848,26.2510637652774));
#43428=CARTESIAN_POINT('Ctrl Pts',(132.515324144737,37.2723954200347,26.2519585752976));
#43429=CARTESIAN_POINT('Ctrl Pts',(132.49371508611,37.2960998415725,26.2538573993943));
#43430=CARTESIAN_POINT('Ctrl Pts',(132.482262300063,37.3084763936837,26.2548625510395));
#43431=CARTESIAN_POINT('Ctrl Pts',(132.450253642737,37.3425532199807,26.2576671177802));
#43432=CARTESIAN_POINT('Ctrl Pts',(132.429502839985,37.3640673256111,26.2594800297852));
#43433=CARTESIAN_POINT('Ctrl Pts',(132.381665254242,37.4123695417553,26.2636418140288));
#43434=CARTESIAN_POINT('Ctrl Pts',(132.354406133022,37.4389808782852,26.2660009032943));
#43435=CARTESIAN_POINT('Ctrl Pts',(132.261683280735,37.5264971981452,26.2739676947997));
#43436=CARTESIAN_POINT('Ctrl Pts',(132.194261612193,37.5852685887009,26.2796662504711));
#43437=CARTESIAN_POINT('Ctrl Pts',(131.894836912965,37.8261185135034,26.3043348915966));
#43438=CARTESIAN_POINT('Ctrl Pts',(131.641889943307,37.9802028589468,26.3234608454401));
#43439=CARTESIAN_POINT('Ctrl Pts',(131.326104938872,38.1199981527272,26.3444371791626));
#43440=CARTESIAN_POINT('Ctrl Pts',(131.279590474274,38.1393616242839,26.3474638417174));
#43441=CARTESIAN_POINT('Ctrl Pts',(131.205095240521,38.1684422212339,26.3522140059146));
#43442=CARTESIAN_POINT('Ctrl Pts',(131.177390408656,38.178841385905,26.3539596947402));
#43443=CARTESIAN_POINT('Ctrl Pts',(131.124544550547,38.1978916919145,26.3572510773682));
#43444=CARTESIAN_POINT('Ctrl Pts',(131.099431131877,38.2066123814533,26.3587989449796));
#43445=CARTESIAN_POINT('Ctrl Pts',(131.041571751205,38.2259445205204,26.3623291770914));
#43446=CARTESIAN_POINT('Ctrl Pts',(131.008761267519,38.2363545218863,26.3643049165404));
#43447=CARTESIAN_POINT('Ctrl Pts',(130.902797165338,38.2682063615257,26.3706068726379));
#43448=CARTESIAN_POINT('Ctrl Pts',(130.829074669472,38.2876818444433,26.3748710192081));
#43449=CARTESIAN_POINT('Ctrl Pts',(130.647451032434,38.3291630761976,26.3851405980968));
#43450=CARTESIAN_POINT('Ctrl Pts',(130.539013511112,38.3484304156418,26.3910711980922));
#43451=CARTESIAN_POINT('Ctrl Pts',(130.21919651251,38.3893137478553,26.4082716381633));
#43452=CARTESIAN_POINT('Ctrl Pts',(130.006518337483,38.3963864385934,26.4193233749639));
#43453=CARTESIAN_POINT('Ctrl Pts',(129.7249755408,38.3792944430617,26.4348116122454));
#43454=CARTESIAN_POINT('Ctrl Pts',(129.655510574254,38.3729208588594,26.4387057544104));
#43455=CARTESIAN_POINT('Ctrl Pts',(129.562606193132,38.361496904243,26.4440690797105));
#43456=CARTESIAN_POINT('Ctrl Pts',(129.538948023096,38.3583337810692,26.4454484618425));
#43457=CARTESIAN_POINT('Ctrl Pts',(129.501432476822,38.3529140377692,26.4476602002746));
#43458=CARTESIAN_POINT('Ctrl Pts',(129.487551875624,38.3508206493504,26.4484838590039));
#43459=CARTESIAN_POINT('Ctrl Pts',(129.458127069433,38.3461958724362,26.4502419541585));
#43460=CARTESIAN_POINT('Ctrl Pts',(129.442586827947,38.3436422684019,26.4511776476971));
#43461=CARTESIAN_POINT('Ctrl Pts',(129.402728566306,38.3368070956997,26.4535950378974));
#43462=CARTESIAN_POINT('Ctrl Pts',(129.378438869474,38.3323679933103,26.4550849553129));
#43463=CARTESIAN_POINT('Ctrl Pts',(129.270951786874,38.3115079878682,26.4617461553046));
#43464=CARTESIAN_POINT('Ctrl Pts',(129.188344702409,38.2922347877404,26.4670461697472));
#43465=CARTESIAN_POINT('Ctrl Pts',(128.924599016786,38.2201703551241,26.4843793302038));
#43466=CARTESIAN_POINT('Ctrl Pts',(128.747112982166,38.1553540329263,26.4966611666724));
#43467=CARTESIAN_POINT('Ctrl Pts',(128.421636549016,38.0046773507659,26.5195942091316));
#43468=CARTESIAN_POINT('Ctrl Pts',(128.272911156707,37.9217280443934,26.5302566622879));
#43469=CARTESIAN_POINT('Ctrl Pts',(128.093959684016,37.803460196987,26.5432216317841));
#43470=CARTESIAN_POINT('Ctrl Pts',(128.057380166286,37.7782381512113,26.5458806918995));
#43471=CARTESIAN_POINT('Ctrl Pts',(127.998275293459,37.7357462962776,26.5501937125388));
#43472=CARTESIAN_POINT('Ctrl Pts',(127.975453123062,37.718900442189,26.5518632917375));
#43473=CARTESIAN_POINT('Ctrl Pts',(127.931313403305,37.6854553758177,26.5551016323908));
#43474=CARTESIAN_POINT('Ctrl Pts',(127.909977604473,37.6688838976175,26.5566712888612));
#43475=CARTESIAN_POINT('Ctrl Pts',(127.859594084819,37.6287763458617,26.5603898069537));
#43476=CARTESIAN_POINT('Ctrl Pts',(127.830732824561,37.6050110627055,26.5625294756689));
#43477=CARTESIAN_POINT('Ctrl Pts',(127.728993602701,37.518372134899,26.5701139594879));
#43478=CARTESIAN_POINT('Ctrl Pts',(127.658404608437,37.4528761678907,26.5754534819271));
#43479=CARTESIAN_POINT('Ctrl Pts',(127.478579338137,37.2711771729287,26.5894012819383));
#43480=CARTESIAN_POINT('Ctrl Pts',(127.374589810402,37.150123819047,26.5978315907567));
#43481=CARTESIAN_POINT('Ctrl Pts',(127.169380576106,36.8740526380048,26.616071228891));
#43482=CARTESIAN_POINT('Ctrl Pts',(127.071555795253,36.7171720423548,26.6258582397219));
#43483=CARTESIAN_POINT('Ctrl Pts',(126.971064171271,36.522222677682,26.6382482074251));
#43484=CARTESIAN_POINT('Ctrl Pts',(126.955609467031,36.4910735132362,26.6402348019939));
#43485=CARTESIAN_POINT('Ctrl Pts',(126.932850421994,36.4433729667018,26.6432955881083));
#43486=CARTESIAN_POINT('Ctrl Pts',(126.92519446344,36.4269908672716,26.6443500590425));
#43487=CARTESIAN_POINT('Ctrl Pts',(126.911451779634,36.3969603658288,26.6462904054207));
#43488=CARTESIAN_POINT('Ctrl Pts',(126.905323713077,36.3833318568459,26.6471738309701));
#43489=CARTESIAN_POINT('Ctrl Pts',(126.891307580864,36.3516014172279,26.6492371126788));
#43490=CARTESIAN_POINT('Ctrl Pts',(126.88348738244,36.3334706637344,26.65042078459));
#43491=CARTESIAN_POINT('Ctrl Pts',(126.85836361659,36.2737940769975,26.6543297314844));
#43492=CARTESIAN_POINT('Ctrl Pts',(126.841729660886,36.2319734444147,26.6570894684764));
#43493=CARTESIAN_POINT('Ctrl Pts',(126.824361661966,36.1856417146286,26.6601597368587));
#43494=CARTESIAN_POINT('Ctrl Pts',(126.822797614578,36.1814440867763,26.6604380167156));
#43495=CARTESIAN_POINT('Ctrl Pts',(126.821241918426,36.1772434418289,26.660716603687));
#43496=CARTESIAN_POINT('Origin',(130.,35.,23.));
#43497=CARTESIAN_POINT('',(126.821241918358,36.1772434416438,27.913420165303));
#43498=CARTESIAN_POINT('',(126.821241849407,36.1772432554656,27.5681926079129));
#43499=CARTESIAN_POINT('',(126.821241918358,36.1772434416438,23.));
#43500=CARTESIAN_POINT('Ctrl Pts',(126.821241849407,36.1772432554656,27.5681926079129));
#43501=CARTESIAN_POINT('Ctrl Pts',(126.84174973112,36.2326180438488,27.5645149152729));
#43502=CARTESIAN_POINT('Ctrl Pts',(126.863708823237,36.2874684205701,27.560875143329));
#43503=CARTESIAN_POINT('Ctrl Pts',(126.908094792219,36.3904461959036,27.5540501120195));
#43504=CARTESIAN_POINT('Ctrl Pts',(126.930230872951,36.4386578534972,27.5508583571272));
#43505=CARTESIAN_POINT('Ctrl Pts',(126.966703979077,36.513416152388,27.545912642408));
#43506=CARTESIAN_POINT('Ctrl Pts',(126.980278559587,36.5403232488672,27.5441332650874));
#43507=CARTESIAN_POINT('Ctrl Pts',(127.006455704018,36.5905342607911,27.5408130429875));
#43508=CARTESIAN_POINT('Ctrl Pts',(127.018976054374,36.6138782423286,27.5392695146579));
#43509=CARTESIAN_POINT('Ctrl Pts',(127.047946222346,36.6664049900041,27.5357954366995));
#43510=CARTESIAN_POINT('Ctrl Pts',(127.064557704424,36.6954957212301,27.5338707303769));
#43511=CARTESIAN_POINT('Ctrl Pts',(127.117602918107,36.7852736030098,27.5279244917695));
#43512=CARTESIAN_POINT('Ctrl Pts',(127.155509017487,36.8450709425282,27.5239552016483));
#43513=CARTESIAN_POINT('Ctrl Pts',(127.334377706038,37.1086080224966,27.5063419690037));
#43514=CARTESIAN_POINT('Ctrl Pts',(127.495538001034,37.2977041148758,27.493434436482));
#43515=CARTESIAN_POINT('Ctrl Pts',(127.772738451284,37.5587924450687,27.4731179030451));
#43516=CARTESIAN_POINT('Ctrl Pts',(127.874886671473,37.644238972395,27.4659315126575));
#43517=CARTESIAN_POINT('Ctrl Pts',(128.009569288014,37.7440457123043,27.4564556370403));
#43518=CARTESIAN_POINT('Ctrl Pts',(128.037669831768,37.7642108109722,27.4544783598304));
#43519=CARTESIAN_POINT('Ctrl Pts',(128.080715429515,37.7941133962775,27.451441159174));
#43520=CARTESIAN_POINT('Ctrl Pts',(128.095437694628,37.8041692759178,27.4504009441274));
#43521=CARTESIAN_POINT('Ctrl Pts',(128.122668895766,37.8224558793165,27.4484729153796));
#43522=CARTESIAN_POINT('Ctrl Pts',(128.135154008266,37.8307205203255,27.4475873106595));
#43523=CARTESIAN_POINT('Ctrl Pts',(128.164237610395,37.8496967816733,27.4455208008625));
#43524=CARTESIAN_POINT('Ctrl Pts',(128.180875448037,37.8603463289733,27.4443360901591));
#43525=CARTESIAN_POINT('Ctrl Pts',(128.235281704718,37.8945040111036,27.4404563256271));
#43526=CARTESIAN_POINT('Ctrl Pts',(128.273418600079,37.9174133068107,27.4377279023964));
#43527=CARTESIAN_POINT('Ctrl Pts',(128.495145996398,38.044737393464,27.4218620742426));
#43528=CARTESIAN_POINT('Ctrl Pts',(128.687718191046,38.13255820633,27.408103943716));
#43529=CARTESIAN_POINT('Ctrl Pts',(128.933002366131,38.2178055231709,27.3914238318584));
#43530=CARTESIAN_POINT('Ctrl Pts',(128.979142033192,38.2327396305289,27.388319323848));
#43531=CARTESIAN_POINT('Ctrl Pts',(129.172328257359,38.2907198498557,27.3754769024027));
#43532=CARTESIAN_POINT('Ctrl Pts',(129.321900194696,38.3247659190711,27.3659172352249));
#43533=CARTESIAN_POINT('Ctrl Pts',(129.515640425054,38.355240633082,27.3540795555603));
#43534=CARTESIAN_POINT('Ctrl Pts',(129.558125279094,38.361099654519,27.3515157407274));
#43535=CARTESIAN_POINT('Ctrl Pts',(129.628566802088,38.3694553393505,27.3473159959942));
#43536=CARTESIAN_POINT('Ctrl Pts',(129.656462760342,38.3724136964487,27.3456660127627));
#43537=CARTESIAN_POINT('Ctrl Pts',(129.711167767749,38.3775292993976,27.342455137609));
#43538=CARTESIAN_POINT('Ctrl Pts',(129.737972055596,38.3797144323193,27.3408934994096));
#43539=CARTESIAN_POINT('Ctrl Pts',(129.796972160738,38.3838180814644,27.3374803530737));
#43540=CARTESIAN_POINT('Ctrl Pts',(129.829175272596,38.3855965686326,27.3356332552991));
#43541=CARTESIAN_POINT('Ctrl Pts',(129.94093078705,38.3901698603592,27.3292736917755));
#43542=CARTESIAN_POINT('Ctrl Pts',(130.020555456256,38.3906223087319,27.3248318949768));
#43543=CARTESIAN_POINT('Ctrl Pts',(130.33685043225,38.3812754888362,27.3074366036708));
#43544=CARTESIAN_POINT('Ctrl Pts',(130.572183542738,38.3494925762648,27.2950988421214));
#43545=CARTESIAN_POINT('Ctrl Pts',(130.928065421479,38.2627992155865,27.2755386718988));
#43546=CARTESIAN_POINT('Ctrl Pts',(131.051974902345,38.2249817013313,27.2685364923311));
#43547=CARTESIAN_POINT('Ctrl Pts',(131.205466811719,38.1683469882307,27.2592840484598));
#43548=CARTESIAN_POINT('Ctrl Pts',(131.237345259842,38.1560338072496,27.2573297118351));
#43549=CARTESIAN_POINT('Ctrl Pts',(131.285486515758,38.1365975849077,27.2543206405524));
#43550=CARTESIAN_POINT('Ctrl Pts',(131.301889403412,38.1298249060935,27.2532850659268));
#43551=CARTESIAN_POINT('Ctrl Pts',(131.332043859615,38.1170962101829,27.2513609024119));
#43552=CARTESIAN_POINT('Ctrl Pts',(131.345810180136,38.1111773586945,27.2504744430772));
#43553=CARTESIAN_POINT('Ctrl Pts',(131.377742144528,38.0971965742605,27.248399785386));
#43554=CARTESIAN_POINT('Ctrl Pts',(131.395876669298,38.0890659297726,27.247207677887));
#43555=CARTESIAN_POINT('Ctrl Pts',(131.45498571281,38.061937531507,27.2432789150226));
#43556=CARTESIAN_POINT('Ctrl Pts',(131.495650617758,38.042281000395,27.2405077789005));
#43557=CARTESIAN_POINT('Ctrl Pts',(131.723618261122,37.926411238217,27.2246313732063));
#43558=CARTESIAN_POINT('Ctrl Pts',(131.902021006087,37.8137256473614,27.2109148855617));
#43559=CARTESIAN_POINT('Ctrl Pts',(132.198835336501,37.5850474743562,27.1868480067767));
#43560=CARTESIAN_POINT('Ctrl Pts',(132.321425233059,37.4755490232633,27.1764468694824));
#43561=CARTESIAN_POINT('Ctrl Pts',(132.479909235462,37.3118201369169,27.1624757311334));
#43562=CARTESIAN_POINT('Ctrl Pts',(132.522912922333,37.2648119928417,27.1586216003407));
#43563=CARTESIAN_POINT('Ctrl Pts',(132.585636553301,37.1922423855049,27.1528999137642));
#43564=CARTESIAN_POINT('Ctrl Pts',(132.606356417777,37.1675676214481,27.1509921928415));
#43565=CARTESIAN_POINT('Ctrl Pts',(132.64179178201,37.1241256241629,27.1476972723839));
#43566=CARTESIAN_POINT('Ctrl Pts',(132.656666605396,37.1054918849347,27.1463038006724));
#43567=CARTESIAN_POINT('Ctrl Pts',(132.68987902583,37.062974180349,27.14316791993));
#43568=CARTESIAN_POINT('Ctrl Pts',(132.708097606682,37.0389995290249,27.1414302166747));
#43569=CARTESIAN_POINT('Ctrl Pts',(132.756619633286,36.9733494435621,27.1367513058747));
#43570=CARTESIAN_POINT('Ctrl Pts',(132.786296829381,36.9312198733415,27.1338337838781));
#43571=CARTESIAN_POINT('Ctrl Pts',(132.949650735728,36.6877148789652,27.1174122987796));
#43572=CARTESIAN_POINT('Ctrl Pts',(133.062447115473,36.4731767677177,27.1046881559627));
#43573=CARTESIAN_POINT('Ctrl Pts',(133.21675677284,36.0836520442633,27.082451282347));
#43574=CARTESIAN_POINT('Ctrl Pts',(133.269007399097,35.9140035793927,27.072999501741));
#43575=CARTESIAN_POINT('Ctrl Pts',(133.314309057919,35.7118007230369,27.0612244768151));
#43576=CARTESIAN_POINT('Ctrl Pts',(133.320477697972,35.6824459887214,27.0595025402855));
#43577=CARTESIAN_POINT('Ctrl Pts',(133.329508525208,35.6364457110599,27.0567793039032));
#43578=CARTESIAN_POINT('Ctrl Pts',(133.332637380287,35.6198533920223,27.0557919994136));
#43579=CARTESIAN_POINT('Ctrl Pts',(133.33834797022,35.5882763702048,27.0539023255508));
#43580=CARTESIAN_POINT('Ctrl Pts',(133.340953034992,35.5732966434007,27.0530012148235));
#43581=CARTESIAN_POINT('Ctrl Pts',(133.346487347797,35.5401536598437,27.0509977372896));
#43582=CARTESIAN_POINT('Ctrl Pts',(133.349369667537,35.5219830861987,27.0498929230021));
#43583=CARTESIAN_POINT('Ctrl Pts',(133.358808397105,35.4591799805184,27.0460543286177));
#43584=CARTESIAN_POINT('Ctrl Pts',(133.364621407311,35.414442367759,27.0432851332842));
#43585=CARTESIAN_POINT('Ctrl Pts',(133.392445744273,35.160778735379,27.0274360881326));
#43586=CARTESIAN_POINT('Ctrl Pts',(133.395888667287,34.9502857097828,27.0137514169556));
#43587=CARTESIAN_POINT('Ctrl Pts',(133.364771354037,34.5444732602922,26.9876098975294));
#43588=CARTESIAN_POINT('Ctrl Pts',(133.332628556801,34.3497707699144,26.9751797635475));
#43589=CARTESIAN_POINT('Ctrl Pts',(133.27260388089,34.1154168988314,26.9605512346294));
#43590=CARTESIAN_POINT('Ctrl Pts',(133.260592348471,34.0721200230522,26.9578613367002));
#43591=CARTESIAN_POINT('Ctrl Pts',(133.239569500702,34.0017991874978,26.9535116197802));
#43592=CARTESIAN_POINT('Ctrl Pts',(133.23107237707,33.9746284673449,26.9518356634807));
#43593=CARTESIAN_POINT('Ctrl Pts',(133.21386297266,33.9219384204237,26.9485937975823));
#43594=CARTESIAN_POINT('Ctrl Pts',(133.205186507776,33.8964097280512,26.9470268753813));
#43595=CARTESIAN_POINT('Ctrl Pts',(133.183860361694,33.8360359828586,26.943328843921));
#43596=CARTESIAN_POINT('Ctrl Pts',(133.170941748151,33.8012891845922,26.9412066479099));
#43597=CARTESIAN_POINT('Ctrl Pts',(133.125432144514,33.6847712507651,26.93410440991));
#43598=CARTESIAN_POINT('Ctrl Pts',(133.090226025618,33.6040567386323,26.9292094912048));
#43599=CARTESIAN_POINT('Ctrl Pts',(132.933596450339,33.2800192882011,26.9095095461876));
#43600=CARTESIAN_POINT('Ctrl Pts',(132.786268353647,33.0503792664814,26.8955158725032));
#43601=CARTESIAN_POINT('Ctrl Pts',(132.570862613999,32.7896906343086,26.8772041577259));
#43602=CARTESIAN_POINT('Ctrl Pts',(132.527135925704,32.739826288371,26.8735693367992));
#43603=CARTESIAN_POINT('Ctrl Pts',(132.451311606521,32.6583117844775,26.8673396245334));
#43604=CARTESIAN_POINT('Ctrl Pts',(132.419993456021,32.625960496851,26.8647859598575));
#43605=CARTESIAN_POINT('Ctrl Pts',(132.374025847732,32.5803313547091,26.8610484204164));
#43606=CARTESIAN_POINT('Ctrl Pts',(132.359888859941,32.5665416365412,26.859900360259));
#43607=CARTESIAN_POINT('Ctrl Pts',(132.334844466412,32.5425359224136,26.8578671991929));
#43608=CARTESIAN_POINT('Ctrl Pts',(132.323988747155,32.5322673026014,26.8569860563863));
#43609=CARTESIAN_POINT('Ctrl Pts',(132.299848281481,32.5097329773295,26.8550265762205));
#43610=CARTESIAN_POINT('Ctrl Pts',(132.286533243774,32.4975017173244,26.8539459337305));
#43611=CARTESIAN_POINT('Ctrl Pts',(132.246519414397,32.461330760321,26.8507005602657));
#43612=CARTESIAN_POINT('Ctrl Pts',(132.219538703033,32.4377083083858,26.8485150568652));
#43613=CARTESIAN_POINT('Ctrl Pts',(132.078643979194,32.3182458249101,26.837138995158));
#43614=CARTESIAN_POINT('Ctrl Pts',(131.958888328919,32.2295639714867,26.827598065087));
#43615=CARTESIAN_POINT('Ctrl Pts',(131.726048860069,32.0798040275783,26.8097653438476));
#43616=CARTESIAN_POINT('Ctrl Pts',(131.614554581721,32.0167124264297,26.8014987711256));
#43617=CARTESIAN_POINT('Ctrl Pts',(131.36499186427,31.8935898024786,26.7837941281575));
#43618=CARTESIAN_POINT('Ctrl Pts',(131.22594259457,31.8361318853769,26.7744251611541));
#43619=CARTESIAN_POINT('Ctrl Pts',(131.043077614443,31.7744432822549,26.7627786588056));
#43620=CARTESIAN_POINT('Ctrl Pts',(131.002376853114,31.7615639665268,26.7602269846072));
#43621=CARTESIAN_POINT('Ctrl Pts',(130.934581474045,31.7415115233497,26.7560416649428));
#43622=CARTESIAN_POINT('Ctrl Pts',(130.907622680837,31.7338997529692,26.7543941617961));
#43623=CARTESIAN_POINT('Ctrl Pts',(130.854578436878,31.7196303075117,26.7511843481561));
#43624=CARTESIAN_POINT('Ctrl Pts',(130.828501964309,31.7129474935023,26.7496213406051));
#43625=CARTESIAN_POINT('Ctrl Pts',(130.7709090476,31.6989166354121,26.7462007406769));
#43626=CARTESIAN_POINT('Ctrl Pts',(130.739361214378,31.6917078066846,26.7443476347643));
#43627=CARTESIAN_POINT('Ctrl Pts',(130.629182261354,31.6681862162432,26.7379427701141));
#43628=CARTESIAN_POINT('Ctrl Pts',(130.550075814619,31.6542158839966,26.7334630773457));
#43629=CARTESIAN_POINT('Ctrl Pts',(130.19197226452,31.6040202769227,26.7135922502048));
#43630=CARTESIAN_POINT('Ctrl Pts',(129.909645010857,31.5998003012233,26.6991317310287));
#43631=CARTESIAN_POINT('Ctrl Pts',(129.563438593948,31.6378118020697,26.6802805678334));
#43632=CARTESIAN_POINT('Ctrl Pts',(129.497064085396,31.6470982858762,26.6766090862874));
#43633=CARTESIAN_POINT('Ctrl Pts',(129.386294991413,31.6659590879004,26.6703232922234));
#43634=CARTESIAN_POINT('Ctrl Pts',(129.341737581999,31.6744695429726,26.6677511785052));
#43635=CARTESIAN_POINT('Ctrl Pts',(129.27799144348,31.6879763047251,26.6639914245659));
#43636=CARTESIAN_POINT('Ctrl Pts',(129.258653113571,31.6922512086516,26.6628401890118));
#43637=CARTESIAN_POINT('Ctrl Pts',(129.224787208086,31.7000494506515,26.6608036212264));
#43638=CARTESIAN_POINT('Ctrl Pts',(129.210243746969,31.7034998028508,26.6599222970913));
#43639=CARTESIAN_POINT('Ctrl Pts',(129.178199947378,31.7113262376537,26.6579652024416));
#43640=CARTESIAN_POINT('Ctrl Pts',(129.160711643262,31.71574582839,26.656887166339));
#43641=CARTESIAN_POINT('Ctrl Pts',(129.10877219126,31.7293137387408,26.6536575548113));
#43642=CARTESIAN_POINT('Ctrl Pts',(129.074430190552,31.7388658510306,26.6514854915809));
#43643=CARTESIAN_POINT('Ctrl Pts',(128.901591763817,31.7898901724134,26.6403893903998));
#43644=CARTESIAN_POINT('Ctrl Pts',(128.76570803256,31.8396483629176,26.6311344485386));
#43645=CARTESIAN_POINT('Ctrl Pts',(128.520060699034,31.947864531237,26.6138494102096));
#43646=CARTESIAN_POINT('Ctrl Pts',(128.409513671725,32.0039849627096,26.6058452079918));
#43647=CARTESIAN_POINT('Ctrl Pts',(128.210942693684,32.1188863209674,26.5912200509964));
#43648=CARTESIAN_POINT('Ctrl Pts',(128.122112945259,32.175980658667,26.5845767806013));
#43649=CARTESIAN_POINT('Ctrl Pts',(127.975712420424,32.2800456771507,26.5734949155237));
#43650=CARTESIAN_POINT('Ctrl Pts',(127.916758582053,32.3249302465901,26.5689919189262));
#43651=CARTESIAN_POINT('Ctrl Pts',(127.83290980495,32.3932232000597,26.5625252675083));
#43652=CARTESIAN_POINT('Ctrl Pts',(127.806825363361,32.4151304987645,26.5605042123048));
#43653=CARTESIAN_POINT('Ctrl Pts',(127.761008829871,32.4548029271644,26.556936207825));
#43654=CARTESIAN_POINT('Ctrl Pts',(127.741147217858,32.4724134500349,26.5553832081525));
#43655=CARTESIAN_POINT('Ctrl Pts',(127.699437805256,32.5102799165774,26.5521074612325));
#43656=CARTESIAN_POINT('Ctrl Pts',(127.677645973352,32.5305943301381,26.5503873280708));
#43657=CARTESIAN_POINT('Ctrl Pts',(127.619028944112,32.5866996423387,26.5457341222069));
#43658=CARTESIAN_POINT('Ctrl Pts',(127.582743943563,32.6230449453872,26.5428247744739));
#43659=CARTESIAN_POINT('Ctrl Pts',(127.375060425673,32.8407500318552,26.5259642020765));
#43660=CARTESIAN_POINT('Ctrl Pts',(127.223285073611,33.0397618764855,26.5128548293274));
#43661=CARTESIAN_POINT('Ctrl Pts',(127.033530045413,33.3554427869589,26.4932945514482));
#43662=CARTESIAN_POINT('Ctrl Pts',(126.977735037592,33.4603819487298,26.486954707205));
#43663=CARTESIAN_POINT('Ctrl Pts',(126.899623357417,33.6279778617142,26.4767708357208));
#43664=CARTESIAN_POINT('Ctrl Pts',(126.873443912479,33.6887311621582,26.4730672340935));
#43665=CARTESIAN_POINT('Ctrl Pts',(126.840668297963,33.7713640512458,26.4679648317604));
#43666=CARTESIAN_POINT('Ctrl Pts',(126.832490137436,33.7926043282475,26.4666476209584));
#43667=CARTESIAN_POINT('Ctrl Pts',(126.819150775209,33.8283177344914,26.4644208700565));
#43668=CARTESIAN_POINT('Ctrl Pts',(126.813872808196,33.8427469452109,26.4635179357086));
#43669=CARTESIAN_POINT('Ctrl Pts',(126.803120702062,33.8727728602793,26.4616313758305));
#43670=CARTESIAN_POINT('Ctrl Pts',(126.797662294472,33.8883744044702,26.4606469693287));
#43671=CARTESIAN_POINT('Ctrl Pts',(126.783160624375,33.9308172629002,26.4579589469619));
#43672=CARTESIAN_POINT('Ctrl Pts',(126.774339525068,33.957732433461,26.4562435270594));
#43673=CARTESIAN_POINT('Ctrl Pts',(126.720193774909,34.1302178169966,26.4451955018039));
#43674=CARTESIAN_POINT('Ctrl Pts',(126.684400452344,34.2785839766073,26.4354521072505));
#43675=CARTESIAN_POINT('Ctrl Pts',(126.626604614875,34.6166890551896,26.4133729314832));
#43676=CARTESIAN_POINT('Ctrl Pts',(126.610389780316,34.8069278845278,26.4010494746156));
#43677=CARTESIAN_POINT('Ctrl Pts',(126.610175022935,35.1016647330484,26.3825795547791));
#43678=CARTESIAN_POINT('Ctrl Pts',(126.614897715772,35.2057547114801,26.3761709170851));
#43679=CARTESIAN_POINT('Ctrl Pts',(126.62800535707,35.3487281028196,26.3675337610334));
#43680=CARTESIAN_POINT('Ctrl Pts',(126.63228909971,35.3879209332811,26.3651830153553));
#43681=CARTESIAN_POINT('Ctrl Pts',(126.64035998537,35.4514767387727,26.3613971096362));
#43682=CARTESIAN_POINT('Ctrl Pts',(126.643730796172,35.4758879624845,26.3599492528049));
#43683=CARTESIAN_POINT('Ctrl Pts',(126.651397953111,35.5272714839633,26.3569141535342));
#43684=CARTESIAN_POINT('Ctrl Pts',(126.65575469729,35.5542330785541,26.3553289021937));
#43685=CARTESIAN_POINT('Ctrl Pts',(126.667133689455,35.6196233185677,26.3515004563569));
#43686=CARTESIAN_POINT('Ctrl Pts',(126.674495371031,35.6579893932487,26.3492679709382));
#43687=CARTESIAN_POINT('Ctrl Pts',(126.705097587925,35.8038084756085,26.340826609284));
#43688=CARTESIAN_POINT('Ctrl Pts',(126.732897811005,35.9102397376974,26.3347591677512));
#43689=CARTESIAN_POINT('Ctrl Pts',(126.782934923845,36.0696551455584,26.3256969442815));
#43690=CARTESIAN_POINT('Ctrl Pts',(126.801414675095,36.1237064934745,26.322628320241));
#43691=CARTESIAN_POINT('Ctrl Pts',(126.821241849252,36.1772432550457,26.31957821124));
#43692=CARTESIAN_POINT('',(126.610250231881,35.0012538096501,26.7339821967504));
#43693=CARTESIAN_POINT('Ctrl Pts',(126.821241918426,36.1772434418289,26.660716603687));
#43694=CARTESIAN_POINT('Ctrl Pts',(126.799783544056,36.1193021711248,26.6645592714981));
#43695=CARTESIAN_POINT('Ctrl Pts',(126.779914062806,36.0607868592372,26.6684601693087));
#43696=CARTESIAN_POINT('Ctrl Pts',(126.717623530252,35.8594237440769,26.681883581533));
#43697=CARTESIAN_POINT('Ctrl Pts',(126.683024607012,35.7143375892325,26.6915468822929));
#43698=CARTESIAN_POINT('Ctrl Pts',(126.626333159024,35.380459596025,26.7132883205415));
#43699=CARTESIAN_POINT('Ctrl Pts',(126.610329828592,35.1911214548352,26.7252549797204));
#43700=CARTESIAN_POINT('Ctrl Pts',(126.6102502979,35.0014211316691,26.7367447340574));
#43701=CARTESIAN_POINT('Ctrl Pts',(126.610250231881,35.0012538096501,26.7339821967504));
#43702=CARTESIAN_POINT('Ctrl Pts',(126.610210918892,34.8949687788819,26.740189865272));
#43703=CARTESIAN_POINT('Ctrl Pts',(126.615174777716,34.7887128757728,26.7463975337937));
#43704=CARTESIAN_POINT('Ctrl Pts',(126.625107297087,34.6829758584513,26.7526052023153));
#43705=CARTESIAN_POINT('Ctrl Pts',(126.635045153883,34.5771820213633,26.7588162066439));
#43706=CARTESIAN_POINT('Ctrl Pts',(126.649956949819,34.4719080254279,26.7650272109724));
#43707=CARTESIAN_POINT('Ctrl Pts',(126.669756487626,34.367636804686,26.771238215301));
#43708=CARTESIAN_POINT('Ctrl Pts',(126.689810650005,34.2620246427923,26.7775290939347));
#43709=CARTESIAN_POINT('Ctrl Pts',(126.714879066246,34.1574416454979,26.7838199725683));
#43710=CARTESIAN_POINT('Ctrl Pts',(126.744819612016,34.0543754951455,26.790110851202));
#43711=CARTESIAN_POINT('Ctrl Pts',(126.774450142089,33.9523765305604,26.7963365917072));
#43712=CARTESIAN_POINT('Ctrl Pts',(126.808852175928,33.8518635051602,26.8025623322124));
#43713=CARTESIAN_POINT('Ctrl Pts',(126.847839093271,33.7532896565007,26.8087880727176));
#43714=CARTESIAN_POINT('Ctrl Pts',(126.887437873932,33.6531687831915,26.8151115204155));
#43715=CARTESIAN_POINT('Ctrl Pts',(126.931766482537,33.5550488623061,26.8214349681134));
#43716=CARTESIAN_POINT('Ctrl Pts',(126.980581021143,33.4593786666999,26.8277584158113));
#43717=CARTESIAN_POINT('Ctrl Pts',(127.029395559749,33.3637084710937,26.8340818635091));
#43718=CARTESIAN_POINT('Ctrl Pts',(127.082695759614,33.2704883394357,26.840405311207));
#43719=CARTESIAN_POINT('Ctrl Pts',(127.140192688397,33.1801353888262,26.8467287589049));
#43720=CARTESIAN_POINT('Ctrl Pts',(127.195672875846,33.0929516254072,26.8528304076542));
#43721=CARTESIAN_POINT('Ctrl Pts',(127.255237266495,33.0081598841338,26.8589320564036));
#43722=CARTESIAN_POINT('Ctrl Pts',(127.318653174024,32.9261667710911,26.8650337051529));
#43723=CARTESIAN_POINT('Ctrl Pts',(127.381985666382,32.8442815090561,26.8711273279969));
#43724=CARTESIAN_POINT('Ctrl Pts',(127.449159344413,32.7651878923461,26.8772209508408));
#43725=CARTESIAN_POINT('Ctrl Pts',(127.519897363508,32.689265057397,26.8833145736848));
#43726=CARTESIAN_POINT('Ctrl Pts',(127.590562576428,32.6134203650273,26.8894019247476));
#43727=CARTESIAN_POINT('Ctrl Pts',(127.66478454543,32.5407402762669,26.8954892758104));
#43728=CARTESIAN_POINT('Ctrl Pts',(127.742245693163,32.4715715251444,26.9015766268732));
#43729=CARTESIAN_POINT('Ctrl Pts',(127.819651737303,32.4024519786474,26.9076596475725));
#43730=CARTESIAN_POINT('Ctrl Pts',(127.900292059834,32.3368390866557,26.9137426682719));
#43731=CARTESIAN_POINT('Ctrl Pts',(127.983812297817,32.2750427137171,26.9198256889713));
#43732=CARTESIAN_POINT('Ctrl Pts',(128.067301613316,32.2132692202315,26.9259064574966));
#43733=CARTESIAN_POINT('Ctrl Pts',(128.153668381654,32.1553096916414,26.9319872260219));
#43734=CARTESIAN_POINT('Ctrl Pts',(128.242525864334,32.1014331601695,26.9380679945473));
#43735=CARTESIAN_POINT('Ctrl Pts',(128.331373469526,32.0475626176675,26.9441480871282));
#43736=CARTESIAN_POINT('Ctrl Pts',(128.422710872735,31.9977743915357,26.9502281797091));
#43737=CARTESIAN_POINT('Ctrl Pts',(128.51612389788,31.9522931938821,26.9563082722901));
#43738=CARTESIAN_POINT('Ctrl Pts',(128.609550740106,31.9068052689289,26.962389264201));
#43739=CARTESIAN_POINT('Ctrl Pts',(128.705053429597,31.8656258254152,26.9684702561119));
#43740=CARTESIAN_POINT('Ctrl Pts',(128.802195670932,31.8289323798183,26.9745512480228));
#43741=CARTESIAN_POINT('Ctrl Pts',(128.899438741757,31.7922008479942,26.9806385517432));
#43742=CARTESIAN_POINT('Ctrl Pts',(128.998324362099,31.7599647645011,26.9867258554636));
#43743=CARTESIAN_POINT('Ctrl Pts',(129.098398877822,31.7323524549017,26.992813159184));
#43744=CARTESIAN_POINT('Ctrl Pts',(129.198527160446,31.7047253100735,26.998903733422));
#43745=CARTESIAN_POINT('Ctrl Pts',(129.299845193589,31.681726982188,27.0049943076599));
#43746=CARTESIAN_POINT('Ctrl Pts',(129.401888827003,31.6634346871018,27.0110848818979));
#43747=CARTESIAN_POINT('Ctrl Pts',(129.504099053315,31.6451125286487,27.0171853993963));
#43748=CARTESIAN_POINT('Ctrl Pts',(129.607036821974,31.6315118072128,27.0232859168946));
#43749=CARTESIAN_POINT('Ctrl Pts',(129.710232315187,31.6226578865419,27.029386434393));
#43750=CARTESIAN_POINT('Ctrl Pts',(129.791551230574,31.6156809226893,27.0341936934198));
#43751=CARTESIAN_POINT('Ctrl Pts',(129.873030044137,31.6116504793404,27.0390009524466));
#43752=CARTESIAN_POINT('Ctrl Pts',(129.95444001818,31.610556188612,27.0438082114734));
#43753=CARTESIAN_POINT('Ctrl Pts',(130.057770259625,31.6091672516112,27.0499098623063));
#43754=CARTESIAN_POINT('Ctrl Pts',(130.161338693267,31.6125054473483,27.0560115131392));
#43755=CARTESIAN_POINT('Ctrl Pts',(130.264677695029,31.6205990500897,27.0621131639721));
#43756=CARTESIAN_POINT('Ctrl Pts',(130.367880768537,31.6286820068093,27.068206788922));
#43757=CARTESIAN_POINT('Ctrl Pts',(130.470854587276,31.6415079020645,27.0743004138719));
#43758=CARTESIAN_POINT('Ctrl Pts',(130.573130296056,31.6590530195404,27.0803940388219));
#43759=CARTESIAN_POINT('Ctrl Pts',(130.675300739269,31.6765800789967,27.0864813920099));
#43760=CARTESIAN_POINT('Ctrl Pts',(130.77677408194,31.6988166302027,27.092568745198));
#43761=CARTESIAN_POINT('Ctrl Pts',(130.877086241145,31.7256871273358,27.0986560983861));
#43762=CARTESIAN_POINT('Ctrl Pts',(130.977327041571,31.752538509679,27.1047391212308));
#43763=CARTESIAN_POINT('Ctrl Pts',(131.076407889174,31.7840171723514,27.1108221440756));
#43764=CARTESIAN_POINT('Ctrl Pts',(131.173875373105,31.8199965926247,27.1169051669204));
#43765=CARTESIAN_POINT('Ctrl Pts',(131.271306770929,31.8559626919715,27.1229859376027));
#43766=CARTESIAN_POINT('Ctrl Pts',(131.367125591384,31.8964260891807,27.1290667082849));
#43767=CARTESIAN_POINT('Ctrl Pts',(131.460894827519,31.9412108007533,27.1351474789672));
#43768=CARTESIAN_POINT('Ctrl Pts',(131.554653640311,31.985990534079,27.141227573714));
#43769=CARTESIAN_POINT('Ctrl Pts',(131.646362935839,32.035090442233,27.1473076684607));
#43770=CARTESIAN_POINT('Ctrl Pts',(131.735607734947,32.0882872990467,27.1533877632075));
#43771=CARTESIAN_POINT('Ctrl Pts',(131.824865734684,32.1414920244646,27.1594687572904));
#43772=CARTESIAN_POINT('Ctrl Pts',(131.911658146298,32.1987946834705,27.1655497513734));
#43773=CARTESIAN_POINT('Ctrl Pts',(131.995597338689,32.2599276789989,27.1716307454564));
#43774=CARTESIAN_POINT('Ctrl Pts',(132.079623656287,32.3211241279004,27.177718051345));
#43775=CARTESIAN_POINT('Ctrl Pts',(132.160790493824,32.3861586008612,27.1838053572336));
#43776=CARTESIAN_POINT('Ctrl Pts',(132.238741846655,32.4547220178269,27.1898926631222));
#43777=CARTESIAN_POINT('Ctrl Pts',(132.316735080305,32.5233222717677,27.1959832395295));
#43778=CARTESIAN_POINT('Ctrl Pts',(132.39150908014,32.5954549493437,27.2020738159367));
#43779=CARTESIAN_POINT('Ctrl Pts',(132.462744834613,32.6707741753775,27.208164392344));
#43780=CARTESIAN_POINT('Ctrl Pts',(132.534096885825,32.7462163646678,27.2142649119909));
#43781=CARTESIAN_POINT('Ctrl Pts',(132.601898872626,32.824855170724,27.2203654316377));
#43782=CARTESIAN_POINT('Ctrl Pts',(132.665872044335,32.90631155476,27.2264659512846));
#43783=CARTESIAN_POINT('Ctrl Pts',(132.716283198355,32.9704995606356,27.2312731888703));
#43784=CARTESIAN_POINT('Ctrl Pts',(132.764317638959,33.0364364599261,27.2360804264561));
#43785=CARTESIAN_POINT('Ctrl Pts',(132.809858653429,33.1039252624829,27.2408876640418));
#43786=CARTESIAN_POINT('Ctrl Pts',(132.86766209271,33.1895861759738,27.2469893038304));
#43787=CARTESIAN_POINT('Ctrl Pts',(132.921642478837,33.2780375419525,27.253090943619));
#43788=CARTESIAN_POINT('Ctrl Pts',(132.971519829651,33.3689037537619,27.2591925834075));
#43789=CARTESIAN_POINT('Ctrl Pts',(133.021331573391,33.4596504430609,27.2652861972941));
#43790=CARTESIAN_POINT('Ctrl Pts',(133.067050807172,33.5528052915461,27.2713798111808));
#43791=CARTESIAN_POINT('Ctrl Pts',(133.10844035734,33.6479631634594,27.2774734250674));
#43792=CARTESIAN_POINT('Ctrl Pts',(133.149787307896,33.7430230954735,27.2835607671878));
#43793=CARTESIAN_POINT('Ctrl Pts',(133.186813266437,33.8400815612675,27.2896481093081));
#43794=CARTESIAN_POINT('Ctrl Pts',(133.219327023952,33.9387090053368,27.2957354514285));
#43795=CARTESIAN_POINT('Ctrl Pts',(133.251817652411,34.0372662895778,27.3018184632442));
#43796=CARTESIAN_POINT('Ctrl Pts',(133.279802329281,34.1373899275475,27.30790147506));
#43797=CARTESIAN_POINT('Ctrl Pts',(133.303138331179,34.2386313458034,27.3139844868757));
#43798=CARTESIAN_POINT('Ctrl Pts',(133.326465693307,34.3398352810896,27.3200652465564));
#43799=CARTESIAN_POINT('Ctrl Pts',(133.345147705063,34.4421557578086,27.326146006237));
#43800=CARTESIAN_POINT('Ctrl Pts',(133.359092002632,34.5451308096242,27.3322267659177));
#43801=CARTESIAN_POINT('Ctrl Pts',(133.37303475025,34.6480944154463,27.3383068497033));
#43802=CARTESIAN_POINT('Ctrl Pts',(133.38224077345,34.7517120278049,27.3443869334888));
#43803=CARTESIAN_POINT('Ctrl Pts',(133.386669295655,34.8555142070427,27.3504670172744));
#43804=CARTESIAN_POINT('Ctrl Pts',(133.391098472945,34.959331741101,27.3565480004494));
#43805=CARTESIAN_POINT('Ctrl Pts',(133.390748726961,35.063333468874,27.3626289836245));
#43806=CARTESIAN_POINT('Ctrl Pts',(133.385631382875,35.1670485013206,27.3687099667996));
#43807=CARTESIAN_POINT('Ctrl Pts',(133.380508727074,35.2708711881793,27.3747972619302));
#43808=CARTESIAN_POINT('Ctrl Pts',(133.370608611354,35.3744061573462,27.3808845570608));
#43809=CARTESIAN_POINT('Ctrl Pts',(133.355994392532,35.4771862317753,27.3869718521914));
#43810=CARTESIAN_POINT('Ctrl Pts',(133.341372321774,35.5800215279423,27.3930624179074));
#43811=CARTESIAN_POINT('Ctrl Pts',(133.322031182432,35.6821007011185,27.3991529836234));
#43812=CARTESIAN_POINT('Ctrl Pts',(133.298085383964,35.7829673445205,27.4052435493394));
#43813=CARTESIAN_POINT('Ctrl Pts',(133.274100491576,35.8839986628428,27.4113440585154));
#43814=CARTESIAN_POINT('Ctrl Pts',(133.245496040138,35.9838130852854,27.4174445676913));
#43815=CARTESIAN_POINT('Ctrl Pts',(133.212436245724,36.0819696990494,27.4235450768672));
#43816=CARTESIAN_POINT('Ctrl Pts',(133.186384340044,36.1593194493689,27.4283524234482));
#43817=CARTESIAN_POINT('Ctrl Pts',(133.157566756941,36.2356400196643,27.4331597700292));
#43818=CARTESIAN_POINT('Ctrl Pts',(133.126084283164,36.310725797813,27.4379671166102));
#43819=CARTESIAN_POINT('Ctrl Pts',(133.086125603402,36.4060273482895,27.4440687725315));
#43820=CARTESIAN_POINT('Ctrl Pts',(133.041737391433,36.499661019544,27.4501704284528));
#43821=CARTESIAN_POINT('Ctrl Pts',(132.993080319361,36.5911867471649,27.4562720843741));
#43822=CARTESIAN_POINT('Ctrl Pts',(132.944487249499,36.682592084295,27.4623657143406));
#43823=CARTESIAN_POINT('Ctrl Pts',(132.891636681759,36.7718946155797,27.4684593443072));
#43824=CARTESIAN_POINT('Ctrl Pts',(132.834737451556,36.8586738937331,27.4745529742737));
#43825=CARTESIAN_POINT('Ctrl Pts',(132.77789678461,36.9453638547353,27.4806403324011));
#43826=CARTESIAN_POINT('Ctrl Pts',(132.717015974739,37.0295353710263,27.4867276905286));
#43827=CARTESIAN_POINT('Ctrl Pts',(132.652349477433,37.1107930528741,27.492815048656));
#43828=CARTESIAN_POINT('Ctrl Pts',(132.587728983149,37.1919929289171,27.498898076305));
#43829=CARTESIAN_POINT('Ctrl Pts',(132.519328422461,37.2702827588664,27.5049811039541));
#43830=CARTESIAN_POINT('Ctrl Pts',(132.44744473493,37.3452972800827,27.5110641316031));
#43831=CARTESIAN_POINT('Ctrl Pts',(132.375587662402,37.4202840271022,27.5171449070055));
#43832=CARTESIAN_POINT('Ctrl Pts',(132.300250321725,37.4919975670229,27.5232256824078));
#43833=CARTESIAN_POINT('Ctrl Pts',(132.221768459159,37.5601074150091,27.5293064578102));
#43834=CARTESIAN_POINT('Ctrl Pts',(132.143295321744,37.6282096909439,27.5353865571877));
#43835=CARTESIAN_POINT('Ctrl Pts',(132.061678680655,37.6927087912504,27.5414666565653));
#43836=CARTESIAN_POINT('Ctrl Pts',(131.977288810877,37.7533132805549,27.5475467559429));
#43837=CARTESIAN_POINT('Ctrl Pts',(131.892886459905,37.8139267332147,27.5536277545623));
#43838=CARTESIAN_POINT('Ctrl Pts',(131.805710412839,37.8706441809512,27.5597087531817));
#43839=CARTESIAN_POINT('Ctrl Pts',(131.716160717207,37.9232169702598,27.5657897518011));
#43840=CARTESIAN_POINT('Ctrl Pts',(131.626518075536,37.9758443262817,27.5718770620526));
#43841=CARTESIAN_POINT('Ctrl Pts',(131.534497234732,38.0243182157326,27.5779643723042));
#43842=CARTESIAN_POINT('Ctrl Pts',(131.440523659614,38.0684355376302,27.5840516825558));
#43843=CARTESIAN_POINT('Ctrl Pts',(131.346499596856,38.1125765617171,27.5901422632366));
#43844=CARTESIAN_POINT('Ctrl Pts',(131.250521105259,38.1523561921926,27.5962328439174));
#43845=CARTESIAN_POINT('Ctrl Pts',(131.153032627016,38.1876199308476,27.6023234245982));
#43846=CARTESIAN_POINT('Ctrl Pts',(131.055384996012,38.222941238576,27.6084239483281));
#43847=CARTESIAN_POINT('Ctrl Pts',(130.956222862647,38.2537317998478,27.614524472058));
#43848=CARTESIAN_POINT('Ctrl Pts',(130.856005012664,38.2798872664763,27.620624995788));
#43849=CARTESIAN_POINT('Ctrl Pts',(130.777033701207,38.3004976817045,27.6254321869182));
#43850=CARTESIAN_POINT('Ctrl Pts',(130.697407166111,38.3182309901524,27.6302393780484));
#43851=CARTESIAN_POINT('Ctrl Pts',(130.617352600307,38.3330587797688,27.6350465691787));
#43852=CARTESIAN_POINT('Ctrl Pts',(130.515741023488,38.3518793812989,27.6411482357845));
#43853=CARTESIAN_POINT('Ctrl Pts',(130.413096307233,38.3660809580804,27.6472499023904));
#43854=CARTESIAN_POINT('Ctrl Pts',(130.309874585369,38.3755566657727,27.6533515689962));
#43855=CARTESIAN_POINT('Ctrl Pts',(130.206788634955,38.3850199097069,27.6594452098483));
#43856=CARTESIAN_POINT('Ctrl Pts',(130.103127610138,38.3897696036588,27.6655388507005));
#43857=CARTESIAN_POINT('Ctrl Pts',(129.999357638686,38.3897499391359,27.6716324915526));
#43858=CARTESIAN_POINT('Ctrl Pts',(129.895694468648,38.389730294852,27.6777198607497));
#43859=CARTESIAN_POINT('Ctrl Pts',(129.791923000431,38.3849510531249,27.6838072299467));
#43860=CARTESIAN_POINT('Ctrl Pts',(129.688513411436,38.3754082964354,27.6898945991438));
#43861=CARTESIAN_POINT('Ctrl Pts',(129.585177382847,38.3658723279853,27.6959776380911));
#43862=CARTESIAN_POINT('Ctrl Pts',(129.482203146275,38.3515796221331,27.7020606770384));
#43863=CARTESIAN_POINT('Ctrl Pts',(129.380058969734,38.3325783083813,27.7081437159857));
#43864=CARTESIAN_POINT('Ctrl Pts',(129.277952609821,38.3135840294466,27.7142245028221));
#43865=CARTESIAN_POINT('Ctrl Pts',(129.176676119256,38.2898846853788,27.7203052896585));
#43866=CARTESIAN_POINT('Ctrl Pts',(129.076689951158,38.2615799263866,27.7263860764948));
#43867=CARTESIAN_POINT('Ctrl Pts',(128.976714896919,38.2332783135805,27.7324661874277));
#43868=CARTESIAN_POINT('Ctrl Pts',(128.878030291518,38.2003724202943,27.7385462983605));
#43869=CARTESIAN_POINT('Ctrl Pts',(128.781082855486,38.1630121810245,27.7446264092933));
#43870=CARTESIAN_POINT('Ctrl Pts',(128.684121079331,38.1256464155598,27.7507074195747));
#43871=CARTESIAN_POINT('Ctrl Pts',(128.588897382226,38.0838251489321,27.7567884298561));
#43872=CARTESIAN_POINT('Ctrl Pts',(128.495839023297,38.0377466679536,27.7628694401375));
#43873=CARTESIAN_POINT('Ctrl Pts',(128.402684075371,37.9916203602747,27.768956762143));
#43874=CARTESIAN_POINT('Ctrl Pts',(128.311699338125,37.9412282038409,27.7750440841484));
#43875=CARTESIAN_POINT('Ctrl Pts',(128.223287904622,37.8868147139431,27.7811314061539));
#43876=CARTESIAN_POINT('Ctrl Pts',(128.134828970858,37.8323719896477,27.787221998657));
#43877=CARTESIAN_POINT('Ctrl Pts',(128.048946448402,37.7739038690723,27.7933125911601));
#43878=CARTESIAN_POINT('Ctrl Pts',(127.966013183012,37.7116973818659,27.7994031836632));
#43879=CARTESIAN_POINT('Ctrl Pts',(127.882944527085,37.6493893410834,27.805503719204));
#43880=CARTESIAN_POINT('Ctrl Pts',(127.802835076882,37.5833310140908,27.8116042547449));
#43881=CARTESIAN_POINT('Ctrl Pts',(127.726023596702,37.5138489174461,27.8177047902857));
#43882=CARTESIAN_POINT('Ctrl Pts',(127.665497974148,37.4590986750873,27.8225118674395));
#43883=CARTESIAN_POINT('Ctrl Pts',(127.60701941582,37.4022234011004,27.8273189445933));
#43884=CARTESIAN_POINT('Ctrl Pts',(127.550736212838,37.3433975256871,27.8321260217471));
#43885=CARTESIAN_POINT('Ctrl Pts',(127.480210871469,37.2696861033617,27.8381495019205));
#43886=CARTESIAN_POINT('Ctrl Pts',(127.412881596586,37.1926473030203,27.8441729820939));
#43887=CARTESIAN_POINT('Ctrl Pts',(127.349084150531,37.1125932456429,27.8501964622673));
#43888=CARTESIAN_POINT('Ctrl Pts',(127.285385720088,37.0326634346403,27.8562105938131));
#43889=CARTESIAN_POINT('Ctrl Pts',(127.225208489255,36.9497280139285,27.8622247253588));
#43890=CARTESIAN_POINT('Ctrl Pts',(127.168851230835,36.8641356467162,27.8682388569045));
#43891=CARTESIAN_POINT('Ctrl Pts',(127.112544511846,36.7786200360664,27.8742475951649));
#43892=CARTESIAN_POINT('Ctrl Pts',(127.060051203334,36.6904525754194,27.8802563334252));
#43893=CARTESIAN_POINT('Ctrl Pts',(127.011629290659,36.6000142393288,27.8862650716856));
#43894=CARTESIAN_POINT('Ctrl Pts',(126.963239521667,36.5096359384768,27.8922698211946));
#43895=CARTESIAN_POINT('Ctrl Pts',(126.918915984628,36.4169901445685,27.8982745707036));
#43896=CARTESIAN_POINT('Ctrl Pts',(126.878872253773,36.3224850298713,27.9042793202126));
#43897=CARTESIAN_POINT('Ctrl Pts',(126.858553141375,36.2745309554951,27.907326268576));
#43898=CARTESIAN_POINT('Ctrl Pts',(126.839335262965,36.2260985580622,27.9103732169395));
#43899=CARTESIAN_POINT('Ctrl Pts',(126.821241918358,36.1772434416438,27.913420165303));
#43900=CARTESIAN_POINT('Origin',(130.,35.,23.));
#43901=CARTESIAN_POINT('',(126.821241934448,36.17724348509,29.1634527466974));
#43902=CARTESIAN_POINT('',(126.821241918358,36.1772434416436,28.8235740826546));
#43903=CARTESIAN_POINT('',(126.821241918358,36.1772434416438,23.));
#43904=CARTESIAN_POINT('',(132.573234427015,37.2065515280923,30.));
#43905=CARTESIAN_POINT('Ctrl Pts',(132.573234427015,37.2065515280921,29.9999999999999));
#43906=CARTESIAN_POINT('Ctrl Pts',(132.579543502806,37.1991940153298,29.999431170887));
#43907=CARTESIAN_POINT('Ctrl Pts',(132.585821065603,37.1918093942846,29.9988641961783));
#43908=CARTESIAN_POINT('Ctrl Pts',(132.599714029705,37.1753236187309,29.9976069824885));
#43909=CARTESIAN_POINT('Ctrl Pts',(132.60731351268,37.166209162608,29.9969176352125));
#43910=CARTESIAN_POINT('Ctrl Pts',(132.636602405948,37.1307040370924,29.9942536828936));
#43911=CARTESIAN_POINT('Ctrl Pts',(132.657940874235,37.1040252846207,29.9922974533084));
#43912=CARTESIAN_POINT('Ctrl Pts',(132.773829252144,36.9545567649187,29.9815615504326));
#43913=CARTESIAN_POINT('Ctrl Pts',(132.860282271052,36.8257089538147,29.9731252601069));
#43914=CARTESIAN_POINT('Ctrl Pts',(133.018347198056,36.5511804425255,29.9559328731301));
#43915=CARTESIAN_POINT('Ctrl Pts',(133.088931743976,36.405374905407,29.9471969570919));
#43916=CARTESIAN_POINT('Ctrl Pts',(133.170151634526,36.2016068031044,29.9350254270888));
#43917=CARTESIAN_POINT('Ctrl Pts',(133.190103632595,36.147588212588,29.9318033302057));
#43918=CARTESIAN_POINT('Ctrl Pts',(133.224142504401,36.0476700300939,29.9258303603832));
#43919=CARTESIAN_POINT('Ctrl Pts',(133.238648741697,36.001928852775,29.9230911528992));
#43920=CARTESIAN_POINT('Ctrl Pts',(133.260934604744,35.9261072468255,29.9185337556719));
#43921=CARTESIAN_POINT('Ctrl Pts',(133.26928051528,35.896199730786,29.9167318836821));
#43922=CARTESIAN_POINT('Ctrl Pts',(133.284811176684,35.8374392397412,29.9131811344762));
#43923=CARTESIAN_POINT('Ctrl Pts',(133.292029485041,35.8085980084427,29.9114334138339));
#43924=CARTESIAN_POINT('Ctrl Pts',(133.307087210171,35.7448868470315,29.9075600154555));
#43925=CARTESIAN_POINT('Ctrl Pts',(133.314756329506,35.709980682258,29.905429579274));
#43926=CARTESIAN_POINT('Ctrl Pts',(133.335889145256,35.6059738755283,29.8990540301905));
#43927=CARTESIAN_POINT('Ctrl Pts',(133.347753148856,35.5365710943665,29.8947632501768));
#43928=CARTESIAN_POINT('Ctrl Pts',(133.393624784718,35.2066777904556,29.8741797628565));
#43929=CARTESIAN_POINT('Ctrl Pts',(133.399432763104,34.9432083554542,29.8570994967609));
#43930=CARTESIAN_POINT('Ctrl Pts',(133.364495018107,34.5727113607211,29.8329906909243));
#43931=CARTESIAN_POINT('Ctrl Pts',(133.348931797021,34.464219511136,29.8259340540569));
#43932=CARTESIAN_POINT('Ctrl Pts',(133.316043421954,34.2940788387603,29.8150230129187));
#43933=CARTESIAN_POINT('Ctrl Pts',(133.302181190938,34.2318404201251,29.8110657881638));
#43934=CARTESIAN_POINT('Ctrl Pts',(133.281033934727,34.1481004927447,29.8058179643617));
#43935=CARTESIAN_POINT('Ctrl Pts',(133.275277526079,34.126230213497,29.8044545666945));
#43936=CARTESIAN_POINT('Ctrl Pts',(133.265239119605,34.0895852082588,29.8021839383872));
#43937=CARTESIAN_POINT('Ctrl Pts',(133.261074734494,34.0747793786584,29.8012703447512));
#43938=CARTESIAN_POINT('Ctrl Pts',(133.252321869158,34.0444533368971,29.7994076076095));
#43939=CARTESIAN_POINT('Ctrl Pts',(133.247722751505,34.0289367111117,29.7984591779236));
#43940=CARTESIAN_POINT('Ctrl Pts',(133.234924289306,33.9868651321377,29.7958987887815));
#43941=CARTESIAN_POINT('Ctrl Pts',(133.226509004075,33.9603764271592,29.7942988807161));
#43942=CARTESIAN_POINT('Ctrl Pts',(133.171839494331,33.7953551080938,29.7843900347279));
#43943=CARTESIAN_POINT('Ctrl Pts',(133.116993251934,33.6598144652685,29.7765061627368));
#43944=CARTESIAN_POINT('Ctrl Pts',(132.944979851788,33.3029298753189,29.7553956919803));
#43945=CARTESIAN_POINT('Ctrl Pts',(132.8118011791,33.090360633968,29.7423721876542));
#43946=CARTESIAN_POINT('Ctrl Pts',(132.61715667909,32.8447974239,29.7249895683762));
#43947=CARTESIAN_POINT('Ctrl Pts',(132.576481306061,32.7963324679505,29.7214339043033));
#43948=CARTESIAN_POINT('Ctrl Pts',(132.5136286147,32.7255634100047,29.7160314421877));
#43949=CARTESIAN_POINT('Ctrl Pts',(132.492457221272,32.702382208203,29.7142263747315));
#43950=CARTESIAN_POINT('Ctrl Pts',(132.453571716938,32.6609752824088,29.7109350850109));
#43951=CARTESIAN_POINT('Ctrl Pts',(132.435968644666,32.6426482001669,29.7094537467989));
#43952=CARTESIAN_POINT('Ctrl Pts',(132.397479758546,32.6034677445963,29.7062321106564));
#43953=CARTESIAN_POINT('Ctrl Pts',(132.376524444496,32.582685886613,29.7044887499999));
#43954=CARTESIAN_POINT('Ctrl Pts',(132.317919073489,32.5260642611729,29.699640583135));
#43955=CARTESIAN_POINT('Ctrl Pts',(132.27971316248,32.4908140165465,29.6965103205222));
#43956=CARTESIAN_POINT('Ctrl Pts',(132.016355063005,32.2588107922306,29.6751229616274));
#43957=CARTESIAN_POINT('Ctrl Pts',(131.766862907665,32.0917469731511,29.6556014388477));
#43958=CARTESIAN_POINT('Ctrl Pts',(131.382402485095,31.9022262470931,29.6278695643384));
#43959=CARTESIAN_POINT('Ctrl Pts',(131.262819949973,31.8515828266004,29.6195591923214));
#43960=CARTESIAN_POINT('Ctrl Pts',(131.108994411807,31.7966167501559,29.6094932214696));
#43961=CARTESIAN_POINT('Ctrl Pts',(131.077202575661,31.7857866191262,29.6074455889445));
#43962=CARTESIAN_POINT('Ctrl Pts',(131.029020014237,31.7701681009778,29.6043970460613));
#43963=CARTESIAN_POINT('Ctrl Pts',(131.012746418862,31.7650284381931,29.6033767382018));
#43964=CARTESIAN_POINT('Ctrl Pts',(130.982367034029,31.7556854841539,29.6014903155602));
#43965=CARTESIAN_POINT('Ctrl Pts',(130.968271440575,31.7514507694914,29.6006223258154));
#43966=CARTESIAN_POINT('Ctrl Pts',(130.935695117675,31.7418947937145,29.5986321345464));
#43967=CARTESIAN_POINT('Ctrl Pts',(130.917195616119,31.7366386764378,29.5975136270731));
#43968=CARTESIAN_POINT('Ctrl Pts',(130.856792604257,31.7200310738578,29.593896562386));
#43969=CARTESIAN_POINT('Ctrl Pts',(130.814714011916,31.7093266393166,29.5914314007824));
#43970=CARTESIAN_POINT('Ctrl Pts',(130.564651183838,31.6508038505701,29.5770410367168));
#43971=CARTESIAN_POINT('Ctrl Pts',(130.352714136749,31.6219004168492,29.5658760995767));
#43972=CARTESIAN_POINT('Ctrl Pts',(129.973225695019,31.6062755965984,29.5457252523382));
#43973=CARTESIAN_POINT('Ctrl Pts',(129.806733774014,31.6116782805812,29.5368323813005));
#43974=CARTESIAN_POINT('Ctrl Pts',(129.577290737996,31.6360932864945,29.524020356432));
#43975=CARTESIAN_POINT('Ctrl Pts',(129.51346969133,31.6447296648041,29.5203980037632));
#43976=CARTESIAN_POINT('Ctrl Pts',(129.417834692579,31.6604570704717,29.5148625070593));
#43977=CARTESIAN_POINT('Ctrl Pts',(129.38581191603,31.6661979188677,29.5129907465977));
#43978=CARTESIAN_POINT('Ctrl Pts',(129.330246921808,31.6769870096695,29.5097090662008));
#43979=CARTESIAN_POINT('Ctrl Pts',(129.306666354747,31.681826868247,29.5083057153445));
#43980=CARTESIAN_POINT('Ctrl Pts',(129.253415977728,31.6933487896156,29.5051115664288));
#43981=CARTESIAN_POINT('Ctrl Pts',(129.223780830528,31.7001797562397,29.5033162244936));
#43982=CARTESIAN_POINT('Ctrl Pts',(129.143587570761,31.7198045211257,29.4984082845861));
#43983=CARTESIAN_POINT('Ctrl Pts',(129.093227870037,31.7333674084522,29.4952720645511));
#43984=CARTESIAN_POINT('Ctrl Pts',(128.832936408414,31.8099518695685,29.4787729543286));
#43985=CARTESIAN_POINT('Ctrl Pts',(128.629193389014,31.89205713254,29.4648217502512));
#43986=CARTESIAN_POINT('Ctrl Pts',(128.318101573545,32.0539959479666,29.4422922916578));
#43987=CARTESIAN_POINT('Ctrl Pts',(128.205008187947,32.1215057671064,29.4338247481737));
#43988=CARTESIAN_POINT('Ctrl Pts',(128.038062758905,32.2348360296538,29.4211366806577));
#43989=CARTESIAN_POINT('Ctrl Pts',(127.981236338199,32.2760462332199,29.4167826496236));
#43990=CARTESIAN_POINT('Ctrl Pts',(127.907173516086,32.3333480456181,29.4111016653535));
#43991=CARTESIAN_POINT('Ctrl Pts',(127.888769205194,32.3478951878976,29.4096894529985));
#43992=CARTESIAN_POINT('Ctrl Pts',(127.858313202438,32.3724862045089,29.4073536973156));
#43993=CARTESIAN_POINT('Ctrl Pts',(127.846177734222,32.3824246407634,29.4064233263937));
#43994=CARTESIAN_POINT('Ctrl Pts',(127.821321495395,32.4030707606196,29.4045191623325));
#43995=CARTESIAN_POINT('Ctrl Pts',(127.808609715539,32.4137884566159,29.4035460945967));
#43996=CARTESIAN_POINT('Ctrl Pts',(127.774413908781,32.4430531646311,29.4009288994761));
#43997=CARTESIAN_POINT('Ctrl Pts',(127.753082663019,32.4617775590151,29.3992967791197));
#43998=CARTESIAN_POINT('Ctrl Pts',(127.627027030361,32.575262808709,29.3896373875369));
#43999=CARTESIAN_POINT('Ctrl Pts',(127.528062719975,32.6762346833468,29.3819902458382));
#44000=CARTESIAN_POINT('Ctrl Pts',(127.306067691046,32.9330191558556,29.3638553958639));
#44001=CARTESIAN_POINT('Ctrl Pts',(127.189856811042,33.094015857445,29.35348307448));
#44002=CARTESIAN_POINT('Ctrl Pts',(127.050934312555,33.3270495162919,29.3387478273863));
#44003=CARTESIAN_POINT('Ctrl Pts',(127.015535652641,33.3910489645016,29.3347302675267));
#44004=CARTESIAN_POINT('Ctrl Pts',(126.956287582004,33.5068604929344,29.3274676792414));
#44005=CARTESIAN_POINT('Ctrl Pts',(126.931623655667,33.5582243718561,29.3242492696531));
#44006=CARTESIAN_POINT('Ctrl Pts',(126.895545594211,33.6384822601704,29.3192112457515));
#44007=CARTESIAN_POINT('Ctrl Pts',(126.883213953513,33.6669537283064,29.3174223195902));
#44008=CARTESIAN_POINT('Ctrl Pts',(126.861052524359,33.7201095638191,29.3140773917719));
#44009=CARTESIAN_POINT('Ctrl Pts',(126.851118702481,33.7447481135677,29.3125249957522));
#44010=CARTESIAN_POINT('Ctrl Pts',(126.829609147711,33.7999601996466,29.3090407659347));
#44011=CARTESIAN_POINT('Ctrl Pts',(126.818184154466,33.8305892543389,29.3071041588329));
#44012=CARTESIAN_POINT('Ctrl Pts',(126.785147744064,33.923226239808,29.3012338234429));
#44013=CARTESIAN_POINT('Ctrl Pts',(126.764894271259,33.985698863947,29.2972571783176));
#44014=CARTESIAN_POINT('Ctrl Pts',(126.661228848593,34.3402503030917,29.274580814602));
#44015=CARTESIAN_POINT('Ctrl Pts',(126.615569582305,34.6418953961436,29.2547104726883));
#44016=CARTESIAN_POINT('Ctrl Pts',(126.60958560063,35.0140739890281,29.230981199355));
#44017=CARTESIAN_POINT('Ctrl Pts',(126.610564120949,35.0826634886745,29.2266490881475));
#44018=CARTESIAN_POINT('Ctrl Pts',(126.615680867445,35.1972773075019,29.2195242613778));
#44019=CARTESIAN_POINT('Ctrl Pts',(126.618680020258,35.2433309753297,29.2166924126869));
#44020=CARTESIAN_POINT('Ctrl Pts',(126.624323894424,35.3092167976886,29.2126986865175));
#44021=CARTESIAN_POINT('Ctrl Pts',(126.62620501545,35.3291073421322,29.2115005575774));
#44022=CARTESIAN_POINT('Ctrl Pts',(126.629803075381,35.3638706358091,29.209421125578));
#44023=CARTESIAN_POINT('Ctrl Pts',(126.631442850777,35.3787504627889,29.2085357966238));
#44024=CARTESIAN_POINT('Ctrl Pts',(126.635258912827,35.411391072945,29.2066044350555));
#44025=CARTESIAN_POINT('Ctrl Pts',(126.63747730604,35.4291460850888,29.2055606746302));
#44026=CARTESIAN_POINT('Ctrl Pts',(126.644464772336,35.4816856185259,29.2024900568527));
#44027=CARTESIAN_POINT('Ctrl Pts',(126.649633917006,35.5164155420274,29.2004837357089));
#44028=CARTESIAN_POINT('Ctrl Pts',(126.68544509628,35.7337713432637,29.188039763442));
#44029=CARTESIAN_POINT('Ctrl Pts',(126.730472684173,35.9137287668374,29.1782253639928));
#44030=CARTESIAN_POINT('Ctrl Pts',(126.799998047657,36.1186440237703,29.1667563461289));
#44031=CARTESIAN_POINT('Ctrl Pts',(126.810419332266,36.148020614536,29.165105224614));
#44032=CARTESIAN_POINT('Ctrl Pts',(126.821241934448,36.17724348509,29.1634527466974));
#44033=CARTESIAN_POINT('',(127.462900812983,37.2480064007332,30.));
#44034=CARTESIAN_POINT('Origin',(130.,35.,30.));
#44035=CARTESIAN_POINT('Ctrl Pts',(127.462900812983,37.2480064007329,29.9999999999999));
#44036=CARTESIAN_POINT('Ctrl Pts',(127.478117849802,37.2651803428221,29.9985918573257));
#44037=CARTESIAN_POINT('Ctrl Pts',(127.493508854484,37.2821993118563,29.9971740439912));
#44038=CARTESIAN_POINT('Ctrl Pts',(127.658101727054,37.4605282678587,29.9820908018274));
#44039=CARTESIAN_POINT('Ctrl Pts',(127.822472262042,37.6071160583103,29.9677449542209));
#44040=CARTESIAN_POINT('Ctrl Pts',(128.101798222967,37.8112586652844,29.9455445514229));
#44041=CARTESIAN_POINT('Ctrl Pts',(128.207820718677,37.8800075148949,29.937532612846));
#44042=CARTESIAN_POINT('Ctrl Pts',(128.390146127328,37.9842570301074,29.9245087482649));
#44043=CARTESIAN_POINT('Ctrl Pts',(128.464372478913,38.0231224647332,29.9193981623304));
#44044=CARTESIAN_POINT('Ctrl Pts',(128.572286864749,38.0746256244688,29.9122349161533));
#44045=CARTESIAN_POINT('Ctrl Pts',(128.604849527171,38.0895376404814,29.9101068158507));
#44046=CARTESIAN_POINT('Ctrl Pts',(128.662342021915,38.1147718598676,29.9064061054776));
#44047=CARTESIAN_POINT('Ctrl Pts',(128.6871697164,38.1253174740691,29.9048261741106));
#44048=CARTESIAN_POINT('Ctrl Pts',(128.739289134993,38.1467246134861,29.901546238517));
#44049=CARTESIAN_POINT('Ctrl Pts',(128.766601553822,38.1575300519343,29.8998481808724));
#44050=CARTESIAN_POINT('Ctrl Pts',(128.839348796321,38.1852225998621,29.8953777787254));
#44051=CARTESIAN_POINT('Ctrl Pts',(128.88501206646,38.2014928486645,29.8926253785995));
#44052=CARTESIAN_POINT('Ctrl Pts',(129.181085841966,38.2998831524024,29.8750894211646));
#44053=CARTESIAN_POINT('Ctrl Pts',(129.439994122515,38.3535432528616,29.8612585804505));
#44054=CARTESIAN_POINT('Ctrl Pts',(129.844770929947,38.3892037207016,29.8395615335009));
#44055=CARTESIAN_POINT('Ctrl Pts',(129.987661194082,38.3927331741491,29.8318668538269));
#44056=CARTESIAN_POINT('Ctrl Pts',(130.166121615511,38.3858664096661,29.8217768437165));
#44057=CARTESIAN_POINT('Ctrl Pts',(130.201884035525,38.3839223339755,29.8197304548625));
#44058=CARTESIAN_POINT('Ctrl Pts',(130.25582799341,38.380131761888,29.8165979455674));
#44059=CARTESIAN_POINT('Ctrl Pts',(130.274037449334,38.3787042093047,29.8155326381145));
#44060=CARTESIAN_POINT('Ctrl Pts',(130.307341319321,38.3758223168553,29.8135683816065));
#44061=CARTESIAN_POINT('Ctrl Pts',(130.322438762146,38.3744137598175,29.8126718443432));
#44062=CARTESIAN_POINT('Ctrl Pts',(130.357305303917,38.370924666362,29.8105872841581));
#44063=CARTESIAN_POINT('Ctrl Pts',(130.377065932835,38.3687715011547,29.8093955407772));
#44064=CARTESIAN_POINT('Ctrl Pts',(130.442981566568,38.3610019644911,29.805388279165));
#44065=CARTESIAN_POINT('Ctrl Pts',(130.489037976877,38.3546100044673,29.8025359538501));
#44066=CARTESIAN_POINT('Ctrl Pts',(130.741906137056,38.3141977742004,29.7866376125801));
#44067=CARTESIAN_POINT('Ctrl Pts',(130.945343166554,38.2620011290399,29.772997467042));
#44068=CARTESIAN_POINT('Ctrl Pts',(131.295610522636,38.1365897490847,29.7491192806637));
#44069=CARTESIAN_POINT('Ctrl Pts',(131.444450934583,38.0708913578075,29.7388296333424));
#44070=CARTESIAN_POINT('Ctrl Pts',(131.644653186378,37.9647310777899,29.7249343755634));
#44071=CARTESIAN_POINT('Ctrl Pts',(131.700427393834,37.9330976748062,29.7210549320412));
#44072=CARTESIAN_POINT('Ctrl Pts',(131.782990151824,37.8831234489878,29.7152972335149));
#44073=CARTESIAN_POINT('Ctrl Pts',(131.81046522756,37.8659501865912,29.7133785464316));
#44074=CARTESIAN_POINT('Ctrl Pts',(131.857834388023,37.8353890598971,29.7100648297688));
#44075=CARTESIAN_POINT('Ctrl Pts',(131.877840107333,37.822179354524,29.7086634942706));
#44076=CARTESIAN_POINT('Ctrl Pts',(131.922792188439,37.7918080111974,29.7055097554022));
#44077=CARTESIAN_POINT('Ctrl Pts',(131.947652310103,37.7745220012697,29.7037620873418));
#44078=CARTESIAN_POINT('Ctrl Pts',(132.014435168709,37.7267458256772,29.6990550485609));
#44079=CARTESIAN_POINT('Ctrl Pts',(132.055896373624,37.6956228119713,29.6961195437228));
#44080=CARTESIAN_POINT('Ctrl Pts',(132.285675537508,37.5147514640486,29.6797402903712));
#44081=CARTESIAN_POINT('Ctrl Pts',(132.458343912125,37.3462403951417,29.6670640870943));
#44082=CARTESIAN_POINT('Ctrl Pts',(132.691009760089,37.0650279231619,29.6476875016497));
#44083=CARTESIAN_POINT('Ctrl Pts',(132.764955498168,36.9649151355708,29.6410602893032));
#44084=CARTESIAN_POINT('Ctrl Pts',(132.87058883755,36.8040941486077,29.6304724136616));
#44085=CARTESIAN_POINT('Ctrl Pts',(132.906225027213,36.7461073381031,29.626664916079));
#44086=CARTESIAN_POINT('Ctrl Pts',(132.951554711617,36.6671114233039,29.6214382482017));
#44087=CARTESIAN_POINT('Ctrl Pts',(132.962815444465,36.6470155716039,29.6201052809632));
#44088=CARTESIAN_POINT('Ctrl Pts',(132.981281728464,36.6132584466571,29.6178579851844));
#44089=CARTESIAN_POINT('Ctrl Pts',(132.98860052641,36.5996594770144,29.6169504770649));
#44090=CARTESIAN_POINT('Ctrl Pts',(133.00349885901,36.5715179256244,29.6150670479207));
#44091=CARTESIAN_POINT('Ctrl Pts',(133.01106620254,36.5569695840981,29.6140904680651));
#44092=CARTESIAN_POINT('Ctrl Pts',(133.031221032418,36.517525081759,29.6114360571237));
#44093=CARTESIAN_POINT('Ctrl Pts',(133.043606956059,36.4925280260277,29.6097468025566));
#44094=CARTESIAN_POINT('Ctrl Pts',(133.111976697401,36.3501545721132,29.6000974754614));
#44095=CARTESIAN_POINT('Ctrl Pts',(133.161473464185,36.2297949978379,29.5918371166948));
#44096=CARTESIAN_POINT('Ctrl Pts',(133.271856857366,35.9102901768983,29.5701329181773));
#44097=CARTESIAN_POINT('Ctrl Pts',(133.321546649492,35.7078245061683,29.5566221564843));
#44098=CARTESIAN_POINT('Ctrl Pts',(133.368732334231,35.3927647529445,29.5366175010145));
#44099=CARTESIAN_POINT('Ctrl Pts',(133.379748476982,35.2827118151283,29.529806863054));
#44100=CARTESIAN_POINT('Ctrl Pts',(133.387350997142,35.1333432881135,29.5208120952739));
#44101=CARTESIAN_POINT('Ctrl Pts',(133.38866140773,35.0943465197464,29.5184862352233));
#44102=CARTESIAN_POINT('Ctrl Pts',(133.389742338794,35.0281383747375,29.5145740616786));
#44103=CARTESIAN_POINT('Ctrl Pts',(133.389859005575,35.0009372713536,29.5129772495642));
#44104=CARTESIAN_POINT('Ctrl Pts',(133.389433506699,34.9460198171519,29.509773562024));
#44105=CARTESIAN_POINT('Ctrl Pts',(133.388878790023,34.9183056313543,29.5081671970383));
#44106=CARTESIAN_POINT('Ctrl Pts',(133.386638238652,34.848918021057,29.504169709681));
#44107=CARTESIAN_POINT('Ctrl Pts',(133.384523125122,34.8072624702924,29.5017919413971));
#44108=CARTESIAN_POINT('Ctrl Pts',(133.372795943351,34.638037008602,29.4922100853011));
#44109=CARTESIAN_POINT('Ctrl Pts',(133.356734698258,34.5110149166854,29.4852030982287));
#44110=CARTESIAN_POINT('Ctrl Pts',(133.291922423045,34.1595968896442,29.4659731802995));
#44111=CARTESIAN_POINT('Ctrl Pts',(133.227524837606,33.9388188216643,29.4541002424322));
#44112=CARTESIAN_POINT('Ctrl Pts',(133.106664216691,33.6407526985984,29.4366497275216));
#44113=CARTESIAN_POINT('Ctrl Pts',(133.068525500484,33.5567175384529,29.4315533664364));
#44114=CARTESIAN_POINT('Ctrl Pts',(133.015654636829,33.4518175726498,29.4248379527263));
#44115=CARTESIAN_POINT('Ctrl Pts',(133.004047409048,33.429413867341,29.4233824938021));
#44116=CARTESIAN_POINT('Ctrl Pts',(132.984765846177,33.3931933448236,29.4209913413125));
#44117=CARTESIAN_POINT('Ctrl Pts',(132.977242832909,33.3792964860299,29.4200646774961));
#44118=CARTESIAN_POINT('Ctrl Pts',(132.962911506226,33.3532595244232,29.418310096787));
#44119=CARTESIAN_POINT('Ctrl Pts',(132.95612505258,33.3411077654539,29.4174836166903));
#44120=CARTESIAN_POINT('Ctrl Pts',(132.937807246257,33.3087774265661,29.4152650857196));
#44121=CARTESIAN_POINT('Ctrl Pts',(132.926143087348,33.2886754323102,29.4138650891572));
#44122=CARTESIAN_POINT('Ctrl Pts',(132.881232139369,33.213077643167,29.4085263680866));
#44123=CARTESIAN_POINT('Ctrl Pts',(132.846607438647,33.1584204749311,29.404514713979));
#44124=CARTESIAN_POINT('Ctrl Pts',(132.702154559927,32.9442084447895,29.3882742934291));
#44125=CARTESIAN_POINT('Ctrl Pts',(132.580305908436,32.7932066257174,29.3756642189649));
#44126=CARTESIAN_POINT('Ctrl Pts',(132.326575404897,32.5286987145862,29.3521543999739));
#44127=CARTESIAN_POINT('Ctrl Pts',(132.197539714227,32.4132808873563,29.3412484409462));
#44128=CARTESIAN_POINT('Ctrl Pts',(132.018417709447,32.2761847322142,29.3275238950633));
#44129=CARTESIAN_POINT('Ctrl Pts',(131.975846736311,32.2451479526931,29.3243549625648));
#44130=CARTESIAN_POINT('Ctrl Pts',(131.907849366188,32.1979612603903,29.3194346321943));
#44131=CARTESIAN_POINT('Ctrl Pts',(131.882903049924,32.1811373757809,29.3176583229723));
#44132=CARTESIAN_POINT('Ctrl Pts',(131.835536862737,32.15010284226,29.3143382953861));
#44133=CARTESIAN_POINT('Ctrl Pts',(131.813167807197,32.1358191492085,29.3127919737489));
#44134=CARTESIAN_POINT('Ctrl Pts',(131.762026658838,32.1040023894909,29.309304123544));
#44135=CARTESIAN_POINT('Ctrl Pts',(131.733156058135,32.0866324809796,29.3073685690024));
#44136=CARTESIAN_POINT('Ctrl Pts',(131.64200786455,32.0336279892345,29.3013570985733));
#44137=CARTESIAN_POINT('Ctrl Pts',(131.578853086716,31.9995372597811,29.2973349803857));
#44138=CARTESIAN_POINT('Ctrl Pts',(131.252041653444,31.8363041766667,29.2771424565233));
#44139=CARTESIAN_POINT('Ctrl Pts',(130.973518179817,31.7398110085746,29.2620654744137));
#44140=CARTESIAN_POINT('Ctrl Pts',(130.619654923719,31.6666788248659,29.242512375996));
#44141=CARTESIAN_POINT('Ctrl Pts',(130.552861772203,31.6549521350261,29.238798627151));
#44142=CARTESIAN_POINT('Ctrl Pts',(130.440488724307,31.6386806582955,29.232448062967));
#44143=CARTESIAN_POINT('Ctrl Pts',(130.395086070095,31.6330422318763,29.229854401965));
#44144=CARTESIAN_POINT('Ctrl Pts',(130.329794477347,31.6262726009943,29.2260672936508));
#44145=CARTESIAN_POINT('Ctrl Pts',(130.309986230686,31.6243949497358,29.2249108177791));
#44146=CARTESIAN_POINT('Ctrl Pts',(130.275238890605,31.6214096145749,29.2228671719588));
#44147=CARTESIAN_POINT('Ctrl Pts',(130.26030718412,31.6202263983687,29.2219840665314));
#44148=CARTESIAN_POINT('Ctrl Pts',(130.22738442505,31.6178370109096,29.2200256982347));
#44149=CARTESIAN_POINT('Ctrl Pts',(130.209391533693,31.61667540501,29.2189482036346));
#44150=CARTESIAN_POINT('Ctrl Pts',(130.156968170767,31.6137107692029,29.2157895394178));
#44151=CARTESIAN_POINT('Ctrl Pts',(130.122519361727,31.6122894795468,29.2136896584942));
#44152=CARTESIAN_POINT('Ctrl Pts',(129.895418420125,31.6063880329707,29.1997124205796));
#44153=CARTESIAN_POINT('Ctrl Pts',(129.702718164474,31.6178183357135,29.1872387209001));
#44154=CARTESIAN_POINT('Ctrl Pts',(129.359552834562,31.6677365880789,29.1648974729263));
#44155=CARTESIAN_POINT('Ctrl Pts',(129.208736362133,31.70029380636,29.1550298705524));
#44156=CARTESIAN_POINT('Ctrl Pts',(128.969964925965,31.7691579384153,29.1395374135534));
#44157=CARTESIAN_POINT('Ctrl Pts',(128.880407081276,31.7990896708485,29.1337544714835));
#44158=CARTESIAN_POINT('Ctrl Pts',(128.757503538842,31.8459570095804,29.1258603909076));
#44159=CARTESIAN_POINT('Ctrl Pts',(128.723017450146,31.8597610961331,29.1236498622348));
#44160=CARTESIAN_POINT('Ctrl Pts',(128.663881751335,31.8845672586581,29.1198657557421));
#44161=CARTESIAN_POINT('Ctrl Pts',(128.639124357407,31.8953018362051,29.1182834958549));
#44162=CARTESIAN_POINT('Ctrl Pts',(128.588523152817,31.9179636373577,29.115052625006));
#44163=CARTESIAN_POINT('Ctrl Pts',(128.562696050417,31.9299230532415,29.1134052517419));
#44164=CARTESIAN_POINT('Ctrl Pts',(128.496561847067,31.9615644589303,29.1091893537274));
#44165=CARTESIAN_POINT('Ctrl Pts',(128.456488609414,31.9817240569353,29.1066372099883));
#44166=CARTESIAN_POINT('Ctrl Pts',(128.25432265732,32.0885071927156,29.0937551582498));
#44167=CARTESIAN_POINT('Ctrl Pts',(128.099061540752,32.1874170745686,29.0838614437335));
#44168=CARTESIAN_POINT('Ctrl Pts',(127.811353682883,32.4054616617986,29.0646669692373));
#44169=CARTESIAN_POINT('Ctrl Pts',(127.678752245693,32.523388502055,29.0553820673352));
#44170=CARTESIAN_POINT('Ctrl Pts',(127.498935769655,32.7104890326141,29.0412242664885));
#44171=CARTESIAN_POINT('Ctrl Pts',(127.444074420526,32.7719010017034,29.0366527478963));
#44172=CARTESIAN_POINT('Ctrl Pts',(127.375879876727,32.85407422525,29.0305396321504));
#44173=CARTESIAN_POINT('Ctrl Pts',(127.360457615728,32.873072690533,29.0291265128249));
#44174=CARTESIAN_POINT('Ctrl Pts',(127.335478339087,32.9045344236397,29.0267836639857));
#44175=CARTESIAN_POINT('Ctrl Pts',(127.325799554906,32.9169004762236,29.0258621324421));
#44176=CARTESIAN_POINT('Ctrl Pts',(127.307612713588,32.9404724540948,29.024103316386));
#44177=CARTESIAN_POINT('Ctrl Pts',(127.299087827608,32.9516649605973,29.0232672841928));
#44178=CARTESIAN_POINT('Ctrl Pts',(127.276172125178,32.9821432638267,29.0209889823996));
#44179=CARTESIAN_POINT('Ctrl Pts',(127.261916869223,33.0015293857175,29.019538010938));
#44180=CARTESIAN_POINT('Ctrl Pts',(127.206137571674,33.0791023721337,29.0137301344299));
#44181=CARTESIAN_POINT('Ctrl Pts',(127.166254566074,33.1384414168332,29.0092836109307));
#44182=CARTESIAN_POINT('Ctrl Pts',(127.02823455371,33.3585153431092,28.9928991426864));
#44183=CARTESIAN_POINT('Ctrl Pts',(126.941657351632,33.5260935052429,28.9806427878136));
#44184=CARTESIAN_POINT('Ctrl Pts',(126.798563933177,33.8706771973782,28.9567221888633));
#44185=CARTESIAN_POINT('Ctrl Pts',(126.741753844291,34.0468935515748,28.9450928169622));
#44186=CARTESIAN_POINT('Ctrl Pts',(126.68944108561,34.2702156167127,28.9312282178701));
#44187=CARTESIAN_POINT('Ctrl Pts',(126.680145061556,34.3137427290265,28.9285644142146));
#44188=CARTESIAN_POINT('Ctrl Pts',(126.666330871604,34.3852968031259,28.9242464007384));
#44189=CARTESIAN_POINT('Ctrl Pts',(126.661302993951,34.4132187351067,28.9225764757834));
#44190=CARTESIAN_POINT('Ctrl Pts',(126.652177297309,34.467819090193,28.9193393158131));
#44191=CARTESIAN_POINT('Ctrl Pts',(126.648046417002,34.4944897541941,28.9177711615604));
#44192=CARTESIAN_POINT('Ctrl Pts',(126.638966772336,34.5581272555422,28.914059226215));
#44193=CARTESIAN_POINT('Ctrl Pts',(126.634308647977,34.5951324183887,28.9119245724412));
#44194=CARTESIAN_POINT('Ctrl Pts',(126.620540178399,34.7212801693608,28.9047218423056));
#44195=CARTESIAN_POINT('Ctrl Pts',(126.614353322164,34.8107070684153,28.899742453578));
#44196=CARTESIAN_POINT('Ctrl Pts',(126.603771081865,35.1702684500139,28.8800694472354));
#44197=CARTESIAN_POINT('Ctrl Pts',(126.628122353902,35.4402203034712,28.8661653493926));
#44198=CARTESIAN_POINT('Ctrl Pts',(126.697999968844,35.7691423114793,28.8479565103754));
#44199=CARTESIAN_POINT('Ctrl Pts',(126.713643286946,35.8334523266386,28.8443289963956));
#44200=CARTESIAN_POINT('Ctrl Pts',(126.743057386354,35.9406119691821,28.8381106137182));
#44201=CARTESIAN_POINT('Ctrl Pts',(126.755817688955,35.9837208943478,28.8355608235598));
#44202=CARTESIAN_POINT('Ctrl Pts',(126.775405856459,36.0453645009853,28.8318283427567));
#44203=CARTESIAN_POINT('Ctrl Pts',(126.781544802124,36.0641148570927,28.8306813769202));
#44204=CARTESIAN_POINT('Ctrl Pts',(126.792618524998,36.0969650256828,28.8286496727444));
#44205=CARTESIAN_POINT('Ctrl Pts',(126.797483360558,36.1110874651656,28.8277688806398));
#44206=CARTESIAN_POINT('Ctrl Pts',(126.808444365314,36.1422367254611,28.8258095158838));
#44207=CARTESIAN_POINT('Ctrl Pts',(126.814583471908,36.1592470040824,28.8247286292288));
#44208=CARTESIAN_POINT('Ctrl Pts',(126.820986075039,36.1765524481033,28.823618425201));
#44209=CARTESIAN_POINT('Ctrl Pts',(126.821113968604,36.1768979554873,28.8235962553991));
#44210=CARTESIAN_POINT('Ctrl Pts',(126.821241918358,36.1772434416436,28.8235740826546));
#44211=CARTESIAN_POINT('Origin',(-10.,35.,32.7603849714045));
#44212=CARTESIAN_POINT('',(-7.51282733495085,38.2405550657615,18.0469656644349));
#44213=CARTESIAN_POINT('',(-7.51282733495087,38.2405550657615,17.9425398374177));
#44214=CARTESIAN_POINT('',(-7.51282733495086,38.2405550657615,32.7603849714045));
#44215=CARTESIAN_POINT('',(-14.0827629539364,34.9944901030589,17.1353849829093));
#44216=CARTESIAN_POINT('Ctrl Pts',(-7.51282733495087,38.2405550657615,17.9425398374177));
#44217=CARTESIAN_POINT('Ctrl Pts',(-7.4183033415916,38.1680065400603,17.9367380921735));
#44218=CARTESIAN_POINT('Ctrl Pts',(-7.32687001393603,38.0912526206094,17.9309363469293));
#44219=CARTESIAN_POINT('Ctrl Pts',(-7.23891909304243,38.0105908432124,17.925134601685));
#44220=CARTESIAN_POINT('Ctrl Pts',(-7.15101721148065,37.929974040895,17.9193360913553));
#44221=CARTESIAN_POINT('Ctrl Pts',(-7.0665941758643,37.8454539901771,17.9135375810256));
#44222=CARTESIAN_POINT('Ctrl Pts',(-6.98600847518456,37.7573683265644,17.9077390706959));
#44223=CARTESIAN_POINT('Ctrl Pts',(-6.9054455566571,37.669307565397,17.9019421996465));
#44224=CARTESIAN_POINT('Ctrl Pts',(-6.82871809216569,37.5776834973517,17.896145328597));
#44225=CARTESIAN_POINT('Ctrl Pts',(-6.75614709878714,37.482869983566,17.8903484575475));
#44226=CARTESIAN_POINT('Ctrl Pts',(-6.68357939025863,37.3880607614147,17.8845518488873));
#44227=CARTESIAN_POINT('Ctrl Pts',(-6.61516802742511,37.2900627057404,17.8787552402272));
#44228=CARTESIAN_POINT('Ctrl Pts',(-6.55119276284196,37.1892815353276,17.872958631567));
#44229=CARTESIAN_POINT('Ctrl Pts',(-6.48720520356606,37.0884809969054,17.8671609089212));
#44230=CARTESIAN_POINT('Ctrl Pts',(-6.42765565715021,36.984896625763,17.8613631862754));
#44231=CARTESIAN_POINT('Ctrl Pts',(-6.37277934104189,36.8789612266429,17.8555654636297));
#44232=CARTESIAN_POINT('Ctrl Pts',(-6.31784510984411,36.7729140259561,17.8497616222127));
#44233=CARTESIAN_POINT('Ctrl Pts',(-6.26759414824649,36.6645112056742,17.8439577807956));
#44234=CARTESIAN_POINT('Ctrl Pts',(-6.22221477081377,36.5542084037034,17.8381539393786));
#44235=CARTESIAN_POINT('Ctrl Pts',(-6.17681086915101,36.4438459911465,17.8323469614104));
#44236=CARTESIAN_POINT('Ctrl Pts',(-6.13628393538455,36.3315819363009,17.8265399834421));
#44237=CARTESIAN_POINT('Ctrl Pts',(-6.10077276455028,36.2178883226007,17.8207330054739));
#44238=CARTESIAN_POINT('Ctrl Pts',(-6.06520417671164,36.104010880923,17.8149166383677));
#44239=CARTESIAN_POINT('Ctrl Pts',(-6.03466765964787,35.988699658222,17.8091002712616));
#44240=CARTESIAN_POINT('Ctrl Pts',(-6.00925125311316,35.8724387882374,17.8032839041555));
#44241=CARTESIAN_POINT('Ctrl Pts',(-5.98745160169316,35.7727218421778,17.7982952061949));
#44242=CARTESIAN_POINT('Ctrl Pts',(-5.96941771976481,35.6723065937043,17.7933065082343));
#44243=CARTESIAN_POINT('Ctrl Pts',(-5.95517468308408,35.571500792332,17.7883178102738));
#44244=CARTESIAN_POINT('Ctrl Pts',(-5.93851904215847,35.4536196642752,17.7824840850802));
#44245=CARTESIAN_POINT('Ctrl Pts',(-5.92699445772989,35.3348226640355,17.7766503598866));
#44246=CARTESIAN_POINT('Ctrl Pts',(-5.92069312782201,35.2155932341272,17.770816634693));
#44247=CARTESIAN_POINT('Ctrl Pts',(-5.91439975786786,35.0965144169879,17.7649902787665));
#44248=CARTESIAN_POINT('Ctrl Pts',(-5.91331653925813,34.9770046594567,17.7591639228399));
#44249=CARTESIAN_POINT('Ctrl Pts',(-5.91748428809018,34.8575554072299,17.7533375669133));
#44250=CARTESIAN_POINT('Ctrl Pts',(-5.92164784806494,34.7382262092316,17.7475170668515));
#44251=CARTESIAN_POINT('Ctrl Pts',(-5.93105186156511,34.6189577997927,17.7416965667897));
#44252=CARTESIAN_POINT('Ctrl Pts',(-5.94568515168971,34.5002439487403,17.7358760667279));
#44253=CARTESIAN_POINT('Ctrl Pts',(-5.96083652425654,34.3773271083836,17.7298494955186));
#44254=CARTESIAN_POINT('Ctrl Pts',(-5.98159433369207,34.2550052647982,17.7238229243093));
#44255=CARTESIAN_POINT('Ctrl Pts',(-6.00788729115695,34.1338238516942,17.7177963531001));
#44256=CARTESIAN_POINT('Ctrl Pts',(-6.03325201513153,34.016920566914,17.7119825409627));
#44257=CARTESIAN_POINT('Ctrl Pts',(-6.06376758361259,33.9010789832808,17.7061687288253));
#44258=CARTESIAN_POINT('Ctrl Pts',(-6.09931768119087,33.7867801321566,17.700354916688));
#44259=CARTESIAN_POINT('Ctrl Pts',(-6.13486209666282,33.6724995498494,17.6945420337942));
#44260=CARTESIAN_POINT('Ctrl Pts',(-6.17543931998105,33.5597615979302,17.6887291509004));
#44261=CARTESIAN_POINT('Ctrl Pts',(-6.22088303717803,33.4490325660056,17.6829162680066));
#44262=CARTESIAN_POINT('Ctrl Pts',(-6.26633011389279,33.3382953482156,17.6771029553837));
#44263=CARTESIAN_POINT('Ctrl Pts',(-6.31664424526961,33.2295677220171,17.6712896427609));
#44264=CARTESIAN_POINT('Ctrl Pts',(-6.37161104484388,33.1232958171035,17.6654763301381));
#44265=CARTESIAN_POINT('Ctrl Pts',(-6.42659475686175,33.0169912139501,17.6596612288479));
#44266=CARTESIAN_POINT('Ctrl Pts',(-6.48623379744393,32.9131441959916,17.6538461275577));
#44267=CARTESIAN_POINT('Ctrl Pts',(-6.55026823437055,32.8121755680112,17.6480310262675));
#44268=CARTESIAN_POINT('Ctrl Pts',(-6.61437141346114,32.7110985483229,17.6422096823575));
#44269=CARTESIAN_POINT('Ctrl Pts',(-6.6828791897496,32.6129064304381,17.6363883384474));
#44270=CARTESIAN_POINT('Ctrl Pts',(-6.75548868636104,32.5179904642269,17.6305669945374));
#44271=CARTESIAN_POINT('Ctrl Pts',(-6.82814457559643,32.4230138530458,17.624741931177));
#44272=CARTESIAN_POINT('Ctrl Pts',(-6.90490714451128,32.3313178741207,17.6189168678166));
#44273=CARTESIAN_POINT('Ctrl Pts',(-6.98543474817405,32.2432589271962,17.6130918044561));
#44274=CARTESIAN_POINT('Ctrl Pts',(-7.06607455930401,32.1550772786023,17.6072586244304));
#44275=CARTESIAN_POINT('Ctrl Pts',(-7.1504895902578,32.0705430644841,17.6014254444047));
#44276=CARTESIAN_POINT('Ctrl Pts',(-7.23830297666916,31.9899743271318,17.595592264379));
#44277=CARTESIAN_POINT('Ctrl Pts',(-7.26015105310161,31.9699287281215,17.5941409621545));
#44278=CARTESIAN_POINT('Ctrl Pts',(-7.28220934456464,31.9501283972475,17.5926896599299));
#44279=CARTESIAN_POINT('Ctrl Pts',(-7.30447175887145,31.9305778228992,17.5912383577053));
#44280=CARTESIAN_POINT('Ctrl Pts',(-7.39387101201482,31.8520685147364,17.5854103584069));
#44281=CARTESIAN_POINT('Ctrl Pts',(-7.48684416404283,31.7773442700337,17.5795823591084));
#44282=CARTESIAN_POINT('Ctrl Pts',(-7.58303761970974,31.706746615843,17.57375435981));
#44283=CARTESIAN_POINT('Ctrl Pts',(-7.67911152471163,31.6362367014725,17.5679336036362));
#44284=CARTESIAN_POINT('Ctrl Pts',(-7.77839744686426,31.56984341552,17.5621128474624));
#44285=CARTESIAN_POINT('Ctrl Pts',(-7.8805069604902,31.5078696680293,17.5562920912886));
#44286=CARTESIAN_POINT('Ctrl Pts',(-7.9825160475301,31.44595687286,17.5504770599357));
#44287=CARTESIAN_POINT('Ctrl Pts',(-8.0873428547323,31.3884551787733,17.5446620285827));
#44288=CARTESIAN_POINT('Ctrl Pts',(-8.19456855147211,31.3356252532435,17.5388469972298));
#44289=CARTESIAN_POINT('Ctrl Pts',(-8.30573362625101,31.2808544025926,17.5328183267259));
#44290=CARTESIAN_POINT('Ctrl Pts',(-8.41947687947959,31.2311054465056,17.526789656222));
#44291=CARTESIAN_POINT('Ctrl Pts',(-8.53530150854896,31.1866178621674,17.5207609857182));
#44292=CARTESIAN_POINT('Ctrl Pts',(-8.64690001636399,31.1437535070787,17.5149522847731));
#44293=CARTESIAN_POINT('Ctrl Pts',(-8.76043025743789,31.1057734553835,17.509143583828));
#44294=CARTESIAN_POINT('Ctrl Pts',(-8.87542649629038,31.0728433396725,17.5033348828829));
#44295=CARTESIAN_POINT('Ctrl Pts',(-8.99040711539206,31.0399176968052,17.4975269709241));
#44296=CARTESIAN_POINT('Ctrl Pts',(-9.10685294459492,31.0120407379528,17.4917190589654));
#44297=CARTESIAN_POINT('Ctrl Pts',(-9.22428325402143,30.9893281697441,17.4859111470066));
#44298=CARTESIAN_POINT('Ctrl Pts',(-9.34172518549361,30.9666133536786,17.4801026602404));
#44299=CARTESIAN_POINT('Ctrl Pts',(-9.46015139082179,30.9490640219931,17.4742941734742));
#44300=CARTESIAN_POINT('Ctrl Pts',(-9.57907174529857,30.9367446050742,17.468485686708));
#44301=CARTESIAN_POINT('Ctrl Pts',(-9.69803179132901,30.9244210763545,17.4626752612672));
#44302=CARTESIAN_POINT('Ctrl Pts',(-9.81748590941725,30.9173309761372,17.4568648358264));
#44303=CARTESIAN_POINT('Ctrl Pts',(-9.93694029613936,30.915486751919,17.4510544103857));
#44304=CARTESIAN_POINT('Ctrl Pts',(-10.0565280337012,30.913640468933,17.4452374985769));
#44305=CARTESIAN_POINT('Ctrl Pts',(-10.1761156328021,30.9170517577107,17.4394205867682));
#44306=CARTESIAN_POINT('Ctrl Pts',(-10.2952105629053,30.9256809497108,17.4336036749594));
#44307=CARTESIAN_POINT('Ctrl Pts',(-10.4143844498564,30.9343158626414,17.427782906689));
#44308=CARTESIAN_POINT('Ctrl Pts',(-10.5330646134808,30.9481755212524,17.4219621384187));
#44309=CARTESIAN_POINT('Ctrl Pts',(-10.6507665506426,30.9671687493072,17.4161413701484));
#44310=CARTESIAN_POINT('Ctrl Pts',(-10.7686372902992,30.9861892165421,17.4103122540103));
#44311=CARTESIAN_POINT('Ctrl Pts',(-10.8855266056535,31.0103578659512,17.4044831378722));
#44312=CARTESIAN_POINT('Ctrl Pts',(-11.0009628848836,31.0395330700679,17.3986540217341));
#44313=CARTESIAN_POINT('Ctrl Pts',(-11.0306357387891,31.0470325457544,17.397155649535));
#44314=CARTESIAN_POINT('Ctrl Pts',(-11.0602126778042,31.0548625757694,17.395657277336));
#44315=CARTESIAN_POINT('Ctrl Pts',(-11.0896858991661,31.0630202386654,17.3941589051369));
#44316=CARTESIAN_POINT('Ctrl Pts',(-11.2031708726653,31.0944308587056,17.3883895076483));
#44317=CARTESIAN_POINT('Ctrl Pts',(-11.3154990757746,31.1308085462832,17.3826201101598));
#44318=CARTESIAN_POINT('Ctrl Pts',(-11.4261981271612,31.1720522597504,17.3768507126713));
#44319=CARTESIAN_POINT('Ctrl Pts',(-11.5367558093482,31.2132433025696,17.3710886830427));
#44320=CARTESIAN_POINT('Ctrl Pts',(-11.6456880894902,31.2592878728293,17.3653266534141));
#44321=CARTESIAN_POINT('Ctrl Pts',(-11.7525351267066,31.3100344676868,17.3595646237854));
#44322=CARTESIAN_POINT('Ctrl Pts',(-11.8592748935706,31.3607301148975,17.3538083790149));
#44323=CARTESIAN_POINT('Ctrl Pts',(-11.963933206448,31.4161182219792,17.3480521342444));
#44324=CARTESIAN_POINT('Ctrl Pts',(-12.0660683609068,31.4759985062347,17.3422958894739));
#44325=CARTESIAN_POINT('Ctrl Pts',(-12.1734278736667,31.5389417521295,17.3362452046029));
#44326=CARTESIAN_POINT('Ctrl Pts',(-12.2779988274438,31.6068487403076,17.3301945197318));
#44327=CARTESIAN_POINT('Ctrl Pts',(-12.3792952275086,31.6794308890862,17.3241438348608));
#44328=CARTESIAN_POINT('Ctrl Pts',(-12.4755596833424,31.7484074869806,17.3183937204819));
#44329=CARTESIAN_POINT('Ctrl Pts',(-12.5688667050551,31.8216056715209,17.3126436061031));
#44330=CARTESIAN_POINT('Ctrl Pts',(-12.6588281203624,31.8987328353768,17.3068934917243));
#44331=CARTESIAN_POINT('Ctrl Pts',(-12.7487797405037,31.9758516014838,17.3011440034286));
#44332=CARTESIAN_POINT('Ctrl Pts',(-12.8353861617372,32.0568982255982,17.2953945151329));
#44333=CARTESIAN_POINT('Ctrl Pts',(-12.9182926742957,32.1415401232216,17.2896450268373));
#44334=CARTESIAN_POINT('Ctrl Pts',(-13.0012106444888,32.2261937183089,17.2838947439654));
#44335=CARTESIAN_POINT('Ctrl Pts',(-13.0804273978305,32.3144432769193,17.2781444610936));
#44336=CARTESIAN_POINT('Ctrl Pts',(-13.1556259804814,32.4059202650437,17.2723941782218));
#44337=CARTESIAN_POINT('Ctrl Pts',(-13.2308535373257,32.4974324994701,17.2666416797523));
#44338=CARTESIAN_POINT('Ctrl Pts',(-13.3020595810806,32.5921743139375,17.2608891812828));
#44339=CARTESIAN_POINT('Ctrl Pts',(-13.3689687108363,32.6897457227816,17.2551366828132));
#44340=CARTESIAN_POINT('Ctrl Pts',(-13.4359614234129,32.7874390177363,17.2493769983281));
#44341=CARTESIAN_POINT('Ctrl Pts',(-13.498646273364,32.8879686178449,17.243617313843));
#44342=CARTESIAN_POINT('Ctrl Pts',(-13.5567922492037,32.990907195771,17.2378576293579));
#44343=CARTESIAN_POINT('Ctrl Pts',(-13.6149804832775,33.0939205854527,17.232093758958));
#44344=CARTESIAN_POINT('Ctrl Pts',(-13.6686230900308,33.1993460671065,17.2263298885582));
#44345=CARTESIAN_POINT('Ctrl Pts',(-13.7175367147721,33.3067351730099,17.2205660181584));
#44346=CARTESIAN_POINT('Ctrl Pts',(-13.7665291072191,33.414297212192,17.2147928659511));
#44347=CARTESIAN_POINT('Ctrl Pts',(-13.81077716563,33.5238288013093,17.2090197137437));
#44348=CARTESIAN_POINT('Ctrl Pts',(-13.8501469330714,33.6348649906472,17.2032465615364));
#44349=CARTESIAN_POINT('Ctrl Pts',(-13.8641657127107,33.6744027367777,17.2011908585471));
#44350=CARTESIAN_POINT('Ctrl Pts',(-13.877566430735,33.7141311528221,17.1991351555578));
#44351=CARTESIAN_POINT('Ctrl Pts',(-13.8903446080909,33.7540289608912,17.1970794525685));
#44352=CARTESIAN_POINT('Ctrl Pts',(-13.9364896150878,33.8981093395885,17.189655825068));
#44353=CARTESIAN_POINT('Ctrl Pts',(-13.9746373453614,34.0447885994859,17.1822321975675));
#44354=CARTESIAN_POINT('Ctrl Pts',(-14.004551758706,34.193284305443,17.174808570067));
#44355=CARTESIAN_POINT('Ctrl Pts',(-14.033969026612,34.3393121721674,17.1675083152867));
#44356=CARTESIAN_POINT('Ctrl Pts',(-14.0554244147101,34.4870967690664,17.1602080605065));
#44357=CARTESIAN_POINT('Ctrl Pts',(-14.0687390147019,34.6358738814061,17.1529078057263));
#44358=CARTESIAN_POINT('Ctrl Pts',(-14.0793920292548,34.7549104836218,17.1470668701773));
#44359=CARTESIAN_POINT('Ctrl Pts',(-14.0848344524003,34.8745821123516,17.1412259346282));
#44360=CARTESIAN_POINT('Ctrl Pts',(-14.0849962795766,34.9944867572603,17.1353849990792));
#44361=CARTESIAN_POINT('',(-13.1750507821943,37.570267988068,17.));
#44362=CARTESIAN_POINT('Ctrl Pts',(-14.0811739487135,34.9944924835857,17.1353849714045));
#44363=CARTESIAN_POINT('Ctrl Pts',(-14.0735484049167,35.9200466893068,17.090256647603));
#44364=CARTESIAN_POINT('Ctrl Pts',(-13.7580895933996,36.8500404311904,17.0451283238015));
#44365=CARTESIAN_POINT('Ctrl Pts',(-13.1750507821943,37.570267988068,17.));
#44366=CARTESIAN_POINT('',(-11.4626270635503,38.8141771160986,17.0000001028261));
#44367=CARTESIAN_POINT('Origin',(-10.,35.,17.));
#44368=CARTESIAN_POINT('',(-14.0849987342305,35.0032157946179,17.2396150285694));
#44369=CARTESIAN_POINT('Ctrl Pts',(-14.0849987342305,35.0032157946178,17.2396150285694));
#44370=CARTESIAN_POINT('Ctrl Pts',(-14.0848793000589,35.1549320880902,17.2322291681083));
#44371=CARTESIAN_POINT('Ctrl Pts',(-14.0763041428688,35.3062908916574,17.2248433076472));
#44372=CARTESIAN_POINT('Ctrl Pts',(-14.059414157619,35.4564884411704,17.2174574471862));
#44373=CARTESIAN_POINT('Ctrl Pts',(-14.0421962898582,35.6096017510568,17.2099282062284));
#44374=CARTESIAN_POINT('Ctrl Pts',(-14.0163376314483,35.7615085205179,17.2023989652706));
#44375=CARTESIAN_POINT('Ctrl Pts',(-13.9820359968326,35.9113804474144,17.1948697243128));
#44376=CARTESIAN_POINT('Ctrl Pts',(-13.9743911680411,35.9447825063723,17.1931916772256));
#44377=CARTESIAN_POINT('Ctrl Pts',(-13.9663271537708,35.9780835733154,17.1915136301384));
#44378=CARTESIAN_POINT('Ctrl Pts',(-13.9578464672157,36.0112746125304,17.1898355830512));
#44379=CARTESIAN_POINT('Ctrl Pts',(-13.9285721977973,36.1258459291263,17.1840431743579));
#44380=CARTESIAN_POINT('Ctrl Pts',(-13.8942697521635,36.2393372344149,17.1782507656646));
#44381=CARTESIAN_POINT('Ctrl Pts',(-13.855034425663,36.3512714667873,17.1724583569712));
#44382=CARTESIAN_POINT('Ctrl Pts',(-13.8158480556437,36.463066031502,17.1666731758448));
#44383=CARTESIAN_POINT('Ctrl Pts',(-13.7717411799201,36.5733070003613,17.1608879947184));
#44384=CARTESIAN_POINT('Ctrl Pts',(-13.7228597190487,36.6815292183857,17.155102813592));
#44385=CARTESIAN_POINT('Ctrl Pts',(-13.6740261466227,36.789645412701,17.1493233001222));
#44386=CARTESIAN_POINT('Ctrl Pts',(-13.6204274618174,36.8957464154687,17.1435437866523));
#44387=CARTESIAN_POINT('Ctrl Pts',(-13.5622586122089,36.9993845502413,17.1377642731824));
#44388=CARTESIAN_POINT('Ctrl Pts',(-13.5041295541281,37.1029517893414,17.1319887133006));
#44389=CARTESIAN_POINT('Ctrl Pts',(-13.4414367513126,37.2040591524435,17.1262131534188));
#44390=CARTESIAN_POINT('Ctrl Pts',(-13.3744219785508,37.3022817617905,17.120437593537));
#44391=CARTESIAN_POINT('Ctrl Pts',(-13.3074313226107,37.4004690234514,17.1146641121245));
#44392=CARTESIAN_POINT('Ctrl Pts',(-13.2361220211795,37.4957732542151,17.108890630712));
#44393=CARTESIAN_POINT('Ctrl Pts',(-13.1607799203636,37.5877973829158,17.1031171492995));
#44394=CARTESIAN_POINT('Ctrl Pts',(-13.0854466514282,37.6798107242069,17.097344344676));
#44395=CARTESIAN_POINT('Ctrl Pts',(-13.0060817849086,37.7685444084177,17.0915715400524));
#44396=CARTESIAN_POINT('Ctrl Pts',(-12.9230118657337,37.8536339346139,17.0857987354288));
#44397=CARTESIAN_POINT('Ctrl Pts',(-12.8399315271689,37.9387341335176,17.0800252067272));
#44398=CARTESIAN_POINT('Ctrl Pts',(-12.7531455009603,38.020188970308,17.0742516780256));
#44399=CARTESIAN_POINT('Ctrl Pts',(-12.6630171327591,38.0976708589893,17.068478149324));
#44400=CARTESIAN_POINT('Ctrl Pts',(-12.5727996533326,38.1752293551381,17.0626989122508));
#44401=CARTESIAN_POINT('Ctrl Pts',(-12.4792335449056,38.2488067870086,17.0569196751776));
#44402=CARTESIAN_POINT('Ctrl Pts',(-12.3827153287825,38.3181158301037,17.0511404381044));
#44403=CARTESIAN_POINT('Ctrl Pts',(-12.2861497208749,38.3874589049015,17.0453583633455));
#44404=CARTESIAN_POINT('Ctrl Pts',(-12.1866294636243,38.452529189814,17.0395762885867));
#44405=CARTESIAN_POINT('Ctrl Pts',(-12.0845786339523,38.5130836766108,17.0337942138278));
#44406=CARTESIAN_POINT('Ctrl Pts',(-11.982363678535,38.5737355516436,17.0280028399057));
#44407=CARTESIAN_POINT('Ctrl Pts',(-11.8776103833025,38.6298569217935,17.0222114659835));
#44408=CARTESIAN_POINT('Ctrl Pts',(-11.7707663916904,38.6812513342693,17.0164200920614));
#44409=CARTESIAN_POINT('Ctrl Pts',(-11.6697899385664,38.7298233260482,17.0109467623163));
#44410=CARTESIAN_POINT('Ctrl Pts',(-11.5669465668444,38.7741735913199,17.0054734325712));
#44411=CARTESIAN_POINT('Ctrl Pts',(-11.4626270635503,38.8141771160986,17.0000001028261));
#44412=CARTESIAN_POINT('Ctrl Pts',(-7.51282733495085,38.2405550657615,18.0469656644349));
#44413=CARTESIAN_POINT('Ctrl Pts',(-7.41799580939191,38.1677705046697,18.0411565278969));
#44414=CARTESIAN_POINT('Ctrl Pts',(-7.32640791336297,38.0908551206141,18.035347391359));
#44415=CARTESIAN_POINT('Ctrl Pts',(-7.23842896479515,38.0101412620536,18.029538254821));
#44416=CARTESIAN_POINT('Ctrl Pts',(-7.15040477028745,37.9293858938541,18.0237261307519));
#44417=CARTESIAN_POINT('Ctrl Pts',(-7.06599350988609,37.8448284480232,18.0179140066829));
#44418=CARTESIAN_POINT('Ctrl Pts',(-6.98552275644513,37.7568373089629,18.0121018826139));
#44419=CARTESIAN_POINT('Ctrl Pts',(-6.90492115276495,37.6687030910684,18.0062803076848));
#44420=CARTESIAN_POINT('Ctrl Pts',(-6.82827312247758,37.5771243363809,18.0004587327558));
#44421=CARTESIAN_POINT('Ctrl Pts',(-6.75586553378204,37.4825020775614,17.9946371578267));
#44422=CARTESIAN_POINT('Ctrl Pts',(-6.68752494125946,37.3931945705715,17.9891425696595));
#44423=CARTESIAN_POINT('Ctrl Pts',(-6.6229615963789,37.3011763603051,17.9836479814922));
#44424=CARTESIAN_POINT('Ctrl Pts',(-6.56237959198754,37.2068055941601,17.978153393325));
#44425=CARTESIAN_POINT('Ctrl Pts',(-6.49815823619039,37.1067656794967,17.9723287279777));
#44426=CARTESIAN_POINT('Ctrl Pts',(-6.43820405998836,37.0037589441355,17.9665040626304));
#44427=CARTESIAN_POINT('Ctrl Pts',(-6.38280233067359,36.8981849280351,17.9606793972832));
#44428=CARTESIAN_POINT('Ctrl Pts',(-6.32747052185801,36.7927441530446,17.9548620830333));
#44429=CARTESIAN_POINT('Ctrl Pts',(-6.2766799202222,36.6847429000424,17.9490447687834));
#44430=CARTESIAN_POINT('Ctrl Pts',(-6.2306724747935,36.5746094778454,17.9432274545335));
#44431=CARTESIAN_POINT('Ctrl Pts',(-6.18471111391979,36.4645863736569,17.9374159673478));
#44432=CARTESIAN_POINT('Ctrl Pts',(-6.14352353417009,36.3524357235726,17.9316044801622));
#44433=CARTESIAN_POINT('Ctrl Pts',(-6.10730542645452,36.2386096871451,17.9257929929765));
#44434=CARTESIAN_POINT('Ctrl Pts',(-6.06972575841709,36.1205045476785,17.9197630324673));
#44435=CARTESIAN_POINT('Ctrl Pts',(-6.03749674247662,36.0005959791163,17.9137330719582));
#44436=CARTESIAN_POINT('Ctrl Pts',(-6.01078195992056,35.879411410379,17.907703111449));
#44437=CARTESIAN_POINT('Ctrl Pts',(-5.9850641472194,35.7627493325756,17.9018981832358));
#44438=CARTESIAN_POINT('Ctrl Pts',(-5.96445646557269,35.6449052207303,17.8960932550225));
#44439=CARTESIAN_POINT('Ctrl Pts',(-5.94905364667441,35.5263636029192,17.8902883268093));
#44440=CARTESIAN_POINT('Ctrl Pts',(-5.93365312577556,35.407839670739,17.8844842646533));
#44441=CARTESIAN_POINT('Ctrl Pts',(-5.92345597590759,35.2886188442069,17.8786802024972));
#44442=CARTESIAN_POINT('Ctrl Pts',(-5.91850533560985,35.1691930984252,17.8728761403411));
#44443=CARTESIAN_POINT('Ctrl Pts',(-5.91355426670033,35.0497570131161,17.8670715756866));
#44444=CARTESIAN_POINT('Ctrl Pts',(-5.91385062737332,34.930116381129,17.861267011032));
#44445=CARTESIAN_POINT('Ctrl Pts',(-5.91938545454085,34.8107648780294,17.8554624463774));
#44446=CARTESIAN_POINT('Ctrl Pts',(-5.92492206583707,34.6913749024654,17.8496560106454));
#44447=CARTESIAN_POINT('Ctrl Pts',(-5.93570048298359,34.5722746486728,17.8438495749133));
#44448=CARTESIAN_POINT('Ctrl Pts',(-5.95165978867681,34.4539537259685,17.8380431391813));
#44449=CARTESIAN_POINT('Ctrl Pts',(-5.9676367064291,34.3355022289698,17.8322302956962));
#44450=CARTESIAN_POINT('Ctrl Pts',(-5.98880587063381,34.2178321845306,17.8264174522112));
#44451=CARTESIAN_POINT('Ctrl Pts',(-6.01505501390461,34.1014242058717,17.8206046087261));
#44452=CARTESIAN_POINT('Ctrl Pts',(-6.04132134427662,33.9849400069838,17.8147879591767));
#44453=CARTESIAN_POINT('Ctrl Pts',(-6.07267417110744,33.8697199125778,17.8089713096273));
#44454=CARTESIAN_POINT('Ctrl Pts',(-6.10895148188831,33.7562289480371,17.8031546600778));
#44455=CARTESIAN_POINT('Ctrl Pts',(-6.14528059883978,33.6425759116079,17.7973297040048));
#44456=CARTESIAN_POINT('Ctrl Pts',(-6.186548095489,33.5306573152795,17.7915047479317));
#44457=CARTESIAN_POINT('Ctrl Pts',(-6.23254398375756,33.4209179357365,17.7856797918587));
#44458=CARTESIAN_POINT('Ctrl Pts',(-6.24466712025368,33.3919939269331,17.784144508158));
#44459=CARTESIAN_POINT('Ctrl Pts',(-6.25711848824365,33.3632211702652,17.7826092244573));
#44460=CARTESIAN_POINT('Ctrl Pts',(-6.26989372335423,33.3346075042418,17.7810739407566));
#44461=CARTESIAN_POINT('Ctrl Pts',(-6.31836100253144,33.2260516516537,17.7752493102826));
#44462=CARTESIAN_POINT('Ctrl Pts',(-6.37164897662962,33.1194389214489,17.7694246798086));
#44463=CARTESIAN_POINT('Ctrl Pts',(-6.42957975018663,33.0152269047262,17.7636000493346));
#44464=CARTESIAN_POINT('Ctrl Pts',(-6.48743758471783,32.9111460984555,17.7577827524908));
#44465=CARTESIAN_POINT('Ctrl Pts',(-6.54992639521803,32.809460347201,17.7519654556471));
#44466=CARTESIAN_POINT('Ctrl Pts',(-6.61682048404191,32.710606769731,17.7461481588033));
#44467=CARTESIAN_POINT('Ctrl Pts',(-6.68364776473429,32.611851918814,17.7403366717813));
#44468=CARTESIAN_POINT('Ctrl Pts',(-6.75487134372906,32.5159239507107,17.7345251847593));
#44469=CARTESIAN_POINT('Ctrl Pts',(-6.83022022433124,32.4232343580059,17.7287136977373));
#44470=CARTESIAN_POINT('Ctrl Pts',(-6.90840180963993,32.3270601449139,17.7226837306727));
#44471=CARTESIAN_POINT('Ctrl Pts',(-6.99102474449253,32.2343729681636,17.7166537636082));
#44472=CARTESIAN_POINT('Ctrl Pts',(-7.07773747670501,32.1455987063929,17.7106237965436));
#44473=CARTESIAN_POINT('Ctrl Pts',(-7.16121469147295,32.0601368840445,17.7048188260064));
#44474=CARTESIAN_POINT('Ctrl Pts',(-7.24848165424397,31.9783015195646,17.6990138554693));
#44475=CARTESIAN_POINT('Ctrl Pts',(-7.33918496830152,31.9004373910038,17.6932088849321));
#44476=CARTESIAN_POINT('Ctrl Pts',(-7.4298749923951,31.8225846711933,17.6874047649465));
#44477=CARTESIAN_POINT('Ctrl Pts',(-7.52400005685096,31.7487022959226,17.681600644961));
#44478=CARTESIAN_POINT('Ctrl Pts',(-7.62117226406248,31.6790959660456,17.6757965249754));
#44479=CARTESIAN_POINT('Ctrl Pts',(-7.71835314130074,31.609483425661,17.669991887127));
#44480=CARTESIAN_POINT('Ctrl Pts',(-7.81858137002927,31.5441479269376,17.6641872492786));
#44481=CARTESIAN_POINT('Ctrl Pts',(-7.9214390800406,31.4833525195127,17.6583826114302));
#44482=CARTESIAN_POINT('Ctrl Pts',(-8.02433021534186,31.4225373556289,17.6525760872701));
#44483=CARTESIAN_POINT('Ctrl Pts',(-8.12985218014831,31.3662654248431,17.64676956311));
#44484=CARTESIAN_POINT('Ctrl Pts',(-8.23756203615051,31.3147540891303,17.6409630389498));
#44485=CARTESIAN_POINT('Ctrl Pts',(-8.34539116131664,31.2631857139396,17.6351500851155));
#44486=CARTESIAN_POINT('Ctrl Pts',(-8.45541264515805,31.2163886324068,17.6293371312812));
#44487=CARTESIAN_POINT('Ctrl Pts',(-8.56716293433242,31.1745323235911,17.6235241774469));
#44488=CARTESIAN_POINT('Ctrl Pts',(-8.67898664029595,31.1326485163607,17.6177074046658));
#44489=CARTESIAN_POINT('Ctrl Pts',(-8.79254102629172,31.0957120722684,17.6118906318847));
#44490=CARTESIAN_POINT('Ctrl Pts',(-8.90734831928826,31.0638423171019,17.6060738591037));
#44491=CARTESIAN_POINT('Ctrl Pts',(-9.02231991125934,31.0319269536125,17.6002487620273));
#44492=CARTESIAN_POINT('Ctrl Pts',(-9.13854759271531,31.0050928429122,17.594423664951));
#44493=CARTESIAN_POINT('Ctrl Pts',(-9.25554423799079,30.9834080841575,17.5885985678747));
#44494=CARTESIAN_POINT('Ctrl Pts',(-9.28636843833458,30.9776949686516,17.5870638746458));
#44495=CARTESIAN_POINT('Ctrl Pts',(-9.31724599351994,30.9723390017576,17.585529181417));
#44496=CARTESIAN_POINT('Ctrl Pts',(-9.34816796603897,30.9673408277537,17.5839944881881));
#44497=CARTESIAN_POINT('Ctrl Pts',(-9.4653745462179,30.9483957594282,17.5781773901725));
#44498=CARTESIAN_POINT('Ctrl Pts',(-9.58359933606191,30.9345337715468,17.572360292157));
#44499=CARTESIAN_POINT('Ctrl Pts',(-9.70236334270299,30.9258574619642,17.5665431941414));
#44500=CARTESIAN_POINT('Ctrl Pts',(-9.8209770473109,30.917192132703,17.5607334579662));
#44501=CARTESIAN_POINT('Ctrl Pts',(-9.94012820689428,30.9136994588333,17.5549237217911));
#44502=CARTESIAN_POINT('Ctrl Pts',(-10.0593286541284,30.915430853713,17.5491139856159));
#44503=CARTESIAN_POINT('Ctrl Pts',(-10.1784095075453,30.9171605114842,17.5433100783494));
#44504=CARTESIAN_POINT('Ctrl Pts',(-10.2975391433226,30.9241038056909,17.5375061710829));
#44505=CARTESIAN_POINT('Ctrl Pts',(-10.4162259165701,30.9362602216215,17.5317022638165));
#44506=CARTESIAN_POINT('Ctrl Pts',(-10.53959344679,30.9488960610554,17.5256694626416));
#44507=CARTESIAN_POINT('Ctrl Pts',(-10.6624820156081,30.9671646983021,17.5196366614667));
#44508=CARTESIAN_POINT('Ctrl Pts',(-10.7843409195185,30.9910058216594,17.5136038602919));
#44509=CARTESIAN_POINT('Ctrl Pts',(-10.9014446806331,31.0139166236176,17.5078064693343));
#44510=CARTESIAN_POINT('Ctrl Pts',(-11.0175971881947,31.0419730899628,17.5020090783767));
#44511=CARTESIAN_POINT('Ctrl Pts',(-11.1323173311832,31.0750691137929,17.4962116874191));
#44512=CARTESIAN_POINT('Ctrl Pts',(-11.2470208997623,31.1081603560126,17.4904151340505));
#44513=CARTESIAN_POINT('Ctrl Pts',(-11.3602921220666,31.146289594431,17.4846185806819));
#44514=CARTESIAN_POINT('Ctrl Pts',(-11.4716636378013,31.1893004399227,17.4788220273133));
#44515=CARTESIAN_POINT('Ctrl Pts',(-11.5830455072493,31.2323152839409,17.473024935065));
#44516=CARTESIAN_POINT('Ctrl Pts',(-11.692526937101,31.2802124898519,17.4672278428167));
#44517=CARTESIAN_POINT('Ctrl Pts',(-11.7996598050395,31.3327872183189,17.4614307505684));
#44518=CARTESIAN_POINT('Ctrl Pts',(-11.9068280705152,31.3853793178872,17.4556317429154));
#44519=CARTESIAN_POINT('Ctrl Pts',(-12.0116458635929,31.4426518332669,17.4498327352625));
#44520=CARTESIAN_POINT('Ctrl Pts',(-12.1136895424318,31.5043539197719,17.4440337276096));
#44521=CARTESIAN_POINT('Ctrl Pts',(-12.2158477829119,31.5661252775181,17.4382282095698));
#44522=CARTESIAN_POINT('Ctrl Pts',(-12.3152253421021,31.6323359207464,17.4324226915299));
#44523=CARTESIAN_POINT('Ctrl Pts',(-12.4114273401869,31.7026915244401,17.4266171734901));
#44524=CARTESIAN_POINT('Ctrl Pts',(-12.5076932531773,31.7730938711522,17.4208077983667));
#44525=CARTESIAN_POINT('Ctrl Pts',(-12.600779084965,31.8476464069538,17.4149984232434));
#44526=CARTESIAN_POINT('Ctrl Pts',(-12.6903241425304,31.926015450898,17.4091890481201));
#44527=CARTESIAN_POINT('Ctrl Pts',(-12.7799992418815,32.0044983062651,17.4033712363333));
#44528=CARTESIAN_POINT('Ctrl Pts',(-12.8661230090778,32.0868084503061,17.3975534245465));
#44529=CARTESIAN_POINT('Ctrl Pts',(-12.948372500504,32.1725763320168,17.3917356127597));
#44530=CARTESIAN_POINT('Ctrl Pts',(-12.9710895192435,32.1962651177136,17.390128753713));
#44531=CARTESIAN_POINT('Ctrl Pts',(-12.9935112341829,32.220217488981,17.3885218946664));
#44532=CARTESIAN_POINT('Ctrl Pts',(-13.0156314083634,32.2444252489014,17.3869150356197));
#44533=CARTESIAN_POINT('Ctrl Pts',(-13.0950954777897,32.3313887194088,17.3811425874553));
#44534=CARTESIAN_POINT('Ctrl Pts',(-13.1709349916773,32.4219460065299,17.3753701392909));
#44535=CARTESIAN_POINT('Ctrl Pts',(-13.2428036170308,32.515759733566,17.3695976911265));
#44536=CARTESIAN_POINT('Ctrl Pts',(-13.3145580842969,32.6094244443158,17.3638344120765));
#44537=CARTESIAN_POINT('Ctrl Pts',(-13.3823539658873,32.7063349721867,17.3580711330264));
#44538=CARTESIAN_POINT('Ctrl Pts',(-13.4458827470682,32.8061182590081,17.3523078539764));
#44539=CARTESIAN_POINT('Ctrl Pts',(-13.5093535973036,32.9058105549425,17.3465498303743));
#44540=CARTESIAN_POINT('Ctrl Pts',(-13.5685648588005,33.0083700540876,17.3407918067722));
#44541=CARTESIAN_POINT('Ctrl Pts',(-13.6232492660118,33.1133919971692,17.3350337831701));
#44542=CARTESIAN_POINT('Ctrl Pts',(-13.6778973144575,33.2183441128832,17.3292795879835));
#44543=CARTESIAN_POINT('Ctrl Pts',(-13.728024301,33.3257550493138,17.3235253927969));
#44544=CARTESIAN_POINT('Ctrl Pts',(-13.7734075587941,33.4351931763838,17.3177711976103));
#44545=CARTESIAN_POINT('Ctrl Pts',(-13.8187718496968,33.5445855662994,17.3120194072575));
#44546=CARTESIAN_POINT('Ctrl Pts',(-13.859396196102,33.6560030774838,17.3062676169047));
#44547=CARTESIAN_POINT('Ctrl Pts',(-13.8951052977852,33.768992396788,17.300515826552));
#44548=CARTESIAN_POINT('Ctrl Pts',(-13.93081740448,33.8819912244305,17.2947635521715));
#44549=CARTESIAN_POINT('Ctrl Pts',(-13.9616133050997,33.9965617302525,17.2890112777909));
#44550=CARTESIAN_POINT('Ctrl Pts',(-13.9873671243155,34.11223403088,17.2832590034104));
#44551=CARTESIAN_POINT('Ctrl Pts',(-14.0131218752288,34.227910516191,17.2775065209295));
#44552=CARTESIAN_POINT('Ctrl Pts',(-14.033834098558,34.3446884673207,17.2717540384486));
#44553=CARTESIAN_POINT('Ctrl Pts',(-14.0494289930285,34.4620875253162,17.2660015559677));
#44554=CARTESIAN_POINT('Ctrl Pts',(-14.0650344310494,34.5795659556281,17.2602451842916));
#44555=CARTESIAN_POINT('Ctrl Pts',(-14.0755155851035,34.6976659171536,17.2544888126154));
#44556=CARTESIAN_POINT('Ctrl Pts',(-14.0808495272278,34.815901830198,17.2487324409393));
#44557=CARTESIAN_POINT('Ctrl Pts',(-14.0836656385158,34.8783257338717,17.2456933034914));
#44558=CARTESIAN_POINT('Ctrl Pts',(-14.0850478790537,34.9407874999945,17.2426541660434));
#44559=CARTESIAN_POINT('Ctrl Pts',(-14.0849987342309,35.0032157940822,17.2396150285955));
#44560=CARTESIAN_POINT('Origin',(-10.,35.,32.7603849714045));
#44561=CARTESIAN_POINT('',(-7.51282733495084,38.2405550657615,19.2967866609659));
#44562=CARTESIAN_POINT('',(-7.51282733495087,38.2405550657615,19.1927507857623));
#44563=CARTESIAN_POINT('',(-7.51282733495086,38.2405550657615,32.7603849714045));
#44564=CARTESIAN_POINT('',(-14.0849999333317,35.0007380241213,18.3853849714444));
#44565=CARTESIAN_POINT('Ctrl Pts',(-7.51282733495087,38.2405550657615,19.1927507857623));
#44566=CARTESIAN_POINT('Ctrl Pts',(-7.41816085919388,38.1678971827688,19.1869271965536));
#44567=CARTESIAN_POINT('Ctrl Pts',(-7.32679476472752,38.0911750994162,19.1811036073449));
#44568=CARTESIAN_POINT('Ctrl Pts',(-7.23907757352064,38.0107361815615,19.1752800181361));
#44569=CARTESIAN_POINT('Ctrl Pts',(-7.20189334496105,37.9766372886826,19.1728113381751));
#44570=CARTESIAN_POINT('Ctrl Pts',(-7.16536434784443,37.941870910604,19.170342658214));
#44571=CARTESIAN_POINT('Ctrl Pts',(-7.12951495706164,37.9064653134464,19.1678739782529));
#44572=CARTESIAN_POINT('Ctrl Pts',(-7.04494813906446,37.8229453811538,19.1620504927095));
#44573=CARTESIAN_POINT('Ctrl Pts',(-6.96389310497571,37.7355968276586,19.1562270071662));
#44574=CARTESIAN_POINT('Ctrl Pts',(-6.88671567260117,37.6447468114685,19.1504035216228));
#44575=CARTESIAN_POINT('Ctrl Pts',(-6.80963561420458,37.5540114198157,19.1445873835116));
#44576=CARTESIAN_POINT('Ctrl Pts',(-6.73642368884896,37.459783660754,19.1387712454005));
#44577=CARTESIAN_POINT('Ctrl Pts',(-6.66740975917089,37.3624282606527,19.1329551072893));
#44578=CARTESIAN_POINT('Ctrl Pts',(-6.59846491381403,37.2651703152503,19.1271447912485));
#44579=CARTESIAN_POINT('Ctrl Pts',(-6.53370993903152,37.1647912884284,19.1213344752077));
#44580=CARTESIAN_POINT('Ctrl Pts',(-6.47343479399331,37.0616893189283,19.1155241591669));
#44581=CARTESIAN_POINT('Ctrl Pts',(-6.41087652415465,36.9546820139306,19.1094937577718));
#44582=CARTESIAN_POINT('Ctrl Pts',(-6.35314446173313,36.8447417480414,19.1034633563767));
#44583=CARTESIAN_POINT('Ctrl Pts',(-6.3005139448485,36.7323475193331,19.0974329549816));
#44584=CARTESIAN_POINT('Ctrl Pts',(-6.24986130149476,36.6241771056878,19.0916291782143));
#44585=CARTESIAN_POINT('Ctrl Pts',(-6.20393387604689,36.5137342455091,19.085825401447));
#44586=CARTESIAN_POINT('Ctrl Pts',(-6.16293020497594,36.401470794599,19.0800216246797));
#44587=CARTESIAN_POINT('Ctrl Pts',(-6.12193258746479,36.2892239176565,19.0742187047505));
#44588=CARTESIAN_POINT('Ctrl Pts',(-6.08585741878447,36.1751573679706,19.0684157848214));
#44589=CARTESIAN_POINT('Ctrl Pts',(-6.05485452695307,36.0597415706187,19.0626128648922));
#44590=CARTESIAN_POINT('Ctrl Pts',(-6.02384889478502,35.9443155716977,19.0568094320447));
#44591=CARTESIAN_POINT('Ctrl Pts',(-5.99791653680995,35.8275404823864,19.0510059991971));
#44592=CARTESIAN_POINT('Ctrl Pts',(-5.97715681697477,35.7098997991177,19.0452025663495));
#44593=CARTESIAN_POINT('Ctrl Pts',(-5.95639036242527,35.5922209517313,19.0393972507953));
#44594=CARTESIAN_POINT('Ctrl Pts',(-5.94079995424183,35.4736763538543,19.0335919352411));
#44595=CARTESIAN_POINT('Ctrl Pts',(-5.93043337277146,35.3547569119097,19.0277866196869));
#44596=CARTESIAN_POINT('Ctrl Pts',(-5.92005530830509,35.2357057436598,19.0219748736218));
#44597=CARTESIAN_POINT('Ctrl Pts',(-5.91491265618143,35.1162793095952,19.0161631275567));
#44598=CARTESIAN_POINT('Ctrl Pts',(-5.91500112300383,34.9969709836484,19.0103513814916));
#44599=CARTESIAN_POINT('Ctrl Pts',(-5.91508964794459,34.8775842779968,19.004535817395));
#44600=CARTESIAN_POINT('Ctrl Pts',(-5.92041611769691,34.7583162419962,18.9987202532984));
#44601=CARTESIAN_POINT('Ctrl Pts',(-5.93092428797763,34.6396559285493,18.9929046892019));
#44602=CARTESIAN_POINT('Ctrl Pts',(-5.94144751381989,34.5208256047578,18.9870807928666));
#44603=CARTESIAN_POINT('Ctrl Pts',(-5.95716720459475,34.4026051447689,18.9812568965313));
#44604=CARTESIAN_POINT('Ctrl Pts',(-5.97797587157177,34.2854743459181,18.9754330001961));
#44605=CARTESIAN_POINT('Ctrl Pts',(-5.98350026428286,34.2543778546277,18.9738868420255));
#44606=CARTESIAN_POINT('Ctrl Pts',(-5.98938306682778,34.2233580850842,18.972340683855));
#44607=CARTESIAN_POINT('Ctrl Pts',(-5.99562168069339,34.1924238265853,18.9707945256844));
#44608=CARTESIAN_POINT('Ctrl Pts',(-6.01911980050726,34.0759080542969,18.9649708265863));
#44609=CARTESIAN_POINT('Ctrl Pts',(-6.04774543487043,33.9602308548337,18.9591471274881));
#44610=CARTESIAN_POINT('Ctrl Pts',(-6.08142546695665,33.8458775502642,18.95332342839));
#44611=CARTESIAN_POINT('Ctrl Pts',(-6.1150630040176,33.7316685284126,18.9475070772136));
#44612=CARTESIAN_POINT('Ctrl Pts',(-6.15374214020114,33.6187804673103,18.9416907260373));
#44613=CARTESIAN_POINT('Ctrl Pts',(-6.19733862899554,33.5076892088206,18.9358743748609));
#44614=CARTESIAN_POINT('Ctrl Pts',(-6.24089147294573,33.3967091648072,18.9300638464869));
#44615=CARTESIAN_POINT('Ctrl Pts',(-6.28935172787708,33.2875227228382,18.924253318113));
#44616=CARTESIAN_POINT('Ctrl Pts',(-6.34254532887773,33.1805906648899,18.918442789739));
#44617=CARTESIAN_POINT('Ctrl Pts',(-6.3977510686166,33.0696137193591,18.9124124682131));
#44618=CARTESIAN_POINT('Ctrl Pts',(-6.45805519237411,32.9610655072652,18.9063821466871));
#44619=CARTESIAN_POINT('Ctrl Pts',(-6.52320802882969,32.8554388352846,18.9003518251611));
#44620=CARTESIAN_POINT('Ctrl Pts',(-6.58591548917144,32.7537766405961,18.8945478392028));
#44621=CARTESIAN_POINT('Ctrl Pts',(-6.65311401549713,32.6548210093335,18.8887438532444));
#44622=CARTESIAN_POINT('Ctrl Pts',(-6.72453450385764,32.5589857059859,18.882939867286));
#44623=CARTESIAN_POINT('Ctrl Pts',(-6.7959444298385,32.4631645757263,18.8771367396794));
#44624=CARTESIAN_POINT('Ctrl Pts',(-6.87157483221681,32.370463182986,18.8713336120728));
#44625=CARTESIAN_POINT('Ctrl Pts',(-6.95111437587402,32.2812647331897,18.8655304844662));
#44626=CARTESIAN_POINT('Ctrl Pts',(-7.0306609260148,32.1920584260756,18.8597268456733));
#44627=CARTESIAN_POINT('Ctrl Pts',(-7.11411703031398,32.1063559801816,18.8539232068805));
#44628=CARTESIAN_POINT('Ctrl Pts',(-7.20113275808643,32.0245055600551,18.8481195680877));
#44629=CARTESIAN_POINT('Ctrl Pts',(-7.28817668458438,31.9426286150969,18.8423140485404));
#44630=CARTESIAN_POINT('Ctrl Pts',(-7.37878223143703,31.8646064581257,18.8365085289932));
#44631=CARTESIAN_POINT('Ctrl Pts',(-7.4725649933112,31.7907481733332,18.8307030094459));
#44632=CARTESIAN_POINT('Ctrl Pts',(-7.56645157108528,31.7168081286933,18.8248910632886));
#44633=CARTESIAN_POINT('Ctrl Pts',(-7.66352206338473,31.6470414096444,18.8190791171313));
#44634=CARTESIAN_POINT('Ctrl Pts',(-7.76336145521262,31.5817149007183,18.8132671709741));
#44635=CARTESIAN_POINT('Ctrl Pts',(-7.86326639937157,31.5163454998548,18.8074514088218));
#44636=CARTESIAN_POINT('Ctrl Pts',(-7.96594351330009,31.4554223229835,18.8016356466695));
#44637=CARTESIAN_POINT('Ctrl Pts',(-8.07095291650907,31.3991664368267,18.7958198845173));
#44638=CARTESIAN_POINT('Ctrl Pts',(-8.17611268573994,31.3428299962286,18.7899957946058));
#44639=CARTESIAN_POINT('Ctrl Pts',(-8.28361104332895,31.2911743619366,18.7841717046944));
#44640=CARTESIAN_POINT('Ctrl Pts',(-8.39298775763767,31.2443726685283,18.778347614783));
#44641=CARTESIAN_POINT('Ctrl Pts',(-8.42198754954446,31.2319638173545,18.7768034342273));
#44642=CARTESIAN_POINT('Ctrl Pts',(-8.45111930268121,31.2198959143175,18.7752592536717));
#44643=CARTESIAN_POINT('Ctrl Pts',(-8.48037427561966,31.2081715943622,18.773715073116));
#44644=CARTESIAN_POINT('Ctrl Pts',(-8.59070780167218,31.1639539646294,18.7678912808354));
#44645=CARTESIAN_POINT('Ctrl Pts',(-8.70315069552679,31.1244847482118,18.7620674885548));
#44646=CARTESIAN_POINT('Ctrl Pts',(-8.81725694322182,31.089968815771,18.7562436962742));
#44647=CARTESIAN_POINT('Ctrl Pts',(-8.93121926730304,31.0554964187004,18.7504272496145));
#44648=CARTESIAN_POINT('Ctrl Pts',(-9.04684038495362,31.0259649963554,18.7446108029547));
#44649=CARTESIAN_POINT('Ctrl Pts',(-9.16365418619704,31.0015314582037,18.738794356295));
#44650=CARTESIAN_POINT('Ctrl Pts',(-9.28035108931023,30.977122371229,18.7329837302808));
#44651=CARTESIAN_POINT('Ctrl Pts',(-9.39823790424308,30.9578011026136,18.7271731042667));
#44652=CARTESIAN_POINT('Ctrl Pts',(-9.51683381037535,30.9436746391341,18.7213624782525));
#44653=CARTESIAN_POINT('Ctrl Pts',(-9.63991301037189,30.9290141514282,18.7153321925148));
#44654=CARTESIAN_POINT('Ctrl Pts',(-9.76375554226951,30.9199491087418,18.7093019067771));
#44655=CARTESIAN_POINT('Ctrl Pts',(-9.88781239446962,30.9165408118649,18.7032716210394));
#44656=CARTESIAN_POINT('Ctrl Pts',(-10.0072158449064,30.913260361007,18.6974675327409));
#44657=CARTESIAN_POINT('Ctrl Pts',(-10.1268173820277,30.9152199397431,18.6916634444424));
#44658=CARTESIAN_POINT('Ctrl Pts',(-10.2461234163943,30.9224212743465,18.685859356144));
#44659=CARTESIAN_POINT('Ctrl Pts',(-10.3654118386774,30.9296215458811,18.6800561246511));
#44660=CARTESIAN_POINT('Ctrl Pts',(-10.4844044375049,30.9420620098548,18.6742528931583));
#44661=CARTESIAN_POINT('Ctrl Pts',(-10.6026100342064,30.9596923202962,18.6684496616655));
#44662=CARTESIAN_POINT('Ctrl Pts',(-10.7208260722507,30.977324188059,18.6626459175614));
#44663=CARTESIAN_POINT('Ctrl Pts',(-10.8382545660942,31.0001467535251,18.6568421734572));
#44664=CARTESIAN_POINT('Ctrl Pts',(-10.9544124889484,31.0280581825838,18.6510384293531));
#44665=CARTESIAN_POINT('Ctrl Pts',(-11.0706080799226,31.0559786628638,18.6452328031894));
#44666=CARTESIAN_POINT('Ctrl Pts',(-11.1855318836809,31.0889911933418,18.6394271770257));
#44667=CARTESIAN_POINT('Ctrl Pts',(-11.2987146624959,31.1269436841923,18.633621550862));
#44668=CARTESIAN_POINT('Ctrl Pts',(-11.4120227572256,31.1649381960212,18.6278094967119));
#44669=CARTESIAN_POINT('Ctrl Pts',(-11.5235855918826,31.207883455975,18.6219974425619));
#44670=CARTESIAN_POINT('Ctrl Pts',(-11.6329524450306,31.2555786411959,18.6161853884119));
#44671=CARTESIAN_POINT('Ctrl Pts',(-11.7423911221245,31.303305149037,18.6103695173406));
#44672=CARTESIAN_POINT('Ctrl Pts',(-11.8496305797145,31.3557876154431,18.6045536462694));
#44673=CARTESIAN_POINT('Ctrl Pts',(-11.9542447873468,31.412779305489,18.5987377751982));
#44674=CARTESIAN_POINT('Ctrl Pts',(-12.0590088014886,31.4698526070708,18.5929135758571));
#44675=CARTESIAN_POINT('Ctrl Pts',(-12.1611397138472,31.5314478103286,18.5870893765161));
#44676=CARTESIAN_POINT('Ctrl Pts',(-12.2602404277346,31.5972748849144,18.5812651771751));
#44677=CARTESIAN_POINT('Ctrl Pts',(-12.2864982496202,31.6147164908517,18.5797219916326));
#44678=CARTESIAN_POINT('Ctrl Pts',(-12.3125435203847,31.6324549745908,18.5781788060901));
#44679=CARTESIAN_POINT('Ctrl Pts',(-12.3383692581764,31.6504844809412,18.5766356205475));
#44680=CARTESIAN_POINT('Ctrl Pts',(-12.4353485371795,31.7181878139787,18.5708407417144));
#44681=CARTESIAN_POINT('Ctrl Pts',(-12.529549225962,31.7902211139549,18.5650458628812));
#44682=CARTESIAN_POINT('Ctrl Pts',(-12.6205578142079,31.8663277544718,18.559250984048));
#44683=CARTESIAN_POINT('Ctrl Pts',(-12.7114512408163,31.9423380901725,18.5534634380144));
#44684=CARTESIAN_POINT('Ctrl Pts',(-12.7991602853564,32.0224112542013,18.5476758919808));
#44685=CARTESIAN_POINT('Ctrl Pts',(-12.8833003257636,32.1062473790161,18.5418883459472));
#44686=CARTESIAN_POINT('Ctrl Pts',(-12.9673564177595,32.1899998586429,18.5361065742784));
#44687=CARTESIAN_POINT('Ctrl Pts',(-13.047850297363,32.2775075419245,18.5303248026097));
#44688=CARTESIAN_POINT('Ctrl Pts',(-13.1244308869851,32.3684307661675,18.524543030941));
#44689=CARTESIAN_POINT('Ctrl Pts',(-13.2012297678581,32.4596131650193,18.518744778462));
#44690=CARTESIAN_POINT('Ctrl Pts',(-13.274092698496,32.5542303324158,18.5129465259829));
#44691=CARTESIAN_POINT('Ctrl Pts',(-13.342703073328,32.6519026503223,18.5071482735039));
#44692=CARTESIAN_POINT('Ctrl Pts',(-13.4110440602726,32.7491914731751,18.5013727869548));
#44693=CARTESIAN_POINT('Ctrl Pts',(-13.4751655872742,32.849511157776,18.4955973004057));
#44694=CARTESIAN_POINT('Ctrl Pts',(-13.5347959679208,32.9524545267148,18.4898218138566));
#44695=CARTESIAN_POINT('Ctrl Pts',(-13.5944183664386,33.0553841156436,18.4840471004147));
#44696=CARTESIAN_POINT('Ctrl Pts',(-13.6495506071614,33.1609363333146,18.4782723869729));
#44697=CARTESIAN_POINT('Ctrl Pts',(-13.6999657706881,33.2686772987867,18.472497673531));
#44698=CARTESIAN_POINT('Ctrl Pts',(-13.7503864001868,33.3764299454487,18.4667223339993));
#44699=CARTESIAN_POINT('Ctrl Pts',(-13.7960887610852,33.4863714375386,18.4609469944676));
#44700=CARTESIAN_POINT('Ctrl Pts',(-13.8368934036505,33.598046359888,18.4551716549359));
#44701=CARTESIAN_POINT('Ctrl Pts',(-13.8779821953434,33.7104989469777,18.4493560979783));
#44702=CARTESIAN_POINT('Ctrl Pts',(-13.9141046401688,33.8247088036354,18.4435405410206));
#44703=CARTESIAN_POINT('Ctrl Pts',(-13.9451284266687,33.9401949721339,18.437724984063));
#44704=CARTESIAN_POINT('Ctrl Pts',(-13.9759825901072,34.0550497181122,18.4319412237584));
#44705=CARTESIAN_POINT('Ctrl Pts',(-14.0017936775757,34.1711664361819,18.4261574634538));
#44706=CARTESIAN_POINT('Ctrl Pts',(-14.0224830443867,34.2880623920447,18.4203737031492));
#44707=CARTESIAN_POINT('Ctrl Pts',(-14.0433430232002,34.4059223142426,18.4145422478651));
#44708=CARTESIAN_POINT('Ctrl Pts',(-14.0589963762885,34.5245739590227,18.408710792581));
#44709=CARTESIAN_POINT('Ctrl Pts',(-14.069415969644,34.6435190523933,18.4028793372968));
#44710=CARTESIAN_POINT('Ctrl Pts',(-14.0798355629994,34.7624641457639,18.3970478820127));
#44711=CARTESIAN_POINT('Ctrl Pts',(-14.0850214391494,34.8817022618907,18.3912164267285));
#44712=CARTESIAN_POINT('Ctrl Pts',(-14.0849999333317,35.0007380241213,18.3853849714444));
#44713=CARTESIAN_POINT('Ctrl Pts',(-14.0849999333316,35.0007380249352,18.3853849714045));
#44714=CARTESIAN_POINT('Ctrl Pts',(-14.0849927679777,35.0403985684774,18.3834420369294));
#44715=CARTESIAN_POINT('Ctrl Pts',(-14.0844080310192,35.0800533014694,18.3814991024543));
#44716=CARTESIAN_POINT('Ctrl Pts',(-14.0832461438359,35.119690972297,18.3795561679791));
#44717=CARTESIAN_POINT('Ctrl Pts',(-14.0797629567325,35.2385195692697,18.3737315023802));
#44718=CARTESIAN_POINT('Ctrl Pts',(-14.071082720807,35.3573873330334,18.3679068367812));
#44719=CARTESIAN_POINT('Ctrl Pts',(-14.0571955944118,35.475803434924,18.3620821711823));
#44720=CARTESIAN_POINT('Ctrl Pts',(-14.043325994456,35.5940700881394,18.3562648566829));
#44721=CARTESIAN_POINT('Ctrl Pts',(-14.0242626216709,35.7118858114284,18.3504475421835));
#44722=CARTESIAN_POINT('Ctrl Pts',(-14.0000476306313,35.828760491747,18.3446302276842));
#44723=CARTESIAN_POINT('Ctrl Pts',(-13.9758568951768,35.9455181014567,18.3388187402515));
#44724=CARTESIAN_POINT('Ctrl Pts',(-13.9465248895661,36.0613361460438,18.3330072528187));
#44725=CARTESIAN_POINT('Ctrl Pts',(-13.9121454139528,36.1757309471506,18.327195765386));
#44726=CARTESIAN_POINT('Ctrl Pts',(-13.8764735004439,36.2944262261845,18.3211658049704));
#44727=CARTESIAN_POINT('Ctrl Pts',(-13.8353672182095,36.4115887078271,18.3151358445547));
#44728=CARTESIAN_POINT('Ctrl Pts',(-13.7889893690839,36.5266907221075,18.3091058841391));
#44729=CARTESIAN_POINT('Ctrl Pts',(-13.7443422939109,36.6374972467962,18.3033009556863));
#44730=CARTESIAN_POINT('Ctrl Pts',(-13.6948102278603,36.7463939255093,18.2974960272336));
#44731=CARTESIAN_POINT('Ctrl Pts',(-13.6405885728166,36.8529273713444,18.2916910987808));
#44732=CARTESIAN_POINT('Ctrl Pts',(-13.5863750073168,36.9594449230317,18.2858870363884));
#44733=CARTESIAN_POINT('Ctrl Pts',(-13.5274734293382,37.0635995793517,18.2800829739959));
#44734=CARTESIAN_POINT('Ctrl Pts',(-13.4641260272299,37.1649609390167,18.2742789116035));
#44735=CARTESIAN_POINT('Ctrl Pts',(-13.4007731407284,37.2663310741887,18.2684743467159));
#44736=CARTESIAN_POINT('Ctrl Pts',(-13.3329738811572,37.3649070857318,18.2626697818283));
#44737=CARTESIAN_POINT('Ctrl Pts',(-13.2610143982138,37.4602865879085,18.2568652169407));
#44738=CARTESIAN_POINT('Ctrl Pts',(-13.1890317194737,37.5556968352134,18.2510587809793));
#44739=CARTESIAN_POINT('Ctrl Pts',(-13.112886396056,37.6479081982739,18.2452523450179));
#44740=CARTESIAN_POINT('Ctrl Pts',(-13.0329051611896,37.7365509831227,18.2394459090565));
#44741=CARTESIAN_POINT('Ctrl Pts',(-12.9528356622855,37.8252915905434,18.2336330653485));
#44742=CARTESIAN_POINT('Ctrl Pts',(-12.868922075769,37.9104554556389,18.2278202216405));
#44743=CARTESIAN_POINT('Ctrl Pts',(-12.7815284361686,37.9917093038572,18.2220073779326));
#44744=CARTESIAN_POINT('Ctrl Pts',(-12.694077574057,38.073016354451,18.2161907281637));
#44745=CARTESIAN_POINT('Ctrl Pts',(-12.6031424309925,38.150408025542,18.2103740783949));
#44746=CARTESIAN_POINT('Ctrl Pts',(-12.5091192961749,38.2235919961376,18.204557428626));
#44747=CARTESIAN_POINT('Ctrl Pts',(-12.4149618908088,38.2968804777337,18.1987324723403));
#44748=CARTESIAN_POINT('Ctrl Pts',(-12.3177080234843,38.365949029947,18.1929075160545));
#44749=CARTESIAN_POINT('Ctrl Pts',(-12.2177821458632,38.4305491329363,18.1870825597688));
#44750=CARTESIAN_POINT('Ctrl Pts',(-12.1914447213347,38.4475757568452,18.1855472783161));
#44751=CARTESIAN_POINT('Ctrl Pts',(-12.1649218010831,38.4642922135478,18.1840119968634));
#44752=CARTESIAN_POINT('Ctrl Pts',(-12.1382214131198,38.4806944980098,18.1824767154107));
#44753=CARTESIAN_POINT('Ctrl Pts',(-12.0369240773754,38.5429223472234,18.1766520839113));
#44754=CARTESIAN_POINT('Ctrl Pts',(-11.9327452401376,38.6008244834567,18.1708274524119));
#44755=CARTESIAN_POINT('Ctrl Pts',(-11.8260901017685,38.6541236897816,18.1650028209125));
#44756=CARTESIAN_POINT('Ctrl Pts',(-11.7195692497886,38.7073557886228,18.1591855230376));
#44757=CARTESIAN_POINT('Ctrl Pts',(-11.6105786599547,38.7559963037591,18.1533682251627));
#44758=CARTESIAN_POINT('Ctrl Pts',(-11.4995514257018,38.7998119060916,18.1475509272877));
#44759=CARTESIAN_POINT('Ctrl Pts',(-11.38863507591,38.8435837491656,18.14173943923));
#44760=CARTESIAN_POINT('Ctrl Pts',(-11.2756865056747,38.8825401167798,18.1359279511724));
#44761=CARTESIAN_POINT('Ctrl Pts',(-11.1611617254819,38.9164944079209,18.1301164631147));
#44762=CARTESIAN_POINT('Ctrl Pts',(-11.042331470388,38.9517251856709,18.1240864964367));
#44763=CARTESIAN_POINT('Ctrl Pts',(-10.9218045669189,38.9815702060192,18.1180565297586));
#44764=CARTESIAN_POINT('Ctrl Pts',(-10.8001116333098,39.0058764801529,18.1120265630806));
#44765=CARTESIAN_POINT('Ctrl Pts',(-10.6829594070215,39.0292758184964,18.1062215915032));
#44766=CARTESIAN_POINT('Ctrl Pts',(-10.5647270436356,39.0475422523483,18.1004166199258));
#44767=CARTESIAN_POINT('Ctrl Pts',(-10.4459008909407,39.0605907692672,18.0946116483484));
#44768=CARTESIAN_POINT('Ctrl Pts',(-10.3270921488026,39.0736373743011,18.0888075273226));
#44769=CARTESIAN_POINT('Ctrl Pts',(-10.2076901959899,39.081467538296,18.0830034062969));
#44770=CARTESIAN_POINT('Ctrl Pts',(-10.0881877902054,39.084047981312,18.0771992852712));
#44771=CARTESIAN_POINT('Ctrl Pts',(-9.96867472204712,39.0866286545631,18.0713946463839));
#44772=CARTESIAN_POINT('Ctrl Pts',(-9.84906159118034,39.0839586667239,18.0655900074966));
#44773=CARTESIAN_POINT('Ctrl Pts',(-9.72984180982053,39.0760568632293,18.0597853686093));
#44774=CARTESIAN_POINT('Ctrl Pts',(-9.61058328610529,39.0681524919187,18.0539788434127));
#44775=CARTESIAN_POINT('Ctrl Pts',(-9.49171877317047,39.055012950657,18.048172318216));
#44776=CARTESIAN_POINT('Ctrl Pts',(-9.37373657538421,39.0367089470246,18.0423657930194));
#44777=CARTESIAN_POINT('Ctrl Pts',(-9.25562373387619,39.0183846750534,18.0365528381573));
#44778=CARTESIAN_POINT('Ctrl Pts',(-9.13839556127501,38.9948845882849,18.0307398832953));
#44779=CARTESIAN_POINT('Ctrl Pts',(-9.02253033929591,38.9663305538499,18.0249269284332));
#44780=CARTESIAN_POINT('Ctrl Pts',(-8.90658899722417,38.9377577602418,18.0191101546282));
#44781=CARTESIAN_POINT('Ctrl Pts',(-8.79201277977996,38.9041245211396,18.0132933808233));
#44782=CARTESIAN_POINT('Ctrl Pts',(-8.67926338579312,38.8656021259169,18.0074766070184));
#44783=CARTESIAN_POINT('Ctrl Pts',(-8.56635263814957,38.8270246019781,18.0016515089317));
#44784=CARTESIAN_POINT('Ctrl Pts',(-8.45527431078127,38.7835441049257,17.9958264108449));
#44785=CARTESIAN_POINT('Ctrl Pts',(-8.34646889662311,38.7353794840906,17.9900013127582));
#44786=CARTESIAN_POINT('Ctrl Pts',(-8.31780296685609,38.7226900085825,17.9884666294529));
#44787=CARTESIAN_POINT('Ctrl Pts',(-8.28929466225861,38.7096756441621,17.9869319461476));
#44788=CARTESIAN_POINT('Ctrl Pts',(-8.26095172288859,38.6963409055275,17.9853972628422));
#44789=CARTESIAN_POINT('Ctrl Pts',(-8.15351046874027,38.6457921242617,17.9795796482013));
#44790=CARTESIAN_POINT('Ctrl Pts',(-8.04809935594169,38.5904723324018,17.9737620335603));
#44791=CARTESIAN_POINT('Ctrl Pts',(-7.94517176492508,38.530567365784,17.9679444189194));
#44792=CARTESIAN_POINT('Ctrl Pts',(-7.8423892622281,38.470746842131,17.9621350048778));
#44793=CARTESIAN_POINT('Ctrl Pts',(-7.74208366574298,38.4063542092715,17.9563255908361));
#44794=CARTESIAN_POINT('Ctrl Pts',(-7.64468683351894,38.3376226401139,17.9505161767945));
#44795=CARTESIAN_POINT('Ctrl Pts',(-7.60011147230471,38.3061664371548,17.9478573970022));
#44796=CARTESIAN_POINT('Ctrl Pts',(-7.55614507346746,38.2738020536891,17.9451986172099));
#44797=CARTESIAN_POINT('Ctrl Pts',(-7.51282733495087,38.2405550657615,17.9425398374177));
#44798=CARTESIAN_POINT('',(-14.0849995332602,34.9980472419391,18.4896150286338));
#44799=CARTESIAN_POINT('Ctrl Pts',(-14.0849995332606,34.9980472427294,18.4896150285955));
#44800=CARTESIAN_POINT('Ctrl Pts',(-14.0850575831595,35.1194826169903,18.4837275467034));
#44801=CARTESIAN_POINT('Ctrl Pts',(-14.079696394968,35.2409097711324,18.4778400648113));
#44802=CARTESIAN_POINT('Ctrl Pts',(-14.0689446252189,35.3618212775702,18.4719525829192));
#44803=CARTESIAN_POINT('Ctrl Pts',(-14.0581894988055,35.4827705321505,18.4660632629762));
#44804=CARTESIAN_POINT('Ctrl Pts',(-14.0420404743837,35.6032034284576,18.4601739430332));
#44805=CARTESIAN_POINT('Ctrl Pts',(-14.0205780237788,35.7226184018604,18.4542846230902));
#44806=CARTESIAN_POINT('Ctrl Pts',(-13.9991044168668,35.8420954478629,18.4483922418444));
#44807=CARTESIAN_POINT('Ctrl Pts',(-13.9723119534402,35.9605531323285,18.4424998605985));
#44808=CARTESIAN_POINT('Ctrl Pts',(-13.9403319792833,36.0775012264666,18.4366074793527));
#44809=CARTESIAN_POINT('Ctrl Pts',(-13.9083066364416,36.1946152300958,18.4307067388259));
#44810=CARTESIAN_POINT('Ctrl Pts',(-13.8710791873055,36.3102149878166,18.4248059982991));
#44811=CARTESIAN_POINT('Ctrl Pts',(-13.8288307107525,36.4238259684381,18.4189052577723));
#44812=CARTESIAN_POINT('Ctrl Pts',(-13.7865496276371,36.5375246318313,18.4129999631674));
#44813=CARTESIAN_POINT('Ctrl Pts',(-13.7392399463767,36.6492310991074,18.4070946685624));
#44814=CARTESIAN_POINT('Ctrl Pts',(-13.6871299964566,36.7584929312426,18.4011893739575));
#44815=CARTESIAN_POINT('Ctrl Pts',(-13.6349282140381,36.867947313688,18.3952736725501));
#44816=CARTESIAN_POINT('Ctrl Pts',(-13.5779094458923,36.9749481085648,18.3893579711426));
#44817=CARTESIAN_POINT('Ctrl Pts',(-13.5163472182928,37.0790688397464,18.3834422697352));
#44818=CARTESIAN_POINT('Ctrl Pts',(-13.4777389013461,37.1443674221228,18.3797322793107));
#44819=CARTESIAN_POINT('Ctrl Pts',(-13.4373444700697,37.2085338354459,18.3760222888863));
#44820=CARTESIAN_POINT('Ctrl Pts',(-13.3952395715432,37.271469403674,18.3723122984619));
#44821=CARTESIAN_POINT('Ctrl Pts',(-13.3291450141728,37.3702630991931,18.3664885063728));
#44822=CARTESIAN_POINT('Ctrl Pts',(-13.2586283516628,37.4663288203657,18.3606647142837));
#44823=CARTESIAN_POINT('Ctrl Pts',(-13.183942014477,37.5592456405058,18.3548409221946));
#44824=CARTESIAN_POINT('Ctrl Pts',(-13.1093498801037,37.652045263497,18.3490244757274));
#44825=CARTESIAN_POINT('Ctrl Pts',(-13.0305987851725,37.7417035697452,18.3432080292603));
#44826=CARTESIAN_POINT('Ctrl Pts',(-12.9479848271691,37.8278278693692,18.3373915827931));
#44827=CARTESIAN_POINT('Ctrl Pts',(-12.8654535427777,37.9138659825047,18.3315809569723));
#44828=CARTESIAN_POINT('Ctrl Pts',(-12.7790673665881,37.9963768316084,18.3257703311515));
#44829=CARTESIAN_POINT('Ctrl Pts',(-12.6891627259359,38.075000623323,18.3199597053308));
#44830=CARTESIAN_POINT('Ctrl Pts',(-12.5958594062092,38.1565966424302,18.3139294195209));
#44831=CARTESIAN_POINT('Ctrl Pts',(-12.4987666351617,38.2340055693401,18.307899133711));
#44832=CARTESIAN_POINT('Ctrl Pts',(-12.3983029168726,38.306866813,18.3018688479011));
#44833=CARTESIAN_POINT('Ctrl Pts',(-12.3016076207253,38.3769950110533,18.2960647597967));
#44834=CARTESIAN_POINT('Ctrl Pts',(-12.2017900731062,38.4429102895892,18.2902606716924));
#44835=CARTESIAN_POINT('Ctrl Pts',(-12.0992566748516,38.5043325203369,18.2844565835881));
#44836=CARTESIAN_POINT('Ctrl Pts',(-11.9967384126859,38.56574568387,18.2786533522893));
#44837=CARTESIAN_POINT('Ctrl Pts',(-11.8915054473537,38.6226669088808,18.2728501209906));
#44838=CARTESIAN_POINT('Ctrl Pts',(-11.7839915924143,38.6748604052664,18.2670468896919));
#44839=CARTESIAN_POINT('Ctrl Pts',(-11.6764682405506,38.7270585120131,18.2612431457816));
#44840=CARTESIAN_POINT('Ctrl Pts',(-11.5666639658243,38.7745278815008,18.2554394018713));
#44841=CARTESIAN_POINT('Ctrl Pts',(-11.4550349263738,38.8170798214122,18.249635657961));
#44842=CARTESIAN_POINT('Ctrl Pts',(-11.3433696874364,38.8596455602276,18.2438300319907));
#44843=CARTESIAN_POINT('Ctrl Pts',(-11.2298788882609,38.897290552718,18.2380244060204));
#44844=CARTESIAN_POINT('Ctrl Pts',(-11.1150356831317,38.9298753702049,18.2322187800501));
#44845=CARTESIAN_POINT('Ctrl Pts',(-11.0000653236272,38.9624962655956,18.2264067260918));
#44846=CARTESIAN_POINT('Ctrl Pts',(-10.8837399622936,38.9900456911426,18.2205946721334));
#44847=CARTESIAN_POINT('Ctrl Pts',(-10.7665449882451,39.0124348943,18.2147826181751));
#44848=CARTESIAN_POINT('Ctrl Pts',(-10.6492730493103,39.0348388010101,18.2089667472949));
#44849=CARTESIAN_POINT('Ctrl Pts',(-10.5311307634036,39.052075677528,18.2031508764146));
#44850=CARTESIAN_POINT('Ctrl Pts',(-10.4126090654447,39.0641086057231,18.1973350055343));
#44851=CARTESIAN_POINT('Ctrl Pts',(-10.2939176455307,39.0761587649581,18.1915108063817));
#44852=CARTESIAN_POINT('Ctrl Pts',(-10.1748461353257,39.0829900787603,18.1856866072291));
#44853=CARTESIAN_POINT('Ctrl Pts',(-10.0558860363671,39.0846176994841,18.1798624080765));
#44854=CARTESIAN_POINT('Ctrl Pts',(-10.0243662135838,39.0850489559914,18.1783192206821));
#44855=CARTESIAN_POINT('Ctrl Pts',(-9.99285418524738,39.0851151723714,18.1767760332878));
#44856=CARTESIAN_POINT('Ctrl Pts',(-9.96135901985522,39.0848172388313,18.1752328458934));
#44857=CARTESIAN_POINT('Ctrl Pts',(-9.84254219543945,39.0836932721311,18.1694111071156));
#44858=CARTESIAN_POINT('Ctrl Pts',(-9.72358255591783,39.0773790740118,18.1635893683379));
#44859=CARTESIAN_POINT('Ctrl Pts',(-9.60497011596792,39.0658549397048,18.1577676295601));
#44860=CARTESIAN_POINT('Ctrl Pts',(-9.48649786732683,39.0543444260894,18.1519527716557));
#44861=CARTESIAN_POINT('Ctrl Pts',(-9.36837240499521,39.0376362587188,18.1461379137513));
#44862=CARTESIAN_POINT('Ctrl Pts',(-9.25108419494506,39.0157627067518,18.1403230558469));
#44863=CARTESIAN_POINT('Ctrl Pts',(-9.13390689647571,38.9939098391335,18.1345136966629));
#44864=CARTESIAN_POINT('Ctrl Pts',(-9.0175656748106,38.9669013755368,18.128704337479));
#44865=CARTESIAN_POINT('Ctrl Pts',(-8.90254568416089,38.934821345963,18.1228949782951));
#44866=CARTESIAN_POINT('Ctrl Pts',(-8.78760728663151,38.9027640733873,18.1170897401665));
#44867=CARTESIAN_POINT('Ctrl Pts',(-8.67398864760348,38.8656425013601,18.1112845020378));
#44868=CARTESIAN_POINT('Ctrl Pts',(-8.56216390622729,38.8235915534278,18.1054792639092));
#44869=CARTESIAN_POINT('Ctrl Pts',(-8.45038395661472,38.7815574491394,18.0996763510876));
#44870=CARTESIAN_POINT('Ctrl Pts',(-8.34039685749402,38.7345980387547,18.093873438266));
#44871=CARTESIAN_POINT('Ctrl Pts',(-8.23266026355598,38.6828976711261,18.0880705254443));
#44872=CARTESIAN_POINT('Ctrl Pts',(-8.12494841703871,38.6312091792279,18.0822689455693));
#44873=CARTESIAN_POINT('Ctrl Pts',(-8.01948641360687,38.5747820767256,18.0764673656943));
#44874=CARTESIAN_POINT('Ctrl Pts',(-7.91670996681592,38.5138479815774,18.0706657858192));
#44875=CARTESIAN_POINT('Ctrl Pts',(-7.81391316543473,38.4529018186007,18.0648630569574));
#44876=CARTESIAN_POINT('Ctrl Pts',(-7.71380333385899,38.3874470893049,18.0590603280956));
#44877=CARTESIAN_POINT('Ctrl Pts',(-7.61678939141035,38.3177601171733,18.0532575992337));
#44878=CARTESIAN_POINT('Ctrl Pts',(-7.58172511877826,38.2925727788583,18.0511602876341));
#44879=CARTESIAN_POINT('Ctrl Pts',(-7.54706499785715,38.2668329649385,18.0490629760345));
#44880=CARTESIAN_POINT('Ctrl Pts',(-7.51282733495085,38.2405550657615,18.0469656644349));
#44881=CARTESIAN_POINT('Ctrl Pts',(-7.51282733495083,38.2405550657615,19.2967866609659));
#44882=CARTESIAN_POINT('Ctrl Pts',(-7.41811218255726,38.1678598227495,19.2909817422586));
#44883=CARTESIAN_POINT('Ctrl Pts',(-7.3265292139763,38.0909644348317,19.2851768235514));
#44884=CARTESIAN_POINT('Ctrl Pts',(-7.23846551527048,38.0101747938699,19.2793719048441));
#44885=CARTESIAN_POINT('Ctrl Pts',(-7.1504261827437,37.9294075064418,19.2735685922889));
#44886=CARTESIAN_POINT('Ctrl Pts',(-7.06590448452307,37.8447483843177,19.2677652797336));
#44887=CARTESIAN_POINT('Ctrl Pts',(-6.98525330733249,37.7565426495976,19.2619619671784));
#44888=CARTESIAN_POINT('Ctrl Pts',(-6.90460541135285,37.6683405034379,19.2561588907251));
#44889=CARTESIAN_POINT('Ctrl Pts',(-6.82782799866911,37.576592333092,19.2503558142717));
#44890=CARTESIAN_POINT('Ctrl Pts',(-6.75523561031701,37.4816786769131,19.2445527378183));
#44891=CARTESIAN_POINT('Ctrl Pts',(-6.68262904333245,37.3867464823464,19.2387485279171));
#44892=CARTESIAN_POINT('Ctrl Pts',(-6.61420937421198,37.2886478967719,19.2329443180158));
#44893=CARTESIAN_POINT('Ctrl Pts',(-6.55024913470335,37.187794315603,19.2271401081146));
#44894=CARTESIAN_POINT('Ctrl Pts',(-6.4862220837446,37.0868353850162,19.2213298352642));
#44895=CARTESIAN_POINT('Ctrl Pts',(-6.42666398505913,36.9831160565537,19.2155195624138));
#44896=CARTESIAN_POINT('Ctrl Pts',(-6.37180263230093,36.8770745486052,19.2097092895634));
#44897=CARTESIAN_POINT('Ctrl Pts',(-6.31691159195473,36.7709756575184,19.2038958725509));
#44898=CARTESIAN_POINT('Ctrl Pts',(-6.26672253250245,36.6625524538866,19.1980824555384));
#44899=CARTESIAN_POINT('Ctrl Pts',(-6.22141536100894,36.5522638712477,19.1922690385259));
#44900=CARTESIAN_POINT('Ctrl Pts',(-6.17603640724264,36.4418005532443,19.1864464110447));
#44901=CARTESIAN_POINT('Ctrl Pts',(-6.13555493258404,36.3294663360085,19.1806237835634));
#44902=CARTESIAN_POINT('Ctrl Pts',(-6.10010133507654,36.2157365682286,19.1748011560822));
#44903=CARTESIAN_POINT('Ctrl Pts',(-6.07133914191992,36.123471811518,19.1700774736334));
#44904=CARTESIAN_POINT('Ctrl Pts',(-6.04588509371599,36.0302889351828,19.1653537911845));
#44905=CARTESIAN_POINT('Ctrl Pts',(-6.0237839425562,35.9364458684441,19.1606301087357));
#44906=CARTESIAN_POINT('Ctrl Pts',(-5.99653648737942,35.8207512271955,19.1548065059349));
#44907=CARTESIAN_POINT('Ctrl Pts',(-5.97429877800222,35.7036798183631,19.1489829031342));
#44908=CARTESIAN_POINT('Ctrl Pts',(-5.95720681326372,35.5857032092099,19.1431593003334));
#44909=CARTESIAN_POINT('Ctrl Pts',(-5.94013641280084,35.4678754466144,19.1373430449487));
#44910=CARTESIAN_POINT('Ctrl Pts',(-5.92819890219626,35.3491451557764,19.131526789564));
#44911=CARTESIAN_POINT('Ctrl Pts',(-5.92147985708011,35.2299966169245,19.1257105341793));
#44912=CARTESIAN_POINT('Ctrl Pts',(-5.91476753786673,35.1109673482181,19.1199001009862));
#44913=CARTESIAN_POINT('Ctrl Pts',(-5.91326331491296,34.9915210697442,19.1140896677931));
#44914=CARTESIAN_POINT('Ctrl Pts',(-5.91700120477437,34.8721491564906,19.1082792346001));
#44915=CARTESIAN_POINT('Ctrl Pts',(-5.92088057334584,34.7482590297715,19.1022488771654));
#44916=CARTESIAN_POINT('Ctrl Pts',(-5.9304067859898,34.6244494525114,19.0962185197307));
#44917=CARTESIAN_POINT('Ctrl Pts',(-5.94555850207841,34.5012724792722,19.090188162296));
#44918=CARTESIAN_POINT('Ctrl Pts',(-5.96014120934238,34.3827213044808,19.0843842694133));
#44919=CARTESIAN_POINT('Ctrl Pts',(-5.97993446366303,34.2647565185023,19.0785803765306));
#44920=CARTESIAN_POINT('Ctrl Pts',(-6.00486629199975,34.1478664100036,19.0727764836479));
#44921=CARTESIAN_POINT('Ctrl Pts',(-6.029794437115,34.0309935698797,19.0669734481841));
#44922=CARTESIAN_POINT('Ctrl Pts',(-6.05985956141968,33.9151954907488,19.0611704127204));
#44923=CARTESIAN_POINT('Ctrl Pts',(-6.09493856300208,33.8009503040859,19.0553673772567));
#44924=CARTESIAN_POINT('Ctrl Pts',(-6.13002066089168,33.686695033379,19.0495638295783));
#44925=CARTESIAN_POINT('Ctrl Pts',(-6.17011739610909,33.573993318034,19.0437602818999));
#44926=CARTESIAN_POINT('Ctrl Pts',(-6.21505597259766,33.4633075423393,19.0379567342214));
#44927=CARTESIAN_POINT('Ctrl Pts',(-6.26000912103195,33.3525858752737,19.0321513046636));
#44928=CARTESIAN_POINT('Ctrl Pts',(-6.30980707965028,33.2438818260596,19.0263458751058));
#44929=CARTESIAN_POINT('Ctrl Pts',(-6.36422941860888,33.1376366413906,19.020540445548));
#44930=CARTESIAN_POINT('Ctrl Pts',(-6.41871202285655,33.0312738047264,19.0147285872717));
#44931=CARTESIAN_POINT('Ctrl Pts',(-6.47782904286411,32.9273756313071,19.0089167289955));
#44932=CARTESIAN_POINT('Ctrl Pts',(-6.54131462650677,32.8263577830784,19.0031048707193));
#44933=CARTESIAN_POINT('Ctrl Pts',(-6.60484190628768,32.7252735882254,18.9972891953238));
#44934=CARTESIAN_POINT('Ctrl Pts',(-6.67274323206694,32.6270738211096,18.9914735199283));
#44935=CARTESIAN_POINT('Ctrl Pts',(-6.74471104103503,32.5321428741435,18.9856578445328));
#44936=CARTESIAN_POINT('Ctrl Pts',(-6.81678193279979,32.4370759532239,18.9798338390785));
#44937=CARTESIAN_POINT('Ctrl Pts',(-6.89293067356589,32.345287510785,18.9740098336241));
#44938=CARTESIAN_POINT('Ctrl Pts',(-6.97281121072416,32.2571268651134,18.9681858281698));
#44939=CARTESIAN_POINT('Ctrl Pts',(-6.99400281343857,32.2337386225629,18.9666407708356));
#44940=CARTESIAN_POINT('Ctrl Pts',(-7.01545686912637,32.2106054893505,18.9650957135014));
#44941=CARTESIAN_POINT('Ctrl Pts',(-7.03716652042704,32.1877335168371,18.9635506561672));
#44942=CARTESIAN_POINT('Ctrl Pts',(-7.1189944886594,32.1015245301369,18.9577270295825));
#44943=CARTESIAN_POINT('Ctrl Pts',(-7.20472013130725,32.0187508998506,18.9519034029978));
#44944=CARTESIAN_POINT('Ctrl Pts',(-7.29402358738557,31.9397848679587,18.9460797764131));
#44945=CARTESIAN_POINT('Ctrl Pts',(-7.38321437769467,31.8609184600804,18.9402634969502));
#44946=CARTESIAN_POINT('Ctrl Pts',(-7.47597370040877,31.785850364272,18.9344472174873));
#44947=CARTESIAN_POINT('Ctrl Pts',(-7.57194342192194,31.7149176184376,18.9286309380244));
#44948=CARTESIAN_POINT('Ctrl Pts',(-7.66781708048372,31.6440558742567,18.9228204804912));
#44949=CARTESIAN_POINT('Ctrl Pts',(-7.76689441846199,31.5773214865998,18.917010022958));
#44950=CARTESIAN_POINT('Ctrl Pts',(-7.86878310589314,31.5150122596667,18.9111995654248));
#44951=CARTESIAN_POINT('Ctrl Pts',(-7.97452766743188,31.4503450031931,18.9051692170154));
#44952=CARTESIAN_POINT('Ctrl Pts',(-8.08330023142771,31.390444752136,18.899138868606));
#44953=CARTESIAN_POINT('Ctrl Pts',(-8.19462738046408,31.3355962688822,18.8931085201966));
#44954=CARTESIAN_POINT('Ctrl Pts',(-8.30177435914308,31.2828072653315,18.8873046024816));
#44955=CARTESIAN_POINT('Ctrl Pts',(-8.41128714073893,31.2346976934736,18.8815006847666));
#44956=CARTESIAN_POINT('Ctrl Pts',(-8.52271787763656,31.1914750189942,18.8756967670516));
#44957=CARTESIAN_POINT('Ctrl Pts',(-8.63413215539231,31.1482587288227,18.8698937066181));
#44958=CARTESIAN_POINT('Ctrl Pts',(-8.74746344447043,31.1099280481632,18.8640906461846));
#44959=CARTESIAN_POINT('Ctrl Pts',(-8.86224436564803,31.076642112106,18.8582875857511));
#44960=CARTESIAN_POINT('Ctrl Pts',(-8.97703542028208,31.0433532373933,18.8524840129932));
#44961=CARTESIAN_POINT('Ctrl Pts',(-9.09327596927955,31.015110106533,18.8466804402353));
#44962=CARTESIAN_POINT('Ctrl Pts',(-9.21048456353993,30.9920216597902,18.8408768674775));
#44963=CARTESIAN_POINT('Ctrl Pts',(-9.32773116577276,30.9689257260106,18.8350714127583));
#44964=CARTESIAN_POINT('Ctrl Pts',(-9.44594603714658,30.9509878795476,18.8292659580392));
#44965=CARTESIAN_POINT('Ctrl Pts',(-9.56463929642827,30.9382656342659,18.8234605033201));
#44966=CARTESIAN_POINT('Ctrl Pts',(-9.68346399152251,30.9255293009167,18.81764861989));
#44967=CARTESIAN_POINT('Ctrl Pts',(-9.80276772569672,30.918020140751,18.8118367364599));
#44968=CARTESIAN_POINT('Ctrl Pts',(-9.92205711728293,30.9157436531195,18.8060248530298));
#44969=CARTESIAN_POINT('Ctrl Pts',(-10.0414248560725,30.9134656703303,18.8002091524555));
#44970=CARTESIAN_POINT('Ctrl Pts',(-10.1607778262462,30.9164271943039,18.7943934518811));
#44971=CARTESIAN_POINT('Ctrl Pts',(-10.2796259347861,30.9245816979609,18.7885777513068));
#44972=CARTESIAN_POINT('Ctrl Pts',(-10.3986442709859,30.9327478814175,18.7827537208305));
#44973=CARTESIAN_POINT('Ctrl Pts',(-10.5171558979279,30.9461218447179,18.7769296903541));
#44974=CARTESIAN_POINT('Ctrl Pts',(-10.6346789588496,30.9646056426672,18.7711056598778));
#44975=CARTESIAN_POINT('Ctrl Pts',(-10.6658518433224,30.9695084531758,18.7695608411181));
#44976=CARTESIAN_POINT('Ctrl Pts',(-10.6969552497768,30.9747705023045,18.7680160223585));
#44977=CARTESIAN_POINT('Ctrl Pts',(-10.7279803621977,30.9803893730543,18.7664712035988));
#44978=CARTESIAN_POINT('Ctrl Pts',(-10.8449353738875,31.0015707658987,18.7606477179771));
#44979=CARTESIAN_POINT('Ctrl Pts',(-10.9611538121788,31.0278949622146,18.7548242323554));
#44980=CARTESIAN_POINT('Ctrl Pts',(-11.0761490267025,31.0592985050467,18.7490007467337));
#44981=CARTESIAN_POINT('Ctrl Pts',(-11.190999152942,31.0906624263504,18.7431846085442));
#44982=CARTESIAN_POINT('Ctrl Pts',(-11.3046287346005,31.1270928410789,18.7373684703546));
#44983=CARTESIAN_POINT('Ctrl Pts',(-11.4165595837332,31.1684749843263,18.7315523321651));
#44984=CARTESIAN_POINT('Ctrl Pts',(-11.5283783878524,31.2098157032224,18.7257420160459));
#44985=CARTESIAN_POINT('Ctrl Pts',(-11.6385014614945,31.2560981489563,18.7199316999268));
#44986=CARTESIAN_POINT('Ctrl Pts',(-11.7464646841815,31.3071574489417,18.7141213838077));
#44987=CARTESIAN_POINT('Ctrl Pts',(-11.8585173767009,31.3601507914812,18.7080909824419));
#44988=CARTESIAN_POINT('Ctrl Pts',(-11.9682429275002,31.4182899039562,18.7020605810762));
#44989=CARTESIAN_POINT('Ctrl Pts',(-12.0751436264263,31.4813349222038,18.6960301797105));
#44990=CARTESIAN_POINT('Ctrl Pts',(-12.1780269609712,31.5420106873665,18.6902264028654));
#44991=CARTESIAN_POINT('Ctrl Pts',(-12.2782935465882,31.6072300550486,18.6844226260203));
#44992=CARTESIAN_POINT('Ctrl Pts',(-12.3755243858113,31.6767321967052,18.6786188491753));
#44993=CARTESIAN_POINT('Ctrl Pts',(-12.4727408703948,31.7462240774383,18.6728159291687));
#44994=CARTESIAN_POINT('Ctrl Pts',(-12.566922167756,31.8199972373276,18.6670130091621));
#44995=CARTESIAN_POINT('Ctrl Pts',(-12.6576789960419,31.8977480189389,18.6612100891555));
#44996=CARTESIAN_POINT('Ctrl Pts',(-12.7484438462911,31.9755056729138,18.6554066562309));
#44997=CARTESIAN_POINT('Ctrl Pts',(-12.8357833155193,32.057241381952,18.6496032233063));
#44998=CARTESIAN_POINT('Ctrl Pts',(-12.9193423908359,32.1426122060406,18.6437997903818));
#44999=CARTESIAN_POINT('Ctrl Pts',(-13.0029285737598,32.2280107254902,18.6379944747511));
#45000=CARTESIAN_POINT('Ctrl Pts',(-13.0827316382375,32.3170464136244,18.6321891591204));
#45001=CARTESIAN_POINT('Ctrl Pts',(-13.1584349609951,32.4093410882241,18.6263838434897));
#45002=CARTESIAN_POINT('Ctrl Pts',(-13.2342221398235,32.5017379970255,18.6205720973492));
#45003=CARTESIAN_POINT('Ctrl Pts',(-13.3059002530701,32.5974007821578,18.6147603512088));
#45004=CARTESIAN_POINT('Ctrl Pts',(-13.3731942623637,32.6959198216302,18.6089486050683));
#45005=CARTESIAN_POINT('Ctrl Pts',(-13.4405324805062,32.7945035832581,18.6031330408969));
#45006=CARTESIAN_POINT('Ctrl Pts',(-13.5034806440173,32.8959469899746,18.5973174767255));
#45007=CARTESIAN_POINT('Ctrl Pts',(-13.5618090311546,32.9998146521921,18.5915019125542));
#45008=CARTESIAN_POINT('Ctrl Pts',(-13.6202209881655,33.1038311305834,18.5856780161455));
#45009=CARTESIAN_POINT('Ctrl Pts',(-13.6739997742077,33.2102784338999,18.5798541197368));
#45010=CARTESIAN_POINT('Ctrl Pts',(-13.7229631873897,33.3186998764821,18.5740302233282));
#45011=CARTESIAN_POINT('Ctrl Pts',(-13.7359622416147,33.3474841486495,18.5724840658956));
#45012=CARTESIAN_POINT('Ctrl Pts',(-13.7486221680768,33.3764074745468,18.570937908463));
#45013=CARTESIAN_POINT('Ctrl Pts',(-13.7609401485724,33.4054611328486,18.5693917510304));
#45014=CARTESIAN_POINT('Ctrl Pts',(-13.8139041444415,33.5303840322502,18.5627436908306));
#45015=CARTESIAN_POINT('Ctrl Pts',(-13.8606921381242,33.6580718198479,18.5560956306309));
#45016=CARTESIAN_POINT('Ctrl Pts',(-13.9010386252039,33.7879263039455,18.5494475704312));
#45017=CARTESIAN_POINT('Ctrl Pts',(-13.9400043430179,33.913336805589,18.543027025385));
#45018=CARTESIAN_POINT('Ctrl Pts',(-13.9729620170383,34.040767878319,18.5366064803388));
#45019=CARTESIAN_POINT('Ctrl Pts',(-13.999719495407,34.1696573249187,18.5301859352926));
#45020=CARTESIAN_POINT('Ctrl Pts',(-14.0264024485984,34.2981877874345,18.5237832728081));
#45021=CARTESIAN_POINT('Ctrl Pts',(-14.0469195731717,34.428168277178,18.5173806103235));
#45022=CARTESIAN_POINT('Ctrl Pts',(-14.0611283268584,34.5590218681288,18.510977947839));
#45023=CARTESIAN_POINT('Ctrl Pts',(-14.0752785381356,34.6893363206963,18.5046016653803));
#45024=CARTESIAN_POINT('Ctrl Pts',(-14.0831721555653,34.8205164481573,18.4982253829215));
#45025=CARTESIAN_POINT('Ctrl Pts',(-14.0847177095373,34.9519767411296,18.4918491004628));
#45026=CARTESIAN_POINT('Ctrl Pts',(-14.0848982158961,34.9673300831989,18.4911044098531));
#45027=CARTESIAN_POINT('Ctrl Pts',(-14.0849921906929,34.9826872315731,18.4903597192435));
#45028=CARTESIAN_POINT('Ctrl Pts',(-14.0849995332602,34.9980472419391,18.4896150286338));
#45029=CARTESIAN_POINT('Origin',(-10.,35.,32.7603849714045));
#45030=CARTESIAN_POINT('',(-7.51282733495085,38.2405550657615,20.5469196478657));
#45031=CARTESIAN_POINT('',(-7.51282733495086,38.2405550657615,20.4426717868481));
#45032=CARTESIAN_POINT('',(-7.51282733495086,38.2405550657615,32.7603849714045));
#45033=CARTESIAN_POINT('',(-14.0849992317297,35.0025053477764,19.6353849713615));
#45034=CARTESIAN_POINT('Ctrl Pts',(-7.51282733495086,38.2405550657615,20.4426717868481));
#45035=CARTESIAN_POINT('Ctrl Pts',(-7.41801445252157,38.1677848135401,20.4368682809325));
#45036=CARTESIAN_POINT('Ctrl Pts',(-7.32640760621858,38.090857480237,20.4310647750169));
#45037=CARTESIAN_POINT('Ctrl Pts',(-7.2383799075348,38.0100962550876,20.4252612691014));
#45038=CARTESIAN_POINT('Ctrl Pts',(-7.15032426427737,37.9293093921215,20.4194559208509));
#45039=CARTESIAN_POINT('Ctrl Pts',(-7.06585032903301,37.8446864927464,20.4136505726005));
#45040=CARTESIAN_POINT('Ctrl Pts',(-6.98529479736551,37.7565880252966,20.4078452243501));
#45041=CARTESIAN_POINT('Ctrl Pts',(-6.90465031166474,37.6683922744717,20.4020334655015));
#45042=CARTESIAN_POINT('Ctrl Pts',(-6.82793314244132,37.576713596073,20.3962217066529));
#45043=CARTESIAN_POINT('Ctrl Pts',(-6.75544017465018,37.4819461194244,20.3904099478043));
#45044=CARTESIAN_POINT('Ctrl Pts',(-6.68290003758068,37.3871169800571,20.3845944073963));
#45045=CARTESIAN_POINT('Ctrl Pts',(-6.61458980900607,37.289195373977,20.3787788669882));
#45046=CARTESIAN_POINT('Ctrl Pts',(-6.5507625249852,37.1886036281048,20.3729633265801));
#45047=CARTESIAN_POINT('Ctrl Pts',(-6.48684332500794,37.0878670227628,20.3671394113686));
#45048=CARTESIAN_POINT('Ctrl Pts',(-6.42742015841111,36.9844529552749,20.3613154961571));
#45049=CARTESIAN_POINT('Ctrl Pts',(-6.3726997764162,36.8788076239969,20.3554915809455));
#45050=CARTESIAN_POINT('Ctrl Pts',(-6.35659884856678,36.8477225366031,20.3537779518515));
#45051=CARTESIAN_POINT('Ctrl Pts',(-6.34090475411754,36.8164443971796,20.3520643227575));
#45052=CARTESIAN_POINT('Ctrl Pts',(-6.32562195112683,36.7849848609887,20.3503506936635));
#45053=CARTESIAN_POINT('Ctrl Pts',(-6.27368491836625,36.6780728656717,20.3445271015875));
#45054=CARTESIAN_POINT('Ctrl Pts',(-6.22633417317533,36.5687197963928,20.3387035095116));
#45055=CARTESIAN_POINT('Ctrl Pts',(-6.18380574208759,36.4573559571623,20.3328799174356));
#45056=CARTESIAN_POINT('Ctrl Pts',(-6.14133096694234,36.3461326199818,20.3270636726874));
#45057=CARTESIAN_POINT('Ctrl Pts',(-6.10366654922815,36.23290393676,20.3212474279392));
#45058=CARTESIAN_POINT('Ctrl Pts',(-6.07100210351602,36.1181236646384,20.315431183191));
#45059=CARTESIAN_POINT('Ctrl Pts',(-6.03837035508901,36.003458288184,20.3096207605349));
#45060=CARTESIAN_POINT('Ctrl Pts',(-6.01072873296436,35.8872448031128,20.3038103378788));
#45061=CARTESIAN_POINT('Ctrl Pts',(-5.98821810037733,35.7699551869167,20.2979999152228));
#45062=CARTESIAN_POINT('Ctrl Pts',(-5.96485538506858,35.6482258707249,20.2919695538008));
#45063=CARTESIAN_POINT('Ctrl Pts',(-5.94701993537065,35.5253377640211,20.2859391923788));
#45064=CARTESIAN_POINT('Ctrl Pts',(-5.93481189990426,35.4018341832646,20.2799088309568));
#45065=CARTESIAN_POINT('Ctrl Pts',(-5.92306235450141,35.2829689544154,20.2741049482995));
#45066=CARTESIAN_POINT('Ctrl Pts',(-5.91652519884472,35.1635340907011,20.2683010656422));
#45067=CARTESIAN_POINT('Ctrl Pts',(-5.9152372060822,35.0440217835264,20.2624971829849));
#45068=CARTESIAN_POINT('Ctrl Pts',(-5.9139494035681,34.9245271294228,20.2566941576146));
#45069=CARTESIAN_POINT('Ctrl Pts',(-5.91790922642153,34.8049554628107,20.2508911322444));
#45070=CARTESIAN_POINT('Ctrl Pts',(-5.92710133581934,34.6858002684352,20.2450881068741));
#45071=CARTESIAN_POINT('Ctrl Pts',(-5.93629425680091,34.5666345536865,20.2392845691469));
#45072=CARTESIAN_POINT('Ctrl Pts',(-5.95072035141718,34.4478857914314,20.2334810314197));
#45073=CARTESIAN_POINT('Ctrl Pts',(-5.9703123438196,34.3300429912097,20.2276774936925));
#45074=CARTESIAN_POINT('Ctrl Pts',(-5.98991068971902,34.2121619756874,20.2218720739331));
#45075=CARTESIAN_POINT('Ctrl Pts',(-6.01467819816725,34.0951879090913,20.2160666541737));
#45076=CARTESIAN_POINT('Ctrl Pts',(-6.04449648540219,33.9795996148548,20.2102612344144));
#45077=CARTESIAN_POINT('Ctrl Pts',(-6.0743477937702,33.863883316739,20.2044493856627));
#45078=CARTESIAN_POINT('Ctrl Pts',(-6.10926094355822,33.7495562498452,20.1986375369111));
#45079=CARTESIAN_POINT('Ctrl Pts',(-6.1490676263635,33.6370822278368,20.1928256881595));
#45080=CARTESIAN_POINT('Ctrl Pts',(-6.1889004545081,33.5245343320147,20.1870100221403));
#45081=CARTESIAN_POINT('Ctrl Pts',(-6.23363306400828,33.4138422826733,20.1811943561211));
#45082=CARTESIAN_POINT('Ctrl Pts',(-6.28304959755292,33.3054485237242,20.175378690102));
#45083=CARTESIAN_POINT('Ctrl Pts',(-6.33253691522382,33.1968995018101,20.1695546937365));
#45084=CARTESIAN_POINT('Ctrl Pts',(-6.38672136336078,33.0906557035423,20.163730697371));
#45085=CARTESIAN_POINT('Ctrl Pts',(-6.44534184466881,32.9871337851865,20.1579067010056));
#45086=CARTESIAN_POINT('Ctrl Pts',(-6.46089433211237,32.9596685836147,20.1563615477021));
#45087=CARTESIAN_POINT('Ctrl Pts',(-6.47675883397401,32.9323948043757,20.1548163943986));
#45088=CARTESIAN_POINT('Ctrl Pts',(-6.49292998453718,32.9053198557676,20.1532712410951));
#45089=CARTESIAN_POINT('Ctrl Pts',(-6.55387812436898,32.8032759259147,20.1474476468347));
#45090=CARTESIAN_POINT('Ctrl Pts',(-6.61938194651444,32.7037297289456,20.1416240525744));
#45091=CARTESIAN_POINT('Ctrl Pts',(-6.68921093804276,32.6071145478263,20.1358004583141));
#45092=CARTESIAN_POINT('Ctrl Pts',(-6.75895182978661,32.5106212613019,20.1299842113945));
#45093=CARTESIAN_POINT('Ctrl Pts',(-6.83300680027765,32.4170519635853,20.124167964475));
#45094=CARTESIAN_POINT('Ctrl Pts',(-6.91110027972097,32.3268139761588,20.1183517175555));
#45095=CARTESIAN_POINT('Ctrl Pts',(-6.98911558699545,32.2366663176463,20.1125412927435));
#45096=CARTESIAN_POINT('Ctrl Pts',(-7.07116109533737,32.1498436425087,20.1067308679315));
#45097=CARTESIAN_POINT('Ctrl Pts',(-7.1569192722743,32.0667224857449,20.1009204431196));
#45098=CARTESIAN_POINT('Ctrl Pts',(-7.24592356176301,31.9804550327335,20.0948900825115));
#45099=CARTESIAN_POINT('Ctrl Pts',(-7.33892687398621,31.8981752172698,20.0888597219035));
#45100=CARTESIAN_POINT('Ctrl Pts',(-7.43552969293926,31.8202646267018,20.0828293612954));
#45101=CARTESIAN_POINT('Ctrl Pts',(-7.52850450245564,31.7452800414084,20.0770254765339));
#45102=CARTESIAN_POINT('Ctrl Pts',(-7.6248129822553,31.6743426980231,20.0712215917723));
#45103=CARTESIAN_POINT('Ctrl Pts',(-7.72406363515827,31.6077531541483,20.0654177070107));
#45104=CARTESIAN_POINT('Ctrl Pts',(-7.82329962744296,31.5411734464191,20.0596146795587));
#45105=CARTESIAN_POINT('Ctrl Pts',(-7.92547658955635,31.4789404884555,20.0538116521068));
#45106=CARTESIAN_POINT('Ctrl Pts',(-8.03017337671437,31.4213119618783,20.0480086246548));
#45107=CARTESIAN_POINT('Ctrl Pts',(-8.13487940724463,31.3636783474476,20.0422050848705));
#45108=CARTESIAN_POINT('Ctrl Pts',(-8.24210534739603,31.3106501695605,20.0364015450863));
#45109=CARTESIAN_POINT('Ctrl Pts',(-8.35140532531963,31.2624392180708,20.0305980053021));
#45110=CARTESIAN_POINT('Ctrl Pts',(-8.46074074766888,31.2142126324563,20.0247925835126));
#45111=CARTESIAN_POINT('Ctrl Pts',(-8.57215117198729,31.1708065447275,20.0189871617231));
#45112=CARTESIAN_POINT('Ctrl Pts',(-8.6851712302782,31.1323844159079,20.0131817399336));
#45113=CARTESIAN_POINT('Ctrl Pts',(-8.79831644733963,31.0939197383012,20.0073698892016));
#45114=CARTESIAN_POINT('Ctrl Pts',(-8.91307446958729,31.0604501680115,20.0015580384696));
#45115=CARTESIAN_POINT('Ctrl Pts',(-9.02896511587748,31.0320891827289,19.9957461877376));
#45116=CARTESIAN_POINT('Ctrl Pts',(-9.14493187948949,31.0037095698666,19.9899305197647));
#45117=CARTESIAN_POINT('Ctrl Pts',(-9.26203234907246,30.9804453036296,19.9841148517919));
#45118=CARTESIAN_POINT('Ctrl Pts',(-9.37977815191968,30.9623583790579,19.978299183819));
#45119=CARTESIAN_POINT('Ctrl Pts',(-9.49769261243319,30.9442455469938,19.9724751855536));
#45120=CARTESIAN_POINT('Ctrl Pts',(-9.61625384670567,30.9313249025324,19.9666511872881));
#45121=CARTESIAN_POINT('Ctrl Pts',(-9.73497025113626,30.9236064674498,19.9608271890227));
#45122=CARTESIAN_POINT('Ctrl Pts',(-9.76646625868438,30.9215587311594,19.959282055524));
#45123=CARTESIAN_POINT('Ctrl Pts',(-9.79797320078038,30.9198768761249,19.9577369220253));
#45124=CARTESIAN_POINT('Ctrl Pts',(-9.82948194040127,30.918560475598,19.9561917885266));
#45125=CARTESIAN_POINT('Ctrl Pts',(-9.94823818743541,30.9135989700585,19.9503681898147));
#45126=CARTESIAN_POINT('Ctrl Pts',(-10.0674026600072,30.9138168806141,19.9445445911028));
#45127=CARTESIAN_POINT('Ctrl Pts',(-10.186486613217,30.9192589223168,19.9387209923909));
#45128=CARTESIAN_POINT('Ctrl Pts',(-10.3054203249576,30.9246940981042,19.9329047409832));
#45129=CARTESIAN_POINT('Ctrl Pts',(-10.4242733150749,30.9353402772369,19.9270884895754));
#45130=CARTESIAN_POINT('Ctrl Pts',(-10.5425538536446,30.9511902593607,19.9212722381677));
#45131=CARTESIAN_POINT('Ctrl Pts',(-10.6607159932118,30.9670243756279,19.9154618088366));
#45132=CARTESIAN_POINT('Ctrl Pts',(-10.7783064188011,30.988051878274,19.9096513795056));
#45133=CARTESIAN_POINT('Ctrl Pts',(-10.8948361470651,31.0142135945455,19.9038409501745));
#45134=CARTESIAN_POINT('Ctrl Pts',(-11.0157766227005,31.0413655535902,19.8978105912488));
#45135=CARTESIAN_POINT('Ctrl Pts',(-11.1355740702196,31.0740480535646,19.8917802323231));
#45136=CARTESIAN_POINT('Ctrl Pts',(-11.2536903419425,31.1121361229436,19.8857498733975));
#45137=CARTESIAN_POINT('Ctrl Pts',(-11.3673707675015,31.1487937982373,19.8799459840692));
#45138=CARTESIAN_POINT('Ctrl Pts',(-11.4794935894149,31.1904582166419,19.874142094741));
#45139=CARTESIAN_POINT('Ctrl Pts',(-11.5895928249534,31.2369666954893,19.8683382054127));
#45140=CARTESIAN_POINT('Ctrl Pts',(-11.69967579759,31.2834683045085,19.8625351733846));
#45141=CARTESIAN_POINT('Ctrl Pts',(-11.8077354022319,31.3348123921697,19.8567321413564));
#45142=CARTESIAN_POINT('Ctrl Pts',(-11.9133252646715,31.3907879763625,19.8509291093282));
#45143=CARTESIAN_POINT('Ctrl Pts',(-12.018924449405,31.446768502515,19.8451255649633));
#45144=CARTESIAN_POINT('Ctrl Pts',(-12.1220530976098,31.507381146935,19.8393220205983));
#45145=CARTESIAN_POINT('Ctrl Pts',(-12.2222896631662,31.5723690903214,19.8335184762334));
#45146=CARTESIAN_POINT('Ctrl Pts',(-12.3225587339777,31.637378108349,19.8277130498637));
#45147=CARTESIAN_POINT('Ctrl Pts',(-12.4199335144992,31.7067650250812,19.821907623494));
#45148=CARTESIAN_POINT('Ctrl Pts',(-12.5140221923776,31.7802302231009,19.8161021971244));
#45149=CARTESIAN_POINT('Ctrl Pts',(-12.6082150638857,31.8537767763464,19.8102903418361));
#45150=CARTESIAN_POINT('Ctrl Pts',(-12.6991142469081,31.9314103743132,19.8044784865479));
#45151=CARTESIAN_POINT('Ctrl Pts',(-12.7863616136823,32.0127916112535,19.7986666312597));
#45152=CARTESIAN_POINT('Ctrl Pts',(-12.8736662846126,32.09422629947,19.7928509587393));
#45153=CARTESIAN_POINT('Ctrl Pts',(-12.9573140771527,32.1794132380182,19.7870352862188));
#45154=CARTESIAN_POINT('Ctrl Pts',(-13.036985431817,32.2679779490401,19.7812196136983));
#45155=CARTESIAN_POINT('Ctrl Pts',(-13.1167709060288,32.3566695182632,19.7753956109327));
#45156=CARTESIAN_POINT('Ctrl Pts',(-13.1925683153322,32.4487482027003,19.7695716081671));
#45157=CARTESIAN_POINT('Ctrl Pts',(-13.2640997981118,32.5438083324043,19.7637476054014));
#45158=CARTESIAN_POINT('Ctrl Pts',(-13.2830768779487,32.5690274890693,19.762202515587));
#45159=CARTESIAN_POINT('Ctrl Pts',(-13.3017539560937,32.5944563419323,19.7606574257726));
#45160=CARTESIAN_POINT('Ctrl Pts',(-13.3201263812762,32.620087015802,19.7591123359582));
#45161=CARTESIAN_POINT('Ctrl Pts',(-13.3898878288234,32.7174085666047,19.7532455164733));
#45162=CARTESIAN_POINT('Ctrl Pts',(-13.4554778687479,32.8179551023663,19.7473786969884));
#45163=CARTESIAN_POINT('Ctrl Pts',(-13.5165873049546,32.9213372744401,19.7415118775035));
#45164=CARTESIAN_POINT('Ctrl Pts',(-13.5776176330624,33.0245856150207,19.7356526528021));
#45165=CARTESIAN_POINT('Ctrl Pts',(-13.6341786926365,33.130661949438,19.7297934281007));
#45166=CARTESIAN_POINT('Ctrl Pts',(-13.6860029530911,33.2391458806011,19.7239342033993));
#45167=CARTESIAN_POINT('Ctrl Pts',(-13.7377717246662,33.3475136566716,19.7180812522426));
#45168=CARTESIAN_POINT('Ctrl Pts',(-13.7848136157239,33.4582835422107,19.7122283010859));
#45169=CARTESIAN_POINT('Ctrl Pts',(-13.8269059407739,33.5710087752301,19.7063753499291));
#45170=CARTESIAN_POINT('Ctrl Pts',(-13.869450718731,33.6849456984881,19.7004594850521));
#45171=CARTESIAN_POINT('Ctrl Pts',(-13.9069386738898,33.8008799030811,19.694543620175));
#45172=CARTESIAN_POINT('Ctrl Pts',(-13.9391887239996,33.9183266682058,19.688627755298));
#45173=CARTESIAN_POINT('Ctrl Pts',(-13.9710477411261,34.0343493872042,19.682783620489));
#45174=CARTESIAN_POINT('Ctrl Pts',(-13.9977950631134,34.1518477927289,19.6769394856801));
#45175=CARTESIAN_POINT('Ctrl Pts',(-14.019305630051,34.270337576519,19.6710953508711));
#45176=CARTESIAN_POINT('Ctrl Pts',(-14.0412122233848,34.3910088500948,19.66514362096));
#45177=CARTESIAN_POINT('Ctrl Pts',(-14.0576872012397,34.512707961776,19.6591918910489));
#45178=CARTESIAN_POINT('Ctrl Pts',(-14.0686527748495,34.6349115207107,19.6532401611378));
#45179=CARTESIAN_POINT('Ctrl Pts',(-14.0796183484592,34.7571150796453,19.6472884312267));
#45180=CARTESIAN_POINT('Ctrl Pts',(-14.0850744735353,34.8798226489189,19.6413367013156));
#45181=CARTESIAN_POINT('Ctrl Pts',(-14.0849992317303,35.0025053468896,19.6353849714045));
#45182=CARTESIAN_POINT('Ctrl Pts',(-14.0849992317297,35.0025053477764,19.6353849713615));
#45183=CARTESIAN_POINT('Ctrl Pts',(-14.0849166368293,35.1371773114109,19.6288516038417));
#45184=CARTESIAN_POINT('Ctrl Pts',(-14.0781702966957,35.2716029408522,19.622318236322));
#45185=CARTESIAN_POINT('Ctrl Pts',(-14.0648574523362,35.4051652652772,19.6157848688022));
#45186=CARTESIAN_POINT('Ctrl Pts',(-14.0514920356939,35.5392550259205,19.6092257010827));
#45187=CARTESIAN_POINT('Ctrl Pts',(-14.0315082634781,35.6724744539174,19.6026665333631));
#45188=CARTESIAN_POINT('Ctrl Pts',(-14.0050544117836,35.8042164874292,19.5961073656435));
#45189=CARTESIAN_POINT('Ctrl Pts',(-13.9784604826347,35.9366561164707,19.5895134660623));
#45190=CARTESIAN_POINT('Ctrl Pts',(-13.9453278743482,36.0676024707254,19.5829195664811));
#45191=CARTESIAN_POINT('Ctrl Pts',(-13.9058559320516,36.1964591251094,19.5763256668999));
#45192=CARTESIAN_POINT('Ctrl Pts',(-13.8773364437467,36.2895613550451,19.5715614057298));
#45193=CARTESIAN_POINT('Ctrl Pts',(-13.8455085704644,36.3815730886471,19.5667971445598));
#45194=CARTESIAN_POINT('Ctrl Pts',(-13.8104627254334,36.4722767464314,19.5620328833897));
#45195=CARTESIAN_POINT('Ctrl Pts',(-13.7676243767153,36.5831485179276,19.5562092805859));
#45196=CARTESIAN_POINT('Ctrl Pts',(-13.7198739330841,36.6923278457604,19.550385677782));
#45197=CARTESIAN_POINT('Ctrl Pts',(-13.6673654190107,36.7993487386953,19.5445620749782));
#45198=CARTESIAN_POINT('Ctrl Pts',(-13.6149231529138,36.9062346074779,19.5387458195904));
#45199=CARTESIAN_POINT('Ctrl Pts',(-13.5577349346273,37.0109670944149,19.5329295642026));
#45200=CARTESIAN_POINT('Ctrl Pts',(-13.4960035828856,37.1130981871298,19.5271133088149));
#45201=CARTESIAN_POINT('Ctrl Pts',(-13.4343340255014,37.2151270445124,19.5213028756188));
#45202=CARTESIAN_POINT('Ctrl Pts',(-13.3681305918992,37.3145593406558,19.5154924424228));
#45203=CARTESIAN_POINT('Ctrl Pts',(-13.2976426602438,37.4109703202943,19.5096820092268));
#45204=CARTESIAN_POINT('Ctrl Pts',(-13.2244867683692,37.5110304445784,19.5036516517932));
#45205=CARTESIAN_POINT('Ctrl Pts',(-13.1467158323389,37.6078356182348,19.4976212943596));
#45206=CARTESIAN_POINT('Ctrl Pts',(-13.0646591809277,37.7009422623884,19.4915909369261));
#45207=CARTESIAN_POINT('Ctrl Pts',(-12.9856840918765,37.790552371829,19.4857870440407));
#45208=CARTESIAN_POINT('Ctrl Pts',(-12.9027396693396,37.8767363983482,19.4799831511552));
#45209=CARTESIAN_POINT('Ctrl Pts',(-12.8161610255012,37.9591319805726,19.4741792582698));
#45210=CARTESIAN_POINT('Ctrl Pts',(-12.7295951720748,38.0415153903561,19.4683762228035));
#45211=CARTESIAN_POINT('Ctrl Pts',(-12.6393964607655,38.1201111874317,19.4625731873371));
#45212=CARTESIAN_POINT('Ctrl Pts',(-12.545936466874,38.1945942632267,19.4567701518708));
#45213=CARTESIAN_POINT('Ctrl Pts',(-12.4524682235801,38.2690839133948,19.4509666041898));
#45214=CARTESIAN_POINT('Ctrl Pts',(-12.3557384447104,38.3394598660146,19.4451630565089));
#45215=CARTESIAN_POINT('Ctrl Pts',(-12.2561508281849,38.4054380688071,19.4393595088279));
#45216=CARTESIAN_POINT('Ctrl Pts',(-12.1565309190185,38.4714376659303,19.4335540792676));
#45217=CARTESIAN_POINT('Ctrl Pts',(-12.0540516694452,38.5330364517656,19.4277486497073));
#45218=CARTESIAN_POINT('Ctrl Pts',(-11.949144155848,38.5899947158351,19.4219432201469));
#45219=CARTESIAN_POINT('Ctrl Pts',(-11.8441204715464,38.6470160533816,19.4161313618684));
#45220=CARTESIAN_POINT('Ctrl Pts',(-11.7366635148745,38.6993864168409,19.4103195035899));
#45221=CARTESIAN_POINT('Ctrl Pts',(-11.6272274043801,38.7469128591995,19.4045076453114));
#45222=CARTESIAN_POINT('Ctrl Pts',(-11.5177194183068,38.7944705160314,19.3986919699137));
#45223=CARTESIAN_POINT('Ctrl Pts',(-11.406230070125,38.8371777701989,19.392876294516));
#45224=CARTESIAN_POINT('Ctrl Pts',(-11.2932302473512,38.8748910342532,19.3870606191183));
#45225=CARTESIAN_POINT('Ctrl Pts',(-11.1800685697464,38.912658316746,19.3812366136618));
#45226=CARTESIAN_POINT('Ctrl Pts',(-11.0653924905132,38.9454172201218,19.3754126082054));
#45227=CARTESIAN_POINT('Ctrl Pts',(-10.9496848595851,38.97307483789,19.369588602749));
#45228=CARTESIAN_POINT('Ctrl Pts',(-10.9189886450579,38.9804121600832,19.3680435454397));
#45229=CARTESIAN_POINT('Ctrl Pts',(-10.8882198660469,38.9873907390189,19.3664984881305));
#45230=CARTESIAN_POINT('Ctrl Pts',(-10.8573875990365,38.9940094522946,19.3649534308213));
#45231=CARTESIAN_POINT('Ctrl Pts',(-10.7411646735354,39.0189588411828,19.3591293024663));
#45232=CARTESIAN_POINT('Ctrl Pts',(-10.6236644106922,39.0388712407908,19.3533051741113));
#45233=CARTESIAN_POINT('Ctrl Pts',(-10.5053611106736,39.0536200053556,19.3474810457563));
#45234=CARTESIAN_POINT('Ctrl Pts',(-10.3872094693508,39.0683498627689,19.3416643836318));
#45235=CARTESIAN_POINT('Ctrl Pts',(-10.2682572403599,39.0779292021587,19.3358477215073));
#45236=CARTESIAN_POINT('Ctrl Pts',(-10.1489904075468,39.0822820650292,19.3300310593828));
#45237=CARTESIAN_POINT('Ctrl Pts',(-10.0298630210115,39.0866298385508,19.3242211980752));
#45238=CARTESIAN_POINT('Ctrl Pts',(-9.91042216868238,39.085763286278,19.3184113367675));
#45239=CARTESIAN_POINT('Ctrl Pts',(-9.79115965652278,39.0796581610395,19.3126014754599));
#45240=CARTESIAN_POINT('Ctrl Pts',(-9.67197560514657,39.0735570522593,19.3067954363614));
#45241=CARTESIAN_POINT('Ctrl Pts',(-9.55297006689244,39.0622242445947,19.3009893972629));
#45242=CARTESIAN_POINT('Ctrl Pts',(-9.43463532006182,39.0456875532693,19.2951833581645));
#45243=CARTESIAN_POINT('Ctrl Pts',(-9.31635049644983,39.029157838465,19.2893797685254));
#45244=CARTESIAN_POINT('Ctrl Pts',(-9.19873630501614,39.0074286634322,19.2835761788864));
#45245=CARTESIAN_POINT('Ctrl Pts',(-9.08227973382074,38.9805796704807,19.2777725892473));
#45246=CARTESIAN_POINT('Ctrl Pts',(-8.96584481065281,38.9537356684689,19.2719700784333));
#45247=CARTESIAN_POINT('Ctrl Pts',(-8.85056747696325,38.9217738347375,19.2661675676193));
#45248=CARTESIAN_POINT('Ctrl Pts',(-8.73692373103594,38.884824750073,19.2603650568053));
#45249=CARTESIAN_POINT('Ctrl Pts',(-8.62322683247863,38.8478583838502,19.254559832083));
#45250=CARTESIAN_POINT('Ctrl Pts',(-8.51116543836122,38.8059002282797,19.2487546073606));
#45251=CARTESIAN_POINT('Ctrl Pts',(-8.40119956722646,38.7591305079982,19.2429493826383));
#45252=CARTESIAN_POINT('Ctrl Pts',(-8.29121019275929,38.7123507914855,19.237142917148));
#45253=CARTESIAN_POINT('Ctrl Pts',(-8.18331760511866,38.6607576315025,19.2313364516578));
#45254=CARTESIAN_POINT('Ctrl Pts',(-8.07795978764544,38.6045785359861,19.2255299861675));
#45255=CARTESIAN_POINT('Ctrl Pts',(-7.97248665224614,38.5483379504262,19.2197171652916));
#45256=CARTESIAN_POINT('Ctrl Pts',(-7.86955418587233,38.4875016023944,19.2139043444157));
#45257=CARTESIAN_POINT('Ctrl Pts',(-7.76957405592466,38.4223420501165,19.2080915235398));
#45258=CARTESIAN_POINT('Ctrl Pts',(-7.68162083497658,38.3650207353575,19.2029779442807));
#45259=CARTESIAN_POINT('Ctrl Pts',(-7.59595210725508,38.304354525196,19.1978643650215));
#45260=CARTESIAN_POINT('Ctrl Pts',(-7.51282733495087,38.2405550657615,19.1927507857623));
#45261=CARTESIAN_POINT('',(-14.0849997388207,34.9985392348549,19.7396150285601));
#45262=CARTESIAN_POINT('Ctrl Pts',(-14.0849997388207,34.9985392348549,19.7396150285601));
#45263=CARTESIAN_POINT('Ctrl Pts',(-14.0850418772222,35.1163784095191,19.7338448932763));
#45264=CARTESIAN_POINT('Ctrl Pts',(-14.0799808576043,35.2344196440369,19.7280747579925));
#45265=CARTESIAN_POINT('Ctrl Pts',(-14.0697904347134,35.3521800924462,19.7223046227086));
#45266=CARTESIAN_POINT('Ctrl Pts',(-14.0596124124487,35.4697972393143,19.7165415090461));
#45267=CARTESIAN_POINT('Ctrl Pts',(-14.0443174331508,35.5871338681316,19.7107783953837));
#45268=CARTESIAN_POINT('Ctrl Pts',(-14.0239312542512,35.7037060899698,19.7050152817212));
#45269=CARTESIAN_POINT('Ctrl Pts',(-14.0035643215084,35.8201682584586,19.6992576088914));
#45270=CARTESIAN_POINT('Ctrl Pts',(-13.9781158193346,35.9358670471083,19.6934999360617));
#45271=CARTESIAN_POINT('Ctrl Pts',(-13.947663338309,36.0503233632415,19.6877422632319));
#45272=CARTESIAN_POINT('Ctrl Pts',(-13.9172299732922,36.1647078314375,19.6819882046799));
#45273=CARTESIAN_POINT('Ctrl Pts',(-13.8817989825304,36.2778509767239,19.6762341461279));
#45274=CARTESIAN_POINT('Ctrl Pts',(-13.8414989711434,36.3892842238738,19.6704800875759));
#45275=CARTESIAN_POINT('Ctrl Pts',(-13.8012118049636,36.5006819528411,19.6647278630699));
#45276=CARTESIAN_POINT('Ctrl Pts',(-13.7560588443521,36.6103704756653,19.6589756385639));
#45277=CARTESIAN_POINT('Ctrl Pts',(-13.706218251875,36.7178973396186,19.6532234140579));
#45278=CARTESIAN_POINT('Ctrl Pts',(-13.6563812420875,36.825416474222,19.6474716030389));
#45279=CARTESIAN_POINT('Ctrl Pts',(-13.6018574457932,36.9307738811283,19.6417197920198));
#45280=CARTESIAN_POINT('Ctrl Pts',(-13.5428724623509,37.0335387174862,19.6359679810008));
#45281=CARTESIAN_POINT('Ctrl Pts',(-13.4838771575834,37.1363215358666,19.6302151635169));
#45282=CARTESIAN_POINT('Ctrl Pts',(-13.4204193217302,37.2365105209835,19.624462346033));
#45283=CARTESIAN_POINT('Ctrl Pts',(-13.3527692484885,37.3337016446816,19.6187095285492));
#45284=CARTESIAN_POINT('Ctrl Pts',(-13.2850503482449,37.4309916503666,19.6129508581643));
#45285=CARTESIAN_POINT('Ctrl Pts',(-13.2131309324407,37.5252773621647,19.6071921877795));
#45286=CARTESIAN_POINT('Ctrl Pts',(-13.1373232309764,37.6161857625894,19.6014335173946));
#45287=CARTESIAN_POINT('Ctrl Pts',(-13.0614743853006,37.7071435030467,19.5956717215232));
#45288=CARTESIAN_POINT('Ctrl Pts',(-12.9817333321907,37.7947199746858,19.5899099256517));
#45289=CARTESIAN_POINT('Ctrl Pts',(-12.8984497566299,37.8785784700599,19.5841481297803));
#45290=CARTESIAN_POINT('Ctrl Pts',(-12.8150375635516,37.9625664708187,19.5783774357813));
#45291=CARTESIAN_POINT('Ctrl Pts',(-12.7280722283443,38.0428247465532,19.5726067417823));
#45292=CARTESIAN_POINT('Ctrl Pts',(-12.6379373774227,38.1190561701894,19.5668360477833));
#45293=CARTESIAN_POINT('Ctrl Pts',(-12.5752148460843,38.1721036630193,19.562820369813));
#45294=CARTESIAN_POINT('Ctrl Pts',(-12.5109581858319,38.2232020492989,19.5588046918428));
#45295=CARTESIAN_POINT('Ctrl Pts',(-12.4453045396966,38.2722638506299,19.5547890138725));
#45296=CARTESIAN_POINT('Ctrl Pts',(-12.3500926000171,38.343414038683,19.5489654151666));
#45297=CARTESIAN_POINT('Ctrl Pts',(-12.2516191994198,38.4105199874075,19.5431418164606));
#45298=CARTESIAN_POINT('Ctrl Pts',(-12.1502624669472,38.4732688239234,19.5373182177547));
#45299=CARTESIAN_POINT('Ctrl Pts',(-12.0490336105157,38.535938493791,19.5315019663529));
#45300=CARTESIAN_POINT('Ctrl Pts',(-11.9449290017087,38.5942617720503,19.5256857149512));
#45301=CARTESIAN_POINT('Ctrl Pts',(-11.8383585470582,38.6479669478297,19.5198694635494));
#45302=CARTESIAN_POINT('Ctrl Pts',(-11.7318947695989,38.7016183646445,19.5140590342244));
#45303=CARTESIAN_POINT('Ctrl Pts',(-11.6229704192588,38.7506606926182,19.5082486048994));
#45304=CARTESIAN_POINT('Ctrl Pts',(-11.5120224817609,38.7948666662545,19.5024381755743));
#45305=CARTESIAN_POINT('Ctrl Pts',(-11.3968750721636,38.8407458729144,19.4964078166464));
#45306=CARTESIAN_POINT('Ctrl Pts',(-11.2795482409027,38.8814151354747,19.4903774577185));
#45307=CARTESIAN_POINT('Ctrl Pts',(-11.1605567036874,38.9166737338622,19.4843470987906));
#45308=CARTESIAN_POINT('Ctrl Pts',(-11.0460338833157,38.9506081986502,19.4785432094683));
#45309=CARTESIAN_POINT('Ctrl Pts',(-10.929969564689,38.9795309383138,19.4727393201461));
#45310=CARTESIAN_POINT('Ctrl Pts',(-10.8128401968705,39.0033131047111,19.4669354308239));
#45311=CARTESIAN_POINT('Ctrl Pts',(-10.6957281303837,39.0270917582136,19.4611323988017));
#45312=CARTESIAN_POINT('Ctrl Pts',(-10.5775517276272,39.0457312672697,19.4553293667795));
#45313=CARTESIAN_POINT('Ctrl Pts',(-10.4587985262156,39.0591537187377,19.4495263347574));
#45314=CARTESIAN_POINT('Ctrl Pts',(-10.3400348403481,39.0725773552441,19.4437227903984));
#45315=CARTESIAN_POINT('Ctrl Pts',(-10.2206946603482,39.0807829725099,19.4379192460395));
#45316=CARTESIAN_POINT('Ctrl Pts',(-10.1012709142005,39.0837445074266,19.4321157016805));
#45317=CARTESIAN_POINT('Ctrl Pts',(-9.98180844067378,39.0867070027259,19.4263102753168));
#45318=CARTESIAN_POINT('Ctrl Pts',(-9.86226275510547,39.0844220234896,19.4205048489531));
#45319=CARTESIAN_POINT('Ctrl Pts',(-9.74312641102951,39.0769156183676,19.4146994225893));
#45320=CARTESIAN_POINT('Ctrl Pts',(-9.62385813558292,39.0694009006662,19.408887567307));
#45321=CARTESIAN_POINT('Ctrl Pts',(-9.50500051423202,39.05665324101,19.4030757120247));
#45322=CARTESIAN_POINT('Ctrl Pts',(-9.38704076585035,39.0387505465516,19.3972638567424));
#45323=CARTESIAN_POINT('Ctrl Pts',(-9.26900354139001,39.0208360935859,19.3914481842278));
#45324=CARTESIAN_POINT('Ctrl Pts',(-9.15186576406399,38.9977599415919,19.3856325117132));
#45325=CARTESIAN_POINT('Ctrl Pts',(-9.0361026244213,38.9696507213296,19.3798168391986));
#45326=CARTESIAN_POINT('Ctrl Pts',(-8.92017366812708,38.9415012380198,19.3739928364388));
#45327=CARTESIAN_POINT('Ctrl Pts',(-8.80562367034322,38.9083044104079,19.368168833679));
#45328=CARTESIAN_POINT('Ctrl Pts',(-8.69291101949768,38.8702381576654,19.3623448309191));
#45329=CARTESIAN_POINT('Ctrl Pts',(-8.66300870275553,38.8601392988581,19.3607997410475));
#45330=CARTESIAN_POINT('Ctrl Pts',(-8.63323558306982,38.8496979759635,19.3592546511758));
#45331=CARTESIAN_POINT('Ctrl Pts',(-8.60359994598701,38.8389180623129,19.3577095613041));
#45332=CARTESIAN_POINT('Ctrl Pts',(-8.49191615552896,38.7982932694686,19.3518867914752));
#45333=CARTESIAN_POINT('Ctrl Pts',(-8.38182657469041,38.7527251855687,19.3460640216462));
#45334=CARTESIAN_POINT('Ctrl Pts',(-8.27379996102366,38.7023584949918,19.3402412518173));
#45335=CARTESIAN_POINT('Ctrl Pts',(-8.16589302847115,38.6520476049389,19.3344249329503));
#45336=CARTESIAN_POINT('Ctrl Pts',(-8.06004488713174,38.5969488455534,19.3286086140834));
#45337=CARTESIAN_POINT('Ctrl Pts',(-7.95670750458039,38.5372561086472,19.3227922952165));
#45338=CARTESIAN_POINT('Ctrl Pts',(-7.85348150833941,38.4776277139331,19.3169822457003));
#45339=CARTESIAN_POINT('Ctrl Pts',(-7.75276123655803,38.4134153993639,19.3111721961842));
#45340=CARTESIAN_POINT('Ctrl Pts',(-7.65497622910664,38.344860014103,19.305362146668));
#45341=CARTESIAN_POINT('Ctrl Pts',(-7.60686683227912,38.3111313442369,19.3025036514339));
#45342=CARTESIAN_POINT('Ctrl Pts',(-7.55946757667728,38.2763521227345,19.2996451561999));
#45343=CARTESIAN_POINT('Ctrl Pts',(-7.51282733495083,38.2405550657615,19.2967866609659));
#45344=CARTESIAN_POINT('Ctrl Pts',(-7.51282733495085,38.2405550657615,20.5469196478657));
#45345=CARTESIAN_POINT('Ctrl Pts',(-7.47644404336342,38.2126303656825,20.5446751908154));
#45346=CARTESIAN_POINT('Ctrl Pts',(-7.44055209258124,38.1841089670783,20.5424307337651));
#45347=CARTESIAN_POINT('Ctrl Pts',(-7.40517161095562,38.1550104011571,20.5401862767148));
#45348=CARTESIAN_POINT('Ctrl Pts',(-7.31337143935251,38.0795096385265,20.5343626832275));
#45349=CARTESIAN_POINT('Ctrl Pts',(-7.22472119485878,37.9998771861964,20.5285390897402));
#45350=CARTESIAN_POINT('Ctrl Pts',(-7.1396148866694,37.9164056651016,20.5227154962529));
#45351=CARTESIAN_POINT('Ctrl Pts',(-7.05461595272924,37.8330394557293,20.5168992500938));
#45352=CARTESIAN_POINT('Ctrl Pts',(-6.97315235093204,37.7458440947145,20.5110830039347));
#45353=CARTESIAN_POINT('Ctrl Pts',(-6.89558569271732,37.6551528786001,20.5052667577756));
#45354=CARTESIAN_POINT('Ctrl Pts',(-6.81809667915196,37.5645524448894,20.4994563337107));
#45355=CARTESIAN_POINT('Ctrl Pts',(-6.74449711277133,37.4704634261763,20.4936459096458));
#45356=CARTESIAN_POINT('Ctrl Pts',(-6.67511189832342,37.3732560147042,20.4878354855809));
#45357=CARTESIAN_POINT('Ctrl Pts',(-6.60310030689818,37.2723690973092,20.4818051246878));
#45358=CARTESIAN_POINT('Ctrl Pts',(-6.53562873547309,37.1681233610124,20.4757747637947));
#45359=CARTESIAN_POINT('Ctrl Pts',(-6.47301484400611,37.0609708172118,20.4697444029016));
#45360=CARTESIAN_POINT('Ctrl Pts',(-6.41275248615357,36.9578425051387,20.4639405188496));
#45361=CARTESIAN_POINT('Ctrl Pts',(-6.35698974174589,36.852022169106,20.4581366347976));
#45362=CARTESIAN_POINT('Ctrl Pts',(-6.30596534635692,36.7439417930894,20.4523327507455));
#45363=CARTESIAN_POINT('Ctrl Pts',(-6.25494848780699,36.6358773816795,20.4465297239881));
#45364=CARTESIAN_POINT('Ctrl Pts',(-6.20866876066544,36.5255539633277,20.4407266972307));
#45365=CARTESIAN_POINT('Ctrl Pts',(-6.1673180785442,36.4134264356329,20.4349236704733));
#45366=CARTESIAN_POINT('Ctrl Pts',(-6.12596374558054,36.3012890082239,20.429120131368));
#45367=CARTESIAN_POINT('Ctrl Pts',(-6.08953946418185,36.1873475379103,20.4233165922627));
#45368=CARTESIAN_POINT('Ctrl Pts',(-6.05818807868422,36.0720745202516,20.4175130531573));
#45369=CARTESIAN_POINT('Ctrl Pts',(-6.02682652628934,35.9567641208663,20.4117076320304));
#45370=CARTESIAN_POINT('Ctrl Pts',(-6.00054124860252,35.8401217091931,20.4059022109034));
#45371=CARTESIAN_POINT('Ctrl Pts',(-5.979424391948,35.7226318425985,20.4000967897765));
#45372=CARTESIAN_POINT('Ctrl Pts',(-5.95828415031718,35.605011866784,20.3942849396796));
#45373=CARTESIAN_POINT('Ctrl Pts',(-5.94232382669346,35.4865429649003,20.3884730895828));
#45374=CARTESIAN_POINT('Ctrl Pts',(-5.93158393263372,35.3677168785845,20.3826612394859));
#45375=CARTESIAN_POINT('Ctrl Pts',(-5.9208369845507,35.2488127466218,20.376845572133));
#45376=CARTESIAN_POINT('Ctrl Pts',(-5.9153173134238,35.1295513699764,20.3710299047801));
#45377=CARTESIAN_POINT('Ctrl Pts',(-5.91501330217704,35.0104249033315,20.3652142374271));
#45378=CARTESIAN_POINT('Ctrl Pts',(-5.91470885546679,34.8911278008061,20.3593902397548));
#45379=CARTESIAN_POINT('Ctrl Pts',(-5.91963496328685,34.7719664005263,20.3535662420825));
#45380=CARTESIAN_POINT('Ctrl Pts',(-5.92972813547437,34.6534282919063,20.3477422444101));
#45381=CARTESIAN_POINT('Ctrl Pts',(-5.93240591212172,34.6219794497397,20.3461971043222));
#45382=CARTESIAN_POINT('Ctrl Pts',(-5.93544710453927,34.5905744243414,20.3446519642342));
#45383=CARTESIAN_POINT('Ctrl Pts',(-5.93884992652121,34.5592221867163,20.3431068241463));
#45384=CARTESIAN_POINT('Ctrl Pts',(-5.95167507597917,34.4410564009306,20.3372832304742));
#45385=CARTESIAN_POINT('Ctrl Pts',(-5.9696825270576,34.3232602815359,20.3314596368022));
#45386=CARTESIAN_POINT('Ctrl Pts',(-5.99284352153456,34.2063237706139,20.3256360431301));
#45387=CARTESIAN_POINT('Ctrl Pts',(-6.01597529497003,34.0895347925038,20.3198197967882));
#45388=CARTESIAN_POINT('Ctrl Pts',(-6.04424760091767,33.9736036627986,20.3140035504462));
#45389=CARTESIAN_POINT('Ctrl Pts',(-6.07757990198118,33.8590155239189,20.3081873041043));
#45390=CARTESIAN_POINT('Ctrl Pts',(-6.11087883721793,33.7445420884311,20.3023768798587));
#45391=CARTESIAN_POINT('Ctrl Pts',(-6.14922757781491,33.6314093591995,20.2965664556131));
#45392=CARTESIAN_POINT('Ctrl Pts',(-6.19249460660536,33.520092003106,20.2907560313675));
#45393=CARTESIAN_POINT('Ctrl Pts',(-6.23739938195125,33.4045610547785,20.2847256705429));
#45394=CARTESIAN_POINT('Ctrl Pts',(-6.28760204991982,33.2909860659518,20.2786953097183));
#45395=CARTESIAN_POINT('Ctrl Pts',(-6.34289869086028,33.1798804943937,20.2726649488938));
#45396=CARTESIAN_POINT('Ctrl Pts',(-6.39611860778833,33.0729476104427,20.2668610646673));
#45397=CARTESIAN_POINT('Ctrl Pts',(-6.45405658031249,32.9683024039722,20.2610571804409));
#45398=CARTESIAN_POINT('Ctrl Pts',(-6.51648217564307,32.8663813444321,20.2552532962144));
#45399=CARTESIAN_POINT('Ctrl Pts',(-6.57889855002973,32.7644753397483,20.2494502692853));
#45400=CARTESIAN_POINT('Ctrl Pts',(-6.64580101576262,32.6652930298942,20.2436472423561));
#45401=CARTESIAN_POINT('Ctrl Pts',(-6.71691430966396,32.5692442841966,20.2378442154269));
#45402=CARTESIAN_POINT('Ctrl Pts',(-6.78803388210761,32.4731870584234,20.2320406761525));
#45403=CARTESIAN_POINT('Ctrl Pts',(-6.8633647788998,32.3802642750675,20.2262371368782));
#45404=CARTESIAN_POINT('Ctrl Pts',(-6.94259012044536,32.290854409892,20.2204335976039));
#45405=CARTESIAN_POINT('Ctrl Pts',(-7.0218411538256,32.201415550162,20.2146281763109));
#45406=CARTESIAN_POINT('Ctrl Pts',(-7.104988872959,32.1154921796808,20.2088227550179));
#45407=CARTESIAN_POINT('Ctrl Pts',(-7.19167851929846,32.0334269837015,20.2030173337249));
#45408=CARTESIAN_POINT('Ctrl Pts',(-7.27846416636655,31.9512709081427,20.1972054834672));
#45409=CARTESIAN_POINT('Ctrl Pts',(-7.36879927328299,31.8729818163873,20.1913936332096));
#45410=CARTESIAN_POINT('Ctrl Pts',(-7.46229476848371,31.798863146016,20.1855817829519));
#45411=CARTESIAN_POINT('Ctrl Pts',(-7.55585167200815,31.7246957941194,20.179766115441));
#45412=CARTESIAN_POINT('Ctrl Pts',(-7.6525727676968,31.6547045575369,20.1739504479301));
#45413=CARTESIAN_POINT('Ctrl Pts',(-7.75204006350553,31.589149501383,20.1681347804191));
#45414=CARTESIAN_POINT('Ctrl Pts',(-7.85164983544689,31.5235005447083,20.1623107825941));
#45415=CARTESIAN_POINT('Ctrl Pts',(-7.95401330959738,31.46230066019,20.1564867847691));
#45416=CARTESIAN_POINT('Ctrl Pts',(-8.05868787723299,31.4057640252763,20.1506627869441));
#45417=CARTESIAN_POINT('Ctrl Pts',(-8.08645861215048,31.3907645470193,20.1491176484887));
#45418=CARTESIAN_POINT('Ctrl Pts',(-8.11439191093491,31.3760930372918,20.1475725100333));
#45419=CARTESIAN_POINT('Ctrl Pts',(-8.14247929139104,31.3617529197306,20.1460273715779));
#45420=CARTESIAN_POINT('Ctrl Pts',(-8.24834003867474,31.3077053176931,20.1402037771774));
#45421=CARTESIAN_POINT('Ctrl Pts',(-8.35673235697298,31.2581946822142,20.134380182777));
#45422=CARTESIAN_POINT('Ctrl Pts',(-8.46723070851764,31.2134655291297,20.1285565883766));
#45423=CARTESIAN_POINT('Ctrl Pts',(-8.57758965004794,31.1687928084878,20.1227403413018));
#45424=CARTESIAN_POINT('Ctrl Pts',(-8.69004896480404,31.1288897235107,20.1169240942271));
#45425=CARTESIAN_POINT('Ctrl Pts',(-8.80415874586783,31.0939548524223,20.1111078471524));
#45426=CARTESIAN_POINT('Ctrl Pts',(-8.91815430246159,31.0590549513171,20.1052974221705));
#45427=CARTESIAN_POINT('Ctrl Pts',(-9.03379665046037,31.02911348937,20.0994869971886));
#45428=CARTESIAN_POINT('Ctrl Pts',(-9.15061669913917,31.0042806644837,20.0936765722067));
#45429=CARTESIAN_POINT('Ctrl Pts',(-9.27185860746496,30.9785078702384,20.0876462116568));
#45430=CARTESIAN_POINT('Ctrl Pts',(-9.39436871897362,30.9582382657709,20.0816158511069));
#45431=CARTESIAN_POINT('Ctrl Pts',(-9.51760581123321,30.9435827573283,20.075585490557));
#45432=CARTESIAN_POINT('Ctrl Pts',(-9.63621462428657,30.9294776496112,20.0697816055903));
#45433=CARTESIAN_POINT('Ctrl Pts',(-9.75549635605137,30.9205726101855,20.0639777206236));
#45434=CARTESIAN_POINT('Ctrl Pts',(-9.87495964110511,30.9169141683468,20.0581738356569));
#45435=CARTESIAN_POINT('Ctrl Pts',(-9.99440528012957,30.9132562668997,20.0523708079873));
#45436=CARTESIAN_POINT('Ctrl Pts',(-10.1140320110764,30.9148434343454,20.0465677803176));
#45437=CARTESIAN_POINT('Ctrl Pts',(-10.2333461417158,30.9216701239176,20.040764752648));
#45438=CARTESIAN_POINT('Ctrl Pts',(-10.3526708065008,30.9284974162125,20.0349612126339));
#45439=CARTESIAN_POINT('Ctrl Pts',(-10.4716824084144,30.9405651270542,20.0291576726197));
#45440=CARTESIAN_POINT('Ctrl Pts',(-10.589890699295,30.9578156940974,20.0233541326056));
#45441=CARTESIAN_POINT('Ctrl Pts',(-10.7081373236823,30.9750718552891,20.0175487105742));
#45442=CARTESIAN_POINT('Ctrl Pts',(-10.825579715104,30.9975141563537,20.0117432885429));
#45443=CARTESIAN_POINT('Ctrl Pts',(-10.9417367956866,31.0250337350299,20.0059378665115));
#45444=CARTESIAN_POINT('Ctrl Pts',(-11.0580225093099,31.052583789051,20.0001260155213));
#45445=CARTESIAN_POINT('Ctrl Pts',(-11.1730196733704,31.0852222496975,19.9943141645311));
#45446=CARTESIAN_POINT('Ctrl Pts',(-11.2862612264689,31.1227900421459,19.9885023135409));
#45447=CARTESIAN_POINT('Ctrl Pts',(-11.3995771571447,31.1603825092947,19.9826866453));
#45448=CARTESIAN_POINT('Ctrl Pts',(-11.5111347997691,31.2029106109023,19.9768709770592));
#45449=CARTESIAN_POINT('Ctrl Pts',(-11.620487515265,31.2501673086829,19.9710553088183));
#45450=CARTESIAN_POINT('Ctrl Pts',(-11.7299968664924,31.2974916964829,19.9652313102726));
#45451=CARTESIAN_POINT('Ctrl Pts',(-11.8372946207,31.3495580217486,19.959407311727));
#45452=CARTESIAN_POINT('Ctrl Pts',(-11.9419590239602,31.4061135035648,19.9535833131813));
#45453=CARTESIAN_POINT('Ctrl Pts',(-11.9697269318143,31.4211179115468,19.9520381817907));
#45454=CARTESIAN_POINT('Ctrl Pts',(-11.9973096495272,31.4364380607679,19.9504930504001));
#45455=CARTESIAN_POINT('Ctrl Pts',(-12.0246996641409,31.4520687337509,19.9489479190094));
#45456=CARTESIAN_POINT('Ctrl Pts',(-12.1279324850377,31.5109806579436,19.9431243269318));
#45457=CARTESIAN_POINT('Ctrl Pts',(-12.2287584357382,31.5744969117993,19.9373007348541));
#45458=CARTESIAN_POINT('Ctrl Pts',(-12.3267397461459,31.642395622813,19.9314771427765));
#45459=CARTESIAN_POINT('Ctrl Pts',(-12.4245974385545,31.710208669502,19.9256608980266));
#45460=CARTESIAN_POINT('Ctrl Pts',(-12.5196172963132,31.7823929455247,19.9198446532766));
#45461=CARTESIAN_POINT('Ctrl Pts',(-12.6113866119169,31.8586810153852,19.9140284085267));
#45462=CARTESIAN_POINT('Ctrl Pts',(-12.7030640659445,31.9348927204794,19.9082179858689));
#45463=CARTESIAN_POINT('Ctrl Pts',(-12.7914971386674,32.0151997876799,19.9024075632112));
#45464=CARTESIAN_POINT('Ctrl Pts',(-12.8763030706051,32.0992922163672,19.8965971405534));
#45465=CARTESIAN_POINT('Ctrl Pts',(-12.9643191152854,32.1865677499473,19.890566779132));
#45466=CARTESIAN_POINT('Ctrl Pts',(-13.0484276328377,32.2779206224034,19.8845364177107));
#45467=CARTESIAN_POINT('Ctrl Pts',(-13.1282391855969,32.3729589653574,19.8785060562893));
#45468=CARTESIAN_POINT('Ctrl Pts',(-13.2050533024765,32.4644280087644,19.8727021736304));
#45469=CARTESIAN_POINT('Ctrl Pts',(-13.2778871049818,32.5593103479768,19.8668982909714));
#45470=CARTESIAN_POINT('Ctrl Pts',(-13.3464323288902,32.6572205250688,19.8610944083124));
#45471=CARTESIAN_POINT('Ctrl Pts',(-13.414967428036,32.7551162399235,19.8552913829405));
#45472=CARTESIAN_POINT('Ctrl Pts',(-13.4792149742207,32.8560385688199,19.8494883575686));
#45473=CARTESIAN_POINT('Ctrl Pts',(-13.5389089826654,32.9595715615562,19.8436853321967));
#45474=CARTESIAN_POINT('Ctrl Pts',(-13.5986082615749,33.0631136953605,19.8378817944678));
#45475=CARTESIAN_POINT('Ctrl Pts',(-13.6537529994241,33.1692665975251,19.8320782567389));
#45476=CARTESIAN_POINT('Ctrl Pts',(-13.7041226036779,33.2775886853244,19.82627471901));
#45477=CARTESIAN_POINT('Ctrl Pts',(-13.7545085423157,33.3859459009474,19.820469299249));
#45478=CARTESIAN_POINT('Ctrl Pts',(-13.8001160955967,33.4964733311269,19.814663879488));
#45479=CARTESIAN_POINT('Ctrl Pts',(-13.8407726035764,33.6087089421631,19.808858459727));
#45480=CARTESIAN_POINT('Ctrl Pts',(-13.881474135066,33.7210688442758,19.8030466109737));
#45481=CARTESIAN_POINT('Ctrl Pts',(-13.9172135378649,33.8351403190091,19.7972347622205));
#45482=CARTESIAN_POINT('Ctrl Pts',(-13.9478678316903,33.9504455309489,19.7914229134673));
#45483=CARTESIAN_POINT('Ctrl Pts',(-13.9785422594946,34.06582647625,19.7856072474465));
#45484=CARTESIAN_POINT('Ctrl Pts',(-14.0041248394553,34.1824423746108,19.7797915814257));
#45485=CARTESIAN_POINT('Ctrl Pts',(-14.0245439013221,34.2998061794537,19.773975915405));
#45486=CARTESIAN_POINT('Ctrl Pts',(-14.0449922114049,34.4173380959335,19.7681519190379));
#45487=CARTESIAN_POINT('Ctrl Pts',(-14.0602621888624,34.5356196536117,19.7623279226709));
#45488=CARTESIAN_POINT('Ctrl Pts',(-14.0703340623937,34.6541595447062,19.7565039263038));
#45489=CARTESIAN_POINT('Ctrl Pts',(-14.0730062118111,34.6856091354846,19.7549587730162));
#45490=CARTESIAN_POINT('Ctrl Pts',(-14.0753127595328,34.7170769169523,19.7534136197286));
#45491=CARTESIAN_POINT('Ctrl Pts',(-14.0772539509919,34.7485537450649,19.751868466441));
#45492=CARTESIAN_POINT('Ctrl Pts',(-14.0823853229795,34.8317600219526,19.7477839871591));
#45493=CARTESIAN_POINT('Ctrl Pts',(-14.0849699104881,34.9151249563342,19.7436995078773));
#45494=CARTESIAN_POINT('Ctrl Pts',(-14.0849997388204,34.9985392341328,19.7396150285955));
#45495=CARTESIAN_POINT('Origin',(-10.,35.,32.7603849714045));
#45496=CARTESIAN_POINT('',(-7.51282733495087,38.2405550657615,21.796951697066));
#45497=CARTESIAN_POINT('',(-7.51282733495086,38.2405550657615,21.6925401826178));
#45498=CARTESIAN_POINT('',(-7.51282733495086,38.2405550657615,32.7603849714045));
#45499=CARTESIAN_POINT('',(-14.084998525967,34.996529719382,20.8853849714301));
#45500=CARTESIAN_POINT('Ctrl Pts',(-7.51282733495086,38.2405550657615,21.6925401826178));
#45501=CARTESIAN_POINT('Ctrl Pts',(-7.4182381975729,38.1679565410881,21.6867304536884));
#45502=CARTESIAN_POINT('Ctrl Pts',(-7.32673645481531,38.0911410533406,21.680920724759));
#45503=CARTESIAN_POINT('Ctrl Pts',(-7.23871595880767,38.0104045315965,21.6751109958296));
#45504=CARTESIAN_POINT('Ctrl Pts',(-7.14889627851993,37.9280177137584,21.6691825130481));
#45505=CARTESIAN_POINT('Ctrl Pts',(-7.06270208366081,37.8415480444578,21.6632540302666));
#45506=CARTESIAN_POINT('Ctrl Pts',(-6.98051717086134,37.7513539293477,21.6573255474852));
#45507=CARTESIAN_POINT('Ctrl Pts',(-6.90006201646432,37.6630581435434,21.6515218423856));
#45508=CARTESIAN_POINT('Ctrl Pts',(-6.82344932057546,37.5711934669989,21.645718137286));
#45509=CARTESIAN_POINT('Ctrl Pts',(-6.75100187895214,37.4761333181853,21.6399144321864));
#45510=CARTESIAN_POINT('Ctrl Pts',(-6.67856303800499,37.3810844545399,21.6341114160799));
#45511=CARTESIAN_POINT('Ctrl Pts',(-6.61028871537809,37.2828411977853,21.6283083999734));
#45512=CARTESIAN_POINT('Ctrl Pts',(-6.54646060282584,37.1818090274279,21.622505383867));
#45513=CARTESIAN_POINT('Ctrl Pts',(-6.482625004261,37.0807650076194,21.6167016871599));
#45514=CARTESIAN_POINT('Ctrl Pts',(-6.42323687074606,36.9769317690469,21.6108979904528));
#45515=CARTESIAN_POINT('Ctrl Pts',(-6.36853349851039,36.870742111719,21.6050942937457));
#45516=CARTESIAN_POINT('Ctrl Pts',(-6.31177021911534,36.7605537825278,21.5990720533564));
#45517=CARTESIAN_POINT('Ctrl Pts',(-6.26005167499529,36.647828502816,21.5930498129671));
#45518=CARTESIAN_POINT('Ctrl Pts',(-6.21358909714194,36.533074517014,21.5870275725778));
#45519=CARTESIAN_POINT('Ctrl Pts',(-6.16874563957074,36.4223194592623,21.5812151942325));
#45520=CARTESIAN_POINT('Ctrl Pts',(-6.12879802966201,36.3096751367095,21.5754028158873));
#45521=CARTESIAN_POINT('Ctrl Pts',(-6.09388551090899,36.1956147364905,21.569590437542));
#45522=CARTESIAN_POINT('Ctrl Pts',(-6.05894887807914,36.0814755547527,21.563774044587));
#45523=CARTESIAN_POINT('Ctrl Pts',(-6.02905436381748,35.9659187417862,21.5579576516319));
#45524=CARTESIAN_POINT('Ctrl Pts',(-6.00429025138867,35.8494283988968,21.5521412586769));
#45525=CARTESIAN_POINT('Ctrl Pts',(-5.97949170059666,35.7327760580053,21.5463167771197));
#45526=CARTESIAN_POINT('Ctrl Pts',(-5.9598378545568,35.6151879976554,21.5404922955625));
#45527=CARTESIAN_POINT('Ctrl Pts',(-5.94536528078422,35.4971541951246,21.5346678140054));
#45528=CARTESIAN_POINT('Ctrl Pts',(-5.94384094504857,35.4847221877954,21.534054345695));
#45529=CARTESIAN_POINT('Ctrl Pts',(-5.94237404025469,35.4722852357941,21.5334408773846));
#45530=CARTESIAN_POINT('Ctrl Pts',(-5.94096457550343,35.4598439112155,21.5328274090742));
#45531=CARTESIAN_POINT('Ctrl Pts',(-5.92758466681423,35.3417396544853,21.5270038154232));
#45532=CARTESIAN_POINT('Ctrl Pts',(-5.91934211447414,35.2228604957279,21.5211802217721));
#45533=CARTESIAN_POINT('Ctrl Pts',(-5.91631621890921,35.1036907713156,21.5153566281211));
#45534=CARTESIAN_POINT('Ctrl Pts',(-5.91329414096098,34.9846713972114,21.5095403817985));
#45535=CARTESIAN_POINT('Ctrl Pts',(-5.91547563943873,34.8653625912019,21.5037241354758));
#45536=CARTESIAN_POINT('Ctrl Pts',(-5.92288844228433,34.7462553528815,21.4979078891532));
#45537=CARTESIAN_POINT('Ctrl Pts',(-5.93029382487344,34.6272673415628,21.4920974649252));
#45538=CARTESIAN_POINT('Ctrl Pts',(-5.94292006911531,34.5084809017419,21.4862870406972));
#45539=CARTESIAN_POINT('Ctrl Pts',(-5.96074286670309,34.3903879831318,21.4804766164691));
#45540=CARTESIAN_POINT('Ctrl Pts',(-5.97924029413158,34.2678250027103,21.4744462556373));
#45541=CARTESIAN_POINT('Ctrl Pts',(-6.00333545989573,34.1460095313729,21.4684158948055));
#45542=CARTESIAN_POINT('Ctrl Pts',(-6.03294191299889,34.0254872323263,21.4623855339737));
#45543=CARTESIAN_POINT('Ctrl Pts',(-6.06143646424841,33.9094912764808,21.4565816497605));
#45544=CARTESIAN_POINT('Ctrl Pts',(-6.09503569745824,33.7946935438724,21.4507777655472));
#45545=CARTESIAN_POINT('Ctrl Pts',(-6.13361042261505,33.6815703902411,21.444973881334));
#45546=CARTESIAN_POINT('Ctrl Pts',(-6.17217944987339,33.5684639461066,21.4391708544164));
#45547=CARTESIAN_POINT('Ctrl Pts',(-6.21572237577386,33.4570319754221,21.4333678274988));
#45548=CARTESIAN_POINT('Ctrl Pts',(-6.26406044064626,33.3477347038518,21.4275648005812));
#45549=CARTESIAN_POINT('Ctrl Pts',(-6.31240277326573,33.2384277824721,21.4217612613168));
#45550=CARTESIAN_POINT('Ctrl Pts',(-6.36554092143188,33.1312563083968,21.4159577220525));
#45551=CARTESIAN_POINT('Ctrl Pts',(-6.42324864130282,33.0266589960025,21.4101541827881));
#45552=CARTESIAN_POINT('Ctrl Pts',(-6.48097507511621,32.9220277639161,21.4043487615034));
#45553=CARTESIAN_POINT('Ctrl Pts',(-6.54327383056353,32.8199727110296,21.3985433402188));
#45554=CARTESIAN_POINT('Ctrl Pts',(-6.6098738627712,32.720905931367,21.3927379189341));
#45555=CARTESIAN_POINT('Ctrl Pts',(-6.67654764835466,32.6217294444087,21.3869260686823));
#45556=CARTESIAN_POINT('Ctrl Pts',(-6.74753199063213,32.5255481752715,21.3811142184305));
#45557=CARTESIAN_POINT('Ctrl Pts',(-6.8225137654087,32.4327434430928,21.3753023681788));
#45558=CARTESIAN_POINT('Ctrl Pts',(-6.89754478862016,32.3398777562645,21.3694867006723));
#45559=CARTESIAN_POINT('Ctrl Pts',(-6.97657820346002,32.2503933284084,21.3636710331659));
#45560=CARTESIAN_POINT('Ctrl Pts',(-7.0592631640353,32.164635497577,21.3578553656594));
#45561=CARTESIAN_POINT('Ctrl Pts',(-7.14206656189467,32.0787548279065,21.3520313678368));
#45562=CARTESIAN_POINT('Ctrl Pts',(-7.22853165018271,31.9966116897609,21.3462073700142));
#45563=CARTESIAN_POINT('Ctrl Pts',(-7.31827350936087,31.9185120429565,21.3403833721916));
#45564=CARTESIAN_POINT('Ctrl Pts',(-7.34208251675777,31.8977917783498,21.3388382336296));
#45565=CARTESIAN_POINT('Ctrl Pts',(-7.36612200402485,31.8773558892563,21.3372930950677));
#45566=CARTESIAN_POINT('Ctrl Pts',(-7.39038444532685,31.8572095747874,21.3357479565057));
#45567=CARTESIAN_POINT('Ctrl Pts',(-7.48182905933954,31.78127855336,21.3299243628436));
#45568=CARTESIAN_POINT('Ctrl Pts',(-7.57673789068907,31.7092194954885,21.3241007691814));
#45569=CARTESIAN_POINT('Ctrl Pts',(-7.67474932401372,31.6413642213206,21.3182771755193));
#45570=CARTESIAN_POINT('Ctrl Pts',(-7.77263710135293,31.5735945566628,21.3124609291858));
#45571=CARTESIAN_POINT('Ctrl Pts',(-7.87361936226054,31.5100183571618,21.3066446828523));
#45572=CARTESIAN_POINT('Ctrl Pts',(-7.97730064829077,31.4509279617631,21.3008284365188));
